#372230=CARTESIAN_POINT('Ctrl Pts',(-1.35705080756888,6.03041012221051E-16,
1.4375));
#372231=CARTESIAN_POINT('Ctrl Pts',(-1.01778810567666,-0.587620236790416,
1.47916666666667));
#372232=CARTESIAN_POINT('Ctrl Pts',(-0.678525403784438,-1.17524047358083,
1.52083333333333));
#372233=CARTESIAN_POINT('Ctrl Pts',(-1.43925448419919E-16,-1.17524047358083,
1.5625));
#372234=CARTESIAN_POINT('Ctrl Pts',(-1.43925448419919E-16,-1.17524047358083,
1.));
#372235=CARTESIAN_POINT('Ctrl Pts',(0.678525403784437,-1.17524047358083,
1.04166666666667));
#372236=CARTESIAN_POINT('Ctrl Pts',(1.01778810567666,-0.587620236790417,
1.08333333333333));
#372237=CARTESIAN_POINT('Ctrl Pts',(1.35705080756888,2.7065942666714E-16,
1.125));
#372238=CARTESIAN_POINT('Ctrl Pts',(1.01778810567666,0.587620236790417,
1.16666666666667));
#372239=CARTESIAN_POINT('Ctrl Pts',(0.678525403784439,1.17524047358083,
1.20833333333333));
#372240=CARTESIAN_POINT('Ctrl Pts',(0.,1.17524047358083,1.25));
#372241=CARTESIAN_POINT('Ctrl Pts',(-0.678525403784438,1.17524047358083,
1.29166666666667));
#372242=CARTESIAN_POINT('Ctrl Pts',(-1.01778810567666,0.587620236790418,
1.33333333333333));
#372243=CARTESIAN_POINT('Ctrl Pts',(-1.35705080756888,6.03041012221051E-16,
1.375));
#372244=CARTESIAN_POINT('Ctrl Pts',(-1.01778810567666,-0.587620236790416,
1.41666666666667));
#372245=CARTESIAN_POINT('Ctrl Pts',(-0.678525403784438,-1.17524047358083,
1.45833333333333));
#372246=CARTESIAN_POINT('Ctrl Pts',(-1.43925448419919E-16,-1.17524047358083,
1.5));
#372247=CARTESIAN_POINT('Origin',(6.93889390390723E-17,9.71445146547012E-16,
-9.21875));
#372248=CARTESIAN_POINT('',(6.93889390390724E-17,-1.17524047358083,2.0625));
#372249=CARTESIAN_POINT('',(6.93889390390724E-17,-1.17524047358083,2.));
#372250=CARTESIAN_POINT('',(2.82703326498063E-16,-1.17524047358083,-9.21875));
#372251=CARTESIAN_POINT('Ctrl Pts',(-1.43925448419919E-16,-1.17524047358083,
1.5625));
#372252=CARTESIAN_POINT('Ctrl Pts',(0.678525403784437,-1.17524047358083,
1.60416666666667));
#372253=CARTESIAN_POINT('Ctrl Pts',(1.01778810567666,-0.587620236790417,
1.64583333333333));
#372254=CARTESIAN_POINT('Ctrl Pts',(1.35705080756888,2.7065942666714E-16,
1.6875));
#372255=CARTESIAN_POINT('Ctrl Pts',(1.01778810567666,0.587620236790417,
1.72916666666667));
#372256=CARTESIAN_POINT('Ctrl Pts',(0.678525403784439,1.17524047358083,
1.77083333333333));
#372257=CARTESIAN_POINT('Ctrl Pts',(0.,1.17524047358083,1.8125));
#372258=CARTESIAN_POINT('Ctrl Pts',(-0.678525403784438,1.17524047358083,
1.85416666666667));
#372259=CARTESIAN_POINT('Ctrl Pts',(-1.01778810567666,0.587620236790418,
1.89583333333333));
#372260=CARTESIAN_POINT('Ctrl Pts',(-1.35705080756888,6.03041012221051E-16,
1.9375));
#372261=CARTESIAN_POINT('Ctrl Pts',(-1.01778810567666,-0.587620236790416,
1.97916666666667));
#372262=CARTESIAN_POINT('Ctrl Pts',(-0.678525403784438,-1.17524047358083,
2.02083333333333));
#372263=CARTESIAN_POINT('Ctrl Pts',(-1.43925448419919E-16,-1.17524047358083,
2.0625));
#372264=CARTESIAN_POINT('Ctrl Pts',(-1.43925448419919E-16,-1.17524047358083,
1.5));
#372265=CARTESIAN_POINT('Ctrl Pts',(0.678525403784437,-1.17524047358083,
1.54166666666667));
#372266=CARTESIAN_POINT('Ctrl Pts',(1.01778810567666,-0.587620236790417,
1.58333333333333));
#372267=CARTESIAN_POINT('Ctrl Pts',(1.35705080756888,2.7065942666714E-16,
1.625));
#372268=CARTESIAN_POINT('Ctrl Pts',(1.01778810567666,0.587620236790417,
1.66666666666667));
#372269=CARTESIAN_POINT('Ctrl Pts',(0.678525403784439,1.17524047358083,
1.70833333333333));
#372270=CARTESIAN_POINT('Ctrl Pts',(0.,1.17524047358083,1.75));
#372271=CARTESIAN_POINT('Ctrl Pts',(-0.678525403784438,1.17524047358083,
1.79166666666667));
#372272=CARTESIAN_POINT('Ctrl Pts',(-1.01778810567666,0.587620236790418,
1.83333333333333));
#372273=CARTESIAN_POINT('Ctrl Pts',(-1.35705080756888,6.03041012221051E-16,
1.875));
#372274=CARTESIAN_POINT('Ctrl Pts',(-1.01778810567666,-0.587620236790416,
1.91666666666667));
#372275=CARTESIAN_POINT('Ctrl Pts',(-0.678525403784438,-1.17524047358083,
1.95833333333333));
#372276=CARTESIAN_POINT('Ctrl Pts',(-1.43925448419919E-16,-1.17524047358083,
2.));
#372277=CARTESIAN_POINT('Origin',(6.93889390390723E-17,9.71445146547012E-16,
-9.21875));
#372278=CARTESIAN_POINT('',(6.93889390390724E-17,-1.17524047358083,2.5625));
#372279=CARTESIAN_POINT('',(6.93889390390724E-17,-1.17524047358083,2.5));
#372280=CARTESIAN_POINT('',(2.82703326498063E-16,-1.17524047358083,-9.21875));
#372281=CARTESIAN_POINT('Ctrl Pts',(-1.43925448419919E-16,-1.17524047358083,
2.0625));
#372282=CARTESIAN_POINT('Ctrl Pts',(0.678525403784437,-1.17524047358083,
2.10416666666667));
#372283=CARTESIAN_POINT('Ctrl Pts',(1.01778810567666,-0.587620236790417,
2.14583333333333));
#372284=CARTESIAN_POINT('Ctrl Pts',(1.35705080756888,2.7065942666714E-16,
2.1875));
#372285=CARTESIAN_POINT('Ctrl Pts',(1.01778810567666,0.587620236790417,
2.22916666666667));
#372286=CARTESIAN_POINT('Ctrl Pts',(0.678525403784439,1.17524047358083,
2.27083333333333));
#372287=CARTESIAN_POINT('Ctrl Pts',(0.,1.17524047358083,2.3125));
#372288=CARTESIAN_POINT('Ctrl Pts',(-0.678525403784438,1.17524047358083,
2.35416666666667));
#372289=CARTESIAN_POINT('Ctrl Pts',(-1.01778810567666,0.587620236790418,
2.39583333333333));
#372290=CARTESIAN_POINT('Ctrl Pts',(-1.35705080756888,6.03041012221051E-16,
2.4375));
#372291=CARTESIAN_POINT('Ctrl Pts',(-1.01778810567666,-0.587620236790416,
2.47916666666667));
#372292=CARTESIAN_POINT('Ctrl Pts',(-0.678525403784438,-1.17524047358083,
2.52083333333333));
#372293=CARTESIAN_POINT('Ctrl Pts',(-1.43925448419919E-16,-1.17524047358083,
2.5625));
#372294=CARTESIAN_POINT('Ctrl Pts',(-1.43925448419919E-16,-1.17524047358083,
2.));
#372295=CARTESIAN_POINT('Ctrl Pts',(0.678525403784437,-1.17524047358083,
2.04166666666667));
#372296=CARTESIAN_POINT('Ctrl Pts',(1.01778810567666,-0.587620236790417,
2.08333333333333));
#372297=CARTESIAN_POINT('Ctrl Pts',(1.35705080756888,2.7065942666714E-16,
2.125));
#372298=CARTESIAN_POINT('Ctrl Pts',(1.01778810567666,0.587620236790417,
2.16666666666667));
#372299=CARTESIAN_POINT('Ctrl Pts',(0.678525403784439,1.17524047358083,
2.20833333333333));
#372300=CARTESIAN_POINT('Ctrl Pts',(0.,1.17524047358083,2.25));
#372301=CARTESIAN_POINT('Ctrl Pts',(-0.678525403784438,1.17524047358083,
2.29166666666667));
#372302=CARTESIAN_POINT('Ctrl Pts',(-1.01778810567666,0.587620236790418,
2.33333333333333));
#372303=CARTESIAN_POINT('Ctrl Pts',(-1.35705080756888,6.03041012221051E-16,
2.375));
#372304=CARTESIAN_POINT('Ctrl Pts',(-1.01778810567666,-0.587620236790416,
2.41666666666667));
#372305=CARTESIAN_POINT('Ctrl Pts',(-0.678525403784438,-1.17524047358083,
2.45833333333333));
#372306=CARTESIAN_POINT('Ctrl Pts',(-1.43925448419919E-16,-1.17524047358083,
2.5));
#372307=CARTESIAN_POINT('Origin',(6.93889390390723E-17,9.71445146547012E-16,
-9.21875));
#372308=CARTESIAN_POINT('',(6.93889390390724E-17,-1.17524047358083,3.0625));
#372309=CARTESIAN_POINT('',(6.93889390390724E-17,-1.17524047358083,3.));
#372310=CARTESIAN_POINT('',(2.82703326498063E-16,-1.17524047358083,-9.21875));
#372311=CARTESIAN_POINT('Ctrl Pts',(-1.43925448419919E-16,-1.17524047358083,
2.5625));
#372312=CARTESIAN_POINT('Ctrl Pts',(0.678525403784437,-1.17524047358083,
2.60416666666667));
#372313=CARTESIAN_POINT('Ctrl Pts',(1.01778810567666,-0.587620236790417,
2.64583333333333));
#372314=CARTESIAN_POINT('Ctrl Pts',(1.35705080756888,2.7065942666714E-16,
2.6875));
#372315=CARTESIAN_POINT('Ctrl Pts',(1.01778810567666,0.587620236790417,
2.72916666666667));
#372316=CARTESIAN_POINT('Ctrl Pts',(0.678525403784439,1.17524047358083,
2.77083333333333));
#372317=CARTESIAN_POINT('Ctrl Pts',(0.,1.17524047358083,2.8125));
#372318=CARTESIAN_POINT('Ctrl Pts',(-0.678525403784438,1.17524047358083,
2.85416666666667));
#372319=CARTESIAN_POINT('Ctrl Pts',(-1.01778810567666,0.587620236790418,
2.89583333333333));
#372320=CARTESIAN_POINT('Ctrl Pts',(-1.35705080756888,6.03041012221051E-16,
2.9375));
#372321=CARTESIAN_POINT('Ctrl Pts',(-1.01778810567666,-0.587620236790416,
2.97916666666667));
#372322=CARTESIAN_POINT('Ctrl Pts',(-0.678525403784438,-1.17524047358083,
3.02083333333333));
#372323=CARTESIAN_POINT('Ctrl Pts',(-1.43925448419919E-16,-1.17524047358083,
3.0625));
#372324=CARTESIAN_POINT('Ctrl Pts',(-1.43925448419919E-16,-1.17524047358083,
2.5));
#372325=CARTESIAN_POINT('Ctrl Pts',(0.678525403784437,-1.17524047358083,
2.54166666666667));
#372326=CARTESIAN_POINT('Ctrl Pts',(1.01778810567666,-0.587620236790417,
2.58333333333333));
#372327=CARTESIAN_POINT('Ctrl Pts',(1.35705080756888,2.7065942666714E-16,
2.625));
#372328=CARTESIAN_POINT('Ctrl Pts',(1.01778810567666,0.587620236790417,
2.66666666666667));
#372329=CARTESIAN_POINT('Ctrl Pts',(0.678525403784439,1.17524047358083,
2.70833333333333));
#372330=CARTESIAN_POINT('Ctrl Pts',(0.,1.17524047358083,2.75));
#372331=CARTESIAN_POINT('Ctrl Pts',(-0.678525403784438,1.17524047358083,
2.79166666666667));
#372332=CARTESIAN_POINT('Ctrl Pts',(-1.01778810567666,0.587620236790418,
2.83333333333333));
#372333=CARTESIAN_POINT('Ctrl Pts',(-1.35705080756888,6.03041012221051E-16,
2.875));
#372334=CARTESIAN_POINT('Ctrl Pts',(-1.01778810567666,-0.587620236790416,
2.91666666666667));
#372335=CARTESIAN_POINT('Ctrl Pts',(-0.678525403784438,-1.17524047358083,
2.95833333333333));
#372336=CARTESIAN_POINT('Ctrl Pts',(-1.43925448419919E-16,-1.17524047358083,
3.));
#372337=CARTESIAN_POINT('Origin',(6.93889390390723E-17,9.71445146547012E-16,
-9.21875));
#372338=CARTESIAN_POINT('',(6.93889390390724E-17,-1.17524047358083,3.5625));
#372339=CARTESIAN_POINT('',(6.93889390390724E-17,-1.17524047358083,3.5));
#372340=CARTESIAN_POINT('',(2.82703326498063E-16,-1.17524047358083,-9.21875));
#372341=CARTESIAN_POINT('Ctrl Pts',(-1.43925448419919E-16,-1.17524047358083,
3.0625));
#372342=CARTESIAN_POINT('Ctrl Pts',(0.678525403784437,-1.17524047358083,
3.10416666666667));
#372343=CARTESIAN_POINT('Ctrl Pts',(1.01778810567666,-0.587620236790417,
3.14583333333333));
#372344=CARTESIAN_POINT('Ctrl Pts',(1.35705080756888,2.7065942666714E-16,
3.1875));
#372345=CARTESIAN_POINT('Ctrl Pts',(1.01778810567666,0.587620236790417,
3.22916666666667));
#372346=CARTESIAN_POINT('Ctrl Pts',(0.678525403784439,1.17524047358083,
3.27083333333333));
#372347=CARTESIAN_POINT('Ctrl Pts',(0.,1.17524047358083,3.3125));
#372348=CARTESIAN_POINT('Ctrl Pts',(-0.678525403784438,1.17524047358083,
3.35416666666667));
#372349=CARTESIAN_POINT('Ctrl Pts',(-1.01778810567666,0.587620236790418,
3.39583333333333));
#372350=CARTESIAN_POINT('Ctrl Pts',(-1.35705080756888,6.03041012221051E-16,
3.4375));
#372351=CARTESIAN_POINT('Ctrl Pts',(-1.01778810567666,-0.587620236790416,
3.47916666666667));
#372352=CARTESIAN_POINT('Ctrl Pts',(-0.678525403784438,-1.17524047358083,
3.52083333333333));
#372353=CARTESIAN_POINT('Ctrl Pts',(-1.43925448419919E-16,-1.17524047358083,
3.5625));
#372354=CARTESIAN_POINT('Ctrl Pts',(-1.43925448419919E-16,-1.17524047358083,
3.));
#372355=CARTESIAN_POINT('Ctrl Pts',(0.678525403784437,-1.17524047358083,
3.04166666666667));
#372356=CARTESIAN_POINT('Ctrl Pts',(1.01778810567666,-0.587620236790417,
3.08333333333333));
#372357=CARTESIAN_POINT('Ctrl Pts',(1.35705080756888,2.7065942666714E-16,
3.125));
#372358=CARTESIAN_POINT('Ctrl Pts',(1.01778810567666,0.587620236790417,
3.16666666666667));
#372359=CARTESIAN_POINT('Ctrl Pts',(0.678525403784439,1.17524047358083,
3.20833333333333));
#372360=CARTESIAN_POINT('Ctrl Pts',(0.,1.17524047358083,3.25));
#372361=CARTESIAN_POINT('Ctrl Pts',(-0.678525403784438,1.17524047358083,
3.29166666666667));
#372362=CARTESIAN_POINT('Ctrl Pts',(-1.01778810567666,0.587620236790418,
3.33333333333333));
#372363=CARTESIAN_POINT('Ctrl Pts',(-1.35705080756888,6.03041012221051E-16,
3.375));
#372364=CARTESIAN_POINT('Ctrl Pts',(-1.01778810567666,-0.587620236790416,
3.41666666666667));
#372365=CARTESIAN_POINT('Ctrl Pts',(-0.678525403784438,-1.17524047358083,
3.45833333333333));
#372366=CARTESIAN_POINT('Ctrl Pts',(-1.43925448419919E-16,-1.17524047358083,
3.5));
#372367=CARTESIAN_POINT('Origin',(6.93889390390723E-17,9.71445146547012E-16,
-9.21875));
#372368=CARTESIAN_POINT('',(6.93889390390724E-17,-1.17524047358083,4.0625));
#372369=CARTESIAN_POINT('',(6.93889390390724E-17,-1.17524047358083,4.));
#372370=CARTESIAN_POINT('',(2.82703326498063E-16,-1.17524047358083,-9.21875));
#372371=CARTESIAN_POINT('Ctrl Pts',(-1.43925448419919E-16,-1.17524047358083,
3.5625));
#372372=CARTESIAN_POINT('Ctrl Pts',(0.678525403784437,-1.17524047358083,
3.60416666666667));
#372373=CARTESIAN_POINT('Ctrl Pts',(1.01778810567666,-0.587620236790417,
3.64583333333333));
#372374=CARTESIAN_POINT('Ctrl Pts',(1.35705080756888,2.7065942666714E-16,
3.6875));
#372375=CARTESIAN_POINT('Ctrl Pts',(1.01778810567666,0.587620236790417,
3.72916666666667));
#372376=CARTESIAN_POINT('Ctrl Pts',(0.678525403784439,1.17524047358083,
3.77083333333333));
#372377=CARTESIAN_POINT('Ctrl Pts',(0.,1.17524047358083,3.8125));
#372378=CARTESIAN_POINT('Ctrl Pts',(-0.678525403784438,1.17524047358083,
3.85416666666667));
#372379=CARTESIAN_POINT('Ctrl Pts',(-1.01778810567666,0.587620236790418,
3.89583333333333));
#372380=CARTESIAN_POINT('Ctrl Pts',(-1.35705080756888,6.03041012221051E-16,
3.9375));
#372381=CARTESIAN_POINT('Ctrl Pts',(-1.01778810567666,-0.587620236790416,
3.97916666666667));
#372382=CARTESIAN_POINT('Ctrl Pts',(-0.678525403784438,-1.17524047358083,
4.02083333333333));
#372383=CARTESIAN_POINT('Ctrl Pts',(-1.43925448419919E-16,-1.17524047358083,
4.0625));
#372384=CARTESIAN_POINT('Ctrl Pts',(-1.43925448419919E-16,-1.17524047358083,
3.5));
#372385=CARTESIAN_POINT('Ctrl Pts',(0.678525403784437,-1.17524047358083,
3.54166666666667));
#372386=CARTESIAN_POINT('Ctrl Pts',(1.01778810567666,-0.587620236790417,
3.58333333333333));
#372387=CARTESIAN_POINT('Ctrl Pts',(1.35705080756888,2.7065942666714E-16,
3.625));
#372388=CARTESIAN_POINT('Ctrl Pts',(1.01778810567666,0.587620236790417,
3.66666666666667));
#372389=CARTESIAN_POINT('Ctrl Pts',(0.678525403784439,1.17524047358083,
3.70833333333333));
#372390=CARTESIAN_POINT('Ctrl Pts',(0.,1.17524047358083,3.75));
#372391=CARTESIAN_POINT('Ctrl Pts',(-0.678525403784438,1.17524047358083,
3.79166666666667));
#372392=CARTESIAN_POINT('Ctrl Pts',(-1.01778810567666,0.587620236790418,
3.83333333333333));
#372393=CARTESIAN_POINT('Ctrl Pts',(-1.35705080756888,6.03041012221051E-16,
3.875));
#372394=CARTESIAN_POINT('Ctrl Pts',(-1.01778810567666,-0.587620236790416,
3.91666666666667));
#372395=CARTESIAN_POINT('Ctrl Pts',(-0.678525403784438,-1.17524047358083,
3.95833333333333));
#372396=CARTESIAN_POINT('Ctrl Pts',(-1.43925448419919E-16,-1.17524047358083,
4.));
#372397=CARTESIAN_POINT('Origin',(6.93889390390723E-17,9.71445146547012E-16,
-9.21875));
#372398=CARTESIAN_POINT('',(6.93889390390724E-17,-1.17524047358083,4.5625));
#372399=CARTESIAN_POINT('',(6.93889390390724E-17,-1.17524047358083,4.5));
#372400=CARTESIAN_POINT('',(2.82703326498063E-16,-1.17524047358083,-9.21875));
#372401=CARTESIAN_POINT('Ctrl Pts',(-1.43925448419919E-16,-1.17524047358083,
4.0625));
#372402=CARTESIAN_POINT('Ctrl Pts',(0.678525403784437,-1.17524047358083,
4.10416666666667));
#372403=CARTESIAN_POINT('Ctrl Pts',(1.01778810567666,-0.587620236790417,
4.14583333333333));
#372404=CARTESIAN_POINT('Ctrl Pts',(1.35705080756888,2.7065942666714E-16,
4.1875));
#372405=CARTESIAN_POINT('Ctrl Pts',(1.01778810567666,0.587620236790417,
4.22916666666667));
#372406=CARTESIAN_POINT('Ctrl Pts',(0.678525403784439,1.17524047358083,
4.27083333333333));
#372407=CARTESIAN_POINT('Ctrl Pts',(0.,1.17524047358083,4.3125));
#372408=CARTESIAN_POINT('Ctrl Pts',(-0.678525403784438,1.17524047358083,
4.35416666666667));
#372409=CARTESIAN_POINT('Ctrl Pts',(-1.01778810567666,0.587620236790418,
4.39583333333333));
#372410=CARTESIAN_POINT('Ctrl Pts',(-1.35705080756888,6.03041012221051E-16,
4.4375));
#372411=CARTESIAN_POINT('Ctrl Pts',(-1.01778810567666,-0.587620236790416,
4.47916666666667));
#372412=CARTESIAN_POINT('Ctrl Pts',(-0.678525403784438,-1.17524047358083,
4.52083333333333));
#372413=CARTESIAN_POINT('Ctrl Pts',(-1.43925448419919E-16,-1.17524047358083,
4.5625));
#372414=CARTESIAN_POINT('Ctrl Pts',(-1.43925448419919E-16,-1.17524047358083,
4.));
#372415=CARTESIAN_POINT('Ctrl Pts',(0.678525403784437,-1.17524047358083,
4.04166666666667));
#372416=CARTESIAN_POINT('Ctrl Pts',(1.01778810567666,-0.587620236790417,
4.08333333333333));
#372417=CARTESIAN_POINT('Ctrl Pts',(1.35705080756888,2.7065942666714E-16,
4.125));
#372418=CARTESIAN_POINT('Ctrl Pts',(1.01778810567666,0.587620236790417,
4.16666666666667));
#372419=CARTESIAN_POINT('Ctrl Pts',(0.678525403784439,1.17524047358083,
4.20833333333333));
#372420=CARTESIAN_POINT('Ctrl Pts',(0.,1.17524047358083,4.25));
#372421=CARTESIAN_POINT('Ctrl Pts',(-0.678525403784438,1.17524047358083,
4.29166666666667));
#372422=CARTESIAN_POINT('Ctrl Pts',(-1.01778810567666,0.587620236790418,
4.33333333333333));
#372423=CARTESIAN_POINT('Ctrl Pts',(-1.35705080756888,6.03041012221051E-16,
4.375));
#372424=CARTESIAN_POINT('Ctrl Pts',(-1.01778810567666,-0.587620236790416,
4.41666666666667));
#372425=CARTESIAN_POINT('Ctrl Pts',(-0.678525403784438,-1.17524047358083,
4.45833333333333));
#372426=CARTESIAN_POINT('Ctrl Pts',(-1.43925448419919E-16,-1.17524047358083,
4.5));
#372427=CARTESIAN_POINT('Origin',(6.93889390390723E-17,9.71445146547012E-16,
-9.21875));
#372428=CARTESIAN_POINT('',(6.93889390390724E-17,-1.17524047358083,5.0625));
#372429=CARTESIAN_POINT('',(6.93889390390724E-17,-1.17524047358083,5.));
#372430=CARTESIAN_POINT('',(2.82703326498063E-16,-1.17524047358083,-9.21875));
#372431=CARTESIAN_POINT('Ctrl Pts',(-1.43925448419919E-16,-1.17524047358083,
4.5625));
#372432=CARTESIAN_POINT('Ctrl Pts',(0.678525403784437,-1.17524047358083,
4.60416666666667));
#372433=CARTESIAN_POINT('Ctrl Pts',(1.01778810567666,-0.587620236790417,
4.64583333333333));
#372434=CARTESIAN_POINT('Ctrl Pts',(1.35705080756888,2.7065942666714E-16,
4.6875));
#372435=CARTESIAN_POINT('Ctrl Pts',(1.01778810567666,0.587620236790417,
4.72916666666667));
#372436=CARTESIAN_POINT('Ctrl Pts',(0.678525403784439,1.17524047358083,
4.77083333333333));
#372437=CARTESIAN_POINT('Ctrl Pts',(0.,1.17524047358083,4.8125));
#372438=CARTESIAN_POINT('Ctrl Pts',(-0.678525403784438,1.17524047358083,
4.85416666666667));
#372439=CARTESIAN_POINT('Ctrl Pts',(-1.01778810567666,0.587620236790418,
4.89583333333333));
#372440=CARTESIAN_POINT('Ctrl Pts',(-1.35705080756888,6.03041012221051E-16,
4.9375));
#372441=CARTESIAN_POINT('Ctrl Pts',(-1.01778810567666,-0.587620236790416,
4.97916666666667));
#372442=CARTESIAN_POINT('Ctrl Pts',(-0.678525403784438,-1.17524047358083,
5.02083333333334));
#372443=CARTESIAN_POINT('Ctrl Pts',(-1.43925448419919E-16,-1.17524047358083,
5.0625));
#372444=CARTESIAN_POINT('Ctrl Pts',(-1.43925448419919E-16,-1.17524047358083,
4.5));
#372445=CARTESIAN_POINT('Ctrl Pts',(0.678525403784437,-1.17524047358083,
4.54166666666667));
#372446=CARTESIAN_POINT('Ctrl Pts',(1.01778810567666,-0.587620236790417,
4.58333333333333));
#372447=CARTESIAN_POINT('Ctrl Pts',(1.35705080756888,2.7065942666714E-16,
4.625));
#372448=CARTESIAN_POINT('Ctrl Pts',(1.01778810567666,0.587620236790417,
4.66666666666667));
#372449=CARTESIAN_POINT('Ctrl Pts',(0.678525403784439,1.17524047358083,
4.70833333333333));
#372450=CARTESIAN_POINT('Ctrl Pts',(0.,1.17524047358083,4.75));
#372451=CARTESIAN_POINT('Ctrl Pts',(-0.678525403784438,1.17524047358083,
4.79166666666667));
#372452=CARTESIAN_POINT('Ctrl Pts',(-1.01778810567666,0.587620236790418,
4.83333333333333));
#372453=CARTESIAN_POINT('Ctrl Pts',(-1.35705080756888,6.03041012221051E-16,
4.875));
#372454=CARTESIAN_POINT('Ctrl Pts',(-1.01778810567666,-0.587620236790416,
4.91666666666667));
#372455=CARTESIAN_POINT('Ctrl Pts',(-0.678525403784438,-1.17524047358083,
4.95833333333333));
#372456=CARTESIAN_POINT('Ctrl Pts',(-1.43925448419919E-16,-1.17524047358083,
5.));
#372457=CARTESIAN_POINT('Origin',(0.,2.04523456705693E-15,3.99999999999998));
#372458=CARTESIAN_POINT('',(-1.02859918696353E-15,-1.5,5.25));
#372459=CARTESIAN_POINT('',(-3.11727555887454E-14,-1.5,5.3125));
#372460=CARTESIAN_POINT('',(-1.83697019872103E-16,-1.5,3.99999999999998));
#372461=CARTESIAN_POINT('',(0.,1.5,5.5));
#372462=CARTESIAN_POINT('Ctrl Pts',(2.34187669256869E-15,-1.5,5.25));
#372463=CARTESIAN_POINT('Ctrl Pts',(0.1013142184298,-1.5,5.25487448260693));
#372464=CARTESIAN_POINT('Ctrl Pts',(0.202585377762413,-1.48973761941226,
5.26003195965966));
#372465=CARTESIAN_POINT('Ctrl Pts',(0.497494643078012,-1.42906343675683,
5.27590618226536));
#372466=CARTESIAN_POINT('Ctrl Pts',(0.682749667466072,-1.35039445539259,
5.28700451826429));
#372467=CARTESIAN_POINT('Ctrl Pts',(1.00543736318142,-1.12954128016014,
5.3086646476862));
#372468=CARTESIAN_POINT('Ctrl Pts',(1.14147220648853,-0.991881889660697,
5.31903349909473));
#372469=CARTESIAN_POINT('Ctrl Pts',(1.35790964618256,-0.667374587809761,
5.33846094198532));
#372470=CARTESIAN_POINT('Ctrl Pts',(1.43414603945203,-0.482241430142021,
5.34820880943671));
#372471=CARTESIAN_POINT('Ctrl Pts',(1.50990524563617,-0.0944424733214634,
5.36975319592674));
#372472=CARTESIAN_POINT('Ctrl Pts',(1.50925882253586,0.104265632731634,
5.38079253515191));
#372473=CARTESIAN_POINT('Ctrl Pts',(1.43263199824449,0.483378097020384,
5.40185433872351));
#372474=CARTESIAN_POINT('Ctrl Pts',(1.35997826725094,0.660697896700975,
5.41125406779552));
#372475=CARTESIAN_POINT('Ctrl Pts',(1.14752287537316,0.986274573606487,
5.43051962918385));
#372476=CARTESIAN_POINT('Ctrl Pts',(1.00682301552788,1.12952668237106,5.44126827959036));
#372477=CARTESIAN_POINT('Ctrl Pts',(0.716631896201004,1.32646655903961,
5.46070065845836));
#372478=CARTESIAN_POINT('Ctrl Pts',(0.578704042072479,1.39218522049725,
5.46916223380784));
#372479=CARTESIAN_POINT('Ctrl Pts',(0.292687271883244,1.4784772415699,5.48532022266499));
#372480=CARTESIAN_POINT('Ctrl Pts',(0.146711014173142,1.50000000000011,
5.49294136303951));
#372481=CARTESIAN_POINT('Ctrl Pts',(-1.07483466571523E-12,1.5,5.50000000000005));
#372482=CARTESIAN_POINT('',(-1.83697019872103E-16,-1.5,5.5));
#372483=CARTESIAN_POINT('Origin',(0.,1.86551418677864E-15,5.5));
#372484=CARTESIAN_POINT('',(-1.83697019872103E-16,-1.5,5.875));
#372485=CARTESIAN_POINT('',(-1.83697019872103E-16,-1.5,3.99999999999998));
#372486=CARTESIAN_POINT('Origin',(0.,1.82058409170907E-15,5.875));
#372487=CARTESIAN_POINT('',(1.05094390383306,1.07028823734363,5.5));
#372488=CARTESIAN_POINT('Origin',(0.,1.86551418677864E-15,5.5));
#372489=CARTESIAN_POINT('Ctrl Pts',(1.05094390383211,1.07028823734456,5.50000000000007));
#372490=CARTESIAN_POINT('Ctrl Pts',(1.15240189416463,0.970663993412324,
5.49235126005502));
#372491=CARTESIAN_POINT('Ctrl Pts',(1.23913482730881,0.857166793728004,
5.48512037742933));
#372492=CARTESIAN_POINT('Ctrl Pts',(1.37842494689544,0.608569005404991,
5.47130938918917));
#372493=CARTESIAN_POINT('Ctrl Pts',(1.43008604020435,0.474609193904058,
5.46386717743895));
#372494=CARTESIAN_POINT('Ctrl Pts',(1.50591325346079,0.144072283175914,
5.44550401573184));
#372495=CARTESIAN_POINT('Ctrl Pts',(1.51182377709547,-0.0540169751539241,
5.43449905693574));
#372496=CARTESIAN_POINT('Ctrl Pts',(1.44639389913366,-0.444944484987569,
5.41278086194498));
#372497=CARTESIAN_POINT('Ctrl Pts',(1.37422890585589,-0.633632259374769,
5.4026833896331));
#372498=CARTESIAN_POINT('Ctrl Pts',(1.16483810558126,-0.964245461497677,
5.38342536999877));
#372499=CARTESIAN_POINT('Ctrl Pts',(1.03247383541499,-1.1048043760253,5.3731525767887));
#372500=CARTESIAN_POINT('Ctrl Pts',(0.716072516089344,-1.33294901920865,
5.35159236001545));
#372501=CARTESIAN_POINT('Ctrl Pts',(0.533315805628695,-1.41601407028835,
5.34049211115374));
#372502=CARTESIAN_POINT('Ctrl Pts',(0.228050315786412,-1.48698613535804,
5.32383357217391));
#372503=CARTESIAN_POINT('Ctrl Pts',(0.11409269091585,-1.5,5.31798928715107));
#372504=CARTESIAN_POINT('Ctrl Pts',(-6.63705201908726E-14,-1.5,5.3125));
#372505=CARTESIAN_POINT('Origin',(0.,2.04523456705693E-15,3.99999999999998));
#372506=CARTESIAN_POINT('',(-9.30610584359856E-14,-1.5,4.74999999999999));
#372507=CARTESIAN_POINT('',(-1.24089882572763E-13,-1.5,4.81249999999999));
#372508=CARTESIAN_POINT('',(-1.83697019872103E-16,-1.5,3.99999999999998));
#372509=CARTESIAN_POINT('Ctrl Pts',(-1.86101134502792E-13,-1.5,4.74999999999999));
#372510=CARTESIAN_POINT('Ctrl Pts',(0.132337359508786,-1.50000000000001,
4.75636708417802));
#372511=CARTESIAN_POINT('Ctrl Pts',(0.264341985951988,-1.48249172459084,
4.76320450071267));
#372512=CARTESIAN_POINT('Ctrl Pts',(0.583774760997631,-1.39586701723942,
4.78097945913859));
#372513=CARTESIAN_POINT('Ctrl Pts',(0.762797992040203,-1.306664258553,4.79207057276601));
#372514=CARTESIAN_POINT('Ctrl Pts',(1.06996317836528,-1.0684234189941,4.81346686578241));
#372515=CARTESIAN_POINT('Ctrl Pts',(1.19699132836069,-0.923897060647313,
4.8235931315638));
#372516=CARTESIAN_POINT('Ctrl Pts',(1.39415333877414,-0.588066282504838,
4.84240772593883));
#372517=CARTESIAN_POINT('Ctrl Pts',(1.45974822466939,-0.398344079750572,
4.85286977334732));
#372518=CARTESIAN_POINT('Ctrl Pts',(1.51269341320913,-0.00736604210121602,
4.87459077543895));
#372519=CARTESIAN_POINT('Ctrl Pts',(1.50075352346208,0.189841157089107,
4.88554673094952));
#372520=CARTESIAN_POINT('Ctrl Pts',(1.40321020875678,0.563169765903798,
4.906287209217));
#372521=CARTESIAN_POINT('Ctrl Pts',(1.32061199135457,0.736297374579946,
4.91524806412427));
#372522=CARTESIAN_POINT('Ctrl Pts',(1.08993684967038,1.04957253614588,4.93504851487444));
#372523=CARTESIAN_POINT('Ctrl Pts',(0.941322354847056,1.18467648763986,
4.94595162063192));
#372524=CARTESIAN_POINT('Ctrl Pts',(0.60474475673763,1.38625828944633,4.96774471236585));
#372525=CARTESIAN_POINT('Ctrl Pts',(0.421081105146126,1.45262981129201,
4.97842488730767));
#372526=CARTESIAN_POINT('Ctrl Pts',(0.0389123015268975,1.51189479414534,
4.9984582419685));
#372527=CARTESIAN_POINT('Ctrl Pts',(-0.155939684676095,1.50433577026112,
5.00738221351442));
#372528=CARTESIAN_POINT('Ctrl Pts',(-0.537476109603411,1.41443190762156,
5.0282362228353));
#372529=CARTESIAN_POINT('Ctrl Pts',(-0.719934574271997,1.33085837095527,
5.03933624693928));
#372530=CARTESIAN_POINT('Ctrl Pts',(-1.03559141172507,1.10187350663975,
5.06088398428763));
#372531=CARTESIAN_POINT('Ctrl Pts',(-1.16752312838274,0.960982260328454,
5.07114519769574));
#372532=CARTESIAN_POINT('Ctrl Pts',(-1.37608593538413,0.629656626788052,
5.09038317024674));
#372533=CARTESIAN_POINT('Ctrl Pts',(-1.44776902614139,0.440547850918076,
5.10052511939358));
#372534=CARTESIAN_POINT('Ctrl Pts',(-1.51197833241709,0.0492603879786804,
5.12226331177909));
#372535=CARTESIAN_POINT('Ctrl Pts',(-1.50545082908663,-0.148747153270871,
5.1332637307374));
#372536=CARTESIAN_POINT('Ctrl Pts',(-1.41794504592827,-0.524896618648321,
5.15416092325837));
#372537=CARTESIAN_POINT('Ctrl Pts',(-1.34016456864257,-0.700019794165874,
5.16329962974384));
#372538=CARTESIAN_POINT('Ctrl Pts',(-1.11829112315409,-1.01930451755138,
5.18284354096112));
#372539=CARTESIAN_POINT('Ctrl Pts',(-0.9734531234724,-1.15841480273464,
5.1936762370583));
#372540=CARTESIAN_POINT('Ctrl Pts',(-0.642123617261976,-1.36941735503731,
5.21547851736679));
#372541=CARTESIAN_POINT('Ctrl Pts',(-0.459826381711669,-1.44090204461358,
5.22623498302315));
#372542=CARTESIAN_POINT('Ctrl Pts',(-0.18001487423605,-1.4919012135564,
5.24111406403517));
#372543=CARTESIAN_POINT('Ctrl Pts',(-0.0900013938564301,-1.5,5.24566980591913));
#372544=CARTESIAN_POINT('Ctrl Pts',(-2.74887016421606E-16,-1.5,5.25));
#372545=CARTESIAN_POINT('Ctrl Pts',(-6.21618141576187E-14,-1.5,5.3125));
#372546=CARTESIAN_POINT('Ctrl Pts',(-0.0781666029860376,-1.49999999999999,
5.30873920756036));
#372547=CARTESIAN_POINT('Ctrl Pts',(-0.156380097833171,-1.49389088525685,
5.3048064614031));
#372548=CARTESIAN_POINT('Ctrl Pts',(-0.425120326327988,-1.45145985509196,
5.29069805140434));
#372549=CARTESIAN_POINT('Ctrl Pts',(-0.608648585849205,-1.38455614161338,
5.28000960741563));
#372550=CARTESIAN_POINT('Ctrl Pts',(-0.944693493081018,-1.18198957786974,
5.25821479028525));
#372551=CARTESIAN_POINT('Ctrl Pts',(-1.09292093000477,-1.04646448570185,
5.24731860850759));
#372552=CARTESIAN_POINT('Ctrl Pts',(-1.32268404489021,-0.732560575680372,
5.22754457243236));
#372553=CARTESIAN_POINT('Ctrl Pts',(-1.4047815617659,-0.55922860385983,
5.21856825576985));
#372554=CARTESIAN_POINT('Ctrl Pts',(-1.50129034805554,-0.185605472482953,
5.19781141513781));
#372555=CARTESIAN_POINT('Ctrl Pts',(-1.51267328803592,0.0116910409612078,
5.18685049772425));
#372556=CARTESIAN_POINT('Ctrl Pts',(-1.4585882153116,0.402573071914142,
5.16513482933798));
#372557=CARTESIAN_POINT('Ctrl Pts',(-1.39244195273024,0.592110506921991,
5.15471304727201));
#372558=CARTESIAN_POINT('Ctrl Pts',(-1.19427093735495,0.927422166609085,
5.13586432708022));
#372559=CARTESIAN_POINT('Ctrl Pts',(-1.06677763582743,1.07161391255723,
5.12572497647415));
#372560=CARTESIAN_POINT('Ctrl Pts',(-0.758802919877356,1.3089975002654,
5.10431354749692));
#372561=CARTESIAN_POINT('Ctrl Pts',(-0.579449637439399,1.39767670128007,
5.093221097533));
#372562=CARTESIAN_POINT('Ctrl Pts',(-0.200110007463219,1.49926990007539,
5.07214807777638));
#372563=CARTESIAN_POINT('Ctrl Pts',(-0.00420925884862429,1.51255730384018,
5.06305133205621));
#372564=CARTESIAN_POINT('Ctrl Pts',(0.380226113100054,1.46378504761527,
5.04320039170437));
#372565=CARTESIAN_POINT('Ctrl Pts',(0.565168529376356,1.40278531907301,
5.03260790864861));
#372566=CARTESIAN_POINT('Ctrl Pts',(0.908448348456497,1.21035688739411,
5.01074661643921));
#372567=CARTESIAN_POINT('Ctrl Pts',(1.0620114849816,1.07814223110912,4.99968567724709));
#372568=CARTESIAN_POINT('Ctrl Pts',(1.30181427141735,0.769134375830037,
4.97956460876981));
#372569=CARTESIAN_POINT('Ctrl Pts',(1.38886175096562,0.597792825375605,
4.97071071252075));
#372570=CARTESIAN_POINT('Ctrl Pts',(1.49550756795418,0.227092567281358,
4.95011625373774));
#372571=CARTESIAN_POINT('Ctrl Pts',(1.51233653549556,0.0307386628157603,
4.93920770348966));
#372572=CARTESIAN_POINT('Ctrl Pts',(1.46944397407567,-0.360886484990905,
4.91745075083374));
#372573=CARTESIAN_POINT('Ctrl Pts',(1.4087453892702,-0.552238149629713,
4.90682010279825));
#372574=CARTESIAN_POINT('Ctrl Pts',(1.2204081434847,-0.892623842777975,
4.88790978651224));
#372575=CARTESIAN_POINT('Ctrl Pts',(1.09748369894562,-1.04007136398357,
4.87807850452959));
#372576=CARTESIAN_POINT('Ctrl Pts',(0.797378551679508,-1.28577242495924,
4.8568146594281));
#372577=CARTESIAN_POINT('Ctrl Pts',(0.621299834175413,-1.37949731331861,
4.84573959906122));
#372578=CARTESIAN_POINT('Ctrl Pts',(0.291688127647154,-1.47865655639298,
4.82712672501815));
#372579=CARTESIAN_POINT('Ctrl Pts',(0.146113885494368,-1.50000000000002,
4.81952990759354));
#372580=CARTESIAN_POINT('Ctrl Pts',(-2.4983487501018E-13,-1.5,4.81249999999999));
#372581=CARTESIAN_POINT('Origin',(0.,2.04523456705693E-15,3.99999999999998));
#372582=CARTESIAN_POINT('',(-9.30610584359856E-14,-1.5,4.24999999999999));
#372583=CARTESIAN_POINT('',(-3.11727555887454E-14,-1.5,4.3125));
#372584=CARTESIAN_POINT('',(-1.83697019872103E-16,-1.5,3.99999999999998));
#372585=CARTESIAN_POINT('Ctrl Pts',(-1.85858273216155E-13,-1.5,4.24999999999999));
#372586=CARTESIAN_POINT('Ctrl Pts',(0.163534910421258,-1.50000000000002,
4.25786807704614));
#372587=CARTESIAN_POINT('Ctrl Pts',(0.326190684501579,-1.47326229929913,
4.26643657053385));
#372588=CARTESIAN_POINT('Ctrl Pts',(0.667990021365253,-1.35740629940923,
4.28609962101527));
#372589=CARTESIAN_POINT('Ctrl Pts',(0.840196725402017,-1.25810649223897,
4.2971432479032));
#372590=CARTESIAN_POINT('Ctrl Pts',(1.13122312734384,-1.00320978004929,
4.31822572642256));
#372591=CARTESIAN_POINT('Ctrl Pts',(1.2490305329715,-0.852050769110481,
4.32766384616067));
#372592=CARTESIAN_POINT('Ctrl Pts',(1.42604267402587,-0.505912163077925,
4.34689376871803));
#372593=CARTESIAN_POINT('Ctrl Pts',(1.48046532813874,-0.312640018756726,
4.35763111006921));
#372594=CARTESIAN_POINT('Ctrl Pts',(1.51047312143187,0.0796059131719647,
4.37942255073191));
#372595=CARTESIAN_POINT('Ctrl Pts',(1.4874208354067,0.274691213374741,4.3902606229654));
#372596=CARTESIAN_POINT('Ctrl Pts',(1.36911846990398,0.641930210830453,
4.41066278949071));
#372597=CARTESIAN_POINT('Ctrl Pts',(1.27625099543952,0.811012624525723,
4.41945780714498));
#372598=CARTESIAN_POINT('Ctrl Pts',(1.02638328536396,1.11199346834159,4.43984015194602));
#372599=CARTESIAN_POINT('Ctrl Pts',(0.869168052732768,1.23875949404383,
4.45092545184444));
#372600=CARTESIAN_POINT('Ctrl Pts',(0.521083697970173,1.41967196683104,
4.47269801463766));
#372601=CARTESIAN_POINT('Ctrl Pts',(0.334912309122096,1.47473694490812,
4.48318477248426));
#372602=CARTESIAN_POINT('Ctrl Pts',(-0.0519432957329438,1.51189047531382,
4.50282941396224));
#372603=CARTESIAN_POINT('Ctrl Pts',(-0.249069874090919,1.49214228260642,
4.51220164983219));
#372604=CARTESIAN_POINT('Ctrl Pts',(-0.625765335375153,1.37746828716819,
4.5335108074256));
#372605=CARTESIAN_POINT('Ctrl Pts',(-0.80148385209002,1.2832077073044,4.54458341794351));
#372606=CARTESIAN_POINT('Ctrl Pts',(-1.1007294145725,1.03662777910022,4.56583031923137));
#372607=CARTESIAN_POINT('Ctrl Pts',(-1.22316683171971,0.888831648925115,
4.57562046394874));
#372608=CARTESIAN_POINT('Ctrl Pts',(-1.41043936006761,0.547898537307782,
4.59456119237192));
#372609=CARTESIAN_POINT('Ctrl Pts',(-1.47054956730788,0.356356974518528,
4.60520239030466));
#372610=CARTESIAN_POINT('Ctrl Pts',(-1.51222837316115,-0.0353448297905851,
4.62696360165516));
#372611=CARTESIAN_POINT('Ctrl Pts',(-1.49481056950729,-0.231587514103256,
4.63786597300586));
#372612=CARTESIAN_POINT('Ctrl Pts',(-1.38706553932082,-0.601965922302877,
4.65844255123917));
#372613=CARTESIAN_POINT('Ctrl Pts',(-1.29947526964824,-0.773093177466047,
4.66728711075724));
#372614=CARTESIAN_POINT('Ctrl Pts',(-1.05872747359096,-1.08135566705396,
4.68743294142861));
#372615=CARTESIAN_POINT('Ctrl Pts',(-0.904815168934766,-1.21306506743986,
4.69849664509418));
#372616=CARTESIAN_POINT('Ctrl Pts',(-0.561070447600619,-1.40442192262524,
4.72035053891));
#372617=CARTESIAN_POINT('Ctrl Pts',(-0.376005221910598,-1.46486781226288,
4.73093354622241));
#372618=CARTESIAN_POINT('Ctrl Pts',(-0.123202739728906,-1.49620944194601,
4.74396711214189));
#372619=CARTESIAN_POINT('Ctrl Pts',(-0.0615704629692202,-1.49999999999999,
4.74703768971922));
#372620=CARTESIAN_POINT('Ctrl Pts',(-1.85938419852099E-13,-1.5,4.74999999999999));
#372621=CARTESIAN_POINT('Ctrl Pts',(-2.47996068125655E-13,-1.5,4.81249999999999));
#372622=CARTESIAN_POINT('Ctrl Pts',(-0.0492637934033634,-1.49999999999999,
4.81012979463477));
#372623=CARTESIAN_POINT('Ctrl Pts',(-0.0985824301404427,-1.49757322656534,
4.80768954024514));
#372624=CARTESIAN_POINT('Ctrl Pts',(-0.339292525452773,-1.47374263063355,
4.7954464093866));
#372625=CARTESIAN_POINT('Ctrl Pts',(-0.525353669177403,-1.41810503365377,
4.78494904963034));
#372626=CARTESIAN_POINT('Ctrl Pts',(-0.872991424837885,-1.23607824286241,
4.76316702056855));
#372627=CARTESIAN_POINT('Ctrl Pts',(-1.02986284823744,-1.10878319847344,
4.75208356723598));
#372628=CARTESIAN_POINT('Ctrl Pts',(-1.27876514977376,-0.807023777370858,
4.73172604352809));
#372629=CARTESIAN_POINT('Ctrl Pts',(-1.37107046921521,-0.637726763123372,
4.72292926461787));
#372630=CARTESIAN_POINT('Ctrl Pts',(-1.48825946539048,-0.270152588186515,
4.70250847712138));
#372631=CARTESIAN_POINT('Ctrl Pts',(-1.51071949717048,-0.0749376417989757,
4.69166320232207));
#372632=CARTESIAN_POINT('Ctrl Pts',(-1.47948007658163,0.317267354827136,
4.66987403584285));
#372633=CARTESIAN_POINT('Ctrl Pts',(-1.42445466752569,0.510365031604566,
4.65914638713299));
#372634=CARTESIAN_POINT('Ctrl Pts',(-1.24635752091359,0.85595920847827,
4.63994671064001));
#372635=CARTESIAN_POINT('Ctrl Pts',(-1.12806576335496,1.00676220302361,
4.63047513926063));
#372636=CARTESIAN_POINT('Ctrl Pts',(-0.836175776888841,1.26079227363434,
4.60937518488867));
#372637=CARTESIAN_POINT('Ctrl Pts',(-0.663594441140983,1.35956972361122,
4.59832804344617));
#372638=CARTESIAN_POINT('Ctrl Pts',(-0.289247880464149,1.48509060641666,
4.57683059495905));
#372639=CARTESIAN_POINT('Ctrl Pts',(-0.0910715305443453,1.51024593205019,
4.5671662902798));
#372640=CARTESIAN_POINT('Ctrl Pts',(0.297701778274559,1.4826354295215,4.54769446733454));
#372641=CARTESIAN_POINT('Ctrl Pts',(0.484737018724916,1.43242588434229,
4.53730102054439));
#372642=CARTESIAN_POINT('Ctrl Pts',(0.836463753097666,1.26098931384478,
4.51561643318852));
#372643=CARTESIAN_POINT('Ctrl Pts',(0.996521375751348,1.13873717146129,
4.50451976438413));
#372644=CARTESIAN_POINT('Ctrl Pts',(1.25453023926176,0.84439732766198,4.48393020037851));
#372645=CARTESIAN_POINT('Ctrl Pts',(1.35217355313513,0.677110988015738,
4.4751172771119));
#372646=CARTESIAN_POINT('Ctrl Pts',(1.47982766403363,0.31272423517926,4.45487356862099));
#372647=CARTESIAN_POINT('Ctrl Pts',(1.50783339833044,0.118797860144214,
4.44409988111904));
#372648=CARTESIAN_POINT('Ctrl Pts',(1.48817173561793,-0.273638462821338,
4.42229786317651));
#372649=CARTESIAN_POINT('Ctrl Pts',(1.4388361788813,-0.468300107990309,
4.41148332733379));
#372650=CARTESIAN_POINT('Ctrl Pts',(1.27096497526889,-0.818967732484933,
4.39200179263965));
#372651=CARTESIAN_POINT('Ctrl Pts',(1.15719181702216,-0.973131571865142,
4.38281065136992));
#372652=CARTESIAN_POINT('Ctrl Pts',(0.873387965745884,-1.23521327749103,
4.36187608483048));
#372653=CARTESIAN_POINT('Ctrl Pts',(0.704364537477269,-1.338815408904,4.3508661043626));
#372654=CARTESIAN_POINT('Ctrl Pts',(0.353475962893003,-1.46855342446925,
4.33038013618092));
#372655=CARTESIAN_POINT('Ctrl Pts',(0.17734521529577,-1.5,4.32103252564921));
#372656=CARTESIAN_POINT('Ctrl Pts',(-5.98132654516803E-14,-1.5,4.3125));
#372657=CARTESIAN_POINT('Origin',(0.,2.04523456705693E-15,3.99999999999998));
#372658=CARTESIAN_POINT('',(-2.29292018146855E-16,-1.5,3.75));
#372659=CARTESIAN_POINT('',(-4.8449908341125E-15,-1.5,3.8125));
#372660=CARTESIAN_POINT('',(-1.83697019872103E-16,-1.5,3.99999999999998));
#372661=CARTESIAN_POINT('Ctrl Pts',(2.42861286636753E-15,-1.5,3.75));
#372662=CARTESIAN_POINT('Ctrl Pts',(0.193317174447722,-1.5,3.7593009768922));
#372663=CARTESIAN_POINT('Ctrl Pts',(0.384935667136526,-1.46262884767149,
3.76955831348497));
#372664=CARTESIAN_POINT('Ctrl Pts',(0.745639566529835,-1.31618466565995,
3.79098058188077));
#372665=CARTESIAN_POINT('Ctrl Pts',(0.910865964988617,-1.20774522917046,
3.80194224725221));
#372666=CARTESIAN_POINT('Ctrl Pts',(1.18629623939077,-0.937468647541969,
3.82270157533098));
#372667=CARTESIAN_POINT('Ctrl Pts',(1.29542242527005,-0.779754510200248,
3.83168030498901));
#372668=CARTESIAN_POINT('Ctrl Pts',(1.45254177348479,-0.423894276102234,
3.85145031799445));
#372669=CARTESIAN_POINT('Ctrl Pts',(1.49588111718185,-0.227782106418506,
3.86234543853244));
#372670=CARTESIAN_POINT('Ctrl Pts',(1.50345672710943,0.164529044750317,
3.88414050248626));
#372671=CARTESIAN_POINT('Ctrl Pts',(1.46971337247465,0.356943553614525,
3.89483019742316));
#372672=CARTESIAN_POINT('Ctrl Pts',(1.33112237295684,0.717914269568467,
3.91488412608726));
#372673=CARTESIAN_POINT('Ctrl Pts',(1.22776875417754,0.883105026681858,
3.92379297679183));
#372674=CARTESIAN_POINT('Ctrl Pts',(0.960169961217741,1.16944379999735,
3.94462168453532));
#372675=CARTESIAN_POINT('Ctrl Pts',(0.796899563869198,1.28626107029131,
3.95572195936514));
#372676=CARTESIAN_POINT('Ctrl Pts',(0.441174140060695,1.44636211553748,
3.97728405805476));
#372677=CARTESIAN_POINT('Ctrl Pts',(0.253275421369734,1.49079566610575,
3.98755860466638));
#372678=CARTESIAN_POINT('Ctrl Pts',(-0.137708502264893,1.50698986612346,
4.00681966635236));
#372679=CARTESIAN_POINT('Ctrl Pts',(-0.337180643988774,1.47523796094839,
4.01691044571594));
#372680=CARTESIAN_POINT('Ctrl Pts',(-0.708493892957603,1.33662597697244,
4.03862559562465));
#372681=CARTESIAN_POINT('Ctrl Pts',(-0.877146433261387,1.2325377380485,
4.04963123472341));
#372682=CARTESIAN_POINT('Ctrl Pts',(-1.16012139503677,0.969638499902146,
4.07054863053483));
#372683=CARTESIAN_POINT('Ctrl Pts',(-1.27343327571507,0.815126535815214,
4.07971519245486));
#372684=CARTESIAN_POINT('Ctrl Pts',(-1.4402476744218,0.463942020344171,
4.09922544331436));
#372685=CARTESIAN_POINT('Ctrl Pts',(-1.48899427959348,0.269128999797649,
4.11004838890027));
#372686=CARTESIAN_POINT('Ctrl Pts',(-1.50746366959263,-0.123311635354483,
4.13185064640872));
#372687=CARTESIAN_POINT('Ctrl Pts',(-1.47888959224984,-0.317096438885883,
4.14261646882713));
#372688=CARTESIAN_POINT('Ctrl Pts',(-1.35015742029248,-0.681150531106146,
4.1628416961727));
#372689=CARTESIAN_POINT('Ctrl Pts',(-1.25195759418559,-0.848229850102839,
4.17166043577936));
#372690=CARTESIAN_POINT('Ctrl Pts',(-0.993006531798035,-1.14179263176492,
4.19227374629023));
#372691=CARTESIAN_POINT('Ctrl Pts',(-0.832626718069013,-1.26351647183078,
4.20337124145558));
#372692=CARTESIAN_POINT('Ctrl Pts',(-0.4804930256072,-1.43384767725927,
4.22504470400639));
#372693=CARTESIAN_POINT('Ctrl Pts',(-0.293365512428091,-1.48349245009655,
4.23542690214965));
#372694=CARTESIAN_POINT('Ctrl Pts',(-0.0679647259223738,-1.49884641485544,
4.24669800156779));
#372695=CARTESIAN_POINT('Ctrl Pts',(-0.0339649311946905,-1.49999999999999,
4.24836586148598));
#372696=CARTESIAN_POINT('Ctrl Pts',(-1.85938419852099E-13,-1.5,4.24999999999999));
#372697=CARTESIAN_POINT('Ctrl Pts',(-6.21618141576187E-14,-1.5,4.3125));
#372698=CARTESIAN_POINT('Ctrl Pts',(-0.0220361068876159,-1.5,4.31143978731305));
#372699=CARTESIAN_POINT('Ctrl Pts',(-0.0440896866934215,-1.49951441502509,
4.31036524548832));
#372700=CARTESIAN_POINT('Ctrl Pts',(-0.257374002006283,-1.49010014052068,
4.29984209145821));
#372701=CARTESIAN_POINT('Ctrl Pts',(-0.445200616684323,-1.44513467194479,
4.28955623845232));
#372702=CARTESIAN_POINT('Ctrl Pts',(-0.800572894706048,-1.28398687415068,
4.26798205403763));
#372703=CARTESIAN_POINT('Ctrl Pts',(-0.963555031472045,-1.16666615388507,
4.25688166343012));
#372704=CARTESIAN_POINT('Ctrl Pts',(-1.23027480355594,-0.879585335516549,
4.23607463523564));
#372705=CARTESIAN_POINT('Ctrl Pts',(-1.33310063097869,-0.71420340219919,
4.22717796678877));
#372706=CARTESIAN_POINT('Ctrl Pts',(-1.4706923207297,-0.352916777050933,
4.20710648761387));
#372707=CARTESIAN_POINT('Ctrl Pts',(-1.50391414802456,-0.160357206271801,
4.19640873368169));
#372708=CARTESIAN_POINT('Ctrl Pts',(-1.49523538390863,0.231980923190581,
4.17461217093378));
#372709=CARTESIAN_POINT('Ctrl Pts',(-1.45134634220585,0.427968435029026,
4.16372397583165));
#372710=CARTESIAN_POINT('Ctrl Pts',(-1.29324177051268,0.783359016052853,
4.14398005466366));
#372711=CARTESIAN_POINT('Ctrl Pts',(-1.18369387177651,0.940746994757387,
4.13498530366013));
#372712=CARTESIAN_POINT('Ctrl Pts',(-0.907501794458939,1.21028380197535,
4.11420987261069));
#372713=CARTESIAN_POINT('Ctrl Pts',(-0.741925439127871,1.31828993756297,
4.10324340606755));
#372714=CARTESIAN_POINT('Ctrl Pts',(-0.375817827893553,1.46571065719209,
4.08153402541964));
#372715=CARTESIAN_POINT('Ctrl Pts',(-0.178470546812078,1.50254525226168,
4.07115736963867));
#372716=CARTESIAN_POINT('Ctrl Pts',(0.211061997787556,1.49728809463546,
4.05226994419216));
#372717=CARTESIAN_POINT('Ctrl Pts',(0.399615093233784,1.45832188862504,
4.04211578454639));
#372718=CARTESIAN_POINT('Ctrl Pts',(0.758793702467989,1.30901333118062,
4.02068733572334));
#372719=CARTESIAN_POINT('Ctrl Pts',(0.924938044307028,1.19740529082038,
4.00959348900624));
#372720=CARTESIAN_POINT('Ctrl Pts',(1.20152709152664,0.91876120286303,3.98854597871294));
#372721=CARTESIAN_POINT('Ctrl Pts',(1.31033315597123,0.755519761486827,
3.97947332008253));
#372722=CARTESIAN_POINT('Ctrl Pts',(1.45911184323506,0.397812888832886,
3.9596007160462));
#372723=CARTESIAN_POINT('Ctrl Pts',(1.49813742054345,0.206955371786397,
3.94899752065473));
#372724=CARTESIAN_POINT('Ctrl Pts',(1.50180400732931,-0.186695812584385,
3.92712801041191));
#372725=CARTESIAN_POINT('Ctrl Pts',(1.4633855571079,-0.385733709395978,
3.91607034947793));
#372726=CARTESIAN_POINT('Ctrl Pts',(1.31440271657819,-0.747402673668362,
3.89597762924058));
#372727=CARTESIAN_POINT('Ctrl Pts',(1.20901812608092,-0.908045177286519,
3.88711210123208));
#372728=CARTESIAN_POINT('Ctrl Pts',(0.940358863902646,-1.18484804164848,
3.86649725799934));
#372729=CARTESIAN_POINT('Ctrl Pts',(0.778280646850072,-1.29707823040083,
3.85558176090246));
#372730=CARTESIAN_POINT('Ctrl Pts',(0.417063112188425,-1.45449684338638,
3.83382993491346));
#372731=CARTESIAN_POINT('Ctrl Pts',(0.220852438302694,-1.49691451375519,
3.82321147584329));
#372732=CARTESIAN_POINT('Ctrl Pts',(0.0147017533215045,-1.49994598046505,
3.81320883897905));
#372733=CARTESIAN_POINT('Ctrl Pts',(0.00734980117470292,-1.5,3.81285361747389));
#372734=CARTESIAN_POINT('Ctrl Pts',(-1.70803542250024E-16,-1.5,3.8125));
#372735=CARTESIAN_POINT('Origin',(0.,2.04523456705693E-15,3.99999999999998));
#372736=CARTESIAN_POINT('',(3.08529632092537E-14,-1.5,3.25));
#372737=CARTESIAN_POINT('',(9.27932528099019E-14,-1.5,3.31250000000001));
#372738=CARTESIAN_POINT('',(-1.83697019872103E-16,-1.5,3.99999999999998));
#372739=CARTESIAN_POINT('Ctrl Pts',(6.18896234383795E-14,-1.5,3.25));
#372740=CARTESIAN_POINT('Ctrl Pts',(0.0236193760181181,-1.5,3.25113638775851));
#372741=CARTESIAN_POINT('Ctrl Pts',(0.0472571121222557,-1.49944213161188,
3.25228915521126));
#372742=CARTESIAN_POINT('Ctrl Pts',(0.26952666508563,-1.48892536666519,
3.26327523642389));
#372743=CARTESIAN_POINT('Ctrl Pts',(0.46428967906935,-1.44012316639196,
3.27400139297746));
#372744=CARTESIAN_POINT('Ctrl Pts',(0.819657363376108,-1.27124126752953,
3.29579019251773));
#372745=CARTESIAN_POINT('Ctrl Pts',(0.977550814569531,-1.15425150163482,
3.30663656044951));
#372746=CARTESIAN_POINT('Ctrl Pts',(1.2374143858276,-0.869097677339169,
3.32706019191482));
#372747=CARTESIAN_POINT('Ctrl Pts',(1.33794863026607,-0.704568367963706,
3.33585731289099));
#372748=CARTESIAN_POINT('Ctrl Pts',(1.47500556900581,-0.33820133932665,
3.35621103670416));
#372749=CARTESIAN_POINT('Ctrl Pts',(1.50690689687966,-0.138704427976324,
3.36729419844584));
#372750=CARTESIAN_POINT('Ctrl Pts',(1.49090952643366,0.253397825780057,
3.38907765698787));
#372751=CARTESIAN_POINT('Ctrl Pts',(1.44614680111722,0.442379325511738,
3.39957662919518));
#372752=CARTESIAN_POINT('Ctrl Pts',(1.28614841229457,0.79640059753073,3.41924447764068));
#372753=CARTESIAN_POINT('Ctrl Pts',(1.1711814584489,0.957485365441749,3.42858165484803));
#372754=CARTESIAN_POINT('Ctrl Pts',(0.884638191269975,1.22737339053452,
3.44986486380396));
#372755=CARTESIAN_POINT('Ctrl Pts',(0.715474203179367,1.33308805117331,
3.46094028832681));
#372756=CARTESIAN_POINT('Ctrl Pts',(0.352688975476681,1.47031697544214,
3.48220671529584));
#372757=CARTESIAN_POINT('Ctrl Pts',(0.16354229998072,1.50313990839815,3.49204434774589));
#372758=CARTESIAN_POINT('Ctrl Pts',(-0.22541776572076,1.49623432439379,
3.51095001941019));
#372759=CARTESIAN_POINT('Ctrl Pts',(-0.421502081379421,1.45321725354962,
3.52157904908053));
#372760=CARTESIAN_POINT('Ctrl Pts',(-0.782187844893288,1.29471707709067,
3.54333533364808));
#372761=CARTESIAN_POINT('Ctrl Pts',(-0.943880324387888,1.18203523116139,
3.55424481797074));
#372762=CARTESIAN_POINT('Ctrl Pts',(-1.21171955625412,0.904447836702659,
3.57484199997938));
#372763=CARTESIAN_POINT('Ctrl Pts',(-1.31665163765559,0.743446995699806,
3.5836973891279));
#372764=CARTESIAN_POINT('Ctrl Pts',(-1.46452924323748,0.381335799830201,
3.60381467778732));
#372765=CARTESIAN_POINT('Ctrl Pts',(-1.50234222138092,0.182246636753049,
3.61487518684716));
#372766=CARTESIAN_POINT('Ctrl Pts',(-1.49752713751633,-0.21127662527178,
3.63673759029298));
#372767=CARTESIAN_POINT('Ctrl Pts',(-1.45796575375281,-0.401967180432297,
3.64733151002412));
#372768=CARTESIAN_POINT('Ctrl Pts',(-1.30814645231051,-0.759336240874781,
3.66718534671537));
#372769=CARTESIAN_POINT('Ctrl Pts',(-1.1987759596943,-0.92237829952708,
3.67627881751247));
#372770=CARTESIAN_POINT('Ctrl Pts',(-0.92126584426853,-1.20022289459525,
3.69734843458468));
#372771=CARTESIAN_POINT('Ctrl Pts',(-0.754834825628767,-1.311291111728,
3.70844107895614));
#372772=CARTESIAN_POINT('Ctrl Pts',(-0.395318964041526,-1.45948519404714,
3.72985479619822));
#372773=CARTESIAN_POINT('Ctrl Pts',(-0.206707458644523,-1.49788856755131,
3.73999613185777));
#372774=CARTESIAN_POINT('Ctrl Pts',(-0.0106224566113999,-1.49997179727876,
3.74948814340919));
#372775=CARTESIAN_POINT('Ctrl Pts',(-0.00531062459895978,-1.5,3.74974449245485));
#372776=CARTESIAN_POINT('Ctrl Pts',(-2.74887016421606E-16,-1.5,3.75));
#372777=CARTESIAN_POINT('Ctrl Pts',(1.00613961606655E-15,-1.5,3.8125));
#372778=CARTESIAN_POINT('Ctrl Pts',(-0.182773440490596,-1.5,3.80370630874434));
#372779=CARTESIAN_POINT('Ctrl Pts',(-0.364128623411885,-1.46659527466693,
3.7940529444007));
#372780=CARTESIAN_POINT('Ctrl Pts',(-0.719708419004184,-1.33081615141452,
3.77317346119616));
#372781=CARTESIAN_POINT('Ctrl Pts',(-0.888588458717918,-1.22452674710187,
3.76209573304391));
#372782=CARTESIAN_POINT('Ctrl Pts',(-1.17417053184609,-0.953781845274569,
3.7408349674268));
#372783=CARTESIAN_POINT('Ctrl Pts',(-1.28853656997239,-0.79248842607806,
3.73152713478205));
#372784=CARTESIAN_POINT('Ctrl Pts',(-1.44745392865247,-0.438107871400596,
3.71183932618886));
#372785=CARTESIAN_POINT('Ctrl Pts',(-1.49166782250349,-0.248938403619751,
3.70132991131215));
#372786=CARTESIAN_POINT('Ctrl Pts',(-1.50648239108423,0.143329287662172,
3.67953726179648));
#372787=CARTESIAN_POINT('Ctrl Pts',(-1.47395433674677,0.342790948256581,
3.66845605843013));
#372788=CARTESIAN_POINT('Ctrl Pts',(-1.33574739983272,0.708712101293154,
3.64812710548365));
#372789=CARTESIAN_POINT('Ctrl Pts',(-1.23474837821021,0.872864648331606,
3.63932728548026));
#372790=CARTESIAN_POINT('Ctrl Pts',(-0.974041709728056,1.15722403395568,
3.61888515822173));
#372791=CARTESIAN_POINT('Ctrl Pts',(-0.815742745402805,1.27376574153387,
3.60803172609465));
#372792=CARTESIAN_POINT('Ctrl Pts',(-0.45980061970787,1.44156217831801,
3.5862454404546));
#372793=CARTESIAN_POINT('Ctrl Pts',(-0.26489011284581,1.48975679839026,
3.57552906487442));
#372794=CARTESIAN_POINT('Ctrl Pts',(0.123531837441048,1.50692421504699,
3.55636423239308));
#372795=CARTESIAN_POINT('Ctrl Pts',(0.313201827534702,1.47919447145629,
3.54685313869835));
#372796=CARTESIAN_POINT('Ctrl Pts',(0.678774778125591,1.35206517988781,
3.52573313270211));
#372797=CARTESIAN_POINT('Ctrl Pts',(0.850301629224248,1.25132059946621,
3.51468208266359));
#372798=CARTESIAN_POINT('Ctrl Pts',(1.14507492269931,0.988874219287773,
3.4932096187416));
#372799=CARTESIAN_POINT('Ctrl Pts',(1.26524264242336,0.829583920442607,
3.48358799558008));
#372800=CARTESIAN_POINT('Ctrl Pts',(1.43448023552564,0.478669870633699,
3.4640927705907));
#372801=CARTESIAN_POINT('Ctrl Pts',(1.48389686604776,0.291356187896974,
3.45368645488311));
#372802=CARTESIAN_POINT('Ctrl Pts',(1.50995189198597,-0.0991931473211767,
3.43198926959321));
#372803=CARTESIAN_POINT('Ctrl Pts',(1.48339355440948,-0.298913730684295,
3.42089368162859));
#372804=CARTESIAN_POINT('Ctrl Pts',(1.35617351730245,-0.66903123867981,
3.40033159785107));
#372805=CARTESIAN_POINT('Ctrl Pts',(1.25959301474578,-0.836800304160145,
3.39152441095101));
#372806=CARTESIAN_POINT('Ctrl Pts',(1.00689720493403,-1.12865830545299,
3.37125941143027));
#372807=CARTESIAN_POINT('Ctrl Pts',(0.852486342285255,-1.24938664153487,
3.3604767504461));
#372808=CARTESIAN_POINT('Ctrl Pts',(0.502115094222749,-1.42737944320944,
3.33867526142305));
#372809=CARTESIAN_POINT('Ctrl Pts',(0.308678900877465,-1.48130708221946,
3.32787056825897));
#372810=CARTESIAN_POINT('Ctrl Pts',(0.0735707215714186,-1.49864822341032,
3.31607722234164));
#372811=CARTESIAN_POINT('Ctrl Pts',(0.0367671122311343,-1.5,3.31426895851199));
#372812=CARTESIAN_POINT('Ctrl Pts',(1.85770202639676E-13,-1.5,3.31250000000001));
#372813=CARTESIAN_POINT('Origin',(0.,2.04523456705693E-15,3.99999999999998));
#372814=CARTESIAN_POINT('',(1.08281712706529E-13,-1.5,2.75000000000001));
#372815=CARTESIAN_POINT('',(6.17977475022196E-14,-1.5,2.8125));
#372816=CARTESIAN_POINT('',(-1.83697019872103E-16,-1.5,3.99999999999998));
#372817=CARTESIAN_POINT('Ctrl Pts',(2.16747122432931E-13,-1.5,2.75000000000001));
#372818=CARTESIAN_POINT('Ctrl Pts',(0.0522124451313231,-1.5,2.75251207243764));
#372819=CARTESIAN_POINT('Ctrl Pts',(0.10447874118418,-1.49727405122371,
2.75510245657833));
#372820=CARTESIAN_POINT('Ctrl Pts',(0.354406824394528,-1.47104006355408,
2.76785584896801));
#372821=CARTESIAN_POINT('Ctrl Pts',(0.546107038494388,-1.41113817496362,
2.77874297116893));
#372822=CARTESIAN_POINT('Ctrl Pts',(0.890309400649009,-1.22263015121861,
2.80053974903232));
#372823=CARTESIAN_POINT('Ctrl Pts',(1.04051930921944,-1.09763783034302,
2.81123873554121));
#372824=CARTESIAN_POINT('Ctrl Pts',(1.28472571765059,-0.797945454648135,
2.83131291005875));
#372825=CARTESIAN_POINT('Ctrl Pts',(1.37660375336644,-0.626260206772226,
2.84020776629049));
#372826=CARTESIAN_POINT('Ctrl Pts',(1.49202937496029,-0.251793770944039,
2.86101145716983));
#372827=CARTESIAN_POINT('Ctrl Pts',(1.5122301925727,-0.0519865643527668,
2.87211185753601));
#372828=CARTESIAN_POINT('Ctrl Pts',(1.47426865201774,0.336381921397972,
2.89368788452216));
#372829=CARTESIAN_POINT('Ctrl Pts',(1.41937297020844,0.521558431255365,
2.90397546840313));
#372830=CARTESIAN_POINT('Ctrl Pts',(1.23907502217178,0.868665674093023,
2.92325920411633));
#372831=CARTESIAN_POINT('Ctrl Pts',(1.11252577833543,1.02577158220901,2.93330056692789));
#372832=CARTESIAN_POINT('Ctrl Pts',(0.807873326352072,1.27902322098119,
2.95499293260172));
#372833=CARTESIAN_POINT('Ctrl Pts',(0.633675855472049,1.37368732240572,
2.96600357070002));
#372834=CARTESIAN_POINT('Ctrl Pts',(0.264849678828112,1.48860078663452,
2.9869407690705));
#372835=CARTESIAN_POINT('Ctrl Pts',(0.0744641039108102,1.51013733163361,
2.99613575158486));
#372836=CARTESIAN_POINT('Ctrl Pts',(-0.313170845636526,1.48036428077972,
3.01561287598095));
#372837=CARTESIAN_POINT('Ctrl Pts',(-0.506445454007791,1.4258491961316,
3.02642611281874));
#372838=CARTESIAN_POINT('Ctrl Pts',(-0.856226709513093,1.24681742407431,
3.04822807610006));
#372839=CARTESIAN_POINT('Ctrl Pts',(-1.01023130739802,1.12566531934954,
3.05900296201285));
#372840=CARTESIAN_POINT('Ctrl Pts',(-1.26209924684952,0.83303798094694,
3.07924950107758));
#372841=CARTESIAN_POINT('Ctrl Pts',(-1.35822194558857,0.664891162678306,
3.08806160207349));
#372842=CARTESIAN_POINT('Ctrl Pts',(-1.48429856811928,0.294344634871367,
3.10864752028499));
#372843=CARTESIAN_POINT('Ctrl Pts',(-1.5102380377602,0.09460703958459,3.11974405335647));
#372844=CARTESIAN_POINT('Ctrl Pts',(-1.48302106788286,-0.295745923053602,
3.14143032905859));
#372845=CARTESIAN_POINT('Ctrl Pts',(-1.43306828305171,-0.482858861267118,
3.15182549229268));
#372846=CARTESIAN_POINT('Ctrl Pts',(-1.26275751331793,-0.833407725948767,
3.17130042921943));
#372847=CARTESIAN_POINT('Ctrl Pts',(-1.14197808626569,-0.992488035128005,
3.18095899912744));
#372848=CARTESIAN_POINT('Ctrl Pts',(-0.846247312071301,-1.25405610530601,
3.20245313236201));
#372849=CARTESIAN_POINT('Ctrl Pts',(-0.674453619273247,-1.35421681136905,
3.21350080209559));
#372850=CARTESIAN_POINT('Ctrl Pts',(-0.330944750833914,-1.47246172076396,
3.23331246105066));
#372851=CARTESIAN_POINT('Ctrl Pts',(-0.165961922362418,-1.5,3.2420151532874));
#372852=CARTESIAN_POINT('Ctrl Pts',(6.6717464886068E-14,-1.5,3.25));
#372853=CARTESIAN_POINT('Ctrl Pts',(1.88425663960601E-13,-1.5,3.31250000000001));
#372854=CARTESIAN_POINT('Ctrl Pts',(-0.152607701100013,-1.5,3.30515765855747));
#372855=CARTESIAN_POINT('Ctrl Pts',(-0.304524679208517,-1.4767167661864,
3.29720179304546));
#372856=CARTESIAN_POINT('Ctrl Pts',(-0.637881204779632,-1.37174810773761,
3.27824737366289));
#372857=CARTESIAN_POINT('Ctrl Pts',(-0.811840182694752,-1.27651825179612,
3.26723249465947));
#372858=CARTESIAN_POINT('Ctrl Pts',(-1.11558185250335,-1.02240635105325,
3.2455600528476));
#372859=CARTESIAN_POINT('Ctrl Pts',(-1.24153613759052,-0.865097180051025,
3.23556095444722));
#372860=CARTESIAN_POINT('Ctrl Pts',(-1.42081536541909,-0.517635286571265,
3.21625751592057));
#372861=CARTESIAN_POINT('Ctrl Pts',(-1.47521081639495,-0.332255685912234,
3.20595864921729));
#372862=CARTESIAN_POINT('Ctrl Pts',(-1.51208229193674,0.0563280922715262,
3.18437066154042));
#372863=CARTESIAN_POINT('Ctrl Pts',(-1.49129795191174,0.2561354974193,3.17327025014332));
#372864=CARTESIAN_POINT('Ctrl Pts',(-1.37478505061458,0.630208162207134,
3.15248843543289));
#372865=CARTESIAN_POINT('Ctrl Pts',(-1.28247518031101,0.801530606296313,
3.14360504348462));
#372866=CARTESIAN_POINT('Ctrl Pts',(-1.03749078900277,1.10051002620746,
3.12351324257578));
#372867=CARTESIAN_POINT('Ctrl Pts',(-0.886892799455015,1.22511913749658,
3.11280622922291));
#372868=CARTESIAN_POINT('Ctrl Pts',(-0.542114383767811,1.4126764710966,
3.09100814403059));
#372869=CARTESIAN_POINT('Ctrl Pts',(-0.350247890791992,1.47203555681224,
3.08012809959115));
#372870=CARTESIAN_POINT('Ctrl Pts',(0.0366799443214752,1.51154513430789,
3.06041453718074));
#372871=CARTESIAN_POINT('Ctrl Pts',(0.227673498706082,1.49475418374031,
3.05140033656785));
#372872=CARTESIAN_POINT('Ctrl Pts',(0.598892177156894,1.38913607705811,
3.03060623327681));
#372873=CARTESIAN_POINT('Ctrl Pts',(0.774981653006425,1.29914199429579,
3.01963428878759));
#372874=CARTESIAN_POINT('Ctrl Pts',(1.08494916107576,1.0547200111272,2.99793147056981));
#372875=CARTESIAN_POINT('Ctrl Pts',(1.21501958033426,0.901790420280011,
2.98759946779328));
#372876=CARTESIAN_POINT('Ctrl Pts',(1.40413285092575,0.561118340799233,
2.96867324115546));
#372877=CARTESIAN_POINT('Ctrl Pts',(1.46406184662414,0.378076856399767,
2.95850426979994));
#372878=CARTESIAN_POINT('Ctrl Pts',(1.51302625577521,-0.00793947459916036,
2.93705891807778));
#372879=CARTESIAN_POINT('Ctrl Pts',(1.49873234713959,-0.207651602247236,
2.92596379987511));
#372880=CARTESIAN_POINT('Ctrl Pts',(1.39437436880055,-0.586042286108765,
2.90494209521614));
#372881=CARTESIAN_POINT('Ctrl Pts',(1.30687737144127,-0.761440127297383,
2.89589271886943));
#372882=CARTESIAN_POINT('Ctrl Pts',(1.07053769069727,-1.06828631993652,
2.87599831532686));
#372883=CARTESIAN_POINT('Ctrl Pts',(0.924283752090724,-1.19706732666361,
2.86538441923795));
#372884=CARTESIAN_POINT('Ctrl Pts',(0.584410274341166,-1.39598135855799,
2.84350685914068));
#372885=CARTESIAN_POINT('Ctrl Pts',(0.392530146371773,-1.4615871174733,
2.83245263998732));
#372886=CARTESIAN_POINT('Ctrl Pts',(0.129150917970223,-1.49583416689111,
2.81882949402433));
#372887=CARTESIAN_POINT('Ctrl Pts',(0.0645467119743484,-1.5,2.8156055051278));
#372888=CARTESIAN_POINT('Ctrl Pts',(1.23779192024311E-13,-1.5,2.8125));
#372889=CARTESIAN_POINT('Origin',(0.,2.04523456705693E-15,3.99999999999998));
#372890=CARTESIAN_POINT('',(1.53125027804872E-14,-1.5,2.25));
#372891=CARTESIAN_POINT('',(1.52431070176988E-14,-1.5,2.3125));
#372892=CARTESIAN_POINT('',(-1.83697019872103E-16,-1.5,3.99999999999998));
#372893=CARTESIAN_POINT('Ctrl Pts',(3.08087025808465E-14,-1.5,2.25));
#372894=CARTESIAN_POINT('Ctrl Pts',(0.0808582836836842,-1.5,2.25389029598758));
#372895=CARTESIAN_POINT('Ctrl Pts',(0.16175453469314,-1.49346296475911,
2.25796400299127));
#372896=CARTESIAN_POINT('Ctrl Pts',(0.43941581054574,-1.44809001830053,
2.27258334697821));
#372897=CARTESIAN_POINT('Ctrl Pts',(0.628462258701575,-1.37661598127761,
2.28366423837319));
#372898=CARTESIAN_POINT('Ctrl Pts',(0.960882035050376,-1.16779804180548,
2.30545829063843));
#372899=CARTESIAN_POINT('Ctrl Pts',(1.10266810963985,-1.03498199083381,
2.31596931108195));
#372900=CARTESIAN_POINT('Ctrl Pts',(1.33024348271686,-0.720282150838644,
2.33566019854628));
#372901=CARTESIAN_POINT('Ctrl Pts',(1.41281889958196,-0.540655708541785,
2.34496357174773));
#372902=CARTESIAN_POINT('Ctrl Pts',(1.50468845633309,-0.158024426932706,
2.36622086517045));
#372903=CARTESIAN_POINT('Ctrl Pts',(1.5123965356432,0.0413809023853515,
2.37729893902146));
#372904=CARTESIAN_POINT('Ctrl Pts',(1.45121353764186,0.424524588612146,
2.39858469936739));
#372905=CARTESIAN_POINT('Ctrl Pts',(1.38569001068393,0.605026344035973,
2.40847057894424));
#372906=CARTESIAN_POINT('Ctrl Pts',(1.18638164624256,0.939163043957149,
2.42734138209721));
#372907=CARTESIAN_POINT('Ctrl Pts',(1.05161195027867,1.08794060110316,2.43795820203822));
#372908=CARTESIAN_POINT('Ctrl Pts',(0.734778389573018,1.32220909884669,
2.45970932210568));
#372909=CARTESIAN_POINT('Ctrl Pts',(0.556575816602285,1.40654416171405,
2.47062573803046));
#372910=CARTESIAN_POINT('Ctrl Pts',(0.182569497469227,1.50097846673481,
2.4912433005891));
#372911=CARTESIAN_POINT('Ctrl Pts',(-0.00923039425979297,1.51201094511843,
2.50011046018654));
#372912=CARTESIAN_POINT('Ctrl Pts',(-0.396962349093565,1.46038094829539,
2.52019938913968));
#372913=CARTESIAN_POINT('Ctrl Pts',(-0.588583117065401,1.3942181726357,
2.53125660251669));
#372914=CARTESIAN_POINT('Ctrl Pts',(-0.927767071615718,1.19436080871201,
2.55312719158105));
#372915=CARTESIAN_POINT('Ctrl Pts',(-1.0736052072278,1.06519365227555,2.56373180871987));
#372916=CARTESIAN_POINT('Ctrl Pts',(-1.30912426207158,0.757606940798347,
2.58360729984813));
#372917=CARTESIAN_POINT('Ctrl Pts',(-1.39616247157342,0.58181724405329,
2.59267681977487));
#372918=CARTESIAN_POINT('Ctrl Pts',(-1.49935819859759,0.203023435309446,
2.61372092026064));
#372919=CARTESIAN_POINT('Ctrl Pts',(-1.51303547644827,0.00333102406007514,
2.62481494310783));
#372920=CARTESIAN_POINT('Ctrl Pts',(-1.46292579985952,-0.382421581918602,
2.64624564343997));
#372921=CARTESIAN_POINT('Ctrl Pts',(-1.4024745750708,-0.56523185884661,
2.65640176993597));
#372922=CARTESIAN_POINT('Ctrl Pts',(-1.21240661635006,-0.90529816770916,
2.67529434265056));
#372923=CARTESIAN_POINT('Ctrl Pts',(-1.08189976900056,-1.05784684540797,
2.68566504102233));
#372924=CARTESIAN_POINT('Ctrl Pts',(-0.771275797713282,-1.30133724975859,
2.70737356615202));
#372925=CARTESIAN_POINT('Ctrl Pts',(-0.594982522266591,-1.39080747307205,
2.71834076430257));
#372926=CARTESIAN_POINT('Ctrl Pts',(-0.27394416727951,-1.4811861030294,
2.73629724685739));
#372927=CARTESIAN_POINT('Ctrl Pts',(-0.13718321777196,-1.5,2.74339976935758));
#372928=CARTESIAN_POINT('Ctrl Pts',(2.12121986642444E-13,-1.5,2.75000000000001));
#372929=CARTESIAN_POINT('Ctrl Pts',(1.25732757538799E-13,-1.5,2.8125));
#372930=CARTESIAN_POINT('Ctrl Pts',(-0.125068644536108,-1.5,2.80648263203416));
#372931=CARTESIAN_POINT('Ctrl Pts',(-0.249879261089443,-1.48436218482603,
2.80004329469055));
#372932=CARTESIAN_POINT('Ctrl Pts',(-0.560819973154951,-1.40486536800048,
2.78287490779431));
#372933=CARTESIAN_POINT('Ctrl Pts',(-0.738819729590105,-1.31996381251163,
2.7719525139785));
#372934=CARTESIAN_POINT('Ctrl Pts',(-1.05497027342245,-1.08468356605574,
2.75020615144477));
#372935=CARTESIAN_POINT('Ctrl Pts',(-1.18927677596674,-0.935493387614889,
2.73960015520493));
#372936=CARTESIAN_POINT('Ctrl Pts',(-1.38757347699829,-0.600708235287357,
2.72076001316361));
#372937=CARTESIAN_POINT('Ctrl Pts',(-1.45254878301697,-0.419955776142848,
2.71083087645234));
#372938=CARTESIAN_POINT('Ctrl Pts',(-1.51253033572044,-0.0365073802504774,
2.68952818779166));
#372939=CARTESIAN_POINT('Ctrl Pts',(-1.50417280301816,0.162937666001922,
2.6784479074443));
#372940=CARTESIAN_POINT('Ctrl Pts',(-1.41106400963208,0.54515718868444,
2.6572134895175));
#372941=CARTESIAN_POINT('Ctrl Pts',(-1.32800083044783,0.724362315220717,
2.64793896098909));
#372942=CARTESIAN_POINT('Ctrl Pts',(-1.09956096666915,1.03829286473376,
2.62822784987654));
#372943=CARTESIAN_POINT('Ctrl Pts',(-0.957331683565913,1.17071965804038,
2.61770631826639));
#372944=CARTESIAN_POINT('Ctrl Pts',(-0.624168195026001,1.37857754843603,
2.59590315216156));
#372945=CARTESIAN_POINT('Ctrl Pts',(-0.434836132007832,1.44948073533607,
2.58482437606297));
#372946=CARTESIAN_POINT('Ctrl Pts',(-0.0486163057092892,1.51132307459164,
2.56452452324922));
#372947=CARTESIAN_POINT('Ctrl Pts',(0.143934424738931,1.5052396812014,2.55572049846095));
#372948=CARTESIAN_POINT('Ctrl Pts',(0.520236531724272,1.4203186948451,2.53525673860956));
#372949=CARTESIAN_POINT('Ctrl Pts',(0.700094458610885,1.34082435632475,
2.52439514399756));
#372950=CARTESIAN_POINT('Ctrl Pts',(1.02261141707528,1.11524984086218,2.50261208083574));
#372951=CARTESIAN_POINT('Ctrl Pts',(1.16127195756225,0.970045360100909,
2.49190731467214));
#372952=CARTESIAN_POINT('Ctrl Pts',(1.36916321610676,0.641468401698581,
2.4727780040985));
#372953=CARTESIAN_POINT('Ctrl Pts',(1.43933947070695,0.463059693474664,
2.46322553852634));
#372954=CARTESIAN_POINT('Ctrl Pts',(1.51063981501737,0.0825332381250036,
2.4420851798958));
#372955=CARTESIAN_POINT('Ctrl Pts',(1.50840435404898,-0.116454606961533,
2.43103029961322));
#372956=CARTESIAN_POINT('Ctrl Pts',(1.42705084815203,-0.502498436699463,
2.40958342018333));
#372957=CARTESIAN_POINT('Ctrl Pts',(1.34861280625527,-0.68571361679187,
2.40000423009386));
#372958=CARTESIAN_POINT('Ctrl Pts',(1.12832858207098,-1.00685537477425,
2.38048519602788));
#372959=CARTESIAN_POINT('Ctrl Pts',(0.990299485101312,-1.14287804995166,
2.37006586035978));
#372960=CARTESIAN_POINT('Ctrl Pts',(0.66422042262994,-1.35964487887696,
2.34835607334839));
#372961=CARTESIAN_POINT('Ctrl Pts',(0.477633199931601,-1.43586269523415,
2.33726172984523));
#372962=CARTESIAN_POINT('Ctrl Pts',(0.1885624580824,-1.49111209387676,2.32181910177559));
#372963=CARTESIAN_POINT('Ctrl Pts',(0.0942846646342436,-1.5,2.31703627304225));
#372964=CARTESIAN_POINT('Ctrl Pts',(3.06699110552697E-14,-1.5,2.3125));
#372965=CARTESIAN_POINT('Origin',(0.,2.04523456705693E-15,3.99999999999998));
#372966=CARTESIAN_POINT('',(-1.56323089387029E-14,-1.5,1.75));
#372967=CARTESIAN_POINT('',(-6.21522480643445E-14,-1.5,1.81249999999999));
#372968=CARTESIAN_POINT('',(-1.83697019872103E-16,-1.5,3.99999999999998));
#372969=CARTESIAN_POINT('Ctrl Pts',(-3.27862736959617E-14,-1.5,1.75));
#372970=CARTESIAN_POINT('Ctrl Pts',(0.110465980352864,-1.5,1.75531479695775));
#372971=CARTESIAN_POINT('Ctrl Pts',(0.220826650588412,-1.48780022182646,
1.7609634099072));
#372972=CARTESIAN_POINT('Ctrl Pts',(0.523187787936054,-1.41980742425771,
1.7773994557319));
#372973=CARTESIAN_POINT('Ctrl Pts',(0.706663478164997,-1.33798206582024,
1.78849986061712));
#372974=CARTESIAN_POINT('Ctrl Pts',(1.02486460638805,-1.11188867721038,
1.81008969144261));
#372975=CARTESIAN_POINT('Ctrl Pts',(1.15827642974689,-0.972142672853255,
1.82039030424109));
#372976=CARTESIAN_POINT('Ctrl Pts',(1.36967438783033,-0.643260876612614,
1.83969679869269));
#372977=CARTESIAN_POINT('Ctrl Pts',(1.44300442220864,-0.45559082607096,
1.84968939855165));
#372978=CARTESIAN_POINT('Ctrl Pts',(1.51138716216324,-0.0655426848016987,
1.87135873973328));
#372979=CARTESIAN_POINT('Ctrl Pts',(1.50697374411077,0.132736822001649,
1.88237426788902));
#372980=CARTESIAN_POINT('Ctrl Pts',(1.42338094597886,0.50996348712316,1.90333130484022));
#372981=CARTESIAN_POINT('Ctrl Pts',(1.34745527842838,0.685872585531904,
1.91255587728802));
#372982=CARTESIAN_POINT('Ctrl Pts',(1.12898409138924,1.00744632259985,1.93199968098273));
#372983=CARTESIAN_POINT('Ctrl Pts',(0.9856297739892,1.14807028978956,1.94280304010526));
#372984=CARTESIAN_POINT('Ctrl Pts',(0.65639193832536,1.36266393223992,1.96460443737176));
#372985=CARTESIAN_POINT('Ctrl Pts',(0.474658265785483,1.43611088421253,
1.97538829587892));
#372986=CARTESIAN_POINT('Ctrl Pts',(0.0955931180921214,1.5091936725856,
1.99565615375549));
#372987=CARTESIAN_POINT('Ctrl Pts',(-0.0979742429755275,1.50904098461822,
2.00446264950139));
#372988=CARTESIAN_POINT('Ctrl Pts',(-0.482146305565531,1.43434467581502,
2.02502103394744));
#372989=CARTESIAN_POINT('Ctrl Pts',(-0.668434095227935,1.35756902850466,
2.0361164662762));
#372990=CARTESIAN_POINT('Ctrl Pts',(-0.993748366577721,1.13987096052055,
2.05781532500923));
#372991=CARTESIAN_POINT('Ctrl Pts',(-1.13132684273033,1.00347457456687,
2.06822336102806));
#372992=CARTESIAN_POINT('Ctrl Pts',(-1.35074056268981,0.681569212981403,
2.0877217241512));
#372993=CARTESIAN_POINT('Ctrl Pts',(-1.42868159347472,0.497921452399993,
2.09733769708893));
#372994=CARTESIAN_POINT('Ctrl Pts',(-1.50877191600071,0.111477628688774,
2.11880679840622));
#372995=CARTESIAN_POINT('Ctrl Pts',(-1.51035481506967,-0.0874505114863162,
2.12985836174928));
#372996=CARTESIAN_POINT('Ctrl Pts',(-1.43784842849668,-0.467658955411782,
2.15098105307848));
#372997=CARTESIAN_POINT('Ctrl Pts',(-1.36711298429262,-0.645820324970424,
2.16049753268028));
#372998=CARTESIAN_POINT('Ctrl Pts',(-1.15819103191155,-0.973722457299709,
2.17965768736555));
#372999=CARTESIAN_POINT('Ctrl Pts',(-1.01906810208961,-1.118489200093,2.19037254085841));
#373000=CARTESIAN_POINT('Ctrl Pts',(-0.695882317517152,-1.34300659885496,
2.21215841857856));
#373001=CARTESIAN_POINT('Ctrl Pts',(-0.515833568513887,-1.42191558898578,
2.22301293444644));
#373002=CARTESIAN_POINT('Ctrl Pts',(-0.218540308087038,-1.48805180668198,
2.23915358026597));
#373003=CARTESIAN_POINT('Ctrl Pts',(-0.109320999056845,-1.5,2.24474029098054));
#373004=CARTESIAN_POINT('Ctrl Pts',(3.46944695195361E-14,-1.5,2.25));
#373005=CARTESIAN_POINT('Ctrl Pts',(3.06699110552697E-14,-1.5,2.3125));
#373006=CARTESIAN_POINT('Ctrl Pts',(-0.0965880711665686,-1.5,2.30785290425929));
#373007=CARTESIAN_POINT('Ctrl Pts',(-0.193158137690027,-1.4906725807854,
2.30294757978916));
#373008=CARTESIAN_POINT('Ctrl Pts',(-0.479015211220926,-1.43467130791224,
2.28763868401328));
#373009=CARTESIAN_POINT('Ctrl Pts',(-0.660579011765522,-1.36064740788891,
2.27684697214157));
#373010=CARTESIAN_POINT('Ctrl Pts',(-0.989193594360455,-1.14500049552058,
2.2550463036546));
#373011=CARTESIAN_POINT('Ctrl Pts',(-1.13210802585101,-1.00393400821821,
2.24425181632741));
#373012=CARTESIAN_POINT('Ctrl Pts',(-1.34957613319165,-0.681688912067382,
2.22483762446378));
#373013=CARTESIAN_POINT('Ctrl Pts',(-1.42495560561359,-0.505546483895616,
2.21558591577195));
#373014=CARTESIAN_POINT('Ctrl Pts',(-1.50739111574804,-0.128003682012438,
2.19461131566733));
#373015=CARTESIAN_POINT('Ctrl Pts',(-1.51117896410855,0.0703519564588762,
2.18359155797448));
#373016=CARTESIAN_POINT('Ctrl Pts',(-1.44156601709098,0.460030181085983,
2.16194276771742));
#373017=CARTESIAN_POINT('Ctrl Pts',(-1.36775091328919,0.647276578730561,
2.15199270819955));
#373018=CARTESIAN_POINT('Ctrl Pts',(-1.1555150408507,0.975433740479151,
2.13266602831064));
#373019=CARTESIAN_POINT('Ctrl Pts',(-1.02166635155199,1.11483732583894,
2.12235390842865));
#373020=CARTESIAN_POINT('Ctrl Pts',(-0.702715978000763,1.34006834118604,
2.10075198433335));
#373021=CARTESIAN_POINT('Ctrl Pts',(-0.518941844775744,1.42137322325474,
2.0896516782797));
#373022=CARTESIAN_POINT('Ctrl Pts',(-0.136491021717308,1.50615937001468,
2.06889583373266));
#373023=CARTESIAN_POINT('Ctrl Pts',(0.0579178943444623,1.51122112856893,
2.06002512202488));
#373024=CARTESIAN_POINT('Ctrl Pts',(0.439062286518284,1.44732779216569,
2.03991248900632));
#373025=CARTESIAN_POINT('Ctrl Pts',(0.62211066169564,1.37858561025607,2.02919606489633));
#373026=CARTESIAN_POINT('Ctrl Pts',(0.956291225897921,1.17262469136765,
2.00739665836887));
#373027=CARTESIAN_POINT('Ctrl Pts',(1.10317084007132,1.0356521579006,1.99652511704077));
#373028=CARTESIAN_POINT('Ctrl Pts',(1.32977620972735,0.71958221691235,1.97684284052687));
#373029=CARTESIAN_POINT('Ctrl Pts',(1.41014293676257,0.545538436502839,
1.9678076909168));
#373030=CARTESIAN_POINT('Ctrl Pts',(1.50306004150702,0.170899505389093,
1.94699441696604));
#373031=CARTESIAN_POINT('Ctrl Pts',(1.51250765220232,-0.0266949177684643,
1.93601694901284));
#373032=CARTESIAN_POINT('Ctrl Pts',(1.45446866407842,-0.417219669807208,
1.91432112945513));
#373033=CARTESIAN_POINT('Ctrl Pts',(1.38641298054374,-0.606104201316678,
1.90403426447937));
#373034=CARTESIAN_POINT('Ctrl Pts',(1.18475132210135,-0.939591370600925,
1.88506828093367));
#373035=CARTESIAN_POINT('Ctrl Pts',(1.05565072199852,-1.0826106135082,1.87488416866775));
#373036=CARTESIAN_POINT('Ctrl Pts',(0.744885128346205,-1.31699893814408,
1.85342166527648));
#373037=CARTESIAN_POINT('Ctrl Pts',(0.564398045291385,-1.40385240762055,
1.84232538006989));
#373038=CARTESIAN_POINT('Ctrl Pts',(0.250343776141915,-1.48430541194397,
1.82498063132477));
#373039=CARTESIAN_POINT('Ctrl Pts',(0.125295181136604,-1.5,1.81852826721312));
#373040=CARTESIAN_POINT('Ctrl Pts',(-1.25906229886397E-13,-1.49999999999999,
1.81249999999999));
#373041=CARTESIAN_POINT('Origin',(0.,2.04523456705693E-15,3.99999999999998));
#373042=CARTESIAN_POINT('',(-1.08601518864753E-13,-1.5,1.24999999999999));
#373043=CARTESIAN_POINT('',(-1.08584123502877E-13,-1.5,1.31249999999999));
#373044=CARTESIAN_POINT('',(-1.83697019872103E-16,-1.5,3.99999999999998));
#373045=CARTESIAN_POINT('Ctrl Pts',(-2.14515905039292E-13,-1.5,1.24999999999999));
#373046=CARTESIAN_POINT('Ctrl Pts',(0.142046010209568,-1.50000000000002,
1.25683419185265));
#373047=CARTESIAN_POINT('Ctrl Pts',(0.283618928461168,-1.47982853466809,
1.26420594053933));
#373048=CARTESIAN_POINT('Ctrl Pts',(0.610273392442458,-1.38443304740553,
1.28257198541148));
#373049=CARTESIAN_POINT('Ctrl Pts',(0.787232533826629,-1.29203315350746,
1.29365259979035));
#373050=CARTESIAN_POINT('Ctrl Pts',(1.08945269237421,-1.04850212355775,
1.31495792477995));
#373051=CARTESIAN_POINT('Ctrl Pts',(1.21357794911698,-0.901910093035529,
1.32489388372028));
#373052=CARTESIAN_POINT('Ctrl Pts',(1.40452842820938,-0.562873685428105,
1.34372923969847));
#373053=CARTESIAN_POINT('Ctrl Pts',(1.46666942429647,-0.371996296491918,
1.35433353908381));
#373054=CARTESIAN_POINT('Ctrl Pts',(1.51254266554068,0.0194245347427818,
1.37607914081908));
#373055=CARTESIAN_POINT('Ctrl Pts',(1.49716203510275,0.216044242038897,
1.38700245789108));
#373056=CARTESIAN_POINT('Ctrl Pts',(1.39321705231764,0.587531249040284,
1.40764062494672));
#373057=CARTESIAN_POINT('Ctrl Pts',(1.30749811300545,0.759400562987588,
1.41652076112397));
#373058=CARTESIAN_POINT('Ctrl Pts',(1.07001351269348,1.07022980169436,1.43658088980348));
#373059=CARTESIAN_POINT('Ctrl Pts',(0.917312276987485,1.20367827683049,
1.44763463351896));
#373060=CARTESIAN_POINT('Ctrl Pts',(0.575184773746649,1.39872671094257,
1.46951326275207));
#373061=CARTESIAN_POINT('Ctrl Pts',(0.390550034024555,1.46108197715838,
1.48012859653698));
#373062=CARTESIAN_POINT('Ctrl Pts',(0.00667963752372162,1.51250336222095,
1.50002594140708));
#373063=CARTESIAN_POINT('Ctrl Pts',(-0.188950779722364,1.50067134499163,
1.50907225015607));
#373064=CARTESIAN_POINT('Ctrl Pts',(-0.568861669400175,1.40204066404771,
1.53009046249537));
#373065=CARTESIAN_POINT('Ctrl Pts',(-0.749014905039891,1.31464516172283,
1.54118574192872));
#373066=CARTESIAN_POINT('Ctrl Pts',(-1.05895709623939,1.07936663988191,
1.56263335705116));
#373067=CARTESIAN_POINT('Ctrl Pts',(-1.18758289078589,0.935998387392519,
1.57280431993471));
#373068=CARTESIAN_POINT('Ctrl Pts',(-1.38821273327314,0.601967247945771,
1.59173577049441));
#373069=CARTESIAN_POINT('Ctrl Pts',(-1.45570368464549,0.412887480677177,
1.60206180662908));
#373070=CARTESIAN_POINT('Ctrl Pts',(-1.51257219096668,0.0222530178901751,
1.62376372122836));
#373071=CARTESIAN_POINT('Ctrl Pts',(-1.50255110561474,-0.175255140108835,
1.63473639667275));
#373072=CARTESIAN_POINT('Ctrl Pts',(-1.40857020455048,-0.549594300042889,
1.65553301666909));
#373073=CARTESIAN_POINT('Ctrl Pts',(-1.32769205341188,-0.723426877757731,
1.66454991067901));
#373074=CARTESIAN_POINT('Ctrl Pts',(-1.10015281575383,-1.0388579891019,
1.68425937267021));
#373075=CARTESIAN_POINT('Ctrl Pts',(-0.952873363457998,-1.17540418952279,
1.69513830863433));
#373076=CARTESIAN_POINT('Ctrl Pts',(-0.618138225247735,-1.38036373829122,
1.71693658127953));
#373077=CARTESIAN_POINT('Ctrl Pts',(-0.434946138927554,-1.44856289323058,
1.7276448356126));
#373078=CARTESIAN_POINT('Ctrl Pts',(-0.163054354521467,-1.4933575782512,
1.74197053199517));
#373079=CARTESIAN_POINT('Ctrl Pts',(-0.0815074860315138,-1.49999999999999,
1.7460784692499));
#373080=CARTESIAN_POINT('Ctrl Pts',(-3.10809208575337E-14,-1.5,1.75));
#373081=CARTESIAN_POINT('Ctrl Pts',(-1.24120799108817E-13,-1.5,1.81249999999999));
#373082=CARTESIAN_POINT('Ctrl Pts',(-0.0679352573890632,-1.49999999999999,
1.80923146340491));
#373083=CARTESIAN_POINT('Ctrl Pts',(-0.13593055666763,-1.49538533503665,
1.80583185290518));
#373084=CARTESIAN_POINT('Ctrl Pts',(-0.394898614181489,-1.45992007408125,
1.7923871002911));
#373085=CARTESIAN_POINT('Ctrl Pts',(-0.579400643834895,-1.39699345401102,
1.78176228058195));
#373086=CARTESIAN_POINT('Ctrl Pts',(-0.92103628833535,-1.20084185565978,
1.75987667246243));
#373087=CARTESIAN_POINT('Ctrl Pts',(-1.07337112290149,-1.06687452860672,
1.74882614467676));
#373088=CARTESIAN_POINT('Ctrl Pts',(-1.3098763453813,-0.755278781434875,
1.72879184443336));
#373089=CARTESIAN_POINT('Ctrl Pts',(-1.39503524027109,-0.58318558970749,
1.71989919942817));
#373090=CARTESIAN_POINT('Ctrl Pts',(-1.49783729078981,-0.211367390247104,
1.69924263279148));
#373091=CARTESIAN_POINT('Ctrl Pts',(-1.51260439447891,-0.0146384036827817,
1.68831324464902));
#373092=CARTESIAN_POINT('Ctrl Pts',(-1.46547054554408,0.376689140912213,
1.66657282550485));
#373093=CARTESIAN_POINT('Ctrl Pts',(-1.40272058491593,0.567362552788369,
1.6559798581784));
#373094=CARTESIAN_POINT('Ctrl Pts',(-1.21066545730874,0.905826170861375,
1.63717632384101));
#373095=CARTESIAN_POINT('Ctrl Pts',(-1.08603023851022,1.05205660652591,
1.62719452625359));
#373096=CARTESIAN_POINT('Ctrl Pts',(-0.782913804513272,1.29466475481155,
1.6058717147931));
#373097=CARTESIAN_POINT('Ctrl Pts',(-0.605584098510224,1.38650019717125,
1.59478895082509));
#373098=CARTESIAN_POINT('Ctrl Pts',(-0.227706574714818,1.49544911728569,
1.5735819510927));
#373099=CARTESIAN_POINT('Ctrl Pts',(-0.0311225690518228,1.51236222680461,
1.56434078049065));
#373100=CARTESIAN_POINT('Ctrl Pts',(0.354688511733669,1.47013891344908,
1.54460556639624));
#373101=CARTESIAN_POINT('Ctrl Pts',(0.540347704282607,1.41248683200107,
1.53407158762304));
#373102=CARTESIAN_POINT('Ctrl Pts',(0.886385588657729,1.22654525458887,
1.51225778833156));
#373103=CARTESIAN_POINT('Ctrl Pts',(1.04203298693861,1.09739470579444,1.50118168414592));
#373104=CARTESIAN_POINT('Ctrl Pts',(1.28752949502232,0.792903459705068,
1.48091213772451));
#373105=CARTESIAN_POINT('Ctrl Pts',(1.37785847669754,0.622845987199162,
1.47210255484438));
#373106=CARTESIAN_POINT('Ctrl Pts',(1.49111190625469,0.254094740726321,
1.45161637448478));
#373107=CARTESIAN_POINT('Ctrl Pts',(1.51147456813654,0.0584358280814496,
1.44074643489339));
#373108=CARTESIAN_POINT('Ctrl Pts',(1.47588274641145,-0.333593357307579,
1.41896703570512));
#373109=CARTESIAN_POINT('Ctrl Pts',(1.41873210864635,-0.526059065733415,
1.40827449634813));
#373110=CARTESIAN_POINT('Ctrl Pts',(1.23680525040245,-0.869720120377004,
1.38918221553459));
#373111=CARTESIAN_POINT('Ctrl Pts',(1.11679411652883,-1.01926735639925,
1.37958546652839));
#373112=CARTESIAN_POINT('Ctrl Pts',(0.821845392338527,-1.27021444053289,
1.35842398708231));
#373113=CARTESIAN_POINT('Ctrl Pts',(0.647947697679443,-1.36712826231966,
1.34736527974188));
#373114=CARTESIAN_POINT('Ctrl Pts',(0.311311645264392,-1.47566491337257,
1.32815396314479));
#373115=CARTESIAN_POINT('Ctrl Pts',(0.156016598079475,-1.50000000000002,
1.32000635207494));
#373116=CARTESIAN_POINT('Ctrl Pts',(-2.21801743638395E-13,-1.49999999999999,
1.31249999999999));
#373117=CARTESIAN_POINT('Origin',(0.,2.04523456705693E-15,3.99999999999998));
#373118=CARTESIAN_POINT('',(-6.21175810866611E-14,-1.5,0.749999999999995));
#373119=CARTESIAN_POINT('',(-1.77250281061063E-16,-1.5,0.812500000000001));
#373120=CARTESIAN_POINT('',(-1.83697019872103E-16,-1.5,3.99999999999998));
#373121=CARTESIAN_POINT('Ctrl Pts',(-1.26981758441502E-13,-1.5,0.749999999999995));
#373122=CARTESIAN_POINT('Ctrl Pts',(0.173384566787578,-1.50000000000001,
0.758341968859011));
#373123=CARTESIAN_POINT('Ctrl Pts',(0.345657063026003,-1.4699430379504,
0.767465348811296));
#373124=CARTESIAN_POINT('Ctrl Pts',(0.693992244817146,-1.34424321965294,
0.787716294678613));
#373125=CARTESIAN_POINT('Ctrl Pts',(0.863938649032978,-1.24186420207643,
0.798736706463112));
#373126=CARTESIAN_POINT('Ctrl Pts',(1.14981628665739,-0.981834134196356,
0.81971405815737));
#373127=CARTESIAN_POINT('Ctrl Pts',(1.26474494903649,-0.828538224367302,
0.828970098646288));
#373128=CARTESIAN_POINT('Ctrl Pts',(1.43525308335351,-0.479166451138578,
0.84837964160344));
#373129=CARTESIAN_POINT('Ctrl Pts',(1.48605755906629,-0.284890893244485,
0.859172728153113));
#373130=CARTESIAN_POINT('Ctrl Pts',(1.5086978727434,0.107518734382283,0.880973263021266));
#373131=CARTESIAN_POINT('Ctrl Pts',(1.48211426808514,0.301791556356168,
0.891766197575371));
#373132=CARTESIAN_POINT('Ctrl Pts',(1.35715289650818,0.667005850024354,
0.912055880556936));
#373133=CARTESIAN_POINT('Ctrl Pts',(1.26089428601025,0.83480906539487,0.920857669418136));
#373134=CARTESIAN_POINT('Ctrl Pts',(1.00523551024145,1.13107944512606,0.941387790772681));
#373135=CARTESIAN_POINT('Ctrl Pts',(0.84598771678392,1.25464405070159,0.952481953962604));
#373136=CARTESIAN_POINT('Ctrl Pts',(0.495289357898476,1.42882999593108,
0.974193435100107));
#373137=CARTESIAN_POINT('Ctrl Pts',(0.308491280707698,1.48044575440365,
0.984614532847973));
#373138=CARTESIAN_POINT('Ctrl Pts',(-0.0797322763589896,1.51082443319568,
1.00413679963482));
#373139=CARTESIAN_POINT('Ctrl Pts',(-0.27760059194994,1.48724731902885,
1.01371030584558));
#373140=CARTESIAN_POINT('Ctrl Pts',(-0.652645548149537,1.3648820972632,
1.03515369865185));
#373141=CARTESIAN_POINT('Ctrl Pts',(-0.826150819576611,1.2674080418253,
1.04620908756659));
#373142=CARTESIAN_POINT('Ctrl Pts',(-1.12018365389917,1.01553559153652,
1.06735220585628));
#373143=CARTESIAN_POINT('Ctrl Pts',(-1.23967930040037,0.865613174862536,
1.07691037917434));
#373144=CARTESIAN_POINT('Ctrl Pts',(-1.42046156818003,0.521372499608716,
1.09603486113288));
#373145=CARTESIAN_POINT('Ctrl Pts',(-1.47697743270121,0.328715277685212,
1.10673804012863));
#373146=CARTESIAN_POINT('Ctrl Pts',(-1.51126764366641,-0.0633715758174975,
1.128520643101));
#373147=CARTESIAN_POINT('Ctrl Pts',(-1.49027702721395,-0.258900036336387,
1.13938333535205));
#373148=CARTESIAN_POINT('Ctrl Pts',(-1.37584643246876,-0.62730047372594,
1.15985002631814));
#373149=CARTESIAN_POINT('Ctrl Pts',(-1.28492805400909,-0.797130166849572,
1.16865470814546));
#373150=CARTESIAN_POINT('Ctrl Pts',(-1.03841395698962,-1.10080759809765,
1.18895060736956));
#373151=CARTESIAN_POINT('Ctrl Pts',(-0.882399037793513,-1.22940552156971,
1.20002904321007));
#373152=CARTESIAN_POINT('Ctrl Pts',(-0.535879186602947,-1.41418011314842,
1.22183361486762));
#373153=CARTESIAN_POINT('Ctrl Pts',(-0.350097780224434,-1.47123122899152,
1.23235678016741));
#373154=CARTESIAN_POINT('Ctrl Pts',(-0.105814197624947,-1.49720410709341,
1.24483134835127));
#373155=CARTESIAN_POINT('Ctrl Pts',(-0.0528780712322903,-1.49999999999999,
1.24745590261165));
#373156=CARTESIAN_POINT('Ctrl Pts',(-2.17019340709635E-13,-1.5,1.24999999999999));
#373157=CARTESIAN_POINT('Ctrl Pts',(-2.16984549985882E-13,-1.5,1.31249999999999));
#373158=CARTESIAN_POINT('Ctrl Pts',(-0.0405322108119921,-1.49999999999999,
1.31054989309807));
#373159=CARTESIAN_POINT('Ctrl Pts',(-0.0811087443154879,-1.49835720581244,
1.30855202054776));
#373160=CARTESIAN_POINT('Ctrl Pts',(-0.313115738324047,-1.47948217772521,
1.29686527250828));
#373161=CARTESIAN_POINT('Ctrl Pts',(-0.499808848192362,-1.4272632921762,
1.28643247147317));
#373162=CARTESIAN_POINT('Ctrl Pts',(-0.850059522106373,-1.25189938256099,
1.26470980835596));
#373163=CARTESIAN_POINT('Ctrl Pts',(-1.00895664386298,-1.1277731486574,
1.25361691607922));
#373164=CARTESIAN_POINT('Ctrl Pts',(-1.26360571809193,-0.83067644960973,
1.23311242069832));
#373165=CARTESIAN_POINT('Ctrl Pts',(-1.35927065028476,-0.662651140882278,
1.22431395227122));
#373166=CARTESIAN_POINT('Ctrl Pts',(-1.48307334863835,-0.297082086435002,
1.20400456035748));
#373167=CARTESIAN_POINT('Ctrl Pts',(-1.50904390700285,-0.102663343036432,
1.19320351905756));
#373168=CARTESIAN_POINT('Ctrl Pts',(-1.48512163304604,0.289727796531464,
1.17140401130379));
#373169=CARTESIAN_POINT('Ctrl Pts',(-1.43368604030662,0.483833715114844,
1.16062034916027));
#373170=CARTESIAN_POINT('Ctrl Pts',(-1.26204439514748,0.832645785094674,
1.14124190082806));
#373171=CARTESIAN_POINT('Ctrl Pts',(-1.14661700524226,0.985568902270797,
1.13195638910085));
#373172=CARTESIAN_POINT('Ctrl Pts',(-0.859845498615502,1.24471185801849,
1.11096067311784));
#373173=CARTESIAN_POINT('Ctrl Pts',(-0.6895034643601,1.34656063150023,1.09993595557682));
#373174=CARTESIAN_POINT('Ctrl Pts',(-0.316872979842725,1.47960511561658,
1.07831208291712));
#373175=CARTESIAN_POINT('Ctrl Pts',(-0.117955001656985,1.50854144107688,
1.06841237491536));
#373176=CARTESIAN_POINT('Ctrl Pts',(0.272102436470558,1.48750490166672,
1.04906137935655));
#373177=CARTESIAN_POINT('Ctrl Pts',(0.459657314220201,1.44062637172882,
1.03873545970634));
#373178=CARTESIAN_POINT('Ctrl Pts',(0.81373421671715,1.27571866671084,1.0171191572083));
#373179=CARTESIAN_POINT('Ctrl Pts',(0.975666881366397,1.15659220468503,
1.00601909985821));
#373180=CARTESIAN_POINT('Ctrl Pts',(1.23921847007258,0.866851603428119,
0.985290618099559));
#373181=CARTESIAN_POINT('Ctrl Pts',(1.34014951631224,0.700779301288413,
0.976432183404897));
#373182=CARTESIAN_POINT('Ctrl Pts',(1.47413432584509,0.338358760845283,
0.956297708935835));
#373183=CARTESIAN_POINT('Ctrl Pts',(1.50546906377203,0.145287134359055,
0.945571507464378));
#373184=CARTESIAN_POINT('Ctrl Pts',(1.49280633965443,-0.247122392043873,
0.923770978219772));
#373185=CARTESIAN_POINT('Ctrl Pts',(1.446936108067,-0.442646750903302,0.912908513838693));
#373186=CARTESIAN_POINT('Ctrl Pts',(1.28528021777334,-0.796334054501323,
0.89325921919436));
#373187=CARTESIAN_POINT('Ctrl Pts',(1.17420552689302,-0.952547821731117,
0.884200994704871));
#373188=CARTESIAN_POINT('Ctrl Pts',(0.895258274487633,-1.2193995977598,
0.863367589431912));
#373189=CARTESIAN_POINT('Ctrl Pts',(0.728423672339838,-1.32582725035303,
0.85238443221042));
#373190=CARTESIAN_POINT('Ctrl Pts',(0.371751064568077,-1.46517581908719,
0.831353219792006));
#373191=CARTESIAN_POINT('Ctrl Pts',(0.186619235362833,-1.5,0.821478722147725));
#373192=CARTESIAN_POINT('Ctrl Pts',(-1.04083408558608E-16,-1.5,0.812500000000001));
#373193=CARTESIAN_POINT('Origin',(0.,2.04523456705693E-15,3.99999999999998));
#373194=CARTESIAN_POINT('',(-4.50788613606587E-8,-1.49999999999999,0.249999995662285));
#373195=CARTESIAN_POINT('',(1.52431070176988E-14,-1.5,0.312500000000002));
#373196=CARTESIAN_POINT('',(-1.83697019872103E-16,-1.5,3.99999999999998));
#373197=CARTESIAN_POINT('Ctrl Pts',(-4.51837430147789E-8,-1.49999999999999,
0.249999997826096));
#373198=CARTESIAN_POINT('Ctrl Pts',(0.00348282355345849,-1.50000000010491,
0.250167567429258));
#373199=CARTESIAN_POINT('Ctrl Pts',(0.00696619430317118,-1.49998786983704,
0.250335498128669));
#373200=CARTESIAN_POINT('Ctrl Pts',(0.209254267662016,-1.49857856147727,
0.260107235050405));
#373201=CARTESIAN_POINT('Ctrl Pts',(0.405777232132074,-1.45768418329109,
0.270698405536583));
#373202=CARTESIAN_POINT('Ctrl Pts',(0.768330064713747,-1.30301918211526,
0.292437986859785));
#373203=CARTESIAN_POINT('Ctrl Pts',(0.931381977277525,-1.19194128837559,
0.303368322708991));
#373204=CARTESIAN_POINT('Ctrl Pts',(1.20212022338398,-0.917133022467638,
0.324027785590003));
#373205=CARTESIAN_POINT('Ctrl Pts',(1.30865255207445,-0.757395376448475,
0.332922479086215));
#373206=CARTESIAN_POINT('Ctrl Pts',(1.46043143136339,-0.396851323959125,
0.352952704224513));
#373207=CARTESIAN_POINT('Ctrl Pts',(1.50038276079889,-0.197951118063682,
0.364002715663149));
#373208=CARTESIAN_POINT('Ctrl Pts',(1.49962649441611,0.196009289988444,
0.385889404999379));
#373209=CARTESIAN_POINT('Ctrl Pts',(1.46195998285909,0.387282791440873,
0.396515710635625));
#373210=CARTESIAN_POINT('Ctrl Pts',(1.31581458969238,0.745840837156813,
0.416435602064289));
#373211=CARTESIAN_POINT('Ctrl Pts',(1.20843055145291,0.909586471241854,
0.425458982186326));
#373212=CARTESIAN_POINT('Ctrl Pts',(0.934170098346782,1.19024237788855,
0.446450341795587));
#373213=CARTESIAN_POINT('Ctrl Pts',(0.768757015230046,1.3032101208217,0.457546775326919));
#373214=CARTESIAN_POINT('Ctrl Pts',(0.410444839870971,1.45532904822187,
0.479011603662826));
#373215=CARTESIAN_POINT('Ctrl Pts',(0.222046611647017,1.49571599277423,
0.489197777215388));
#373216=CARTESIAN_POINT('Ctrl Pts',(-0.167599313780493,1.50379997668454,
0.508169180651858));
#373217=CARTESIAN_POINT('Ctrl Pts',(-0.365223633275425,1.46838801912668,
0.518449940828671));
#373218=CARTESIAN_POINT('Ctrl Pts',(-0.732524358587354,1.32355716682777,
0.540144784445228));
#373219=CARTESIAN_POINT('Ctrl Pts',(-0.89897911089993,1.21664955586623,
0.551122998309901));
#373220=CARTESIAN_POINT('Ctrl Pts',(-1.1770918951988,0.948982970424738,
0.571938888812166));
#373221=CARTESIAN_POINT('Ctrl Pts',(-1.28770388209791,0.792414448668057,
0.580976975074022));
#373222=CARTESIAN_POINT('Ctrl Pts',(-1.44828613126506,0.438210499638932,
0.600654972242306));
#373223=CARTESIAN_POINT('Ctrl Pts',(-1.49355746160076,0.242543837284878,
0.611525342373087));
#373224=CARTESIAN_POINT('Ctrl Pts',(-1.50501452892094,-0.149848383426528,
0.633324910190388));
#373225=CARTESIAN_POINT('Ctrl Pts',(-1.47310810476986,-0.34276700151942,
0.644042611195548));
#373226=CARTESIAN_POINT('Ctrl Pts',(-1.33803206466294,-0.704845530579388,
0.664158085032213));
#373227=CARTESIAN_POINT('Ctrl Pts',(-1.23652944619448,-0.870708896224865,
0.673027140843388));
#373228=CARTESIAN_POINT('Ctrl Pts',(-0.972020111275437,-1.15964785062779,
0.693779434220025));
#373229=CARTESIAN_POINT('Ctrl Pts',(-0.809768461712522,-1.27822989206776,
0.704879715944881));
#373230=CARTESIAN_POINT('Ctrl Pts',(-0.455296254992094,-1.44200309956987,
0.726483523706352));
#373231=CARTESIAN_POINT('Ctrl Pts',(-0.267657278756777,-1.48830399007212,
0.736797444006965));
#373232=CARTESIAN_POINT('Ctrl Pts',(-0.0509015997152728,-1.4993528318024,
0.747533018747499));
#373233=CARTESIAN_POINT('Ctrl Pts',(-0.0254396825847984,-1.49999999999999,
0.748776032700964));
#373234=CARTESIAN_POINT('Ctrl Pts',(-1.2405146515345E-13,-1.5,0.749999999999995));
#373235=CARTESIAN_POINT('Ctrl Pts',(-1.70803542250024E-16,-1.5,0.812500000000001));
#373236=CARTESIAN_POINT('Ctrl Pts',(-0.0119425753744356,-1.5,0.811925412574397));
#373237=CARTESIAN_POINT('Ctrl Pts',(-0.0238908671823992,-1.49985737526137,
0.81134658831845));
#373238=CARTESIAN_POINT('Ctrl Pts',(-0.226821223276692,-1.49500698913326,
0.801448364060632));
#373239=CARTESIAN_POINT('Ctrl Pts',(-0.415148767636273,-1.45400207372324,
0.791248425429924));
#373240=CARTESIAN_POINT('Ctrl Pts',(-0.773077310249116,-1.30066201483827,
0.769768134314104));
#373241=CARTESIAN_POINT('Ctrl Pts',(-0.938168916315346,-1.187104171216,
0.758670776168768));
#373242=CARTESIAN_POINT('Ctrl Pts',(-1.21141488703134,-0.905575960850558,
0.737703995207406));
#373243=CARTESIAN_POINT('Ctrl Pts',(-1.31818157918045,-0.741610570018196,
0.728700587223223));
#373244=CARTESIAN_POINT('Ctrl Pts',(-1.46317859948516,-0.382682975762146,
0.70876016532011));
#373245=CARTESIAN_POINT('Ctrl Pts',(-1.50025101871615,-0.191231002705516,
0.698123944594742));
#373246=CARTESIAN_POINT('Ctrl Pts',(-1.49973635554699,0.202857738527839,
0.676230125637334));
#373247=CARTESIAN_POINT('Ctrl Pts',(-1.45911625076073,0.401694321978298,
0.665183648778974));
#373248=CARTESIAN_POINT('Ctrl Pts',(-1.30611837209093,0.761745197464029,
0.6451808223631));
#373249=CARTESIAN_POINT('Ctrl Pts',(-1.19908428845553,0.921089090541452,
0.636271828322799));
#373250=CARTESIAN_POINT('Ctrl Pts',(-0.92743766004034,1.19502329549003,
0.615592940348674));
#373251=CARTESIAN_POINT('Ctrl Pts',(-0.763962245148437,1.30559446577423,
0.604656304385748));
#373252=CARTESIAN_POINT('Ctrl Pts',(-0.400831821334879,1.45905114337201,
0.582922498235279));
#373253=CARTESIAN_POINT('Ctrl Pts',(-0.204176053948586,1.4992783205916,
0.572343471625999));
#373254=CARTESIAN_POINT('Ctrl Pts',(0.18503638089729,1.50067236949698,0.553578756042776));
#373255=CARTESIAN_POINT('Ctrl Pts',(0.373923463154697,1.46509146512387,
0.543539917466597));
#373256=CARTESIAN_POINT('Ctrl Pts',(0.735156364550241,1.32237962218791,
0.522195873535526));
#373257=CARTESIAN_POINT('Ctrl Pts',(0.902980093128755,1.21399098351906,
0.511110655111013));
#373258=CARTESIAN_POINT('Ctrl Pts',(1.18503413357111,0.940122108026969,
0.489932854999392));
#373259=CARTESIAN_POINT('Ctrl Pts',(1.29720572931344,0.778063845741863,
0.480725769207872));
#373260=CARTESIAN_POINT('Ctrl Pts',(1.45215110685594,0.42237084518817,0.460965046954891));
#373261=CARTESIAN_POINT('Ctrl Pts',(1.49434106495004,0.232523854121758,
0.450417991895646));
#373262=CARTESIAN_POINT('Ctrl Pts',(1.50479969486777,-0.16032215158135,
0.42859321380103));
#373263=CARTESIAN_POINT('Ctrl Pts',(1.46996649084184,-0.3596378809732,0.417520117723705));
#373264=CARTESIAN_POINT('Ctrl Pts',(1.3275358794875,-0.723908254097641,
0.397282874772348));
#373265=CARTESIAN_POINT('Ctrl Pts',(1.22482468313652,-0.886680660751951,
0.388466053355688));
#373266=CARTESIAN_POINT('Ctrl Pts',(0.96101225989259,-1.16810260828488,
0.367956095904041));
#373267=CARTESIAN_POINT('Ctrl Pts',(0.801227349234453,-1.28297879352365,
0.35707743566011));
#373268=CARTESIAN_POINT('Ctrl Pts',(0.443193904486032,-1.44675205425625,
0.335302286275506));
#373269=CARTESIAN_POINT('Ctrl Pts',(0.247755919662054,-1.49270029722171,
0.324622931764132));
#373270=CARTESIAN_POINT('Ctrl Pts',(0.0326763919887163,-1.49973322184082,
0.314079554146987));
#373271=CARTESIAN_POINT('Ctrl Pts',(0.0163333853167089,-1.5,0.313285840367448));
#373272=CARTESIAN_POINT('Ctrl Pts',(3.06699110552697E-14,-1.5,0.312500000000002));
#373273=CARTESIAN_POINT('Origin',(0.,2.04523456705693E-15,3.99999999999998));
#373274=CARTESIAN_POINT('',(7.73382353572088E-14,-1.5,-0.249999999999993));
#373275=CARTESIAN_POINT('',(1.08229622940747E-13,-1.5,-0.18749999999999));
#373276=CARTESIAN_POINT('',(-1.83697019872103E-16,-1.5,3.99999999999998));
#373277=CARTESIAN_POINT('Ctrl Pts',(1.5486016773429E-13,-1.5,-0.249999999999993));
#373278=CARTESIAN_POINT('Ctrl Pts',(0.032860455885365,-1.5,-0.248419000579072));
#373279=CARTESIAN_POINT('Ctrl Pts',(0.0657519915310822,-1.49892021763245,
-0.246806511877816));
#373280=CARTESIAN_POINT('Ctrl Pts',(0.297065083808075,-1.48367883097131,
-0.235254083685017));
#373281=CARTESIAN_POINT('Ctrl Pts',(0.490910090902343,-1.43127059459545,
-0.224471927088997));
#373282=CARTESIAN_POINT('Ctrl Pts',(0.842790719159963,-1.25597008082433,
-0.202672603752536));
#373283=CARTESIAN_POINT('Ctrl Pts',(0.998245550468655,-1.13634232069776,
-0.191870286357112));
#373284=CARTESIAN_POINT('Ctrl Pts',(1.25307683006948,-0.846472584804176,
-0.171557773592667));
#373285=CARTESIAN_POINT('Ctrl Pts',(1.35083608504267,-0.679675474119084,
-0.162759748562156));
#373286=CARTESIAN_POINT('Ctrl Pts',(1.48099815554993,-0.310667784306506,
-0.142259321350346));
#373287=CARTESIAN_POINT('Ctrl Pts',(1.50915093165956,-0.110999542458538,
-0.131166641247681));
#373288=CARTESIAN_POINT('Ctrl Pts',(1.48609240045633,0.280039930965759,
-0.109442226057442));
#373289=CARTESIAN_POINT('Ctrl Pts',(1.43805988182893,0.467863568677401,
-0.0990075795179057));
#373290=CARTESIAN_POINT('Ctrl Pts',(1.2715841280139,0.819713330899575,-0.0794603705055627));
#373291=CARTESIAN_POINT('Ctrl Pts',(1.15298332135301,0.979542414678213,
-0.069930091060669));
#373292=CARTESIAN_POINT('Ctrl Pts',(0.860672783550812,1.24423569732698,
-0.0485137025687251));
#373293=CARTESIAN_POINT('Ctrl Pts',(0.689840047383048,1.34647667691424,
-0.0374544815068962));
#373294=CARTESIAN_POINT('Ctrl Pts',(0.325093633437915,1.47663503667349,
-0.0162901014904864));
#373295=CARTESIAN_POINT('Ctrl Pts',(0.135586908706809,1.50589444815122,
-0.00668716285755389));
#373296=CARTESIAN_POINT('Ctrl Pts',(-0.253006716819572,1.49181979884168,
0.0124000191485191));
#373297=CARTESIAN_POINT('Ctrl Pts',(-0.44828599000737,1.44518296954627,
0.0230908650407911));
#373298=CARTESIAN_POINT('Ctrl Pts',(-0.805683809008424,1.28017481456344,
0.0448697354854288));
#373299=CARTESIAN_POINT('Ctrl Pts',(-0.965015455486543,1.1647865999199,
0.0557408110853518));
#373300=CARTESIAN_POINT('Ctrl Pts',(-1.22787773770585,0.88246416929183,
0.076230068274947));
#373301=CARTESIAN_POINT('Ctrl Pts',(-1.33006509885902,0.71927082538992,
0.0850405097005798));
#373302=CARTESIAN_POINT('Ctrl Pts',(-1.47120566569572,0.354494062141217,
0.105305885436618));
#373303=CARTESIAN_POINT('Ctrl Pts',(-1.50533426870155,0.155131010997178,
0.116381610500176));
#373304=CARTESIAN_POINT('Ctrl Pts',(-1.49354326838503,-0.23754326002992,
0.138196847779459));
#373305=CARTESIAN_POINT('Ctrl Pts',(-1.45073378385078,-0.427185465663105,
0.148732525870191));
#373306=CARTESIAN_POINT('Ctrl Pts',(-1.29457497008243,-0.782478789741982,
0.168471043874573));
#373307=CARTESIAN_POINT('Ctrl Pts',(-1.18173521246989,-0.944303668118952,
0.177707728861905));
#373308=CARTESIAN_POINT('Ctrl Pts',(-0.898603989372673,-1.21722222304294,
0.198910957154612));
#373309=CARTESIAN_POINT('Ctrl Pts',(-0.730455409049272,-1.32497165006399,
0.209994049136883));
#373310=CARTESIAN_POINT('Ctrl Pts',(-0.37209496343298,-1.46509978331248,
0.231128122261297));
#373311=CARTESIAN_POINT('Ctrl Pts',(-0.186815895788635,-1.49999999437264,
0.241011815866812));
#373312=CARTESIAN_POINT('Ctrl Pts',(-4.5183745252253E-8,-1.49999999999999,
0.249999997826096));
#373313=CARTESIAN_POINT('Ctrl Pts',(3.2682190287403E-14,-1.5,0.312500000000002));
#373314=CARTESIAN_POINT('Ctrl Pts',(-0.173451403441322,-1.5,0.304154815460988));
#373315=CARTESIAN_POINT('Ctrl Pts',(-0.345738678826419,-1.46991848495802,
0.295030042419132));
#373316=CARTESIAN_POINT('Ctrl Pts',(-0.694724820475537,-1.34397330137361,
0.274740961528629));
#373317=CARTESIAN_POINT('Ctrl Pts',(-0.865246151889541,-1.24107115352004,
0.263678357149826));
#373318=CARTESIAN_POINT('Ctrl Pts',(-1.15646444213004,-0.975386913975008,
0.242286992862745));
#373319=CARTESIAN_POINT('Ctrl Pts',(-1.27437325899852,-0.815319430751239,
0.23279552393062));
#373320=CARTESIAN_POINT('Ctrl Pts',(-1.43962337775053,-0.463056308150473,
0.2132253504528));
#373321=CARTESIAN_POINT('Ctrl Pts',(-1.48703970257091,-0.275009459948132,
0.202778303330447));
#373322=CARTESIAN_POINT('Ctrl Pts',(-1.50876566366178,0.116240468830023,
0.181042196176105));
#373323=CARTESIAN_POINT('Ctrl Pts',(-1.47990453460223,0.315881524199714,
0.169951026433344));
#373324=CARTESIAN_POINT('Ctrl Pts',(-1.34843726471597,0.684393653585345,
0.149478130356364));
#373325=CARTESIAN_POINT('Ctrl Pts',(-1.2501541581696,0.850760295813159,
0.140682506206385));
#373326=CARTESIAN_POINT('Ctrl Pts',(-0.994373222012351,1.13974345531941,
0.120348930191437));
#373327=CARTESIAN_POINT('Ctrl Pts',(-0.838455863131078,1.25887818084316,
0.109538054833435));
#373328=CARTESIAN_POINT('Ctrl Pts',(-0.485909638788608,1.43297539889288,
0.0877401328715617));
#373329=CARTESIAN_POINT('Ctrl Pts',(-0.291886496354003,1.48470586992773,
0.0769682325500131));
#373330=CARTESIAN_POINT('Ctrl Pts',(0.0961134619130744,1.50891295317755,
0.0576281568749298));
#373331=CARTESIAN_POINT('Ctrl Pts',(0.286173113423018,1.48464949424262,
0.0483050867231545));
#373332=CARTESIAN_POINT('Ctrl Pts',(0.653585225433785,1.3643677539121,0.0272868037884504));
#373333=CARTESIAN_POINT('Ctrl Pts',(0.826634636240301,1.2670229746827,0.0162569384838358));
#373334=CARTESIAN_POINT('Ctrl Pts',(1.12695650359022,1.0097041504712,-0.00534004921298362));
#373335=CARTESIAN_POINT('Ctrl Pts',(1.25068904169858,0.851635471447732,
-0.0151869182529077));
#373336=CARTESIAN_POINT('Ctrl Pts',(1.4261416971664,0.502848746380216,-0.034563958534436));
#373337=CARTESIAN_POINT('Ctrl Pts',(1.4786500184448,0.316717507606887,-0.0449045829107318));
#373338=CARTESIAN_POINT('Ctrl Pts',(1.51141470029083,-0.0726489674713217,
-0.0665360537484097));
#373339=CARTESIAN_POINT('Ctrl Pts',(1.48843464297174,-0.27244234664173,
-0.0776356859245436));
#373340=CARTESIAN_POINT('Ctrl Pts',(1.3678393689196,-0.645023521480528,
-0.0983346400822544));
#373341=CARTESIAN_POINT('Ctrl Pts',(1.27390529358518,-0.814986953888903,
-0.107181062815792));
#373342=CARTESIAN_POINT('Ctrl Pts',(1.02599149417605,-1.11127283481478,
-0.127338984410234));
#373343=CARTESIAN_POINT('Ctrl Pts',(0.873937684757876,-1.2344253143386,
-0.138075578935803));
#373344=CARTESIAN_POINT('Ctrl Pts',(0.52700932844199,-1.41837933893976,
-0.159877011278209));
#373345=CARTESIAN_POINT('Ctrl Pts',(0.334529625819275,-1.47568594816069,
-0.170729545544577));
#373346=CARTESIAN_POINT('Ctrl Pts',(0.0910182157037006,-1.49793118858919,
-0.183063417071561));
#373347=CARTESIAN_POINT('Ctrl Pts',(0.0454853740099916,-1.5,-0.185311583922599));
#373348=CARTESIAN_POINT('Ctrl Pts',(2.16642942901365E-13,-1.5,-0.18749999999999));
#373349=CARTESIAN_POINT('Origin',(0.,2.04523456705693E-15,3.99999999999998));
#373350=CARTESIAN_POINT('',(7.73382353572088E-14,-1.5,-0.749999999999992));
#373351=CARTESIAN_POINT('',(3.08182550266226E-14,-1.5,-0.687499999999998));
#373352=CARTESIAN_POINT('',(-1.83697019872103E-16,-1.5,3.99999999999998));
#373353=CARTESIAN_POINT('Ctrl Pts',(1.5486016773429E-13,-1.5,-0.749999999999992));
#373354=CARTESIAN_POINT('Ctrl Pts',(0.0605270531518406,-1.5,-0.747087890797456));
#373355=CARTESIAN_POINT('Ctrl Pts',(0.121111815912754,-1.49633682152687,
-0.744071250082467));
#373356=CARTESIAN_POINT('Ctrl Pts',(0.380907005258931,-1.46468181567999,
-0.730692542489233));
#373357=CARTESIAN_POINT('Ctrl Pts',(0.573458929788626,-1.40053904367085,
-0.719646640033961));
#373358=CARTESIAN_POINT('Ctrl Pts',(0.915125828010041,-1.20410581994117,
-0.697751705291916));
#373359=CARTESIAN_POINT('Ctrl Pts',(1.06246375204514,-1.07634209434518,
-0.687113913738957));
#373360=CARTESIAN_POINT('Ctrl Pts',(1.30094807582981,-0.771436277330007,
-0.667170225332875));
#373361=CARTESIAN_POINT('Ctrl Pts',(1.38964235735141,-0.59705846915719,
-0.658169914953168));
#373362=CARTESIAN_POINT('Ctrl Pts',(1.49703089523062,-0.219727003413118,
-0.637207055745163));
#373363=CARTESIAN_POINT('Ctrl Pts',(1.51293605277923,-0.0199721092192588,
-0.626109561623282));
#373364=CARTESIAN_POINT('Ctrl Pts',(1.46696719957355,0.366717079076811,
-0.604626828940168));
#373365=CARTESIAN_POINT('Ctrl Pts',(1.40840564943819,0.550355260220075,
-0.594424707765542));
#373366=CARTESIAN_POINT('Ctrl Pts',(1.22179400429212,0.89259639043274,-0.575411311642616));
#373367=CARTESIAN_POINT('Ctrl Pts',(1.09286815607941,1.0465149197047,-0.565177451461071));
#373368=CARTESIAN_POINT('Ctrl Pts',(0.784626975107821,1.29336119748035,
-0.543490349677642));
#373369=CARTESIAN_POINT('Ctrl Pts',(0.609076727214449,1.38472090647381,
-0.532506414743584));
#373370=CARTESIAN_POINT('Ctrl Pts',(0.238548693852844,1.4930503343714,-0.511670225651682));
#373371=CARTESIAN_POINT('Ctrl Pts',(0.0477382601695704,1.51122894014668,
-0.502608723117359));
#373372=CARTESIAN_POINT('Ctrl Pts',(-0.339405970527289,1.47457237426477,
-0.482963999692192));
#373373=CARTESIAN_POINT('Ctrl Pts',(-0.531698004873539,1.41662884683185,
-0.472102802447431));
#373374=CARTESIAN_POINT('Ctrl Pts',(-0.877963968207817,1.23155521756417,
-0.450302139372585));
#373375=CARTESIAN_POINT('Ctrl Pts',(-1.02956797170921,1.10794943345765,
-0.439574594350313));
#373376=CARTESIAN_POINT('Ctrl Pts',(-1.27657478448722,0.810828070813583,
-0.419437102345001));
#373377=CARTESIAN_POINT('Ctrl Pts',(-1.37000627001517,0.640445066970175,
-0.410580281498331));
#373378=CARTESIAN_POINT('Ctrl Pts',(-1.48933954887378,0.267400636282404,
-0.389855590904567));
#373379=CARTESIAN_POINT('Ctrl Pts',(-1.51164004661096,0.0676004233373413,
-0.378755579074287));
#373380=CARTESIAN_POINT('Ctrl Pts',(-1.4776034925801,-0.321528438969358,
-0.357137308946137));
#373381=CARTESIAN_POINT('Ctrl Pts',(-1.42451030310986,-0.507429171138638,
-0.346809490492288));
#373382=CARTESIAN_POINT('Ctrl Pts',(-1.24787445641846,-0.855807485190914,
-0.327455139711605));
#373383=CARTESIAN_POINT('Ctrl Pts',(-1.12345714577022,-1.01364197081179,
-0.317562302383004));
#373384=CARTESIAN_POINT('Ctrl Pts',(-0.822078108419088,-1.2699733049106,
-0.295941881851693));
#373385=CARTESIAN_POINT('Ctrl Pts',(-0.648745156586937,-1.36666587614998,
-0.284916491561733));
#373386=CARTESIAN_POINT('Ctrl Pts',(-0.312337813768908,-1.4754965967708,
-0.265708010161154));
#373387=CARTESIAN_POINT('Ctrl Pts',(-0.156554135230396,-1.5,-0.257532214343177));
#373388=CARTESIAN_POINT('Ctrl Pts',(1.55014889813287E-13,-1.5,-0.249999999999993));
#373389=CARTESIAN_POINT('Ctrl Pts',(2.14377127161214E-13,-1.5,-0.18749999999999));
#373390=CARTESIAN_POINT('Ctrl Pts',(-0.143866319824192,-1.5,-0.194421771539806));
#373391=CARTESIAN_POINT('Ctrl Pts',(-0.287202401435548,-1.47930819185578,
-0.201892804430179));
#373392=CARTESIAN_POINT('Ctrl Pts',(-0.613653851873503,-1.38270765947202,
-0.220282555284259));
#373393=CARTESIAN_POINT('Ctrl Pts',(-0.788957812087736,-1.29073374629065,
-0.231271701924271));
#373394=CARTESIAN_POINT('Ctrl Pts',(-1.09791823757522,-1.04158724780001,
-0.253057303395467));
#373395=CARTESIAN_POINT('Ctrl Pts',(-1.22730056572081,-0.885449105131343,
-0.26330838304826));
#373396=CARTESIAN_POINT('Ctrl Pts',(-1.41241538793125,-0.540029980306386,
-0.282498334427425));
#373397=CARTESIAN_POINT('Ctrl Pts',(-1.4696637265307,-0.355830537243378,
-0.292731636819814));
#373398=CARTESIAN_POINT('Ctrl Pts',(-1.51276028827358,0.0314809184981216,
-0.314248939916565));
#373399=CARTESIAN_POINT('Ctrl Pts',(-1.49531235561511,0.231264916379955,
-0.32534805091));
#373400=CARTESIAN_POINT('Ctrl Pts',(-1.38503041627651,0.607574273005967,
-0.346254126278111));
#373401=CARTESIAN_POINT('Ctrl Pts',(-1.29519151853042,0.780980599048122,
-0.355212307872812));
#373402=CARTESIAN_POINT('Ctrl Pts',(-1.05465300357619,1.08402094088197,
-0.375203009842583));
#373403=CARTESIAN_POINT('Ctrl Pts',(-0.906280583038949,1.21079931160738,
-0.38586320266308));
#373404=CARTESIAN_POINT('Ctrl Pts',(-0.56482212083892,1.40375369382997,
-0.407651474536063));
#373405=CARTESIAN_POINT('Ctrl Pts',(-0.373924919213404,1.46620146978531,
-0.41857068087477));
#373406=CARTESIAN_POINT('Ctrl Pts',(0.0125016797145877,1.51196053764197,
-0.438433724502437));
#373407=CARTESIAN_POINT('Ctrl Pts',(0.203910620206974,1.49820204996122,
-0.447360597345563));
#373408=CARTESIAN_POINT('Ctrl Pts',(0.576612990887898,1.39848768859079,
-0.468062091886984));
#373409=CARTESIAN_POINT('Ctrl Pts',(0.753840313387179,1.31147603597659,
-0.479005935766771));
#373410=CARTESIAN_POINT('Ctrl Pts',(1.06750320474121,1.07236929448121,-0.500738902593701));
#373411=CARTESIAN_POINT('Ctrl Pts',(1.20003911969275,0.921619379896505,
-0.511298923339085));
#373412=CARTESIAN_POINT('Ctrl Pts',(1.39455116730487,0.584424044107407,
-0.530031997549591));
#373413=CARTESIAN_POINT('Ctrl Pts',(1.4574360415234,0.402715778033152,-0.540126901220382));
#373414=CARTESIAN_POINT('Ctrl Pts',(1.51289210709091,0.0182420408411633,
-0.561486553286604));
#373415=CARTESIAN_POINT('Ctrl Pts',(1.50209794537431,-0.181333525994842,
-0.572574084777493));
#373416=CARTESIAN_POINT('Ctrl Pts',(1.4043552255257,-0.561995603514428,
-0.593721977973025));
#373417=CARTESIAN_POINT('Ctrl Pts',(1.31946718554587,-0.739628522719427,
-0.602895675512057));
#373418=CARTESIAN_POINT('Ctrl Pts',(1.08778462340069,-1.05066302556747,
-0.622682355281814));
#373419=CARTESIAN_POINT('Ctrl Pts',(0.943897572384442,-1.18161263521891,
-0.63324261340856));
#373420=CARTESIAN_POINT('Ctrl Pts',(0.607960621860351,-1.3858364241278,
-0.655078270501792));
#373421=CARTESIAN_POINT('Ctrl Pts',(0.417568947214438,-1.45458270049018,
-0.666148113006993));
#373422=CARTESIAN_POINT('Ctrl Pts',(0.146526068430488,-1.49463699899561,
-0.680301288995575));
#373423=CARTESIAN_POINT('Ctrl Pts',(0.0732374219065056,-1.5,-0.683976362895629));
#373424=CARTESIAN_POINT('Ctrl Pts',(6.18202070731173E-14,-1.5,-0.687499999999998));
#373425=CARTESIAN_POINT('Origin',(0.,2.04523456705693E-15,3.99999999999998));
#373426=CARTESIAN_POINT('',(-2.29292018146854E-16,-1.5,-1.25));
#373427=CARTESIAN_POINT('',(-1.77250281061063E-16,-1.5,-1.1875));
#373428=CARTESIAN_POINT('',(-1.83697019872103E-16,-1.5,3.99999999999998));
#373429=CARTESIAN_POINT('Ctrl Pts',(-2.74887016421606E-16,-1.5,-1.25));
#373430=CARTESIAN_POINT('Ctrl Pts',(0.0900358162878159,-1.5,-1.24566814976913));
#373431=CARTESIAN_POINT('Ctrl Pts',(0.180082196644308,-1.49189502111387,
-1.24111065297187));
#373432=CARTESIAN_POINT('Ctrl Pts',(0.465578429116048,-1.43984022717801,
-1.22592874258447));
#373433=CARTESIAN_POINT('Ctrl Pts',(0.652956059384571,-1.36511486420352,
-1.21483782761776));
#373434=CARTESIAN_POINT('Ctrl Pts',(0.981061243802619,-1.15084317520299,
-1.19309986821111));
#373435=CARTESIAN_POINT('Ctrl Pts',(1.12028672749574,-1.01582386492302,
-1.18265084260709));
#373436=CARTESIAN_POINT('Ctrl Pts',(1.342886050056,-0.696718611169778,-1.16307699288048));
#373437=CARTESIAN_POINT('Ctrl Pts',(1.42264260296975,-0.514649669801069,
-1.15359164832228));
#373438=CARTESIAN_POINT('Ctrl Pts',(1.5073476097853,-0.129677478171334,
-1.13220430434285));
#373439=CARTESIAN_POINT('Ctrl Pts',(1.5113195465766,0.0694589165068009,
-1.12114117130517));
#373440=CARTESIAN_POINT('Ctrl Pts',(1.44322862617289,0.450825439691474,
-1.09995414223936));
#373441=CARTESIAN_POINT('Ctrl Pts',(1.37453556995427,0.629894589817241,
-1.09030196817094));
#373442=CARTESIAN_POINT('Ctrl Pts',(1.1693792801673,0.960254665911306,-1.07125471279601));
#373443=CARTESIAN_POINT('Ctrl Pts',(1.03195084041089,1.1066117276265,-1.06057720996884));
#373444=CARTESIAN_POINT('Ctrl Pts',(0.711223003369554,1.33497784091084,
-1.03880268156769));
#373445=CARTESIAN_POINT('Ctrl Pts',(0.531879763453132,1.41602128727827,
-1.02792281907056));
#373446=CARTESIAN_POINT('Ctrl Pts',(0.156303877194832,1.50398228927571,
-1.00740955465126));
#373447=CARTESIAN_POINT('Ctrl Pts',(-0.0360004374524879,1.51165277426085,
-0.998591616319393));
#373448=CARTESIAN_POINT('Ctrl Pts',(-0.422715986129613,1.45308522923991,
-0.978358879558099));
#373449=CARTESIAN_POINT('Ctrl Pts',(-0.612794656082124,1.38369525968752,
-0.967286216131843));
#373450=CARTESIAN_POINT('Ctrl Pts',(-0.947909934791437,1.17838584415295,
-0.945459935447073));
#373451=CARTESIAN_POINT('Ctrl Pts',(-1.09130502719597,1.0469943407134,-0.934911071862623));
#373452=CARTESIAN_POINT('Ctrl Pts',(-1.32202372870725,0.735097289813444,
-0.915146806191128));
#373453=CARTESIAN_POINT('Ctrl Pts',(-1.40637010167788,0.556998399808634,
-0.905944355544917));
#373454=CARTESIAN_POINT('Ctrl Pts',(-1.50273781462483,0.175871277265909,
-0.884770626514766));
#373455=CARTESIAN_POINT('Ctrl Pts',(-1.51280764934617,-0.0236685359105637,
-0.873685081338296));
#373456=CARTESIAN_POINT('Ctrl Pts',(-1.45599503486762,-0.407914323054937,
-0.852338093163609));
#373457=CARTESIAN_POINT('Ctrl Pts',(-1.39246163036462,-0.589330217116489,
-0.842291224285139));
#373458=CARTESIAN_POINT('Ctrl Pts',(-1.19682557106127,-0.925814031427701,
-0.823531907373551));
#373459=CARTESIAN_POINT('Ctrl Pts',(-1.06374166172616,-1.07608073639503,
-0.812954829662284));
#373460=CARTESIAN_POINT('Ctrl Pts',(-0.749400300188114,-1.31400853300462,
-0.791221968392454));
#373461=CARTESIAN_POINT('Ctrl Pts',(-0.571941574505609,-1.40039569225495,
-0.780284338159708));
#373462=CARTESIAN_POINT('Ctrl Pts',(-0.257687088986563,-1.48336447077953,
-0.762860073883319));
#373463=CARTESIAN_POINT('Ctrl Pts',(-0.128997012608126,-1.5,-0.756206371662836));
#373464=CARTESIAN_POINT('Ctrl Pts',(1.55639390264639E-13,-1.5,-0.749999999999992));
#373465=CARTESIAN_POINT('Ctrl Pts',(6.50521303491303E-14,-1.5,-0.687499999999997));
#373466=CARTESIAN_POINT('Ctrl Pts',(-0.116639952633668,-1.5,-0.693111842337607));
#373467=CARTESIAN_POINT('Ctrl Pts',(-0.23311324418047,-1.48639868526909,
-0.69909348048802));
#373468=CARTESIAN_POINT('Ctrl Pts',(-0.536820232812539,-1.41416492733363,
-0.715712083067463));
#373469=CARTESIAN_POINT('Ctrl Pts',(-0.715940634650769,-1.332463629502,
-0.72659949791434));
#373470=CARTESIAN_POINT('Ctrl Pts',(-1.03590028118403,-1.10291468377004,
-0.748369923189322));
#373471=CARTESIAN_POINT('Ctrl Pts',(-1.17280179174001,-0.956070753908902,
-0.759035598238684));
#373472=CARTESIAN_POINT('Ctrl Pts',(-1.3767933757908,-0.624954618657059,
-0.778047818326026));
#373473=CARTESIAN_POINT('Ctrl Pts',(-1.44485502153325,-0.445602379258366,
-0.787744312263425));
#373474=CARTESIAN_POINT('Ctrl Pts',(-1.51157510457803,-0.0638798043074548,
-0.808951121982921));
#373475=CARTESIAN_POINT('Ctrl Pts',(-1.50686154990082,0.135315468900849,
-0.820017526050049));
#373476=CARTESIAN_POINT('Ctrl Pts',(-1.42072944177977,0.519826796441412,
-0.841379266468969));
#373477=CARTESIAN_POINT('Ctrl Pts',(-1.34041147848882,0.701408342574253,
-0.850826321066076));
#373478=CARTESIAN_POINT('Ctrl Pts',(-1.11301247659109,1.02506664015431,
-0.870757568913055));
#373479=CARTESIAN_POINT('Ctrl Pts',(-0.967454351703998,1.16343026506801,
-0.881604171497448));
#373480=CARTESIAN_POINT('Ctrl Pts',(-0.635115562016325,1.37266797728933,
-0.903405987644295));
#373481=CARTESIAN_POINT('Ctrl Pts',(-0.452550112791165,1.44319101552553,
-0.914148645199875));
#373482=CARTESIAN_POINT('Ctrl Pts',(-0.0721853899205506,1.51056168593121,
-0.934320358972779));
#373483=CARTESIAN_POINT('Ctrl Pts',(0.121898984874503,1.5073650006368,-0.943160284293108));
#373484=CARTESIAN_POINT('Ctrl Pts',(0.505015634751395,1.42640810437434,
-0.963841795378523));
#373485=CARTESIAN_POINT('Ctrl Pts',(0.689756384050045,1.34681347846234,
-0.974941100654235));
#373486=CARTESIAN_POINT('Ctrl Pts',(1.01114244221697,1.12442097539839,-0.996581364116831));
#373487=CARTESIAN_POINT('Ctrl Pts',(1.14641454539783,0.986147182545734,
-1.00693058490596));
#373488=CARTESIAN_POINT('Ctrl Pts',(1.36138438016108,0.660361894575678,
-1.02632291723582));
#373489=CARTESIAN_POINT('Ctrl Pts',(1.43677705693931,0.474492717363865,
-1.03613929347965));
#373490=CARTESIAN_POINT('Ctrl Pts',(1.51039363418377,0.0860327684066216,
-1.05772040175505));
#373491=CARTESIAN_POINT('Ctrl Pts',(1.50864909123881,-0.112557774460352,
-1.06875320969211));
#373492=CARTESIAN_POINT('Ctrl Pts',(1.42999222080605,-0.491124924634311,
-1.08978471803511));
#373493=CARTESIAN_POINT('Ctrl Pts',(1.35638881218185,-0.668032060615846,
-1.09913049230816));
#373494=CARTESIAN_POINT('Ctrl Pts',(1.14218573227621,-0.992451568091215,
-1.11844799578065));
#373495=CARTESIAN_POINT('Ctrl Pts',(1.00071070989974,-1.13494655346006,
-1.1292129100064));
#373496=CARTESIAN_POINT('Ctrl Pts',(0.674145277752562,-1.35400436702194,
-1.15100973595186));
#373497=CARTESIAN_POINT('Ctrl Pts',(0.493146045688107,-1.42990112156553,
-1.16182630874659));
#373498=CARTESIAN_POINT('Ctrl Pts',(0.202873194368312,-1.48970817965823,
-1.17745337498649));
#373499=CARTESIAN_POINT('Ctrl Pts',(0.101459517442463,-1.49999999999999,
-1.18261852669106));
#373500=CARTESIAN_POINT('Ctrl Pts',(-1.52655665885959E-15,-1.5,-1.1875));
#373501=CARTESIAN_POINT('Origin',(0.,2.04523456705693E-15,3.99999999999998));
#373502=CARTESIAN_POINT('',(-3.11589194069134E-14,-1.5,-1.75));
#373503=CARTESIAN_POINT('',(-7.75886181951911E-14,-1.5,-1.68750000000001));
#373504=CARTESIAN_POINT('',(-1.83697019872103E-16,-1.5,3.99999999999998));
#373505=CARTESIAN_POINT('Ctrl Pts',(-6.02989880249538E-14,-1.49999999999999,
-1.75));
#373506=CARTESIAN_POINT('Ctrl Pts',(0.118890713075185,-1.5,-1.74427986790016));
#373507=CARTESIAN_POINT('Ctrl Pts',(0.237602307351081,-1.48586871165855,
-1.7381758178703));
#373508=CARTESIAN_POINT('Ctrl Pts',(0.546666267057612,-1.41088712561192,
-1.72122314934122));
#373509=CARTESIAN_POINT('Ctrl Pts',(0.728459862929731,-1.32619188177961,
-1.71012395521974));
#373510=CARTESIAN_POINT('Ctrl Pts',(1.042461392657,-1.09535588767151,-1.68860443862946));
#373511=CARTESIAN_POINT('Ctrl Pts',(1.1734329245697,-0.953733812956441,
-1.67836912134243));
#373512=CARTESIAN_POINT('Ctrl Pts',(1.38015928113032,-0.620831811155973,
-1.65917571704723));
#373513=CARTESIAN_POINT('Ctrl Pts',(1.45077075562653,-0.4307868926055,-1.64893260514475));
#373514=CARTESIAN_POINT('Ctrl Pts',(1.51226779727029,-0.0387070076876947,
-1.62715038931598));
#373515=CARTESIAN_POINT('Ctrl Pts',(1.50437321178324,0.159112556164134,
-1.61616041354643));
#373516=CARTESIAN_POINT('Ctrl Pts',(1.41433511710263,0.534558138909894,
-1.59530232561611));
#373517=CARTESIAN_POINT('Ctrl Pts',(1.3353474978557,0.709175132572235,-1.58621429387427));
#373518=CARTESIAN_POINT('Ctrl Pts',(1.11126353645838,1.02696264563013,-1.56660561833651));
#373519=CARTESIAN_POINT('Ctrl Pts',(0.965468576997061,1.16507896747882,
-1.55575449058309));
#373520=CARTESIAN_POINT('Ctrl Pts',(0.632798716902561,1.3737330804517,-1.5339529568941));
#373521=CARTESIAN_POINT('Ctrl Pts',(0.450145830252578,1.44393850638475,
-1.52321491506744));
#373522=CARTESIAN_POINT('Ctrl Pts',(0.0696414072599108,1.51068893531618,
-1.50305370889912));
#373523=CARTESIAN_POINT('Ctrl Pts',(-0.124500319721521,1.50716026437133,
-1.49420887180708));
#373524=CARTESIAN_POINT('Ctrl Pts',(-0.50749951875255,1.42552135196551,
-1.47351406668525));
#373525=CARTESIAN_POINT('Ctrl Pts',(-0.692069231833775,1.34562133072832,
-1.46241450718991));
#373526=CARTESIAN_POINT('Ctrl Pts',(-1.0130232940995,1.122721426836,-1.44078093367235));
#373527=CARTESIAN_POINT('Ctrl Pts',(-1.14804257451774,0.984245374055827,
-1.43043825849274));
#373528=CARTESIAN_POINT('Ctrl Pts',(-1.36252636145643,0.658037569027983,
-1.41105757456481));
#373529=CARTESIAN_POINT('Ctrl Pts',(-1.43763913704559,0.47192412387742,
-1.40121800688207));
#373530=CARTESIAN_POINT('Ctrl Pts',(-1.51054509999985,0.0832463366017405,
-1.37962479647787));
#373531=CARTESIAN_POINT('Ctrl Pts',(-1.5084370634031,-0.115303956207632,
-1.36859422465513));
#373532=CARTESIAN_POINT('Ctrl Pts',(-1.42910812788447,-0.493689801146634,
-1.34757278882518));
#373533=CARTESIAN_POINT('Ctrl Pts',(-1.35518963527169,-0.670460604022503,
-1.33824435272663));
#373534=CARTESIAN_POINT('Ctrl Pts',(-1.14040697609685,-0.994495332354895,
-1.31890965254308));
#373535=CARTESIAN_POINT('Ctrl Pts',(-0.99867560474559,-1.13673807636535,
-1.30813941142593));
#373536=CARTESIAN_POINT('Ctrl Pts',(-0.67174415438103,-1.35519238150162,
-1.28634173954371));
#373537=CARTESIAN_POINT('Ctrl Pts',(-0.490643410544042,-1.4307572611263,
-1.2755295015093));
#373538=CARTESIAN_POINT('Ctrl Pts',(-0.20115025991711,-1.48988270973585,
-1.25995888223323));
#373539=CARTESIAN_POINT('Ctrl Pts',(-0.100595398491377,-1.5,-1.25483989836652));
#373540=CARTESIAN_POINT('Ctrl Pts',(-6.07153216591882E-16,-1.5,-1.25));
#373541=CARTESIAN_POINT('Ctrl Pts',(-1.70803542250024E-16,-1.5,-1.1875));
#373542=CARTESIAN_POINT('Ctrl Pts',(-0.0891224322423083,-1.5,-1.19178790502049));
#373543=CARTESIAN_POINT('Ctrl Pts',(-0.17825876817414,-1.49205861462193,
-1.1962970730207));
#373544=CARTESIAN_POINT('Ctrl Pts',(-0.462982132261434,-1.44068225222714,
-1.21142295344003));
#373545=CARTESIAN_POINT('Ctrl Pts',(-0.650528214500254,-1.36627879298293,
-1.22251303128566));
#373546=CARTESIAN_POINT('Ctrl Pts',(-0.979066611739039,-1.15254596551894,
-1.24425686527785));
#373547=CARTESIAN_POINT('Ctrl Pts',(-1.11854839282021,-1.01774373462307,
-1.25471219201281));
#373548=CARTESIAN_POINT('Ctrl Pts',(-1.34164444619969,-0.699076518440931,
-1.2742977730018));
#373549=CARTESIAN_POINT('Ctrl Pts',(-1.42168329624434,-0.51725270976017,
-1.28376373834652));
#373550=CARTESIAN_POINT('Ctrl Pts',(-1.50710590224472,-0.132511918964616,
-1.30513822672405));
#373551=CARTESIAN_POINT('Ctrl Pts',(-1.5114505885865,0.0666544100360032,
-1.31620302277964));
#373552=CARTESIAN_POINT('Ctrl Pts',(-1.44404865814611,0.448200094555797,
-1.33740000525297));
#373553=CARTESIAN_POINT('Ctrl Pts',(-1.37567310705197,0.627411452301136,
-1.34707432600766));
#373554=CARTESIAN_POINT('Ctrl Pts',(-1.17110246502015,0.958151941051232,
-1.36610397141006));
#373555=CARTESIAN_POINT('Ctrl Pts',(-1.03393881583429,1.10475411093668,
-1.37677554305525));
#373556=CARTESIAN_POINT('Ctrl Pts',(-0.713596781309212,1.33371543591048,
-1.39854804318224));
#373557=CARTESIAN_POINT('Ctrl Pts',(-0.534365319017502,1.41508980830061,
-1.40943172016541));
#373558=CARTESIAN_POINT('Ctrl Pts',(-0.158945587367972,1.50370072773037,
-1.4299555248546));
#373559=CARTESIAN_POINT('Ctrl Pts',(0.0333068351863567,1.51170981039486,
-1.43877720334395));
#373560=CARTESIAN_POINT('Ctrl Pts',(0.420126818038397,1.45384098740134,
-1.45899555575162));
#373561=CARTESIAN_POINT('Ctrl Pts',(0.610363243336896,1.3847747412201,-1.47006681686964));
#373562=CARTESIAN_POINT('Ctrl Pts',(0.945892390419239,1.18001118896129,
-1.49189784693702));
#373563=CARTESIAN_POINT('Ctrl Pts',(1.08953518990553,1.04884180942881,-1.50245245822548));
#373564=CARTESIAN_POINT('Ctrl Pts',(1.32073903794679,0.737378727795451,
-1.52222801081843));
#373565=CARTESIAN_POINT('Ctrl Pts',(1.40535812934366,0.55951452188571,-1.5314158598951));
#373566=CARTESIAN_POINT('Ctrl Pts',(1.50241818589091,0.178621252830884,
-1.55257659706482));
#373567=CARTESIAN_POINT('Ctrl Pts',(1.51285259677747,-0.0209368779816766,
-1.56366315988774));
#373568=CARTESIAN_POINT('Ctrl Pts',(1.45671497336007,-0.405351321204523,
-1.58501951784456));
#373569=CARTESIAN_POINT('Ctrl Pts',(1.39348794957596,-0.586908934735619,
-1.59509213906472));
#373570=CARTESIAN_POINT('Ctrl Pts',(1.19841716461937,-0.923752394666512,
-1.61383424935772));
#373571=CARTESIAN_POINT('Ctrl Pts',(1.06559381468328,-1.07424619729206,
-1.62440509916735));
#373572=CARTESIAN_POINT('Ctrl Pts',(0.751639208296201,-1.3127339875866,
-1.64613490805144));
#373573=CARTESIAN_POINT('Ctrl Pts',(0.574296844781584,-1.39943597200853,
-1.65707568495043));
#373574=CARTESIAN_POINT('Ctrl Pts',(0.259343809553784,-1.48314872736857,
-1.67455422423856));
#373575=CARTESIAN_POINT('Ctrl Pts',(0.129830828717176,-1.50000000000001,
-1.68125351134092));
#373576=CARTESIAN_POINT('Ctrl Pts',(-1.55327140038963E-13,-1.5,-1.68750000000001));
#373577=CARTESIAN_POINT('Origin',(0.,2.04523456705693E-15,3.99999999999998));
#373578=CARTESIAN_POINT('',(-1.24084586568037E-13,-1.5,-2.25000000000001));
#373579=CARTESIAN_POINT('',(-7.76217529874747E-14,-1.5,-2.18750000000001));
#373580=CARTESIAN_POINT('',(-1.83697019872103E-16,-1.5,3.99999999999998));
#373581=CARTESIAN_POINT('Ctrl Pts',(-2.50077736296817E-13,-1.49999999999999,
-2.25000000000001));
#373582=CARTESIAN_POINT('Ctrl Pts',(0.15137822816204,-1.50000000000002,
-2.24271681160177));
#373583=CARTESIAN_POINT('Ctrl Pts',(0.302123674236074,-1.47709065200341,
-2.23482769716825));
#373584=CARTESIAN_POINT('Ctrl Pts',(0.635500754617079,-1.37298397441661,
-2.21589623275476));
#373585=CARTESIAN_POINT('Ctrl Pts',(0.810426639220842,-1.27755733234257,
-2.20482936715013));
#373586=CARTESIAN_POINT('Ctrl Pts',(1.10779197182812,-1.02906110387188,
-2.18361969790135));
#373587=CARTESIAN_POINT('Ctrl Pts',(1.22916603383622,-0.880500500729423,
-2.17391669448497));
#373588=CARTESIAN_POINT('Ctrl Pts',(1.41410422301827,-0.538371936808744,
-2.15490955204493));
#373589=CARTESIAN_POINT('Ctrl Pts',(1.47292312942534,-0.346420806891367,
-2.14424560038285));
#373590=CARTESIAN_POINT('Ctrl Pts',(1.51194236713472,0.0454357372948264,
-2.12247579237251));
#373591=CARTESIAN_POINT('Ctrl Pts',(1.49323620480947,0.24142868694008,-2.11158729516999));
#373592=CARTESIAN_POINT('Ctrl Pts',(1.38308362845326,0.611098841720022,
-2.09105006434889));
#373593=CARTESIAN_POINT('Ctrl Pts',(1.29430022173091,0.781757708685455,
-2.08222322321111));
#373594=CARTESIAN_POINT('Ctrl Pts',(1.05147957165038,1.0883793409421,-2.06202324167436));
#373595=CARTESIAN_POINT('Ctrl Pts',(0.896805860442969,1.21897585527822,
-2.0509538183204));
#373596=CARTESIAN_POINT('Ctrl Pts',(0.552051291897144,1.40797513353587,
-2.02911682645594));
#373597=CARTESIAN_POINT('Ctrl Pts',(0.366722026935949,1.46720368714329,
-2.0185549304379));
#373598=CARTESIAN_POINT('Ctrl Pts',(-0.018444638594273,1.51251237367315,
-1.99876501597651));
#373599=CARTESIAN_POINT('Ctrl Pts',(-0.214704164387485,1.49731244788828,
-1.98959538684923));
#373600=CARTESIAN_POINT('Ctrl Pts',(-0.593279482434409,1.39183463507412,
-1.96845123412248));
#373601=CARTESIAN_POINT('Ctrl Pts',(-0.771570684384589,1.30148301662169,
-1.95736342748991));
#373602=CARTESIAN_POINT('Ctrl Pts',(-1.07694491947251,1.06136375609258,
-1.9360011232948));
#373603=CARTESIAN_POINT('Ctrl Pts',(-1.20294566781614,0.916105716146694,
-1.92590396390956));
#373604=CARTESIAN_POINT('Ctrl Pts',(-1.3978809398763,0.579142218359234,
-1.90716503909892));
#373605=CARTESIAN_POINT('Ctrl Pts',(-1.46225987747819,0.389018390923116,
-1.89661213282906));
#373606=CARTESIAN_POINT('Ctrl Pts',(-1.51269414803051,-0.00216019987483579,
-1.87487998889584));
#373607=CARTESIAN_POINT('Ctrl Pts',(-1.49952897924019,-0.199165252005918,
-1.86393526377745));
#373608=CARTESIAN_POINT('Ctrl Pts',(-1.39970813854547,-0.571842430541103,
-1.84323097608105));
#373609=CARTESIAN_POINT('Ctrl Pts',(-1.31600412169686,-0.744521148433023,
-1.834301801481));
#373610=CARTESIAN_POINT('Ctrl Pts',(-1.08331725769131,-1.05640436976061,
-1.81444322670214));
#373611=CARTESIAN_POINT('Ctrl Pts',(-0.933852575747988,-1.19057451095622,
-1.80352515547273));
#373612=CARTESIAN_POINT('Ctrl Pts',(-0.596109210807379,-1.38997725389203,
-1.78173650516906));
#373613=CARTESIAN_POINT('Ctrl Pts',(-0.412152027269476,-1.45517302032402,
-1.77107486753748));
#373614=CARTESIAN_POINT('Ctrl Pts',(-0.147590902778664,-1.49455896509157,
-1.75725211047933));
#373615=CARTESIAN_POINT('Ctrl Pts',(-0.0737683192890569,-1.49999999999999,
-1.7535491799166));
#373616=CARTESIAN_POINT('Ctrl Pts',(-6.21341417939547E-14,-1.5,-1.75));
#373617=CARTESIAN_POINT('Ctrl Pts',(-1.5499353937051E-13,-1.5,-1.68750000000001));
#373618=CARTESIAN_POINT('Ctrl Pts',(-0.0596763528147572,-1.49999999999999,
-1.69037117986349));
#373619=CARTESIAN_POINT('Ctrl Pts',(-0.119410271247936,-1.49643905972868,
-1.69334404436148));
#373620=CARTESIAN_POINT('Ctrl Pts',(-0.376383239736843,-1.46557247182356,
-1.70656506729203));
#373621=CARTESIAN_POINT('Ctrl Pts',(-0.5671766414312,-1.4028042181917,-1.7174881817119));
#373622=CARTESIAN_POINT('Ctrl Pts',(-0.908284760041371,-1.20929160666783,
-1.73927510404054));
#373623=CARTESIAN_POINT('Ctrl Pts',(-1.05642384570278,-1.08228973211698,
-1.74993027897119));
#373624=CARTESIAN_POINT('Ctrl Pts',(-1.29649837243605,-0.7788274321849,
-1.76991037835556));
#373625=CARTESIAN_POINT('Ctrl Pts',(-1.38607890643986,-0.605202148773951,
-1.77887765840131));
#373626=CARTESIAN_POINT('Ctrl Pts',(-1.49570810019784,-0.228661286203849,
-1.79979659521076));
#373627=CARTESIAN_POINT('Ctrl Pts',(-1.51280761426486,-0.0288828491712062,
-1.81089539726813));
#373628=CARTESIAN_POINT('Ctrl Pts',(-1.46906203259689,0.358289953203854,
-1.83240499740008));
#373629=CARTESIAN_POINT('Ctrl Pts',(-1.41151678854936,0.542363502300319,
-1.84263130568322));
#373630=CARTESIAN_POINT('Ctrl Pts',(-1.22579098571212,0.887567173592386,
-1.86180928742167));
#373631=CARTESIAN_POINT('Ctrl Pts',(-1.09604694951024,1.04358172875388,
-1.87208813124212));
#373632=CARTESIAN_POINT('Ctrl Pts',(-0.786539963597927,1.2922030619363,
-1.89388544118879));
#373633=CARTESIAN_POINT('Ctrl Pts',(-0.611098183816944,1.38383399431454,
-1.90487169143127));
#373634=CARTESIAN_POINT('Ctrl Pts',(-0.240708184574894,1.49270255667511,
-1.92571621531081));
#373635=CARTESIAN_POINT('Ctrl Pts',(-0.0499335931999016,1.51115673901871,
-1.93478765945971));
#373636=CARTESIAN_POINT('Ctrl Pts',(0.337252655791109,1.47506620261309,
-1.95441868144999));
#373637=CARTESIAN_POINT('Ctrl Pts',(0.52962784592717,1.41740390921588,-1.96527606747301));
#373638=CARTESIAN_POINT('Ctrl Pts',(0.876186819683551,1.23282448716524,
-1.98707710004012));
#373639=CARTESIAN_POINT('Ctrl Pts',(1.02798965381075,1.10941871911367,-1.99780865530381));
#373640=CARTESIAN_POINT('Ctrl Pts',(1.27539717593949,0.81266630562079,-2.01795517785921));
#373641=CARTESIAN_POINT('Ctrl Pts',(1.36905073696059,0.642468802256435,
-2.02680728876339));
#373642=CARTESIAN_POINT('Ctrl Pts',(1.48894178607173,0.269628878302083,
-2.04752061787197));
#373643=CARTESIAN_POINT('Ctrl Pts',(1.51154254627943,0.0698314094303458,
-2.05862047725374));
#373644=CARTESIAN_POINT('Ctrl Pts',(1.47806787363015,-0.319402952898901,
-2.08024460849425));
#373645=CARTESIAN_POINT('Ctrl Pts',(1.42523301741552,-0.505405768351132,
-2.0905780982416));
#373646=CARTESIAN_POINT('Ctrl Pts',(1.24912008159399,-0.853964715151503,
-2.10994248417496));
#373647=CARTESIAN_POINT('Ctrl Pts',(1.12500564835859,-1.01190277176006,
-2.11981488416656));
#373648=CARTESIAN_POINT('Ctrl Pts',(0.824093856174803,-1.26867097782277,
-2.14142495968661));
#373649=CARTESIAN_POINT('Ctrl Pts',(0.650885962917394,-1.36565198501259,
-2.15245234520282));
#373650=CARTESIAN_POINT('Ctrl Pts',(0.313880864981918,-1.47525183690481,
-2.17171095086744));
#373651=CARTESIAN_POINT('Ctrl Pts',(0.157333807750998,-1.50000000000001,
-2.17993027364519));
#373652=CARTESIAN_POINT('Ctrl Pts',(-1.5484141746569E-13,-1.5,-2.18750000000001));
#373653=CARTESIAN_POINT('Origin',(0.,2.04523456705693E-15,3.99999999999998));
#373654=CARTESIAN_POINT('',(-7.92750261663246E-15,-1.5,-2.75));
#373655=CARTESIAN_POINT('',(2.81886895545316E-8,-1.49999999999999,-2.68749999728754));
#373656=CARTESIAN_POINT('',(-1.83697019872103E-16,-1.5,3.99999999999998));
#373657=CARTESIAN_POINT('Ctrl Pts',(-1.57512891618694E-14,-1.49999999999999,
-2.75));
#373658=CARTESIAN_POINT('Ctrl Pts',(0.175163016033045,-1.5,-2.74157246546177));
#373659=CARTESIAN_POINT('Ctrl Pts',(0.349117234507293,-1.46932142419033,
-2.73235090656183));
#373660=CARTESIAN_POINT('Ctrl Pts',(0.699332793758691,-1.3415912281678,
-2.71195309161052));
#373661=CARTESIAN_POINT('Ctrl Pts',(0.869557542793228,-1.23806504880211,
-2.70088742234943));
#373662=CARTESIAN_POINT('Ctrl Pts',(1.15974259819827,-0.971446494831827,
-2.67951981641807));
#373663=CARTESIAN_POINT('Ctrl Pts',(1.27699845725887,-0.811153772458503,
-2.67006409846992));
#373664=CARTESIAN_POINT('Ctrl Pts',(1.44108871190044,-0.458500535932944,
-2.65047225199627));
#373665=CARTESIAN_POINT('Ctrl Pts',(1.48792081687523,-0.270244218523759,
-2.64001356769576));
#373666=CARTESIAN_POINT('Ctrl Pts',(1.50838416942693,0.121200861562273,
-2.61826661880209));
#373667=CARTESIAN_POINT('Ctrl Pts',(1.47885227826653,0.320813943583571,
-2.60717700313424));
#373668=CARTESIAN_POINT('Ctrl Pts',(1.34615009396296,0.688855334413892,
-2.58673025919923));
#373669=CARTESIAN_POINT('Ctrl Pts',(1.24737073993788,0.854815193722011,
-2.57793595288125));
#373670=CARTESIAN_POINT('Ctrl Pts',(0.99069001715621,1.14295689273815,-2.55758245976466));
#373671=CARTESIAN_POINT('Ctrl Pts',(0.834335404076568,1.26162241498806,
-2.5467635804285));
#373672=CARTESIAN_POINT('Ctrl Pts',(0.481161746154804,1.43457608369148,
-2.52496723631409));
#373673=CARTESIAN_POINT('Ctrl Pts',(0.286971912806408,1.48566319164258,
-2.51420518726898));
#373674=CARTESIAN_POINT('Ctrl Pts',(-0.101108231842388,1.5085871782716,
-2.49489689519761));
#373675=CARTESIAN_POINT('Ctrl Pts',(-0.291094986015094,1.48369344631382,
-2.48554172613075));
#373676=CARTESIAN_POINT('Ctrl Pts',(-0.658176161474092,1.36216847385968,
-2.46450483116266));
#373677=CARTESIAN_POINT('Ctrl Pts',(-0.830953964747722,1.26420474562025,
-2.45347084055351));
#373678=CARTESIAN_POINT('Ctrl Pts',(-1.13027043874279,1.0059499679797,-2.43189622616067));
#373679=CARTESIAN_POINT('Ctrl Pts',(-1.25335341632362,0.847659026260113,
-2.42209216812556));
#373680=CARTESIAN_POINT('Ctrl Pts',(-1.42768057231883,0.498484823681387,
-2.40269360131563));
#373681=CARTESIAN_POINT('Ctrl Pts',(-1.47963142692091,0.312135909405832,
-2.39234088385588));
#373682=CARTESIAN_POINT('Ctrl Pts',(-1.51118459316081,-0.0774529204248046,
-2.3706970599764));
#373683=CARTESIAN_POINT('Ctrl Pts',(-1.48755760137254,-0.27723771912035,
-2.35959790449331));
#373684=CARTESIAN_POINT('Ctrl Pts',(-1.36576210682761,-0.649376506090869,
-2.3389235274394));
#373685=CARTESIAN_POINT('Ctrl Pts',(-1.27134960904108,-0.818941361342293,
-2.33008613210933));
#373686=CARTESIAN_POINT('Ctrl Pts',(-1.01876421638275,-1.11895309720847,
-2.30959995240885));
#373687=CARTESIAN_POINT('Ctrl Pts',(-0.860805519902715,-1.24456301647905,
-2.29851099665078));
#373688=CARTESIAN_POINT('Ctrl Pts',(-0.511759732876251,-1.42304305712749,
-2.27675974448561));
#373689=CARTESIAN_POINT('Ctrl Pts',(-0.325354062737634,-1.47685928132321,
-2.26629640238298));
#373690=CARTESIAN_POINT('Ctrl Pts',(-0.0892703169527611,-1.49801001581249,
-2.25435029746548));
#373691=CARTESIAN_POINT('Ctrl Pts',(-0.0446103398246381,-1.49999999999999,
-2.25214631597553));
#373692=CARTESIAN_POINT('Ctrl Pts',(-2.47985476116201E-13,-1.5,-2.25000000000001));
#373693=CARTESIAN_POINT('Ctrl Pts',(-1.55059808955077E-13,-1.5,-2.18750000000001));
#373694=CARTESIAN_POINT('Ctrl Pts',(-0.0320907701424565,-1.49999999999999,
-2.18904396789835));
#373695=CARTESIAN_POINT('Ctrl Pts',(-0.0642115404450032,-1.49897020703486,
-2.19061798454009));
#373696=CARTESIAN_POINT('Ctrl Pts',(-0.294774887254793,-1.48413534957626,
-2.20212304810943));
#373697=CARTESIAN_POINT('Ctrl Pts',(-0.488698988986171,-1.43202683042019,
-2.21290068466963));
#373698=CARTESIAN_POINT('Ctrl Pts',(-0.840874537428373,-1.25725825310949,
-2.2346994213473));
#373699=CARTESIAN_POINT('Ctrl Pts',(-0.996534144617197,-1.13784836038626,
-2.24550553915453));
#373700=CARTESIAN_POINT('Ctrl Pts',(-1.25178559953188,-0.848370697709088,
-2.26582737669052));
#373701=CARTESIAN_POINT('Ctrl Pts',(-1.3497766463203,-0.681764192329304,
-2.27462421153712));
#373702=CARTESIAN_POINT('Ctrl Pts',(-1.48051643545944,-0.312975601528768,
-2.2951124665816));
#373703=CARTESIAN_POINT('Ctrl Pts',(-1.50898267362771,-0.113319091924842,
-2.30620449489293));
#373704=CARTESIAN_POINT('Ctrl Pts',(-1.48651373348182,0.277814066187296,
-2.32793411478806));
#373705=CARTESIAN_POINT('Ctrl Pts',(-1.438753797226,0.465736733279212,-2.33837426295983));
#373706=CARTESIAN_POINT('Ctrl Pts',(-1.27282051378257,0.81776959295667,
-2.35793164405303));
#373707=CARTESIAN_POINT('Ctrl Pts',(-1.15452623884263,0.977704243723731,
-2.36744461498256));
#373708=CARTESIAN_POINT('Ctrl Pts',(-0.862699185980956,1.2428365926044,
-2.38884993807868));
#373709=CARTESIAN_POINT('Ctrl Pts',(-0.692004024660368,1.34537042866645,
-2.39991067496967));
#373710=CARTESIAN_POINT('Ctrl Pts',(-0.327420632201285,1.47612274447825,
-2.42108371039041));
#373711=CARTESIAN_POINT('Ctrl Pts',(-0.137945278740974,1.50568186893175,
-2.43070527498944));
#373712=CARTESIAN_POINT('Ctrl Pts',(0.250680959569865,1.49221214633594,
-2.44977722255901));
#373713=CARTESIAN_POINT('Ctrl Pts',(0.446030851030766,1.44588029580342,
-2.46046299444223));
#373714=CARTESIAN_POINT('Ctrl Pts',(0.803710783288726,1.28141890135308,
-2.48224025027471));
#373715=CARTESIAN_POINT('Ctrl Pts',(0.963243425251321,1.16625730467924,
-2.49311470133078));
#373716=CARTESIAN_POINT('Ctrl Pts',(1.22652673135604,0.88433369310823,-2.51361313673437));
#373717=CARTESIAN_POINT('Ctrl Pts',(1.32894620751343,0.72132701314505,-2.52242627704736));
#373718=CARTESIAN_POINT('Ctrl Pts',(1.47065864309764,0.356774492714373,
-2.54267919484907));
#373719=CARTESIAN_POINT('Ctrl Pts',(1.50509953521437,0.157432120196595,
-2.55375377110006));
#373720=CARTESIAN_POINT('Ctrl Pts',(1.49389896064446,-0.235318813030891,
-2.57557326739048));
#373721=CARTESIAN_POINT('Ctrl Pts',(1.45136396314214,-0.425052033288715,
-2.58611400184925));
#373722=CARTESIAN_POINT('Ctrl Pts',(1.29574302933759,-0.780522660203829,
-2.6058623700112));
#373723=CARTESIAN_POINT('Ctrl Pts',(1.18319968994291,-0.942451018260852,
-2.61508580666042));
#373724=CARTESIAN_POINT('Ctrl Pts',(0.900546019732095,-1.21579125958081,
-2.63627777219017));
#373725=CARTESIAN_POINT('Ctrl Pts',(0.732541205007289,-1.32382425951471,
-2.64736182427221));
#373726=CARTESIAN_POINT('Ctrl Pts',(0.373645074360534,-1.46480484870421,
-2.66854534988637));
#373727=CARTESIAN_POINT('Ctrl Pts',(0.187602774442,-1.49999999646629,-2.67847395720811));
#373728=CARTESIAN_POINT('Ctrl Pts',(2.82541730636798E-8,-1.5,-2.68749999864062));
#373729=CARTESIAN_POINT('Origin',(0.,2.04523456705693E-15,3.99999999999998));
#373730=CARTESIAN_POINT('',(7.56010857688836E-15,-1.5,-3.25));
#373731=CARTESIAN_POINT('',(5.4022942157451E-14,-1.5,-3.18749999999999));
#373732=CARTESIAN_POINT('',(-1.83697019872103E-16,-1.5,3.99999999999998));
#373733=CARTESIAN_POINT('Ctrl Pts',(1.53039141736488E-14,-1.5,-3.25));
#373734=CARTESIAN_POINT('Ctrl Pts',(0.0154330977189969,-1.5,-3.24925747473979));
#373735=CARTESIAN_POINT('Ctrl Pts',(0.0308755078629297,-1.49976182060752,
-3.2485078853411));
#373736=CARTESIAN_POINT('Ctrl Pts',(0.237395999187744,-1.49338117750452,
-3.23839442348327));
#373737=CARTESIAN_POINT('Ctrl Pts',(0.425559701281857,-1.4510066607058,
-3.22816432323422));
#373738=CARTESIAN_POINT('Ctrl Pts',(0.782623369709154,-1.29496299027641,
-3.20665054307637));
#373739=CARTESIAN_POINT('Ctrl Pts',(0.946995122227405,-1.1801001721097,
-3.19555156960811));
#373740=CARTESIAN_POINT('Ctrl Pts',(1.21798910903121,-0.896644503164139,
-3.17463959675713));
#373741=CARTESIAN_POINT('Ctrl Pts',(1.32339002900625,-0.732190954109843,
-3.16567727522832));
#373742=CARTESIAN_POINT('Ctrl Pts',(1.4658352660189,-0.372445769911063,
-3.14569143166172));
#373743=CARTESIAN_POINT('Ctrl Pts',(1.50158458221272,-0.180603642510261,
-3.13503353569501));
#373744=CARTESIAN_POINT('Ctrl Pts',(1.49826067554571,0.211574253785341,
-3.1132458747897));
#373745=CARTESIAN_POINT('Ctrl Pts',(1.45704443977926,0.408152285478764,
-3.10232487302896));
#373746=CARTESIAN_POINT('Ctrl Pts',(1.30373031096641,0.765814626563727,
-3.08245474296868));
#373747=CARTESIAN_POINT('Ctrl Pts',(1.19622559605682,0.924790202756146,
-3.07353148074802));
#373748=CARTESIAN_POINT('Ctrl Pts',(0.92372723529977,1.19790343580508,-3.05283441855748));
#373749=CARTESIAN_POINT('Ctrl Pts',(0.759855816388863,1.30799769726818,
-3.04189197730955));
#373750=CARTESIAN_POINT('Ctrl Pts',(0.396187080606716,1.46031857135712,
-3.02016382170989));
#373751=CARTESIAN_POINT('Ctrl Pts',(0.199408818214532,1.49991927713665,
-3.00959630354133));
#373752=CARTESIAN_POINT('Ctrl Pts',(-0.189856778671457,1.50007709674746,
-2.99086336990089));
#373753=CARTESIAN_POINT('Ctrl Pts',(-0.378687652851797,1.46387523445677,
-2.98077691609773));
#373754=CARTESIAN_POINT('Ctrl Pts',(-0.739566877190839,1.31992792042753,
-2.9594155698205));
#373755=CARTESIAN_POINT('Ctrl Pts',(-0.907083090981407,1.21093924646165,
-2.94832847906098));
#373756=CARTESIAN_POINT('Ctrl Pts',(-1.18812362100217,0.936178993106713,
-2.92717468099606));
#373757=CARTESIAN_POINT('Ctrl Pts',(-1.29966801217108,0.773901223266376,
-2.91799451240369));
#373758=CARTESIAN_POINT('Ctrl Pts',(-1.45347108661435,0.41783299888567,
-2.89821294438254));
#373759=CARTESIAN_POINT('Ctrl Pts',(-1.49507687549898,0.227795003267051,
-2.88765527795928));
#373760=CARTESIAN_POINT('Ctrl Pts',(-1.50427996417078,-0.165208685895577,
-2.86582173967247));
#373761=CARTESIAN_POINT('Ctrl Pts',(-1.46878317917199,-0.364477662027525,
-2.85475124099847));
#373762=CARTESIAN_POINT('Ctrl Pts',(-1.32513837329591,-0.728269669186224,
-2.8345405739341));
#373763=CARTESIAN_POINT('Ctrl Pts',(-1.22193340796847,-0.890646368877972,
-2.82571678825526));
#373764=CARTESIAN_POINT('Ctrl Pts',(-0.957225466308382,-1.17121810923077,
-2.80518736201984));
#373765=CARTESIAN_POINT('Ctrl Pts',(-0.797014441261015,-1.28560969202727,
-2.79430166151675));
#373766=CARTESIAN_POINT('Ctrl Pts',(-0.438385311437803,-1.44821577761855,
-2.77253027375232));
#373767=CARTESIAN_POINT('Ctrl Pts',(-0.242799898516706,-1.4935139455441,
-2.76186188374332));
#373768=CARTESIAN_POINT('Ctrl Pts',(-0.0293617344802457,-1.49978458922724,
-2.75141865074141));
#373769=CARTESIAN_POINT('Ctrl Pts',(-0.0146769070534305,-1.5,-2.75070614301985));
#373770=CARTESIAN_POINT('Ctrl Pts',(-1.56713082133928E-14,-1.5,-2.75));
#373771=CARTESIAN_POINT('Ctrl Pts',(2.82541728888338E-8,-1.5,-2.68749999864062));
#373772=CARTESIAN_POINT('Ctrl Pts',(-0.0027320928716755,-1.50000000005146,
-2.687631447881));
#373773=CARTESIAN_POINT('Ctrl Pts',(-0.00546452515622478,-1.49999253561752,
-2.68776311943298));
#373774=CARTESIAN_POINT('Ctrl Pts',(-0.207001458014825,-1.49889115499487,
-2.6974901635423));
#373775=CARTESIAN_POINT('Ctrl Pts',(-0.40358363203981,-1.45829274468987,
-2.70807596141949));
#373776=CARTESIAN_POINT('Ctrl Pts',(-0.766393227447706,-1.30416358286693,
-2.72981301182346));
#373777=CARTESIAN_POINT('Ctrl Pts',(-0.92963322737301,-1.19331031809287,
-2.74074615733658));
#373778=CARTESIAN_POINT('Ctrl Pts',(-1.20077459221899,-0.918889747502195,
-2.76141424596263));
#373779=CARTESIAN_POINT('Ctrl Pts',(-1.30752956616432,-0.759326959880522,
-2.77031516889539));
#373780=CARTESIAN_POINT('Ctrl Pts',(-1.45984960981038,-0.399001644028943,
-2.79033324199826));
#373781=CARTESIAN_POINT('Ctrl Pts',(-1.50009780204417,-0.200129413280295,
-2.80138169926208));
#373782=CARTESIAN_POINT('Ctrl Pts',(-1.49990559923608,0.193888453867102,
-2.82327158077027));
#373783=CARTESIAN_POINT('Ctrl Pts',(-1.46250271323157,0.385241403380367,
-2.83390230018768));
#373784=CARTESIAN_POINT('Ctrl Pts',(-1.31686710612883,0.743963622581648,
-2.85383131236553));
#373785=CARTESIAN_POINT('Ctrl Pts',(-1.20975732903253,0.90780681842778,
-2.86284571276972));
#373786=CARTESIAN_POINT('Ctrl Pts',(-0.935947302566849,1.18885033502406,
-2.88382616816019));
#373787=CARTESIAN_POINT('Ctrl Pts',(-0.770676738163206,1.30208025119187,
-2.89492302734659));
#373788=CARTESIAN_POINT('Ctrl Pts',(-0.412534434467264,1.45474160075709,
-2.91639475001066));
#373789=CARTESIAN_POINT('Ctrl Pts',(-0.224167349469574,1.4954029972334,
-2.92658704884861));
#373790=CARTESIAN_POINT('Ctrl Pts',(0.16549812277975,1.50403330736282,-2.94557456846029));
#373791=CARTESIAN_POINT('Ctrl Pts',(0.363174829007174,1.46889642578174,
-2.95583724528012));
#373792=CARTESIAN_POINT('Ctrl Pts',(0.730704038992162,1.32456691867321,
-2.97752915561535));
#373793=CARTESIAN_POINT('Ctrl Pts',(0.897327655309507,1.21787230515505,
-2.98850957735759));
#373794=CARTESIAN_POINT('Ctrl Pts',(1.17581111208616,0.950567488669378,
-3.0093332527101));
#373795=CARTESIAN_POINT('Ctrl Pts',(1.28662860170944,0.794156643403929,
-3.01838018647743));
#373796=CARTESIAN_POINT('Ctrl Pts',(1.44768797357916,0.440182107776354,
-3.03804543845674));
#373797=CARTESIAN_POINT('Ctrl Pts',(1.49322546113538,0.244578440345993,
-3.04891230886954));
#373798=CARTESIAN_POINT('Ctrl Pts',(1.50521819068071,-0.147821929795448,
-3.07071232943296));
#373799=CARTESIAN_POINT('Ctrl Pts',(1.47356569707093,-0.340808737409749,
-3.08143381874486));
#373800=CARTESIAN_POINT('Ctrl Pts',(1.33897451148274,-0.703039340644609,
-3.1015577411468));
#373801=CARTESIAN_POINT('Ctrl Pts',(1.23772603215813,-0.868995531784903,
-3.11042197661755));
#373802=CARTESIAN_POINT('Ctrl Pts',(0.973642324634376,-1.15829099819762,
-3.13116369509797));
#373803=CARTESIAN_POINT('Ctrl Pts',(0.811532249540049,-1.27711513932012,
-3.14226389030921));
#373804=CARTESIAN_POINT('Ctrl Pts',(0.457235322458853,-1.44139275207604,
-3.16387327618216));
#373805=CARTESIAN_POINT('Ctrl Pts',(0.26963351173158,-1.48795042209609,
-3.17419254112082));
#373806=CARTESIAN_POINT('Ctrl Pts',(0.0522115465392471,-1.49931910388413,
-3.18496905701478));
#373807=CARTESIAN_POINT('Ctrl Pts',(0.0260941836402007,-1.5,-3.18624454300425));
#373808=CARTESIAN_POINT('Ctrl Pts',(1.08229581334774E-13,-1.5,-3.18749999999999));
#373809=CARTESIAN_POINT('Origin',(0.,2.04523456705693E-15,3.99999999999998));
#373810=CARTESIAN_POINT('',(1.15973386931536E-13,-1.49999999999999,-3.74999999999999));
#373811=CARTESIAN_POINT('',(1.15973386931537E-13,-1.49999999999999,-3.68749999999999));
#373812=CARTESIAN_POINT('',(-1.83697019872103E-16,-1.5,3.99999999999998));
#373813=CARTESIAN_POINT('Ctrl Pts',(2.32130470882944E-13,-1.49999999999999,
-3.74999999999999));
#373814=CARTESIAN_POINT('Ctrl Pts',(0.0420030761821631,-1.49999999999999,
-3.74797912605495));
#373815=CARTESIAN_POINT('Ctrl Pts',(0.0840524578334832,-1.49823581808009,
-3.74590701918365));
#373816=CARTESIAN_POINT('Ctrl Pts',(0.317532157721825,-1.47854786920351,
-3.73412683441645));
#373817=CARTESIAN_POINT('Ctrl Pts',(0.504123157769973,-1.42575275674287,
-3.72368293983925));
#373818=CARTESIAN_POINT('Ctrl Pts',(0.853942399427975,-1.24926412137683,
-3.70194979163417));
#373819=CARTESIAN_POINT('Ctrl Pts',(1.01250261650075,-1.12460203240067,
-3.69085822382847));
#373820=CARTESIAN_POINT('Ctrl Pts',(1.26618588593558,-0.826716944862991,
-3.67037829607211));
#373821=CARTESIAN_POINT('Ctrl Pts',(1.36128392355952,-0.658478841679479,
-3.66158215787108));
#373822=CARTESIAN_POINT('Ctrl Pts',(1.48397740638111,-0.292571139284737,
-3.64125395218248));
#373823=CARTESIAN_POINT('Ctrl Pts',(1.50936051504709,-0.0980144946652442,
-3.63044524970362));
#373824=CARTESIAN_POINT('Ctrl Pts',(1.48421097083258,0.294354999955967,
-3.60864694444689));
#373825=CARTESIAN_POINT('Ctrl Pts',(1.43217179477893,0.488296558661019,
-3.59787241340772));
#373826=CARTESIAN_POINT('Ctrl Pts',(1.25944573706426,0.836571673933364,
-3.57852379589259));
#373827=CARTESIAN_POINT('Ctrl Pts',(1.14354006376931,0.989138303288629,
-3.56920919965695));
#373828=CARTESIAN_POINT('Ctrl Pts',(0.85591204017378,1.24742962295239,-3.54819593103996));
#373829=CARTESIAN_POINT('Ctrl Pts',(0.685192166379378,1.34876859625304,
-3.53716719580178));
#373830=CARTESIAN_POINT('Ctrl Pts',(0.312269766249229,1.48055548880213,
-3.5155642114447));
#373831=CARTESIAN_POINT('Ctrl Pts',(0.113476387161101,1.50885794998208,
-3.50570568938901));
#373832=CARTESIAN_POINT('Ctrl Pts',(-0.27636898959008,1.48672502335481,
-3.48633444143745));
#373833=CARTESIAN_POINT('Ctrl Pts',(-0.463841446690415,1.43929184955474,
-3.47599708047863));
#373834=CARTESIAN_POINT('Ctrl Pts',(-0.817535381145995,1.27329545295664,
-3.45436896210629));
#373835=CARTESIAN_POINT('Ctrl Pts',(-0.979160045924644,1.15364690708048,
-3.4432692210777));
#373836=CARTESIAN_POINT('Ctrl Pts',(-1.24179108047367,0.863137736198284,
-3.42256368034533));
#373837=CARTESIAN_POINT('Ctrl Pts',(-1.34217373310823,0.696864398573333,
-3.41371468880963));
#373838=CARTESIAN_POINT('Ctrl Pts',(-1.47510896404006,0.334115757684514,
-3.39356198653803));
#373839=CARTESIAN_POINT('Ctrl Pts',(-1.50589322665991,0.140898531544399,
-3.38282769619691));
#373840=CARTESIAN_POINT('Ctrl Pts',(-1.492070616974,-0.25152412225069,-3.36102643765274));
#373841=CARTESIAN_POINT('Ctrl Pts',(-1.4456247627367,-0.446909828186021,
-3.35017167621189));
#373842=CARTESIAN_POINT('Ctrl Pts',(-1.28293685010969,-0.800099124751201,
-3.33055004862493));
#373843=CARTESIAN_POINT('Ctrl Pts',(-1.17141645804915,-0.955972075839512,
-3.32147168739789));
#373844=CARTESIAN_POINT('Ctrl Pts',(-0.89166584427233,-1.22203810273209,
-3.30062145674782));
#373845=CARTESIAN_POINT('Ctrl Pts',(-0.724466581195555,-1.32800215144422,
-3.28963363265478));
#373846=CARTESIAN_POINT('Ctrl Pts',(-0.368720817963472,-1.46575064069154,
-3.26869145971749));
#373847=CARTESIAN_POINT('Ctrl Pts',(-0.185075007272709,-1.49999999999999,
-3.2589044254391));
#373848=CARTESIAN_POINT('Ctrl Pts',(1.67227343084164E-14,-1.49999999999999,
-3.25));
#373849=CARTESIAN_POINT('Ctrl Pts',(1.05748743095546E-13,-1.5,-3.1875));
#373850=CARTESIAN_POINT('Ctrl Pts',(-0.172624793809803,-1.5,-3.19580541426457));
#373851=CARTESIAN_POINT('Ctrl Pts',(-0.344156579903346,-1.47020600738534,
-3.20488585207672));
#373852=CARTESIAN_POINT('Ctrl Pts',(-0.691996997468058,-1.34527564392206,
-3.2250916198437));
#373853=CARTESIAN_POINT('Ctrl Pts',(-0.86211954019817,-1.24313224950465,
-3.23611396100867));
#373854=CARTESIAN_POINT('Ctrl Pts',(-1.14839476463202,-0.983496554079989,
-3.25709948681679));
#373855=CARTESIAN_POINT('Ctrl Pts',(-1.26354520632856,-0.830366556260505,
-3.26636852465207));
#373856=CARTESIAN_POINT('Ctrl Pts',(-1.4345577472031,-0.48124365055675,
-3.28576424163561));
#373857=CARTESIAN_POINT('Ctrl Pts',(-1.48564309176012,-0.287043308368793,
-3.29655314953494));
#373858=CARTESIAN_POINT('Ctrl Pts',(-1.50885375884096,0.105358613817684,
-3.31835325632308));
#373859=CARTESIAN_POINT('Ctrl Pts',(-1.48254282957616,0.299696593854507,
-3.32914981076958));
#373860=CARTESIAN_POINT('Ctrl Pts',(-1.35809696534895,0.665068852552179,
-3.34944826958612));
#373861=CARTESIAN_POINT('Ctrl Pts',(-1.26210268023943,0.832970856633082,
-3.35824846916903));
#373862=CARTESIAN_POINT('Ctrl Pts',(-1.00689323710206,1.12960922700053,
-3.37876719395939));
#373863=CARTESIAN_POINT('Ctrl Pts',(-0.84780130228411,1.25342394453506,
-3.38986080595143));
#373864=CARTESIAN_POINT('Ctrl Pts',(-0.497301745488257,1.42813436872872,
-3.41157729107906));
#373865=CARTESIAN_POINT('Ctrl Pts',(-0.310550154863041,1.48001861721066,
-3.42200361029681));
#373866=CARTESIAN_POINT('Ctrl Pts',(0.0775679172145885,1.51092539479631,
-3.4415354713457));
#373867=CARTESIAN_POINT('Ctrl Pts',(0.275377779215376,1.48764844687008,
-3.45109221827783));
#373868=CARTESIAN_POINT('Ctrl Pts',(0.650554370936392,1.36588439585195,
-3.47252524521366));
#373869=CARTESIAN_POINT('Ctrl Pts',(0.824234619747844,1.26865964712896,
-3.4835821275452));
#373870=CARTESIAN_POINT('Ctrl Pts',(1.11867540841364,1.01719913638398,-3.50473343078228));
#373871=CARTESIAN_POINT('Ctrl Pts',(1.23840059250391,0.867443918796923,
-3.51430867117782));
#373872=CARTESIAN_POINT('Ctrl Pts',(1.41969290810348,0.523461335807366,
-3.53341881467724));
#373873=CARTESIAN_POINT('Ctrl Pts',(1.47649168137935,0.33088917789354,-3.54411726789468));
#373874=CARTESIAN_POINT('Ctrl Pts',(1.51136182986144,-0.061172518020671,
-3.56589847322325));
#373875=CARTESIAN_POINT('Ctrl Pts',(1.49065092451211,-0.256759346419735,
-3.57676440813431));
#373876=CARTESIAN_POINT('Ctrl Pts',(1.37674479462488,-0.625316213987474,
-3.59723978966586));
#373877=CARTESIAN_POINT('Ctrl Pts',(1.2860891936887,-0.795247355491489,
-3.60604654247091));
#373878=CARTESIAN_POINT('Ctrl Pts',(1.04002858388445,-1.09928771354101,
-3.62633070458124));
#373879=CARTESIAN_POINT('Ctrl Pts',(0.884177261008663,-1.22813210013013,
-3.63740811558783));
#373880=CARTESIAN_POINT('Ctrl Pts',(0.53787178324674,-1.41342704098718,
-3.65921682734561));
#373881=CARTESIAN_POINT('Ctrl Pts',(0.352144619071328,-1.47074607461982,
-3.669744825077));
#373882=CARTESIAN_POINT('Ctrl Pts',(0.107185427923135,-1.49713116707827,
-3.68226334889112));
#373883=CARTESIAN_POINT('Ctrl Pts',(0.0535634300530825,-1.49999999999999,
-3.68492292827002));
#373884=CARTESIAN_POINT('Ctrl Pts',(2.32130470882946E-13,-1.49999999999999,
-3.68749999999999));
#373885=CARTESIAN_POINT('Origin',(0.,2.04523456705693E-15,3.99999999999998));
#373886=CARTESIAN_POINT('',(4.6279136560691E-14,-1.5,-4.24999999999999));
#373887=CARTESIAN_POINT('',(7.56010857688827E-15,-1.5,-4.1875));
#373888=CARTESIAN_POINT('',(-1.83697019872103E-16,-1.5,3.99999999999998));
#373889=CARTESIAN_POINT('Ctrl Pts',(9.2741970141254E-14,-1.49999999999999,
-4.25));
#373890=CARTESIAN_POINT('Ctrl Pts',(0.0693232899188041,-1.49999999999999,
-4.24666468165869));
#373891=CARTESIAN_POINT('Ctrl Pts',(0.138705632270155,-1.49519485879729,
-4.24319304601137));
#373892=CARTESIAN_POINT('Ctrl Pts',(0.399009714721784,-1.45880886234304,
-4.22965843788142));
#373893=CARTESIAN_POINT('Ctrl Pts',(0.583384578401812,-1.39534188150886,
-4.21902472642679));
#373894=CARTESIAN_POINT('Ctrl Pts',(0.924551674788282,-1.19814759239858,
-4.19713269770673));
#373895=CARTESIAN_POINT('Ctrl Pts',(1.07653828060304,-1.0636902135809,-4.18608531153565));
#373896=CARTESIAN_POINT('Ctrl Pts',(1.31211599018145,-0.751370166077832,
-4.16607551682389));
#373897=CARTESIAN_POINT('Ctrl Pts',(1.39674515418371,-0.57906444187859,
-4.15717024677103));
#373898=CARTESIAN_POINT('Ctrl Pts',(1.49846374621891,-0.206933243758507,
-4.13649629131991));
#373899=CARTESIAN_POINT('Ctrl Pts',(1.51264892419061,-0.0101024249300511,
-4.12556124582944));
#373900=CARTESIAN_POINT('Ctrl Pts',(1.46432051278063,0.381132946040274,
-4.1038259474422));
#373901=CARTESIAN_POINT('Ctrl Pts',(1.40099407937911,0.571611205590939,
-4.09324382191161));
#373902=CARTESIAN_POINT('Ctrl Pts',(1.20789244880423,0.909530858192071,
-4.07447050787821));
#373903=CARTESIAN_POINT('Ctrl Pts',(1.08277279888511,1.05541873660482,-4.06444441011438));
#373904=CARTESIAN_POINT('Ctrl Pts',(0.778806050866134,1.29714949545131,
-4.0431050598303));
#373905=CARTESIAN_POINT('Ctrl Pts',(0.601126187418435,1.38844780784244,
-4.03202036918128));
#373906=CARTESIAN_POINT('Ctrl Pts',(0.222993889241262,1.49613749901354,
-4.01083609019249));
#373907=CARTESIAN_POINT('Ctrl Pts',(0.0265280057553068,1.51242862909709,
-4.00162156896913));
#373908=CARTESIAN_POINT('Ctrl Pts',(-0.359050275912133,1.46908704568924,
-3.98186649237049));
#373909=CARTESIAN_POINT('Ctrl Pts',(-0.544591484364593,1.41086374167892,
-3.97132232281638));
#373910=CARTESIAN_POINT('Ctrl Pts',(-0.89016755138681,1.22381363159918,
-3.94949995014855));
#373911=CARTESIAN_POINT('Ctrl Pts',(-1.04546374828784,1.09413852903051,
-3.93842617220901));
#373912=CARTESIAN_POINT('Ctrl Pts',(-1.28999177385172,0.78887462257984,
-3.91818175913674));
#373913=CARTESIAN_POINT('Ctrl Pts',(-1.37976064818862,0.618599897004113,
-3.90936666094467));
#373914=CARTESIAN_POINT('Ctrl Pts',(-1.49189268104597,0.249515467065523,
-3.88886197039252));
#373915=CARTESIAN_POINT('Ctrl Pts',(-1.51165667168068,0.0537341457075633,
-3.87798523031708));
#373916=CARTESIAN_POINT('Ctrl Pts',(-1.47482512978302,-0.338236073364855,
-3.85620910703528));
#373917=CARTESIAN_POINT('Ctrl Pts',(-1.41707052806472,-0.530517375765477,
-3.84552681245747));
#373918=CARTESIAN_POINT('Ctrl Pts',(-1.23405402718182,-0.873625163654692,
-3.82646526868585));
#373919=CARTESIAN_POINT('Ctrl Pts',(-1.11355085321239,-1.02281532049236,
-3.8168308703912));
#373920=CARTESIAN_POINT('Ctrl Pts',(-0.817728849491741,-1.27287830481274,
-3.79565193359227));
#373921=CARTESIAN_POINT('Ctrl Pts',(-0.643458386551141,-1.36925621168849,
-3.78459017795484));
#373922=CARTESIAN_POINT('Ctrl Pts',(-0.307993231357976,-1.47618493681224,
-3.76547986078575));
#373923=CARTESIAN_POINT('Ctrl Pts',(-0.154340990313575,-1.49999999999999,
-3.75742573435872));
#373924=CARTESIAN_POINT('Ctrl Pts',(2.21316021065121E-13,-1.49999999999999,
-3.74999999999999));
#373925=CARTESIAN_POINT('Ctrl Pts',(2.33910113500713E-13,-1.5,-3.68749999999999));
#373926=CARTESIAN_POINT('Ctrl Pts',(-0.141276695353502,-1.5,-3.69429717817437));
#373927=CARTESIAN_POINT('Ctrl Pts',(-0.282092362620038,-1.48004645163004,
-3.70162644035696));
#373928=CARTESIAN_POINT('Ctrl Pts',(-0.608182943233829,-1.38535690811647,
-3.71994574582936));
#373929=CARTESIAN_POINT('Ctrl Pts',(-0.785307562700868,-1.29320857142521,
-3.73102733407602));
#373930=CARTESIAN_POINT('Ctrl Pts',(-1.08792750627408,-1.05008895026412,
-3.75234046570973));
#373931=CARTESIAN_POINT('Ctrl Pts',(-1.21228015028828,-0.903658276744491,
-3.76229676240296));
#373932=CARTESIAN_POINT('Ctrl Pts',(-1.40372356070962,-0.564877289250618,
-3.78111792837485));
#373933=CARTESIAN_POINT('Ctrl Pts',(-1.46613635494529,-0.3740906654696,
-3.79171718525157));
#373934=CARTESIAN_POINT('Ctrl Pts',(-1.51257207849374,0.0172890465575684,
-3.81346050258642));
#373935=CARTESIAN_POINT('Ctrl Pts',(-1.49746513068593,0.213957744631522,
-3.82438654136831));
#373936=CARTESIAN_POINT('Ctrl Pts',(-1.394030070704,0.585592642461911,-3.84503292458111));
#373937=CARTESIAN_POINT('Ctrl Pts',(-1.30856115445774,0.757561799800549,
-3.8539185387629));
#373938=CARTESIAN_POINT('Ctrl Pts',(-1.07151362690525,1.06873333016387,
-3.87396714687104));
#373939=CARTESIAN_POINT('Ctrl Pts',(-0.918975741690193,1.20241353352463,
-3.8850194682775));
#373940=CARTESIAN_POINT('Ctrl Pts',(-0.577067375488448,1.3979545577994,
-3.90690123733498));
#373941=CARTESIAN_POINT('Ctrl Pts',(-0.392491661844923,1.46056490371438,
-3.91752081677356));
#373942=CARTESIAN_POINT('Ctrl Pts',(-0.00872809933920568,1.51248465847023,
-3.93742686519327));
#373943=CARTESIAN_POINT('Ctrl Pts',(0.18685186838331,1.50092573252532,-3.94646419991666));
#373944=CARTESIAN_POINT('Ctrl Pts',(0.566868952789501,1.40285153334342,
-3.96747206372549));
#373945=CARTESIAN_POINT('Ctrl Pts',(0.74717147729129,1.31569795057346,-3.97856780583493));
#373946=CARTESIAN_POINT('Ctrl Pts',(1.05748170470374,1.08081664238639,-4.00002209439531));
#373947=CARTESIAN_POINT('Ctrl Pts',(1.18631966062852,0.937604065057542,
-4.01019894058792));
#373948=CARTESIAN_POINT('Ctrl Pts',(1.3874104900289,0.603815469614292,-4.0291458330574));
#373949=CARTESIAN_POINT('Ctrl Pts',(1.45515371489895,0.414822693444069,
-4.03945429480855));
#373950=CARTESIAN_POINT('Ctrl Pts',(1.51254497872842,0.0242368175648848,
-4.06115351013518));
#373951=CARTESIAN_POINT('Ctrl Pts',(1.50277995913657,-0.173310068174655,
-4.07212833712071));
#373952=CARTESIAN_POINT('Ctrl Pts',(1.40927410874699,-0.547783208284312,
-4.09293240046014));
#373953=CARTESIAN_POINT('Ctrl Pts',(1.3286244643216,-0.721710061443943,
-4.101957360696));
#373954=CARTESIAN_POINT('Ctrl Pts',(1.10150240283646,-1.0374267303463,-4.12165468344362));
#373955=CARTESIAN_POINT('Ctrl Pts',(0.954401438343342,-1.17416356172977,
-4.13253032721384));
#373956=CARTESIAN_POINT('Ctrl Pts',(0.61991370621179,-1.37957069884262,
-4.1543291295381));
#373957=CARTESIAN_POINT('Ctrl Pts',(0.436785632905365,-1.44801250520404,
-4.16504104436089));
#373958=CARTESIAN_POINT('Ctrl Pts',(0.164305308462188,-1.49325512192942,
-4.17940749943655));
#373959=CARTESIAN_POINT('Ctrl Pts',(0.08213376367161,-1.5,-4.18354833745289));
#373960=CARTESIAN_POINT('Ctrl Pts',(1.53039141736487E-14,-1.5,-4.1875));
#373961=CARTESIAN_POINT('Origin',(0.,2.04523456705693E-15,3.99999999999998));
#373962=CARTESIAN_POINT('',(7.56010857688836E-15,-1.5,-4.75));
#373963=CARTESIAN_POINT('',(-7.92750261663254E-15,-1.5,-4.6875));
#373964=CARTESIAN_POINT('',(-1.83697019872103E-16,-1.5,3.99999999999998));
#373965=CARTESIAN_POINT('Ctrl Pts',(1.53039141736488E-14,-1.5,-4.75));
#373966=CARTESIAN_POINT('Ctrl Pts',(0.0979950813416671,-1.5,-4.74528520945068));
#373967=CARTESIAN_POINT('Ctrl Pts',(0.195964627823619,-1.49039890558719,
-4.74030495038083));
#373968=CARTESIAN_POINT('Ctrl Pts',(0.48310212608443,-1.43330761243503,
-4.72490417180033));
#373969=CARTESIAN_POINT('Ctrl Pts',(0.66450478786642,-1.35874230503128,
-4.71410517362704));
#373970=CARTESIAN_POINT('Ctrl Pts',(0.992531086681102,-1.14210808027211,
-4.69230538361246));
#373971=CARTESIAN_POINT('Ctrl Pts',(1.13503121685614,-1.00062738452671,
-4.68151932357652));
#373972=CARTESIAN_POINT('Ctrl Pts',(1.35155687454217,-0.677752945802649,
-4.66213299360489));
#373973=CARTESIAN_POINT('Ctrl Pts',(1.42642341357834,-0.501390609042993,
-4.65285503383571));
#373974=CARTESIAN_POINT('Ctrl Pts',(1.50777006032532,-0.123551390243716,
-4.63186396612464));
#373975=CARTESIAN_POINT('Ctrl Pts',(1.51096921547043,0.0748740853935728,
-4.62084032858923));
#373976=CARTESIAN_POINT('Ctrl Pts',(1.44020051357598,0.464202881123239,
-4.5992109510487));
#373977=CARTESIAN_POINT('Ctrl Pts',(1.36592984409968,0.651051461324218,
-4.58930023411752));
#373978=CARTESIAN_POINT('Ctrl Pts',(1.15290584784697,0.978526060633627,
-4.56995459567167));
#373979=CARTESIAN_POINT('Ctrl Pts',(1.01864650714161,1.11760592881781,-4.55963171045843));
#373980=CARTESIAN_POINT('Ctrl Pts',(0.698992571526539,1.34202256564563,
-4.53801855784309));
#373981=CARTESIAN_POINT('Ctrl Pts',(0.51493865994717,1.42283631721542,-4.52691843346095));
#373982=CARTESIAN_POINT('Ctrl Pts',(0.132294604949322,1.50652034927885,
-4.50618390633501));
#373983=CARTESIAN_POINT('Ctrl Pts',(-0.0620202766589267,1.51104502951983,
-4.49732285442352));
#373984=CARTESIAN_POINT('Ctrl Pts',(-0.442941434862766,1.44615212709081,
-4.47719319603141));
#373985=CARTESIAN_POINT('Ctrl Pts',(-0.625852808074851,1.37689799405716,
-4.46646914256698));
#373986=CARTESIAN_POINT('Ctrl Pts',(-0.959507530504752,1.16999394844625,
-4.44466883764907));
#373987=CARTESIAN_POINT('Ctrl Pts',(-1.10600885552506,1.03262040074767,
-4.43380435748213));
#373988=CARTESIAN_POINT('Ctrl Pts',(-1.33173288654911,0.715948899065067,
-4.41414777437365));
#373989=CARTESIAN_POINT('Ctrl Pts',(-1.41161727845045,0.541705253267488,
-4.40509473629263));
#373990=CARTESIAN_POINT('Ctrl Pts',(-1.50352918131627,0.166783910363671,
-4.38426577279797));
#373991=CARTESIAN_POINT('Ctrl Pts',(-1.51243471580371,-0.0308905016303464,
-4.37328386102053));
#373992=CARTESIAN_POINT('Ctrl Pts',(-1.45329021145476,-0.421308564944836,
-4.35159396861417));
#373993=CARTESIAN_POINT('Ctrl Pts',(-1.38470154651078,-0.610007171654256,
-4.34134350722837));
#373994=CARTESIAN_POINT('Ctrl Pts',(-1.18206653673657,-0.942977568277008,
-4.32234504809104));
#373995=CARTESIAN_POINT('Ctrl Pts',(-1.05251826643873,-1.08566569770916,
-4.31214859487936));
#373996=CARTESIAN_POINT('Ctrl Pts',(-0.740977133552966,-1.31921053196782,
-4.29067220862757));
#373997=CARTESIAN_POINT('Ctrl Pts',(-0.560176122715327,-1.40555085271442,
-4.27957507369487));
#373998=CARTESIAN_POINT('Ctrl Pts',(-0.247304238444433,-1.48468591115563,
-4.26232382207658));
#373999=CARTESIAN_POINT('Ctrl Pts',(-0.123766901248376,-1.5,-4.25595473781271));
#374000=CARTESIAN_POINT('Ctrl Pts',(8.97198981775205E-14,-1.5,-4.25));
#374001=CARTESIAN_POINT('Ctrl Pts',(1.6826817716975E-14,-1.49999999999999,
-4.1875));
#374002=CARTESIAN_POINT('Ctrl Pts',(-0.109787828417629,-1.49999999999999,
-4.19278216935755));
#374003=CARTESIAN_POINT('Ctrl Pts',(-0.219475581345938,-1.4879495279894,
-4.1983942591644));
#374004=CARTESIAN_POINT('Ctrl Pts',(-0.521290520832159,-1.4205088711852,
-4.21478868878879));
#374005=CARTESIAN_POINT('Ctrl Pts',(-0.704899784450703,-1.33891602798461,
-4.22588906147013));
#374006=CARTESIAN_POINT('Ctrl Pts',(-1.02343609181701,-1.11320780716232,
-4.24748431950447));
#374007=CARTESIAN_POINT('Ctrl Pts',(-1.15704329256801,-0.973614691781268,
-4.2577900854861));
#374008=CARTESIAN_POINT('Ctrl Pts',(-1.36881592191344,-0.645056780305522,
-4.27710560951818));
#374009=CARTESIAN_POINT('Ctrl Pts',(-1.44236294662618,-0.457576254107109,
-4.28707909699394));
#374010=CARTESIAN_POINT('Ctrl Pts',(-1.51129595325695,-0.0676933169888792,
-4.30873926016718));
#374011=CARTESIAN_POINT('Ctrl Pts',(-1.50716221617281,0.130620471611318,
-4.31975669286719));
#374012=CARTESIAN_POINT('Ctrl Pts',(-1.42408684985495,0.50798862270464,
-4.34072159015016));
#374013=CARTESIAN_POINT('Ctrl Pts',(-1.34840552196579,0.684001993990453,
-4.34995819779821));
#374014=CARTESIAN_POINT('Ctrl Pts',(-1.13038299794658,1.00587621585134,
-4.36938876198311));
#374015=CARTESIAN_POINT('Ctrl Pts',(-0.987225298387312,1.14669832783564,
-4.38018816534744));
#374016=CARTESIAN_POINT('Ctrl Pts',(-0.658265867242106,1.36176339312966,
-4.40198926294929));
#374017=CARTESIAN_POINT('Ctrl Pts',(-0.476607967494566,1.43546849574518,
-4.41277664668747));
#374018=CARTESIAN_POINT('Ctrl Pts',(-0.0976586420292757,1.50905587449095,
-4.43305294846374));
#374019=CARTESIAN_POINT('Ctrl Pts',(0.0958638183741212,1.50917093989091,
-4.44185750178158));
#374020=CARTESIAN_POINT('Ctrl Pts',(0.480126971699187,1.43502584781182,
-4.46240495725699));
#374021=CARTESIAN_POINT('Ctrl Pts',(0.666548976661914,1.35849973316441,
-4.47349991555954));
#374022=CARTESIAN_POINT('Ctrl Pts',(0.992205866389971,1.14121814093558,
-4.49520368975601));
#374023=CARTESIAN_POINT('Ctrl Pts',(1.12998615066959,1.00498883680653,-4.50561679411108));
#374024=CARTESIAN_POINT('Ctrl Pts',(1.34978962446225,0.683425221208888,
-4.52512441633016));
#374025=CARTESIAN_POINT('Ctrl Pts',(1.42795326901029,0.499971247219071,
-4.53472381959884));
#374026=CARTESIAN_POINT('Ctrl Pts',(1.50860936195778,0.113706312543667,
-4.55618298263636));
#374027=CARTESIAN_POINT('Ctrl Pts',(1.51048440759924,-0.0852488195093594,
-4.5672360455282));
#374028=CARTESIAN_POINT('Ctrl Pts',(1.43851795645481,-0.465599791205705,
-4.58836665506689));
#374029=CARTESIAN_POINT('Ctrl Pts',(1.36803298263095,-0.643871835427663,
-4.59789914452992));
#374030=CARTESIAN_POINT('Ctrl Pts',(1.15957266202618,-0.97207640577981,
-4.61704549000219));
#374031=CARTESIAN_POINT('Ctrl Pts',(1.02065669668349,-1.11703943284086,
-4.62775583825267));
#374032=CARTESIAN_POINT('Ctrl Pts',(0.697770099942208,-1.34203064007821,
-4.64954048263812));
#374033=CARTESIAN_POINT('Ctrl Pts',(0.517806603748821,-1.42120190289142,
-4.66039818213056));
#374034=CARTESIAN_POINT('Ctrl Pts',(0.219906998174013,-1.48790138370002,
-4.6765836469422));
#374035=CARTESIAN_POINT('Ctrl Pts',(0.110007116758885,-1.5,-4.68220728012721));
#374036=CARTESIAN_POINT('Ctrl Pts',(-1.65145674912992E-14,-1.5,-4.6875));
#374037=CARTESIAN_POINT('Origin',(0.,2.04523456705693E-15,3.99999999999998));
#374038=CARTESIAN_POINT('',(-6.2134141793955E-14,-1.5,-5.25000000000001));
#374039=CARTESIAN_POINT('',(-1.00853169777756E-13,-1.5,-5.18750000000001));
#374040=CARTESIAN_POINT('',(-1.83697019872103E-16,-1.5,3.99999999999998));
#374041=CARTESIAN_POINT('Ctrl Pts',(-1.24518451105615E-13,-1.49999999999999,
-5.25000000000001));
#374042=CARTESIAN_POINT('Ctrl Pts',(0.126459591807601,-1.50000000000001,
-5.24391571005236));
#374043=CARTESIAN_POINT('Ctrl Pts',(0.252644307137019,-1.4840124481302,
-5.23740054644236));
#374044=CARTESIAN_POINT('Ctrl Pts',(0.564762610399708,-1.40329255650796,
-5.22014152836333));
#374045=CARTESIAN_POINT('Ctrl Pts',(0.742572157483927,-1.31786453941667,
-5.20921366206577));
#374046=CARTESIAN_POINT('Ctrl Pts',(1.0580845573139,-1.08164511676511,-5.18747191402202));
#374047=CARTESIAN_POINT('Ctrl Pts',(1.19195911089947,-0.932072521810604,
-5.17687607725521));
#374048=CARTESIAN_POINT('Ctrl Pts',(1.38931421438151,-0.596685101977259,
-5.15806450819417));
#374049=CARTESIAN_POINT('Ctrl Pts',(1.45377925744972,-0.415698533628166,
-5.14809436297933));
#374050=CARTESIAN_POINT('Ctrl Pts',(1.51264085248949,-0.0319672768883563,
-5.12677595982711));
#374051=CARTESIAN_POINT('Ctrl Pts',(1.50367803973268,0.167512915529909,
-5.11569372691499));
#374052=CARTESIAN_POINT('Ctrl Pts',(1.40941588211803,0.549347408453337,
-5.09448069953035));
#374053=CARTESIAN_POINT('Ctrl Pts',(1.32589865595609,0.728160736685422,
-5.08523230836436));
#374054=CARTESIAN_POINT('Ctrl Pts',(1.09665318872791,1.04137334491635,-5.06550238045117));
#374055=CARTESIAN_POINT('Ctrl Pts',(0.954011352740898,1.17343566962486,
-5.05497112400887));
#374056=CARTESIAN_POINT('Ctrl Pts',(0.620156428552317,1.38039557202895,
-5.03315963530176));
#374057=CARTESIAN_POINT('Ctrl Pts',(0.430559381159025,1.45076520782745,
-5.02208293100041));
#374058=CARTESIAN_POINT('Ctrl Pts',(0.0441633336528842,1.51145122361622,
-5.00180671983615));
#374059=CARTESIAN_POINT('Ctrl Pts',(-0.148299786727769,1.50480739621165,
-4.99299846196797));
#374060=CARTESIAN_POINT('Ctrl Pts',(-0.52434652523053,1.41881411933161,
-4.97251720269054));
#374061=CARTESIAN_POINT('Ctrl Pts',(-0.70402444441196,1.33877315524592,
-4.96164908465981));
#374062=CARTESIAN_POINT('Ctrl Pts',(-1.02591325372277,1.11221258184287,
-4.93986885283989));
#374063=CARTESIAN_POINT('Ctrl Pts',(-1.16414042313644,0.96660041979913,
-4.92917361277171));
#374064=CARTESIAN_POINT('Ctrl Pts',(-1.37106782256107,0.6373938083197,-4.91007318552835));
#374065=CARTESIAN_POINT('Ctrl Pts',(-1.44072127261361,0.458753032930355,
-4.90048627960722));
#374066=CARTESIAN_POINT('Ctrl Pts',(-1.51089207521126,0.0779298891515337,
-4.87932943828618));
#374067=CARTESIAN_POINT('Ctrl Pts',(-1.50804545052884,-0.121111949225657,
-4.86827155837634));
#374068=CARTESIAN_POINT('Ctrl Pts',(-1.42551074484792,-0.506779807045686,
-4.84684556627523));
#374069=CARTESIAN_POINT('Ctrl Pts',(-1.34660798787456,-0.68959075654184,
-4.83730007489818));
#374070=CARTESIAN_POINT('Ctrl Pts',(-1.12550874088751,-1.01001651653471,
-4.81776171686236));
#374071=CARTESIAN_POINT('Ctrl Pts',(-0.987058116230062,-1.14568753259791,
-4.80733186874265));
#374072=CARTESIAN_POINT('Ctrl Pts',(-0.660264453047603,-1.36157902302987,
-4.78561201544666));
#374073=CARTESIAN_POINT('Ctrl Pts',(-0.473397980327392,-1.43727290020981,
-4.77451879038659));
#374074=CARTESIAN_POINT('Ctrl Pts',(-0.185580428376253,-1.49139155404108,
-4.75916786602213));
#374075=CARTESIAN_POINT('Ctrl Pts',(-0.0927904026472573,-1.5,-4.75446438032889));
#374076=CARTESIAN_POINT('Ctrl Pts',(1.53039141736488E-14,-1.5,-4.75));
#374077=CARTESIAN_POINT('Ctrl Pts',(-1.5671308213393E-14,-1.5,-4.6875));
#374078=CARTESIAN_POINT('Ctrl Pts',(-0.0801408922694299,-1.49999999999999,
-4.69135578047707));
#374079=CARTESIAN_POINT('Ctrl Pts',(-0.160321345391785,-1.49357843265124,
-4.69539184119727));
#374080=CARTESIAN_POINT('Ctrl Pts',(-0.437363833383036,-1.44871509963516,
-4.70996725781039));
#374081=CARTESIAN_POINT('Ctrl Pts',(-0.626538492873636,-1.37749677542739,
-4.72104721464233));
#374082=CARTESIAN_POINT('Ctrl Pts',(-0.959291920697377,-1.16910879918003,
-4.74284537629875));
#374083=CARTESIAN_POINT('Ctrl Pts',(-1.10127676354813,-1.03646702810196,
-4.75336111887653));
#374084=CARTESIAN_POINT('Ctrl Pts',(-1.32923971646631,-0.722111941960987,
-4.77306107728872));
#374085=CARTESIAN_POINT('Ctrl Pts',(-1.41203388153095,-0.542674501574207,
-4.78235141657912));
#374086=CARTESIAN_POINT('Ctrl Pts',(-1.50445922943713,-0.160227643083699,
-4.80359846427304));
#374087=CARTESIAN_POINT('Ctrl Pts',(-1.51245847028538,0.0391957489669181,
-4.81467754160918));
#374088=CARTESIAN_POINT('Ctrl Pts',(-1.45181407158714,0.422476196298371,
-4.83597089979427));
#374089=CARTESIAN_POINT('Ctrl Pts',(-1.38653641547424,0.603090284120421,
-4.84587607683253));
#374090=CARTESIAN_POINT('Ctrl Pts',(-1.18768177155032,0.937517984135334,
-4.86473313368287));
#374091=CARTESIAN_POINT('Ctrl Pts',(-1.05311969738469,1.08648082145367,
-4.87534511108691));
#374092=CARTESIAN_POINT('Ctrl Pts',(-0.736592126888934,1.32120342148533,
-4.89709412314598));
#374093=CARTESIAN_POINT('Ctrl Pts',(-0.558480316497194,1.4057926596232,
-4.90801323267833));
#374094=CARTESIAN_POINT('Ctrl Pts',(-0.184596736411954,1.50072769862936,
-4.92863879922915));
#374095=CARTESIAN_POINT('Ctrl Pts',(0.00716528927516818,1.5120192998048,
-4.93751087070187));
#374096=CARTESIAN_POINT('Ctrl Pts',(0.394973694910186,1.46092392160392,
-4.95758862737863));
#374097=CARTESIAN_POINT('Ctrl Pts',(0.586711051446983,1.39501101129075,
-4.96864450942151));
#374098=CARTESIAN_POINT('Ctrl Pts',(0.926204769872095,1.19557672223827,
-4.99051824992749));
#374099=CARTESIAN_POINT('Ctrl Pts',(1.07222963706745,1.06658270381478,-5.00112704180456));
#374100=CARTESIAN_POINT('Ctrl Pts',(1.30811708788819,0.759328293706288,
-5.02101102679895));
#374101=CARTESIAN_POINT('Ctrl Pts',(1.39536130354334,0.583714614795568,
-5.03007141028904));
#374102=CARTESIAN_POINT('Ctrl Pts',(1.49907896999085,0.205101626873878,
-5.05110546517359));
#374103=CARTESIAN_POINT('Ctrl Pts',(1.51303307166772,0.0054001348051989,
-5.06219999251074));
#374104=CARTESIAN_POINT('Ctrl Pts',(1.46343746122895,-0.380471291437901,
-5.08363729396869));
#374105=CARTESIAN_POINT('Ctrl Pts',(1.40322060533542,-0.563385559529108,
-5.09379919775153));
#374106=CARTESIAN_POINT('Ctrl Pts',(1.21358105044737,-0.90372417817919,
-5.11270689878765));
#374107=CARTESIAN_POINT('Ctrl Pts',(1.0832700197804,-1.05644402571708,-5.12306014758717));
#374108=CARTESIAN_POINT('Ctrl Pts',(0.772940467773571,-1.30035290347364,
-5.14476613172391));
#374109=CARTESIAN_POINT('Ctrl Pts',(0.596738508392062,-1.39005838763646,
-5.15573547145182));
#374110=CARTESIAN_POINT('Ctrl Pts',(0.275187786580223,-1.48101383286055,
-5.17373262791328));
#374111=CARTESIAN_POINT('Ctrl Pts',(0.137809822202473,-1.50000000000001,
-5.18086962183787));
#374112=CARTESIAN_POINT('Ctrl Pts',(-2.00776895109556E-13,-1.49999999999999,
-5.18750000000001));
#374113=CARTESIAN_POINT('Origin',(0.,2.04523456705693E-15,3.99999999999998));
#374114=CARTESIAN_POINT('',(-9.31093641809959E-14,-1.49999999999999,-5.75000000000001));
#374115=CARTESIAN_POINT('',(-3.50308222052939E-14,-1.49999999999999,-5.6875));
#374116=CARTESIAN_POINT('',(-1.83697019872103E-16,-1.5,3.99999999999998));
#374117=CARTESIAN_POINT('Ctrl Pts',(-1.85788884277116E-13,-1.49999999999999,
-5.75000000000001));
#374118=CARTESIAN_POINT('Ctrl Pts',(0.154014098631083,-1.50000000000001,
-5.7425899932247));
#374119=CARTESIAN_POINT('Ctrl Pts',(0.307309583004072,-1.4762855174169,
-5.73455582516667));
#374120=CARTESIAN_POINT('Ctrl Pts',(0.641758139830316,-1.36994648501272,
-5.71551079946263));
#374121=CARTESIAN_POINT('Ctrl Pts',(0.815495357558683,-1.274194834344,-5.70449209560319));
#374122=CARTESIAN_POINT('Ctrl Pts',(1.11839551347547,-1.01929042407315,
-5.68283812699377));
#374123=CARTESIAN_POINT('Ctrl Pts',(1.24380131179792,-0.861793831632132,
-5.67287743509064));
#374124=CARTESIAN_POINT('Ctrl Pts',(1.42213916078022,-0.514004943539909,
-5.65355583019663));
#374125=CARTESIAN_POINT('Ctrl Pts',(1.47607154328307,-0.328438783103053,
-5.64324659906125));
#374126=CARTESIAN_POINT('Ctrl Pts',(1.51193448137251,0.0603413622924671,
-5.62164770209483));
#374127=CARTESIAN_POINT('Ctrl Pts',(1.49061052871905,0.26014748319706,-5.61054736204458));
#374128=CARTESIAN_POINT('Ctrl Pts',(1.37309306628448,0.633855035717469,
-5.589785831349));
#374129=CARTESIAN_POINT('Ctrl Pts',(1.28038394458198,0.804842593549846,
-5.58091242921279));
#374130=CARTESIAN_POINT('Ctrl Pts',(1.03467992929997,1.10316165015626,-5.5608043488045));
#374131=CARTESIAN_POINT('Ctrl Pts',(0.883723504268778,1.22741493681494,
-5.5500899742339));
#374132=CARTESIAN_POINT('Ctrl Pts',(0.538414130864237,1.41409054620938,
-5.52829083566554));
#374133=CARTESIAN_POINT('Ctrl Pts',(0.346395106010818,1.47294668593921,
-5.51741742325455));
#374134=CARTESIAN_POINT('Ctrl Pts',(-0.0406105562722997,1.51144182268113,
-5.49772829529252));
#374135=CARTESIAN_POINT('Ctrl Pts',(-0.231538528745554,1.49415771958094,
-5.48869781177453));
#374136=CARTESIAN_POINT('Ctrl Pts',(-0.602512606107136,1.38757672171473,
-5.46788872988154));
#374137=CARTESIAN_POINT('Ctrl Pts',(-0.778411779409511,1.2970973463507,
-5.45691246097785));
#374138=CARTESIAN_POINT('Ctrl Pts',(-1.08776831186437,1.05181315973582,
-5.43521508824229));
#374139=CARTESIAN_POINT('Ctrl Pts',(-1.21743313452807,0.898531461080216,
-5.42491841450443));
#374140=CARTESIAN_POINT('Ctrl Pts',(-1.40565955761461,0.557300116317758,
-5.40596111757318));
#374141=CARTESIAN_POINT('Ctrl Pts',(-1.46510361883548,0.374045587193807,
-5.39578031039963));
#374142=CARTESIAN_POINT('Ctrl Pts',(-1.51300517467058,-0.0122122812649184,
-5.3743215399297));
#374143=CARTESIAN_POINT('Ctrl Pts',(-1.49813931299167,-0.211941038534931,
-5.36322549785915));
#374144=CARTESIAN_POINT('Ctrl Pts',(-1.39270451515173,-0.589956695012463,
-5.34222462805484));
#374145=CARTESIAN_POINT('Ctrl Pts',(-1.30478227037473,-0.764991809558107,
-5.33319326043181));
#374146=CARTESIAN_POINT('Ctrl Pts',(-1.06768136212527,-1.07115012178327,
-5.31328134010309));
#374147=CARTESIAN_POINT('Ctrl Pts',(-0.921042220249182,-1.19957139300912,
-5.30265890356605));
#374148=CARTESIAN_POINT('Ctrl Pts',(-0.58053074595446,-1.39760743819024,
-5.2807750363655));
#374149=CARTESIAN_POINT('Ctrl Pts',(-0.388411166202108,-1.46269511984064,
-5.26972368761799));
#374150=CARTESIAN_POINT('Ctrl Pts',(-0.126300182789163,-1.49601611959712,
-5.25618728372217));
#374151=CARTESIAN_POINT('Ctrl Pts',(-0.0631212183253676,-1.49999999999999,
-5.25303692103264));
#374152=CARTESIAN_POINT('Ctrl Pts',(-1.24084586568038E-13,-1.49999999999999,
-5.25000000000001));
#374153=CARTESIAN_POINT('Ctrl Pts',(-2.0152264253564E-13,-1.5,-5.18750000000001));
#374154=CARTESIAN_POINT('Ctrl Pts',(-0.0515794141709448,-1.49999999999999,
-5.18998161572135));
#374155=CARTESIAN_POINT('Ctrl Pts',(-0.103212185204464,-1.49733974540289,
-5.1925396945369));
#374156=CARTESIAN_POINT('Ctrl Pts',(-0.352539087313576,-1.47148866811489,
-5.20525352618786));
#374157=CARTESIAN_POINT('Ctrl Pts',(-0.5443141847556,-1.41183053316366,
-5.21613748028084));
#374158=CARTESIAN_POINT('Ctrl Pts',(-0.888775620428316,-1.22374931416049,
-5.23793486713741));
#374159=CARTESIAN_POINT('Ctrl Pts',(-1.03915996200753,-1.09892897471503,
-5.2486374687964));
#374160=CARTESIAN_POINT('Ctrl Pts',(-1.28371590709219,-0.799556796655997,
-5.26871956602526));
#374161=CARTESIAN_POINT('Ctrl Pts',(-1.37578798701838,-0.628034648928745,
-5.27760918617054));
#374162=CARTESIAN_POINT('Ctrl Pts',(-1.49170226899784,-0.253745006143942,
-5.29840305521414));
#374163=CARTESIAN_POINT('Ctrl Pts',(-1.51216527352526,-0.0539375062348138,
-5.30950347187576));
#374164=CARTESIAN_POINT('Ctrl Pts',(-1.47469344897427,0.33452809305927,
-5.33108489405877));
#374165=CARTESIAN_POINT('Ctrl Pts',(-1.42002246298498,0.519796028805142,
-5.34137755715577));
#374166=CARTESIAN_POINT('Ctrl Pts',(-1.24018233990018,0.867062757702468,
-5.36067015320562));
#374167=CARTESIAN_POINT('Ctrl Pts',(-1.11390065900744,1.02426007244313,
-5.37069243156819));
#374168=CARTESIAN_POINT('Ctrl Pts',(-0.809657539496625,1.27789866355297,
-5.3923758519003));
#374169=CARTESIAN_POINT('Ctrl Pts',(-0.635567058477546,1.37281716149636,
-5.40338840901649));
#374170=CARTESIAN_POINT('Ctrl Pts',(-0.266873761100909,1.48823898832821,
-5.42433333541366));
#374171=CARTESIAN_POINT('Ctrl Pts',(-0.0765198328215434,1.51003416255151,
-5.43353971108922));
#374172=CARTESIAN_POINT('Ctrl Pts',(0.311151008931872,1.48078997964258,
-5.45300387157364));
#374173=CARTESIAN_POINT('Ctrl Pts',(0.504498514843458,1.42653902888245,
-5.46381327864352));
#374174=CARTESIAN_POINT('Ctrl Pts',(0.854545493613196,1.24797427576227,
-5.48561505379311));
#374175=CARTESIAN_POINT('Ctrl Pts',(1.00873294315632,1.12701258997474,-5.4963934477455));
#374176=CARTESIAN_POINT('Ctrl Pts',(1.26097329689781,0.8347311900718,-5.51664829519834));
#374177=CARTESIAN_POINT('Ctrl Pts',(1.35730195217515,0.666754413238933,
-5.52545808815331));
#374178=CARTESIAN_POINT('Ctrl Pts',(1.48389311483301,0.296400750530683,
-5.54603329163711));
#374179=CARTESIAN_POINT('Ctrl Pts',(1.51011101383677,0.0966705802162286,
-5.55712941221014));
#374180=CARTESIAN_POINT('Ctrl Pts',(1.48341672623158,-0.293771154987738,
-5.57882061972147));
#374181=CARTESIAN_POINT('Ctrl Pts',(1.43370508323016,-0.48097460288667,
-5.58922081127141));
#374182=CARTESIAN_POINT('Ctrl Pts',(1.26387722187823,-0.831687904208848,
-5.60870488356709));
#374183=CARTESIAN_POINT('Ctrl Pts',(1.14337324878343,-0.990862750387745,
-5.61834672754103));
#374184=CARTESIAN_POINT('Ctrl Pts',(0.848073356367948,-1.25282640619913,
-5.63983111845616));
#374185=CARTESIAN_POINT('Ctrl Pts',(0.676399536691874,-1.35325001025456,
-5.65088032351349));
#374186=CARTESIAN_POINT('Ctrl Pts',(0.332360099323595,-1.47222341002712,
-5.67073774532188));
#374187=CARTESIAN_POINT('Ctrl Pts',(0.166678078102972,-1.5,-5.67948069722827));
#374188=CARTESIAN_POINT('Ctrl Pts',(-7.03603841856193E-14,-1.49999999999999,
-5.6875));
#374189=CARTESIAN_POINT('Origin',(0.,2.04523456705693E-15,3.99999999999998));
#374190=CARTESIAN_POINT('',(1.6836001146047E-16,-1.49999999999999,-6.25));
#374191=CARTESIAN_POINT('',(8.96943871370729E-16,-1.49999999999999,-6.1875));
#374192=CARTESIAN_POINT('',(-1.83697019872103E-16,-1.5,3.99999999999998));
#374193=CARTESIAN_POINT('Ctrl Pts',(-3.46944695195361E-16,-1.49999999999999,
-6.25));
#374194=CARTESIAN_POINT('Ctrl Pts',(0.184225546784952,-1.49999999999999,
-6.24113644424768));
#374195=CARTESIAN_POINT('Ctrl Pts',(0.366990843976295,-1.46606186050117,
-6.23140041868945));
#374196=CARTESIAN_POINT('Ctrl Pts',(0.723575025607657,-1.32872633861587,
-6.21042937864373));
#374197=CARTESIAN_POINT('Ctrl Pts',(0.892193681677509,-1.22191184689028,
-6.19934964055644));
#374198=CARTESIAN_POINT('Ctrl Pts',(1.17689583931665,-0.950384706872383,
-6.1781094810544));
#374199=CARTESIAN_POINT('Ctrl Pts',(1.29071292993964,-0.788900396449992,
-6.16882779980274));
#374200=CARTESIAN_POINT('Ctrl Pts',(1.44864026327719,-0.434191587073927,
-6.1491217548374));
#374201=CARTESIAN_POINT('Ctrl Pts',(1.49235076568262,-0.244851310904274,
-6.13860285060576));
#374202=CARTESIAN_POINT('Ctrl Pts',(1.50608106375903,0.147564878348468,
-6.11680195120283));
#374203=CARTESIAN_POINT('Ctrl Pts',(1.4729787888214,0.346992580603692,-6.10572263441087));
#374204=CARTESIAN_POINT('Ctrl Pts',(1.33371884038559,0.712504109963185,
-6.08541643833535));
#374205=CARTESIAN_POINT('Ctrl Pts',(1.23229372293241,0.876312040285589,
-6.07661342493556));
#374206=CARTESIAN_POINT('Ctrl Pts',(0.970814115657846,1.15994198807361,
-6.05615437180415));
#374207=CARTESIAN_POINT('Ctrl Pts',(0.812144175300407,1.27607139308219,
-6.04529454393355));
#374208=CARTESIAN_POINT('Ctrl Pts',(0.455677918591778,1.4428701772103,-6.02351075360213));
#374209=CARTESIAN_POINT('Ctrl Pts',(0.260633800603809,1.49050693322332,
-6.01280344587753));
#374210=CARTESIAN_POINT('Ctrl Pts',(-0.127850612998576,1.50656622384496,
-5.99366638940726));
#374211=CARTESIAN_POINT('Ctrl Pts',(-0.317461551819455,1.47828890900868,
-5.98412303810574));
#374212=CARTESIAN_POINT('Ctrl Pts',(-0.682739682995172,1.35007577555382,
-5.96298710989615));
#374213=CARTESIAN_POINT('Ctrl Pts',(-0.854019612196042,1.24879521492711,
-5.95193305155395));
#374214=CARTESIAN_POINT('Ctrl Pts',(-1.14791226642593,0.985543370965803,
-5.93048058341343));
#374215=CARTESIAN_POINT('Ctrl Pts',(-1.26751861985257,0.826060200022174,
-5.92089223333453));
#374216=CARTESIAN_POINT('Ctrl Pts',(-1.43576888205435,0.474810965013767,
-5.90137838694517));
#374217=CARTESIAN_POINT('Ctrl Pts',(-1.48469141456904,0.287313872985764,
-5.89096188183251));
#374218=CARTESIAN_POINT('Ctrl Pts',(-1.50967624051698,-0.10341320537901,
-5.86925482192336));
#374219=CARTESIAN_POINT('Ctrl Pts',(-1.48254819423185,-0.303116494536361,
-5.85816019474795));
#374220=CARTESIAN_POINT('Ctrl Pts',(-1.35427630041851,-0.672838245320214,
-5.83762009748218));
#374221=CARTESIAN_POINT('Ctrl Pts',(-1.25727455558041,-0.840259727840265,
-5.82881676893021));
#374222=CARTESIAN_POINT('Ctrl Pts',(-1.00381612065346,-1.13140836976017,
-5.80853478201853));
#374223=CARTESIAN_POINT('Ctrl Pts',(-0.849031785362385,-1.25174491652487,
-5.79774503536007));
#374224=CARTESIAN_POINT('Ctrl Pts',(-0.498119450944072,-1.42877830793129,
-5.77594416359281));
#374225=CARTESIAN_POINT('Ctrl Pts',(-0.304535941796269,-1.48216403035491,
-5.76514743593239));
#374226=CARTESIAN_POINT('Ctrl Pts',(-0.0707802209747663,-1.49874880089135,
-5.75344017050019));
#374227=CARTESIAN_POINT('Ctrl Pts',(-0.0353728198106626,-1.49999999999999,
-5.75170187558664));
#374228=CARTESIAN_POINT('Ctrl Pts',(-1.8603503134212E-13,-1.49999999999999,
-5.75000000000001));
#374229=CARTESIAN_POINT('Ctrl Pts',(-6.98779473907157E-14,-1.49999999999999,
-5.6875));
#374230=CARTESIAN_POINT('Ctrl Pts',(-0.0229199955894006,-1.49999999999999,
-5.68860273880195));
#374231=CARTESIAN_POINT('Ctrl Pts',(-0.0458574412197106,-1.49947467953825,
-5.68972090940436));
#374232=CARTESIAN_POINT('Ctrl Pts',(-0.267439001380728,-1.48930157366741,
-5.70066434346242));
#374233=CARTESIAN_POINT('Ctrl Pts',(-0.462268677088592,-1.44077292807513,
-5.71138610853854));
#374234=CARTESIAN_POINT('Ctrl Pts',(-0.817895460871673,-1.27237960162864,
-5.73317380255219));
#374235=CARTESIAN_POINT('Ctrl Pts',(-0.975971679508033,-1.15559144028853,
-5.74402336376015));
#374236=CARTESIAN_POINT('Ctrl Pts',(-1.23621500950152,-0.870795301504995,
-5.76445533066746));
#374237=CARTESIAN_POINT('Ctrl Pts',(-1.3369586063428,-0.706435810274456,
-5.7732535660958));
#374238=CARTESIAN_POINT('Ctrl Pts',(-1.47453372400099,-0.340269498138311,
-5.79359613899225));
#374239=CARTESIAN_POINT('Ctrl Pts',(-1.50671739912168,-0.140788233463958,
-5.80467843147416));
#374240=CARTESIAN_POINT('Ctrl Pts',(-1.49125281491075,0.251388985978111,
-5.8264660547765));
#374241=CARTESIAN_POINT('Ctrl Pts',(-1.44673726812926,0.440455366519274,
-5.83696974258434));
#374242=CARTESIAN_POINT('Ctrl Pts',(-1.28722595845462,0.79463863076866,
-5.8566465905982));
#374243=CARTESIAN_POINT('Ctrl Pts',(-1.1725299540558,0.955817438983461,
-5.86597044403223));
#374244=CARTESIAN_POINT('Ctrl Pts',(-0.886419821865895,1.22609190056284,
-5.88724354811813));
#374245=CARTESIAN_POINT('Ctrl Pts',(-0.717383582587183,1.33206570215302,
-5.89832002468317));
#374246=CARTESIAN_POINT('Ctrl Pts',(-0.354747129091054,1.4698244043826,
-5.91959400980432));
#374247=CARTESIAN_POINT('Ctrl Pts',(-0.165626270643064,1.50291400057419,
-5.92945035787782));
#374248=CARTESIAN_POINT('Ctrl Pts',(0.223359368904149,1.49654276868739,
-5.94834241684997));
#374249=CARTESIAN_POINT('Ctrl Pts',(0.419500896834944,1.45379593874528,
-5.95896669245532));
#374250=CARTESIAN_POINT('Ctrl Pts',(0.780426854798376,1.29578325048949,
-5.98072099204473));
#374251=CARTESIAN_POINT('Ctrl Pts',(0.942293426823095,1.18330491199423,
-5.99163319941387));
#374252=CARTESIAN_POINT('Ctrl Pts',(1.21050251090383,0.906071204019553,
-6.01223835132093));
#374253=CARTESIAN_POINT('Ctrl Pts',(1.31563867143019,0.745232081922239,
-6.02109821767093));
#374254=CARTESIAN_POINT('Ctrl Pts',(1.46401492968457,0.383320238168483,
-6.0412044312128));
#374255=CARTESIAN_POINT('Ctrl Pts',(1.50210104752628,0.184253983531882,
-6.05226366758151));
#374256=CARTESIAN_POINT('Ctrl Pts',(1.49780399834789,-0.209327391973654,
-6.07412929955404));
#374257=CARTESIAN_POINT('Ctrl Pts',(1.45848425593042,-0.400093452658332,
-6.08472741403652));
#374258=CARTESIAN_POINT('Ctrl Pts',(1.30913443149913,-0.757615020015232,
-6.10458972333413));
#374259=CARTESIAN_POINT('Ctrl Pts',(1.20001875731217,-0.920747042116454,
-6.11367371067817));
#374260=CARTESIAN_POINT('Ctrl Pts',(0.9229242446361,-1.1989526463398,-6.13473336008587));
#374261=CARTESIAN_POINT('Ctrl Pts',(0.756622398667581,-1.31026458135817,
-6.14582655957554));
#374262=CARTESIAN_POINT('Ctrl Pts',(0.397258326831598,-1.45896173369225,
-6.1672469479969));
#374263=CARTESIAN_POINT('Ctrl Pts',(0.208672976728849,-1.4976191275389,
-6.1773940813799));
#374264=CARTESIAN_POINT('Ctrl Pts',(0.0119181219976294,-1.4999644986125,
-6.18692560293834));
#374265=CARTESIAN_POINT('Ctrl Pts',(0.00595830572275474,-1.49999999999999,
-6.18721333088225));
#374266=CARTESIAN_POINT('Ctrl Pts',(-1.83697019872102E-16,-1.49999999999999,
-6.1875));
#374267=CARTESIAN_POINT('Origin',(0.,2.04523456705693E-15,3.99999999999998));
#374268=CARTESIAN_POINT('',(3.85353309639304E-14,-1.5,-6.75));
#374269=CARTESIAN_POINT('',(9.66138729396351E-14,-1.49999999999999,-6.68749999999999));
#374270=CARTESIAN_POINT('',(-1.83697019872103E-16,-1.5,3.99999999999998));
#374271=CARTESIAN_POINT('Ctrl Pts',(7.72543589477329E-14,-1.49999999999999,
-6.75));
#374272=CARTESIAN_POINT('Ctrl Pts',(0.0232667500201416,-1.49999999999999,
-6.74888057796773));
#374273=CARTESIAN_POINT('Ctrl Pts',(0.0465526615425619,-1.49945866467968,
-6.74774519693496));
#374274=CARTESIAN_POINT('Ctrl Pts',(0.26109336989109,-1.48945893012235,
-6.7371453318875));
#374275=CARTESIAN_POINT('Ctrl Pts',(0.448853229789164,-1.44401059158026,
-6.72684927756784));
#374276=CARTESIAN_POINT('Ctrl Pts',(0.803902279500261,-1.28191306194867,
-6.70526426304256));
#374277=CARTESIAN_POINT('Ctrl Pts',(0.96662140318891,-1.16413583124507,
-6.69416384581213));
#374278=CARTESIAN_POINT('Ctrl Pts',(1.23254250830526,-0.876382347002333,
-6.67337655833688));
#374279=CARTESIAN_POINT('Ctrl Pts',(1.33488958156617,-0.710826583354251,
-6.66449036574186));
#374280=CARTESIAN_POINT('Ctrl Pts',(1.4715727808645,-0.349253418196932,
-6.64440296767756));
#374281=CARTESIAN_POINT('Ctrl Pts',(1.50431998104034,-0.156563169032898,
-6.63369795383511));
#374282=CARTESIAN_POINT('Ctrl Pts',(1.49463806837838,0.235796778059404,
-6.61190017899665));
#374283=CARTESIAN_POINT('Ctrl Pts',(1.4502495785818,0.431669580882313,-6.6010183566176));
#374284=CARTESIAN_POINT('Ctrl Pts',(1.29124981480343,0.786632339865288,
-6.58129820334077));
#374285=CARTESIAN_POINT('Ctrl Pts',(1.18131804850252,0.943724119100809,
-6.57228829891116));
#374286=CARTESIAN_POINT('Ctrl Pts',(0.904432822699591,1.21258683472204,
-6.55149824350625));
#374287=CARTESIAN_POINT('Ctrl Pts',(0.73853881639193,1.32019753175719,-6.54052747837761));
#374288=CARTESIAN_POINT('Ctrl Pts',(0.37199886870174,1.4666851530346,-6.51882321633093));
#374289=CARTESIAN_POINT('Ctrl Pts',(0.174550537027293,1.5030068728719,-6.50848159087472));
#374290=CARTESIAN_POINT('Ctrl Pts',(-0.215025253801735,1.49673036131451,
-6.48956376935605));
#374291=CARTESIAN_POINT('Ctrl Pts',(-0.403523717010473,1.45725170989118,
-6.47939800361023));
#374292=CARTESIAN_POINT('Ctrl Pts',(-0.762392310665629,1.30692900901181,
-6.45795629976771));
#374293=CARTESIAN_POINT('Ctrl Pts',(-0.928274152621032,1.19483005017501,
-6.4468614459578));
#374294=CARTESIAN_POINT('Ctrl Pts',(-1.20402389510064,0.915459286317851,
-6.42583413129097));
#374295=CARTESIAN_POINT('Ctrl Pts',(-1.31231660320128,0.752036143782759,
-6.41677978576566));
#374296=CARTESIAN_POINT('Ctrl Pts',(-1.46014657514565,0.394022007304996,
-6.3968901115169));
#374297=CARTESIAN_POINT('Ctrl Pts',(-1.49868303625013,0.203013542218261,
-6.3862785301232));
#374298=CARTESIAN_POINT('Ctrl Pts',(-1.501301757405,-0.190751443848303,
-6.36440269756394));
#374299=CARTESIAN_POINT('Ctrl Pts',(-1.46233116010113,-0.389741049238268,
-6.35334771948672));
#374300=CARTESIAN_POINT('Ctrl Pts',(-1.31234084291122,-0.751005695645993,
-6.33327746135296));
#374301=CARTESIAN_POINT('Ctrl Pts',(-1.2065431930395,-0.911321883774327,
-6.32440200633597));
#374302=CARTESIAN_POINT('Ctrl Pts',(-0.937135562044617,-1.18740768650955,
-6.30377107557028));
#374303=CARTESIAN_POINT('Ctrl Pts',(-0.774706139362372,-1.2992242782468,
-6.29285016989064));
#374304=CARTESIAN_POINT('Ctrl Pts',(-0.413005804342069,-1.45565358411587,
-6.27110259591178));
#374305=CARTESIAN_POINT('Ctrl Pts',(-0.216681381152124,-1.49752351779781,
-6.26049387898363));
#374306=CARTESIAN_POINT('Ctrl Pts',(-0.0119189402414127,-1.49996449327836,
-6.25057443657752));
#374307=CARTESIAN_POINT('Ctrl Pts',(-0.00595875314440546,-1.49999999999999,
-6.25028669064433));
#374308=CARTESIAN_POINT('Ctrl Pts',(-1.83697019872102E-16,-1.49999999999999,
-6.25));
#374309=CARTESIAN_POINT('Ctrl Pts',(-5.55111512312578E-16,-1.49999999999999,
-6.1875));
#374310=CARTESIAN_POINT('Ctrl Pts',(-0.192662798346109,-1.49999999999999,
-6.19676949320733));
#374311=CARTESIAN_POINT('Ctrl Pts',(-0.383648229024422,-1.46288166459859,
-6.20698934889733));
#374312=CARTESIAN_POINT('Ctrl Pts',(-0.743963998216072,-1.3171361389242,
-6.22837353624962));
#374313=CARTESIAN_POINT('Ctrl Pts',(-0.90934848008717,-1.20889212997927,
-6.23933737886988));
#374314=CARTESIAN_POINT('Ctrl Pts',(-1.18512264087765,-0.938949350636919,
-6.2601039799045));
#374315=CARTESIAN_POINT('Ctrl Pts',(-1.29443917043375,-0.7813825258734,
-6.26908985967365));
#374316=CARTESIAN_POINT('Ctrl Pts',(-1.45200343693213,-0.425734227595574,
-6.28884809846687));
#374317=CARTESIAN_POINT('Ctrl Pts',(-1.49559102134978,-0.229678146345099,
-6.29974010298079));
#374318=CARTESIAN_POINT('Ctrl Pts',(-1.50366469040147,0.162645572469948,
-6.32153586513718));
#374319=CARTESIAN_POINT('Ctrl Pts',(-1.47015674430518,0.355125750711791,
-6.33222920837284));
#374320=CARTESIAN_POINT('Ctrl Pts',(-1.33201695307452,0.716239199926321,
-6.35229106666254));
#374321=CARTESIAN_POINT('Ctrl Pts',(-1.22890179572686,0.881516273384371,
-6.36119433126865));
#374322=CARTESIAN_POINT('Ctrl Pts',(-0.961699964356268,1.16819037229097,
-6.38201325478854));
#374323=CARTESIAN_POINT('Ctrl Pts',(-0.798559586219515,1.28523512905986,
-6.39311359313487));
#374324=CARTESIAN_POINT('Ctrl Pts',(-0.442993303102102,1.44580907279673,
-6.41468117123361));
#374325=CARTESIAN_POINT('Ctrl Pts',(-0.255126968641665,1.49048289525025,
-6.42496083397724));
#374326=CARTESIAN_POINT('Ctrl Pts',(0.135766507784468,1.50715365684147,
-6.44423078184137));
#374327=CARTESIAN_POINT('Ctrl Pts',(0.33518385049537,1.47568001957899,-6.45430209553762));
#374328=CARTESIAN_POINT('Ctrl Pts',(0.706628778545216,1.33761690521872,
-6.47600833448086));
#374329=CARTESIAN_POINT('Ctrl Pts',(0.875449082209859,1.23374816864286,
-6.48701594781064));
#374330=CARTESIAN_POINT('Ctrl Pts',(1.15879866469514,0.971218242450404,
-6.50794110890399));
#374331=CARTESIAN_POINT('Ctrl Pts',(1.27231898273961,0.816863702036046,
-6.51711868322019));
#374332=CARTESIAN_POINT('Ctrl Pts',(1.43961121071636,0.465912722300956,
-6.53661595987214));
#374333=CARTESIAN_POINT('Ctrl Pts',(1.48862412376949,0.27116790750538,-6.54743511624967));
#374334=CARTESIAN_POINT('Ctrl Pts',(1.50763248614143,-0.121271229630326,
-6.56923729053499));
#374335=CARTESIAN_POINT('Ctrl Pts',(1.47931526745495,-0.315120236426917,
-6.58000667980147));
#374336=CARTESIAN_POINT('Ctrl Pts',(1.35107045234328,-0.679324824317332,
-6.60024026801761));
#374337=CARTESIAN_POINT('Ctrl Pts',(1.25312237646632,-0.84649771413236,
-6.60905628027751));
#374338=CARTESIAN_POINT('Ctrl Pts',(0.994597339128767,-1.14041209074646,
-6.62965886017505));
#374339=CARTESIAN_POINT('Ctrl Pts',(0.834363033638614,-1.26237496255653,
-6.64075599434268));
#374340=CARTESIAN_POINT('Ctrl Pts',(0.48241297577243,-1.43320619890963,
-6.66243451151779));
#374341=CARTESIAN_POINT('Ctrl Pts',(0.29532698578952,-1.48310641479776,
-6.67282180751565));
#374342=CARTESIAN_POINT('Ctrl Pts',(0.0692686773756122,-1.49880173726729,
-6.68413402412997));
#374343=CARTESIAN_POINT('Ctrl Pts',(0.0346164231920939,-1.49999999999999,
-6.68583451656264));
#374344=CARTESIAN_POINT('Ctrl Pts',(1.93411442899142E-13,-1.49999999999999,
-6.68749999999999));
#374345=CARTESIAN_POINT('Origin',(0.,2.04523456705693E-15,3.99999999999998));
#374346=CARTESIAN_POINT('',(1.21781241129107E-13,-1.49999999999999,-7.24999999999999));
#374347=CARTESIAN_POINT('',(8.11262617461138E-14,-1.49999999999999,-7.18749999999999));
#374348=CARTESIAN_POINT('',(-1.83697019872103E-16,-1.5,3.99999999999998));
#374349=CARTESIAN_POINT('Ctrl Pts',(2.43746179278087E-13,-1.49999999999999,
-7.24999999999999));
#374350=CARTESIAN_POINT('Ctrl Pts',(0.0505804368405312,-1.49999999999999,
-7.24756644759786));
#374351=CARTESIAN_POINT('Ctrl Pts',(0.101216981078785,-1.49744178419118,
-7.245059134177));
#374352=CARTESIAN_POINT('Ctrl Pts',(0.34323090569452,-1.47283692653746,
-7.2327317655318));
#374353=CARTESIAN_POINT('Ctrl Pts',(0.529191373170625,-1.41668427876357,
-7.2222249425973));
#374354=CARTESIAN_POINT('Ctrl Pts',(0.876424344163527,-1.23365577819351,
-7.20043456347528));
#374355=CARTESIAN_POINT('Ctrl Pts',(1.03298496670605,-1.10588550053493,
-7.18935286263176));
#374356=CARTESIAN_POINT('Ctrl Pts',(1.2810179099327,-0.80342656691991,-7.16901773504191));
#374357=CARTESIAN_POINT('Ctrl Pts',(1.37281774817456,-0.633935948345838,
-7.16021866379694));
#374358=CARTESIAN_POINT('Ctrl Pts',(1.48900331988238,-0.266060519028003,
-7.13978113994595));
#374359=CARTESIAN_POINT('Ctrl Pts',(1.51092916119493,-0.0707302567385103,
-7.12892945870764));
#374360=CARTESIAN_POINT('Ctrl Pts',(1.47857984332832,0.321434519883531,
-7.10714252667309));
#374361=CARTESIAN_POINT('Ctrl Pts',(1.42301176927557,0.514373323390137,
-7.09642370425605));
#374362=CARTESIAN_POINT('Ctrl Pts',(1.24393735982193,0.85947590277909,-7.07725133873445));
#374363=CARTESIAN_POINT('Ctrl Pts',(1.125208310326,1.00995833176182,-7.06774887863388));
#374364=CARTESIAN_POINT('Ctrl Pts',(0.832539360702016,1.26320526018224,
-7.04663320032924));
#374365=CARTESIAN_POINT('Ctrl Pts',(0.659621221770886,1.36151009664086,
-7.03558298258931));
#374366=CARTESIAN_POINT('Ctrl Pts',(0.285019425604324,1.48588424625999,
-7.01410510777858));
#374367=CARTESIAN_POINT('Ctrl Pts',(0.0869552392775818,1.51046555989123,
-7.00447434589729));
#374368=CARTESIAN_POINT('Ctrl Pts',(-0.301619063180882,1.48184988803323,
-6.98498417627974));
#374369=CARTESIAN_POINT('Ctrl Pts',(-0.488569448527852,1.4311299529593,
-6.97458063458559));
#374370=CARTESIAN_POINT('Ctrl Pts',(-0.839925423151456,1.25869501755417,
-6.95288615305792));
#374371=CARTESIAN_POINT('Ctrl Pts',(-0.999690372362026,1.13596602621689,
-6.94179031970685));
#374372=CARTESIAN_POINT('Ctrl Pts',(-1.2568468840452,0.840924871256338,
-6.92122228363205));
#374373=CARTESIAN_POINT('Ctrl Pts',(-1.35398756602698,0.673450998433365,
-6.91241394435736));
#374374=CARTESIAN_POINT('Ctrl Pts',(-1.4806657203477,0.308763861472977,
-6.89215354785956));
#374375=CARTESIAN_POINT('Ctrl Pts',(-1.50815645010109,0.114710740560849,
-6.88137281892));
#374376=CARTESIAN_POINT('Ctrl Pts',(-1.48741533558303,-0.277718535298315,
-6.85957119248338));
#374377=CARTESIAN_POINT('Ctrl Pts',(-1.43754704272193,-0.472241568275601,
-6.84876435731798));
#374378=CARTESIAN_POINT('Ctrl Pts',(-1.2687196939139,-0.82244032610959,
-6.82930887077165));
#374379=CARTESIAN_POINT('Ctrl Pts',(-1.15452830518383,-0.976289341653814,
-6.82009478726942));
#374380=CARTESIAN_POINT('Ctrl Pts',(-0.869973418591145,-1.23762907166495,
-6.79914469696021));
#374381=CARTESIAN_POINT('Ctrl Pts',(-0.700614908967324,-1.34078938616193,
-6.78813086757523));
#374382=CARTESIAN_POINT('Ctrl Pts',(-0.350645763193648,-1.46906016400802,
-6.76772989203613));
#374383=CARTESIAN_POINT('Ctrl Pts',(-0.175911284893246,-1.5,-6.75846353564056));
#374384=CARTESIAN_POINT('Ctrl Pts',(7.79237785408782E-14,-1.5,-6.75));
#374385=CARTESIAN_POINT('Ctrl Pts',(1.91322652165482E-13,-1.49999999999999,
-6.68749999999999));
#374386=CARTESIAN_POINT('Ctrl Pts',(-0.162786381555151,-1.5,-6.69533206343426));
#374387=CARTESIAN_POINT('Ctrl Pts',(-0.324710088578347,-1.47350658779939,
-6.70385854953744));
#374388=CARTESIAN_POINT('Ctrl Pts',(-0.666002058072663,-1.35838692766106,
-6.72347673541294));
#374389=CARTESIAN_POINT('Ctrl Pts',(-0.838378458746723,-1.25932329927725,
-6.7345219663123));
#374390=CARTESIAN_POINT('Ctrl Pts',(-1.12979566663392,-1.00481857195472,
-6.75561235902294));
#374391=CARTESIAN_POINT('Ctrl Pts',(-1.24782220338759,-0.85382075474369,
-6.76506551362534));
#374392=CARTESIAN_POINT('Ctrl Pts',(-1.4253255584943,-0.507928449458877,
-6.78428175280783));
#374393=CARTESIAN_POINT('Ctrl Pts',(-1.48002113080588,-0.314735041226525,
-6.79501471993186));
#374394=CARTESIAN_POINT('Ctrl Pts',(-1.51058643373556,0.0774928425069627,
-6.81680515791705));
#374395=CARTESIAN_POINT('Ctrl Pts',(-1.48780216978478,0.272637047754367,
-6.82764650265302));
#374396=CARTESIAN_POINT('Ctrl Pts',(-1.3700037705473,0.640027882315319,
-6.84805710457308));
#374397=CARTESIAN_POINT('Ctrl Pts',(-1.27739092395359,0.809207407080584,
-6.8568528173796));
#374398=CARTESIAN_POINT('Ctrl Pts',(-1.02796030885468,1.11054098969522,
-6.87722393073875));
#374399=CARTESIAN_POINT('Ctrl Pts',(-0.870900564212917,1.23754669865543,
-6.88830840758607));
#374400=CARTESIAN_POINT('Ctrl Pts',(-0.523018030216007,1.41896393786654,
-6.91008528156273));
#374401=CARTESIAN_POINT('Ctrl Pts',(-0.336896352617723,1.474288258976,-6.92057685164883));
#374402=CARTESIAN_POINT('Ctrl Pts',(0.0498552654747803,1.51195041648126,
-6.94023061859191));
#374403=CARTESIAN_POINT('Ctrl Pts',(0.246926905216432,1.49248780031196,
-6.94958894847998));
#374404=CARTESIAN_POINT('Ctrl Pts',(0.623742977622026,1.37838936499508,
-6.97088792119753));
#374405=CARTESIAN_POINT('Ctrl Pts',(0.799624885290026,1.28437132678396,
-6.98196165559821));
#374406=CARTESIAN_POINT('Ctrl Pts',(1.09925996059572,1.03818943041962,-7.00321624089053));
#374407=CARTESIAN_POINT('Ctrl Pts',(1.22191799893799,0.890551336592612,
-7.01302492574487));
#374408=CARTESIAN_POINT('Ctrl Pts',(1.40967318496998,0.549866213456369,
-7.03195187703022));
#374409=CARTESIAN_POINT('Ctrl Pts',(1.47005016346408,0.358410495614678,
-7.04258830579921));
#374410=CARTESIAN_POINT('Ctrl Pts',(1.51227913759432,-0.0332570310114007,
-7.06434761283399));
#374411=CARTESIAN_POINT('Ctrl Pts',(1.49512817303511,-0.229550342745992,
-7.07525279681925));
#374412=CARTESIAN_POINT('Ctrl Pts',(1.38788135235578,-0.600074744888264,
-7.09583748582715));
#374413=CARTESIAN_POINT('Ctrl Pts',(1.30053724896104,-0.771299092575987,
-7.10468618056224));
#374414=CARTESIAN_POINT('Ctrl Pts',(1.06021787981432,-1.07989970708138,
-7.12482079089309));
#374415=CARTESIAN_POINT('Ctrl Pts',(0.9064637152035,-1.21183833271368,-7.13588325341013));
#374416=CARTESIAN_POINT('Ctrl Pts',(0.562929411680457,-1.40368124708872,
-7.15774052513845));
#374417=CARTESIAN_POINT('Ctrl Pts',(0.377919674176932,-1.46437831282019,
-7.16832783988797));
#374418=CARTESIAN_POINT('Ctrl Pts',(0.124490572931739,-1.49612975091501,
-7.18140293759819));
#374419=CARTESIAN_POINT('Ctrl Pts',(0.0622143729691964,-1.49999999999999,
-7.1845067095849));
#374420=CARTESIAN_POINT('Ctrl Pts',(1.624362205121E-13,-1.49999999999999,
-7.18749999999999));
#374421=CARTESIAN_POINT('Origin',(0.,2.04523456705693E-15,3.99999999999998));
#374422=CARTESIAN_POINT('',(5.62415717769822E-15,-1.49999999999999,-7.75));
#374423=CARTESIAN_POINT('',(1.752254379318E-15,-1.49999999999999,-7.6875));
#374424=CARTESIAN_POINT('',(-1.83697019872103E-16,-1.5,3.99999999999998));
#374425=CARTESIAN_POINT('Ctrl Pts',(1.14320113752685E-14,-1.49999999999999,
-7.75));
#374426=CARTESIAN_POINT('Ctrl Pts',(0.0793911424341125,-1.49999999999999,
-7.7461802918787));
#374427=CARTESIAN_POINT('Ctrl Pts',(0.158826622847581,-1.49369800153929,
-7.74218339503251));
#374428=CARTESIAN_POINT('Ctrl Pts',(0.428724322123408,-1.45040567746368,
-7.72799537136398));
#374429=CARTESIAN_POINT('Ctrl Pts',(0.612130401408451,-1.38302694792622,
-7.71729961088408));
#374430=CARTESIAN_POINT('Ctrl Pts',(0.94769719923993,-1.1795822442898,-7.69550340402815));
#374431=CARTESIAN_POINT('Ctrl Pts',(1.09557798558456,-1.04368206740413,
-7.68461348146432));
#374432=CARTESIAN_POINT('Ctrl Pts',(1.32452628266381,-0.729217625494919,
-7.66486307799885));
#374433=CARTESIAN_POINT('Ctrl Pts',(1.40617678145354,-0.555702613677449,
-7.65587236742646));
#374434=CARTESIAN_POINT('Ctrl Pts',(1.50176023982819,-0.181816780657192,
-7.63510093225867));
#374435=CARTESIAN_POINT('Ctrl Pts',(1.51264482580004,0.0155582913297568,
-7.62413565048162));
#374436=CARTESIAN_POINT('Ctrl Pts',(1.45754056210491,0.406351840753956,
-7.60242489773583));
#374437=CARTESIAN_POINT('Ctrl Pts',(1.39090164260854,0.59572276810637,-7.59203859847834));
#374438=CARTESIAN_POINT('Ctrl Pts',(1.19182946286311,0.930567676884839,
-7.57315948629859));
#374439=CARTESIAN_POINT('Ctrl Pts',(1.06392093210996,1.07445894599363,-7.56300850454596));
#374440=CARTESIAN_POINT('Ctrl Pts',(0.755224267438086,1.31107367371899,
-7.5415836980164));
#374441=CARTESIAN_POINT('Ctrl Pts',(0.575577084393085,1.3992836939761,-7.53049014055174));
#374442=CARTESIAN_POINT('Ctrl Pts',(0.196027137929204,1.49979221781333,
-7.50943713179834));
#374443=CARTESIAN_POINT('Ctrl Pts',(0.000225705107454212,1.51254645028954,
-7.50035937175002));
#374444=CARTESIAN_POINT('Ctrl Pts',(-0.384003545441531,1.46280504294404,
-7.48049142755418));
#374445=CARTESIAN_POINT('Ctrl Pts',(-0.568834589062393,1.40130948299218,
-7.46989052982309));
#374446=CARTESIAN_POINT('Ctrl Pts',(-0.911695294333243,1.20792225401907,
-7.44802276897806));
#374447=CARTESIAN_POINT('Ctrl Pts',(-1.06494436667421,1.07525582562551,
-7.43696439098082));
#374448=CARTESIAN_POINT('Ctrl Pts',(-1.30390007262948,0.765581267101937,
-7.41686555814758));
#374449=CARTESIAN_POINT('Ctrl Pts',(-1.39046161160093,0.594047214686918,
-7.4080026230381));
#374450=CARTESIAN_POINT('Ctrl Pts',(-1.4961212510204,0.223059015381023,
-7.38739216752111));
#374451=CARTESIAN_POINT('Ctrl Pts',(-1.51242162242496,0.0266068244045978,
-7.37647815691131));
#374452=CARTESIAN_POINT('Ctrl Pts',(-1.46844042785702,-0.364946348707522,
-7.35472520284953));
#374453=CARTESIAN_POINT('Ctrl Pts',(-1.40721461990083,-0.556126100840495,
-7.3441041055088));
#374454=CARTESIAN_POINT('Ctrl Pts',(-1.21792271522213,-0.896019815330353,
-7.32522112137048));
#374455=CARTESIAN_POINT('Ctrl Pts',(-1.09456049740161,-1.04315479321923,
-7.31535221111767));
#374456=CARTESIAN_POINT('Ctrl Pts',(-0.79368356374764,-1.28806524540754,
-7.29407319478149));
#374457=CARTESIAN_POINT('Ctrl Pts',(-0.617282604111907,-1.38130777081686,
-7.28299602950365));
#374458=CARTESIAN_POINT('Ctrl Pts',(-0.288744953791062,-1.47908794514549,
-7.26447313847911));
#374459=CARTESIAN_POINT('Ctrl Pts',(-0.144629888666687,-1.49999999999999,
-7.25695850876289));
#374460=CARTESIAN_POINT('Ctrl Pts',(2.4308680068863E-13,-1.49999999999999,
-7.24999999999999));
#374461=CARTESIAN_POINT('Ctrl Pts',(1.61641533491519E-13,-1.5,-7.18749999999999));
#374462=CARTESIAN_POINT('Ctrl Pts',(-0.131622357866343,-1.5,-7.19383268364545));
#374463=CARTESIAN_POINT('Ctrl Pts',(-0.262921317301102,-1.48268039727666,
-7.20063090785231));
#374464=CARTESIAN_POINT('Ctrl Pts',(-0.581813302325864,-1.39668966571048,
-7.21836223706774));
#374465=CARTESIAN_POINT('Ctrl Pts',(-0.760986449107481,-1.30772428277316,
-7.22945396974872));
#374466=CARTESIAN_POINT('Ctrl Pts',(-1.06851918038896,-1.06987201850085,
-7.25085715252211));
#374467=CARTESIAN_POINT('Ctrl Pts',(-1.19575846111547,-0.925497279701485,
-7.26098936468145));
#374468=CARTESIAN_POINT('Ctrl Pts',(-1.3933783893132,-0.589901638636698,
-7.27981945905066));
#374469=CARTESIAN_POINT('Ctrl Pts',(-1.45922347640908,-0.400263072301958,
-7.29026316264993));
#374470=CARTESIAN_POINT('Ctrl Pts',(-1.51268581454927,-0.00932820601693203,
-7.31198176633244));
#374471=CARTESIAN_POINT('Ctrl Pts',(-1.50099855028636,0.187919703858646,
-7.32293998354775));
#374472=CARTESIAN_POINT('Ctrl Pts',(-1.40392453846296,0.56138202670716,
-7.34368789037266));
#374473=CARTESIAN_POINT('Ctrl Pts',(-1.32155358063126,0.734602306409417,
-7.35265567666203));
#374474=CARTESIAN_POINT('Ctrl Pts',(-1.09129230738471,1.04816296412075,
-7.3724441456062));
#374475=CARTESIAN_POINT('Ctrl Pts',(-0.942853330910693,1.1834581959791,
-7.38334412007661));
#374476=CARTESIAN_POINT('Ctrl Pts',(-0.60651714013915,1.38548711548125,
-7.40513801703057));
#374477=CARTESIAN_POINT('Ctrl Pts',(-0.422914749264889,1.45210020630605,
-7.41582195481419));
#374478=CARTESIAN_POINT('Ctrl Pts',(-0.0408496404733512,1.5118368221128,
-7.43586342137066));
#374479=CARTESIAN_POINT('Ctrl Pts',(0.153956628964715,1.50453306863169,
-7.44478132319164));
#374480=CARTESIAN_POINT('Ctrl Pts',(0.535587727485882,1.41515179392173,
-7.46562537116655));
#374481=CARTESIAN_POINT('Ctrl Pts',(0.718181777986944,1.33180900745106,
-7.47672550891929));
#374482=CARTESIAN_POINT('Ctrl Pts',(1.03417691378856,1.10320535164218,-7.49827893352934));
#374483=CARTESIAN_POINT('Ctrl Pts',(1.1663051313683,0.962464837359553,-7.50854541409168));
#374484=CARTESIAN_POINT('Ctrl Pts',(1.37524402475767,0.631462669396288,
-7.52779249595254));
#374485=CARTESIAN_POINT('Ctrl Pts',(1.44714609790656,0.442545202076605,
-7.53791415544024));
#374486=CARTESIAN_POINT('Ctrl Pts',(1.51190998266283,0.05142103028195,-7.5596432760955));
#374487=CARTESIAN_POINT('Ctrl Pts',(1.50566267484778,-0.146623862090228,
-7.57064577011617));
#374488=CARTESIAN_POINT('Ctrl Pts',(1.41867570620449,-0.522916883378641,
-7.59155093796553));
#374489=CARTESIAN_POINT('Ctrl Pts',(1.34114187901499,-0.698143998507512,
-7.60070050344159));
#374490=CARTESIAN_POINT('Ctrl Pts',(1.11972047582304,-1.01773391998754,
-7.62023114348858));
#374491=CARTESIAN_POINT('Ctrl Pts',(0.975078857061156,-1.1570464511819,
-7.6310600091491));
#374492=CARTESIAN_POINT('Ctrl Pts',(0.644025265587001,-1.3685277794625,
-7.65286231383638));
#374493=CARTESIAN_POINT('Ctrl Pts',(0.461801781543798,-1.44027365666263,
-7.66362248633347));
#374494=CARTESIAN_POINT('Ctrl Pts',(0.181365339759811,-1.49177900289783,
-7.67854569499177));
#374495=CARTESIAN_POINT('Ctrl Pts',(0.0906779845837288,-1.49999999999999,
-7.68313725343258));
#374496=CARTESIAN_POINT('Ctrl Pts',(3.68820577850811E-15,-1.49999999999999,
-7.6875));
#374497=CARTESIAN_POINT('Origin',(0.,2.04523456705693E-15,3.99999999999998));
#374498=CARTESIAN_POINT('',(-4.27253208704016E-15,-1.49999999999999,-8.25));
#374499=CARTESIAN_POINT('',(-3.69667736044839E-14,-1.49999999999999,-8.1875));
#374500=CARTESIAN_POINT('',(-1.83697019872103E-16,-1.5,3.99999999999998));
#374501=CARTESIAN_POINT('Ctrl Pts',(-8.11850586757146E-15,-1.49999999999999,
-8.25));
#374502=CARTESIAN_POINT('Ctrl Pts',(0.106980697927961,-1.5,-8.2448528887711));
#374503=CARTESIAN_POINT('Ctrl Pts',(0.213877795545196,-1.48855780985152,
-8.23939196114871));
#374504=CARTESIAN_POINT('Ctrl Pts',(0.509095079291007,-1.42432975528461,
-8.22340420033518));
#374505=CARTESIAN_POINT('Ctrl Pts',(0.689431848522612,-1.34631612532873,
-8.21256069820357));
#374506=CARTESIAN_POINT('Ctrl Pts',(1.01363305676546,-1.12341811902394,
-8.19077094901311));
#374507=CARTESIAN_POINT('Ctrl Pts',(1.15345990845384,-0.979323296244408,
-8.1800408925085));
#374508=CARTESIAN_POINT('Ctrl Pts',(1.36395558444277,-0.652454566336543,
-8.16083372763366));
#374509=CARTESIAN_POINT('Ctrl Pts',(1.43554513383051,-0.474669224619041,
-8.15137051247875));
#374510=CARTESIAN_POINT('Ctrl Pts',(1.50988936886954,-0.0949478172424911,
-8.13027487873561));
#374511=CARTESIAN_POINT('Ctrl Pts',(1.50930086684915,0.103885255945463,
-8.11922859689184));
#374512=CARTESIAN_POINT('Ctrl Pts',(1.43113940933133,0.490935718138837,
-8.09772579343666));
#374513=CARTESIAN_POINT('Ctrl Pts',(1.35395742288841,0.67524459106288,-8.08805217935172));
#374514=CARTESIAN_POINT('Ctrl Pts',(1.13587079804451,0.998311822706801,
-8.06858539195381));
#374515=CARTESIAN_POINT('Ctrl Pts',(0.998980064342097,1.13527418490466,
-8.0581947233967));
#374516=CARTESIAN_POINT('Ctrl Pts',(0.6748347447419,1.35438460105627,-8.03651287398741));
#374517=CARTESIAN_POINT('Ctrl Pts',(0.489005750514352,1.43200713177716,
-8.02541599092512));
#374518=CARTESIAN_POINT('Ctrl Pts',(0.105145394201939,1.50857778172861,
-8.00482053842245));
#374519=CARTESIAN_POINT('Ctrl Pts',(-0.088574936488778,1.5096411960585,
-7.99600624738277));
#374520=CARTESIAN_POINT('Ctrl Pts',(-0.468032439517269,1.43827208746729,
-7.97576711451751));
#374521=CARTESIAN_POINT('Ctrl Pts',(-0.650020674823016,1.36570207352387,
-7.96499536774327));
#374522=CARTESIAN_POINT('Ctrl Pts',(-0.980198636604201,1.15271161612822,
-7.94319327155604));
#374523=CARTESIAN_POINT('Ctrl Pts',(-1.12421838283135,1.01276247139593,
-7.93237664204241));
#374524=CARTESIAN_POINT('Ctrl Pts',(-1.34421180483883,0.692210599243926,
-7.91288798492019));
#374525=CARTESIAN_POINT('Ctrl Pts',(-1.42096690840797,0.516654177373473,
-7.90370300985401));
#374526=CARTESIAN_POINT('Ctrl Pts',(-1.50631278814488,0.139908538316974,
-7.8827726965731));
#374527=CARTESIAN_POINT('Ctrl Pts',(-1.51167357144707,-0.058251900989222,
-7.87176378327831));
#374528=CARTESIAN_POINT('Ctrl Pts',(-1.44515794855276,-0.448857478504078,
-7.85006347341638));
#374529=CARTESIAN_POINT('Ctrl Pts',(-1.372564451948,-0.637170911603667,
-7.84000501266196));
#374530=CARTESIAN_POINT('Ctrl Pts',(-1.16243630201622,-0.967148785610963,
-7.82072916527892));
#374531=CARTESIAN_POINT('Ctrl Pts',(-1.02968703215297,-1.10741027035704,
-7.81044611070068));
#374532=CARTESIAN_POINT('Ctrl Pts',(-0.712623718683101,-1.33480374195274,
-7.78887490959674));
#374533=CARTESIAN_POINT('Ctrl Pts',(-0.529602220340034,-1.41741453994902,
-7.77777453926331));
#374534=CARTESIAN_POINT('Ctrl Pts',(-0.225399412709512,-1.48728797854404,
-7.7611976460073));
#374535=CARTESIAN_POINT('Ctrl Pts',(-0.112761604857976,-1.49999999999999,
-7.75542524524325));
#374536=CARTESIAN_POINT('Ctrl Pts',(1.13797860024079E-14,-1.49999999999999,
-7.75));
#374537=CARTESIAN_POINT('Ctrl Pts',(3.62557206479153E-15,-1.49999999999999,
-7.6875));
#374538=CARTESIAN_POINT('Ctrl Pts',(-0.100589452564642,-1.49999999999999,
-7.69233961229299));
#374539=CARTESIAN_POINT('Ctrl Pts',(-0.201140026213281,-1.48988389579456,
-7.69745835691791));
#374540=CARTESIAN_POINT('Ctrl Pts',(-0.495451818355405,-1.42977698559595,
-7.71328807601389));
#374541=CARTESIAN_POINT('Ctrl Pts',(-0.68084559408579,-1.3513596664345,
-7.72438609707316));
#374542=CARTESIAN_POINT('Ctrl Pts',(-1.00388517650595,-1.1309253649979,
-7.74605152126882));
#374543=CARTESIAN_POINT('Ctrl Pts',(-1.14012647132286,-0.993433368167938,
-7.75642565575609));
#374544=CARTESIAN_POINT('Ctrl Pts',(-1.35696148220815,-0.669272841972499,
-7.77586259414244));
#374545=CARTESIAN_POINT('Ctrl Pts',(-1.43342607099873,-0.484338668640413,
-7.7855922961867));
#374546=CARTESIAN_POINT('Ctrl Pts',(-1.50976492154754,-0.0967196035284116,
-7.80712668869292));
#374547=CARTESIAN_POINT('Ctrl Pts',(-1.50941611595624,0.102019322792505,
-7.81816774015519));
#374548=CARTESIAN_POINT('Ctrl Pts',(-1.43333942566545,0.481278957691876,
-7.83923771987182));
#374549=CARTESIAN_POINT('Ctrl Pts',(-1.36094252496436,0.658710809425312,
-7.84865247805577));
#374550=CARTESIAN_POINT('Ctrl Pts',(-1.14895997271597,0.984599762393011,
-7.86790396427189));
#374551=CARTESIAN_POINT('Ctrl Pts',(-1.008470386414,1.1280558078679,-7.87864816279645));
#374552=CARTESIAN_POINT('Ctrl Pts',(-0.683316256690496,1.34941791257009,
-7.90044109550962));
#374553=CARTESIAN_POINT('Ctrl Pts',(-0.50271108544479,1.42658382171831,
-7.91127396333894));
#374554=CARTESIAN_POINT('Ctrl Pts',(-0.125331847764131,1.50694188021935,
-7.93166279866909));
#374555=CARTESIAN_POINT('Ctrl Pts',(0.0676000990502314,1.51063252236472,
-7.94045706343858));
#374556=CARTESIAN_POINT('Ctrl Pts',(0.453053101091752,1.44385482655744,
-7.96085711564061));
#374557=CARTESIAN_POINT('Ctrl Pts',(0.641237598800616,1.37068394705898,
-7.97194367093858));
#374558=CARTESIAN_POINT('Ctrl Pts',(0.97142244740165,1.15901668018185,-7.9937093431759));
#374559=CARTESIAN_POINT('Ctrl Pts',(1.11187991864011,1.02504781595698,-8.00418846375125));
#374560=CARTESIAN_POINT('Ctrl Pts',(1.33686960467276,0.708053997096517,
-8.0238186689248));
#374561=CARTESIAN_POINT('Ctrl Pts',(1.41798274070534,0.527162031521857,
-8.03321322047106));
#374562=CARTESIAN_POINT('Ctrl Pts',(1.50613608811588,0.143308064344835,
-8.05453844086978));
#374563=CARTESIAN_POINT('Ctrl Pts',(1.5119022342726,-0.0559660969908603,
-8.06560922761065));
#374564=CARTESIAN_POINT('Ctrl Pts',(1.44712806489012,-0.438191225159822,
-8.08684395695337));
#374565=CARTESIAN_POINT('Ctrl Pts',(1.37996060665107,-0.617946335458259,
-8.09660512367491));
#374566=CARTESIAN_POINT('Ctrl Pts',(1.17761874744159,-0.950130047800848,
-8.115567626258));
#374567=CARTESIAN_POINT('Ctrl Pts',(1.04146583313214,-1.09765952383988,
-8.12621632740304));
#374568=CARTESIAN_POINT('Ctrl Pts',(0.722600625896706,-1.32887769876841,
-8.14798046392043));
#374569=CARTESIAN_POINT('Ctrl Pts',(0.54379957003011,-1.41150887834165,
-8.15887834427547));
#374570=CARTESIAN_POINT('Ctrl Pts',(0.237977572203931,-1.48582269186709,
-8.17565648460415));
#374571=CARTESIAN_POINT('Ctrl Pts',(0.119084432358742,-1.5,-8.18177054757678));
#374572=CARTESIAN_POINT('Ctrl Pts',(-7.39339145461315E-14,-1.49999999999999,
-8.1875));
#374573=CARTESIAN_POINT('Origin',(0.,-1.17768352285132E-13,1004.));
#374574=CARTESIAN_POINT('',(2.62566781617011E-12,1.22263611415546,5.22263611415551));
#374575=CARTESIAN_POINT('',(-1.22464679914734E-13,999.999999999989,1004.));
#374576=CARTESIAN_POINT('',(1.16245326511946,-0.172894699616898,5.17524047358083));
#374577=CARTESIAN_POINT('Ctrl Pts',(1.16245326511952,-0.172894699616907,
5.17524047358087));
#374578=CARTESIAN_POINT('Ctrl Pts',(1.19399906804494,-0.0751204590618667,
5.19205905165469));
#374579=CARTESIAN_POINT('Ctrl Pts',(1.21273427617106,0.0263505697178082,
5.20876352342307));
#374580=CARTESIAN_POINT('Ctrl Pts',(1.22403798349754,0.238694528089334,
5.24237097580138));
#374581=CARTESIAN_POINT('Ctrl Pts',(1.21468846965962,0.348742451219363,
5.25905662677932));
#374582=CARTESIAN_POINT('Ctrl Pts',(1.14440902939163,0.659449163520211,
5.30459309397949));
#374583=CARTESIAN_POINT('Ctrl Pts',(1.05176705868767,0.820265983472114,
5.32729141130241));
#374584=CARTESIAN_POINT('Ctrl Pts',(0.868371046406527,1.07627483107919,
5.37112509845121));
#374585=CARTESIAN_POINT('Ctrl Pts',(0.734430946342676,1.20185061729893,
5.39690248949309));
#374586=CARTESIAN_POINT('Ctrl Pts',(0.496444765757832,1.35014966254729,
5.43521886790191));
#374587=CARTESIAN_POINT('Ctrl Pts',(0.407566921813029,1.39321113075102,
5.44830739519754));
#374588=CARTESIAN_POINT('Ctrl Pts',(0.17654814223105,1.47628188585813,5.47964000519515));
#374589=CARTESIAN_POINT('Ctrl Pts',(0.0614240005287953,1.49300777123951,
5.49300777123956));
#374590=CARTESIAN_POINT('Ctrl Pts',(-3.08060338411093E-14,1.49999999999988,
5.49999999999993));
#374591=CARTESIAN_POINT('',(0.943477955795688,0.700742119235096,5.17524047358083));
#374592=CARTESIAN_POINT('Origin',(-2.08166817117217E-15,1.38777878078145E-16,
5.17524047358094));
#374593=CARTESIAN_POINT('Ctrl Pts',(0.943477955795631,0.700742119235054,
5.17524047358087));
#374594=CARTESIAN_POINT('Ctrl Pts',(0.89439950803542,0.772851645360285,
5.17883611947854));
#374595=CARTESIAN_POINT('Ctrl Pts',(0.83757969138554,0.839368825375372,
5.18257660489706));
#374596=CARTESIAN_POINT('Ctrl Pts',(0.712505185698739,0.956945420110407,
5.19008020169398));
#374597=CARTESIAN_POINT('Ctrl Pts',(0.645022284217815,1.00809919656745,
5.19381777605465));
#374598=CARTESIAN_POINT('Ctrl Pts',(0.446868995932777,1.12761359942621,
5.20401348413372));
#374599=CARTESIAN_POINT('Ctrl Pts',(0.308091646309466,1.17965824671919,
5.21034872100051));
#374600=CARTESIAN_POINT('Ctrl Pts',(0.107758738784782,1.21505485062343,
5.21851908836561));
#374601=CARTESIAN_POINT('Ctrl Pts',(0.0531588445461745,1.22064681749215,
5.2206468174922));
#374602=CARTESIAN_POINT('Ctrl Pts',(5.25148536208059E-12,1.22263611415546,
5.22263611415551));
#374603=CARTESIAN_POINT('Origin',(0.,1.84795814293585E-15,-9.));
#374604=CARTESIAN_POINT('',(-1.41298094714294,2.50437193139947E-10,-8.76225952643789));
#374605=CARTESIAN_POINT('',(-1.17524047358083,1.70403269451593E-15,-9.));
#374606=CARTESIAN_POINT('',(-1.17524047358083,1.70403269451593E-15,-9.));
#374607=CARTESIAN_POINT('Ctrl Pts',(-1.41298094714294,5.0087271136201E-10,
-8.76225952643789));
#374608=CARTESIAN_POINT('Ctrl Pts',(-1.40661633259335,0.170222827651176,
-8.76862414092715));
#374609=CARTESIAN_POINT('Ctrl Pts',(-1.36949767217021,0.337954367729962,
-8.77498443124136));
#374610=CARTESIAN_POINT('Ctrl Pts',(-1.25144210016968,0.618423802974436,
-8.78575720460891));
#374611=CARTESIAN_POINT('Ctrl Pts',(-1.16041076134757,0.786810302099258,
-8.79168857309288));
#374612=CARTESIAN_POINT('Ctrl Pts',(-0.870331100473633,1.07132672691966,
-8.80664103487819));
#374613=CARTESIAN_POINT('Ctrl Pts',(-0.718622501884707,1.17036468694909,
-8.81361329796119));
#374614=CARTESIAN_POINT('Ctrl Pts',(-0.397528466238866,1.29897691831306,
-8.82702012864551));
#374615=CARTESIAN_POINT('Ctrl Pts',(-0.232920329340296,1.33196165968486,
-8.83334360207825));
#374616=CARTESIAN_POINT('Ctrl Pts',(0.154659368267121,1.33761280872929,
-8.84697406884231));
#374617=CARTESIAN_POINT('Ctrl Pts',(0.32663216391228,1.28673458420506,-8.85349457293248));
#374618=CARTESIAN_POINT('Ctrl Pts',(0.596915603944153,1.17829870466726,
-8.86497740055058));
#374619=CARTESIAN_POINT('Ctrl Pts',(0.738687100801235,1.08684240050756,
-8.87179108117765));
#374620=CARTESIAN_POINT('Ctrl Pts',(0.983024626099762,0.852598849977181,
-8.88529312369776));
#374621=CARTESIAN_POINT('Ctrl Pts',(1.08299149273678,0.710087044469093,
-8.89149869999885));
#374622=CARTESIAN_POINT('Ctrl Pts',(1.21210093543402,0.413830143095868,
-8.90353581540508));
#374623=CARTESIAN_POINT('Ctrl Pts',(1.24700885086701,0.264141347306251,
-8.90969437811077));
#374624=CARTESIAN_POINT('Ctrl Pts',(1.26190809160109,-0.0512728550184668,
-8.92287899600932));
#374625=CARTESIAN_POINT('Ctrl Pts',(1.23765032069058,-0.2143650511596,-8.92981109575828));
#374626=CARTESIAN_POINT('Ctrl Pts',(1.1437214259834,-0.477800630596949,
-8.94119025592916));
#374627=CARTESIAN_POINT('Ctrl Pts',(1.07131936092985,-0.633771724466625,
-8.94724597180567));
#374628=CARTESIAN_POINT('Ctrl Pts',(0.833879668056824,-0.894264904214086,
-8.96158207726312));
#374629=CARTESIAN_POINT('Ctrl Pts',(0.714102016460339,-0.98463286044948,
-8.96802984706955));
#374630=CARTESIAN_POINT('Ctrl Pts',(0.493798039929723,-1.09406106811124,
-8.97884116477498));
#374631=CARTESIAN_POINT('Ctrl Pts',(0.401788558101966,-1.1265752151692,
-8.98311244451451));
#374632=CARTESIAN_POINT('Ctrl Pts',(0.20619495746093,-1.16997545830358,
-8.99170978455801));
#374633=CARTESIAN_POINT('Ctrl Pts',(0.103058272401581,-1.17925262541455,
-8.99598784816628));
#374634=CARTESIAN_POINT('Ctrl Pts',(-1.21430643318376E-16,-1.17524047358083,
-9.));
#374635=CARTESIAN_POINT('Origin',(0.,1.84795814293585E-15,-9.));
#374636=CARTESIAN_POINT('Origin',(0.,1.84795814293585E-15,-9.));
#374637=CARTESIAN_POINT('Origin',(0.,1.84795814293585E-15,-9.));
#374638=CARTESIAN_POINT('',(1.20419349529493,-0.894381364905022,-8.67524047358084));
#374639=CARTESIAN_POINT('Ctrl Pts',(1.20419349529493,-0.894381364905017,
-8.67524047358084));
#374640=CARTESIAN_POINT('Ctrl Pts',(1.13095118605837,-0.9716143545478,-8.68798858402793));
#374641=CARTESIAN_POINT('Ctrl Pts',(1.04930823985346,-1.04028664032772,
-8.70142161163385));
#374642=CARTESIAN_POINT('Ctrl Pts',(0.878046559880868,-1.15411572512553,
-8.72843423103745));
#374643=CARTESIAN_POINT('Ctrl Pts',(0.789772643293612,-1.20019602678898,
-8.74187275401195));
#374644=CARTESIAN_POINT('Ctrl Pts',(0.529623955243905,-1.30275449886039,
-8.78033713619089));
#374645=CARTESIAN_POINT('Ctrl Pts',(0.350730680924542,-1.33604442248835,
-8.8055512491075));
#374646=CARTESIAN_POINT('Ctrl Pts',(0.0206766763463416,-1.33358695022529,
-8.8497597206349));
#374647=CARTESIAN_POINT('Ctrl Pts',(-0.151348172730456,-1.30940596959337,
-8.87093339811554));
#374648=CARTESIAN_POINT('Ctrl Pts',(-0.428302486918901,-1.1896603066116,
-8.91545734281534));
#374649=CARTESIAN_POINT('Ctrl Pts',(-0.522196352027943,-1.13301202682058,
-8.93233880671145));
#374650=CARTESIAN_POINT('Ctrl Pts',(-0.688752455704374,-0.998922351205504,
-8.9663014666125));
#374651=CARTESIAN_POINT('Ctrl Pts',(-0.761425017394258,-0.922956233174634,
-8.98321102010998));
#374652=CARTESIAN_POINT('Ctrl Pts',(-0.82340787416506,-0.838564036615864,
-8.99999999999999));
#374653=CARTESIAN_POINT('',(0.243337884005315,-1.48013062741361,-8.67524047358084));
#374654=CARTESIAN_POINT('Origin',(0.,1.84795814293585E-15,-8.67524047358084));
#374655=CARTESIAN_POINT('Ctrl Pts',(0.243337884005315,-1.48013062741361,
-8.67524047358084));
#374656=CARTESIAN_POINT('Ctrl Pts',(0.101094102340477,-1.4987275388269,
-8.67996543537092));
#374657=CARTESIAN_POINT('Ctrl Pts',(-0.0426671899127046,-1.49755833949873,
-8.68419131194465));
#374658=CARTESIAN_POINT('Ctrl Pts',(-0.318529374136382,-1.45339200249797,
-8.69334244704395));
#374659=CARTESIAN_POINT('Ctrl Pts',(-0.446787711019286,-1.41439763313783,
-8.69795944692342));
#374660=CARTESIAN_POINT('Ctrl Pts',(-0.738263562285435,-1.28017117867732,
-8.70937165618806));
#374661=CARTESIAN_POINT('Ctrl Pts',(-0.891914693261224,-1.16979592346254,
-8.7161885798986));
#374662=CARTESIAN_POINT('Ctrl Pts',(-1.13959614737799,-0.907361178122547,
-8.728880211953));
#374663=CARTESIAN_POINT('Ctrl Pts',(-1.24531907020817,-0.750705326305741,
-8.73469659578812));
#374664=CARTESIAN_POINT('Ctrl Pts',(-1.38528494839894,-0.392021122233477,
-8.74772314591134));
#374665=CARTESIAN_POINT('Ctrl Pts',(-1.41799325611942,-0.206165197918358,
-8.75455854148613));
#374666=CARTESIAN_POINT('Ctrl Pts',(-1.41341885699457,-0.0128948780533315,
-8.76177751154181));
#374667=CARTESIAN_POINT('Ctrl Pts',(-1.41322194947896,-0.006445652832508,
-8.76201852410416));
#374668=CARTESIAN_POINT('Ctrl Pts',(-1.41298094714294,5.00872780991692E-10,
-8.76225952643789));
#374669=CARTESIAN_POINT('Origin',(0.,-1.17768352285132E-13,1004.));
#374670=CARTESIAN_POINT('Ctrl Pts',(5.25317636612677E-12,1.22263611415552,
5.22263611415548));
#374671=CARTESIAN_POINT('Ctrl Pts',(-0.115296684347476,1.2269507171431,
5.22695071714306));
#374672=CARTESIAN_POINT('Ctrl Pts',(-0.223766436349468,1.2148855018304,
5.23131700863417));
#374673=CARTESIAN_POINT('Ctrl Pts',(-0.478278179729571,1.15760022383143,
5.24208637023804));
#374674=CARTESIAN_POINT('Ctrl Pts',(-0.627381439373727,1.09194410272621,
5.24897616624381));
#374675=CARTESIAN_POINT('Ctrl Pts',(-0.883573773271131,0.913573132610325,
5.26199412924211));
#374676=CARTESIAN_POINT('Ctrl Pts',(-0.990681696781001,0.805713791835157,
5.26803702740709));
#374677=CARTESIAN_POINT('Ctrl Pts',(-1.15952482909877,0.559571469320968,
5.27899700986098));
#374678=CARTESIAN_POINT('Ctrl Pts',(-1.23606073166015,0.401676792848018,
5.28542047422328));
#374679=CARTESIAN_POINT('Ctrl Pts',(-1.30927486236648,0.0515901063597925,
5.29982019456112));
#374680=CARTESIAN_POINT('Ctrl Pts',(-1.3119373462125,-0.115337847574361,
5.3065789426825));
#374681=CARTESIAN_POINT('Ctrl Pts',(-1.25338969407816,-0.447917213019407,
5.31984699526509));
#374682=CARTESIAN_POINT('Ctrl Pts',(-1.19047975461417,-0.608427371489105,
5.3257816690615));
#374683=CARTESIAN_POINT('Ctrl Pts',(-1.00849050415241,-0.89486065873855,
5.3379211316854));
#374684=CARTESIAN_POINT('Ctrl Pts',(-0.893778927178617,-1.01791957302403,
5.34432830437151));
#374685=CARTESIAN_POINT('Ctrl Pts',(-0.614965052842258,-1.22385703407752,
5.35783782669075));
#374686=CARTESIAN_POINT('Ctrl Pts',(-0.450478262988456,-1.30080821357337,
5.36482096360993));
#374687=CARTESIAN_POINT('Ctrl Pts',(-0.0535197887087344,-1.39752886138873,
5.3797460760767));
#374688=CARTESIAN_POINT('Ctrl Pts',(0.138282520270641,-1.38497571780285,
5.38572569203872));
#374689=CARTESIAN_POINT('Ctrl Pts',(0.442514830477669,-1.3366523083962,
5.39679114172506));
#374690=CARTESIAN_POINT('Ctrl Pts',(0.610880602891162,-1.27592998523196,
5.40347638258105));
#374691=CARTESIAN_POINT('Ctrl Pts',(0.923558005877193,-1.0907204668723,
5.41706648777078));
#374692=CARTESIAN_POINT('Ctrl Pts',(1.06322528601953,-0.965103528812707,
5.42383292975859));
#374693=CARTESIAN_POINT('Ctrl Pts',(1.28282155738663,-0.670543286431297,
5.43610666219767));
#374694=CARTESIAN_POINT('Ctrl Pts',(1.36291448343688,-0.5044383426778,5.44192300791259));
#374695=CARTESIAN_POINT('Ctrl Pts',(1.45957001512327,-0.148199386829699,
5.45502607686382));
#374696=CARTESIAN_POINT('Ctrl Pts',(1.47330898038679,0.0407919157890449,
5.46188119746995));
#374697=CARTESIAN_POINT('Ctrl Pts',(1.43234406746629,0.381079555584754,
5.47405531723903));
#374698=CARTESIAN_POINT('Ctrl Pts',(1.38942465639446,0.531038759436448,
5.47935753809352));
#374699=CARTESIAN_POINT('Ctrl Pts',(1.25533045048584,0.817592101860293,
5.48939547357438));
#374700=CARTESIAN_POINT('Ctrl Pts',(1.16271769295252,0.952788278842525,
5.49447277254087));
#374701=CARTESIAN_POINT('Ctrl Pts',(1.0509439038327,1.07028823734397,5.50000000000003));
#374702=CARTESIAN_POINT('Origin',(0.,2.04523456705693E-15,3.99999999999998));
#374703=CARTESIAN_POINT('Ctrl Pts',(-7.37498501890957E-14,-1.49999999999999,
-8.1875));
#374704=CARTESIAN_POINT('Ctrl Pts',(-0.0707075837041045,-1.49999999999999,
-8.19090192020711));
#374705=CARTESIAN_POINT('Ctrl Pts',(-0.141469114138096,-1.49500106821859,
-8.19444529514366));
#374706=CARTESIAN_POINT('Ctrl Pts',(-0.410293528228611,-1.4566657614053,
-8.20844398543069));
#374707=CARTESIAN_POINT('Ctrl Pts',(-0.601123534669336,-1.38883044981847,
-8.2195096126071));
#374708=CARTESIAN_POINT('Ctrl Pts',(-0.938214653084433,-1.18614462758204,
-8.24135807833242));
#374709=CARTESIAN_POINT('Ctrl Pts',(-1.0827939343619,-1.05582191021027,
-8.25193422772871));
#374710=CARTESIAN_POINT('Ctrl Pts',(-1.31583506474116,-0.746005663469679,
-8.27175243119567));
#374711=CARTESIAN_POINT('Ctrl Pts',(-1.40148555690714,-0.56902757212789,
-8.28088735710405));
#374712=CARTESIAN_POINT('Ctrl Pts',(-1.50116293429005,-0.18902395801905,
-8.30199866899899));
#374713=CARTESIAN_POINT('Ctrl Pts',(-1.51297807672142,0.0105976379183958,
-8.31308875766218));
#374714=CARTESIAN_POINT('Ctrl Pts',(-1.45941370735621,0.395532893185297,
-8.33447404962145));
#374715=CARTESIAN_POINT('Ctrl Pts',(-1.39738912175206,0.577635365282228,
-8.34459085362684));
#374716=CARTESIAN_POINT('Ctrl Pts',(-1.20444714400469,0.915854641577226,
-8.363380813421));
#374717=CARTESIAN_POINT('Ctrl Pts',(-1.07262763202685,1.06724487327345,
-8.37387220325007));
#374718=CARTESIAN_POINT('Ctrl Pts',(-0.760035204662309,1.30790925908279,
-8.3955969352519));
#374719=CARTESIAN_POINT('Ctrl Pts',(-0.583135101083686,1.39579330471248,
-8.40654926894335));
#374720=CARTESIAN_POINT('Ctrl Pts',(-0.210863302817571,1.49723221581078,
-8.42727795171891));
#374721=CARTESIAN_POINT('Ctrl Pts',(-0.0195780693232269,1.51187814134585,
-8.43622810132984));
#374722=CARTESIAN_POINT('Ctrl Pts',(0.366999280241712,1.46794990166863,
-8.45604754161259));
#374723=CARTESIAN_POINT('Ctrl Pts',(0.558185703277335,1.40640519943362,
-8.46695557774176));
#374724=CARTESIAN_POINT('Ctrl Pts',(0.900625440472865,1.21502563541599,
-8.48874731627983));
#374725=CARTESIAN_POINT('Ctrl Pts',(1.0496529255059,1.08887867255185,-8.49942148679832));
#374726=CARTESIAN_POINT('Ctrl Pts',(1.29149614569776,0.787026721220456,
-8.51944195058082));
#374727=CARTESIAN_POINT('Ctrl Pts',(1.38206102761909,0.614234598378379,
-8.5283758556457));
#374728=CARTESIAN_POINT('Ctrl Pts',(1.494175951662,0.238578192797074,-8.54924565595578));
#374729=CARTESIAN_POINT('Ctrl Pts',(1.51260341881051,0.0387817213571734,
-8.56034545992466));
#374730=CARTESIAN_POINT('Ctrl Pts',(1.47133257046456,-0.348913673671884,
-8.58188409298183));
#374731=CARTESIAN_POINT('Ctrl Pts',(1.4149199778164,-0.5334643634612,-8.59213690908124));
#374732=CARTESIAN_POINT('Ctrl Pts',(1.23152121190892,-0.879487024884344,
-8.61136039027141));
#374733=CARTESIAN_POINT('Ctrl Pts',(1.10315197137068,-1.03597125398216,
-8.62153488864168));
#374734=CARTESIAN_POINT('Ctrl Pts',(0.846015702352284,-1.24559117952707,
-8.63972913886261));
#374735=CARTESIAN_POINT('Ctrl Pts',(0.733793370559806,-1.31483324275516,
-8.64705182896356));
#374736=CARTESIAN_POINT('Ctrl Pts',(0.495789405867406,-1.42161138720955,
-8.66146885962202));
#374737=CARTESIAN_POINT('Ctrl Pts',(0.371204802885295,-1.45910892507311,
-8.66850453740173));
#374738=CARTESIAN_POINT('Ctrl Pts',(0.243337884005354,-1.4801306274136,
-8.67524047358083));
#374739=CARTESIAN_POINT('Ctrl Pts',(1.20419349529492,-0.894381364905029,
-8.67524047358084));
#374740=CARTESIAN_POINT('Ctrl Pts',(1.2782414791322,-0.794683289815975,
-8.66890844732269));
#374741=CARTESIAN_POINT('Ctrl Pts',(1.33960503944486,-0.686208596444366,
-8.66312269980246));
#374742=CARTESIAN_POINT('Ctrl Pts',(1.43592702107561,-0.452405413158382,
-8.65013363406435));
#374743=CARTESIAN_POINT('Ctrl Pts',(1.46942479488015,-0.327630086744163,
-8.64320167148566));
#374744=CARTESIAN_POINT('Ctrl Pts',(1.51302216223568,-0.00378489863631561,
-8.62521027214634));
#374745=CARTESIAN_POINT('Ctrl Pts',(1.5002965148524,0.195873440965775,-8.61411814216845));
#374746=CARTESIAN_POINT('Ctrl Pts',(1.39889719309338,0.575286936544728,
-8.59303961463629));
#374747=CARTESIAN_POINT('Ctrl Pts',(1.3125677242591,0.751683001948557,-8.58393752735663));
#374748=CARTESIAN_POINT('Ctrl Pts',(1.07831502519926,1.06041034665218,-8.56409127954316));
#374749=CARTESIAN_POINT('Ctrl Pts',(0.933119620966255,1.19017001906558,
-8.55350112705509));
#374750=CARTESIAN_POINT('Ctrl Pts',(0.595003215773495,1.39147663810463,
-8.53164164339661));
#374751=CARTESIAN_POINT('Ctrl Pts',(0.403785151285716,1.4584959421497,-8.52058001264486));
#374752=CARTESIAN_POINT('Ctrl Pts',(0.0163176781344214,1.51196127815833,
-8.50045282692856));
#374753=CARTESIAN_POINT('Ctrl Pts',(-0.175613308436975,1.50181829121292,
-8.49160130884752));
#374754=CARTESIAN_POINT('Ctrl Pts',(-0.55003902760651,1.40910092939278,
-8.47101126076191));
#374755=CARTESIAN_POINT('Ctrl Pts',(-0.728550060234893,1.3256379036634,
-8.46010422731876));
#374756=CARTESIAN_POINT('Ctrl Pts',(-1.04642765622587,1.09292919435903,
-8.43834620353686));
#374757=CARTESIAN_POINT('Ctrl Pts',(-1.18190714024603,0.944789086303314,
-8.42771294082126));
#374758=CARTESIAN_POINT('Ctrl Pts',(-1.38276976512002,0.611651413680171,
-8.40879510903664));
#374759=CARTESIAN_POINT('Ctrl Pts',(-1.44913555775106,0.431533165346498,
-8.39897406474137));
#374760=CARTESIAN_POINT('Ctrl Pts',(-1.51216067476163,0.0488592118263083,
-8.37771440065692));
#374761=CARTESIAN_POINT('Ctrl Pts',(-1.50544860899612,-0.150481167469412,
-8.3666399351405));
#374762=CARTESIAN_POINT('Ctrl Pts',(-1.41548304772181,-0.533741161849835,
-8.34534771323048));
#374763=CARTESIAN_POINT('Ctrl Pts',(-1.33365689272042,-0.714015609107781,
-8.33599849691514));
#374764=CARTESIAN_POINT('Ctrl Pts',(-1.10740755095398,-1.02989318455475,
-8.31633869328833));
#374765=CARTESIAN_POINT('Ctrl Pts',(-0.966302286143343,-1.16330258406064,
-8.30584394641685));
#374766=CARTESIAN_POINT('Ctrl Pts',(-0.635026717709483,-1.37358591619412,
-8.28406423952887));
#374767=CARTESIAN_POINT('Ctrl Pts',(-0.446420881426595,-1.44593213710974,
-8.27298031975216));
#374768=CARTESIAN_POINT('Ctrl Pts',(-0.166651770674125,-1.49306059659345,
-8.25821079826063));
#374769=CARTESIAN_POINT('Ctrl Pts',(-0.0833099133578137,-1.49999999999999,
-8.25400825007527));
#374770=CARTESIAN_POINT('Ctrl Pts',(-7.92750261663253E-15,-1.49999999999999,
-8.25));
#374771=CARTESIAN_POINT('Origin',(0.,1.73472347597681E-15,5.875));
#374772=CARTESIAN_POINT('',(-1.99005104861445E-16,-1.625,6.));
#374773=CARTESIAN_POINT('Origin',(-1.99005104861445E-16,-1.625,5.875));
#374774=CARTESIAN_POINT('Origin',(0.,1.80560739335254E-15,6.));
#374775=CARTESIAN_POINT('Origin',(0.,2.35813972515597E-15,7.5));
#374776=CARTESIAN_POINT('',(0.,2.35813972515597E-15,6.77831216351297));
#374777=CARTESIAN_POINT('',(-1.25,2.54592904999812E-15,7.5));
#374778=CARTESIAN_POINT('',(-1.25,2.20505887526255E-15,7.5));
#374779=CARTESIAN_POINT('',(-0.625,-1.08253175473055,7.5));
#374780=CARTESIAN_POINT('Origin',(0.,2.35813972515597E-15,7.5));
#374781=CARTESIAN_POINT('',(0.625,-1.08253175473055,7.5));
#374782=CARTESIAN_POINT('Origin',(0.,2.35813972515597E-15,7.5));
#374783=CARTESIAN_POINT('',(1.25,1.79477175062954E-15,7.5));
#374784=CARTESIAN_POINT('Origin',(0.,2.35813972515597E-15,7.5));
#374785=CARTESIAN_POINT('',(0.625,1.08253175473055,7.5));
#374786=CARTESIAN_POINT('Origin',(0.,2.35813972515597E-15,7.5));
#374787=CARTESIAN_POINT('',(-0.625,1.08253175473055,7.5));
#374788=CARTESIAN_POINT('Origin',(0.,2.35813972515597E-15,7.5));
#374789=CARTESIAN_POINT('Origin',(0.,2.35813972515597E-15,7.5));
#374790=CARTESIAN_POINT('Origin',(0.,-7.70371977754894E-31,9.));
#374791=CARTESIAN_POINT('',(1.25,0.721687836487031,9.));
#374792=CARTESIAN_POINT('',(1.25,-0.721687836487032,9.));
#374793=CARTESIAN_POINT('Ctrl Pts',(1.25,0.721687836487026,9.));
#374794=CARTESIAN_POINT('Ctrl Pts',(1.25,-7.7715611723761E-16,8.63915608175649));
#374795=CARTESIAN_POINT('Ctrl Pts',(1.25,-0.721687836487028,9.));
#374796=CARTESIAN_POINT('Origin',(0.,-7.70371977754894E-31,9.));
#374797=CARTESIAN_POINT('Origin',(0.,1.73472347597681E-15,6.055));
#374798=CARTESIAN_POINT('',(-2.54610912703474,1.42291503670651E-15,6.01610912703474));
#374799=CARTESIAN_POINT('Origin',(0.,1.84795814293585E-15,6.01610912703474));
#374800=CARTESIAN_POINT('',(-2.50721825406948,1.42767779501581E-15,6.));
#374801=CARTESIAN_POINT('Origin',(-2.50721825406948,1.42767779501581E-15,
6.055));
#374802=CARTESIAN_POINT('Origin',(0.,1.84795814293585E-15,6.));
#374803=CARTESIAN_POINT('Origin',(0.,1.84795814293585E-15,6.01610912703474));
#374804=CARTESIAN_POINT('',(-2.73389087296526,1.51315307225634E-15,6.20389087296526));
#374805=CARTESIAN_POINT('Origin',(0.,1.84795814293585E-15,6.20389087296526));
#374806=CARTESIAN_POINT('',(-2.54610912703474,1.53614970366555E-15,6.01610912703474));
#374807=CARTESIAN_POINT('Origin',(0.,1.73472347597681E-15,6.24278174593052));
#374808=CARTESIAN_POINT('',(-2.75,1.39794560621129E-15,6.24278174593052));
#374809=CARTESIAN_POINT('Origin',(0.,1.84795814293585E-15,6.24278174593052));
#374810=CARTESIAN_POINT('Origin',(-2.695,1.4046811636066E-15,6.24278174593052));
#374811=CARTESIAN_POINT('Origin',(0.,1.84795814293585E-15,8.79610912703474));
#374812=CARTESIAN_POINT('',(-2.73365018604124,0.0362762407020289,8.79610912703474));
#374813=CARTESIAN_POINT('',(-2.73365018604124,-0.0362762407020486,8.79610912703474));
#374814=CARTESIAN_POINT('Origin',(0.,1.84795814293585E-15,8.79610912703474));
#374815=CARTESIAN_POINT('',(-2.66979042840331,-0.0685319131367817,8.85933012996512));
#374816=CARTESIAN_POINT('Ctrl Pts',(-2.73365018604124,-0.0362762407020486,
8.79610912703474));
#374817=CARTESIAN_POINT('Ctrl Pts',(-2.72808418062094,-0.0390874501823592,
8.80163734024559));
#374818=CARTESIAN_POINT('Ctrl Pts',(-2.72251616230074,-0.0418997250385102,
8.80716298614018));
#374819=CARTESIAN_POINT('Ctrl Pts',(-2.71694609217046,-0.0447130856437622,
8.8126860086129));
#374820=CARTESIAN_POINT('Ctrl Pts',(-2.70124415813737,-0.052643901881576,
8.82825531609049));
#374821=CARTESIAN_POINT('Ctrl Pts',(-2.68552590846928,-0.0605833515018367,
8.84380379913848));
#374822=CARTESIAN_POINT('Ctrl Pts',(-2.66979042840331,-0.0685319131367817,
8.85933012996512));
#374823=CARTESIAN_POINT('',(-2.66869591238441,-0.102662953079004,8.85933012996512));
#374824=CARTESIAN_POINT('Origin',(-2.67852080896312,-0.0858949510114057,
8.84999761231046));
#374825=CARTESIAN_POINT('',(-2.73035783527281,-0.138943861495087,8.79610912703474));
#374826=CARTESIAN_POINT('Ctrl Pts',(-2.66869591238441,-0.102662953079004,
8.85933012996512));
#374827=CARTESIAN_POINT('Ctrl Pts',(-2.6740857579175,-0.105834453458509,
8.8538223528706));
#374828=CARTESIAN_POINT('Ctrl Pts',(-2.67947351161323,-0.109004669736153,
8.84831178811348));
#374829=CARTESIAN_POINT('Ctrl Pts',(-2.68485921376854,-0.112173626398928,
8.84279849653635));
#374830=CARTESIAN_POINT('Ctrl Pts',(-2.7000414174675,-0.121106861876859,
8.82725662040549));
#374831=CARTESIAN_POINT('Ctrl Pts',(-2.71520733790511,-0.130030099226532,
8.81169306718667));
#374832=CARTESIAN_POINT('Ctrl Pts',(-2.73035783527281,-0.138943861495087,
8.79610912703474));
#374833=CARTESIAN_POINT('',(-2.7257093818291,-0.211347276044891,8.79610912703474));
#374834=CARTESIAN_POINT('Origin',(0.,1.84795814293585E-15,8.79610912703474));
#374835=CARTESIAN_POINT('',(-2.65991420288366,-0.23944516702142,8.85933012996512));
#374836=CARTESIAN_POINT('Ctrl Pts',(-2.7257093818291,-0.211347276044891,
8.79610912703474));
#374837=CARTESIAN_POINT('Ctrl Pts',(-2.71997469755407,-0.21379609440213,
8.80163734024559));
#374838=CARTESIAN_POINT('Ctrl Pts',(-2.714237936256,-0.216245846979342,
8.80716298614018));
#374839=CARTESIAN_POINT('Ctrl Pts',(-2.70849905779933,-0.218696551614944,
8.8126860086129));
#374840=CARTESIAN_POINT('Ctrl Pts',(-2.69232125593275,-0.225605046772597,
8.82825531609049));
#374841=CARTESIAN_POINT('Ctrl Pts',(-2.67612661881068,-0.232521112228163,
8.84380379913848));
#374842=CARTESIAN_POINT('Ctrl Pts',(-2.65991420288366,-0.23944516702142,
8.85933012996512));
#374843=CARTESIAN_POINT('',(-2.65663515242803,-0.273435955199435,8.85933012996512));
#374844=CARTESIAN_POINT('Origin',(-2.66751419228412,-0.257331888075536,
8.84999761231045));
#374845=CARTESIAN_POINT('',(-2.71584585849932,-0.313593013561955,8.79610912703474));
#374846=CARTESIAN_POINT('Ctrl Pts',(-2.65663515242803,-0.273435955199435,
8.85933012996512));
#374847=CARTESIAN_POINT('Ctrl Pts',(-2.66181072521843,-0.276946267980235,
8.8538223528706));
#374848=CARTESIAN_POINT('Ctrl Pts',(-2.66698429274206,-0.280455165273019,
8.84831178811348));
#374849=CARTESIAN_POINT('Ctrl Pts',(-2.67215589364419,-0.283962674096302,
8.84279849653635));
#374850=CARTESIAN_POINT('Ctrl Pts',(-2.68673454951515,-0.293850282414642,
8.82725662040549));
#374851=CARTESIAN_POINT('Ctrl Pts',(-2.70129759616275,-0.303726869874814,
8.81169306718667));
#374852=CARTESIAN_POINT('Ctrl Pts',(-2.71584585849932,-0.313593013561955,
8.79610912703474));
#374853=CARTESIAN_POINT('',(-2.7065680531042,-0.385549840096616,8.79610912703474));
#374854=CARTESIAN_POINT('Origin',(0.,1.84795814293585E-15,8.79610912703474));
#374855=CARTESIAN_POINT('',(-2.63910781935455,-0.40937448935394,8.85933012996512));
#374856=CARTESIAN_POINT('Ctrl Pts',(-2.7065680531042,-0.385549840096616,
8.79610912703474));
#374857=CARTESIAN_POINT('Ctrl Pts',(-2.70068825502221,-0.387626204610885,
8.80163734024559));
#374858=CARTESIAN_POINT('Ctrl Pts',(-2.69480632432897,-0.389703368350347,
8.80716298614018));
#374859=CARTESIAN_POINT('Ctrl Pts',(-2.68892221982847,-0.391781346545276,
8.8126860086129));
#374860=CARTESIAN_POINT('Ctrl Pts',(-2.67233502818641,-0.397639132134298,
8.82825531609049));
#374861=CARTESIAN_POINT('Ctrl Pts',(-2.65573055084804,-0.403503393828722,
8.84380379913848));
#374862=CARTESIAN_POINT('Ctrl Pts',(-2.63910781935455,-0.40937448935394,
8.85933012996512));
#374863=CARTESIAN_POINT('',(-2.63365770878388,-0.443085350328122,8.85933012996512));
#374864=CARTESIAN_POINT('Origin',(-2.645546187609,-0.427711393214038,8.84999761231048));
#374865=CARTESIAN_POINT('',(-2.69017388854615,-0.486953544670607,8.79610912703474));
#374866=CARTESIAN_POINT('Ctrl Pts',(-2.63365770878388,-0.443085350328122,
8.85933012996512));
#374867=CARTESIAN_POINT('Ctrl Pts',(-2.63859774129283,-0.446920050882042,
8.8538223528706));
#374868=CARTESIAN_POINT('Ctrl Pts',(-2.64353586334569,-0.450753210378334,
8.84831178811348));
#374869=CARTESIAN_POINT('Ctrl Pts',(-2.64847211177722,-0.454584858256012,
8.84279849653635));
#374870=CARTESIAN_POINT('Ctrl Pts',(-2.66238731299609,-0.465386209111295,
8.82725662040549));
#374871=CARTESIAN_POINT('Ctrl Pts',(-2.67628764317125,-0.47617556166557,
8.81169306718667));
#374872=CARTESIAN_POINT('Ctrl Pts',(-2.69017388854615,-0.486953544670607,
8.79610912703474));
#374873=CARTESIAN_POINT('',(-2.67630485569206,-0.558168097155203,8.79610912703474));
#374874=CARTESIAN_POINT('Origin',(0.,1.84795814293585E-15,8.79610912703474));
#374875=CARTESIAN_POINT('',(-2.60745677570886,-0.577621604099153,8.85933012996512));
#374876=CARTESIAN_POINT('Ctrl Pts',(-2.67630485569206,-0.558168097155203,
8.79610912703474));
#374877=CARTESIAN_POINT('Ctrl Pts',(-2.67030410515465,-0.559863475599333,
8.80163734024559));
#374878=CARTESIAN_POINT('Ctrl Pts',(-2.66430117518113,-0.56155951498969,
8.80716298614018));
#374879=CARTESIAN_POINT('Ctrl Pts',(-2.65829602368434,-0.563256227885819,
8.8126860086129));
#374880=CARTESIAN_POINT('Ctrl Pts',(-2.64136760259518,-0.568039233008733,
8.82825531609049));
#374881=CARTESIAN_POINT('Ctrl Pts',(-2.62442151639954,-0.572827593432832,
8.84380379913848));
#374882=CARTESIAN_POINT('Ctrl Pts',(-2.60745677570886,-0.577621604099153,
8.85933012996512));
#374883=CARTESIAN_POINT('',(-2.59985800069652,-0.610914012710802,8.85933012996512));
#374884=CARTESIAN_POINT('Origin',(-2.61270706618115,-0.59633334049403,8.84999761231046));
#374885=CARTESIAN_POINT('',(-2.65344741704445,-0.658313079212999,8.79610912703474));
#374886=CARTESIAN_POINT('Ctrl Pts',(-2.59985800069652,-0.610914012710802,
8.85933012996512));
#374887=CARTESIAN_POINT('Ctrl Pts',(-2.60454219327082,-0.615057343430724,
8.8538223528706));
#374888=CARTESIAN_POINT('Ctrl Pts',(-2.60922457805016,-0.619199013855944,
8.84831178811348));
#374889=CARTESIAN_POINT('Ctrl Pts',(-2.61390518990746,-0.623339055725002,
8.84279849653635));
#374890=CARTESIAN_POINT('Ctrl Pts',(-2.62709975592765,-0.63500976404968,
8.82725662040549));
#374891=CARTESIAN_POINT('Ctrl Pts',(-2.64028025019205,-0.646667545934106,
8.81169306718667));
#374892=CARTESIAN_POINT('Ctrl Pts',(-2.65344741704445,-0.658313079212999,
8.79610912703474));
#374893=CARTESIAN_POINT('',(-2.6350441475623,-0.728492721775898,8.79610912703474));
#374894=CARTESIAN_POINT('Origin',(0.,1.84795814293585E-15,8.79610912703474));
#374895=CARTESIAN_POINT('',(-2.56509113287406,-0.743495147773676,8.85933012996512));
#374896=CARTESIAN_POINT('Ctrl Pts',(-2.6350441475623,-0.728492721775898,
8.79610912703474));
#374897=CARTESIAN_POINT('Ctrl Pts',(-2.62894710294058,-0.729800147476205,
8.80163734024559));
#374898=CARTESIAN_POINT('Ctrl Pts',(-2.62284784101367,-0.731108093127803,
8.80716298614018));
#374899=CARTESIAN_POINT('Ctrl Pts',(-2.61674631897617,-0.732416568567897,
8.8126860086129));
#374900=CARTESIAN_POINT('Ctrl Pts',(-2.59954623095332,-0.736105138830703,
8.82825531609049));
#374901=CARTESIAN_POINT('Ctrl Pts',(-2.58232817100351,-0.739797921584393,
8.84380379913848));
#374902=CARTESIAN_POINT('Ctrl Pts',(-2.56509113287406,-0.743495147773676,
8.85933012996512));
#374903=CARTESIAN_POINT('',(-2.55537491841651,-0.776232298374609,8.85933012996512));
#374904=CARTESIAN_POINT('Origin',(-2.56913177099444,-0.762504826164824,
8.84999761231046));
#374905=CARTESIAN_POINT('',(-2.60581736094343,-0.826967464105193,8.79610912703474));
#374906=CARTESIAN_POINT('Ctrl Pts',(-2.55537491841651,-0.776232298374609,
8.85933012996512));
#374907=CARTESIAN_POINT('Ctrl Pts',(-2.55978402270411,-0.780667233425863,
8.8538223528706));
#374908=CARTESIAN_POINT('Ctrl Pts',(-2.5641914292865,-0.785100395767848,
8.84831178811348));
#374909=CARTESIAN_POINT('Ctrl Pts',(-2.56859717093147,-0.78953181930821,
8.84279849653635));
#374910=CARTESIAN_POINT('Ctrl Pts',(-2.58101688245097,-0.802023927658419,
8.82725662040549));
#374911=CARTESIAN_POINT('Ctrl Pts',(-2.59342337932647,-0.814502234546644,
8.81169306718667));
#374912=CARTESIAN_POINT('Ctrl Pts',(-2.60581736094343,-0.826967464105193,
8.79610912703474));
#374913=CARTESIAN_POINT('',(-2.582955477815,-0.895823813541617,8.79610912703474));
#374914=CARTESIAN_POINT('Origin',(0.,1.84795814293585E-15,8.79610912703474));
#374915=CARTESIAN_POINT('',(-2.51218498036396,-0.906313510406788,8.85933012996512));
#374916=CARTESIAN_POINT('Ctrl Pts',(-2.582955477815,-0.895823813541617,
8.79610912703474));
#374917=CARTESIAN_POINT('Ctrl Pts',(-2.57678719317314,-0.896737914005455,
8.80163734024559));
#374918=CARTESIAN_POINT('Ctrl Pts',(-2.57061666246838,-0.897652391289058,
8.80716298614018));
#374919=CARTESIAN_POINT('Ctrl Pts',(-2.56444384235301,-0.898567252466868,
8.8126860086129));
#374920=CARTESIAN_POINT('Ctrl Pts',(-2.54704276624755,-0.901146230743158,
8.82825531609049));
#374921=CARTESIAN_POINT('Ctrl Pts',(-2.52962348524517,-0.903728261390006,
8.84380379913848));
#374922=CARTESIAN_POINT('Ctrl Pts',(-2.51218498036396,-0.906313510406788,
8.85933012996512));
#374923=CARTESIAN_POINT('',(-2.50039125247053,-0.938360879023088,8.85933012996512));
#374924=CARTESIAN_POINT('Origin',(-2.51499936228368,-0.925543015948133,
8.84999761231046));
#374925=CARTESIAN_POINT('',(-2.54747944236023,-0.992223662303413,8.79610912703474));
#374926=CARTESIAN_POINT('Ctrl Pts',(-2.50039125247053,-0.938360879023088,
8.85933012996512));
#374927=CARTESIAN_POINT('Ctrl Pts',(-2.50450715051616,-0.943069194306258,
8.8538223528706));
#374928=CARTESIAN_POINT('Ctrl Pts',(-2.50862146792258,-0.947775631750034,
8.84831178811348));
#374929=CARTESIAN_POINT('Ctrl Pts',(-2.51273423521776,-0.952480227291835,
8.84279849653635));
#374930=CARTESIAN_POINT('Ctrl Pts',(-2.52432805697791,-0.965742402914816,
8.82725662040549));
#374931=CARTESIAN_POINT('Ctrl Pts',(-2.53590957550768,-0.978989958767248,
8.81169306718667));
#374932=CARTESIAN_POINT('Ctrl Pts',(-2.54747944236023,-0.992223662303413,
8.79610912703474));
#374933=CARTESIAN_POINT('',(-2.52025288996715,-1.05947377310389,8.79610912703474));
#374934=CARTESIAN_POINT('Origin',(0.,1.84795814293585E-15,8.79610912703474));
#374935=CARTESIAN_POINT('',(-2.44895572090755,-1.065407636422,8.85933012996512));
#374936=CARTESIAN_POINT('Ctrl Pts',(-2.52025288996715,-1.05947377310389,
8.79610912703474));
#374937=CARTESIAN_POINT('Ctrl Pts',(-2.51403871210983,-1.05999079209638,
8.80163734024559));
#374938=CARTESIAN_POINT('Ctrl Pts',(-2.50782226866146,-1.06050804322867,
8.80716298614018));
#374939=CARTESIAN_POINT('Ctrl Pts',(-2.50160351591014,-1.06102553078338,
8.8126860086129));
#374940=CARTESIAN_POINT('Ctrl Pts',(-2.48407295647631,-1.06248431949823,
8.82825531609049));
#374941=CARTESIAN_POINT('Ctrl Pts',(-2.46652403398342,-1.06394498792046,
8.84380379913848));
#374942=CARTESIAN_POINT('Ctrl Pts',(-2.44895572090755,-1.065407636422,8.85933012996512));
#374943=CARTESIAN_POINT('',(-2.43513294253591,-1.09663353354188,8.85933012996512));
#374944=CARTESIAN_POINT('Origin',(-2.45053228172762,-1.08477795095056,8.84999761231046));
#374945=CARTESIAN_POINT('',(-2.47867338431574,-1.15340260064192,8.79610912703474));
#374946=CARTESIAN_POINT('Ctrl Pts',(-2.43513294253591,-1.09663353354188,
8.85933012996512));
#374947=CARTESIAN_POINT('Ctrl Pts',(-2.43893872123164,-1.10159588157954,
8.8538223528706));
#374948=CARTESIAN_POINT('Ctrl Pts',(-2.44274304284934,-1.10655625436413,
8.84831178811348));
#374949=CARTESIAN_POINT('Ctrl Pts',(-2.44654593555174,-1.11151468971515,
8.84279849653635));
#374950=CARTESIAN_POINT('Ctrl Pts',(-2.45726622605206,-1.12549243548654,
8.82725662040549));
#374951=CARTESIAN_POINT('Ctrl Pts',(-2.46797517529222,-1.13945480325459,
8.81169306718667));
#374952=CARTESIAN_POINT('Ctrl Pts',(-2.47867338431574,-1.15340260064192,
8.79610912703474));
#374953=CARTESIAN_POINT('',(-2.44719404240188,-1.21877012767606,8.79610912703474));
#374954=CARTESIAN_POINT('Origin',(0.,1.84795814293585E-15,8.79610912703474));
#374955=CARTESIAN_POINT('',(-2.37566317709458,-1.22012377392993,8.85933012996512));
#374956=CARTESIAN_POINT('Ctrl Pts',(-2.44719404240188,-1.21877012767606,
8.79610912703474));
#374957=CARTESIAN_POINT('Ctrl Pts',(-2.44095950671885,-1.21888794065527,
8.80163734024559));
#374958=CARTESIAN_POINT('Ctrl Pts',(-2.43472269522642,-1.2190058401404,
8.80716298614018));
#374959=CARTESIAN_POINT('Ctrl Pts',(-2.42848356402812,-1.21912382760464,
8.8126860086129));
#374960=CARTESIAN_POINT('Ctrl Pts',(-2.41089555809493,-1.21945643228231,
8.82825531609049));
#374961=CARTESIAN_POINT('Ctrl Pts',(-2.39328910639829,-1.21978973628007,
8.84380379913848));
#374962=CARTESIAN_POINT('Ctrl Pts',(-2.37566317709458,-1.22012377392993,
8.85933012996512));
#374963=CARTESIAN_POINT('',(-2.35986814900602,-1.2503998856442,8.85933012996512));
#374964=CARTESIAN_POINT('Origin',(-2.37599543838843,-1.23955530066839,8.84999761231045));
#374965=CARTESIAN_POINT('',(-2.39968192566132,-1.30984196029031,8.79610912703474));
#374966=CARTESIAN_POINT('Ctrl Pts',(-2.35986814900602,-1.2503998856442,
8.85933012996512));
#374967=CARTESIAN_POINT('Ctrl Pts',(-2.36334816959087,-1.25559587508384,
8.8538223528706));
#374968=CARTESIAN_POINT('Ctrl Pts',(-2.36682686264629,-1.26078979997346,
8.84831178811348));
#374969=CARTESIAN_POINT('Ctrl Pts',(-2.37030425385408,-1.26598169985927,
8.84279849653635));
#374970=CARTESIAN_POINT('Ctrl Pts',(-2.38010696112141,-1.28061757822348,
8.82725662040549));
#374971=CARTESIAN_POINT('Ctrl Pts',(-2.38989933570247,-1.29523738354307,
8.81169306718667));
#374972=CARTESIAN_POINT('Ctrl Pts',(-2.39968192566132,-1.30984196029031,
8.79610912703474));
#374973=CARTESIAN_POINT('',(-2.3640791495949,-1.37305829436825,8.79610912703474));
#374974=CARTESIAN_POINT('Origin',(0.,1.84795814293585E-15,8.79610912703474));
#374975=CARTESIAN_POINT('',(-2.29260852370877,-1.36982616113506,8.85933012996512));
#374976=CARTESIAN_POINT('Ctrl Pts',(-2.3640791495949,-1.37305829436825,
8.79610912703474));
#374977=CARTESIAN_POINT('Ctrl Pts',(-2.35784987513059,-1.37277641721536,
8.80163734024559));
#374978=CARTESIAN_POINT('Ctrl Pts',(-2.35161832399032,-1.37249448057906,
8.80716298614018));
#374979=CARTESIAN_POINT('Ctrl Pts',(-2.34538445227342,-1.37221248311704,
8.8126860086129));
#374980=CARTESIAN_POINT('Ctrl Pts',(-2.32781127272986,-1.37141753701356,
8.82825531609049));
#374981=CARTESIAN_POINT('Ctrl Pts',(-2.31021964051606,-1.37062210696923,
8.84380379913848));
#374982=CARTESIAN_POINT('Ctrl Pts',(-2.29260852370877,-1.36982616113506,
8.85933012996512));
#374983=CARTESIAN_POINT('',(-2.27490615106174,-1.39902807640647,8.85933012996512));
#374984=CARTESIAN_POINT('Origin',(-2.29169512014346,-1.389239051772,8.84999761231045));
#374985=CARTESIAN_POINT('',(-2.3108296592442,-1.46089889836364,8.79610912703474));
#374986=CARTESIAN_POINT('Ctrl Pts',(-2.27490615106174,-1.39902807640647,
8.85933012996512));
#374987=CARTESIAN_POINT('Ctrl Pts',(-2.27804611338465,-1.40443635581295,
8.8538223528706));
#374988=CARTESIAN_POINT('Ctrl Pts',(-2.28118488318186,-1.40984248985614,
8.84831178811348));
#374989=CARTESIAN_POINT('Ctrl Pts',(-2.28432248354866,-1.41524651964645,
8.84279849653635));
#374990=CARTESIAN_POINT('Ctrl Pts',(-2.29316732615617,-1.43048038863989,
8.82725662040549));
#374991=CARTESIAN_POINT('Ctrl Pts',(-2.30200288711053,-1.44569755559503,
8.81169306718667));
#374992=CARTESIAN_POINT('Ctrl Pts',(-2.3108296592442,-1.46089889836364,
8.79610912703474));
#374993=CARTESIAN_POINT('',(-2.27124974846884,-1.52170427000879,8.79610912703474));
#374994=CARTESIAN_POINT('Origin',(0.,1.84795814293585E-15,8.79610912703474));
#374995=CARTESIAN_POINT('',(-2.20013305013606,-1.51389963881729,8.85933012996512));
#374996=CARTESIAN_POINT('Ctrl Pts',(-2.27124974846884,-1.52170427000879,
8.79610912703474));
#374997=CARTESIAN_POINT('Ctrl Pts',(-2.2650513326482,-1.52102386101749,
8.80163734024559));
#374998=CARTESIAN_POINT('Ctrl Pts',(-2.25885064864039,-1.52034324679787,
8.80716298614018));
#374999=CARTESIAN_POINT('Ctrl Pts',(-2.25264765272094,-1.51966242319765,
8.8126860086129));
#375000=CARTESIAN_POINT('Ctrl Pts',(-2.2351615115312,-1.51774319291709,
8.82825531609049));
#375001=CARTESIAN_POINT('Ctrl Pts',(-2.21765698659039,-1.51582229742333,
8.84380379913848));
#375002=CARTESIAN_POINT('Ctrl Pts',(-2.20013305013606,-1.51389963881729,
8.85933012996512));
#375003=CARTESIAN_POINT('',(-2.18059607577691,-1.54190736071221,8.85933012996512));
#375004=CARTESIAN_POINT('Origin',(-2.19797773508277,-1.53321412162103,8.84999761231045));
#375005=CARTESIAN_POINT('',(-2.21248169808584,-1.60595268950177,8.79610912703474));
#375006=CARTESIAN_POINT('Ctrl Pts',(-2.18059607577691,-1.54190736071221,
8.85933012996512));
#375007=CARTESIAN_POINT('Ctrl Pts',(-2.18338307705917,-1.54750570630536,
8.8538223528706));
#375008=CARTESIAN_POINT('Ctrl Pts',(-2.18616902571981,-1.55310183453774,
8.84831178811348));
#375009=CARTESIAN_POINT('Ctrl Pts',(-2.1889539421727,-1.55869578791498,
8.84279849653635));
#375010=CARTESIAN_POINT('Ctrl Pts',(-2.1968045747649,-1.5744650483023,8.82725662040549));
#375011=CARTESIAN_POINT('Ctrl Pts',(-2.20464701487737,-1.59021704628989,
8.81169306718667));
#375012=CARTESIAN_POINT('Ctrl Pts',(-2.21248169808584,-1.60595268950177,
8.79610912703474));
#375013=CARTESIAN_POINT('',(-2.16908729494479,-1.66409723639932,8.79610912703474));
#375014=CARTESIAN_POINT('Origin',(0.,1.84795814293585E-15,8.79610912703474));
#375015=CARTESIAN_POINT('',(-2.09861675793328,-1.65175217815317,8.85933012996512));
#375016=CARTESIAN_POINT('Ctrl Pts',(-2.16908729494479,-1.66409723639932,
8.79610912703474));
#375017=CARTESIAN_POINT('Ctrl Pts',(-2.16294520838798,-1.66302109151611,
8.80163734024559));
#375018=CARTESIAN_POINT('Ctrl Pts',(-2.15680087145326,-1.66194459650299,
8.80716298614018));
#375019=CARTESIAN_POINT('Ctrl Pts',(-2.15065424077203,-1.66086774441477,
8.8126860086129));
#375020=CARTESIAN_POINT('Ctrl Pts',(-2.13332699224101,-1.65783211648602,
8.82825531609049));
#375021=CARTESIAN_POINT('Ctrl Pts',(-2.1159815044209,-1.65479364891445,
8.84380379913848));
#375022=CARTESIAN_POINT('Ctrl Pts',(-2.09861675793328,-1.65175217815317,
8.85933012996512));
#375023=CARTESIAN_POINT('',(-2.07732546348032,-1.67845061693468,8.85933012996512));
#375024=CARTESIAN_POINT('Origin',(-2.09522838804386,-1.67088888577092,8.84999761231046));
#375025=CARTESIAN_POINT('',(-2.10504217505421,-1.74440727656297,8.79610912703474));
#375026=CARTESIAN_POINT('Ctrl Pts',(-2.07732546348032,-1.67845061693468,
8.85933012996512));
#375027=CARTESIAN_POINT('Ctrl Pts',(-2.07974805133586,-1.68421602391164,
8.8538223528706));
#375028=CARTESIAN_POINT('Ctrl Pts',(-2.08216973079929,-1.68997915064192,
8.84831178811348));
#375029=CARTESIAN_POINT('Ctrl Pts',(-2.08459051951921,-1.69574004085176,
8.84279849653635));
#375030=CARTESIAN_POINT('Ctrl Pts',(-2.09141468216282,-1.71197989335954,
8.82725662040549));
#375031=CARTESIAN_POINT('Ctrl Pts',(-2.09823177516478,-1.72820199404106,
8.81169306718667));
#375032=CARTESIAN_POINT('Ctrl Pts',(-2.10504217505421,-1.74440727656297,
8.79610912703474));
#375033=CARTESIAN_POINT('',(-2.05801159645804,-1.79965207029775,8.79610912703474));
#375034=CARTESIAN_POINT('Origin',(0.,1.84795814293585E-15,8.79610912703474));
#375035=CARTESIAN_POINT('',(-1.98847679932027,-1.78281731348928,8.85933012996512));
#375036=CARTESIAN_POINT('Ctrl Pts',(-2.05801159645804,-1.79965207029775,
8.79610912703474));
#375037=CARTESIAN_POINT('Ctrl Pts',(-2.0519510783162,-1.79818461163279,
8.80163734024559));
#375038=CARTESIAN_POINT('Ctrl Pts',(-2.04588833685299,-1.79671665937508,
8.80716298614018));
#375039=CARTESIAN_POINT('Ctrl Pts',(-2.03982332923389,-1.79524820381508,
8.8126860086129));
#375040=CARTESIAN_POINT('Ctrl Pts',(-2.0227261747425,-1.79110865228443,
8.82825531609049));
#375041=CARTESIAN_POINT('Ctrl Pts',(-2.00561100037312,-1.78696509835006,
8.84380379913848));
#375042=CARTESIAN_POINT('Ctrl Pts',(-1.98847679932027,-1.78281731348928,
8.85933012996512));
#375043=CARTESIAN_POINT('',(-1.96551867526937,-1.80809675954565,8.85933012996512));
#375044=CARTESIAN_POINT('Origin',(-1.98386929813342,-1.80169760908463,8.84999761231047));
#375045=CARTESIAN_POINT('',(-1.98895258219515,-1.87569371995058,8.79610912703474));
#375046=CARTESIAN_POINT('Ctrl Pts',(-1.96551867526937,-1.80809675954565,
8.85933012996512));
#375047=CARTESIAN_POINT('Ctrl Pts',(-1.96756689476505,-1.81400553661246,
8.8538223528706));
#375048=CARTESIAN_POINT('Ctrl Pts',(-1.96961435383092,-1.81991197991672,
8.84831178811348));
#375049=CARTESIAN_POINT('Ctrl Pts',(-1.97166106727775,-1.82581613422559,
8.84279849653635));
#375050=CARTESIAN_POINT('Ctrl Pts',(-1.97743071802469,-1.84245984581643,
8.82725662040549));
#375051=CARTESIAN_POINT('Ctrl Pts',(-1.98319445101873,-1.85908538910055,
8.81169306718667));
#375052=CARTESIAN_POINT('Ctrl Pts',(-1.98895258219515,-1.87569371995058,
8.79610912703474));
#375053=CARTESIAN_POINT('',(-1.93847908687934,-1.92781174781517,8.79610912703474));
#375054=CARTESIAN_POINT('Origin',(0.,1.84795814293585E-15,8.79610912703474));
#375055=CARTESIAN_POINT('',(-1.87016576301192,-1.90655647007116,8.85933012996512));
#375056=CARTESIAN_POINT('Ctrl Pts',(-1.93847908687934,-1.92781174781517,
8.79610912703474));
#375057=CARTESIAN_POINT('Ctrl Pts',(-1.93252504112149,-1.92595900547087,
8.80163734024559));
#375058=CARTESIAN_POINT('Ctrl Pts',(-1.92656880823491,-1.92410562809928,
8.80716298614018));
#375059=CARTESIAN_POINT('Ctrl Pts',(-1.9206103460952,-1.92225160326638,
8.8126860086129));
#375060=CARTESIAN_POINT('Ctrl Pts',(-1.90381354151856,-1.91702513843901,
8.82825531609049));
#375061=CARTESIAN_POINT('Ctrl Pts',(-1.88699901052261,-1.91179352489374,
8.84380379913848));
#375062=CARTESIAN_POINT('Ctrl Pts',(-1.87016576301192,-1.90655647007116,
8.85933012996512));
#375063=CARTESIAN_POINT('',(-1.84563514921931,-1.9303130447361,8.85933012996512));
#375064=CARTESIAN_POINT('Origin',(-1.86435806373832,-1.92510277045971,8.84999761231044));
#375065=CARTESIAN_POINT('',(-1.86468995654685,-1.99927253550787,8.79610912703474));
#375066=CARTESIAN_POINT('Ctrl Pts',(-1.84563514921931,-1.9303130447361,
8.85933012996512));
#375067=CARTESIAN_POINT('Ctrl Pts',(-1.84730058378188,-1.93634091146037,
8.8538223528706));
#375068=CARTESIAN_POINT('Ctrl Pts',(-1.84896540900169,-1.94236640049616,
8.84831178811348));
#375069=CARTESIAN_POINT('Ctrl Pts',(-1.85062963679087,-1.94838955746755,
8.84279849653635));
#375070=CARTESIAN_POINT('Ctrl Pts',(-1.85532106690864,-1.96536873556046,
8.82725662040549));
#375071=CARTESIAN_POINT('Ctrl Pts',(-1.86000775547958,-1.98232940352366,
8.81169306718667));
#375072=CARTESIAN_POINT('Ctrl Pts',(-1.86468995654685,-1.99927253550787,
8.79610912703474));
#375073=CARTESIAN_POINT('',(-1.8109809509302,-2.0480496333465,8.79610912703474));
#375074=CARTESIAN_POINT('Origin',(0.,1.84795814293585E-15,8.79610912703474));
#375075=CARTESIAN_POINT('',(-1.74416981443405,-2.02246117716243,8.85933012996512));
#375076=CARTESIAN_POINT('Ctrl Pts',(-1.8109809509302,-2.0480496333465,8.79610912703474));
#375077=CARTESIAN_POINT('Ctrl Pts',(-1.80515784400749,-2.04581922063857,
8.80163734024559));
#375078=CARTESIAN_POINT('Ctrl Pts',(-1.79933259513609,-2.04358803407826,
8.80716298614018));
#375079=CARTESIAN_POINT('Ctrl Pts',(-1.79350516307478,-2.04135605855819,
8.8126860086129));
#375080=CARTESIAN_POINT('Ctrl Pts',(-1.77707773008581,-2.03506415709914,
8.82825531609049));
#375081=CARTESIAN_POINT('Ctrl Pts',(-1.76063293697783,-2.02876598176521,
8.84380379913848));
#375082=CARTESIAN_POINT('Ctrl Pts',(-1.74416981443405,-2.02246117716243,
8.85933012996512));
#375083=CARTESIAN_POINT('',(-1.71816751245361,-2.04459725957488,8.85933012996512));
#375084=CARTESIAN_POINT('Origin',(-1.73718578215576,-2.0405972716177,8.84999761231045));
#375085=CARTESIAN_POINT('',(-1.73276491989237,-2.11463591137414,8.79610912703474));
#375086=CARTESIAN_POINT('Ctrl Pts',(-1.71816751245361,-2.04459725957488,
8.85933012996512));
#375087=CARTESIAN_POINT('Ctrl Pts',(-1.71944331845521,-2.05071944615927,
8.8538223528706));
#375088=CARTESIAN_POINT('Ctrl Pts',(-1.72071866870505,-2.05683922089966,
8.84831178811348));
#375089=CARTESIAN_POINT('Ctrl Pts',(-1.72199357216761,-2.06295663008962,
8.84279849653635));
#375090=CARTESIAN_POINT('Ctrl Pts',(-1.72558750356354,-2.0802015035998,
8.82725662040549));
#375091=CARTESIAN_POINT('Ctrl Pts',(-1.72917788910274,-2.09742760121936,
8.81169306718667));
#375092=CARTESIAN_POINT('Ctrl Pts',(-1.73276491989237,-2.11463591137414,
8.79610912703474));
#375093=CARTESIAN_POINT('',(-1.67604110579949,-2.15987164362913,8.79610912703474));
#375094=CARTESIAN_POINT('Origin',(0.,1.84795814293585E-15,8.79610912703474));
#375095=CARTESIAN_POINT('',(-1.61100669796542,-2.13005515746017,8.85933012996512));
#375096=CARTESIAN_POINT('Ctrl Pts',(-1.67604110579949,-2.15987164362913,
8.79610912703474));
#375097=CARTESIAN_POINT('Ctrl Pts',(-1.67037286610732,-2.15727272580181,
8.80163734024559));
#375098=CARTESIAN_POINT('Ctrl Pts',(-1.66470253844822,-2.15467289847695,
8.80716298614018));
#375099=CARTESIAN_POINT('Ctrl Pts',(-1.65903008263363,-2.15207214393587,
8.8126860086129));
#375100=CARTESIAN_POINT('Ctrl Pts',(-1.64303952507815,-2.14474066061786,
8.82825531609049));
#375101=CARTESIAN_POINT('Ctrl Pts',(-1.62703204504044,-2.13740180404866,
8.84380379913848));
#375102=CARTESIAN_POINT('Ctrl Pts',(-1.61100669796542,-2.13005515746017,
8.85933012996512));
#375103=CARTESIAN_POINT('',(-1.58363955683346,-2.15047978570934,8.85933012996512));
#375104=CARTESIAN_POINT('Origin',(-1.60287503156913,-2.14770652087987,8.84999761231047));
#375105=CARTESIAN_POINT('',(-1.59371958050514,-2.2213097946926,8.79610912703474));
#375106=CARTESIAN_POINT('Ctrl Pts',(-1.58363955683346,-2.15047978570934,
8.85933012996512));
#375107=CARTESIAN_POINT('Ctrl Pts',(-1.58452049171358,-2.15667113477596,
8.8538223528706));
#375108=CARTESIAN_POINT('Ctrl Pts',(-1.5854011263057,-2.16286004775386,
8.84831178811348));
#375109=CARTESIAN_POINT('Ctrl Pts',(-1.58628146658985,-2.16904657141585,
8.84279849653635));
#375110=CARTESIAN_POINT('Ctrl Pts',(-1.58876313102894,-2.18648627745903,
8.82725662040549));
#375111=CARTESIAN_POINT('Ctrl Pts',(-1.59124245987209,-2.20390701900485,
8.81169306718667));
#375112=CARTESIAN_POINT('Ctrl Pts',(-1.59371958050514,-2.2213097946926,
8.79610912703474));
#375113=CARTESIAN_POINT('',(-1.53421404825535,-2.26281827803708,8.79610912703474));
#375114=CARTESIAN_POINT('Origin',(0.,1.84795814293585E-15,8.79610912703474));
#375115=CARTESIAN_POINT('',(-1.471223609415,-2.22889628422052,8.85933012996512));
#375116=CARTESIAN_POINT('Ctrl Pts',(-1.53421404825535,-2.26281827803708,
8.79610912703474));
#375117=CARTESIAN_POINT('Ctrl Pts',(-1.52872396780646,-2.25986153460119,
8.80163734024559));
#375118=CARTESIAN_POINT('Ctrl Pts',(-1.52323186195229,-2.25690374975992,
8.80716298614018));
#375119=CARTESIAN_POINT('Ctrl Pts',(-1.51773769172211,-2.2539449032561,
8.8126860086129));
#375120=CARTESIAN_POINT('Ctrl Pts',(-1.50224971823107,-2.24560396471667,
8.82825531609049));
#375121=CARTESIAN_POINT('Ctrl Pts',(-1.48674532943269,-2.23725458384803,
8.84380379913848));
#375122=CARTESIAN_POINT('Ctrl Pts',(-1.471223609415,-2.22889628422052,8.85933012996512));
#375123=CARTESIAN_POINT('',(-1.44260408658466,-2.24752552912784,8.85933012996512));
#375124=CARTESIAN_POINT('Origin',(-1.46197772366218,-2.24599038336614,8.84999761231047));
#375125=CARTESIAN_POINT('',(-1.44812530550984,-2.31885583959521,8.79610912703474));
#375126=CARTESIAN_POINT('Ctrl Pts',(-1.44260408658466,-2.24752552912784,
8.85933012996512));
#375127=CARTESIAN_POINT('Ctrl Pts',(-1.44308653039291,-2.25376059909534,
8.8538223528706));
#375128=CARTESIAN_POINT('Ctrl Pts',(-1.44356883061088,-2.25999321873981,
8.84831178811348));
#375129=CARTESIAN_POINT('Ctrl Pts',(-1.44405099020956,-2.2662234351211,
8.84279849653635));
#375130=CARTESIAN_POINT('Ctrl Pts',(-1.44541019000032,-2.28378631020434,
8.82725662040549));
#375131=CARTESIAN_POINT('Ctrl Pts',(-1.44676827405338,-2.30133011011268,
8.81169306718667));
#375132=CARTESIAN_POINT('Ctrl Pts',(-1.44812530550984,-2.31885583959521,
8.79610912703474));
#375133=CARTESIAN_POINT('',(-1.38608257609906,-2.35646650676757,8.79610912703474));
#375134=CARTESIAN_POINT('Origin',(0.,1.84795814293585E-15,8.79610912703474));
#375135=CARTESIAN_POINT('',(-1.32539494747702,-2.31857839805225,8.85933012996512));
#375136=CARTESIAN_POINT('Ctrl Pts',(-1.38608257609906,-2.35646650676757,
8.79610912703474));
#375137=CARTESIAN_POINT('Ctrl Pts',(-1.38079321481162,-2.35316408761611,
8.80163734024559));
#375138=CARTESIAN_POINT('Ctrl Pts',(-1.37550189900339,-2.34986049943078,
8.80716298614018));
#375139=CARTESIAN_POINT('Ctrl Pts',(-1.37020859108158,-2.34655571949919,
8.8126860086129));
#375140=CARTESIAN_POINT('Ctrl Pts',(-1.35528684506023,-2.33723960044392,
8.82825531609049));
#375141=CARTESIAN_POINT('Ctrl Pts',(-1.34034925836043,-2.32791400467276,
8.84380379913848));
#375142=CARTESIAN_POINT('Ctrl Pts',(-1.32539494747702,-2.31857839805225,
8.85933012996512));
#375143=CARTESIAN_POINT('',(-1.29564064670648,-2.33533570805445,8.85933012996512));
#375144=CARTESIAN_POINT('Origin',(-1.31507283569547,-2.33504498960374,8.84999761231046));
#375145=CARTESIAN_POINT('',(-1.29658037301229,-2.40687320845991,8.79610912703474));
#375146=CARTESIAN_POINT('Ctrl Pts',(-1.29564064670648,-2.33533570805445,
8.85933012996512));
#375147=CARTESIAN_POINT('Ctrl Pts',(-1.29572261697777,-2.34158887768291,
8.8538223528706));
#375148=CARTESIAN_POINT('Ctrl Pts',(-1.29580460094654,-2.34783959282294,
8.84831178811348));
#375149=CARTESIAN_POINT('Ctrl Pts',(-1.29588659856254,-2.35408790062804,
8.84279849653635));
#375150=CARTESIAN_POINT('Ctrl Pts',(-1.29611774846148,-2.3717017751304,
8.82725662040549));
#375151=CARTESIAN_POINT('Ctrl Pts',(-1.29634900706577,-2.38929654216429,
8.81169306718667));
#375152=CARTESIAN_POINT('Ctrl Pts',(-1.29658037301229,-2.40687320845991,
8.79610912703474));
#375153=CARTESIAN_POINT('',(-1.23225539332379,-2.44043150916128,8.79610912703474));
#375154=CARTESIAN_POINT('Origin',(0.,1.84795814293585E-15,8.79610912703474));
#375155=CARTESIAN_POINT('',(-1.17411995340352,-2.39873297591288,8.85933012996512));
#375156=CARTESIAN_POINT('Ctrl Pts',(-1.23225539332379,-2.44043150916128,
8.79610912703474));
#375157=CARTESIAN_POINT('Ctrl Pts',(-1.2271884863179,-2.4367969846429,8.80163734024559));
#375158=CARTESIAN_POINT('Ctrl Pts',(-1.22211970370725,-2.43316116826599,
8.80716298614018));
#375159=CARTESIAN_POINT('Ctrl Pts',(-1.21704900943148,-2.42952403495622,
8.8126860086129));
#375160=CARTESIAN_POINT('Ctrl Pts',(-1.20275480753492,-2.41927101731662,
8.82825531609049));
#375161=CARTESIAN_POINT('Ctrl Pts',(-1.18844540468156,-2.4090075275163,
8.84380379913848));
#375162=CARTESIAN_POINT('Ctrl Pts',(-1.17411995340352,-2.39873297591288,
8.85933012996512));
#375163=CARTESIAN_POINT('',(-1.14335314149693,-2.41354949162872,8.85933012996512));
#375164=CARTESIAN_POINT('Origin',(-1.16276403136464,-2.4145043951135,8.84999761231045));
#375165=CARTESIAN_POINT('',(-1.13970751364642,-2.48500021903835,8.79610912703474));
#375166=CARTESIAN_POINT('Ctrl Pts',(-1.14335314149693,-2.41354949162872,
8.85933012996512));
#375167=CARTESIAN_POINT('Ctrl Pts',(-1.14303430139784,-2.41979506530284,
8.8538223528706));
#375168=CARTESIAN_POINT('Ctrl Pts',(-1.14271563222769,-2.42603819040914,
8.84831178811348));
#375169=CARTESIAN_POINT('Ctrl Pts',(-1.14239713091521,-2.43227891400102,
8.84279849653635));
#375170=CARTESIAN_POINT('Ctrl Pts',(-1.14149928107782,-2.44987140873401,
8.82725662040549));
#375171=CARTESIAN_POINT('Ctrl Pts',(-1.14060276394214,-2.46744484222164,
8.81169306718667));
#375172=CARTESIAN_POINT('Ctrl Pts',(-1.13970751364642,-2.48500021903835,
8.79610912703474));
#375173=CARTESIAN_POINT('',(-1.07336460881941,-2.51436825501292,8.79610912703474));
#375174=CARTESIAN_POINT('Origin',(0.,1.84795814293585E-15,8.79610912703474));
#375175=CARTESIAN_POINT('',(-1.01802024859356,-2.46903064544887,8.85933012996512));
#375176=CARTESIAN_POINT('Ctrl Pts',(-1.07336460881941,-2.51436825501292,
8.79610912703474));
#375177=CARTESIAN_POINT('Ctrl Pts',(-1.0685409771028,-2.51041656016848,
8.80163734024559));
#375178=CARTESIAN_POINT('Ctrl Pts',(-1.06371555640473,-2.50646345594936,
8.80716298614018));
#375179=CARTESIAN_POINT('Ctrl Pts',(-1.05888831234543,-2.50250891502235,
8.8126860086129));
#375180=CARTESIAN_POINT('Ctrl Pts',(-1.04528039251535,-2.49136113064716,
8.82825531609049));
#375181=CARTESIAN_POINT('Ctrl Pts',(-1.03165797391411,-2.48020192169879,
8.84380379913848));
#375182=CARTESIAN_POINT('Ctrl Pts',(-1.01802024859356,-2.46903064544887,
8.85933012996512));
#375183=CARTESIAN_POINT('',(-0.986367352980499,-2.48184548263714,8.85933012996512));
#375184=CARTESIAN_POINT('Origin',(-1.00567718021682,-2.48404208415414,8.84999761231045));
#375185=CARTESIAN_POINT('',(-0.978151351640474,-2.5529158306859,8.79610912703474));
#375186=CARTESIAN_POINT('Ctrl Pts',(-0.986367352980499,-2.48184548263714,
8.85933012996512));
#375187=CARTESIAN_POINT('Ctrl Pts',(-0.985649012693377,-2.48805779595503,
8.8538223528706));
#375188=CARTESIAN_POINT('Ctrl Pts',(-0.984930999864287,-2.49426767668739,
8.84831178811348));
#375189=CARTESIAN_POINT('Ctrl Pts',(-0.984213308413545,-2.50047517159418,
8.84279849653635));
#375190=CARTESIAN_POINT('Ctrl Pts',(-0.982190148297381,-2.51797399522336,
8.82725662040549));
#375191=CARTESIAN_POINT('Ctrl Pts',(-0.98016953940294,-2.53545388215705,
8.81169306718667));
#375192=CARTESIAN_POINT('Ctrl Pts',(-0.978151351640474,-2.5529158306859,
8.79610912703474));
#375193=CARTESIAN_POINT('',(-0.910063138901394,-2.57797292237442,8.79610912703474));
#375194=CARTESIAN_POINT('Origin',(0.,1.84795814293585E-15,8.79610912703474));
#375195=CARTESIAN_POINT('',(-0.857737280217463,-2.5291825384573,8.85933012996512));
#375196=CARTESIAN_POINT('Ctrl Pts',(-0.910063138901394,-2.57797292237442,
8.79610912703474));
#375197=CARTESIAN_POINT('Ctrl Pts',(-0.905502603811463,-2.57372029556567,
8.80163734024559));
#375198=CARTESIAN_POINT('Ctrl Pts',(-0.900940373714666,-2.56946614765751,
8.80716298614018));
#375199=CARTESIAN_POINT('Ctrl Pts',(-0.896376416053125,-2.56521044917018,
8.8126860086129));
#375200=CARTESIAN_POINT('Ctrl Pts',(-0.883510696150999,-2.55321370669659,
8.82825531609049));
#375201=CARTESIAN_POINT('Ctrl Pts',(-0.870631239241901,-2.54120463418337,
8.84380379913848));
#375202=CARTESIAN_POINT('Ctrl Pts',(-0.857737280217463,-2.5291825384573,
8.85933012996512));
#375203=CARTESIAN_POINT('',(-0.825328369435533,-2.53994303820322,8.85933012996512));
#375204=CARTESIAN_POINT('Origin',(-0.844457785818422,-2.54337231144563,
8.84999761231047));
#375205=CARTESIAN_POINT('',(-0.812575755917834,-2.61034096358643,8.79610912703474));
#375206=CARTESIAN_POINT('Ctrl Pts',(-0.825328369435533,-2.53994303820322,
8.85933012996512));
#375207=CARTESIAN_POINT('Ctrl Pts',(-0.824213480774706,-2.54609656343692,
8.8538223528706));
#375208=CARTESIAN_POINT('Ctrl Pts',(-0.823099074755404,-2.5522476820634,
8.84831178811348));
#375209=CARTESIAN_POINT('Ctrl Pts',(-0.821985142314512,-2.55839644035702,
8.84279849653635));
#375210=CARTESIAN_POINT('Ctrl Pts',(-0.818844985518465,-2.57572968646262,
8.82725662040549));
#375211=CARTESIAN_POINT('Ctrl Pts',(-0.815708587980628,-2.59304419823752,
8.81169306718667));
#375212=CARTESIAN_POINT('Ctrl Pts',(-0.812575755917834,-2.61034096358643,
8.79610912703474));
#375213=CARTESIAN_POINT('',(-0.743022024337704,-2.63098414602442,8.79610912703474));
#375214=CARTESIAN_POINT('Origin',(0.,1.84795814293585E-15,8.79610912703474));
#375215=CARTESIAN_POINT('',(-0.693929685372884,-2.57894147790725,8.85933012996512));
#375216=CARTESIAN_POINT('Ctrl Pts',(-0.743022024337704,-2.63098414602442,
8.79610912703474));
#375217=CARTESIAN_POINT('Ctrl Pts',(-0.738743326091364,-2.6264480622071,
8.80163734024559));
#375218=CARTESIAN_POINT('Ctrl Pts',(-0.734463033777905,-2.62191035181617,
8.80716298614018));
#375219=CARTESIAN_POINT('Ctrl Pts',(-0.730181116795117,-2.61737098334645,
8.8126860086129));
#375220=CARTESIAN_POINT('Ctrl Pts',(-0.718110464823709,-2.60457457996258,
8.82825531609049));
#375221=CARTESIAN_POINT('Ctrl Pts',(-0.706026894057835,-2.59176499173941,
8.84380379913848));
#375222=CARTESIAN_POINT('Ctrl Pts',(-0.693929685372884,-2.57894147790725,
8.85933012996512));
#375223=CARTESIAN_POINT('',(-0.660897934588176,-2.58760342300926,8.85933012996512));
#375224=CARTESIAN_POINT('Origin',(-0.679768333242473,-2.59225127635776,
8.84999761231045));
#375225=CARTESIAN_POINT('',(-0.643661112117175,-2.6570396455512,8.79610912703474));
#375226=CARTESIAN_POINT('Ctrl Pts',(-0.660897934588176,-2.58760342300926,
8.85933012996512));
#375227=CARTESIAN_POINT('Ctrl Pts',(-0.659391078870295,-2.59367287400364,
8.8538223528706));
#375228=CARTESIAN_POINT('Ctrl Pts',(-0.657884858994153,-2.59973995425839,
8.84831178811348));
#375229=CARTESIAN_POINT('Ctrl Pts',(-0.656379262950449,-2.60580470937212,
8.84279849653635));
#375230=CARTESIAN_POINT('Ctrl Pts',(-0.652135013052355,-2.62290115192791,
8.82725662040549));
#375231=CARTESIAN_POINT('Ctrl Pts',(-0.64789571500136,-2.6399791395012,
8.81169306718667));
#375232=CARTESIAN_POINT('Ctrl Pts',(-0.643661112117175,-2.6570396455512,
8.79610912703474));
#375233=CARTESIAN_POINT('',(-0.572927672898287,-2.67318409147408,8.79610912703474));
#375234=CARTESIAN_POINT('Origin',(0.,1.84795814293585E-15,8.79610912703474));
#375235=CARTESIAN_POINT('',(-0.527270584603657,-2.61810299364327,8.85933012996512));
#375236=CARTESIAN_POINT('Ctrl Pts',(-0.572927672898287,-2.67318409147408,
8.79610912703474));
#375237=CARTESIAN_POINT('Ctrl Pts',(-0.56894839358441,-2.66838319038958,
8.80163734024559));
#375238=CARTESIAN_POINT('Ctrl Pts',(-0.564967627693525,-2.66358056394121,
8.80716298614018));
#375239=CARTESIAN_POINT('Ctrl Pts',(-0.56098534670484,-2.65877617872783,
8.8126860086129));
#375240=CARTESIAN_POINT('Ctrl Pts',(-0.549759363562247,-2.64523269760001,
8.82825531609049));
#375241=CARTESIAN_POINT('Ctrl Pts',(-0.538521332923791,-2.63167523101254,
8.84380379913848));
#375242=CARTESIAN_POINT('Ctrl Pts',(-0.527270584603657,-2.61810299364327,
8.85933012996512));
#375243=CARTESIAN_POINT('',(-0.493751728365434,-2.62463079031095,8.85933012996512));
#375244=CARTESIAN_POINT('Origin',(-0.512285566775374,-2.63047812473917,
8.84999761231046));
#375245=CARTESIAN_POINT('',(-0.472101526741951,-2.69281998167918,8.79610912703474));
#375246=CARTESIAN_POINT('Ctrl Pts',(-0.493751728365434,-2.62463079031095,
8.85933012996512));
#375247=CARTESIAN_POINT('Ctrl Pts',(-0.491859097583863,-2.63059122639,8.8538223528706));
#375248=CARTESIAN_POINT('Ctrl Pts',(-0.489967253231435,-2.63654933733887,
8.84831178811348));
#375249=CARTESIAN_POINT('Ctrl Pts',(-0.488076180402012,-2.64250516789305,
8.84279849653635));
#375250=CARTESIAN_POINT('Ctrl Pts',(-0.482745277935091,-2.6592945539494,
8.82725662040549));
#375251=CARTESIAN_POINT('Ctrl Pts',(-0.477420499555957,-2.67606584020692,
8.81169306718667));
#375252=CARTESIAN_POINT('Ctrl Pts',(-0.472101526741951,-2.69281998167918,
8.79610912703474));
#375253=CARTESIAN_POINT('',(-0.40047903875833,-2.70439935009569,8.79610912703474));
#375254=CARTESIAN_POINT('Origin',(0.,1.84795814293585E-15,8.79610912703474));
#375255=CARTESIAN_POINT('',(-0.358444815903108,-2.64650616259708,8.85933012996512));
#375256=CARTESIAN_POINT('Ctrl Pts',(-0.40047903875833,-2.70439935009569,
8.79610912703474));
#375257=CARTESIAN_POINT('Ctrl Pts',(-0.396815530089169,-2.69935335967635,
8.80163734024559));
#375258=CARTESIAN_POINT('Ctrl Pts',(-0.393150648441775,-2.69430555219278,
8.80716298614018));
#375259=CARTESIAN_POINT('Ctrl Pts',(-0.389484367493974,-2.68925589248512,
8.8126860086129));
#375260=CARTESIAN_POINT('Ctrl Pts',(-0.379149183152894,-2.67502098668236,
8.82825531609049));
#375261=CARTESIAN_POINT('Ctrl Pts',(-0.3688028721203,-2.66077135226888,
8.84380379913848));
#375262=CARTESIAN_POINT('Ctrl Pts',(-0.358444815903108,-2.64650616259708,
8.85933012996512));
#375263=CARTESIAN_POINT('',(-0.324576590381425,-2.65087298671372,8.85933012996512));
#375264=CARTESIAN_POINT('Origin',(-0.342697709029489,-2.65789577427027,
8.84999761231044));
#375265=CARTESIAN_POINT('',(-0.298601974927885,-2.71753494289437,8.79610912703474));
#375266=CARTESIAN_POINT('Ctrl Pts',(-0.324576590381425,-2.65087298671372,
8.85933012996512));
#375267=CARTESIAN_POINT('Ctrl Pts',(-0.322305961762013,-2.65669991516707,
8.8538223528706));
#375268=CARTESIAN_POINT('Ctrl Pts',(-0.320036266927543,-2.66252457365416,
8.84831178811348));
#375269=CARTESIAN_POINT('Ctrl Pts',(-0.317767488136291,-2.66834700586353,
8.84279849653635));
#375270=CARTESIAN_POINT('Ctrl Pts',(-0.311371838922255,-2.68476034423181,
8.82725662040549));
#375271=CARTESIAN_POINT('Ctrl Pts',(-0.304983460871502,-2.70115601236091,
8.81169306718667));
#375272=CARTESIAN_POINT('Ctrl Pts',(-0.298601974927885,-2.71753494289437,
8.79610912703474));
#375273=CARTESIAN_POINT('',(-0.22638475034563,-2.7245016516959,8.79610912703474));
#375274=CARTESIAN_POINT('Origin',(0.,1.84795814293585E-15,8.79610912703474));
#375275=CARTESIAN_POINT('',(-0.188146120567841,-2.66403427005499,8.85933012996512));
#375276=CARTESIAN_POINT('Ctrl Pts',(-0.22638475034563,-2.7245016516959,
8.79610912703474));
#375277=CARTESIAN_POINT('Ctrl Pts',(-0.223052066464128,-2.71923130699873,
8.80163734024559));
#375278=CARTESIAN_POINT('Ctrl Pts',(-0.219718128845028,-2.71395906100366,
8.80716298614018));
#375279=CARTESIAN_POINT('Ctrl Pts',(-0.216382913472939,-2.70868487693661,
8.8126860086129));
#375280=CARTESIAN_POINT('Ctrl Pts',(-0.206980997422721,-2.69381704074023,
8.82825531609049));
#375281=CARTESIAN_POINT('Ctrl Pts',(-0.197568921207299,-2.67893379330507,
8.84380379913848));
#375282=CARTESIAN_POINT('Ctrl Pts',(-0.188146120567841,-2.66403427005499,
8.85933012996512));
#375283=CARTESIAN_POINT('',(-0.154067697566079,-2.66622217740361,8.85933012996512));
#375284=CARTESIAN_POINT('Origin',(-0.171701632888769,-2.674391559948,8.84999761231045));
#375285=CARTESIAN_POINT('',(-0.123875403548917,-2.7310829701198,8.79610912703474));
#375286=CARTESIAN_POINT('Ctrl Pts',(-0.154067697566079,-2.66622217740361,
8.85933012996512));
#375287=CARTESIAN_POINT('Ctrl Pts',(-0.151428401608871,-2.67189165413237,
8.8538223528706));
#375288=CARTESIAN_POINT('Ctrl Pts',(-0.148790182955282,-2.67755892538658,
8.84831178811348));
#375289=CARTESIAN_POINT('Ctrl Pts',(-0.146153021100905,-2.68322403362827,
8.84279849653635));
#375290=CARTESIAN_POINT('Ctrl Pts',(-0.138718906234236,-2.69919387838049,
8.82725662040549));
#375291=CARTESIAN_POINT('Ctrl Pts',(-0.131293179727579,-2.71514655506395,
8.81169306718667));
#375292=CARTESIAN_POINT('Ctrl Pts',(-0.123875403548917,-2.7310829701198,
8.79610912703474));
#375293=CARTESIAN_POINT('',(-0.0513601984344042,-2.73340839160553,8.79610912703474));
#375294=CARTESIAN_POINT('Origin',(0.,1.84795814293585E-15,8.79610912703474));
#375295=CARTESIAN_POINT('',(-0.0170742924659647,-2.67061528926368,8.85933012996512));
#375296=CARTESIAN_POINT('Ctrl Pts',(-0.0513601984344042,-2.73340839160553,
8.79610912703474));
#375297=CARTESIAN_POINT('Ctrl Pts',(-0.0483720340534879,-2.72793534960737,
8.80163734024559));
#375298=CARTESIAN_POINT('Ctrl Pts',(-0.045382740327487,-2.72246032989048,
8.80716298614018));
#375299=CARTESIAN_POINT('Ctrl Pts',(-0.0423922956464754,-2.71698329421768,
8.8126860086129));
#375300=CARTESIAN_POINT('Ctrl Pts',(-0.0339622823768732,-2.70154362275576,
8.82825531609049));
#375301=CARTESIAN_POINT('Ctrl Pts',(-0.0255231172186754,-2.68608792075508,
8.84380379913848));
#375302=CARTESIAN_POINT('Ctrl Pts',(-0.0170742924659647,-2.67061528926368,
8.85933012996512));
#375303=CARTESIAN_POINT('',(0.0170742924659647,-2.67061528926368,8.85933012996512));
#375304=CARTESIAN_POINT('Origin',(2.09135199175786E-9,-2.67989769705071,
8.84999761231045));
#375305=CARTESIAN_POINT('',(0.0513601984344042,-2.73340839160553,8.79610912703474));
#375306=CARTESIAN_POINT('Ctrl Pts',(0.0170742924659647,-2.67061528926368,
8.85933012996512));
#375307=CARTESIAN_POINT('Ctrl Pts',(0.0200714103277523,-2.67610401717189,
8.8538223528706));
#375308=CARTESIAN_POINT('Ctrl Pts',(0.0230673117941167,-2.68159061315999,
8.84831178811348));
#375309=CARTESIAN_POINT('Ctrl Pts',(0.0260620200478886,-2.68707511828909,
8.84279849653635));
#375310=CARTESIAN_POINT('Ctrl Pts',(0.0345040521945901,-2.70253584590764,
8.82725662040549));
#375311=CARTESIAN_POINT('Ctrl Pts',(0.0429366132541237,-2.71797997817513,
8.81169306718667));
#375312=CARTESIAN_POINT('Ctrl Pts',(0.0513601984344042,-2.73340839160553,
8.79610912703474));
#375313=CARTESIAN_POINT('',(0.123875403548956,-2.73108297011979,8.79610912703474));
#375314=CARTESIAN_POINT('Origin',(0.,1.84795814293585E-15,8.79610912703474));
#375315=CARTESIAN_POINT('',(0.154067697566117,-2.6662221774036,8.85933012996512));
#375316=CARTESIAN_POINT('Ctrl Pts',(0.123875403548956,-2.73108297011979,
8.79610912703474));
#375317=CARTESIAN_POINT('Ctrl Pts',(0.126506769420886,-2.72542972072417,
8.80163734024559));
#375318=CARTESIAN_POINT('Ctrl Pts',(0.129139135604666,-2.71977442531588,
8.80716298614018));
#375319=CARTESIAN_POINT('Ctrl Pts',(0.131772521215958,-2.71411704435172,
8.8126860086129));
#375320=CARTESIAN_POINT('Ctrl Pts',(0.139195990972187,-2.6981689825461,
8.82825531609049));
#375321=CARTESIAN_POINT('Ctrl Pts',(0.146627566733329,-2.68220433677466,
8.84380379913848));
#375322=CARTESIAN_POINT('Ctrl Pts',(0.154067697566117,-2.6662221774036,
8.85933012996512));
#375323=CARTESIAN_POINT('',(0.18814612056788,-2.66403427005499,8.85933012996512));
#375324=CARTESIAN_POINT('Origin',(0.171701637062919,-2.67439155968,8.84999761231045));
#375325=CARTESIAN_POINT('',(0.226384750345669,-2.7245016516959,8.79610912703474));
#375326=CARTESIAN_POINT('Ctrl Pts',(0.18814612056788,-2.66403427005499,
8.85933012996512));
#375327=CARTESIAN_POINT('Ctrl Pts',(0.191488744534073,-2.66931969478233,
8.8538223528706));
#375328=CARTESIAN_POINT('Ctrl Pts',(0.194830018011469,-2.67460306990455,
8.84831178811348));
#375329=CARTESIAN_POINT('Ctrl Pts',(0.198169966766059,-2.67988443491305,
8.84279849653635));
#375330=CARTESIAN_POINT('Ctrl Pts',(0.207585226071892,-2.69477251395182,
8.82725662040549));
#375331=CARTESIAN_POINT('Ctrl Pts',(0.216989970482129,-2.70964463855111,
8.81169306718667));
#375332=CARTESIAN_POINT('Ctrl Pts',(0.226384750345669,-2.7245016516959,
8.79610912703474));
#375333=CARTESIAN_POINT('',(0.298601974927924,-2.71753494289437,8.79610912703474));
#375334=CARTESIAN_POINT('Origin',(0.,1.84795814293585E-15,8.79610912703474));
#375335=CARTESIAN_POINT('',(0.324576590381463,-2.65087298671371,8.85933012996512));
#375336=CARTESIAN_POINT('Ctrl Pts',(0.298601974927924,-2.71753494289437,
8.79610912703474));
#375337=CARTESIAN_POINT('Ctrl Pts',(0.300865729444074,-2.71172471651568,
8.80163734024559));
#375338=CARTESIAN_POINT('Ctrl Pts',(0.303130351128344,-2.70591238423786,
8.80716298614018));
#375339=CARTESIAN_POINT('Ctrl Pts',(0.305395856523578,-2.70009790537424,
8.8126860086129));
#375340=CARTESIAN_POINT('Ctrl Pts',(0.311782278136876,-2.68370698723172,
8.82825531609049));
#375341=CARTESIAN_POINT('Ctrl Pts',(0.318175726562094,-2.6672989998434,
8.84380379913848));
#375342=CARTESIAN_POINT('Ctrl Pts',(0.324576590381463,-2.65087298671371,
8.85933012996512));
#375343=CARTESIAN_POINT('',(0.358444815903146,-2.64650616259708,8.85933012996512));
#375344=CARTESIAN_POINT('Origin',(0.342697713177886,-2.65789577373536,8.84999761231047));
#375345=CARTESIAN_POINT('',(0.400479038758368,-2.70439935009568,8.79610912703474));
#375346=CARTESIAN_POINT('Ctrl Pts',(0.358444815903146,-2.64650616259708,
8.85933012996512));
#375347=CARTESIAN_POINT('Ctrl Pts',(0.362119210414878,-2.65156656519963,
8.8538223528706));
#375348=CARTESIAN_POINT('Ctrl Pts',(0.365792125893886,-2.65662500893431,
8.84831178811348));
#375349=CARTESIAN_POINT('Ctrl Pts',(0.369463590583444,-2.66168153156055,
8.84279849653635));
#375350=CARTESIAN_POINT('Ctrl Pts',(0.379813387728354,-2.67593578370929,
8.82725662040549));
#375351=CARTESIAN_POINT('Ctrl Pts',(0.390151669377202,-2.69017478789034,
8.81169306718667));
#375352=CARTESIAN_POINT('Ctrl Pts',(0.400479038758368,-2.70439935009568,
8.79610912703474));
#375353=CARTESIAN_POINT('',(0.47210152674199,-2.69281998167918,8.79610912703474));
#375354=CARTESIAN_POINT('Origin',(0.,1.84795814293585E-15,8.79610912703474));
#375355=CARTESIAN_POINT('',(0.493751728365472,-2.62463079031094,8.85933012996512));
#375356=CARTESIAN_POINT('Ctrl Pts',(0.47210152674199,-2.69281998167918,
8.79610912703474));
#375357=CARTESIAN_POINT('Ctrl Pts',(0.473988367649479,-2.6868766537839,
8.80163734024559));
#375358=CARTESIAN_POINT('Ctrl Pts',(0.475875939017978,-2.68093116875663,
8.80716298614018));
#375359=CARTESIAN_POINT('Ctrl Pts',(0.477764254749538,-2.67498348493439,
8.8126860086129));
#375360=CARTESIAN_POINT('Ctrl Pts',(0.483087385043613,-2.65821706425346,
8.82825531609049));
#375361=CARTESIAN_POINT('Ctrl Pts',(0.488416434081935,-2.64143315918795,
8.84380379913848));
#375362=CARTESIAN_POINT('Ctrl Pts',(0.493751728365472,-2.62463079031094,
8.85933012996512));
#375363=CARTESIAN_POINT('',(0.527270584603695,-2.61810299364326,8.85933012996512));
#375364=CARTESIAN_POINT('Origin',(0.512285570880988,-2.63047812393962,8.84999761231044));
#375365=CARTESIAN_POINT('',(0.572927672898325,-2.67318409147408,8.79610912703474));
#375366=CARTESIAN_POINT('Ctrl Pts',(0.527270584603695,-2.61810299364326,
8.85933012996512));
#375367=CARTESIAN_POINT('Ctrl Pts',(0.531261650785761,-2.62291757984128,
8.8538223528706));
#375368=CARTESIAN_POINT('Ctrl Pts',(0.53525111546884,-2.62773030595808,
8.84831178811348));
#375369=CARTESIAN_POINT('Ctrl Pts',(0.53923900925743,-2.63254120786596,
8.84279849653635));
#375370=CARTESIAN_POINT('Ctrl Pts',(0.550480814704924,-2.64610305934507,
8.82725662040549));
#375371=CARTESIAN_POINT('Ctrl Pts',(0.561710151375533,-2.65965043198543,
8.81169306718667));
#375372=CARTESIAN_POINT('Ctrl Pts',(0.572927672898325,-2.67318409147408,
8.79610912703474));
#375373=CARTESIAN_POINT('',(0.643661112117213,-2.65703964555119,8.79610912703474));
#375374=CARTESIAN_POINT('Origin',(0.,1.84795814293585E-15,8.79610912703474));
#375375=CARTESIAN_POINT('',(0.660897934588214,-2.58760342300925,8.85933012996512));
#375376=CARTESIAN_POINT('Ctrl Pts',(0.643661112117213,-2.65703964555119,
8.79610912703474));
#375377=CARTESIAN_POINT('Ctrl Pts',(0.645163285982027,-2.65098763854848,
8.80163734024559));
#375378=CARTESIAN_POINT('Ctrl Pts',(0.646666050599119,-2.64493343204504,
8.80716298614018));
#375379=CARTESIAN_POINT('Ctrl Pts',(0.64816941717262,-2.63887698357279,
8.8126860086129));
#375380=CARTESIAN_POINT('Ctrl Pts',(0.652407382263286,-2.62180395717242,
8.82825531609049));
#375381=CARTESIAN_POINT('Ctrl Pts',(0.656650133709137,-2.60471310309575,
8.84380379913848));
#375382=CARTESIAN_POINT('Ctrl Pts',(0.660897934588214,-2.58760342300925,
8.85933012996512));
#375383=CARTESIAN_POINT('',(0.693929685372921,-2.57894147790724,8.85933012996512));
#375384=CARTESIAN_POINT('Origin',(0.679768337288427,-2.59225127529681,8.84999761231044));
#375385=CARTESIAN_POINT('',(0.743022024337742,-2.63098414602441,8.79610912703474));
#375386=CARTESIAN_POINT('Ctrl Pts',(0.693929685372921,-2.57894147790724,
8.85933012996512));
#375387=CARTESIAN_POINT('Ctrl Pts',(0.698221023078299,-2.58349046353331,
8.8538223528706));
#375388=CARTESIAN_POINT('Ctrl Pts',(0.702510643399328,-2.58803769550829,
8.84831178811348));
#375389=CARTESIAN_POINT('Ctrl Pts',(0.706798579175972,-2.59258320766993,
8.84279849653635));
#375390=CARTESIAN_POINT('Ctrl Pts',(0.718886197936108,-2.60539692992268,
8.82725662040549));
#375391=CARTESIAN_POINT('Ctrl Pts',(0.730960445875413,-2.61819700196228,
8.81169306718667));
#375392=CARTESIAN_POINT('Ctrl Pts',(0.743022024337742,-2.63098414602441,
8.79610912703474));
#375393=CARTESIAN_POINT('',(0.812575755917872,-2.61034096358642,8.79610912703474));
#375394=CARTESIAN_POINT('Origin',(0.,1.84795814293585E-15,8.79610912703474));
#375395=CARTESIAN_POINT('',(0.82532836943557,-2.53994303820321,8.85933012996512));
#375396=CARTESIAN_POINT('Ctrl Pts',(0.812575755917872,-2.61034096358642,
8.79610912703474));
#375397=CARTESIAN_POINT('Ctrl Pts',(0.813687089985383,-2.6042051464712,
8.80163734024559));
#375398=CARTESIAN_POINT('Ctrl Pts',(0.814798872668915,-2.59806709652474,
8.80716298614018));
#375399=CARTESIAN_POINT('Ctrl Pts',(0.815911112428636,-2.59192677064835,
8.8126860086129));
#375400=CARTESIAN_POINT('Ctrl Pts',(0.819046497608294,-2.57461729525616,
8.82825531609049));
#375401=CARTESIAN_POINT('Ctrl Pts',(0.822185517085916,-2.55728972215373,
8.84380379913848));
#375402=CARTESIAN_POINT('Ctrl Pts',(0.82532836943557,-2.53994303820321,
8.85933012996512));
#375403=CARTESIAN_POINT('',(0.857737280217499,-2.52918253845728,8.85933012996512));
#375404=CARTESIAN_POINT('Origin',(0.844457789788073,-2.5433723101276,8.84999761231049));
#375405=CARTESIAN_POINT('',(0.910063138901431,-2.57797292237441,8.79610912703474));
#375406=CARTESIAN_POINT('Ctrl Pts',(0.857737280217499,-2.52918253845728,
8.85933012996512));
#375407=CARTESIAN_POINT('Ctrl Pts',(0.862311255419068,-2.53344723075371,
8.8538223528706));
#375408=CARTESIAN_POINT('Ctrl Pts',(0.866883404408027,-2.53771028303531,
8.84831178811348));
#375409=CARTESIAN_POINT('Ctrl Pts',(0.871453762124861,-2.54197172696624,
8.84279849653635));
#375410=CARTESIAN_POINT('Ctrl Pts',(0.884337523579365,-2.55398466565934,
8.82725662040549));
#375411=CARTESIAN_POINT('Ctrl Pts',(0.897207067112666,-2.56598483885656,
8.81169306718667));
#375412=CARTESIAN_POINT('Ctrl Pts',(0.910063138901431,-2.57797292237441,
8.79610912703474));
#375413=CARTESIAN_POINT('',(0.97815135164051,-2.55291583068589,8.79610912703474));
#375414=CARTESIAN_POINT('Origin',(0.,1.84795814293585E-15,8.79610912703474));
#375415=CARTESIAN_POINT('',(0.986367352980535,-2.48184548263713,8.85933012996512));
#375416=CARTESIAN_POINT('Ctrl Pts',(0.97815135164051,-2.55291583068589,
8.79610912703474));
#375417=CARTESIAN_POINT('Ctrl Pts',(0.978867279200656,-2.54672141684682,
8.80163734024559));
#375418=CARTESIAN_POINT('Ctrl Pts',(0.979583511397104,-2.54052474602117,
8.80716298614018));
#375419=CARTESIAN_POINT('Ctrl Pts',(0.980300053911298,-2.53432577465677,
8.8126860086129));
#375420=CARTESIAN_POINT('Ctrl Pts',(0.982319975209707,-2.51685097862002,
8.82825531609049));
#375421=CARTESIAN_POINT('Ctrl Pts',(0.984342363814749,-2.49935788920645,
8.84380379913848));
#375422=CARTESIAN_POINT('Ctrl Pts',(0.986367352980535,-2.48184548263713,
8.85933012996512));
#375423=CARTESIAN_POINT('',(1.01802024859359,-2.46903064544885,8.85933012996512));
#375424=CARTESIAN_POINT('Origin',(1.00567718409387,-2.48404208258446,8.84999761231049));
#375425=CARTESIAN_POINT('',(1.07336460881944,-2.51436825501291,8.79610912703474));
#375426=CARTESIAN_POINT('Ctrl Pts',(1.01802024859359,-2.46903064544885,
8.85933012996512));
#375427=CARTESIAN_POINT('Ctrl Pts',(1.02285806584614,-2.47299351988022,
8.8538223528706));
#375428=CARTESIAN_POINT('Ctrl Pts',(1.02769395556211,-2.47695487467219,
8.84831178811348));
#375429=CARTESIAN_POINT('Ctrl Pts',(1.03252795463893,-2.48091473918521,
8.84279849653635));
#375430=CARTESIAN_POINT('Ctrl Pts',(1.04615491664843,-2.49207753057682,
8.82725662040549));
#375431=CARTESIAN_POINT('Ctrl Pts',(1.05976687206084,-2.50322849364596,
8.81169306718667));
#375432=CARTESIAN_POINT('Ctrl Pts',(1.07336460881944,-2.51436825501291,
8.79610912703474));
#375433=CARTESIAN_POINT('',(1.13970751364645,-2.48500021903834,8.79610912703474));
#375434=CARTESIAN_POINT('Origin',(0.,1.84795814293585E-15,8.79610912703474));
#375435=CARTESIAN_POINT('',(1.14335314149697,-2.4135494916287,8.85933012996512));
#375436=CARTESIAN_POINT('Ctrl Pts',(1.13970751364645,-2.48500021903834,
8.79610912703474));
#375437=CARTESIAN_POINT('Ctrl Pts',(1.14002509279932,-2.47877266265058,
8.80163734024559));
#375438=CARTESIAN_POINT('Ctrl Pts',(1.14034283135696,-2.47254283439536,
8.80716298614018));
#375439=CARTESIAN_POINT('Ctrl Pts',(1.14066073219874,-2.46631069044594,
8.8126860086129));
#375440=CARTESIAN_POINT('Ctrl Pts',(1.14155688932601,-2.44874238144989,
8.82825531609049));
#375441=CARTESIAN_POINT('Ctrl Pts',(1.14245433662989,-2.43115565858184,
8.84380379913848));
#375442=CARTESIAN_POINT('Ctrl Pts',(1.14335314149697,-2.4135494916287,8.85933012996512));
#375443=CARTESIAN_POINT('',(1.17411995340356,-2.39873297591286,8.85933012996512));
#375444=CARTESIAN_POINT('Origin',(1.16276403513316,-2.41450439329867,8.84999761231046));
#375445=CARTESIAN_POINT('',(1.23225539332383,-2.44043150916126,8.79610912703474));
#375446=CARTESIAN_POINT('Ctrl Pts',(1.17411995340356,-2.39873297591286,
8.85933012996512));
#375447=CARTESIAN_POINT('Ctrl Pts',(1.17920173307828,-2.40237774817809,
8.8538223528706));
#375448=CARTESIAN_POINT('Ctrl Pts',(1.18428149181312,-2.40602112742388,
8.84831178811348));
#375449=CARTESIAN_POINT('Ctrl Pts',(1.18935926831084,-2.40966314058634,
8.84279849653635));
#375450=CARTESIAN_POINT('Ctrl Pts',(1.20367343476546,-2.4199299143722,8.82725662040549));
#375451=CARTESIAN_POINT('Ctrl Pts',(1.21797186761244,-2.43018584561414,
8.81169306718667));
#375452=CARTESIAN_POINT('Ctrl Pts',(1.23225539332383,-2.44043150916126,
8.79610912703474));
#375453=CARTESIAN_POINT('',(1.29658037301232,-2.40687320845989,8.79610912703474));
#375454=CARTESIAN_POINT('Origin',(0.,1.84795814293585E-15,8.79610912703474));
#375455=CARTESIAN_POINT('',(1.29564064670651,-2.33533570805443,8.85933012996512));
#375456=CARTESIAN_POINT('Ctrl Pts',(1.29658037301232,-2.40687320845989,
8.79610912703474));
#375457=CARTESIAN_POINT('Ctrl Pts',(1.29649829875706,-2.40063809988845,
8.80163734024559));
#375458=CARTESIAN_POINT('Ctrl Pts',(1.29641623802,-2.39440071390423,8.80716298614018));
#375459=CARTESIAN_POINT('Ctrl Pts',(1.29633419086661,-2.3881610065861,8.8126860086129));
#375460=CARTESIAN_POINT('Ctrl Pts',(1.29610290132089,-2.37057137658079,
8.82825531609049));
#375461=CARTESIAN_POINT('Ctrl Pts',(1.29587171952014,-2.35296328787486,
8.84380379913848));
#375462=CARTESIAN_POINT('Ctrl Pts',(1.29564064670651,-2.33533570805443,
8.85933012996512));
#375463=CARTESIAN_POINT('',(1.32539494747705,-2.31857839805223,8.85933012996512));
#375464=CARTESIAN_POINT('Origin',(1.31507283933998,-2.33504498755122,8.84999761231044));
#375465=CARTESIAN_POINT('',(1.38608257609909,-2.35646650676755,8.79610912703474));
#375466=CARTESIAN_POINT('Ctrl Pts',(1.32539494747705,-2.31857839805223,
8.85933012996512));
#375467=CARTESIAN_POINT('Ctrl Pts',(1.33069980745122,-2.32189009100029,
8.8538223528706));
#375468=CARTESIAN_POINT('Ctrl Pts',(1.33600256138669,-2.32520052327308,
8.84831178811348));
#375469=CARTESIAN_POINT('Ctrl Pts',(1.3413032496325,-2.32850971927166,8.84279849653635));
#375470=CARTESIAN_POINT('Ctrl Pts',(1.3562458005519,-2.33783828707609,8.82725662040549));
#375471=CARTESIAN_POINT('Ctrl Pts',(1.37117195550587,-2.34715704266946,
8.81169306718667));
#375472=CARTESIAN_POINT('Ctrl Pts',(1.38608257609909,-2.35646650676755,
8.79610912703474));
#375473=CARTESIAN_POINT('',(1.44812530550987,-2.31885583959519,8.79610912703474));
#375474=CARTESIAN_POINT('Origin',(0.,1.84795814293585E-15,8.79610912703474));
#375475=CARTESIAN_POINT('',(1.44260408658469,-2.24752552912782,8.85933012996512));
#375476=CARTESIAN_POINT('Ctrl Pts',(1.44812530550987,-2.31885583959519,
8.79610912703474));
#375477=CARTESIAN_POINT('Ctrl Pts',(1.44764391510719,-2.31263880023861,
8.80163734024559));
#375478=CARTESIAN_POINT('Ctrl Pts',(1.4471623922806,-2.30641948728234,8.80716298614018));
#375479=CARTESIAN_POINT('Ctrl Pts',(1.4466807342814,-2.30019785689126,8.8126860086129));
#375480=CARTESIAN_POINT('Ctrl Pts',(1.44532294848104,-2.28265918543935,
8.82825531609049));
#375481=CARTESIAN_POINT('Ctrl Pts',(1.44396408755126,-2.26510208630896,
8.84380379913848));
#375482=CARTESIAN_POINT('Ctrl Pts',(1.44260408658469,-2.24752552912782,
8.85933012996512));
#375483=CARTESIAN_POINT('',(1.47122360941503,-2.2288962842205,8.85933012996512));
#375484=CARTESIAN_POINT('Origin',(1.46197772716769,-2.24599038108432,8.84999761231046));
#375485=CARTESIAN_POINT('',(1.53421404825539,-2.26281827803705,8.79610912703474));
#375486=CARTESIAN_POINT('Ctrl Pts',(1.47122360941503,-2.2288962842205,8.85933012996512));
#375487=CARTESIAN_POINT('Ctrl Pts',(1.47672975088113,-2.23186128939471,
8.8538223528706));
#375488=CARTESIAN_POINT('Ctrl Pts',(1.48223370986387,-2.2348251714182,8.84831178811348));
#375489=CARTESIAN_POINT('Ctrl Pts',(1.48773552819277,-2.23778795205674,
8.84279849653635));
#375490=CARTESIAN_POINT('Ctrl Pts',(1.50324506143006,-2.24613998079365,
8.82725662040549));
#375491=CARTESIAN_POINT('Ctrl Pts',(1.51873760371866,-2.25448326797285,
8.81169306718667));
#375492=CARTESIAN_POINT('Ctrl Pts',(1.53421404825539,-2.26281827803705,
8.79610912703474));
#375493=CARTESIAN_POINT('',(1.59371958050517,-2.22130979469258,8.79610912703474));
#375494=CARTESIAN_POINT('Origin',(0.,1.84795814293585E-15,8.79610912703474));
#375495=CARTESIAN_POINT('',(1.58363955683349,-2.15047978570931,8.85933012996512));
#375496=CARTESIAN_POINT('Ctrl Pts',(1.59371958050517,-2.22130979469258,
8.79610912703474));
#375497=CARTESIAN_POINT('Ctrl Pts',(1.5928408520915,-2.21513637169913,8.80163734024559));
#375498=CARTESIAN_POINT('Ctrl Pts',(1.59196184585596,-2.20896068826177,
8.80716298614018));
#375499=CARTESIAN_POINT('Ctrl Pts',(1.59108255624699,-2.20278270081156,
8.8126860086129));
#375500=CARTESIAN_POINT('Ctrl Pts',(1.58860385362508,-2.18536705807609,
8.82825531609049));
#375501=CARTESIAN_POINT('Ctrl Pts',(1.58612289741731,-2.16793309440754,
8.84380379913848));
#375502=CARTESIAN_POINT('Ctrl Pts',(1.58363955683349,-2.15047978570931,
8.85933012996512));
#375503=CARTESIAN_POINT('',(1.61100669796545,-2.13005515746015,8.85933012996512));
#375504=CARTESIAN_POINT('Origin',(1.60287503492125,-2.14770651837813,8.84999761231045));
#375505=CARTESIAN_POINT('',(1.67604110579952,-2.15987164362911,8.79610912703474));
#375506=CARTESIAN_POINT('Ctrl Pts',(1.61100669796545,-2.13005515746015,
8.85933012996512));
#375507=CARTESIAN_POINT('Ctrl Pts',(1.61669149500713,-2.13266129101826,
8.8538223528706));
#375508=CARTESIAN_POINT('Ctrl Pts',(1.62237404208909,-2.13526644356547,
8.84831178811348));
#375509=CARTESIAN_POINT('Ctrl Pts',(1.62805438234943,-2.1378706341428,8.84279849653635));
#375510=CARTESIAN_POINT('Ctrl Pts',(1.64406716590575,-2.1452118035346,8.82725662040549));
#375511=CARTESIAN_POINT('Ctrl Pts',(1.66006243334958,-2.15254533794299,
8.81169306718667));
#375512=CARTESIAN_POINT('Ctrl Pts',(1.67604110579952,-2.15987164362911,
8.79610912703474));
#375513=CARTESIAN_POINT('',(1.7327649198924,-2.11463591137412,8.79610912703474));
#375514=CARTESIAN_POINT('Origin',(0.,1.84795814293585E-15,8.79610912703474));
#375515=CARTESIAN_POINT('',(1.71816751245364,-2.04459725957486,8.85933012996512));
#375516=CARTESIAN_POINT('Ctrl Pts',(1.7327649198924,-2.11463591137412,8.79610912703474));
#375517=CARTESIAN_POINT('Ctrl Pts',(1.73149246435127,-2.10853147266307,
8.80163734024559));
#375518=CARTESIAN_POINT('Ctrl Pts',(1.73021958673196,-2.10242479595255,
8.80716298614018));
#375519=CARTESIAN_POINT('Ctrl Pts',(1.72894627870281,-2.09631583811882,
8.8126860086129));
#375520=CARTESIAN_POINT('Ctrl Pts',(1.72535684478011,-2.07909478871142,
8.82825531609049));
#375521=CARTESIAN_POINT('Ctrl Pts',(1.72176398807558,-2.06185560040101,
8.84380379913848));
#375522=CARTESIAN_POINT('Ctrl Pts',(1.71816751245364,-2.04459725957486,
8.85933012996512));
#375523=CARTESIAN_POINT('',(1.74416981443408,-2.0224611771624,8.85933012996512));
#375524=CARTESIAN_POINT('Origin',(1.7371857853407,-2.04059726890633,8.84999761231044));
#375525=CARTESIAN_POINT('',(1.81098095093023,-2.04804963334647,8.79610912703474));
#375526=CARTESIAN_POINT('Ctrl Pts',(1.74416981443408,-2.0224611771624,8.85933012996512));
#375527=CARTESIAN_POINT('Ctrl Pts',(1.75000990700091,-2.0246977299426,8.8538223528706));
#375528=CARTESIAN_POINT('Ctrl Pts',(1.75584769137722,-2.02693344788291,
8.84831178811348));
#375529=CARTESIAN_POINT('Ctrl Pts',(1.76168321183244,-2.02916834722135,
8.84279849653635));
#375530=CARTESIAN_POINT('Ctrl Pts',(1.77813344574543,-2.03546849082835,
8.82725662040549));
#375531=CARTESIAN_POINT('Ctrl Pts',(1.79456571035959,-2.0417621374,8.81169306718667));
#375532=CARTESIAN_POINT('Ctrl Pts',(1.81098095093023,-2.04804963334647,
8.79610912703474));
#375533=CARTESIAN_POINT('',(1.86468995654688,-1.99927253550784,8.79610912703474));
#375534=CARTESIAN_POINT('Origin',(0.,1.84795814293585E-15,8.79610912703474));
#375535=CARTESIAN_POINT('',(1.84563514921934,-1.93031304473608,8.85933012996512));
#375536=CARTESIAN_POINT('Ctrl Pts',(1.86468995654688,-1.99927253550784,
8.79610912703474));
#375537=CARTESIAN_POINT('Ctrl Pts',(1.86302900267106,-1.99326216552726,
8.80163734024559));
#375538=CARTESIAN_POINT('Ctrl Pts',(1.86136748419513,-1.98724958918806,
8.80716298614018));
#375539=CARTESIAN_POINT('Ctrl Pts',(1.85970539004164,-1.98123476398891,
8.8126860086129));
#375540=CARTESIAN_POINT('Ctrl Pts',(1.85501997457207,-1.9642790728955,8.82825531609049));
#375541=CARTESIAN_POINT('Ctrl Pts',(1.85032998118963,-1.94730549946579,
8.84380379913848));
#375542=CARTESIAN_POINT('Ctrl Pts',(1.84563514921934,-1.93031304473608,
8.85933012996512));
#375543=CARTESIAN_POINT('',(1.87016576301195,-1.90655647007113,8.85933012996512));
#375544=CARTESIAN_POINT('Origin',(1.86435806674298,-1.92510276754984,8.84999761231046));
#375545=CARTESIAN_POINT('',(1.93847908687937,-1.92781174781514,8.79610912703474));
#375546=CARTESIAN_POINT('Ctrl Pts',(1.87016576301195,-1.90655647007113,
8.85933012996512));
#375547=CARTESIAN_POINT('Ctrl Pts',(1.87613715291088,-1.90841425159831,
8.8538223528706));
#375548=CARTESIAN_POINT('Ctrl Pts',(1.88210618587333,-1.91027134788713,
8.84831178811348));
#375549=CARTESIAN_POINT('Ctrl Pts',(1.88807290711817,-1.91212777230593,
8.84279849653635));
#375550=CARTESIAN_POINT('Ctrl Pts',(1.90489299384811,-1.91736100148666,
8.82725662040549));
#375551=CARTESIAN_POINT('Ctrl Pts',(1.9216947319326,-1.92258889827782,8.81169306718667));
#375552=CARTESIAN_POINT('Ctrl Pts',(1.93847908687937,-1.92781174781514,
8.79610912703474));
#375553=CARTESIAN_POINT('',(1.98895258219517,-1.87569371995055,8.79610912703474));
#375554=CARTESIAN_POINT('Origin',(0.,1.84795814293585E-15,8.79610912703474));
#375555=CARTESIAN_POINT('',(1.9655186752694,-1.80809675954562,8.85933012996512));
#375556=CARTESIAN_POINT('Ctrl Pts',(1.98895258219517,-1.87569371995055,
8.79610912703474));
#375557=CARTESIAN_POINT('Ctrl Pts',(1.9869099552004,-1.86980211659991,8.80163734024559));
#375558=CARTESIAN_POINT('Ctrl Pts',(1.98486662340368,-1.86390834759789,
8.80716298614018));
#375559=CARTESIAN_POINT('Ctrl Pts',(1.98282257302722,-1.85801237124025,
8.8126860086129));
#375560=CARTESIAN_POINT('Ctrl Pts',(1.97706042938797,-1.84139171303252,
8.82825531609049));
#375561=CARTESIAN_POINT('Ctrl Pts',(1.97129257151643,-1.82475350253755,
8.84380379913848));
#375562=CARTESIAN_POINT('Ctrl Pts',(1.9655186752694,-1.80809675954562,8.85933012996512));
#375563=CARTESIAN_POINT('',(1.9884767993203,-1.78281731348926,8.85933012996512));
#375564=CARTESIAN_POINT('Origin',(1.98386930094547,-1.80169760598823,8.84999761231048));
#375565=CARTESIAN_POINT('',(2.05801159645807,-1.79965207029772,8.79610912703474));
#375566=CARTESIAN_POINT('Ctrl Pts',(1.9884767993203,-1.78281731348926,8.85933012996512));
#375567=CARTESIAN_POINT('Ctrl Pts',(1.99455494882937,-1.78428868974062,
8.8538223528706));
#375568=CARTESIAN_POINT('Ctrl Pts',(2.00063070234118,-1.78575953317098,
8.84831178811348));
#375569=CARTESIAN_POINT('Ctrl Pts',(2.00670410583818,-1.78722985422398,
8.84279849653635));
#375570=CARTESIAN_POINT('Ctrl Pts',(2.02382492804081,-1.79137466451721,
8.82725662040549));
#375571=CARTESIAN_POINT('Ctrl Pts',(2.04092709764987,-1.7955153289786,8.81169306718667));
#375572=CARTESIAN_POINT('Ctrl Pts',(2.05801159645807,-1.79965207029772,
8.79610912703474));
#375573=CARTESIAN_POINT('',(2.10504217505423,-1.74440727656294,8.79610912703474));
#375574=CARTESIAN_POINT('Origin',(0.,1.84795814293585E-15,8.79610912703474));
#375575=CARTESIAN_POINT('',(2.07732546348034,-1.67845061693465,8.85933012996512));
#375576=CARTESIAN_POINT('Ctrl Pts',(2.10504217505423,-1.74440727656294,
8.79610912703474));
#375577=CARTESIAN_POINT('Ctrl Pts',(2.10262626853298,-1.73865864970415,
8.80163734024559));
#375578=CARTESIAN_POINT('Ctrl Pts',(2.1002095199041,-1.73290790680036,8.80716298614018));
#375579=CARTESIAN_POINT('Ctrl Pts',(2.09779191274614,-1.72715500711575,
8.8126860086129));
#375580=CARTESIAN_POINT('Ctrl Pts',(2.09097671882138,-1.7109376796434,8.82825531609049));
#375581=CARTESIAN_POINT('Ctrl Pts',(2.08415469782594,-1.69470320205899,
8.84380379913848));
#375582=CARTESIAN_POINT('Ctrl Pts',(2.07732546348034,-1.67845061693465,
8.85933012996512));
#375583=CARTESIAN_POINT('',(2.09861675793331,-1.65175217815314,8.85933012996512));
#375584=CARTESIAN_POINT('Origin',(2.09522839065179,-1.67088888250073,8.84999761231043));
#375585=CARTESIAN_POINT('',(2.16908729494481,-1.66409723639929,8.79610912703474));
#375586=CARTESIAN_POINT('Ctrl Pts',(2.09861675793331,-1.65175217815314,
8.85933012996512));
#375587=CARTESIAN_POINT('Ctrl Pts',(2.10477669063244,-1.65283110292807,
8.8538223528706));
#375588=CARTESIAN_POINT('Ctrl Pts',(2.11093419811917,-1.6539096494888,8.84831178811348));
#375589=CARTESIAN_POINT('Ctrl Pts',(2.11708932695063,-1.65498782531142,
8.84279849653635));
#375590=CARTESIAN_POINT('Ctrl Pts',(2.1344405314951,-1.65802718480261,8.82725662040549));
#375591=CARTESIAN_POINT('Ctrl Pts',(2.1517728561454,-1.66106360205577,8.81169306718667));
#375592=CARTESIAN_POINT('Ctrl Pts',(2.16908729494481,-1.66409723639929,
8.79610912703474));
#375593=CARTESIAN_POINT('',(2.21248169808586,-1.60595268950174,8.79610912703474));
#375594=CARTESIAN_POINT('Origin',(0.,1.84795814293585E-15,8.79610912703474));
#375595=CARTESIAN_POINT('',(2.18059607577693,-1.54190736071218,8.85933012996512));
#375596=CARTESIAN_POINT('Ctrl Pts',(2.21248169808586,-1.60595268950174,
8.79610912703474));
#375597=CARTESIAN_POINT('Ctrl Pts',(2.20970243951623,-1.60037066147564,
8.80163734024559));
#375598=CARTESIAN_POINT('Ctrl Pts',(2.20692220499371,-1.59478657570621,
8.80716298614018));
#375599=CARTESIAN_POINT('Ctrl Pts',(2.20414097552062,-1.58920039259344,
8.8126860086129));
#375600=CARTESIAN_POINT('Ctrl Pts',(2.19630073640405,-1.57345303633365,
8.82825531609049));
#375601=CARTESIAN_POINT('Ctrl Pts',(2.18845258543231,-1.55768900261046,
8.84380379913848));
#375602=CARTESIAN_POINT('Ctrl Pts',(2.18059607577693,-1.54190736071218,
8.85933012996512));
#375603=CARTESIAN_POINT('',(2.20013305013608,-1.51389963881726,8.85933012996512));
#375604=CARTESIAN_POINT('Origin',(2.19797773747577,-1.53321411819045,8.84999761231047));
#375605=CARTESIAN_POINT('',(2.27124974846887,-1.52170427000876,8.79610912703474));
#375606=CARTESIAN_POINT('Ctrl Pts',(2.20013305013608,-1.51389963881726,
8.85933012996512));
#375607=CARTESIAN_POINT('Ctrl Pts',(2.20634945354051,-1.51458167858243,
8.8538223528706));
#375608=CARTESIAN_POINT('Ctrl Pts',(2.21256341248313,-1.51526349629436,
8.84831178811348));
#375609=CARTESIAN_POINT('Ctrl Pts',(2.21877497390439,-1.51594509643089,
8.84279849653635));
#375610=CARTESIAN_POINT('Ctrl Pts',(2.23628526096942,-1.51786651573993,
8.82725662040549));
#375611=CARTESIAN_POINT('Ctrl Pts',(2.2537765184212,-1.51978620849507,8.81169306718667));
#375612=CARTESIAN_POINT('Ctrl Pts',(2.27124974846887,-1.52170427000876,
8.79610912703474));
#375613=CARTESIAN_POINT('',(2.31082965924422,-1.46089889836361,8.79610912703474));
#375614=CARTESIAN_POINT('Origin',(0.,1.84795814293585E-15,8.79610912703474));
#375615=CARTESIAN_POINT('',(2.27490615106176,-1.39902807640644,8.85933012996512));
#375616=CARTESIAN_POINT('Ctrl Pts',(2.31082965924422,-1.46089889836361,
8.79610912703474));
#375617=CARTESIAN_POINT('Ctrl Pts',(2.30769846919582,-1.4555064069207,8.80163734024559));
#375618=CARTESIAN_POINT('Ctrl Pts',(2.30456617335967,-1.45011192449183,
8.80716298614018));
#375619=CARTESIAN_POINT('Ctrl Pts',(2.30143275023993,-1.44471541277554,
8.8126860086129));
#375620=CARTESIAN_POINT('Ctrl Pts',(2.29259968315581,-1.42950273699299,
8.82825531609049));
#375621=CARTESIAN_POINT('Ctrl Pts',(2.28375765194352,-1.41427392492697,
8.84380379913848));
#375622=CARTESIAN_POINT('Ctrl Pts',(2.27490615106176,-1.39902807640644,
8.85933012996512));
#375623=CARTESIAN_POINT('',(2.29260852370879,-1.36982616113503,8.85933012996512));
#375624=CARTESIAN_POINT('Origin',(2.29169512231177,-1.38923904819516,8.84999761231045));
#375625=CARTESIAN_POINT('',(2.36407914959492,-1.37305829436821,8.79610912703474));
#375626=CARTESIAN_POINT('Ctrl Pts',(2.29260852370879,-1.36982616113503,
8.85933012996512));
#375627=CARTESIAN_POINT('Ctrl Pts',(2.2988558532835,-1.37010851324274,8.8538223528706));
#375628=CARTESIAN_POINT('Ctrl Pts',(2.30510072919182,-1.37039080037066,
8.84831178811348));
#375629=CARTESIAN_POINT('Ctrl Pts',(2.31134319856465,-1.37067302397992,
8.84279849653635));
#375630=CARTESIAN_POINT('Ctrl Pts',(2.32894061462473,-1.37146860758273,
8.82725662040549));
#375631=CARTESIAN_POINT('Ctrl Pts',(2.34651892954927,-1.37226368741055,
8.81169306718667));
#375632=CARTESIAN_POINT('Ctrl Pts',(2.36407914959492,-1.37305829436821,
8.79610912703474));
#375633=CARTESIAN_POINT('',(2.39968192566134,-1.30984196029027,8.79610912703474));
#375634=CARTESIAN_POINT('Origin',(0.,1.84795814293585E-15,8.79610912703474));
#375635=CARTESIAN_POINT('',(2.35986814900604,-1.25039988564417,8.85933012996512));
#375636=CARTESIAN_POINT('Ctrl Pts',(2.39968192566134,-1.30984196029027,
8.79610912703474));
#375637=CARTESIAN_POINT('Ctrl Pts',(2.39621167086572,-1.30466116433458,
8.80163734024559));
#375638=CARTESIAN_POINT('Ctrl Pts',(2.3927401849914,-1.29947845233168,8.80716298614018));
#375639=CARTESIAN_POINT('Ctrl Pts',(2.38926744413273,-1.29429378743606,
8.8126860086129));
#375640=CARTESIAN_POINT('Ctrl Pts',(2.3794778460484,-1.27967830427864,8.82825531609049));
#375641=CARTESIAN_POINT('Ctrl Pts',(2.36967826839842,-1.26504729232515,
8.84380379913848));
#375642=CARTESIAN_POINT('Ctrl Pts',(2.35986814900604,-1.25039988564417,
8.85933012996512));
#375643=CARTESIAN_POINT('',(2.3756631770946,-1.2201237739299,8.85933012996512));
#375644=CARTESIAN_POINT('Origin',(2.37599544032312,-1.23955529695998,8.84999761231044));
#375645=CARTESIAN_POINT('',(2.44719404240189,-1.21877012767603,8.79610912703474));
#375646=CARTESIAN_POINT('Ctrl Pts',(2.3756631770946,-1.2201237739299,8.85933012996512));
#375647=CARTESIAN_POINT('Ctrl Pts',(2.38191576122233,-1.22000527813478,
8.8538223528706));
#375648=CARTESIAN_POINT('Ctrl Pts',(2.38816589256171,-1.21988687470032,
8.84831178811348));
#375649=CARTESIAN_POINT('Ctrl Pts',(2.39441361824044,-1.21976856206496,
8.84279849653635));
#375650=CARTESIAN_POINT('Ctrl Pts',(2.41202585173836,-1.21943504073788,
8.82725662040549));
#375651=CARTESIAN_POINT('Ctrl Pts',(2.42961899106908,-1.21910224048481,
8.81169306718667));
#375652=CARTESIAN_POINT('Ctrl Pts',(2.44719404240189,-1.21877012767603,
8.79610912703474));
#375653=CARTESIAN_POINT('',(2.47867338431575,-1.15340260064189,8.79610912703474));
#375654=CARTESIAN_POINT('Origin',(0.,1.84795814293585E-15,8.79610912703474));
#375655=CARTESIAN_POINT('',(2.43513294253592,-1.09663353354185,8.85933012996512));
#375656=CARTESIAN_POINT('Ctrl Pts',(2.47867338431575,-1.15340260064189,
8.79610912703474));
#375657=CARTESIAN_POINT('Ctrl Pts',(2.47487832479424,-1.14845478917526,
8.80163734024559));
#375658=CARTESIAN_POINT('Ctrl Pts',(2.47108191396185,-1.14350514447364,
8.80716298614018));
#375659=CARTESIAN_POINT('Ctrl Pts',(2.46728412560133,-1.13855363129886,
8.8126860086129));
#375660=CARTESIAN_POINT('Ctrl Pts',(2.45657822407517,-1.12459539892188,
8.82825531609049));
#375661=CARTESIAN_POINT('Ctrl Pts',(2.44586136855408,-1.11062230904737,
8.84380379913848));
#375662=CARTESIAN_POINT('Ctrl Pts',(2.43513294253592,-1.09663353354185,
8.85933012996512));
#375663=CARTESIAN_POINT('',(2.44895572090757,-1.06540763642197,8.85933012996512));
#375664=CARTESIAN_POINT('Origin',(2.45053228342073,-1.08477794712581,8.84999761231046));
#375665=CARTESIAN_POINT('',(2.52025288996717,-1.05947377310385,8.79610912703474));
#375666=CARTESIAN_POINT('Ctrl Pts',(2.44895572090757,-1.06540763642197,
8.85933012996512));
#375667=CARTESIAN_POINT('Ctrl Pts',(2.45518786637896,-1.06488877964865,
8.8538223528706));
#375668=CARTESIAN_POINT('Ctrl Pts',(2.46141757001909,-1.06437017219693,
8.84831178811348));
#375669=CARTESIAN_POINT('Ctrl Pts',(2.46764487875877,-1.06385180948896,
8.84279849653635));
#375670=CARTESIAN_POINT('Ctrl Pts',(2.48519955724927,-1.06239055374265,
8.82725662040549));
#375671=CARTESIAN_POINT('Ctrl Pts',(2.50273522700295,-1.06093124095632,
8.81169306718667));
#375672=CARTESIAN_POINT('Ctrl Pts',(2.52025288996717,-1.05947377310385,
8.79610912703474));
#375673=CARTESIAN_POINT('',(2.54747944236024,-0.992223662303376,8.79610912703474));
#375674=CARTESIAN_POINT('Origin',(0.,1.84795814293585E-15,8.79610912703474));
#375675=CARTESIAN_POINT('',(2.50039125247055,-0.938360879023052,8.85933012996512));
#375676=CARTESIAN_POINT('Ctrl Pts',(2.54747944236024,-0.992223662303376,
8.79610912703474));
#375677=CARTESIAN_POINT('Ctrl Pts',(2.54337517282645,-0.987529166944447,
8.80163734024559));
#375678=CARTESIAN_POINT('Ctrl Pts',(2.53926943730241,-0.982832928695883,
8.80716298614018));
#375679=CARTESIAN_POINT('Ctrl Pts',(2.53516220736704,-0.97813491407166,
8.8126860086129));
#375680=CARTESIAN_POINT('Ctrl Pts',(2.52358399524484,-0.964891289845987,
8.82825531609049));
#375681=CARTESIAN_POINT('Ctrl Pts',(2.51199389971073,-0.951633540473973,
8.84380379913848));
#375682=CARTESIAN_POINT('Ctrl Pts',(2.50039125247055,-0.938360879023052,
8.85933012996512));
#375683=CARTESIAN_POINT('',(2.51218498036397,-0.906313510406752,8.85933012996512));
#375684=CARTESIAN_POINT('Origin',(2.51499936372827,-0.925543012022764,8.84999761231044));
#375685=CARTESIAN_POINT('',(2.58295547781501,-0.89582381354158,8.79610912703474));
#375686=CARTESIAN_POINT('Ctrl Pts',(2.51218498036397,-0.906313510406752,
8.85933012996512));
#375687=CARTESIAN_POINT('Ctrl Pts',(2.51837107795649,-0.905396424749024,
8.8538223528706));
#375688=CARTESIAN_POINT('Ctrl Pts',(2.52455475470885,-0.904479744349289,
8.84831178811348));
#375689=CARTESIAN_POINT('Ctrl Pts',(2.53073605716211,-0.903563461632256,
8.84279849653635));
#375690=CARTESIAN_POINT('Ctrl Pts',(2.5481610447058,-0.90098047608002,8.82725662040549));
#375691=CARTESIAN_POINT('Ctrl Pts',(2.56556718705404,-0.898400647389695,
8.81169306718667));
#375692=CARTESIAN_POINT('Ctrl Pts',(2.58295547781501,-0.89582381354158,
8.79610912703474));
#375693=CARTESIAN_POINT('',(2.60581736094344,-0.826967464105156,8.79610912703474));
#375694=CARTESIAN_POINT('Origin',(0.,1.84795814293585E-15,8.79610912703474));
#375695=CARTESIAN_POINT('',(2.55537491841653,-0.776232298374573,8.85933012996512));
#375696=CARTESIAN_POINT('Ctrl Pts',(2.60581736094344,-0.826967464105156,
8.79610912703474));
#375697=CARTESIAN_POINT('Ctrl Pts',(2.60142074672124,-0.822545575542315,
8.80163734024559));
#375698=CARTESIAN_POINT('Ctrl Pts',(2.59702255785351,-0.81812204159711,
8.80716298614018));
#375699=CARTESIAN_POINT('Ctrl Pts',(2.5926227638321,-0.813696830673264,
8.8126860086129));
#375700=CARTESIAN_POINT('Ctrl Pts',(2.58021981847098,-0.80122223549159,
8.82825531609049));
#375701=CARTESIAN_POINT('Ctrl Pts',(2.56780410911246,-0.788734305558017,
8.84380379913848));
#375702=CARTESIAN_POINT('Ctrl Pts',(2.55537491841653,-0.776232298374573,
8.85933012996512));
#375703=CARTESIAN_POINT('',(2.56509113287407,-0.74349514777364,8.85933012996512));
#375704=CARTESIAN_POINT('Origin',(2.56913177218453,-0.762504822154957,8.84999761231048));
#375705=CARTESIAN_POINT('',(2.63504414756231,-0.728492721775861,8.79610912703474));
#375706=CARTESIAN_POINT('Ctrl Pts',(2.56509113287407,-0.74349514777364,
8.85933012996512));
#375707=CARTESIAN_POINT('Ctrl Pts',(2.5712057625858,-0.742183601733178,
8.8538223528706));
#375708=CARTESIAN_POINT('Ctrl Pts',(2.57731800239621,-0.740872615221825,
8.84831178811348));
#375709=CARTESIAN_POINT('Ctrl Pts',(2.5834278982654,-0.739562177697958,
8.84279849653635));
#375710=CARTESIAN_POINT('Ctrl Pts',(2.60065159185081,-0.735868076381477,
8.82725662040549));
#375711=CARTESIAN_POINT('Ctrl Pts',(2.6178566812211,-0.732178332856615,
8.81169306718667));
#375712=CARTESIAN_POINT('Ctrl Pts',(2.63504414756231,-0.728492721775861,
8.79610912703474));
#375713=CARTESIAN_POINT('',(2.65344741704446,-0.65831307921296,8.79610912703474));
#375714=CARTESIAN_POINT('Origin',(0.,1.84795814293585E-15,8.79610912703474));
#375715=CARTESIAN_POINT('',(2.59985800069653,-0.610914012710764,8.85933012996512));
#375716=CARTESIAN_POINT('Ctrl Pts',(2.65344741704446,-0.65831307921296,
8.79610912703474));
#375717=CARTESIAN_POINT('Ctrl Pts',(2.64877652476476,-0.654181967934804,
8.80163734024559));
#375718=CARTESIAN_POINT('Ctrl Pts',(2.6441039556548,-0.650049315542785,
8.80716298614018));
#375719=CARTESIAN_POINT('Ctrl Pts',(2.63942967724473,-0.645915092460206,
8.8126860086129));
#375720=CARTESIAN_POINT('Ctrl Pts',(2.62625296500761,-0.634260787109924,
8.82825531609049));
#375721=CARTESIAN_POINT('Ctrl Pts',(2.6130626606376,-0.622593992197544,
8.84380379913848));
#375722=CARTESIAN_POINT('Ctrl Pts',(2.59985800069653,-0.610914012710764,
8.85933012996512));
#375723=CARTESIAN_POINT('',(2.60745677570887,-0.577621604099114,8.85933012996512));
#375724=CARTESIAN_POINT('Origin',(2.61270706711191,-0.596333336416159,8.84999761231045));
#375725=CARTESIAN_POINT('',(2.67630485569207,-0.558168097155164,8.79610912703474));
#375726=CARTESIAN_POINT('Ctrl Pts',(2.60745677570887,-0.577621604099114,
8.85933012996512));
#375727=CARTESIAN_POINT('Ctrl Pts',(2.61347481121474,-0.575920987099925,
8.8538223528706));
#375728=CARTESIAN_POINT('Ctrl Pts',(2.61949049757874,-0.574221081601735,
8.84831178811348));
#375729=CARTESIAN_POINT('Ctrl Pts',(2.62550387999116,-0.572521874139906,
8.84279849653635));
#375730=CARTESIAN_POINT('Ctrl Pts',(2.64245550376689,-0.567731836913873,
8.82725662040549));
#375731=CARTESIAN_POINT('Ctrl Pts',(2.65938884075651,-0.562947340502065,
8.81169306718667));
#375732=CARTESIAN_POINT('Ctrl Pts',(2.67630485569207,-0.558168097155164,
8.79610912703474));
#375733=CARTESIAN_POINT('',(2.69017388854615,-0.486953544670569,8.79610912703474));
#375734=CARTESIAN_POINT('Origin',(0.,1.84795814293585E-15,8.79610912703474));
#375735=CARTESIAN_POINT('',(2.63365770878388,-0.443085350328085,8.85933012996512));
#375736=CARTESIAN_POINT('Ctrl Pts',(2.69017388854615,-0.486953544670569,
8.79610912703474));
#375737=CARTESIAN_POINT('Ctrl Pts',(2.68524791190724,-0.48313018629946,
8.80163734024559));
#375738=CARTESIAN_POINT('Ctrl Pts',(2.68032016314379,-0.479305397415756,
8.80716298614018));
#375739=CARTESIAN_POINT('Ctrl Pts',(2.67539060795768,-0.475479150583879,
8.8126860086129));
#375740=CARTESIAN_POINT('Ctrl Pts',(2.66149427478153,-0.464693025105514,
8.82825531609049));
#375741=CARTESIAN_POINT('Ctrl Pts',(2.64758357719,-0.45389530657714,8.84380379913848));
#375742=CARTESIAN_POINT('Ctrl Pts',(2.63365770878388,-0.443085350328085,
8.85933012996512));
#375743=CARTESIAN_POINT('',(2.63910781935456,-0.409374489353903,8.85933012996512));
#375744=CARTESIAN_POINT('Origin',(2.64554618827659,-0.427711389084919,8.84999761231045));
#375745=CARTESIAN_POINT('',(2.7065680531042,-0.385549840096578,8.79610912703474));
#375746=CARTESIAN_POINT('Ctrl Pts',(2.63910781935456,-0.409374489353903,
8.85933012996512));
#375747=CARTESIAN_POINT('Ctrl Pts',(2.6450045312558,-0.407291789596017,
8.8538223528706));
#375748=CARTESIAN_POINT('Ctrl Pts',(2.65089894442778,-0.40520995038731,
8.84831178811348));
#375749=CARTESIAN_POINT('Ctrl Pts',(2.65679110310522,-0.403128955395459,
8.84279849653635));
#375750=CARTESIAN_POINT('Ctrl Pts',(2.67340099921307,-0.397262665550295,
8.82725662040549));
#375751=CARTESIAN_POINT('Ctrl Pts',(2.68999300110815,-0.391403076773568,
8.81169306718667));
#375752=CARTESIAN_POINT('Ctrl Pts',(2.7065680531042,-0.385549840096578,
8.79610912703474));
#375753=CARTESIAN_POINT('',(2.71584585849932,-0.313593013561915,8.79610912703474));
#375754=CARTESIAN_POINT('Origin',(0.,1.84795814293585E-15,8.79610912703474));
#375755=CARTESIAN_POINT('',(2.65663515242804,-0.273435955199396,8.85933012996512));
#375756=CARTESIAN_POINT('Ctrl Pts',(2.71584585849932,-0.313593013561915,
8.79610912703474));
#375757=CARTESIAN_POINT('Ctrl Pts',(2.71068503939582,-0.310093119097509,
8.80163734024559));
#375758=CARTESIAN_POINT('Ctrl Pts',(2.70552236015555,-0.306591910600058,
8.80716298614018));
#375759=CARTESIAN_POINT('Ctrl Pts',(2.70035778479304,-0.303089362887842,
8.8126860086129));
#375760=CARTESIAN_POINT('Ctrl Pts',(2.68579893369164,-0.293215739784602,
8.82825531609049));
#375761=CARTESIAN_POINT('Ctrl Pts',(2.67122500491882,-0.283331467781771,
8.84380379913848));
#375762=CARTESIAN_POINT('Ctrl Pts',(2.65663515242804,-0.273435955199396,
8.85933012996512));
#375763=CARTESIAN_POINT('',(2.65991420288367,-0.239445167021381,8.85933012996512));
#375764=CARTESIAN_POINT('Origin',(2.66751419268574,-0.25733188391212,8.84999761231047));
#375765=CARTESIAN_POINT('',(2.7257093818291,-0.211347276044851,8.79610912703474));
#375766=CARTESIAN_POINT('Ctrl Pts',(2.65991420288367,-0.239445167021381,
8.85933012996512));
#375767=CARTESIAN_POINT('Ctrl Pts',(2.66566536032625,-0.236988942764841,
8.8538223528706));
#375768=CARTESIAN_POINT('Ctrl Pts',(2.67141427889812,-0.234533724569479,
8.84831178811348));
#375769=CARTESIAN_POINT('Ctrl Pts',(2.67716100169672,-0.2320794933024,8.84279849653635));
#375770=CARTESIAN_POINT('Ctrl Pts',(2.69336091651076,-0.225161056681394,
8.82725662040549));
#375771=CARTESIAN_POINT('Ctrl Pts',(2.70954340321654,-0.218250453846909,
8.81169306718667));
#375772=CARTESIAN_POINT('Ctrl Pts',(2.7257093818291,-0.211347276044851,
8.79610912703474));
#375773=CARTESIAN_POINT('',(2.73035783527281,-0.138943861495048,8.79610912703474));
#375774=CARTESIAN_POINT('Origin',(0.,1.84795814293585E-15,8.79610912703474));
#375775=CARTESIAN_POINT('',(2.66869591238441,-0.102662953078966,8.85933012996512));
#375776=CARTESIAN_POINT('Ctrl Pts',(2.73035783527281,-0.138943861495048,
8.79610912703474));
#375777=CARTESIAN_POINT('Ctrl Pts',(2.72498338061741,-0.135781812754423,
8.80163734024559));
#375778=CARTESIAN_POINT('Ctrl Pts',(2.7196069854567,-0.132618571859948,
8.80716298614018));
#375779=CARTESIAN_POINT('Ctrl Pts',(2.71422861226575,-0.129454115987237,
8.8126860086129));
#375780=CARTESIAN_POINT('Ctrl Pts',(2.69906706868114,-0.120533568094338,
8.82825531609049));
#375781=CARTESIAN_POINT('Ctrl Pts',(2.68388979612647,-0.11160335921088,
8.84380379913848));
#375782=CARTESIAN_POINT('Ctrl Pts',(2.66869591238441,-0.102662953078966,
8.85933012996512));
#375783=CARTESIAN_POINT('',(2.66979042840332,-0.0685319131367438,8.85933012996512));
#375784=CARTESIAN_POINT('Origin',(2.67852080909721,-0.0858949468308122,
8.84999761231043));
#375785=CARTESIAN_POINT('',(2.73365018604124,-0.0362762407020098,8.79610912703474));
#375786=CARTESIAN_POINT('Ctrl Pts',(2.66979042840332,-0.0685319131367438,
8.85933012996512));
#375787=CARTESIAN_POINT('Ctrl Pts',(2.67537239864768,-0.0657122575338778,
8.8538223528706));
#375788=CARTESIAN_POINT('Ctrl Pts',(2.6809521990799,-0.0628937493700682,
8.84831178811348));
#375789=CARTESIAN_POINT('Ctrl Pts',(2.68652987148302,-0.0600763667904682,
8.84279849653635));
#375790=CARTESIAN_POINT('Ctrl Pts',(2.7022532360784,-0.0521342127336968,
8.82725662040549));
#375791=CARTESIAN_POINT('Ctrl Pts',(2.71795971028587,-0.0442009929908208,
8.81169306718667));
#375792=CARTESIAN_POINT('Ctrl Pts',(2.73365018604124,-0.0362762407020098,
8.79610912703474));
#375793=CARTESIAN_POINT('',(2.73389087296526,1.51315307225634E-15,8.79610912703474));
#375794=CARTESIAN_POINT('Origin',(0.,1.84795814293585E-15,8.79610912703474));
#375795=CARTESIAN_POINT('',(2.54610912703474,1.53614970366555E-15,8.98389087296526));
#375796=CARTESIAN_POINT('',(2.73389087296526,1.51315307225634E-15,8.79610912703474));
#375797=CARTESIAN_POINT('',(-2.54610912703474,2.0465319152471E-15,8.98389087296526));
#375798=CARTESIAN_POINT('Origin',(0.,1.84795814293585E-15,8.98389087296526));
#375799=CARTESIAN_POINT('Origin',(0.,1.84795814293585E-15,8.98389087296526));
#375800=CARTESIAN_POINT('',(2.73365018604124,0.0362762407020695,8.79610912703474));
#375801=CARTESIAN_POINT('Origin',(0.,1.84795814293585E-15,8.79610912703474));
#375802=CARTESIAN_POINT('',(2.66979042840331,0.0685319131368021,8.85933012996512));
#375803=CARTESIAN_POINT('Ctrl Pts',(2.73365018604124,0.0362762407020695,
8.79610912703474));
#375804=CARTESIAN_POINT('Ctrl Pts',(2.72808418062094,0.0390874501823801,
8.80163734024559));
#375805=CARTESIAN_POINT('Ctrl Pts',(2.72251616230074,0.041899725038531,
8.80716298614018));
#375806=CARTESIAN_POINT('Ctrl Pts',(2.71694609217046,0.044713085643783,
8.8126860086129));
#375807=CARTESIAN_POINT('Ctrl Pts',(2.70124415813737,0.0526439018815967,
8.82825531609049));
#375808=CARTESIAN_POINT('Ctrl Pts',(2.68552590846928,0.0605833515018572,
8.84380379913848));
#375809=CARTESIAN_POINT('Ctrl Pts',(2.66979042840331,0.0685319131368021,
8.85933012996512));
#375810=CARTESIAN_POINT('',(2.66869591238441,0.102662953079024,8.85933012996512));
#375811=CARTESIAN_POINT('Origin',(2.67852080896314,0.0858949510114288,8.84999761231043));
#375812=CARTESIAN_POINT('',(2.7303578352728,0.138943861495108,8.79610912703474));
#375813=CARTESIAN_POINT('Ctrl Pts',(2.66869591238441,0.102662953079024,
8.85933012996512));
#375814=CARTESIAN_POINT('Ctrl Pts',(2.67408575791749,0.105834453458529,
8.8538223528706));
#375815=CARTESIAN_POINT('Ctrl Pts',(2.67947351161322,0.109004669736173,
8.84831178811348));
#375816=CARTESIAN_POINT('Ctrl Pts',(2.68485921376854,0.112173626398948,
8.84279849653635));
#375817=CARTESIAN_POINT('Ctrl Pts',(2.7000414174675,0.12110686187688,8.82725662040549));
#375818=CARTESIAN_POINT('Ctrl Pts',(2.71520733790511,0.130030099226553,
8.81169306718667));
#375819=CARTESIAN_POINT('Ctrl Pts',(2.7303578352728,0.138943861495108,8.79610912703474));
#375820=CARTESIAN_POINT('',(2.7257093818291,0.211347276044911,8.79610912703474));
#375821=CARTESIAN_POINT('Origin',(0.,1.84795814293585E-15,8.79610912703474));
#375822=CARTESIAN_POINT('',(2.65991420288366,0.239445167021439,8.85933012996512));
#375823=CARTESIAN_POINT('Ctrl Pts',(2.7257093818291,0.211347276044911,8.79610912703474));
#375824=CARTESIAN_POINT('Ctrl Pts',(2.71997469755407,0.21379609440215,8.80163734024559));
#375825=CARTESIAN_POINT('Ctrl Pts',(2.714237936256,0.216245846979362,8.80716298614018));
#375826=CARTESIAN_POINT('Ctrl Pts',(2.70849905779933,0.218696551614963,
8.8126860086129));
#375827=CARTESIAN_POINT('Ctrl Pts',(2.69232125593275,0.225605046772616,
8.82825531609049));
#375828=CARTESIAN_POINT('Ctrl Pts',(2.67612661881068,0.232521112228182,
8.84380379913848));
#375829=CARTESIAN_POINT('Ctrl Pts',(2.65991420288366,0.239445167021439,
8.85933012996512));
#375830=CARTESIAN_POINT('',(2.65663515242803,0.273435955199454,8.85933012996512));
#375831=CARTESIAN_POINT('Origin',(2.66751419228414,0.257331888075556,8.84999761231043));
#375832=CARTESIAN_POINT('',(2.71584585849932,0.313593013561975,8.79610912703474));
#375833=CARTESIAN_POINT('Ctrl Pts',(2.65663515242803,0.273435955199454,
8.85933012996512));
#375834=CARTESIAN_POINT('Ctrl Pts',(2.66181072521843,0.276946267980254,
8.8538223528706));
#375835=CARTESIAN_POINT('Ctrl Pts',(2.66698429274206,0.280455165273038,
8.84831178811348));
#375836=CARTESIAN_POINT('Ctrl Pts',(2.67215589364419,0.283962674096321,
8.84279849653635));
#375837=CARTESIAN_POINT('Ctrl Pts',(2.68673454951515,0.293850282414661,
8.82725662040549));
#375838=CARTESIAN_POINT('Ctrl Pts',(2.70129759616275,0.303726869874833,
8.81169306718667));
#375839=CARTESIAN_POINT('Ctrl Pts',(2.71584585849932,0.313593013561975,
8.79610912703474));
#375840=CARTESIAN_POINT('',(2.70656805310419,0.385549840096635,8.79610912703474));
#375841=CARTESIAN_POINT('Origin',(0.,1.84795814293585E-15,8.79610912703474));
#375842=CARTESIAN_POINT('',(2.63910781935455,0.409374489353958,8.85933012996512));
#375843=CARTESIAN_POINT('Ctrl Pts',(2.70656805310419,0.385549840096635,
8.79610912703474));
#375844=CARTESIAN_POINT('Ctrl Pts',(2.70068825502221,0.387626204610903,
8.80163734024559));
#375845=CARTESIAN_POINT('Ctrl Pts',(2.69480632432897,0.389703368350366,
8.80716298614018));
#375846=CARTESIAN_POINT('Ctrl Pts',(2.68892221982847,0.391781346545295,
8.8126860086129));
#375847=CARTESIAN_POINT('Ctrl Pts',(2.67233502818641,0.397639132134316,
8.82825531609049));
#375848=CARTESIAN_POINT('Ctrl Pts',(2.65573055084804,0.40350339382874,8.84380379913848));
#375849=CARTESIAN_POINT('Ctrl Pts',(2.63910781935455,0.409374489353958,
8.85933012996512));
#375850=CARTESIAN_POINT('',(2.63365770878388,0.44308535032814,8.85933012996512));
#375851=CARTESIAN_POINT('Origin',(2.64554618760903,0.427711393214063,8.84999761231044));
#375852=CARTESIAN_POINT('',(2.69017388854614,0.486953544670625,8.79610912703474));
#375853=CARTESIAN_POINT('Ctrl Pts',(2.63365770878388,0.44308535032814,8.85933012996512));
#375854=CARTESIAN_POINT('Ctrl Pts',(2.63859774129283,0.446920050882059,
8.8538223528706));
#375855=CARTESIAN_POINT('Ctrl Pts',(2.64353586334568,0.450753210378352,
8.84831178811348));
#375856=CARTESIAN_POINT('Ctrl Pts',(2.64847211177721,0.45458485825603,8.84279849653635));
#375857=CARTESIAN_POINT('Ctrl Pts',(2.66238731299609,0.465386209111313,
8.82725662040549));
#375858=CARTESIAN_POINT('Ctrl Pts',(2.67628764317124,0.476175561665589,
8.81169306718667));
#375859=CARTESIAN_POINT('Ctrl Pts',(2.69017388854614,0.486953544670625,
8.79610912703474));
#375860=CARTESIAN_POINT('',(2.67630485569206,0.558168097155223,8.79610912703474));
#375861=CARTESIAN_POINT('Origin',(0.,1.84795814293585E-15,8.79610912703474));
#375862=CARTESIAN_POINT('',(2.60745677570886,0.577621604099172,8.85933012996512));
#375863=CARTESIAN_POINT('Ctrl Pts',(2.67630485569206,0.558168097155223,
8.79610912703474));
#375864=CARTESIAN_POINT('Ctrl Pts',(2.67030410515465,0.559863475599352,
8.80163734024559));
#375865=CARTESIAN_POINT('Ctrl Pts',(2.66430117518113,0.561559514989709,
8.80716298614018));
#375866=CARTESIAN_POINT('Ctrl Pts',(2.65829602368433,0.563256227885838,
8.8126860086129));
#375867=CARTESIAN_POINT('Ctrl Pts',(2.64136760259518,0.568039233008752,
8.82825531609049));
#375868=CARTESIAN_POINT('Ctrl Pts',(2.62442151639954,0.572827593432851,
8.84380379913848));
#375869=CARTESIAN_POINT('Ctrl Pts',(2.60745677570886,0.577621604099172,
8.85933012996512));
#375870=CARTESIAN_POINT('',(2.59985800069652,0.610914012710821,8.85933012996512));
#375871=CARTESIAN_POINT('Origin',(2.61270706618112,0.596333340494042,8.84999761231048));
#375872=CARTESIAN_POINT('',(2.65344741704445,0.658313079213018,8.79610912703474));
#375873=CARTESIAN_POINT('Ctrl Pts',(2.59985800069652,0.610914012710821,
8.85933012996512));
#375874=CARTESIAN_POINT('Ctrl Pts',(2.60454219327082,0.615057343430743,
8.8538223528706));
#375875=CARTESIAN_POINT('Ctrl Pts',(2.60922457805015,0.619199013855962,
8.84831178811348));
#375876=CARTESIAN_POINT('Ctrl Pts',(2.61390518990746,0.623339055725021,
8.84279849653635));
#375877=CARTESIAN_POINT('Ctrl Pts',(2.62709975592764,0.635009764049699,
8.82725662040549));
#375878=CARTESIAN_POINT('Ctrl Pts',(2.64028025019204,0.646667545934124,
8.81169306718667));
#375879=CARTESIAN_POINT('Ctrl Pts',(2.65344741704445,0.658313079213018,
8.79610912703474));
#375880=CARTESIAN_POINT('',(2.63504414756229,0.728492721775916,8.79610912703474));
#375881=CARTESIAN_POINT('Origin',(0.,1.84795814293585E-15,8.79610912703474));
#375882=CARTESIAN_POINT('',(2.56509113287406,0.743495147773693,8.85933012996512));
#375883=CARTESIAN_POINT('Ctrl Pts',(2.63504414756229,0.728492721775916,
8.79610912703474));
#375884=CARTESIAN_POINT('Ctrl Pts',(2.62894710294057,0.729800147476222,
8.80163734024559));
#375885=CARTESIAN_POINT('Ctrl Pts',(2.62284784101366,0.731108093127821,
8.80716298614018));
#375886=CARTESIAN_POINT('Ctrl Pts',(2.61674631897617,0.732416568567915,
8.8126860086129));
#375887=CARTESIAN_POINT('Ctrl Pts',(2.59954623095331,0.73610513883072,8.82825531609049));
#375888=CARTESIAN_POINT('Ctrl Pts',(2.58232817100351,0.73979792158441,8.84380379913848));
#375889=CARTESIAN_POINT('Ctrl Pts',(2.56509113287406,0.743495147773693,
8.85933012996512));
#375890=CARTESIAN_POINT('',(2.55537491841651,0.776232298374626,8.85933012996512));
#375891=CARTESIAN_POINT('Origin',(2.56913177099444,0.762504826164844,8.84999761231045));
#375892=CARTESIAN_POINT('',(2.60581736094343,0.82696746410521,8.79610912703474));
#375893=CARTESIAN_POINT('Ctrl Pts',(2.55537491841651,0.776232298374626,
8.85933012996512));
#375894=CARTESIAN_POINT('Ctrl Pts',(2.55978402270411,0.78066723342588,8.8538223528706));
#375895=CARTESIAN_POINT('Ctrl Pts',(2.5641914292865,0.785100395767865,8.84831178811348));
#375896=CARTESIAN_POINT('Ctrl Pts',(2.56859717093147,0.789531819308227,
8.84279849653635));
#375897=CARTESIAN_POINT('Ctrl Pts',(2.58101688245096,0.802023927658437,
8.82725662040549));
#375898=CARTESIAN_POINT('Ctrl Pts',(2.59342337932647,0.814502234546662,
8.81169306718667));
#375899=CARTESIAN_POINT('Ctrl Pts',(2.60581736094343,0.82696746410521,8.79610912703474));
#375900=CARTESIAN_POINT('',(2.58295547781499,0.895823813541636,8.79610912703474));
#375901=CARTESIAN_POINT('Origin',(0.,1.84795814293585E-15,8.79610912703474));
#375902=CARTESIAN_POINT('',(2.51218498036395,0.906313510406806,8.85933012996512));
#375903=CARTESIAN_POINT('Ctrl Pts',(2.58295547781499,0.895823813541636,
8.79610912703474));
#375904=CARTESIAN_POINT('Ctrl Pts',(2.57678719317313,0.896737914005474,
8.80163734024559));
#375905=CARTESIAN_POINT('Ctrl Pts',(2.57061666246837,0.897652391289077,
8.80716298614018));
#375906=CARTESIAN_POINT('Ctrl Pts',(2.564443842353,0.898567252466887,8.8126860086129));
#375907=CARTESIAN_POINT('Ctrl Pts',(2.54704276624754,0.901146230743177,
8.82825531609049));
#375908=CARTESIAN_POINT('Ctrl Pts',(2.52962348524516,0.903728261390025,
8.84380379913848));
#375909=CARTESIAN_POINT('Ctrl Pts',(2.51218498036395,0.906313510406806,
8.85933012996512));
#375910=CARTESIAN_POINT('',(2.50039125247053,0.938360879023106,8.85933012996512));
#375911=CARTESIAN_POINT('Origin',(2.51499936228368,0.925543015948154,8.84999761231046));
#375912=CARTESIAN_POINT('',(2.54747944236022,0.992223662303432,8.79610912703474));
#375913=CARTESIAN_POINT('Ctrl Pts',(2.50039125247053,0.938360879023106,
8.85933012996512));
#375914=CARTESIAN_POINT('Ctrl Pts',(2.50450715051616,0.943069194306276,
8.8538223528706));
#375915=CARTESIAN_POINT('Ctrl Pts',(2.50862146792257,0.947775631750053,
8.84831178811348));
#375916=CARTESIAN_POINT('Ctrl Pts',(2.51273423521776,0.952480227291854,
8.84279849653635));
#375917=CARTESIAN_POINT('Ctrl Pts',(2.5243280569779,0.965742402914834,8.82725662040549));
#375918=CARTESIAN_POINT('Ctrl Pts',(2.53590957550767,0.978989958767267,
8.81169306718667));
#375919=CARTESIAN_POINT('Ctrl Pts',(2.54747944236022,0.992223662303432,
8.79610912703474));
#375920=CARTESIAN_POINT('',(2.52025288996714,1.05947377310391,8.79610912703474));
#375921=CARTESIAN_POINT('Origin',(0.,1.84795814293585E-15,8.79610912703474));
#375922=CARTESIAN_POINT('',(2.44895572090754,1.06540763642202,8.85933012996512));
#375923=CARTESIAN_POINT('Ctrl Pts',(2.52025288996714,1.05947377310391,8.79610912703474));
#375924=CARTESIAN_POINT('Ctrl Pts',(2.51403871210982,1.0599907920964,8.80163734024559));
#375925=CARTESIAN_POINT('Ctrl Pts',(2.50782226866145,1.06050804322869,8.80716298614018));
#375926=CARTESIAN_POINT('Ctrl Pts',(2.50160351591013,1.0610255307834,8.8126860086129));
#375927=CARTESIAN_POINT('Ctrl Pts',(2.4840729564763,1.06248431949825,8.82825531609049));
#375928=CARTESIAN_POINT('Ctrl Pts',(2.46652403398341,1.06394498792048,8.84380379913848));
#375929=CARTESIAN_POINT('Ctrl Pts',(2.44895572090754,1.06540763642202,8.85933012996512));
#375930=CARTESIAN_POINT('',(2.4351329425359,1.0966335335419,8.85933012996512));
#375931=CARTESIAN_POINT('Origin',(2.45053228172764,1.08477795095059,8.84999761231044));
#375932=CARTESIAN_POINT('',(2.47867338431573,1.15340260064194,8.79610912703474));
#375933=CARTESIAN_POINT('Ctrl Pts',(2.4351329425359,1.0966335335419,8.85933012996512));
#375934=CARTESIAN_POINT('Ctrl Pts',(2.43893872123164,1.10159588157956,8.8538223528706));
#375935=CARTESIAN_POINT('Ctrl Pts',(2.44274304284933,1.10655625436414,8.84831178811348));
#375936=CARTESIAN_POINT('Ctrl Pts',(2.44654593555173,1.11151468971517,8.84279849653635));
#375937=CARTESIAN_POINT('Ctrl Pts',(2.45726622605205,1.12549243548656,8.82725662040549));
#375938=CARTESIAN_POINT('Ctrl Pts',(2.46797517529221,1.13945480325461,8.81169306718667));
#375939=CARTESIAN_POINT('Ctrl Pts',(2.47867338431573,1.15340260064194,8.79610912703474));
#375940=CARTESIAN_POINT('',(2.44719404240187,1.21877012767608,8.79610912703474));
#375941=CARTESIAN_POINT('Origin',(0.,1.84795814293585E-15,8.79610912703474));
#375942=CARTESIAN_POINT('',(2.37566317709457,1.22012377392995,8.85933012996512));
#375943=CARTESIAN_POINT('Ctrl Pts',(2.44719404240187,1.21877012767608,8.79610912703474));
#375944=CARTESIAN_POINT('Ctrl Pts',(2.44095950671884,1.21888794065528,8.80163734024559));
#375945=CARTESIAN_POINT('Ctrl Pts',(2.43472269522642,1.21900584014042,8.80716298614018));
#375946=CARTESIAN_POINT('Ctrl Pts',(2.42848356402811,1.21912382760466,8.8126860086129));
#375947=CARTESIAN_POINT('Ctrl Pts',(2.41089555809492,1.21945643228233,8.82825531609049));
#375948=CARTESIAN_POINT('Ctrl Pts',(2.39328910639828,1.21978973628009,8.84380379913848));
#375949=CARTESIAN_POINT('Ctrl Pts',(2.37566317709457,1.22012377392995,8.85933012996512));
#375950=CARTESIAN_POINT('',(2.35986814900601,1.25039988564422,8.85933012996512));
#375951=CARTESIAN_POINT('Origin',(2.37599543838842,1.23955530066841,8.84999761231045));
#375952=CARTESIAN_POINT('',(2.39968192566131,1.30984196029033,8.79610912703474));
#375953=CARTESIAN_POINT('Ctrl Pts',(2.35986814900601,1.25039988564422,8.85933012996512));
#375954=CARTESIAN_POINT('Ctrl Pts',(2.36334816959086,1.25559587508386,8.8538223528706));
#375955=CARTESIAN_POINT('Ctrl Pts',(2.36682686264628,1.26078979997348,8.84831178811348));
#375956=CARTESIAN_POINT('Ctrl Pts',(2.37030425385407,1.26598169985929,8.84279849653635));
#375957=CARTESIAN_POINT('Ctrl Pts',(2.3801069611214,1.2806175782235,8.82725662040549));
#375958=CARTESIAN_POINT('Ctrl Pts',(2.38989933570246,1.29523738354309,8.81169306718667));
#375959=CARTESIAN_POINT('Ctrl Pts',(2.39968192566131,1.30984196029033,8.79610912703474));
#375960=CARTESIAN_POINT('',(2.36407914959489,1.37305829436826,8.79610912703474));
#375961=CARTESIAN_POINT('Origin',(0.,1.84795814293585E-15,8.79610912703474));
#375962=CARTESIAN_POINT('',(2.29260852370876,1.36982616113508,8.85933012996512));
#375963=CARTESIAN_POINT('Ctrl Pts',(2.36407914959489,1.37305829436826,8.79610912703474));
#375964=CARTESIAN_POINT('Ctrl Pts',(2.35784987513058,1.37277641721537,8.80163734024559));
#375965=CARTESIAN_POINT('Ctrl Pts',(2.35161832399031,1.37249448057907,8.80716298614018));
#375966=CARTESIAN_POINT('Ctrl Pts',(2.34538445227341,1.37221248311705,8.8126860086129));
#375967=CARTESIAN_POINT('Ctrl Pts',(2.32781127272985,1.37141753701358,8.82825531609049));
#375968=CARTESIAN_POINT('Ctrl Pts',(2.31021964051605,1.37062210696925,8.84380379913848));
#375969=CARTESIAN_POINT('Ctrl Pts',(2.29260852370876,1.36982616113508,8.85933012996512));
#375970=CARTESIAN_POINT('',(2.27490615106173,1.39902807640649,8.85933012996512));
#375971=CARTESIAN_POINT('Origin',(2.29169512014344,1.38923905177201,8.84999761231047));
#375972=CARTESIAN_POINT('',(2.31082965924419,1.46089889836366,8.79610912703474));
#375973=CARTESIAN_POINT('Ctrl Pts',(2.27490615106173,1.39902807640649,8.85933012996512));
#375974=CARTESIAN_POINT('Ctrl Pts',(2.27804611338464,1.40443635581296,8.8538223528706));
#375975=CARTESIAN_POINT('Ctrl Pts',(2.28118488318185,1.40984248985616,8.84831178811348));
#375976=CARTESIAN_POINT('Ctrl Pts',(2.28432248354865,1.41524651964647,8.84279849653635));
#375977=CARTESIAN_POINT('Ctrl Pts',(2.29316732615615,1.43048038863991,8.82725662040549));
#375978=CARTESIAN_POINT('Ctrl Pts',(2.30200288711052,1.44569755559504,8.81169306718667));
#375979=CARTESIAN_POINT('Ctrl Pts',(2.31082965924419,1.46089889836366,8.79610912703474));
#375980=CARTESIAN_POINT('',(2.27124974846883,1.5217042700088,8.79610912703474));
#375981=CARTESIAN_POINT('Origin',(0.,1.84795814293585E-15,8.79610912703474));
#375982=CARTESIAN_POINT('',(2.20013305013605,1.51389963881731,8.85933012996512));
#375983=CARTESIAN_POINT('Ctrl Pts',(2.27124974846883,1.5217042700088,8.79610912703474));
#375984=CARTESIAN_POINT('Ctrl Pts',(2.26505133264819,1.52102386101751,8.80163734024559));
#375985=CARTESIAN_POINT('Ctrl Pts',(2.25885064864038,1.52034324679789,8.80716298614018));
#375986=CARTESIAN_POINT('Ctrl Pts',(2.25264765272093,1.51966242319766,8.8126860086129));
#375987=CARTESIAN_POINT('Ctrl Pts',(2.23516151153118,1.5177431929171,8.82825531609049));
#375988=CARTESIAN_POINT('Ctrl Pts',(2.21765698659038,1.51582229742335,8.84380379913848));
#375989=CARTESIAN_POINT('Ctrl Pts',(2.20013305013605,1.51389963881731,8.85933012996512));
#375990=CARTESIAN_POINT('',(2.1805960757769,1.54190736071222,8.85933012996512));
#375991=CARTESIAN_POINT('Origin',(2.19797773508275,1.53321412162104,8.84999761231047));
#375992=CARTESIAN_POINT('',(2.21248169808583,1.60595268950179,8.79610912703474));
#375993=CARTESIAN_POINT('Ctrl Pts',(2.1805960757769,1.54190736071222,8.85933012996512));
#375994=CARTESIAN_POINT('Ctrl Pts',(2.18338307705916,1.54750570630538,8.8538223528706));
#375995=CARTESIAN_POINT('Ctrl Pts',(2.1861690257198,1.55310183453776,8.84831178811348));
#375996=CARTESIAN_POINT('Ctrl Pts',(2.18895394217269,1.55869578791499,8.84279849653635));
#375997=CARTESIAN_POINT('Ctrl Pts',(2.19680457476489,1.57446504830231,8.82725662040549));
#375998=CARTESIAN_POINT('Ctrl Pts',(2.20464701487736,1.5902170462899,8.81169306718667));
#375999=CARTESIAN_POINT('Ctrl Pts',(2.21248169808583,1.60595268950179,8.79610912703474));
#376000=CARTESIAN_POINT('',(2.16908729494478,1.66409723639934,8.79610912703474));
#376001=CARTESIAN_POINT('Origin',(0.,1.84795814293585E-15,8.79610912703474));
#376002=CARTESIAN_POINT('',(2.09861675793327,1.65175217815318,8.85933012996512));
#376003=CARTESIAN_POINT('Ctrl Pts',(2.16908729494478,1.66409723639934,8.79610912703474));
#376004=CARTESIAN_POINT('Ctrl Pts',(2.16294520838797,1.66302109151613,8.80163734024559));
#376005=CARTESIAN_POINT('Ctrl Pts',(2.15680087145325,1.661944596503,8.80716298614018));
#376006=CARTESIAN_POINT('Ctrl Pts',(2.15065424077201,1.66086774441479,8.8126860086129));
#376007=CARTESIAN_POINT('Ctrl Pts',(2.13332699224099,1.65783211648603,8.82825531609049));
#376008=CARTESIAN_POINT('Ctrl Pts',(2.11598150442088,1.65479364891447,8.84380379913848));
#376009=CARTESIAN_POINT('Ctrl Pts',(2.09861675793327,1.65175217815318,8.85933012996512));
#376010=CARTESIAN_POINT('',(2.07732546348031,1.6784506169347,8.85933012996512));
#376011=CARTESIAN_POINT('Origin',(2.09522838804386,1.67088888577093,8.84999761231045));
#376012=CARTESIAN_POINT('',(2.10504217505419,1.74440727656298,8.79610912703474));
#376013=CARTESIAN_POINT('Ctrl Pts',(2.07732546348031,1.6784506169347,8.85933012996512));
#376014=CARTESIAN_POINT('Ctrl Pts',(2.07974805133585,1.68421602391166,8.8538223528706));
#376015=CARTESIAN_POINT('Ctrl Pts',(2.08216973079928,1.68997915064194,8.84831178811348));
#376016=CARTESIAN_POINT('Ctrl Pts',(2.0845905195192,1.69574004085178,8.84279849653635));
#376017=CARTESIAN_POINT('Ctrl Pts',(2.09141468216281,1.71197989335955,8.82725662040549));
#376018=CARTESIAN_POINT('Ctrl Pts',(2.09823177516477,1.72820199404107,8.81169306718667));
#376019=CARTESIAN_POINT('Ctrl Pts',(2.10504217505419,1.74440727656298,8.79610912703474));
#376020=CARTESIAN_POINT('',(2.05801159645803,1.79965207029777,8.79610912703474));
#376021=CARTESIAN_POINT('Origin',(0.,1.84795814293585E-15,8.79610912703474));
#376022=CARTESIAN_POINT('',(1.98847679932026,1.7828173134893,8.85933012996512));
#376023=CARTESIAN_POINT('Ctrl Pts',(2.05801159645803,1.79965207029777,8.79610912703474));
#376024=CARTESIAN_POINT('Ctrl Pts',(2.05195107831618,1.7981846116328,8.80163734024559));
#376025=CARTESIAN_POINT('Ctrl Pts',(2.04588833685297,1.79671665937509,8.80716298614018));
#376026=CARTESIAN_POINT('Ctrl Pts',(2.03982332923388,1.7952482038151,8.8126860086129));
#376027=CARTESIAN_POINT('Ctrl Pts',(2.02272617474248,1.79110865228445,8.82825531609049));
#376028=CARTESIAN_POINT('Ctrl Pts',(2.00561100037311,1.78696509835008,8.84380379913848));
#376029=CARTESIAN_POINT('Ctrl Pts',(1.98847679932026,1.7828173134893,8.85933012996512));
#376030=CARTESIAN_POINT('',(1.96551867526936,1.80809675954566,8.85933012996512));
#376031=CARTESIAN_POINT('Origin',(1.9838692981334,1.80169760908465,8.84999761231047));
#376032=CARTESIAN_POINT('',(1.98895258219513,1.87569371995059,8.79610912703474));
#376033=CARTESIAN_POINT('Ctrl Pts',(1.96551867526936,1.80809675954566,8.85933012996512));
#376034=CARTESIAN_POINT('Ctrl Pts',(1.96756689476504,1.81400553661248,8.8538223528706));
#376035=CARTESIAN_POINT('Ctrl Pts',(1.9696143538309,1.81991197991674,8.84831178811348));
#376036=CARTESIAN_POINT('Ctrl Pts',(1.97166106727774,1.8258161342256,8.84279849653635));
#376037=CARTESIAN_POINT('Ctrl Pts',(1.97743071802468,1.84245984581644,8.82725662040549));
#376038=CARTESIAN_POINT('Ctrl Pts',(1.98319445101872,1.85908538910056,8.81169306718667));
#376039=CARTESIAN_POINT('Ctrl Pts',(1.98895258219513,1.87569371995059,8.79610912703474));
#376040=CARTESIAN_POINT('',(1.93847908687933,1.92781174781519,8.79610912703474));
#376041=CARTESIAN_POINT('Origin',(0.,1.84795814293585E-15,8.79610912703474));
#376042=CARTESIAN_POINT('',(1.8701657630119,1.90655647007117,8.85933012996512));
#376043=CARTESIAN_POINT('Ctrl Pts',(1.93847908687933,1.92781174781519,8.79610912703474));
#376044=CARTESIAN_POINT('Ctrl Pts',(1.93252504112147,1.92595900547089,8.80163734024559));
#376045=CARTESIAN_POINT('Ctrl Pts',(1.9265688082349,1.9241056280993,8.80716298614018));
#376046=CARTESIAN_POINT('Ctrl Pts',(1.92061034609519,1.9222516032664,8.8126860086129));
#376047=CARTESIAN_POINT('Ctrl Pts',(1.90381354151855,1.91702513843903,8.82825531609049));
#376048=CARTESIAN_POINT('Ctrl Pts',(1.88699901052259,1.91179352489375,8.84380379913848));
#376049=CARTESIAN_POINT('Ctrl Pts',(1.8701657630119,1.90655647007117,8.85933012996512));
#376050=CARTESIAN_POINT('',(1.8456351492193,1.93031304473611,8.85933012996512));
#376051=CARTESIAN_POINT('Origin',(1.86435806373829,1.92510277045971,8.84999761231047));
#376052=CARTESIAN_POINT('',(1.86468995654684,1.99927253550788,8.79610912703474));
#376053=CARTESIAN_POINT('Ctrl Pts',(1.8456351492193,1.93031304473611,8.85933012996512));
#376054=CARTESIAN_POINT('Ctrl Pts',(1.84730058378186,1.93634091146039,8.8538223528706));
#376055=CARTESIAN_POINT('Ctrl Pts',(1.84896540900168,1.94236640049617,8.84831178811348));
#376056=CARTESIAN_POINT('Ctrl Pts',(1.85062963679086,1.94838955746756,8.84279849653635));
#376057=CARTESIAN_POINT('Ctrl Pts',(1.85532106690863,1.96536873556047,8.82725662040549));
#376058=CARTESIAN_POINT('Ctrl Pts',(1.86000775547956,1.98232940352367,8.81169306718667));
#376059=CARTESIAN_POINT('Ctrl Pts',(1.86468995654684,1.99927253550788,8.79610912703474));
#376060=CARTESIAN_POINT('',(1.81098095093019,2.04804963334651,8.79610912703474));
#376061=CARTESIAN_POINT('Origin',(0.,1.84795814293585E-15,8.79610912703474));
#376062=CARTESIAN_POINT('',(1.74416981443404,2.02246117716244,8.85933012996512));
#376063=CARTESIAN_POINT('Ctrl Pts',(1.81098095093019,2.04804963334651,8.79610912703474));
#376064=CARTESIAN_POINT('Ctrl Pts',(1.80515784400747,2.04581922063858,8.80163734024559));
#376065=CARTESIAN_POINT('Ctrl Pts',(1.79933259513608,2.04358803407827,8.80716298614018));
#376066=CARTESIAN_POINT('Ctrl Pts',(1.79350516307477,2.0413560585582,8.8126860086129));
#376067=CARTESIAN_POINT('Ctrl Pts',(1.77707773008579,2.03506415709916,8.82825531609049));
#376068=CARTESIAN_POINT('Ctrl Pts',(1.76063293697782,2.02876598176522,8.84380379913848));
#376069=CARTESIAN_POINT('Ctrl Pts',(1.74416981443404,2.02246117716244,8.85933012996512));
#376070=CARTESIAN_POINT('',(1.71816751245359,2.0445972595749,8.85933012996512));
#376071=CARTESIAN_POINT('Origin',(1.73718578215574,2.0405972716177,8.84999761231047));
#376072=CARTESIAN_POINT('',(1.73276491989236,2.11463591137415,8.79610912703474));
#376073=CARTESIAN_POINT('Ctrl Pts',(1.71816751245359,2.0445972595749,8.85933012996512));
#376074=CARTESIAN_POINT('Ctrl Pts',(1.7194433184552,2.05071944615928,8.8538223528706));
#376075=CARTESIAN_POINT('Ctrl Pts',(1.72071866870503,2.05683922089967,8.84831178811348));
#376076=CARTESIAN_POINT('Ctrl Pts',(1.7219935721676,2.06295663008964,8.84279849653635));
#376077=CARTESIAN_POINT('Ctrl Pts',(1.72558750356353,2.08020150359982,8.82725662040549));
#376078=CARTESIAN_POINT('Ctrl Pts',(1.72917788910273,2.09742760121938,8.81169306718667));
#376079=CARTESIAN_POINT('Ctrl Pts',(1.73276491989236,2.11463591137415,8.79610912703474));
#376080=CARTESIAN_POINT('',(1.67604110579947,2.15987164362914,8.79610912703474));
#376081=CARTESIAN_POINT('Origin',(0.,1.84795814293585E-15,8.79610912703474));
#376082=CARTESIAN_POINT('',(1.61100669796541,2.13005515746019,8.85933012996512));
#376083=CARTESIAN_POINT('Ctrl Pts',(1.67604110579947,2.15987164362914,8.79610912703474));
#376084=CARTESIAN_POINT('Ctrl Pts',(1.6703728661073,2.15727272580182,8.80163734024559));
#376085=CARTESIAN_POINT('Ctrl Pts',(1.6647025384482,2.15467289847697,8.80716298614018));
#376086=CARTESIAN_POINT('Ctrl Pts',(1.65903008263362,2.15207214393589,8.8126860086129));
#376087=CARTESIAN_POINT('Ctrl Pts',(1.64303952507813,2.14474066061787,8.82825531609049));
#376088=CARTESIAN_POINT('Ctrl Pts',(1.62703204504042,2.13740180404867,8.84380379913848));
#376089=CARTESIAN_POINT('Ctrl Pts',(1.61100669796541,2.13005515746019,8.85933012996512));
#376090=CARTESIAN_POINT('',(1.58363955683344,2.15047978570935,8.85933012996512));
#376091=CARTESIAN_POINT('Origin',(1.60287503156912,2.14770652087988,8.84999761231047));
#376092=CARTESIAN_POINT('',(1.59371958050512,2.22130979469261,8.79610912703474));
#376093=CARTESIAN_POINT('Ctrl Pts',(1.58363955683344,2.15047978570935,8.85933012996512));
#376094=CARTESIAN_POINT('Ctrl Pts',(1.58452049171356,2.15667113477597,8.8538223528706));
#376095=CARTESIAN_POINT('Ctrl Pts',(1.58540112630568,2.16286004775387,8.84831178811348));
#376096=CARTESIAN_POINT('Ctrl Pts',(1.58628146658983,2.16904657141586,8.84279849653635));
#376097=CARTESIAN_POINT('Ctrl Pts',(1.58876313102893,2.18648627745904,8.82725662040549));
#376098=CARTESIAN_POINT('Ctrl Pts',(1.59124245987207,2.20390701900486,8.81169306718667));
#376099=CARTESIAN_POINT('Ctrl Pts',(1.59371958050512,2.22130979469261,8.79610912703474));
#376100=CARTESIAN_POINT('',(1.53421404825534,2.26281827803709,8.79610912703474));
#376101=CARTESIAN_POINT('Origin',(0.,1.84795814293585E-15,8.79610912703474));
#376102=CARTESIAN_POINT('',(1.47122360941498,2.22889628422053,8.85933012996512));
#376103=CARTESIAN_POINT('Ctrl Pts',(1.53421404825534,2.26281827803709,8.79610912703474));
#376104=CARTESIAN_POINT('Ctrl Pts',(1.52872396780644,2.2598615346012,8.80163734024559));
#376105=CARTESIAN_POINT('Ctrl Pts',(1.52323186195228,2.25690374975993,8.80716298614018));
#376106=CARTESIAN_POINT('Ctrl Pts',(1.51773769172209,2.25394490325611,8.8126860086129));
#376107=CARTESIAN_POINT('Ctrl Pts',(1.50224971823106,2.24560396471668,8.82825531609049));
#376108=CARTESIAN_POINT('Ctrl Pts',(1.48674532943268,2.23725458384804,8.84380379913848));
#376109=CARTESIAN_POINT('Ctrl Pts',(1.47122360941498,2.22889628422053,8.85933012996512));
#376110=CARTESIAN_POINT('',(1.44260408658464,2.24752552912785,8.85933012996512));
#376111=CARTESIAN_POINT('Origin',(1.46197772366217,2.24599038336617,8.84999761231045));
#376112=CARTESIAN_POINT('',(1.44812530550982,2.31885583959522,8.79610912703474));
#376113=CARTESIAN_POINT('Ctrl Pts',(1.44260408658464,2.24752552912785,8.85933012996512));
#376114=CARTESIAN_POINT('Ctrl Pts',(1.4430865303929,2.25376059909535,8.8538223528706));
#376115=CARTESIAN_POINT('Ctrl Pts',(1.44356883061086,2.25999321873982,8.84831178811348));
#376116=CARTESIAN_POINT('Ctrl Pts',(1.44405099020954,2.26622343512111,8.84279849653635));
#376117=CARTESIAN_POINT('Ctrl Pts',(1.44541019000031,2.28378631020436,8.82725662040549));
#376118=CARTESIAN_POINT('Ctrl Pts',(1.44676827405337,2.30133011011269,8.81169306718667));
#376119=CARTESIAN_POINT('Ctrl Pts',(1.44812530550982,2.31885583959522,8.79610912703474));
#376120=CARTESIAN_POINT('',(1.38608257609904,2.35646650676758,8.79610912703474));
#376121=CARTESIAN_POINT('Origin',(0.,1.84795814293585E-15,8.79610912703474));
#376122=CARTESIAN_POINT('',(1.325394947477,2.31857839805226,8.85933012996512));
#376123=CARTESIAN_POINT('Ctrl Pts',(1.38608257609904,2.35646650676758,8.79610912703474));
#376124=CARTESIAN_POINT('Ctrl Pts',(1.3807932148116,2.35316408761612,8.80163734024559));
#376125=CARTESIAN_POINT('Ctrl Pts',(1.37550189900337,2.34986049943079,8.80716298614018));
#376126=CARTESIAN_POINT('Ctrl Pts',(1.37020859108156,2.3465557194992,8.8126860086129));
#376127=CARTESIAN_POINT('Ctrl Pts',(1.35528684506022,2.33723960044393,8.82825531609049));
#376128=CARTESIAN_POINT('Ctrl Pts',(1.34034925836042,2.32791400467277,8.84380379913848));
#376129=CARTESIAN_POINT('Ctrl Pts',(1.325394947477,2.31857839805226,8.85933012996512));
#376130=CARTESIAN_POINT('',(1.29564064670646,2.33533570805445,8.85933012996512));
#376131=CARTESIAN_POINT('Origin',(1.31507283569545,2.33504498960377,8.84999761231045));
#376132=CARTESIAN_POINT('',(1.29658037301227,2.40687320845992,8.79610912703474));
#376133=CARTESIAN_POINT('Ctrl Pts',(1.29564064670646,2.33533570805445,8.85933012996512));
#376134=CARTESIAN_POINT('Ctrl Pts',(1.29572261697775,2.34158887768292,8.8538223528706));
#376135=CARTESIAN_POINT('Ctrl Pts',(1.29580460094652,2.34783959282295,8.84831178811348));
#376136=CARTESIAN_POINT('Ctrl Pts',(1.29588659856252,2.35408790062805,8.84279849653635));
#376137=CARTESIAN_POINT('Ctrl Pts',(1.29611774846146,2.37170177513041,8.82725662040549));
#376138=CARTESIAN_POINT('Ctrl Pts',(1.29634900706576,2.3892965421643,8.81169306718667));
#376139=CARTESIAN_POINT('Ctrl Pts',(1.29658037301227,2.40687320845992,8.79610912703474));
#376140=CARTESIAN_POINT('',(1.23225539332378,2.44043150916129,8.79610912703474));
#376141=CARTESIAN_POINT('Origin',(0.,1.84795814293585E-15,8.79610912703474));
#376142=CARTESIAN_POINT('',(1.17411995340351,2.39873297591288,8.85933012996512));
#376143=CARTESIAN_POINT('Ctrl Pts',(1.23225539332378,2.44043150916129,8.79610912703474));
#376144=CARTESIAN_POINT('Ctrl Pts',(1.22718848631789,2.43679698464291,8.80163734024559));
#376145=CARTESIAN_POINT('Ctrl Pts',(1.22211970370724,2.433161168266,8.80716298614018));
#376146=CARTESIAN_POINT('Ctrl Pts',(1.21704900943146,2.42952403495623,8.8126860086129));
#376147=CARTESIAN_POINT('Ctrl Pts',(1.20275480753491,2.41927101731663,8.82825531609049));
#376148=CARTESIAN_POINT('Ctrl Pts',(1.18844540468154,2.40900752751631,8.84380379913848));
#376149=CARTESIAN_POINT('Ctrl Pts',(1.17411995340351,2.39873297591288,8.85933012996512));
#376150=CARTESIAN_POINT('',(1.14335314149692,2.41354949162872,8.85933012996512));
#376151=CARTESIAN_POINT('Origin',(1.16276403136462,2.41450439511349,8.84999761231047));
#376152=CARTESIAN_POINT('',(1.1397075136464,2.48500021903836,8.79610912703474));
#376153=CARTESIAN_POINT('Ctrl Pts',(1.14335314149692,2.41354949162872,8.85933012996512));
#376154=CARTESIAN_POINT('Ctrl Pts',(1.14303430139782,2.41979506530285,8.8538223528706));
#376155=CARTESIAN_POINT('Ctrl Pts',(1.14271563222767,2.42603819040915,8.84831178811348));
#376156=CARTESIAN_POINT('Ctrl Pts',(1.1423971309152,2.43227891400103,8.84279849653635));
#376157=CARTESIAN_POINT('Ctrl Pts',(1.1414992810778,2.44987140873402,8.82725662040549));
#376158=CARTESIAN_POINT('Ctrl Pts',(1.14060276394212,2.46744484222165,8.81169306718667));
#376159=CARTESIAN_POINT('Ctrl Pts',(1.1397075136464,2.48500021903836,8.79610912703474));
#376160=CARTESIAN_POINT('',(1.07336460881939,2.51436825501293,8.79610912703474));
#376161=CARTESIAN_POINT('Origin',(0.,1.84795814293585E-15,8.79610912703474));
#376162=CARTESIAN_POINT('',(1.01802024859354,2.46903064544887,8.85933012996512));
#376163=CARTESIAN_POINT('Ctrl Pts',(1.07336460881939,2.51436825501293,8.79610912703474));
#376164=CARTESIAN_POINT('Ctrl Pts',(1.06854097710278,2.51041656016849,8.80163734024559));
#376165=CARTESIAN_POINT('Ctrl Pts',(1.06371555640471,2.50646345594937,8.80716298614018));
#376166=CARTESIAN_POINT('Ctrl Pts',(1.05888831234541,2.50250891502236,8.8126860086129));
#376167=CARTESIAN_POINT('Ctrl Pts',(1.04528039251534,2.49136113064717,8.82825531609049));
#376168=CARTESIAN_POINT('Ctrl Pts',(1.03165797391409,2.4802019216988,8.84380379913848));
#376169=CARTESIAN_POINT('Ctrl Pts',(1.01802024859354,2.46903064544887,8.85933012996512));
#376170=CARTESIAN_POINT('',(0.986367352980481,2.48184548263715,8.85933012996512));
#376171=CARTESIAN_POINT('Origin',(1.00567718021681,2.48404208415414,8.84999761231047));
#376172=CARTESIAN_POINT('',(0.978151351640454,2.55291583068591,8.79610912703474));
#376173=CARTESIAN_POINT('Ctrl Pts',(0.986367352980481,2.48184548263715,
8.85933012996512));
#376174=CARTESIAN_POINT('Ctrl Pts',(0.985649012693359,2.48805779595504,
8.8538223528706));
#376175=CARTESIAN_POINT('Ctrl Pts',(0.984930999864269,2.4942676766874,8.84831178811348));
#376176=CARTESIAN_POINT('Ctrl Pts',(0.984213308413526,2.50047517159419,
8.84279849653635));
#376177=CARTESIAN_POINT('Ctrl Pts',(0.982190148297363,2.51797399522337,
8.82725662040549));
#376178=CARTESIAN_POINT('Ctrl Pts',(0.980169539402921,2.53545388215706,
8.81169306718667));
#376179=CARTESIAN_POINT('Ctrl Pts',(0.978151351640454,2.55291583068591,
8.79610912703474));
#376180=CARTESIAN_POINT('',(0.910063138901376,2.57797292237443,8.79610912703474));
#376181=CARTESIAN_POINT('Origin',(0.,1.84795814293585E-15,8.79610912703474));
#376182=CARTESIAN_POINT('',(0.857737280217445,2.5291825384573,8.85933012996512));
#376183=CARTESIAN_POINT('Ctrl Pts',(0.910063138901376,2.57797292237443,
8.79610912703474));
#376184=CARTESIAN_POINT('Ctrl Pts',(0.905502603811445,2.57372029556567,
8.80163734024559));
#376185=CARTESIAN_POINT('Ctrl Pts',(0.900940373714648,2.56946614765751,
8.80716298614018));
#376186=CARTESIAN_POINT('Ctrl Pts',(0.896376416053107,2.56521044917019,
8.8126860086129));
#376187=CARTESIAN_POINT('Ctrl Pts',(0.883510696150981,2.5532137066966,8.82825531609049));
#376188=CARTESIAN_POINT('Ctrl Pts',(0.870631239241884,2.54120463418338,
8.84380379913848));
#376189=CARTESIAN_POINT('Ctrl Pts',(0.857737280217445,2.5291825384573,8.85933012996512));
#376190=CARTESIAN_POINT('',(0.825328369435515,2.53994303820323,8.85933012996512));
#376191=CARTESIAN_POINT('Origin',(0.844457785818413,2.54337231144565,8.84999761231045));
#376192=CARTESIAN_POINT('',(0.812575755917816,2.61034096358643,8.79610912703474));
#376193=CARTESIAN_POINT('Ctrl Pts',(0.825328369435515,2.53994303820323,
8.85933012996512));
#376194=CARTESIAN_POINT('Ctrl Pts',(0.824213480774689,2.54609656343693,
8.8538223528706));
#376195=CARTESIAN_POINT('Ctrl Pts',(0.823099074755386,2.5522476820634,8.84831178811348));
#376196=CARTESIAN_POINT('Ctrl Pts',(0.821985142314494,2.55839644035703,
8.84279849653635));
#376197=CARTESIAN_POINT('Ctrl Pts',(0.818844985518447,2.57572968646262,
8.82725662040549));
#376198=CARTESIAN_POINT('Ctrl Pts',(0.81570858798061,2.59304419823753,8.81169306718667));
#376199=CARTESIAN_POINT('Ctrl Pts',(0.812575755917816,2.61034096358643,
8.79610912703474));
#376200=CARTESIAN_POINT('',(0.743022024337684,2.63098414602443,8.79610912703474));
#376201=CARTESIAN_POINT('Origin',(0.,1.84795814293585E-15,8.79610912703474));
#376202=CARTESIAN_POINT('',(0.693929685372865,2.57894147790726,8.85933012996512));
#376203=CARTESIAN_POINT('Ctrl Pts',(0.743022024337684,2.63098414602443,
8.79610912703474));
#376204=CARTESIAN_POINT('Ctrl Pts',(0.738743326091345,2.6264480622071,8.80163734024559));
#376205=CARTESIAN_POINT('Ctrl Pts',(0.734463033777886,2.62191035181617,
8.80716298614018));
#376206=CARTESIAN_POINT('Ctrl Pts',(0.730181116795098,2.61737098334645,
8.8126860086129));
#376207=CARTESIAN_POINT('Ctrl Pts',(0.71811046482369,2.60457457996258,8.82825531609049));
#376208=CARTESIAN_POINT('Ctrl Pts',(0.706026894057816,2.59176499173941,
8.84380379913848));
#376209=CARTESIAN_POINT('Ctrl Pts',(0.693929685372865,2.57894147790726,
8.85933012996512));
#376210=CARTESIAN_POINT('',(0.660897934588157,2.58760342300926,8.85933012996512));
#376211=CARTESIAN_POINT('Origin',(0.679768333242446,2.59225127635775,8.84999761231048));
#376212=CARTESIAN_POINT('',(0.643661112117155,2.65703964555121,8.79610912703474));
#376213=CARTESIAN_POINT('Ctrl Pts',(0.660897934588157,2.58760342300926,
8.85933012996512));
#376214=CARTESIAN_POINT('Ctrl Pts',(0.659391078870276,2.59367287400365,
8.8538223528706));
#376215=CARTESIAN_POINT('Ctrl Pts',(0.657884858994133,2.5997399542584,8.84831178811348));
#376216=CARTESIAN_POINT('Ctrl Pts',(0.65637926295043,2.60580470937213,8.84279849653635));
#376217=CARTESIAN_POINT('Ctrl Pts',(0.652135013052335,2.62290115192791,
8.82725662040549));
#376218=CARTESIAN_POINT('Ctrl Pts',(0.647895715001341,2.63997913950121,
8.81169306718667));
#376219=CARTESIAN_POINT('Ctrl Pts',(0.643661112117155,2.65703964555121,
8.79610912703474));
#376220=CARTESIAN_POINT('',(0.572927672898268,2.67318409147409,8.79610912703474));
#376221=CARTESIAN_POINT('Origin',(0.,1.84795814293585E-15,8.79610912703474));
#376222=CARTESIAN_POINT('',(0.527270584603639,2.61810299364327,8.85933012996512));
#376223=CARTESIAN_POINT('Ctrl Pts',(0.572927672898268,2.67318409147409,
8.79610912703474));
#376224=CARTESIAN_POINT('Ctrl Pts',(0.568948393584391,2.66838319038958,
8.80163734024559));
#376225=CARTESIAN_POINT('Ctrl Pts',(0.564967627693506,2.66358056394121,
8.80716298614018));
#376226=CARTESIAN_POINT('Ctrl Pts',(0.560985346704822,2.65877617872783,
8.8126860086129));
#376227=CARTESIAN_POINT('Ctrl Pts',(0.549759363562228,2.64523269760001,
8.82825531609049));
#376228=CARTESIAN_POINT('Ctrl Pts',(0.538521332923773,2.63167523101254,
8.84380379913848));
#376229=CARTESIAN_POINT('Ctrl Pts',(0.527270584603639,2.61810299364327,
8.85933012996512));
#376230=CARTESIAN_POINT('',(0.493751728365416,2.62463079031095,8.85933012996512));
#376231=CARTESIAN_POINT('Origin',(0.512285566775364,2.63047812473921,8.84999761231043));
#376232=CARTESIAN_POINT('',(0.472101526741932,2.69281998167919,8.79610912703474));
#376233=CARTESIAN_POINT('Ctrl Pts',(0.493751728365416,2.62463079031095,
8.85933012996512));
#376234=CARTESIAN_POINT('Ctrl Pts',(0.491859097583844,2.63059122639,8.8538223528706));
#376235=CARTESIAN_POINT('Ctrl Pts',(0.489967253231417,2.63654933733887,
8.84831178811348));
#376236=CARTESIAN_POINT('Ctrl Pts',(0.488076180401994,2.64250516789305,
8.84279849653635));
#376237=CARTESIAN_POINT('Ctrl Pts',(0.482745277935072,2.6592945539494,8.82725662040549));
#376238=CARTESIAN_POINT('Ctrl Pts',(0.477420499555938,2.67606584020692,
8.81169306718667));
#376239=CARTESIAN_POINT('Ctrl Pts',(0.472101526741932,2.69281998167919,
8.79610912703474));
#376240=CARTESIAN_POINT('',(0.40047903875831,2.70439935009569,8.79610912703474));
#376241=CARTESIAN_POINT('Origin',(0.,1.84795814293585E-15,8.79610912703474));
#376242=CARTESIAN_POINT('',(0.358444815903088,2.64650616259708,8.85933012996512));
#376243=CARTESIAN_POINT('Ctrl Pts',(0.40047903875831,2.70439935009569,8.79610912703474));
#376244=CARTESIAN_POINT('Ctrl Pts',(0.396815530089149,2.69935335967635,
8.80163734024559));
#376245=CARTESIAN_POINT('Ctrl Pts',(0.393150648441755,2.69430555219278,
8.80716298614018));
#376246=CARTESIAN_POINT('Ctrl Pts',(0.389484367493953,2.68925589248512,
8.8126860086129));
#376247=CARTESIAN_POINT('Ctrl Pts',(0.379149183152874,2.67502098668236,
8.82825531609049));
#376248=CARTESIAN_POINT('Ctrl Pts',(0.36880287212028,2.66077135226888,8.84380379913848));
#376249=CARTESIAN_POINT('Ctrl Pts',(0.358444815903088,2.64650616259708,
8.85933012996512));
#376250=CARTESIAN_POINT('',(0.324576590381406,2.65087298671372,8.85933012996512));
#376251=CARTESIAN_POINT('Origin',(0.342697709029468,2.65789577427024,8.84999761231047));
#376252=CARTESIAN_POINT('',(0.298601974927864,2.71753494289438,8.79610912703474));
#376253=CARTESIAN_POINT('Ctrl Pts',(0.324576590381406,2.65087298671372,
8.85933012996512));
#376254=CARTESIAN_POINT('Ctrl Pts',(0.322305961761993,2.65669991516707,
8.8538223528706));
#376255=CARTESIAN_POINT('Ctrl Pts',(0.320036266927523,2.66252457365416,
8.84831178811348));
#376256=CARTESIAN_POINT('Ctrl Pts',(0.317767488136271,2.66834700586353,
8.84279849653635));
#376257=CARTESIAN_POINT('Ctrl Pts',(0.311371838922235,2.68476034423181,
8.82725662040549));
#376258=CARTESIAN_POINT('Ctrl Pts',(0.304983460871482,2.70115601236091,
8.81169306718667));
#376259=CARTESIAN_POINT('Ctrl Pts',(0.298601974927864,2.71753494289438,
8.79610912703474));
#376260=CARTESIAN_POINT('',(0.226384750345611,2.72450165169591,8.79610912703474));
#376261=CARTESIAN_POINT('Origin',(0.,1.84795814293585E-15,8.79610912703474));
#376262=CARTESIAN_POINT('',(0.188146120567823,2.66403427005499,8.85933012996512));
#376263=CARTESIAN_POINT('Ctrl Pts',(0.226384750345611,2.72450165169591,
8.79610912703474));
#376264=CARTESIAN_POINT('Ctrl Pts',(0.223052066464109,2.71923130699874,
8.80163734024559));
#376265=CARTESIAN_POINT('Ctrl Pts',(0.219718128845009,2.71395906100366,
8.80716298614018));
#376266=CARTESIAN_POINT('Ctrl Pts',(0.21638291347292,2.70868487693661,8.8126860086129));
#376267=CARTESIAN_POINT('Ctrl Pts',(0.206980997422702,2.69381704074024,
8.82825531609049));
#376268=CARTESIAN_POINT('Ctrl Pts',(0.19756892120728,2.67893379330508,8.84380379913848));
#376269=CARTESIAN_POINT('Ctrl Pts',(0.188146120567823,2.66403427005499,
8.85933012996512));
#376270=CARTESIAN_POINT('',(0.15406769756606,2.66622217740361,8.85933012996512));
#376271=CARTESIAN_POINT('Origin',(0.171701632888751,2.67439155994798,8.84999761231047));
#376272=CARTESIAN_POINT('',(0.123875403548898,2.7310829701198,8.79610912703474));
#376273=CARTESIAN_POINT('Ctrl Pts',(0.15406769756606,2.66622217740361,8.85933012996512));
#376274=CARTESIAN_POINT('Ctrl Pts',(0.151428401608852,2.67189165413237,
8.8538223528706));
#376275=CARTESIAN_POINT('Ctrl Pts',(0.148790182955263,2.67755892538658,
8.84831178811348));
#376276=CARTESIAN_POINT('Ctrl Pts',(0.146153021100887,2.68322403362827,
8.84279849653635));
#376277=CARTESIAN_POINT('Ctrl Pts',(0.138718906234218,2.69919387838049,
8.82725662040549));
#376278=CARTESIAN_POINT('Ctrl Pts',(0.13129317972756,2.71514655506395,8.81169306718667));
#376279=CARTESIAN_POINT('Ctrl Pts',(0.123875403548898,2.7310829701198,8.79610912703474));
#376280=CARTESIAN_POINT('',(0.0513601984344042,2.73340839160553,8.79610912703474));
#376281=CARTESIAN_POINT('Origin',(0.,1.84795814293585E-15,8.79610912703474));
#376282=CARTESIAN_POINT('',(0.0170742924659647,2.67061528926368,8.85933012996512));
#376283=CARTESIAN_POINT('Ctrl Pts',(0.0513601984344042,2.73340839160553,
8.79610912703474));
#376284=CARTESIAN_POINT('Ctrl Pts',(0.0483720340534879,2.72793534960737,
8.80163734024559));
#376285=CARTESIAN_POINT('Ctrl Pts',(0.045382740327487,2.72246032989048,
8.80716298614018));
#376286=CARTESIAN_POINT('Ctrl Pts',(0.0423922956464754,2.71698329421768,
8.8126860086129));
#376287=CARTESIAN_POINT('Ctrl Pts',(0.0339622823768732,2.70154362275576,
8.82825531609049));
#376288=CARTESIAN_POINT('Ctrl Pts',(0.0255231172186754,2.68608792075508,
8.84380379913848));
#376289=CARTESIAN_POINT('Ctrl Pts',(0.0170742924659647,2.67061528926368,
8.85933012996512));
#376290=CARTESIAN_POINT('',(-0.0170742924659647,2.67061528926368,8.85933012996512));
#376291=CARTESIAN_POINT('Origin',(-2.09135470009489E-9,2.6798976970507,
8.84999761231047));
#376292=CARTESIAN_POINT('',(-0.0513601984344042,2.73340839160553,8.79610912703474));
#376293=CARTESIAN_POINT('Ctrl Pts',(-0.0170742924659647,2.67061528926368,
8.85933012996512));
#376294=CARTESIAN_POINT('Ctrl Pts',(-0.0200714103277523,2.67610401717189,
8.8538223528706));
#376295=CARTESIAN_POINT('Ctrl Pts',(-0.0230673117941167,2.68159061315999,
8.84831178811348));
#376296=CARTESIAN_POINT('Ctrl Pts',(-0.0260620200478886,2.68707511828909,
8.84279849653635));
#376297=CARTESIAN_POINT('Ctrl Pts',(-0.0345040521945901,2.70253584590764,
8.82725662040549));
#376298=CARTESIAN_POINT('Ctrl Pts',(-0.0429366132541237,2.71797997817513,
8.81169306718667));
#376299=CARTESIAN_POINT('Ctrl Pts',(-0.0513601984344042,2.73340839160553,
8.79610912703474));
#376300=CARTESIAN_POINT('',(-0.123875403548937,2.73108297011979,8.79610912703474));
#376301=CARTESIAN_POINT('Origin',(0.,1.84795814293585E-15,8.79610912703474));
#376302=CARTESIAN_POINT('',(-0.154067697566098,2.66622217740361,8.85933012996512));
#376303=CARTESIAN_POINT('Ctrl Pts',(-0.123875403548937,2.73108297011979,
8.79610912703474));
#376304=CARTESIAN_POINT('Ctrl Pts',(-0.126506769420867,2.72542972072417,
8.80163734024559));
#376305=CARTESIAN_POINT('Ctrl Pts',(-0.129139135604647,2.71977442531588,
8.80716298614018));
#376306=CARTESIAN_POINT('Ctrl Pts',(-0.131772521215939,2.71411704435172,
8.8126860086129));
#376307=CARTESIAN_POINT('Ctrl Pts',(-0.139195990972168,2.6981689825461,
8.82825531609049));
#376308=CARTESIAN_POINT('Ctrl Pts',(-0.146627566733311,2.68220433677466,
8.84380379913848));
#376309=CARTESIAN_POINT('Ctrl Pts',(-0.154067697566098,2.66622217740361,
8.85933012996512));
#376310=CARTESIAN_POINT('',(-0.188146120567861,2.66403427005499,8.85933012996512));
#376311=CARTESIAN_POINT('Origin',(-0.171701637062902,2.67439155968,8.84999761231046));
#376312=CARTESIAN_POINT('',(-0.22638475034565,2.7245016516959,8.79610912703474));
#376313=CARTESIAN_POINT('Ctrl Pts',(-0.188146120567861,2.66403427005499,
8.85933012996512));
#376314=CARTESIAN_POINT('Ctrl Pts',(-0.191488744534055,2.66931969478233,
8.8538223528706));
#376315=CARTESIAN_POINT('Ctrl Pts',(-0.19483001801145,2.67460306990455,
8.84831178811348));
#376316=CARTESIAN_POINT('Ctrl Pts',(-0.19816996676604,2.67988443491305,
8.84279849653635));
#376317=CARTESIAN_POINT('Ctrl Pts',(-0.207585226071873,2.69477251395182,
8.82725662040549));
#376318=CARTESIAN_POINT('Ctrl Pts',(-0.21698997048211,2.70964463855111,
8.81169306718667));
#376319=CARTESIAN_POINT('Ctrl Pts',(-0.22638475034565,2.7245016516959,8.79610912703474));
#376320=CARTESIAN_POINT('',(-0.298601974927905,2.71753494289437,8.79610912703474));
#376321=CARTESIAN_POINT('Origin',(0.,1.84795814293585E-15,8.79610912703474));
#376322=CARTESIAN_POINT('',(-0.324576590381445,2.65087298671372,8.85933012996512));
#376323=CARTESIAN_POINT('Ctrl Pts',(-0.298601974927905,2.71753494289437,
8.79610912703474));
#376324=CARTESIAN_POINT('Ctrl Pts',(-0.300865729444055,2.71172471651568,
8.80163734024559));
#376325=CARTESIAN_POINT('Ctrl Pts',(-0.303130351128325,2.70591238423786,
8.80716298614018));
#376326=CARTESIAN_POINT('Ctrl Pts',(-0.305395856523559,2.70009790537424,
8.8126860086129));
#376327=CARTESIAN_POINT('Ctrl Pts',(-0.311782278136857,2.68370698723172,
8.82825531609049));
#376328=CARTESIAN_POINT('Ctrl Pts',(-0.318175726562075,2.6672989998434,
8.84380379913848));
#376329=CARTESIAN_POINT('Ctrl Pts',(-0.324576590381445,2.65087298671372,
8.85933012996512));
#376330=CARTESIAN_POINT('',(-0.358444815903127,2.64650616259708,8.85933012996512));
#376331=CARTESIAN_POINT('Origin',(-0.342697713177869,2.65789577373535,8.84999761231049));
#376332=CARTESIAN_POINT('',(-0.400479038758349,2.70439935009568,8.79610912703474));
#376333=CARTESIAN_POINT('Ctrl Pts',(-0.358444815903127,2.64650616259708,
8.85933012996512));
#376334=CARTESIAN_POINT('Ctrl Pts',(-0.36211921041486,2.65156656519963,
8.8538223528706));
#376335=CARTESIAN_POINT('Ctrl Pts',(-0.365792125893867,2.65662500893431,
8.84831178811348));
#376336=CARTESIAN_POINT('Ctrl Pts',(-0.369463590583425,2.66168153156055,
8.84279849653635));
#376337=CARTESIAN_POINT('Ctrl Pts',(-0.379813387728335,2.67593578370929,
8.82725662040549));
#376338=CARTESIAN_POINT('Ctrl Pts',(-0.390151669377183,2.69017478789034,
8.81169306718667));
#376339=CARTESIAN_POINT('Ctrl Pts',(-0.400479038758349,2.70439935009568,
8.79610912703474));
#376340=CARTESIAN_POINT('',(-0.472101526741971,2.69281998167918,8.79610912703474));
#376341=CARTESIAN_POINT('Origin',(0.,1.84795814293585E-15,8.79610912703474));
#376342=CARTESIAN_POINT('',(-0.493751728365454,2.62463079031095,8.85933012996512));
#376343=CARTESIAN_POINT('Ctrl Pts',(-0.472101526741971,2.69281998167918,
8.79610912703474));
#376344=CARTESIAN_POINT('Ctrl Pts',(-0.47398836764946,2.6868766537839,8.80163734024559));
#376345=CARTESIAN_POINT('Ctrl Pts',(-0.475875939017959,2.68093116875663,
8.80716298614018));
#376346=CARTESIAN_POINT('Ctrl Pts',(-0.477764254749519,2.67498348493439,
8.8126860086129));
#376347=CARTESIAN_POINT('Ctrl Pts',(-0.483087385043594,2.65821706425347,
8.82825531609049));
#376348=CARTESIAN_POINT('Ctrl Pts',(-0.488416434081916,2.64143315918795,
8.84380379913848));
#376349=CARTESIAN_POINT('Ctrl Pts',(-0.493751728365454,2.62463079031095,
8.85933012996512));
#376350=CARTESIAN_POINT('',(-0.527270584603676,2.61810299364327,8.85933012996512));
#376351=CARTESIAN_POINT('Origin',(-0.512285570880968,2.63047812393962,8.84999761231045));
#376352=CARTESIAN_POINT('',(-0.572927672898306,2.67318409147408,8.79610912703474));
#376353=CARTESIAN_POINT('Ctrl Pts',(-0.527270584603676,2.61810299364327,
8.85933012996512));
#376354=CARTESIAN_POINT('Ctrl Pts',(-0.531261650785743,2.62291757984128,
8.8538223528706));
#376355=CARTESIAN_POINT('Ctrl Pts',(-0.535251115468821,2.62773030595809,
8.84831178811348));
#376356=CARTESIAN_POINT('Ctrl Pts',(-0.539239009257411,2.63254120786596,
8.84279849653635));
#376357=CARTESIAN_POINT('Ctrl Pts',(-0.550480814704906,2.64610305934508,
8.82725662040549));
#376358=CARTESIAN_POINT('Ctrl Pts',(-0.561710151375514,2.65965043198544,
8.81169306718667));
#376359=CARTESIAN_POINT('Ctrl Pts',(-0.572927672898306,2.67318409147408,
8.79610912703474));
#376360=CARTESIAN_POINT('',(-0.643661112117194,2.6570396455512,8.79610912703474));
#376361=CARTESIAN_POINT('Origin',(0.,1.84795814293585E-15,8.79610912703474));
#376362=CARTESIAN_POINT('',(-0.660897934588195,2.58760342300925,8.85933012996512));
#376363=CARTESIAN_POINT('Ctrl Pts',(-0.643661112117194,2.6570396455512,
8.79610912703474));
#376364=CARTESIAN_POINT('Ctrl Pts',(-0.645163285982008,2.65098763854848,
8.80163734024559));
#376365=CARTESIAN_POINT('Ctrl Pts',(-0.6466660505991,2.64493343204505,8.80716298614018));
#376366=CARTESIAN_POINT('Ctrl Pts',(-0.648169417172601,2.63887698357279,
8.8126860086129));
#376367=CARTESIAN_POINT('Ctrl Pts',(-0.652407382263267,2.62180395717242,
8.82825531609049));
#376368=CARTESIAN_POINT('Ctrl Pts',(-0.656650133709119,2.60471310309576,
8.84380379913848));
#376369=CARTESIAN_POINT('Ctrl Pts',(-0.660897934588195,2.58760342300925,
8.85933012996512));
#376370=CARTESIAN_POINT('',(-0.693929685372903,2.57894147790724,8.85933012996512));
#376371=CARTESIAN_POINT('Origin',(-0.679768337288401,2.59225127529679,8.84999761231047));
#376372=CARTESIAN_POINT('',(-0.743022024337723,2.63098414602442,8.79610912703474));
#376373=CARTESIAN_POINT('Ctrl Pts',(-0.693929685372903,2.57894147790724,
8.85933012996512));
#376374=CARTESIAN_POINT('Ctrl Pts',(-0.698221023078281,2.58349046353331,
8.8538223528706));
#376375=CARTESIAN_POINT('Ctrl Pts',(-0.702510643399309,2.5880376955083,
8.84831178811348));
#376376=CARTESIAN_POINT('Ctrl Pts',(-0.706798579175954,2.59258320766994,
8.84279849653635));
#376377=CARTESIAN_POINT('Ctrl Pts',(-0.718886197936089,2.60539692992268,
8.82725662040549));
#376378=CARTESIAN_POINT('Ctrl Pts',(-0.730960445875394,2.61819700196228,
8.81169306718667));
#376379=CARTESIAN_POINT('Ctrl Pts',(-0.743022024337723,2.63098414602442,
8.79610912703474));
#376380=CARTESIAN_POINT('',(-0.812575755917853,2.61034096358642,8.79610912703474));
#376381=CARTESIAN_POINT('Origin',(0.,1.84795814293585E-15,8.79610912703474));
#376382=CARTESIAN_POINT('',(-0.825328369435551,2.53994303820322,8.85933012996512));
#376383=CARTESIAN_POINT('Ctrl Pts',(-0.812575755917853,2.61034096358642,
8.79610912703474));
#376384=CARTESIAN_POINT('Ctrl Pts',(-0.813687089985364,2.6042051464712,
8.80163734024559));
#376385=CARTESIAN_POINT('Ctrl Pts',(-0.814798872668896,2.59806709652475,
8.80716298614018));
#376386=CARTESIAN_POINT('Ctrl Pts',(-0.815911112428618,2.59192677064835,
8.8126860086129));
#376387=CARTESIAN_POINT('Ctrl Pts',(-0.819046497608276,2.57461729525617,
8.82825531609049));
#376388=CARTESIAN_POINT('Ctrl Pts',(-0.822185517085898,2.55728972215373,
8.84380379913848));
#376389=CARTESIAN_POINT('Ctrl Pts',(-0.825328369435551,2.53994303820322,
8.85933012996512));
#376390=CARTESIAN_POINT('',(-0.857737280217481,2.52918253845729,8.85933012996512));
#376391=CARTESIAN_POINT('Origin',(-0.844457789788063,2.54337231012762,8.84999761231047));
#376392=CARTESIAN_POINT('',(-0.910063138901412,2.57797292237441,8.79610912703474));
#376393=CARTESIAN_POINT('Ctrl Pts',(-0.857737280217481,2.52918253845729,
8.85933012996512));
#376394=CARTESIAN_POINT('Ctrl Pts',(-0.86231125541905,2.53344723075372,
8.8538223528706));
#376395=CARTESIAN_POINT('Ctrl Pts',(-0.866883404408009,2.53771028303531,
8.84831178811348));
#376396=CARTESIAN_POINT('Ctrl Pts',(-0.871453762124842,2.54197172696625,
8.84279849653635));
#376397=CARTESIAN_POINT('Ctrl Pts',(-0.884337523579347,2.55398466565935,
8.82725662040549));
#376398=CARTESIAN_POINT('Ctrl Pts',(-0.897207067112648,2.56598483885656,
8.81169306718667));
#376399=CARTESIAN_POINT('Ctrl Pts',(-0.910063138901412,2.57797292237441,
8.79610912703474));
#376400=CARTESIAN_POINT('',(-0.978151351640492,2.55291583068589,8.79610912703474));
#376401=CARTESIAN_POINT('Origin',(0.,1.84795814293585E-15,8.79610912703474));
#376402=CARTESIAN_POINT('',(-0.986367352980517,2.48184548263713,8.85933012996512));
#376403=CARTESIAN_POINT('Ctrl Pts',(-0.978151351640492,2.55291583068589,
8.79610912703474));
#376404=CARTESIAN_POINT('Ctrl Pts',(-0.978867279200638,2.54672141684682,
8.80163734024559));
#376405=CARTESIAN_POINT('Ctrl Pts',(-0.979583511397086,2.54052474602118,
8.80716298614018));
#376406=CARTESIAN_POINT('Ctrl Pts',(-0.98030005391128,2.53432577465677,
8.8126860086129));
#376407=CARTESIAN_POINT('Ctrl Pts',(-0.982319975209689,2.51685097862003,
8.82825531609049));
#376408=CARTESIAN_POINT('Ctrl Pts',(-0.984342363814731,2.49935788920646,
8.84380379913848));
#376409=CARTESIAN_POINT('Ctrl Pts',(-0.986367352980517,2.48184548263713,
8.85933012996512));
#376410=CARTESIAN_POINT('',(-1.01802024859358,2.46903064544886,8.85933012996512));
#376411=CARTESIAN_POINT('Origin',(-1.00567718409386,2.48404208258451,8.84999761231045));
#376412=CARTESIAN_POINT('',(-1.07336460881942,2.51436825501291,8.79610912703474));
#376413=CARTESIAN_POINT('Ctrl Pts',(-1.01802024859358,2.46903064544886,
8.85933012996512));
#376414=CARTESIAN_POINT('Ctrl Pts',(-1.02285806584612,2.47299351988022,
8.8538223528706));
#376415=CARTESIAN_POINT('Ctrl Pts',(-1.02769395556209,2.47695487467219,
8.84831178811348));
#376416=CARTESIAN_POINT('Ctrl Pts',(-1.03252795463892,2.48091473918522,
8.84279849653635));
#376417=CARTESIAN_POINT('Ctrl Pts',(-1.04615491664841,2.49207753057683,
8.82725662040549));
#376418=CARTESIAN_POINT('Ctrl Pts',(-1.05976687206082,2.50322849364597,
8.81169306718667));
#376419=CARTESIAN_POINT('Ctrl Pts',(-1.07336460881942,2.51436825501291,
8.79610912703474));
#376420=CARTESIAN_POINT('',(-1.13970751364643,2.48500021903835,8.79610912703474));
#376421=CARTESIAN_POINT('Origin',(0.,1.84795814293585E-15,8.79610912703474));
#376422=CARTESIAN_POINT('',(-1.14335314149695,2.41354949162871,8.85933012996512));
#376423=CARTESIAN_POINT('Ctrl Pts',(-1.13970751364643,2.48500021903835,
8.79610912703474));
#376424=CARTESIAN_POINT('Ctrl Pts',(-1.1400250927993,2.47877266265059,8.80163734024559));
#376425=CARTESIAN_POINT('Ctrl Pts',(-1.14034283135694,2.47254283439536,
8.80716298614018));
#376426=CARTESIAN_POINT('Ctrl Pts',(-1.14066073219872,2.46631069044595,
8.8126860086129));
#376427=CARTESIAN_POINT('Ctrl Pts',(-1.14155688932599,2.4487423814499,8.82825531609049));
#376428=CARTESIAN_POINT('Ctrl Pts',(-1.14245433662987,2.43115565858184,
8.84380379913848));
#376429=CARTESIAN_POINT('Ctrl Pts',(-1.14335314149695,2.41354949162871,
8.85933012996512));
#376430=CARTESIAN_POINT('',(-1.17411995340354,2.39873297591287,8.85933012996512));
#376431=CARTESIAN_POINT('Origin',(-1.16276403513314,2.41450439329868,8.84999761231045));
#376432=CARTESIAN_POINT('',(-1.23225539332381,2.44043150916127,8.79610912703474));
#376433=CARTESIAN_POINT('Ctrl Pts',(-1.17411995340354,2.39873297591287,
8.85933012996512));
#376434=CARTESIAN_POINT('Ctrl Pts',(-1.17920173307826,2.4023777481781,8.8538223528706));
#376435=CARTESIAN_POINT('Ctrl Pts',(-1.1842814918131,2.40602112742389,8.84831178811348));
#376436=CARTESIAN_POINT('Ctrl Pts',(-1.18935926831082,2.40966314058634,
8.84279849653635));
#376437=CARTESIAN_POINT('Ctrl Pts',(-1.20367343476545,2.41992991437221,
8.82725662040549));
#376438=CARTESIAN_POINT('Ctrl Pts',(-1.21797186761242,2.43018584561415,
8.81169306718667));
#376439=CARTESIAN_POINT('Ctrl Pts',(-1.23225539332381,2.44043150916127,
8.79610912703474));
#376440=CARTESIAN_POINT('',(-1.29658037301231,2.4068732084599,8.79610912703474));
#376441=CARTESIAN_POINT('Origin',(0.,1.84795814293585E-15,8.79610912703474));
#376442=CARTESIAN_POINT('',(-1.2956406467065,2.33533570805444,8.85933012996512));
#376443=CARTESIAN_POINT('Ctrl Pts',(-1.29658037301231,2.4068732084599,8.79610912703474));
#376444=CARTESIAN_POINT('Ctrl Pts',(-1.29649829875704,2.40063809988846,
8.80163734024559));
#376445=CARTESIAN_POINT('Ctrl Pts',(-1.29641623801998,2.39440071390424,
8.80716298614018));
#376446=CARTESIAN_POINT('Ctrl Pts',(-1.29633419086659,2.38816100658611,
8.8126860086129));
#376447=CARTESIAN_POINT('Ctrl Pts',(-1.29610290132087,2.3705713765808,8.82825531609049));
#376448=CARTESIAN_POINT('Ctrl Pts',(-1.29587171952012,2.35296328787487,
8.84380379913848));
#376449=CARTESIAN_POINT('Ctrl Pts',(-1.2956406467065,2.33533570805444,8.85933012996512));
#376450=CARTESIAN_POINT('',(-1.32539494747703,2.31857839805224,8.85933012996512));
#376451=CARTESIAN_POINT('Origin',(-1.31507283933995,2.33504498755122,8.84999761231046));
#376452=CARTESIAN_POINT('',(-1.38608257609908,2.35646650676756,8.79610912703474));
#376453=CARTESIAN_POINT('Ctrl Pts',(-1.32539494747703,2.31857839805224,
8.85933012996512));
#376454=CARTESIAN_POINT('Ctrl Pts',(-1.3306998074512,2.3218900910003,8.8538223528706));
#376455=CARTESIAN_POINT('Ctrl Pts',(-1.33600256138667,2.32520052327309,
8.84831178811348));
#376456=CARTESIAN_POINT('Ctrl Pts',(-1.34130324963248,2.32850971927167,
8.84279849653635));
#376457=CARTESIAN_POINT('Ctrl Pts',(-1.35624580055189,2.3378382870761,8.82725662040549));
#376458=CARTESIAN_POINT('Ctrl Pts',(-1.37117195550585,2.34715704266947,
8.81169306718667));
#376459=CARTESIAN_POINT('Ctrl Pts',(-1.38608257609908,2.35646650676756,
8.79610912703474));
#376460=CARTESIAN_POINT('',(-1.44812530550985,2.3188558395952,8.79610912703474));
#376461=CARTESIAN_POINT('Origin',(0.,1.84795814293585E-15,8.79610912703474));
#376462=CARTESIAN_POINT('',(-1.44260408658468,2.24752552912783,8.85933012996512));
#376463=CARTESIAN_POINT('Ctrl Pts',(-1.44812530550985,2.3188558395952,8.79610912703474));
#376464=CARTESIAN_POINT('Ctrl Pts',(-1.44764391510717,2.31263880023862,
8.80163734024559));
#376465=CARTESIAN_POINT('Ctrl Pts',(-1.44716239228058,2.30641948728235,
8.80716298614018));
#376466=CARTESIAN_POINT('Ctrl Pts',(-1.44668073428138,2.30019785689127,
8.8126860086129));
#376467=CARTESIAN_POINT('Ctrl Pts',(-1.44532294848102,2.28265918543936,
8.82825531609049));
#376468=CARTESIAN_POINT('Ctrl Pts',(-1.44396408755124,2.26510208630897,
8.84380379913848));
#376469=CARTESIAN_POINT('Ctrl Pts',(-1.44260408658468,2.24752552912783,
8.85933012996512));
#376470=CARTESIAN_POINT('',(-1.47122360941501,2.22889628422051,8.85933012996512));
#376471=CARTESIAN_POINT('Origin',(-1.46197772716767,2.24599038108432,8.84999761231047));
#376472=CARTESIAN_POINT('',(-1.53421404825537,2.26281827803707,8.79610912703474));
#376473=CARTESIAN_POINT('Ctrl Pts',(-1.47122360941501,2.22889628422051,
8.85933012996512));
#376474=CARTESIAN_POINT('Ctrl Pts',(-1.47672975088111,2.23186128939472,
8.8538223528706));
#376475=CARTESIAN_POINT('Ctrl Pts',(-1.48223370986385,2.23482517141821,
8.84831178811348));
#376476=CARTESIAN_POINT('Ctrl Pts',(-1.48773552819275,2.23778795205675,
8.84279849653635));
#376477=CARTESIAN_POINT('Ctrl Pts',(-1.50324506143004,2.24613998079366,
8.82725662040549));
#376478=CARTESIAN_POINT('Ctrl Pts',(-1.51873760371865,2.25448326797286,
8.81169306718667));
#376479=CARTESIAN_POINT('Ctrl Pts',(-1.53421404825537,2.26281827803707,
8.79610912703474));
#376480=CARTESIAN_POINT('',(-1.59371958050516,2.22130979469259,8.79610912703474));
#376481=CARTESIAN_POINT('Origin',(0.,1.84795814293585E-15,8.79610912703474));
#376482=CARTESIAN_POINT('',(-1.58363955683347,2.15047978570932,8.85933012996512));
#376483=CARTESIAN_POINT('Ctrl Pts',(-1.59371958050516,2.22130979469259,
8.79610912703474));
#376484=CARTESIAN_POINT('Ctrl Pts',(-1.59284085209148,2.21513637169914,
8.80163734024559));
#376485=CARTESIAN_POINT('Ctrl Pts',(-1.59196184585595,2.20896068826178,
8.80716298614018));
#376486=CARTESIAN_POINT('Ctrl Pts',(-1.59108255624697,2.20278270081157,
8.8126860086129));
#376487=CARTESIAN_POINT('Ctrl Pts',(-1.58860385362506,2.1853670580761,8.82825531609049));
#376488=CARTESIAN_POINT('Ctrl Pts',(-1.58612289741729,2.16793309440755,
8.84380379913848));
#376489=CARTESIAN_POINT('Ctrl Pts',(-1.58363955683347,2.15047978570932,
8.85933012996512));
#376490=CARTESIAN_POINT('',(-1.61100669796544,2.13005515746016,8.85933012996512));
#376491=CARTESIAN_POINT('Origin',(-1.60287503492123,2.14770651837814,8.84999761231046));
#376492=CARTESIAN_POINT('',(-1.6760411057995,2.15987164362912,8.79610912703474));
#376493=CARTESIAN_POINT('Ctrl Pts',(-1.61100669796544,2.13005515746016,
8.85933012996512));
#376494=CARTESIAN_POINT('Ctrl Pts',(-1.61669149500712,2.13266129101827,
8.8538223528706));
#376495=CARTESIAN_POINT('Ctrl Pts',(-1.62237404208907,2.13526644356548,
8.84831178811348));
#376496=CARTESIAN_POINT('Ctrl Pts',(-1.62805438234941,2.13787063414281,
8.84279849653635));
#376497=CARTESIAN_POINT('Ctrl Pts',(-1.64406716590573,2.14521180353462,
8.82725662040549));
#376498=CARTESIAN_POINT('Ctrl Pts',(-1.66006243334957,2.152545337943,8.81169306718667));
#376499=CARTESIAN_POINT('Ctrl Pts',(-1.6760411057995,2.15987164362912,8.79610912703474));
#376500=CARTESIAN_POINT('',(-1.73276491989239,2.11463591137413,8.79610912703474));
#376501=CARTESIAN_POINT('Origin',(0.,1.84795814293585E-15,8.79610912703474));
#376502=CARTESIAN_POINT('',(-1.71816751245362,2.04459725957487,8.85933012996512));
#376503=CARTESIAN_POINT('Ctrl Pts',(-1.73276491989239,2.11463591137413,
8.79610912703474));
#376504=CARTESIAN_POINT('Ctrl Pts',(-1.73149246435126,2.10853147266309,
8.80163734024559));
#376505=CARTESIAN_POINT('Ctrl Pts',(-1.73021958673194,2.10242479595256,
8.80716298614018));
#376506=CARTESIAN_POINT('Ctrl Pts',(-1.7289462787028,2.09631583811883,8.8126860086129));
#376507=CARTESIAN_POINT('Ctrl Pts',(-1.7253568447801,2.07909478871143,8.82825531609049));
#376508=CARTESIAN_POINT('Ctrl Pts',(-1.72176398807556,2.06185560040102,
8.84380379913848));
#376509=CARTESIAN_POINT('Ctrl Pts',(-1.71816751245362,2.04459725957487,
8.85933012996512));
#376510=CARTESIAN_POINT('',(-1.74416981443406,2.02246117716241,8.85933012996512));
#376511=CARTESIAN_POINT('Origin',(-1.73718578534068,2.04059726890635,8.84999761231045));
#376512=CARTESIAN_POINT('',(-1.81098095093021,2.04804963334648,8.79610912703474));
#376513=CARTESIAN_POINT('Ctrl Pts',(-1.74416981443406,2.02246117716241,
8.85933012996512));
#376514=CARTESIAN_POINT('Ctrl Pts',(-1.7500099070009,2.02469772994261,8.8538223528706));
#376515=CARTESIAN_POINT('Ctrl Pts',(-1.7558476913772,2.02693344788292,8.84831178811348));
#376516=CARTESIAN_POINT('Ctrl Pts',(-1.76168321183243,2.02916834722137,
8.84279849653635));
#376517=CARTESIAN_POINT('Ctrl Pts',(-1.77813344574541,2.03546849082836,
8.82725662040549));
#376518=CARTESIAN_POINT('Ctrl Pts',(-1.79456571035958,2.04176213740001,
8.81169306718667));
#376519=CARTESIAN_POINT('Ctrl Pts',(-1.81098095093021,2.04804963334648,
8.79610912703474));
#376520=CARTESIAN_POINT('',(-1.86468995654687,1.99927253550785,8.79610912703474));
#376521=CARTESIAN_POINT('Origin',(0.,1.84795814293585E-15,8.79610912703474));
#376522=CARTESIAN_POINT('',(-1.84563514921932,1.93031304473609,8.85933012996512));
#376523=CARTESIAN_POINT('Ctrl Pts',(-1.86468995654687,1.99927253550785,
8.79610912703474));
#376524=CARTESIAN_POINT('Ctrl Pts',(-1.86302900267104,1.99326216552728,
8.80163734024559));
#376525=CARTESIAN_POINT('Ctrl Pts',(-1.86136748419512,1.98724958918807,
8.80716298614018));
#376526=CARTESIAN_POINT('Ctrl Pts',(-1.85970539004162,1.98123476398892,
8.8126860086129));
#376527=CARTESIAN_POINT('Ctrl Pts',(-1.85501997457205,1.96427907289552,
8.82825531609049));
#376528=CARTESIAN_POINT('Ctrl Pts',(-1.85032998118961,1.94730549946581,
8.84380379913848));
#376529=CARTESIAN_POINT('Ctrl Pts',(-1.84563514921932,1.93031304473609,
8.85933012996512));
#376530=CARTESIAN_POINT('',(-1.87016576301193,1.90655647007114,8.85933012996512));
#376531=CARTESIAN_POINT('Origin',(-1.86435806674296,1.92510276754984,8.84999761231048));
#376532=CARTESIAN_POINT('',(-1.93847908687936,1.92781174781516,8.79610912703474));
#376533=CARTESIAN_POINT('Ctrl Pts',(-1.87016576301193,1.90655647007114,
8.85933012996512));
#376534=CARTESIAN_POINT('Ctrl Pts',(-1.87613715291086,1.90841425159832,
8.8538223528706));
#376535=CARTESIAN_POINT('Ctrl Pts',(-1.88210618587332,1.91027134788715,
8.84831178811348));
#376536=CARTESIAN_POINT('Ctrl Pts',(-1.88807290711816,1.91212777230594,
8.84279849653635));
#376537=CARTESIAN_POINT('Ctrl Pts',(-1.9048929938481,1.91736100148667,8.82725662040549));
#376538=CARTESIAN_POINT('Ctrl Pts',(-1.92169473193259,1.92258889827783,
8.81169306718667));
#376539=CARTESIAN_POINT('Ctrl Pts',(-1.93847908687936,1.92781174781516,
8.79610912703474));
#376540=CARTESIAN_POINT('',(-1.98895258219516,1.87569371995056,8.79610912703474));
#376541=CARTESIAN_POINT('Origin',(0.,1.84795814293585E-15,8.79610912703474));
#376542=CARTESIAN_POINT('',(-1.96551867526938,1.80809675954563,8.85933012996512));
#376543=CARTESIAN_POINT('Ctrl Pts',(-1.98895258219516,1.87569371995056,
8.79610912703474));
#376544=CARTESIAN_POINT('Ctrl Pts',(-1.98690995520039,1.86980211659992,
8.80163734024559));
#376545=CARTESIAN_POINT('Ctrl Pts',(-1.98486662340367,1.86390834759791,
8.80716298614018));
#376546=CARTESIAN_POINT('Ctrl Pts',(-1.98282257302721,1.85801237124026,
8.8126860086129));
#376547=CARTESIAN_POINT('Ctrl Pts',(-1.97706042938795,1.84139171303254,
8.82825531609049));
#376548=CARTESIAN_POINT('Ctrl Pts',(-1.97129257151642,1.82475350253757,
8.84380379913848));
#376549=CARTESIAN_POINT('Ctrl Pts',(-1.96551867526938,1.80809675954563,
8.85933012996512));
#376550=CARTESIAN_POINT('',(-1.98847679932028,1.78281731348927,8.85933012996512));
#376551=CARTESIAN_POINT('Origin',(-1.98386930094549,1.80169760598827,8.84999761231044));
#376552=CARTESIAN_POINT('',(-2.05801159645805,1.79965207029774,8.79610912703474));
#376553=CARTESIAN_POINT('Ctrl Pts',(-1.98847679932028,1.78281731348927,
8.85933012996512));
#376554=CARTESIAN_POINT('Ctrl Pts',(-1.99455494882936,1.78428868974064,
8.8538223528706));
#376555=CARTESIAN_POINT('Ctrl Pts',(-2.00063070234117,1.78575953317099,
8.84831178811348));
#376556=CARTESIAN_POINT('Ctrl Pts',(-2.00670410583817,1.787229854224,8.84279849653635));
#376557=CARTESIAN_POINT('Ctrl Pts',(-2.0238249280408,1.79137466451723,8.82725662040549));
#376558=CARTESIAN_POINT('Ctrl Pts',(-2.04092709764985,1.79551532897861,
8.81169306718667));
#376559=CARTESIAN_POINT('Ctrl Pts',(-2.05801159645805,1.79965207029774,
8.79610912703474));
#376560=CARTESIAN_POINT('',(-2.10504217505422,1.74440727656295,8.79610912703474));
#376561=CARTESIAN_POINT('Origin',(0.,1.84795814293585E-15,8.79610912703474));
#376562=CARTESIAN_POINT('',(-2.07732546348033,1.67845061693467,8.85933012996512));
#376563=CARTESIAN_POINT('Ctrl Pts',(-2.10504217505422,1.74440727656295,
8.79610912703474));
#376564=CARTESIAN_POINT('Ctrl Pts',(-2.10262626853296,1.73865864970416,
8.80163734024559));
#376565=CARTESIAN_POINT('Ctrl Pts',(-2.10020951990409,1.73290790680038,
8.80716298614018));
#376566=CARTESIAN_POINT('Ctrl Pts',(-2.09779191274612,1.72715500711577,
8.8126860086129));
#376567=CARTESIAN_POINT('Ctrl Pts',(-2.09097671882137,1.71093767964342,
8.82825531609049));
#376568=CARTESIAN_POINT('Ctrl Pts',(-2.08415469782593,1.694703202059,8.84380379913848));
#376569=CARTESIAN_POINT('Ctrl Pts',(-2.07732546348033,1.67845061693467,
8.85933012996512));
#376570=CARTESIAN_POINT('',(-2.0986167579333,1.65175217815315,8.85933012996512));
#376571=CARTESIAN_POINT('Origin',(-2.09522839065177,1.67088888250074,8.84999761231044));
#376572=CARTESIAN_POINT('',(-2.1690872949448,1.66409723639931,8.79610912703474));
#376573=CARTESIAN_POINT('Ctrl Pts',(-2.0986167579333,1.65175217815315,8.85933012996512));
#376574=CARTESIAN_POINT('Ctrl Pts',(-2.10477669063242,1.65283110292808,
8.8538223528706));
#376575=CARTESIAN_POINT('Ctrl Pts',(-2.11093419811916,1.65390964948881,
8.84831178811348));
#376576=CARTESIAN_POINT('Ctrl Pts',(-2.11708932695062,1.65498782531144,
8.84279849653635));
#376577=CARTESIAN_POINT('Ctrl Pts',(-2.13444053149509,1.65802718480262,
8.82725662040549));
#376578=CARTESIAN_POINT('Ctrl Pts',(-2.15177285614539,1.66106360205579,
8.81169306718667));
#376579=CARTESIAN_POINT('Ctrl Pts',(-2.1690872949448,1.66409723639931,8.79610912703474));
#376580=CARTESIAN_POINT('',(-2.21248169808585,1.60595268950176,8.79610912703474));
#376581=CARTESIAN_POINT('Origin',(0.,1.84795814293585E-15,8.79610912703474));
#376582=CARTESIAN_POINT('',(-2.18059607577692,1.54190736071219,8.85933012996512));
#376583=CARTESIAN_POINT('Ctrl Pts',(-2.21248169808585,1.60595268950176,
8.79610912703474));
#376584=CARTESIAN_POINT('Ctrl Pts',(-2.20970243951622,1.60037066147566,
8.80163734024559));
#376585=CARTESIAN_POINT('Ctrl Pts',(-2.2069222049937,1.59478657570622,8.80716298614018));
#376586=CARTESIAN_POINT('Ctrl Pts',(-2.2041409755206,1.58920039259345,8.8126860086129));
#376587=CARTESIAN_POINT('Ctrl Pts',(-2.19630073640404,1.57345303633367,
8.82825531609049));
#376588=CARTESIAN_POINT('Ctrl Pts',(-2.18845258543229,1.55768900261048,
8.84380379913848));
#376589=CARTESIAN_POINT('Ctrl Pts',(-2.18059607577692,1.54190736071219,
8.85933012996512));
#376590=CARTESIAN_POINT('',(-2.20013305013607,1.51389963881728,8.85933012996512));
#376591=CARTESIAN_POINT('Origin',(-2.19797773747577,1.53321411819047,8.84999761231046));
#376592=CARTESIAN_POINT('',(-2.27124974846885,1.52170427000877,8.79610912703474));
#376593=CARTESIAN_POINT('Ctrl Pts',(-2.20013305013607,1.51389963881728,
8.85933012996512));
#376594=CARTESIAN_POINT('Ctrl Pts',(-2.20634945354049,1.51458167858244,
8.8538223528706));
#376595=CARTESIAN_POINT('Ctrl Pts',(-2.21256341248311,1.51526349629438,
8.84831178811348));
#376596=CARTESIAN_POINT('Ctrl Pts',(-2.21877497390438,1.51594509643091,
8.84279849653635));
#376597=CARTESIAN_POINT('Ctrl Pts',(-2.23628526096941,1.51786651573995,
8.82725662040549));
#376598=CARTESIAN_POINT('Ctrl Pts',(-2.25377651842119,1.51978620849509,
8.81169306718667));
#376599=CARTESIAN_POINT('Ctrl Pts',(-2.27124974846885,1.52170427000877,
8.79610912703474));
#376600=CARTESIAN_POINT('',(-2.31082965924421,1.46089889836363,8.79610912703474));
#376601=CARTESIAN_POINT('Origin',(0.,1.84795814293585E-15,8.79610912703474));
#376602=CARTESIAN_POINT('',(-2.27490615106175,1.39902807640646,8.85933012996512));
#376603=CARTESIAN_POINT('Ctrl Pts',(-2.31082965924421,1.46089889836363,
8.79610912703474));
#376604=CARTESIAN_POINT('Ctrl Pts',(-2.30769846919581,1.45550640692072,
8.80163734024559));
#376605=CARTESIAN_POINT('Ctrl Pts',(-2.30456617335966,1.45011192449184,
8.80716298614018));
#376606=CARTESIAN_POINT('Ctrl Pts',(-2.30143275023992,1.44471541277555,
8.8126860086129));
#376607=CARTESIAN_POINT('Ctrl Pts',(-2.2925996831558,1.429502736993,8.82825531609049));
#376608=CARTESIAN_POINT('Ctrl Pts',(-2.28375765194351,1.41427392492699,
8.84380379913848));
#376609=CARTESIAN_POINT('Ctrl Pts',(-2.27490615106175,1.39902807640646,
8.85933012996512));
#376610=CARTESIAN_POINT('',(-2.29260852370878,1.36982616113504,8.85933012996512));
#376611=CARTESIAN_POINT('Origin',(-2.29169512231175,1.38923904819517,8.84999761231045));
#376612=CARTESIAN_POINT('',(-2.36407914959491,1.37305829436823,8.79610912703474));
#376613=CARTESIAN_POINT('Ctrl Pts',(-2.29260852370878,1.36982616113504,
8.85933012996512));
#376614=CARTESIAN_POINT('Ctrl Pts',(-2.29885585328349,1.37010851324275,
8.8538223528706));
#376615=CARTESIAN_POINT('Ctrl Pts',(-2.30510072919181,1.37039080037067,
8.84831178811348));
#376616=CARTESIAN_POINT('Ctrl Pts',(-2.31134319856464,1.37067302397993,
8.84279849653635));
#376617=CARTESIAN_POINT('Ctrl Pts',(-2.32894061462472,1.37146860758275,
8.82725662040549));
#376618=CARTESIAN_POINT('Ctrl Pts',(-2.34651892954926,1.37226368741056,
8.81169306718667));
#376619=CARTESIAN_POINT('Ctrl Pts',(-2.36407914959491,1.37305829436823,
8.79610912703474));
#376620=CARTESIAN_POINT('',(-2.39968192566133,1.30984196029029,8.79610912703474));
#376621=CARTESIAN_POINT('Origin',(0.,1.84795814293585E-15,8.79610912703474));
#376622=CARTESIAN_POINT('',(-2.35986814900603,1.25039988564418,8.85933012996512));
#376623=CARTESIAN_POINT('Ctrl Pts',(-2.39968192566133,1.30984196029029,
8.79610912703474));
#376624=CARTESIAN_POINT('Ctrl Pts',(-2.39621167086571,1.3046611643346,8.80163734024559));
#376625=CARTESIAN_POINT('Ctrl Pts',(-2.39274018499139,1.29947845233169,
8.80716298614018));
#376626=CARTESIAN_POINT('Ctrl Pts',(-2.38926744413272,1.29429378743607,
8.8126860086129));
#376627=CARTESIAN_POINT('Ctrl Pts',(-2.37947784604839,1.27967830427866,
8.82825531609049));
#376628=CARTESIAN_POINT('Ctrl Pts',(-2.36967826839841,1.26504729232517,
8.84380379913848));
#376629=CARTESIAN_POINT('Ctrl Pts',(-2.35986814900603,1.25039988564418,
8.85933012996512));
#376630=CARTESIAN_POINT('',(-2.37566317709459,1.22012377392992,8.85933012996512));
#376631=CARTESIAN_POINT('Origin',(-2.3759954403231,1.23955529695999,8.84999761231045));
#376632=CARTESIAN_POINT('',(-2.44719404240189,1.21877012767605,8.79610912703474));
#376633=CARTESIAN_POINT('Ctrl Pts',(-2.37566317709459,1.22012377392992,
8.85933012996512));
#376634=CARTESIAN_POINT('Ctrl Pts',(-2.38191576122232,1.2200052781348,8.8538223528706));
#376635=CARTESIAN_POINT('Ctrl Pts',(-2.3881658925617,1.21988687470034,8.84831178811348));
#376636=CARTESIAN_POINT('Ctrl Pts',(-2.39441361824043,1.21976856206498,
8.84279849653635));
#376637=CARTESIAN_POINT('Ctrl Pts',(-2.41202585173835,1.2194350407379,8.82725662040549));
#376638=CARTESIAN_POINT('Ctrl Pts',(-2.42961899106907,1.21910224048483,
8.81169306718667));
#376639=CARTESIAN_POINT('Ctrl Pts',(-2.44719404240189,1.21877012767605,
8.79610912703474));
#376640=CARTESIAN_POINT('',(-2.47867338431574,1.1534026006419,8.79610912703474));
#376641=CARTESIAN_POINT('Origin',(0.,1.84795814293585E-15,8.79610912703474));
#376642=CARTESIAN_POINT('',(-2.43513294253591,1.09663353354187,8.85933012996512));
#376643=CARTESIAN_POINT('Ctrl Pts',(-2.47867338431574,1.1534026006419,8.79610912703474));
#376644=CARTESIAN_POINT('Ctrl Pts',(-2.47487832479423,1.14845478917528,
8.80163734024559));
#376645=CARTESIAN_POINT('Ctrl Pts',(-2.47108191396184,1.14350514447366,
8.80716298614018));
#376646=CARTESIAN_POINT('Ctrl Pts',(-2.46728412560132,1.13855363129887,
8.8126860086129));
#376647=CARTESIAN_POINT('Ctrl Pts',(-2.45657822407516,1.12459539892189,
8.82825531609049));
#376648=CARTESIAN_POINT('Ctrl Pts',(-2.44586136855407,1.11062230904738,
8.84380379913848));
#376649=CARTESIAN_POINT('Ctrl Pts',(-2.43513294253591,1.09663353354187,
8.85933012996512));
#376650=CARTESIAN_POINT('',(-2.44895572090756,1.06540763642198,8.85933012996512));
#376651=CARTESIAN_POINT('Origin',(-2.4505322834207,1.08477794712582,8.84999761231048));
#376652=CARTESIAN_POINT('',(-2.52025288996716,1.05947377310387,8.79610912703474));
#376653=CARTESIAN_POINT('Ctrl Pts',(-2.44895572090756,1.06540763642198,
8.85933012996512));
#376654=CARTESIAN_POINT('Ctrl Pts',(-2.45518786637895,1.06488877964867,
8.8538223528706));
#376655=CARTESIAN_POINT('Ctrl Pts',(-2.46141757001908,1.06437017219694,
8.84831178811348));
#376656=CARTESIAN_POINT('Ctrl Pts',(-2.46764487875876,1.06385180948897,
8.84279849653635));
#376657=CARTESIAN_POINT('Ctrl Pts',(-2.48519955724926,1.06239055374266,
8.82725662040549));
#376658=CARTESIAN_POINT('Ctrl Pts',(-2.50273522700294,1.06093124095634,
8.81169306718667));
#376659=CARTESIAN_POINT('Ctrl Pts',(-2.52025288996716,1.05947377310387,
8.79610912703474));
#376660=CARTESIAN_POINT('',(-2.54747944236023,0.992223662303395,8.79610912703474));
#376661=CARTESIAN_POINT('Origin',(0.,1.84795814293585E-15,8.79610912703474));
#376662=CARTESIAN_POINT('',(-2.50039125247054,0.93836087902307,8.85933012996512));
#376663=CARTESIAN_POINT('Ctrl Pts',(-2.54747944236023,0.992223662303395,
8.79610912703474));
#376664=CARTESIAN_POINT('Ctrl Pts',(-2.54337517282644,0.987529166944465,
8.80163734024559));
#376665=CARTESIAN_POINT('Ctrl Pts',(-2.5392694373024,0.982832928695902,
8.80716298614018));
#376666=CARTESIAN_POINT('Ctrl Pts',(-2.53516220736704,0.978134914071679,
8.8126860086129));
#376667=CARTESIAN_POINT('Ctrl Pts',(-2.52358399524484,0.964891289846006,
8.82825531609049));
#376668=CARTESIAN_POINT('Ctrl Pts',(-2.51199389971072,0.951633540473991,
8.84380379913848));
#376669=CARTESIAN_POINT('Ctrl Pts',(-2.50039125247054,0.93836087902307,
8.85933012996512));
#376670=CARTESIAN_POINT('',(-2.51218498036397,0.90631351040677,8.85933012996512));
#376671=CARTESIAN_POINT('Origin',(-2.51499936372825,0.925543012022779,8.84999761231046));
#376672=CARTESIAN_POINT('',(-2.58295547781501,0.895823813541599,8.79610912703474));
#376673=CARTESIAN_POINT('Ctrl Pts',(-2.51218498036397,0.90631351040677,
8.85933012996512));
#376674=CARTESIAN_POINT('Ctrl Pts',(-2.51837107795648,0.905396424749042,
8.8538223528706));
#376675=CARTESIAN_POINT('Ctrl Pts',(-2.52455475470884,0.904479744349307,
8.84831178811348));
#376676=CARTESIAN_POINT('Ctrl Pts',(-2.53073605716211,0.903563461632275,
8.84279849653635));
#376677=CARTESIAN_POINT('Ctrl Pts',(-2.5481610447058,0.900980476080039,
8.82725662040549));
#376678=CARTESIAN_POINT('Ctrl Pts',(-2.56556718705404,0.898400647389714,
8.81169306718667));
#376679=CARTESIAN_POINT('Ctrl Pts',(-2.58295547781501,0.895823813541599,
8.79610912703474));
#376680=CARTESIAN_POINT('',(-2.60581736094344,0.826967464105174,8.79610912703474));
#376681=CARTESIAN_POINT('Origin',(0.,1.84795814293585E-15,8.79610912703474));
#376682=CARTESIAN_POINT('',(-2.55537491841652,0.77623229837459,8.85933012996512));
#376683=CARTESIAN_POINT('Ctrl Pts',(-2.60581736094344,0.826967464105174,
8.79610912703474));
#376684=CARTESIAN_POINT('Ctrl Pts',(-2.60142074672124,0.822545575542333,
8.80163734024559));
#376685=CARTESIAN_POINT('Ctrl Pts',(-2.59702255785351,0.818122041597128,
8.80716298614018));
#376686=CARTESIAN_POINT('Ctrl Pts',(-2.59262276383209,0.813696830673282,
8.8126860086129));
#376687=CARTESIAN_POINT('Ctrl Pts',(-2.58021981847098,0.801222235491608,
8.82825531609049));
#376688=CARTESIAN_POINT('Ctrl Pts',(-2.56780410911246,0.788734305558035,
8.84380379913848));
#376689=CARTESIAN_POINT('Ctrl Pts',(-2.55537491841652,0.77623229837459,
8.85933012996512));
#376690=CARTESIAN_POINT('',(-2.56509113287407,0.743495147773657,8.85933012996512));
#376691=CARTESIAN_POINT('Origin',(-2.56913177218455,0.762504822154984,8.84999761231045));
#376692=CARTESIAN_POINT('',(-2.6350441475623,0.72849272177588,8.79610912703474));
#376693=CARTESIAN_POINT('Ctrl Pts',(-2.56509113287407,0.743495147773657,
8.85933012996512));
#376694=CARTESIAN_POINT('Ctrl Pts',(-2.57120576258579,0.742183601733196,
8.8538223528706));
#376695=CARTESIAN_POINT('Ctrl Pts',(-2.5773180023962,0.740872615221843,
8.84831178811348));
#376696=CARTESIAN_POINT('Ctrl Pts',(-2.58342789826539,0.739562177697975,
8.84279849653635));
#376697=CARTESIAN_POINT('Ctrl Pts',(-2.60065159185081,0.735868076381495,
8.82725662040549));
#376698=CARTESIAN_POINT('Ctrl Pts',(-2.61785668122109,0.732178332856633,
8.81169306718667));
#376699=CARTESIAN_POINT('Ctrl Pts',(-2.6350441475623,0.72849272177588,8.79610912703474));
#376700=CARTESIAN_POINT('',(-2.65344741704446,0.65831307921298,8.79610912703474));
#376701=CARTESIAN_POINT('Origin',(0.,1.84795814293585E-15,8.79610912703474));
#376702=CARTESIAN_POINT('',(-2.59985800069653,0.610914012710784,8.85933012996512));
#376703=CARTESIAN_POINT('Ctrl Pts',(-2.65344741704446,0.65831307921298,
8.79610912703474));
#376704=CARTESIAN_POINT('Ctrl Pts',(-2.64877652476476,0.654181967934824,
8.80163734024559));
#376705=CARTESIAN_POINT('Ctrl Pts',(-2.6441039556548,0.650049315542805,
8.80716298614018));
#376706=CARTESIAN_POINT('Ctrl Pts',(-2.63942967724473,0.645915092460226,
8.8126860086129));
#376707=CARTESIAN_POINT('Ctrl Pts',(-2.62625296500761,0.634260787109944,
8.82825531609049));
#376708=CARTESIAN_POINT('Ctrl Pts',(-2.6130626606376,0.622593992197563,
8.84380379913848));
#376709=CARTESIAN_POINT('Ctrl Pts',(-2.59985800069653,0.610914012710784,
8.85933012996512));
#376710=CARTESIAN_POINT('',(-2.60745677570887,0.577621604099134,8.85933012996512));
#376711=CARTESIAN_POINT('Origin',(-2.61270706711189,0.596333336416169,8.84999761231047));
#376712=CARTESIAN_POINT('',(-2.67630485569206,0.558168097155184,8.79610912703474));
#376713=CARTESIAN_POINT('Ctrl Pts',(-2.60745677570887,0.577621604099134,
8.85933012996512));
#376714=CARTESIAN_POINT('Ctrl Pts',(-2.61347481121473,0.575920987099945,
8.8538223528706));
#376715=CARTESIAN_POINT('Ctrl Pts',(-2.61949049757874,0.574221081601754,
8.84831178811348));
#376716=CARTESIAN_POINT('Ctrl Pts',(-2.62550387999116,0.572521874139925,
8.84279849653635));
#376717=CARTESIAN_POINT('Ctrl Pts',(-2.64245550376689,0.567731836913893,
8.82725662040549));
#376718=CARTESIAN_POINT('Ctrl Pts',(-2.65938884075651,0.562947340502084,
8.81169306718667));
#376719=CARTESIAN_POINT('Ctrl Pts',(-2.67630485569206,0.558168097155184,
8.79610912703474));
#376720=CARTESIAN_POINT('',(-2.69017388854615,0.486953544670587,8.79610912703474));
#376721=CARTESIAN_POINT('Origin',(0.,1.84795814293585E-15,8.79610912703474));
#376722=CARTESIAN_POINT('',(-2.63365770878388,0.443085350328103,8.85933012996512));
#376723=CARTESIAN_POINT('Ctrl Pts',(-2.69017388854615,0.486953544670587,
8.79610912703474));
#376724=CARTESIAN_POINT('Ctrl Pts',(-2.68524791190724,0.483130186299479,
8.80163734024559));
#376725=CARTESIAN_POINT('Ctrl Pts',(-2.68032016314379,0.479305397415775,
8.80716298614018));
#376726=CARTESIAN_POINT('Ctrl Pts',(-2.67539060795767,0.475479150583897,
8.8126860086129));
#376727=CARTESIAN_POINT('Ctrl Pts',(-2.66149427478153,0.464693025105533,
8.82825531609049));
#376728=CARTESIAN_POINT('Ctrl Pts',(-2.64758357718999,0.453895306577159,
8.84380379913848));
#376729=CARTESIAN_POINT('Ctrl Pts',(-2.63365770878388,0.443085350328103,
8.85933012996512));
#376730=CARTESIAN_POINT('',(-2.63910781935455,0.409374489353921,8.85933012996512));
#376731=CARTESIAN_POINT('Origin',(-2.64554618827658,0.427711389084935,8.84999761231045));
#376732=CARTESIAN_POINT('',(-2.7065680531042,0.385549840096597,8.79610912703474));
#376733=CARTESIAN_POINT('Ctrl Pts',(-2.63910781935455,0.409374489353921,
8.85933012996512));
#376734=CARTESIAN_POINT('Ctrl Pts',(-2.6450045312558,0.407291789596035,
8.8538223528706));
#376735=CARTESIAN_POINT('Ctrl Pts',(-2.65089894442778,0.405209950387328,
8.84831178811348));
#376736=CARTESIAN_POINT('Ctrl Pts',(-2.65679110310522,0.403128955395477,
8.84279849653635));
#376737=CARTESIAN_POINT('Ctrl Pts',(-2.67340099921306,0.397262665550314,
8.82725662040549));
#376738=CARTESIAN_POINT('Ctrl Pts',(-2.68999300110814,0.391403076773586,
8.81169306718667));
#376739=CARTESIAN_POINT('Ctrl Pts',(-2.7065680531042,0.385549840096597,
8.79610912703474));
#376740=CARTESIAN_POINT('',(-2.71584585849932,0.313593013561936,8.79610912703474));
#376741=CARTESIAN_POINT('Origin',(0.,1.84795814293585E-15,8.79610912703474));
#376742=CARTESIAN_POINT('',(-2.65663515242803,0.273435955199415,8.85933012996512));
#376743=CARTESIAN_POINT('Ctrl Pts',(-2.71584585849932,0.313593013561936,
8.79610912703474));
#376744=CARTESIAN_POINT('Ctrl Pts',(-2.71068503939582,0.310093119097529,
8.80163734024559));
#376745=CARTESIAN_POINT('Ctrl Pts',(-2.70552236015554,0.306591910600078,
8.80716298614018));
#376746=CARTESIAN_POINT('Ctrl Pts',(-2.70035778479303,0.303089362887862,
8.8126860086129));
#376747=CARTESIAN_POINT('Ctrl Pts',(-2.68579893369164,0.293215739784622,
8.82825531609049));
#376748=CARTESIAN_POINT('Ctrl Pts',(-2.67122500491882,0.283331467781791,
8.84380379913848));
#376749=CARTESIAN_POINT('Ctrl Pts',(-2.65663515242803,0.273435955199415,
8.85933012996512));
#376750=CARTESIAN_POINT('',(-2.65991420288366,0.239445167021401,8.85933012996512));
#376751=CARTESIAN_POINT('Origin',(-2.66751419268574,0.257331883912138,8.84999761231047));
#376752=CARTESIAN_POINT('',(-2.7257093818291,0.211347276044871,8.79610912703474));
#376753=CARTESIAN_POINT('Ctrl Pts',(-2.65991420288366,0.239445167021401,
8.85933012996512));
#376754=CARTESIAN_POINT('Ctrl Pts',(-2.66566536032624,0.236988942764861,
8.8538223528706));
#376755=CARTESIAN_POINT('Ctrl Pts',(-2.67141427889812,0.234533724569499,
8.84831178811348));
#376756=CARTESIAN_POINT('Ctrl Pts',(-2.67716100169672,0.23207949330242,
8.84279849653635));
#376757=CARTESIAN_POINT('Ctrl Pts',(-2.69336091651076,0.225161056681414,
8.82725662040549));
#376758=CARTESIAN_POINT('Ctrl Pts',(-2.70954340321653,0.218250453846929,
8.81169306718667));
#376759=CARTESIAN_POINT('Ctrl Pts',(-2.7257093818291,0.211347276044871,
8.79610912703474));
#376760=CARTESIAN_POINT('',(-2.73035783527281,0.138943861495067,8.79610912703474));
#376761=CARTESIAN_POINT('Origin',(0.,1.84795814293585E-15,8.79610912703474));
#376762=CARTESIAN_POINT('',(-2.66869591238441,0.102662953078985,8.85933012996512));
#376763=CARTESIAN_POINT('Ctrl Pts',(-2.73035783527281,0.138943861495067,
8.79610912703474));
#376764=CARTESIAN_POINT('Ctrl Pts',(-2.72498338061741,0.135781812754442,
8.80163734024559));
#376765=CARTESIAN_POINT('Ctrl Pts',(-2.71960698545669,0.132618571859967,
8.80716298614018));
#376766=CARTESIAN_POINT('Ctrl Pts',(-2.71422861226575,0.129454115987256,
8.8126860086129));
#376767=CARTESIAN_POINT('Ctrl Pts',(-2.69906706868114,0.120533568094357,
8.82825531609049));
#376768=CARTESIAN_POINT('Ctrl Pts',(-2.68388979612647,0.111603359210898,
8.84380379913848));
#376769=CARTESIAN_POINT('Ctrl Pts',(-2.66869591238441,0.102662953078985,
8.85933012996512));
#376770=CARTESIAN_POINT('',(-2.66979042840332,0.0685319131367625,8.85933012996512));
#376771=CARTESIAN_POINT('Origin',(-2.67852080909719,0.0858949468308337,
8.84999761231045));
#376772=CARTESIAN_POINT('Ctrl Pts',(-2.66979042840332,0.0685319131367625,
8.85933012996512));
#376773=CARTESIAN_POINT('Ctrl Pts',(-2.67537239864768,0.0657122575338965,
8.8538223528706));
#376774=CARTESIAN_POINT('Ctrl Pts',(-2.6809521990799,0.0628937493700869,
8.84831178811348));
#376775=CARTESIAN_POINT('Ctrl Pts',(-2.68652987148302,0.0600763667904869,
8.84279849653635));
#376776=CARTESIAN_POINT('Ctrl Pts',(-2.7022532360784,0.0521342127337157,
8.82725662040549));
#376777=CARTESIAN_POINT('Ctrl Pts',(-2.71795971028587,0.0442009929908397,
8.81169306718667));
#376778=CARTESIAN_POINT('Ctrl Pts',(-2.73365018604124,0.0362762407020289,
8.79610912703474));
#376779=CARTESIAN_POINT('Origin',(0.,1.73472347597681E-15,8.945));
#376780=CARTESIAN_POINT('',(-2.50721825406948,1.42767779501581E-15,9.));
#376781=CARTESIAN_POINT('Origin',(0.,1.84795814293585E-15,9.));
#376782=CARTESIAN_POINT('Origin',(-2.50721825406948,1.42767779501581E-15,
8.945));
#376783=CARTESIAN_POINT('Origin',(0.,1.84795814293585E-15,9.));
#376784=CARTESIAN_POINT('',(2.74983646666349,-0.0299901084967912,8.75721825406948));
#376785=CARTESIAN_POINT('',(2.74983646666349,0.0299901084968513,8.75721825406948));
#376786=CARTESIAN_POINT('Origin',(0.,1.84795814293585E-15,8.75721825406948));
#376787=CARTESIAN_POINT('',(2.74983646666349,-0.0299901084967912,7.51860402984325));
#376788=CARTESIAN_POINT('',(2.74983646666349,-0.0299901084967912,9.));
#376789=CARTESIAN_POINT('',(2.74956360331414,-0.0489897063694301,7.49482233047033));
#376790=CARTESIAN_POINT('Origin',(2.74937751092705,-0.0583021276914146,
7.53025004711371));
#376791=CARTESIAN_POINT('',(2.74705311126524,-0.127276093151676,7.49482233047033));
#376792=CARTESIAN_POINT('Origin',(1.8470086919802E-15,-5.92299737674606E-17,
7.49482233047033));
#376793=CARTESIAN_POINT('',(2.74610810557233,-0.146254136727608,7.51860402984325));
#376794=CARTESIAN_POINT('Origin',(2.74746646844579,-0.117918295378179,7.5303083625674));
#376795=CARTESIAN_POINT('',(2.74610810557233,-0.146254136727603,8.75721825406948));
#376796=CARTESIAN_POINT('',(2.74610810557234,-0.146254136727603,9.));
#376797=CARTESIAN_POINT('',(2.74226515987506,-0.206111117932571,8.75721825406948));
#376798=CARTESIAN_POINT('Origin',(0.,1.84795814293585E-15,8.75721825406948));
#376799=CARTESIAN_POINT('',(2.74226515987506,-0.206111117932571,7.51860402984325));
#376800=CARTESIAN_POINT('',(2.74226515987506,-0.206111117932571,9.));
#376801=CARTESIAN_POINT('',(2.74077554873748,-0.225054196678863,7.49482233047033));
#376802=CARTESIAN_POINT('Origin',(2.7399931898145,-0.234335561652256,7.53025004711365));
#376803=CARTESIAN_POINT('',(2.73325438874111,-0.303018887905443,7.49482233047033));
#376804=CARTESIAN_POINT('Origin',(1.83941893708273E-15,-1.77446532635421E-16,
7.49482233047033));
#376805=CARTESIAN_POINT('',(2.73109539723704,-0.321897392332831,7.51860402984325));
#376806=CARTESIAN_POINT('Origin',(2.73426645279687,-0.293706800616635,7.53030836256733));
#376807=CARTESIAN_POINT('',(2.73109539723704,-0.321897392332826,8.75721825406948));
#376808=CARTESIAN_POINT('',(2.73109539723704,-0.321897392332826,9.));
#376809=CARTESIAN_POINT('',(2.72342529733067,-0.381385172574072,8.75721825406948));
#376810=CARTESIAN_POINT('Origin',(0.,1.84795814293585E-15,8.75721825406948));
#376811=CARTESIAN_POINT('',(2.72342529733067,-0.381385172574072,7.51860402984325));
#376812=CARTESIAN_POINT('',(2.72342529733067,-0.381385172574073,9.));
#376813=CARTESIAN_POINT('',(2.72072505953655,-0.40019389102017,7.49482233047033));
#376814=CARTESIAN_POINT('Origin',(2.7193496489583,-0.409406060525646,7.53025004711384));
#376815=CARTESIAN_POINT('',(2.70822413765242,-0.477516513051461,7.49482233047033));
#376816=CARTESIAN_POINT('Origin',(1.82427061521867E-15,-2.94933925638621E-16,
7.49482233047033));
#376817=CARTESIAN_POINT('',(2.70486003209637,-0.496217902506188,7.51860402984325));
#376818=CARTESIAN_POINT('Origin',(2.70983074979512,-0.46828840161129,7.53030836256747));
#376819=CARTESIAN_POINT('',(2.70486003209637,-0.496217902506183,8.75721825406948));
#376820=CARTESIAN_POINT('',(2.70486003209637,-0.496217902506183,9.));
#376821=CARTESIAN_POINT('',(2.69339429606666,-0.555092033734601,8.75721825406948));
#376822=CARTESIAN_POINT('Origin',(0.,1.84795814293585E-15,8.75721825406948));
#376823=CARTESIAN_POINT('',(2.69339429606666,-0.555092033734601,7.51860402984325));
#376824=CARTESIAN_POINT('',(2.69339429606666,-0.555092033734602,9.));
#376825=CARTESIAN_POINT('',(2.68949452747228,-0.573689102821954,7.49482233047033));
#376826=CARTESIAN_POINT('Origin',(2.6875317170959,-0.582794222078666,7.53025004711359));
#376827=CARTESIAN_POINT('',(2.67206521266985,-0.650051920418378,7.49482233047033));
#376828=CARTESIAN_POINT('Origin',(1.80162597409185E-15,-4.11209371878242E-16,
7.49482233047033));
#376829=CARTESIAN_POINT('',(2.66750981689316,-0.668499346879738,7.51860402984325));
#376830=CARTESIAN_POINT('Origin',(2.67425977098555,-0.640945705116414,7.53030836256731));
#376831=CARTESIAN_POINT('',(2.66750981689316,-0.668499346879733,8.75721825406948));
#376832=CARTESIAN_POINT('',(2.66750981689316,-0.668499346879733,9.));
#376833=CARTESIAN_POINT('',(2.65229555990884,-0.72651790266165,8.75721825406948));
#376834=CARTESIAN_POINT('Origin',(0.,1.84795814293585E-15,8.75721825406948));
#376835=CARTESIAN_POINT('',(2.65229555990884,-0.72651790266165,7.51860402984325));
#376836=CARTESIAN_POINT('',(2.65229555990884,-0.72651790266165,9.));
#376837=CARTESIAN_POINT('',(2.64721228549987,-0.744826903044317,7.49482233047033));
#376838=CARTESIAN_POINT('Origin',(2.64467014093421,-0.7537875571643,7.53025004711347));
#376839=CARTESIAN_POINT('',(2.62492619857224,-0.819916125008598,7.49482233047033));
#376840=CARTESIAN_POINT('Origin',(1.77157806538993E-15,-5.25795070604684E-16,
7.49482233047033));
#376841=CARTESIAN_POINT('',(2.61919823167327,-0.838033784044301,7.51860402984325));
#376842=CARTESIAN_POINT('Origin',(2.62769968515011,-0.810969225236613,7.53030836256735));
#376843=CARTESIAN_POINT('',(2.61919823167327,-0.838033784044296,8.75721825406948));
#376844=CARTESIAN_POINT('',(2.61919823167328,-0.838033784044296,9.));
#376845=CARTESIAN_POINT('',(2.60029797237974,-0.894958353689057,8.75721825406948));
#376846=CARTESIAN_POINT('Origin',(0.,1.84795814293585E-15,8.75721825406948));
#376847=CARTESIAN_POINT('',(2.60029797237974,-0.894958353689057,7.51860402984325));
#376848=CARTESIAN_POINT('',(2.60029797237974,-0.894958353689057,9.));
#376849=CARTESIAN_POINT('',(2.59405208042108,-0.912904049757199,7.49482233047033));
#376850=CARTESIAN_POINT('Origin',(2.59094104788344,-0.921683417490723,7.53025004711346));
#376851=CARTESIAN_POINT('',(2.56700079967978,-0.986411118369699,7.49482233047033));
#376852=CARTESIAN_POINT('Origin',(1.73425036241502E-15,-6.38220164603321E-16,
7.49482233047033));
#376853=CARTESIAN_POINT('',(2.56012379910318,-1.00412456063254,7.51860402984325));
#376854=CARTESIAN_POINT('Origin',(2.57034181766862,-0.977660298857871,7.53030836256752));
#376855=CARTESIAN_POINT('',(2.56012379910319,-1.00412456063254,8.75721825406948));
#376856=CARTESIAN_POINT('',(2.56012379910319,-1.00412456063254,9.));
#376857=CARTESIAN_POINT('',(2.53761520271997,-1.05972122887319,8.75721825406948));
#376858=CARTESIAN_POINT('Origin',(0.,1.84795814293585E-15,8.75721825406948));
#376859=CARTESIAN_POINT('',(2.53761520271997,-1.05972122887319,7.51860402984325));
#376860=CARTESIAN_POINT('',(2.53761520271997,-1.05972122887319,9.));
#376861=CARTESIAN_POINT('',(2.53023235892141,-1.07722987791233,7.49482233047033));
#376862=CARTESIAN_POINT('Origin',(2.52656522231176,-1.08579188295431,7.53025004711358));
#376863=CARTESIAN_POINT('',(2.4985270438815,-1.1488527368609,7.49482233047033));
#376864=CARTESIAN_POINT('Origin',(1.68979625270541E-15,-7.48022675047808E-16,
7.49482233047033));
#376865=CARTESIAN_POINT('',(2.49052926869775,-1.1660891740171,7.51860402984325));
#376866=CARTESIAN_POINT('Origin',(2.50242186432163,-1.1403339566039,7.53030836256736));
#376867=CARTESIAN_POINT('',(2.49052926869775,-1.1660891740171,8.75721825406948));
#376868=CARTESIAN_POINT('',(2.49052926869775,-1.1660891740171,9.));
#376869=CARTESIAN_POINT('',(2.46450482787546,-1.2201294822184,8.75721825406948));
#376870=CARTESIAN_POINT('Origin',(0.,1.84795814293585E-15,8.75721825406948));
#376871=CARTESIAN_POINT('',(2.46450482787546,-1.2201294822184,7.51860402984325));
#376872=CARTESIAN_POINT('',(2.46450482787547,-1.2201294822184,9.));
#376873=CARTESIAN_POINT('',(2.4560153699258,-1.23712913743403,7.49482233047033));
#376874=CARTESIAN_POINT('Origin',(2.45180719829513,-1.24543859666903,7.53025004711348));
#376875=CARTESIAN_POINT('',(2.41978630452754,-1.3065734730282,7.49482233047033));
#376876=CARTESIAN_POINT('Origin',(1.63839840773327E-15,-8.5475139987016E-16,
7.49482233047033));
#376877=CARTESIAN_POINT('',(2.41070061931038,-1.32326207686028,7.51860402984325));
#376878=CARTESIAN_POINT('Origin',(2.42421892276641,-1.29832173752123,7.53030836256741));
#376879=CARTESIAN_POINT('',(2.41070061931038,-1.32326207686027,8.75721825406948));
#376880=CARTESIAN_POINT('',(2.41070061931038,-1.32326207686027,9.));
#376881=CARTESIAN_POINT('',(2.38126727405859,-1.37552396180421,8.75721825406948));
#376882=CARTESIAN_POINT('Origin',(0.,1.84795814293585E-15,8.75721825406948));
#376883=CARTESIAN_POINT('',(2.38126727405859,-1.37552396180421,7.51860402984325));
#376884=CARTESIAN_POINT('',(2.38126727405859,-1.37552396180421,9.));
#376885=CARTESIAN_POINT('',(2.37170608696151,-1.39194476796664,7.49482233047033));
#376886=CARTESIAN_POINT('Origin',(2.36697417258961,-1.39996753604449,7.53025004711367));
#376887=CARTESIAN_POINT('',(2.33110214420574,-1.45892521853569,7.49482233047033));
#376888=CARTESIAN_POINT('Origin',(1.5802680322684E-15,-9.57967767846848E-16,
7.49482233047033));
#376889=CARTESIAN_POINT('',(2.3209658839846,-1.47499741199082,7.51860402984325));
#376890=CARTESIAN_POINT('Origin',(2.33605434566413,-1.45097443593007,7.53030836256728));
#376891=CARTESIAN_POINT('',(2.3209658839846,-1.47499741199081,8.75721825406948));
#376892=CARTESIAN_POINT('',(2.3209658839846,-1.47499741199081,9.));
#376893=CARTESIAN_POINT('',(2.28824458223239,-1.52526611838201,8.75721825406948));
#376894=CARTESIAN_POINT('Origin',(0.,1.84795814293585E-15,8.75721825406948));
#376895=CARTESIAN_POINT('',(2.28824458223239,-1.52526611838201,7.51860402984325));
#376896=CARTESIAN_POINT('',(2.28824458223239,-1.52526611838201,9.));
#376897=CARTESIAN_POINT('',(2.27765095495655,-1.54104059887647,7.49482233047033));
#376898=CARTESIAN_POINT('Origin',(2.27241474229462,-1.54874370852212,7.53025004711368));
#376899=CARTESIAN_POINT('',(2.23283898515356,-1.60528192738174,7.49482233047033));
#376900=CARTESIAN_POINT('Origin',(1.51564399649251E-15,-1.05724764078201E-15,
7.49482233047033));
#376901=CARTESIAN_POINT('',(2.22169380199591,-1.62067166636953,7.51860402984325));
#376902=CARTESIAN_POINT('Origin',(2.23829042017357,-1.59766476914842,7.53030836256744));
#376903=CARTESIAN_POINT('',(2.22169380199591,-1.62067166636952,8.75721825406948));
#376904=CARTESIAN_POINT('',(2.22169380199591,-1.62067166636952,9.));
#376905=CARTESIAN_POINT('',(2.18581900259087,-1.66874062931082,8.75721825406948));
#376906=CARTESIAN_POINT('Origin',(0.,1.84795814293585E-15,8.75721825406948));
#376907=CARTESIAN_POINT('',(2.18581900259087,-1.66874062931082,7.51860402984325));
#376908=CARTESIAN_POINT('',(2.18581900259087,-1.66874062931082,9.));
#376909=CARTESIAN_POINT('',(2.17423646662307,-1.68380396341334,7.49482233047033));
#376910=CARTESIAN_POINT('Origin',(2.16851747239208,-1.69115576089697,7.53025004711369));
#376911=CARTESIAN_POINT('',(2.12540061176892,-1.74504218845629,7.49482233047033));
#376912=CARTESIAN_POINT('Origin',(1.44479185443041E-15,-1.15218305638229E-15,
7.49482233047033));
#376913=CARTESIAN_POINT('',(2.11329230362299,-1.75968623323814,7.51860402984325));
#376914=CARTESIAN_POINT('Origin',(2.13132887923455,-1.73778995513257,7.53030836256725));
#376915=CARTESIAN_POINT('',(2.11329230362299,-1.75968623323814,8.75721825406948));
#376916=CARTESIAN_POINT('',(2.113292303623,-1.75968623323814,9.));
#376917=CARTESIAN_POINT('',(2.07441142381099,-1.80535792705005,8.75721825406948));
#376918=CARTESIAN_POINT('Origin',(0.,1.84795814293585E-15,8.75721825406948));
#376919=CARTESIAN_POINT('',(2.07441142381099,-1.80535792705005,7.51860402984325));
#376920=CARTESIAN_POINT('',(2.07441142381099,-1.80535792705005,9.));
#376921=CARTESIAN_POINT('',(2.06188757427597,-1.81964821628972,7.49482233047033));
#376922=CARTESIAN_POINT('Origin',(2.05570929904995,-1.82661849149851,7.5302500471137));
#376923=CARTESIAN_POINT('',(2.00922851137352,-1.8776316968681,7.49482233047033));
#376924=CARTESIAN_POINT('Origin',(1.36800275273158E-15,-1.24238390466141E-15,
7.49482233047033));
#376925=CARTESIAN_POINT('',(1.99620683387471,-1.89146987192287,7.51860402984325));
#376926=CARTESIAN_POINT('Origin',(2.01560925076226,-1.87077418943614,7.53030836256729));
#376927=CARTESIAN_POINT('',(1.99620683387471,-1.89146987192287,8.75721825406948));
#376928=CARTESIAN_POINT('',(1.99620683387471,-1.89146987192287,9.));
#376929=CARTESIAN_POINT('',(1.95447964353083,-1.93455662181897,8.75721825406948));
#376930=CARTESIAN_POINT('Origin',(0.,1.84795814293585E-15,8.75721825406948));
#376931=CARTESIAN_POINT('',(1.95447964353083,-1.93455662181897,7.51860402984325));
#376932=CARTESIAN_POINT('',(1.95447964353083,-1.93455662181897,9.));
#376933=CARTESIAN_POINT('',(1.94106594361268,-1.94801514433206,7.49482233047033));
#376934=CARTESIAN_POINT('Origin',(1.93445377524964,-1.95457525491017,7.53025004711394));
#376935=CARTESIAN_POINT('',(1.88480006004672,-2.00250561388673,7.49482233047033));
#376936=CARTESIAN_POINT('Origin',(1.2855922342861E-15,-1.32747953098576E-15,
7.49482233047033));
#376937=CARTESIAN_POINT('',(1.87091852206101,-2.01548105518485,7.51860402984325));
#376938=CARTESIAN_POINT('Origin',(1.89160705153173,-1.99607101131556,7.53030836256725));
#376939=CARTESIAN_POINT('',(1.87091852206101,-2.01548105518485,8.75721825406948));
#376940=CARTESIAN_POINT('',(1.87091852206102,-2.01548105518485,9.));
#376941=CARTESIAN_POINT('',(1.82651648716082,-2.05580580846774,8.75721825406948));
#376942=CARTESIAN_POINT('Origin',(0.,1.84795814293585E-15,8.75721825406948));
#376943=CARTESIAN_POINT('',(1.82651648716082,-2.05580580846774,7.51860402984325));
#376944=CARTESIAN_POINT('',(1.82651648716082,-2.05580580846774,9.));
#376945=CARTESIAN_POINT('',(1.81226805662974,-2.06837726029839,7.49482233047033));
#376946=CARTESIAN_POINT('Origin',(1.80524916594823,-2.07450024934391,7.53025004711344));
#376947=CARTESIAN_POINT('',(1.75262656098485,-2.11915080580181,7.49482233047033));
#376948=CARTESIAN_POINT('Origin',(1.19789894159128E-15,-1.40712025917382E-15,
7.49482233047033));
#376949=CARTESIAN_POINT('',(1.7379422047294,-2.13121019447175,7.51860402984325));
#376950=CARTESIAN_POINT('Origin',(1.75983183317822,-2.1131655492534,7.53030836256758));
#376951=CARTESIAN_POINT('',(1.73794220472941,-2.13121019447175,8.75721825406948));
#376952=CARTESIAN_POINT('',(1.73794220472941,-2.13121019447175,9.));
#376953=CARTESIAN_POINT('',(1.69104778275851,-2.16860724808056,8.75721825406948));
#376954=CARTESIAN_POINT('Origin',(0.,1.84795814293585E-15,8.75721825406948));
#376955=CARTESIAN_POINT('',(1.69104778275851,-2.16860724808056,7.51860402984325));
#376956=CARTESIAN_POINT('',(1.69104778275851,-2.16860724808056,9.));
#376957=CARTESIAN_POINT('',(1.67602317147183,-2.18023997043663,7.49482233047033));
#376958=CARTESIAN_POINT('Origin',(1.6686264005988,-2.18590067727457,7.53025004711363));
#376959=CARTESIAN_POINT('',(1.61325114344667,-2.22708795249942,7.49482233047033));
#376960=CARTESIAN_POINT('Origin',(1.10528322519694E-15,-1.48097882839059E-15,
7.49482233047033));
#376961=CARTESIAN_POINT('',(1.59782431009112,-2.23818173392641,7.51860402984325));
#376962=CARTESIAN_POINT('Origin',(1.62082508833912,-2.22157663667706,7.53030836256737));
#376963=CARTESIAN_POINT('',(1.59782431009113,-2.23818173392641,8.75721825406948));
#376964=CARTESIAN_POINT('',(1.59782431009113,-2.23818173392641,9.));
#376965=CARTESIAN_POINT('',(1.54863020028824,-2.27249741534621,8.75721825406948));
#376966=CARTESIAN_POINT('Origin',(0.,1.84795814293585E-15,8.75721825406948));
#376967=CARTESIAN_POINT('',(1.54863020028824,-2.27249741534621,7.51860402984325));
#376968=CARTESIAN_POINT('',(1.54863020028824,-2.27249741534621,9.));
#376969=CARTESIAN_POINT('',(1.5328911475965,-2.28314360687634,7.49482233047033));
#376970=CARTESIAN_POINT('Origin',(1.52514689145007,-2.28831877044806,7.53025004711377));
#376971=CARTESIAN_POINT('',(1.46724653091878,-2.32587351709134,7.49482233047033));
#376972=CARTESIAN_POINT('Origin',(1.00812566294775E-15,-1.54875173793254E-15,
7.49482233047033));
#376973=CARTESIAN_POINT('',(1.45114061263044,-2.33595610454789,7.51860402984325));
#376974=CARTESIAN_POINT('Origin',(1.47515802554624,-2.32085878917382,7.53030836256734));
#376975=CARTESIAN_POINT('',(1.45114061263045,-2.33595610454789,8.75721825406948));
#376976=CARTESIAN_POINT('',(1.45114061263045,-2.33595610454789,9.));
#376977=CARTESIAN_POINT('',(1.39984896414485,-2.36704940328304,8.75721825406948));
#376978=CARTESIAN_POINT('Origin',(0.,1.84795814293585E-15,8.75721825406948));
#376979=CARTESIAN_POINT('',(1.39984896414485,-2.36704940328304,7.51860402984325));
#376980=CARTESIAN_POINT('',(1.39984896414485,-2.36704940328304,9.));
#376981=CARTESIAN_POINT('',(1.38346014519158,-2.37666531650262,7.49482233047033));
#376982=CARTESIAN_POINT('Origin',(1.37540022658149,-2.38133367095087,7.53025004711378));
#376983=CARTESIAN_POINT('',(1.31521268767195,-2.41510156850322,7.49482233047033));
#376984=CARTESIAN_POINT('Origin',(9.06825496107236E-16,-1.61016049437712E-15,
7.49482233047033));
#376985=CARTESIAN_POINT('',(1.29849386712378,-2.42413153047477,7.51860402984325));
#376986=CARTESIAN_POINT('Origin',(1.3234292220059,-2.41060403508326,7.53030836256716));
#376987=CARTESIAN_POINT('',(1.29849386712378,-2.42413153047477,8.75721825406948));
#376988=CARTESIAN_POINT('',(1.29849386712378,-2.42413153047477,9.));
#376989=CARTESIAN_POINT('',(1.24531544834112,-2.45187467749128,8.75721825406948));
#376990=CARTESIAN_POINT('Origin',(0.,1.84795814293585E-15,8.75721825406948));
#376991=CARTESIAN_POINT('',(1.24531544834112,-2.45187467749128,7.51860402984325));
#376992=CARTESIAN_POINT('',(1.24531544834112,-2.45187467749128,9.));
#376993=CARTESIAN_POINT('',(1.22834420829879,-2.46042079855028,7.49482233047033));
#376994=CARTESIAN_POINT('Origin',(1.22000174715932,-2.46456316060533,7.53025004711397));
#376995=CARTESIAN_POINT('',(1.15777435337925,-2.49440544953247,7.49482233047033));
#376996=CARTESIAN_POINT('Origin',(8.01798988789759E-16,-1.66495275597196E-15,
7.49482233047033));
#376997=CARTESIAN_POINT('',(1.14051133179104,-2.50234567996835,7.51860402984325));
#376998=CARTESIAN_POINT('Origin',(1.16626216391798,-2.49044359193944,7.53030836256744));
#376999=CARTESIAN_POINT('',(1.14051133179105,-2.50234567996834,8.75721825406948));
#377000=CARTESIAN_POINT('',(1.14051133179105,-2.50234567996834,9.));
#377001=CARTESIAN_POINT('',(1.08566466424083,-2.52662467272424,8.75721825406948));
#377002=CARTESIAN_POINT('Origin',(0.,1.84795814293585E-15,8.75721825406948));
#377003=CARTESIAN_POINT('',(1.08566466424083,-2.52662467272424,7.51860402984325));
#377004=CARTESIAN_POINT('',(1.08566466424083,-2.52662467272424,9.));
#377005=CARTESIAN_POINT('',(1.0681807415751,-2.5340658837781,7.49482233047033));
#377006=CARTESIAN_POINT('Origin',(1.05959001886878,-2.5376652315856,7.53025004711381));
#377007=CARTESIAN_POINT('',(0.995578475926683,-2.5634592835213,7.49482233047033));
#377008=CARTESIAN_POINT('Origin',(6.93477717442E-16,-1.71290336956127E-15,
7.49482233047033));
#377009=CARTESIAN_POINT('',(0.977842190757062,-2.57027715431147,7.51860402984325));
#377010=CARTESIAN_POINT('Origin',(1.00430268443587,-2.56004938187796,7.53030836256745));
#377011=CARTESIAN_POINT('',(0.977842190757066,-2.57027715431146,8.75721825406948));
#377012=CARTESIAN_POINT('',(0.977842190757067,-2.57027715431146,9.));
#377013=CARTESIAN_POINT('',(0.921552651160842,-2.59099222521767,8.75721825406948));
#377014=CARTESIAN_POINT('Origin',(0.,1.84795814293585E-15,8.75721825406948));
#377015=CARTESIAN_POINT('',(0.921552651160842,-2.59099222521767,7.51860402984325));
#377016=CARTESIAN_POINT('',(0.921552651160842,-2.59099222521767,9.));
#377017=CARTESIAN_POINT('',(0.903627891060228,-2.59729794873404,7.49482233047033));
#377018=CARTESIAN_POINT('Origin',(0.894824207909509,-2.60033949180176,7.53025004711349));
#377019=CARTESIAN_POINT('',(0.829291552965625,-2.62197931345384,7.49482233047033));
#377020=CARTESIAN_POINT('Origin',(5.82306797402768E-16,-1.75381529578843E-15,
7.49482233047033));
#377021=CARTESIAN_POINT('',(0.811154886414768,-2.6276468085048,7.51860402984325));
#377022=CARTESIAN_POINT('Origin',(0.838216309801055,-2.61913537977752,7.53030836256733));
#377023=CARTESIAN_POINT('',(0.811154886414773,-2.6276468085048,8.75721825406948));
#377024=CARTESIAN_POINT('',(0.811154886414773,-2.6276468085048,9.));
#377025=CARTESIAN_POINT('',(0.753653780564806,-2.6447128348916,8.75721825406948));
#377026=CARTESIAN_POINT('Origin',(0.,1.84795814293585E-15,8.75721825406948));
#377027=CARTESIAN_POINT('',(0.753653780564806,-2.6447128348916,7.51860402984325));
#377028=CARTESIAN_POINT('',(0.753653780564806,-2.6447128348916,9.));
#377029=CARTESIAN_POINT('',(0.735361839713413,-2.64985715929997,7.49482233047033));
#377030=CARTESIAN_POINT('Origin',(0.726381372340523,-2.65232839927514,7.53025004711344));
#377031=CARTESIAN_POINT('',(0.65959689313095,-2.6697250679746,7.49482233047033));
#377032=CARTESIAN_POINT('Origin',(4.68743053828592E-16,-1.78752041877299E-15,
7.49482233047033));
#377033=CARTESIAN_POINT('',(0.641134372652019,-2.67421889833352,7.51860402984325));
#377034=CARTESIAN_POINT('Origin',(0.668685524552562,-2.66745878859875,7.53030836256735));
#377035=CARTESIAN_POINT('',(0.641134372652024,-2.67421889833351,8.75721825406948));
#377036=CARTESIAN_POINT('',(0.641134372652024,-2.67421889833351,9.));
#377037=CARTESIAN_POINT('',(0.582657984926201,-2.68756575223784,8.75721825406948));
#377038=CARTESIAN_POINT('Origin',(0.,1.84795814293585E-15,8.75721825406948));
#377039=CARTESIAN_POINT('',(0.582657984926201,-2.68756575223784,7.51860402984325));
#377040=CARTESIAN_POINT('',(0.582657984926201,-2.68756575223784,9.));
#377041=CARTESIAN_POINT('',(0.564074028832595,-2.69152753840576,7.49482233047033));
#377042=CARTESIAN_POINT('Origin',(0.554953679904234,-2.69341832043325,7.53025004711345));
#377043=CARTESIAN_POINT('',(0.487191808179311,-2.70650034953683,7.49482233047033));
#377044=CARTESIAN_POINT('Origin',(3.53253144501165E-16,-1.81388023693488E-15,
7.49482233047033));
#377045=CARTESIAN_POINT('',(0.468479300229151,-2.70980204909082,7.51860402984325));
#377046=CARTESIAN_POINT('Origin',(0.496406967050784,-2.70482103708957,7.53030836256699));
#377047=CARTESIAN_POINT('',(0.468479300229156,-2.70980204909082,8.75721825406948));
#377048=CARTESIAN_POINT('',(0.468479300229156,-2.70980204909082,9.));
#377049=CARTESIAN_POINT('',(0.409267922647788,-2.71937488542709,8.75721825406948));
#377050=CARTESIAN_POINT('Origin',(0.,1.84795814293585E-15,8.75721825406948));
#377051=CARTESIAN_POINT('',(0.409267922647788,-2.71937488542709,7.51860402984325));
#377052=CARTESIAN_POINT('',(0.409267922647788,-2.71937488542709,9.));
#377053=CARTESIAN_POINT('',(0.390468316773804,-2.72213785352539,7.49482233047033));
#377054=CARTESIAN_POINT('Origin',(0.38124556375981,-2.72344040797632,7.53025004711372));
#377055=CARTESIAN_POINT('',(0.312784747585547,-2.7321540406203,7.49482233047033));
#377056=CARTESIAN_POINT('Origin',(2.3631164223042E-16,-1.83278643212712E-15,
7.49482233047033));
#377057=CARTESIAN_POINT('',(0.293899145873147,-2.7342500419777,7.51860402984325));
#377058=CARTESIAN_POINT('Origin',(0.322088566843193,-2.73106859575657,7.53030836256759));
#377059=CARTESIAN_POINT('',(0.293899145873152,-2.7342500419777,8.75721825406948));
#377060=CARTESIAN_POINT('',(0.293899145873152,-2.7342500419777,9.));
#377061=CARTESIAN_POINT('',(0.234196090687521,-2.74000952390803,8.75721825406948));
#377062=CARTESIAN_POINT('Origin',(0.,1.84795814293585E-15,8.75721825406948));
#377063=CARTESIAN_POINT('',(0.234196090687521,-2.74000952390803,7.51860402984325));
#377064=CARTESIAN_POINT('',(0.234196090687521,-2.74000952390803,9.));
#377065=CARTESIAN_POINT('',(0.215258086646198,-2.74156232030815,7.49482233047033));
#377066=CARTESIAN_POINT('Origin',(0.205970827817083,-2.74227129470683,7.53025004711386));
#377067=CARTESIAN_POINT('',(0.137092387371836,-2.74658072470567,7.49482233047033));
#377068=CARTESIAN_POINT('Origin',(1.18399084733063E-16,-1.8441613147383E-15,
7.49482233047033));
#377069=CARTESIAN_POINT('',(0.118111296885581,-2.74746241494729,7.51860402984325));
#377070=CARTESIAN_POINT('Origin',(0.146446635625975,-2.74609360775133,7.53030836256733));
#377071=CARTESIAN_POINT('',(0.118111296885586,-2.74746241494729,8.75721825406948));
#377072=CARTESIAN_POINT('',(0.118111296885586,-2.74746241494729,9.));
#377073=CARTESIAN_POINT('',(0.058161896755696,-2.74938487552503,8.75721825406948));
#377074=CARTESIAN_POINT('Origin',(0.,1.84795814293585E-15,8.75721825406948));
#377075=CARTESIAN_POINT('',(0.058161896755696,-2.74938487552503,7.51860402984325));
#377076=CARTESIAN_POINT('',(0.058161896755696,-2.74938487552503,9.));
#377077=CARTESIAN_POINT('',(0.0391633148678293,-2.74972111945349,7.49482233047033));
#377078=CARTESIAN_POINT('Origin',(0.0298497135624777,-2.74983360047203,
7.5302500471137));
#377079=CARTESIAN_POINT('',(-0.0391633148678293,-2.74972111945349,7.49482233047033));
#377080=CARTESIAN_POINT('Origin',(0.,-1.84795814293585E-15,7.49482233047033));
#377081=CARTESIAN_POINT('',(-0.0581618967557012,-2.74938487552503,7.51860402984325));
#377082=CARTESIAN_POINT('Origin',(-0.0297970762295879,-2.74983433207657,
7.53030836256729));
#377083=CARTESIAN_POINT('',(-0.058161896755696,-2.74938487552503,8.75721825406948));
#377084=CARTESIAN_POINT('',(-0.058161896755696,-2.74938487552503,9.));
#377085=CARTESIAN_POINT('',(-0.118111296885546,-2.7474624149473,8.75721825406948));
#377086=CARTESIAN_POINT('Origin',(0.,1.84795814293585E-15,8.75721825406948));
#377087=CARTESIAN_POINT('',(-0.118111296885546,-2.7474624149473,7.51860402984325));
#377088=CARTESIAN_POINT('',(-0.118111296885546,-2.7474624149473,9.));
#377089=CARTESIAN_POINT('',(-0.137092387371797,-2.74658072470567,7.49482233047033));
#377090=CARTESIAN_POINT('Origin',(-0.146394059567869,-2.74609625013545,
7.53025004711355));
#377091=CARTESIAN_POINT('',(-0.215258086646159,-2.74156232030816,7.49482233047033));
#377092=CARTESIAN_POINT('Origin',(-1.18399084733036E-16,-1.8441613147383E-15,
7.49482233047033));
#377093=CARTESIAN_POINT('',(-0.234196090687486,-2.74000952390803,7.51860402984325));
#377094=CARTESIAN_POINT('Origin',(-0.205918345507357,-2.74227539729371,
7.53030836256732));
#377095=CARTESIAN_POINT('',(-0.234196090687482,-2.74000952390803,8.75721825406948));
#377096=CARTESIAN_POINT('',(-0.234196090687482,-2.74000952390803,9.));
#377097=CARTESIAN_POINT('',(-0.293899145873113,-2.7342500419777,8.75721825406948));
#377098=CARTESIAN_POINT('Origin',(0.,1.84795814293585E-15,8.75721825406948));
#377099=CARTESIAN_POINT('',(-0.293899145873113,-2.7342500419777,7.51860402984325));
#377100=CARTESIAN_POINT('',(-0.293899145873113,-2.7342500419777,9.));
#377101=CARTESIAN_POINT('',(-0.312784747585507,-2.73215404062031,7.49482233047033));
#377102=CARTESIAN_POINT('Origin',(-0.322036268106417,-2.73107460127124,
7.53025004711387));
#377103=CARTESIAN_POINT('',(-0.390468316773765,-2.7221378535254,7.49482233047033));
#377104=CARTESIAN_POINT('Origin',(-2.36311642230394E-16,-1.83278643212713E-15,
7.49482233047033));
#377105=CARTESIAN_POINT('',(-0.409267922647754,-2.71937488542709,7.51860402984325));
#377106=CARTESIAN_POINT('Origin',(-0.381193452134136,-2.72344786468713,
7.53030836256735));
#377107=CARTESIAN_POINT('',(-0.409267922647749,-2.71937488542709,8.75721825406948));
#377108=CARTESIAN_POINT('',(-0.409267922647749,-2.71937488542709,9.));
#377109=CARTESIAN_POINT('',(-0.468479300229117,-2.70980204909083,8.75721825406948));
#377110=CARTESIAN_POINT('Origin',(0.,1.84795814293585E-15,8.75721825406948));
#377111=CARTESIAN_POINT('',(-0.468479300229117,-2.70980204909083,7.51860402984325));
#377112=CARTESIAN_POINT('',(-0.468479300229117,-2.70980204909083,9.));
#377113=CARTESIAN_POINT('',(-0.487191808179271,-2.70650034953684,7.49482233047033));
#377114=CARTESIAN_POINT('Origin',(-0.496355160542152,-2.7048303810568,7.53025004711346));
#377115=CARTESIAN_POINT('',(-0.564074028832556,-2.69152753840577,7.49482233047033));
#377116=CARTESIAN_POINT('Origin',(-3.53253144501139E-16,-1.81388023693489E-15,
7.49482233047033));
#377117=CARTESIAN_POINT('',(-0.582657984926168,-2.68756575223785,7.51860402984325));
#377118=CARTESIAN_POINT('Origin',(-0.554902153100284,-2.69342910062684,
7.53030836256744));
#377119=CARTESIAN_POINT('',(-0.582657984926162,-2.68756575223785,8.75721825406948));
#377120=CARTESIAN_POINT('',(-0.582657984926162,-2.68756575223785,9.));
#377121=CARTESIAN_POINT('',(-0.641134372651986,-2.67421889833352,8.75721825406948));
#377122=CARTESIAN_POINT('Origin',(0.,1.84795814293585E-15,8.75721825406948));
#377123=CARTESIAN_POINT('',(-0.641134372651986,-2.67421889833352,7.51860402984325));
#377124=CARTESIAN_POINT('',(-0.641134372651986,-2.67421889833352,9.));
#377125=CARTESIAN_POINT('',(-0.659596893130912,-2.66972506797461,7.49482233047033));
#377126=CARTESIAN_POINT('Origin',(-0.668634423155866,-2.66747143262224,
7.53025004711362));
#377127=CARTESIAN_POINT('',(-0.735361839713374,-2.64985715929998,7.49482233047033));
#377128=CARTESIAN_POINT('Origin',(-4.68743053828567E-16,-1.78752041877299E-15,
7.49482233047033));
#377129=CARTESIAN_POINT('',(-0.753653780564774,-2.64471283489161,7.51860402984325));
#377130=CARTESIAN_POINT('Origin',(-0.726330642093332,-2.65234245865332,
7.53030836256738));
#377131=CARTESIAN_POINT('',(-0.753653780564768,-2.64471283489162,8.75721825406948));
#377132=CARTESIAN_POINT('',(-0.753653780564768,-2.64471283489162,9.));
#377133=CARTESIAN_POINT('',(-0.811154886414735,-2.62764680850481,8.75721825406948));
#377134=CARTESIAN_POINT('Origin',(0.,1.84795814293585E-15,8.75721825406948));
#377135=CARTESIAN_POINT('',(-0.811154886414735,-2.62764680850481,7.51860402984325));
#377136=CARTESIAN_POINT('',(-0.811154886414735,-2.62764680850481,9.));
#377137=CARTESIAN_POINT('',(-0.829291552965587,-2.62197931345385,7.49482233047033));
#377138=CARTESIAN_POINT('Origin',(-0.838166123503155,-2.6191512719002,7.53025004711377));
#377139=CARTESIAN_POINT('',(-0.903627891060191,-2.59729794873405,7.49482233047033));
#377140=CARTESIAN_POINT('Origin',(-5.82306797402743E-16,-1.75381529578843E-15,
7.49482233047033));
#377141=CARTESIAN_POINT('',(-0.92155265116081,-2.59099222521769,7.51860402984325));
#377142=CARTESIAN_POINT('Origin',(-0.894774482680656,-2.60035677259149,
7.53030836256724));
#377143=CARTESIAN_POINT('',(-0.921552651160805,-2.59099222521769,8.75721825406948));
#377144=CARTESIAN_POINT('',(-0.921552651160805,-2.59099222521769,9.));
#377145=CARTESIAN_POINT('',(-0.977842190757029,-2.57027715431148,8.75721825406948));
#377146=CARTESIAN_POINT('Origin',(0.,1.84795814293585E-15,8.75721825406948));
#377147=CARTESIAN_POINT('',(-0.977842190757029,-2.57027715431148,7.51860402984325));
#377148=CARTESIAN_POINT('',(-0.97784219075703,-2.57027715431148,9.));
#377149=CARTESIAN_POINT('',(-0.995578475926647,-2.56345928352131,7.49482233047033));
#377150=CARTESIAN_POINT('Origin',(-1.00425361946274,-2.56006845679578,7.53025004711368));
#377151=CARTESIAN_POINT('',(-1.06818074157507,-2.53406588377811,7.49482233047033));
#377152=CARTESIAN_POINT('Origin',(-6.93477717441975E-16,-1.71290336956128E-15,
7.49482233047033));
#377153=CARTESIAN_POINT('',(-1.0856646642408,-2.52662467272425,7.51860402984325));
#377154=CARTESIAN_POINT('Origin',(-1.0595415029899,-2.53768566277637,7.53030836256737));
#377155=CARTESIAN_POINT('',(-1.0856646642408,-2.52662467272425,8.75721825406948));
#377156=CARTESIAN_POINT('',(-1.0856646642408,-2.52662467272425,9.));
#377157=CARTESIAN_POINT('',(-1.14051133179101,-2.50234567996836,8.75721825406948));
#377158=CARTESIAN_POINT('Origin',(0.,1.84795814293585E-15,8.75721825406948));
#377159=CARTESIAN_POINT('',(-1.14051133179101,-2.50234567996836,7.51860402984325));
#377160=CARTESIAN_POINT('',(-1.14051133179101,-2.50234567996836,9.));
#377161=CARTESIAN_POINT('',(-1.15777435337921,-2.49440544953249,7.49482233047033));
#377162=CARTESIAN_POINT('Origin',(-1.16621442188832,-2.49046577126939,7.53025004711374));
#377163=CARTESIAN_POINT('',(-1.22834420829876,-2.4604207985503,7.49482233047033));
#377164=CARTESIAN_POINT('Origin',(-8.01798988789735E-16,-1.66495275597197E-15,
7.49482233047033));
#377165=CARTESIAN_POINT('',(-1.24531544834109,-2.4518746774913,7.51860402984325));
#377166=CARTESIAN_POINT('Origin',(-1.21995463999254,-2.464586658241,7.5303083625673));
#377167=CARTESIAN_POINT('',(-1.24531544834108,-2.4518746774913,8.75721825406948));
#377168=CARTESIAN_POINT('',(-1.24531544834108,-2.4518746774913,9.));
#377169=CARTESIAN_POINT('',(-1.29849386712375,-2.42413153047479,8.75721825406948));
#377170=CARTESIAN_POINT('Origin',(0.,1.84795814293585E-15,8.75721825406948));
#377171=CARTESIAN_POINT('',(-1.29849386712375,-2.42413153047479,7.51860402984325));
#377172=CARTESIAN_POINT('',(-1.29849386712375,-2.42413153047479,9.));
#377173=CARTESIAN_POINT('',(-1.31521268767192,-2.41510156850324,7.49482233047033));
#377174=CARTESIAN_POINT('Origin',(-1.32338299910195,-2.41062922768572,7.53025004711353));
#377175=CARTESIAN_POINT('',(-1.38346014519155,-2.37666531650264,7.49482233047033));
#377176=CARTESIAN_POINT('Origin',(-9.06825496107213E-16,-1.61016049437713E-15,
7.49482233047033));
#377177=CARTESIAN_POINT('',(-1.39984896414482,-2.36704940328306,7.51860402984325));
#377178=CARTESIAN_POINT('Origin',(-1.37535472169984,-2.38136013847482,7.53030836256751));
#377179=CARTESIAN_POINT('',(-1.39984896414481,-2.36704940328306,8.75721825406948));
#377180=CARTESIAN_POINT('',(-1.39984896414481,-2.36704940328306,9.));
#377181=CARTESIAN_POINT('',(-1.45114061263041,-2.33595610454791,8.75721825406948));
#377182=CARTESIAN_POINT('Origin',(0.,1.84795814293585E-15,8.75721825406948));
#377183=CARTESIAN_POINT('',(-1.45114061263041,-2.33595610454791,7.51860402984325));
#377184=CARTESIAN_POINT('',(-1.45114061263041,-2.33595610454791,9.));
#377185=CARTESIAN_POINT('',(-1.46724653091875,-2.32587351709136,7.49482233047033));
#377186=CARTESIAN_POINT('Origin',(-1.47511351170771,-2.32088689152705,7.53025004711358));
#377187=CARTESIAN_POINT('',(-1.53289114759647,-2.28314360687636,7.49482233047033));
#377188=CARTESIAN_POINT('Origin',(-1.00812566294773E-15,-1.54875173793256E-15,
7.49482233047033));
#377189=CARTESIAN_POINT('',(-1.54863020028821,-2.27249741534623,7.51860402984325));
#377190=CARTESIAN_POINT('Origin',(-1.52510317584316,-2.28834809909943,7.53030836256754));
#377191=CARTESIAN_POINT('',(-1.54863020028821,-2.27249741534623,8.75721825406948));
#377192=CARTESIAN_POINT('',(-1.54863020028821,-2.27249741534624,9.));
#377193=CARTESIAN_POINT('',(-1.5978243100911,-2.23818173392643,8.75721825406948));
#377194=CARTESIAN_POINT('Origin',(0.,1.84795814293585E-15,8.75721825406948));
#377195=CARTESIAN_POINT('',(-1.5978243100911,-2.23818173392643,7.51860402984325));
#377196=CARTESIAN_POINT('',(-1.5978243100911,-2.23818173392643,9.));
#377197=CARTESIAN_POINT('',(-1.61325114344663,-2.22708795249944,7.49482233047033));
#377198=CARTESIAN_POINT('Origin',(-1.62078246648316,-2.22160753330229,7.53025004711383));
#377199=CARTESIAN_POINT('',(-1.6760231714718,-2.18023997043665,7.49482233047033));
#377200=CARTESIAN_POINT('Origin',(-1.10528322519691E-15,-1.48097882839061E-15,
7.49482233047033));
#377201=CARTESIAN_POINT('',(-1.69104778275849,-2.16860724808058,7.51860402984325));
#377202=CARTESIAN_POINT('Origin',(-1.66858465390362,-2.18593274653549,7.53030836256711));
#377203=CARTESIAN_POINT('',(-1.69104778275848,-2.16860724808058,8.75721825406948));
#377204=CARTESIAN_POINT('',(-1.69104778275848,-2.16860724808058,9.));
#377205=CARTESIAN_POINT('',(-1.73794220472938,-2.13121019447177,8.75721825406948));
#377206=CARTESIAN_POINT('Origin',(0.,1.84795814293585E-15,8.75721825406948));
#377207=CARTESIAN_POINT('',(-1.73794220472938,-2.13121019447177,7.51860402984325));
#377208=CARTESIAN_POINT('',(-1.73794220472938,-2.13121019447177,9.));
#377209=CARTESIAN_POINT('',(-1.75262656098482,-2.11915080580183,7.49482233047033));
#377210=CARTESIAN_POINT('Origin',(-1.75979127844685,-2.11319911319003,7.53025004711381));
#377211=CARTESIAN_POINT('',(-1.81226805662971,-2.06837726029842,7.49482233047033));
#377212=CARTESIAN_POINT('Origin',(-1.19789894159126E-15,-1.40712025917384E-15,
7.49482233047033));
#377213=CARTESIAN_POINT('',(-1.8265164871608,-2.05580580846777,7.51860402984325));
#377214=CARTESIAN_POINT('Origin',(-1.80520955971039,-2.07453492743532,7.53030836256744));
#377215=CARTESIAN_POINT('',(-1.82651648716079,-2.05580580846777,8.75721825406948));
#377216=CARTESIAN_POINT('',(-1.82651648716079,-2.05580580846777,9.));
#377217=CARTESIAN_POINT('',(-1.87091852206099,-2.01548105518488,8.75721825406948));
#377218=CARTESIAN_POINT('Origin',(0.,1.84795814293585E-15,8.75721825406948));
#377219=CARTESIAN_POINT('',(-1.87091852206099,-2.01548105518488,7.51860402984325));
#377220=CARTESIAN_POINT('',(-1.87091852206099,-2.01548105518488,9.));
#377221=CARTESIAN_POINT('',(-1.88480006004669,-2.00250561388676,7.49482233047033));
#377222=CARTESIAN_POINT('Origin',(-1.89156873057341,-1.99610710464184,7.53025004711383));
#377223=CARTESIAN_POINT('',(-1.94106594361265,-1.94801514433209,7.49482233047033));
#377224=CARTESIAN_POINT('Origin',(-1.28559223428609E-15,-1.32747953098578E-15,
7.49482233047033));
#377225=CARTESIAN_POINT('',(-1.9544796435308,-1.934556621819,7.51860402984325));
#377226=CARTESIAN_POINT('Origin',(-1.93441647222029,-1.95461239933181,7.53030836256745));
#377227=CARTESIAN_POINT('',(-1.9544796435308,-1.934556621819,8.75721825406948));
#377228=CARTESIAN_POINT('',(-1.9544796435308,-1.934556621819,9.));
#377229=CARTESIAN_POINT('',(-1.99620683387468,-1.8914698719229,8.75721825406948));
#377230=CARTESIAN_POINT('Origin',(0.,1.84795814293585E-15,8.75721825406948));
#377231=CARTESIAN_POINT('',(-1.99620683387468,-1.8914698719229,7.51860402984325));
#377232=CARTESIAN_POINT('',(-1.99620683387468,-1.8914698719229,9.));
#377233=CARTESIAN_POINT('',(-2.00922851137349,-1.87763169686813,7.49482233047033));
#377234=CARTESIAN_POINT('Origin',(-2.01557332104574,-1.87081266383713,7.53025004711374));
#377235=CARTESIAN_POINT('',(-2.06188757427594,-1.81964821628975,7.49482233047033));
#377236=CARTESIAN_POINT('Origin',(-1.36800275273156E-15,-1.24238390466143E-15,
7.49482233047033));
#377237=CARTESIAN_POINT('',(-2.07441142381097,-1.80535792705008,7.51860402984325));
#377238=CARTESIAN_POINT('Origin',(-2.05567445251486,-1.82665794961634,7.53030836256737));
#377239=CARTESIAN_POINT('',(-2.07441142381097,-1.80535792705008,8.75721825406948));
#377240=CARTESIAN_POINT('',(-2.07441142381097,-1.80535792705008,9.));
#377241=CARTESIAN_POINT('',(-2.11329230362297,-1.75968623323817,8.75721825406948));
#377242=CARTESIAN_POINT('Origin',(0.,1.84795814293585E-15,8.75721825406948));
#377243=CARTESIAN_POINT('',(-2.11329230362297,-1.75968623323817,7.51860402984325));
#377244=CARTESIAN_POINT('',(-2.11329230362297,-1.75968623323817,9.));
#377245=CARTESIAN_POINT('',(-2.12540061176889,-1.74504218845632,7.49482233047033));
#377246=CARTESIAN_POINT('Origin',(-2.13129548840281,-1.73783065250862,7.53025004711368));
#377247=CARTESIAN_POINT('',(-2.17423646662304,-1.68380396341337,7.49482233047033));
#377248=CARTESIAN_POINT('Origin',(-1.4447918544304E-15,-1.15218305638231E-15,
7.49482233047033));
#377249=CARTESIAN_POINT('',(-2.18581900259085,-1.66874062931085,7.51860402984325));
#377250=CARTESIAN_POINT('Origin',(-2.16848522554312,-1.69119737056916,7.53030836256759));
#377251=CARTESIAN_POINT('',(-2.18581900259084,-1.66874062931085,8.75721825406948));
#377252=CARTESIAN_POINT('',(-2.18581900259084,-1.66874062931085,9.));
#377253=CARTESIAN_POINT('',(-2.22169380199589,-1.62067166636955,8.75721825406948));
#377254=CARTESIAN_POINT('Origin',(0.,1.84795814293585E-15,8.75721825406948));
#377255=CARTESIAN_POINT('',(-2.22169380199589,-1.62067166636955,7.51860402984325));
#377256=CARTESIAN_POINT('',(-2.22169380199589,-1.62067166636955,9.));
#377257=CARTESIAN_POINT('',(-2.23283898515353,-1.60528192738178,7.49482233047033));
#377258=CARTESIAN_POINT('Origin',(-2.2382597054367,-1.59770752226531,7.53025004711383));
#377259=CARTESIAN_POINT('',(-2.27765095495652,-1.5410405988765,7.49482233047033));
#377260=CARTESIAN_POINT('Origin',(-1.51564399649249E-15,-1.05724764078203E-15,
7.49482233047033));
#377261=CARTESIAN_POINT('',(-2.28824458223237,-1.52526611838204,7.51860402984325));
#377262=CARTESIAN_POINT('Origin',(-2.27238522764112,-1.54878729876548,7.53030836256757));
#377263=CARTESIAN_POINT('',(-2.28824458223237,-1.52526611838204,8.75721825406948));
#377264=CARTESIAN_POINT('',(-2.28824458223237,-1.52526611838205,9.));
#377265=CARTESIAN_POINT('',(-2.32096588398458,-1.47499741199084,8.75721825406948));
#377266=CARTESIAN_POINT('Origin',(0.,1.84795814293585E-15,8.75721825406948));
#377267=CARTESIAN_POINT('',(-2.32096588398458,-1.47499741199084,7.51860402984325));
#377268=CARTESIAN_POINT('',(-2.32096588398458,-1.47499741199084,9.));
#377269=CARTESIAN_POINT('',(-2.33110214420572,-1.45892521853572,7.49482233047033));
#377270=CARTESIAN_POINT('Origin',(-2.33602643323561,-1.45101906910599,7.53025004711374));
#377271=CARTESIAN_POINT('',(-2.37170608696149,-1.39194476796668,7.49482233047033));
#377272=CARTESIAN_POINT('Origin',(-1.58026803226839E-15,-9.5796776784687E-16,
7.49482233047033));
#377273=CARTESIAN_POINT('',(-2.38126727405858,-1.37552396180424,7.51860402984325));
#377274=CARTESIAN_POINT('Origin',(-2.36694751141368,-1.40001292773726,7.53030836256736));
#377275=CARTESIAN_POINT('',(-2.38126727405858,-1.37552396180425,8.75721825406948));
#377276=CARTESIAN_POINT('',(-2.38126727405858,-1.37552396180425,9.));
#377277=CARTESIAN_POINT('',(-2.41070061931036,-1.32326207686031,8.75721825406948));
#377278=CARTESIAN_POINT('Origin',(0.,1.84795814293585E-15,8.75721825406948));
#377279=CARTESIAN_POINT('',(-2.41070061931036,-1.32326207686031,7.51860402984325));
#377280=CARTESIAN_POINT('',(-2.41070061931036,-1.32326207686031,9.));
#377281=CARTESIAN_POINT('',(-2.41978630452752,-1.30657347302823,7.49482233047033));
#377282=CARTESIAN_POINT('Origin',(-2.42419392734421,-1.29836806734923,7.53025004711348));
#377283=CARTESIAN_POINT('',(-2.45601536992578,-1.23712913743406,7.49482233047033));
#377284=CARTESIAN_POINT('Origin',(-1.63839840773326E-15,-8.54751399870184E-16,
7.49482233047033));
#377285=CARTESIAN_POINT('',(-2.46450482787545,-1.22012948221843,7.51860402984325));
#377286=CARTESIAN_POINT('Origin',(-2.45178350015302,-1.24548560328744,7.53030836256769));
#377287=CARTESIAN_POINT('',(-2.46450482787545,-1.22012948221843,8.75721825406948));
#377288=CARTESIAN_POINT('',(-2.46450482787545,-1.22012948221843,9.));
#377289=CARTESIAN_POINT('',(-2.49052926869773,-1.16608917401713,8.75721825406948));
#377290=CARTESIAN_POINT('Origin',(0.,1.84795814293585E-15,8.75721825406948));
#377291=CARTESIAN_POINT('',(-2.49052926869773,-1.16608917401713,7.51860402984325));
#377292=CARTESIAN_POINT('',(-2.49052926869773,-1.16608917401713,9.));
#377293=CARTESIAN_POINT('',(-2.49852704388149,-1.14885273686093,7.49482233047033));
#377294=CARTESIAN_POINT('Origin',(-2.50239988861744,-1.14038179270459,7.53025004711334));
#377295=CARTESIAN_POINT('',(-2.5302323589214,-1.07722987791236,7.49482233047033));
#377296=CARTESIAN_POINT('Origin',(-1.6897962527054E-15,-7.48022675047831E-16,
7.49482233047033));
#377297=CARTESIAN_POINT('',(-2.53761520271995,-1.05972122887322,7.51860402984325));
#377298=CARTESIAN_POINT('Origin',(-2.5265445845846,-1.0858403113373,7.53030836256713));
#377299=CARTESIAN_POINT('',(-2.53761520271995,-1.05972122887323,8.75721825406948));
#377300=CARTESIAN_POINT('',(-2.53761520271995,-1.05972122887323,9.));
#377301=CARTESIAN_POINT('',(-2.56012379910317,-1.00412456063257,8.75721825406948));
#377302=CARTESIAN_POINT('Origin',(0.,1.84795814293585E-15,8.75721825406948));
#377303=CARTESIAN_POINT('',(-2.56012379910317,-1.00412456063257,7.51860402984325));
#377304=CARTESIAN_POINT('',(-2.56012379910317,-1.00412456063257,9.));
#377305=CARTESIAN_POINT('',(-2.56700079967977,-0.986411118369736,7.49482233047033));
#377306=CARTESIAN_POINT('Origin',(-2.5703229519854,-0.977709444662262,7.5302500471136));
#377307=CARTESIAN_POINT('',(-2.59405208042106,-0.912904049757236,7.49482233047033));
#377308=CARTESIAN_POINT('Origin',(-1.73425036241501E-15,-6.38220164603345E-16,
7.49482233047033));
#377309=CARTESIAN_POINT('',(-2.60029797237973,-0.89495835368909,7.51860402984325));
#377310=CARTESIAN_POINT('Origin',(-2.59092355537579,-0.921733068636329,
7.5303083625673));
#377311=CARTESIAN_POINT('',(-2.60029797237973,-0.894958353689095,8.75721825406948));
#377312=CARTESIAN_POINT('',(-2.60029797237973,-0.894958353689095,9.));
#377313=CARTESIAN_POINT('',(-2.61919823167326,-0.838033784044333,8.75721825406948));
#377314=CARTESIAN_POINT('Origin',(0.,1.84795814293585E-15,8.75721825406948));
#377315=CARTESIAN_POINT('',(-2.61919823167326,-0.838033784044333,7.51860402984325));
#377316=CARTESIAN_POINT('',(-2.61919823167326,-0.838033784044333,9.));
#377317=CARTESIAN_POINT('',(-2.62492619857223,-0.819916125008636,7.49482233047033));
#377318=CARTESIAN_POINT('Origin',(-2.62768400701105,-0.811019478793875,
7.53025004711377));
#377319=CARTESIAN_POINT('',(-2.64721228549986,-0.744826903044354,7.49482233047033));
#377320=CARTESIAN_POINT('Origin',(-1.77157806538992E-15,-5.25795070604709E-16,
7.49482233047033));
#377321=CARTESIAN_POINT('',(-2.65229555990883,-0.726517902661682,7.51860402984325));
#377322=CARTESIAN_POINT('Origin',(-2.64465586552658,-0.753838227045237,
7.53030836256741));
#377323=CARTESIAN_POINT('',(-2.65229555990883,-0.726517902661687,8.75721825406948));
#377324=CARTESIAN_POINT('',(-2.65229555990883,-0.726517902661687,9.));
#377325=CARTESIAN_POINT('',(-2.66750981689315,-0.668499346879772,8.75721825406948));
#377326=CARTESIAN_POINT('Origin',(0.,1.84795814293585E-15,8.75721825406948));
#377327=CARTESIAN_POINT('',(-2.66750981689315,-0.668499346879772,7.51860402984325));
#377328=CARTESIAN_POINT('',(-2.66750981689315,-0.668499346879772,9.));
#377329=CARTESIAN_POINT('',(-2.67206521266984,-0.650051920418417,7.49482233047033));
#377330=CARTESIAN_POINT('Origin',(-2.67424734481532,-0.640996859924407,
7.53025004711345));
#377331=CARTESIAN_POINT('',(-2.68949452747227,-0.573689102821993,7.49482233047033));
#377332=CARTESIAN_POINT('Origin',(-1.80162597409185E-15,-4.11209371878269E-16,
7.49482233047033));
#377333=CARTESIAN_POINT('',(-2.69339429606665,-0.555092033734636,7.51860402984325));
#377334=CARTESIAN_POINT('Origin',(-2.68752071744914,-0.582845702480928,
7.53030836256694));
#377335=CARTESIAN_POINT('',(-2.69339429606665,-0.555092033734641,8.75721825406948));
#377336=CARTESIAN_POINT('',(-2.69339429606665,-0.555092033734641,9.));
#377337=CARTESIAN_POINT('',(-2.70486003209636,-0.496217902506221,8.75721825406948));
#377338=CARTESIAN_POINT('Origin',(0.,1.84795814293585E-15,8.75721825406948));
#377339=CARTESIAN_POINT('',(-2.70486003209636,-0.496217902506221,7.51860402984325));
#377340=CARTESIAN_POINT('',(-2.70486003209636,-0.496217902506221,9.));
#377341=CARTESIAN_POINT('',(-2.70822413765241,-0.4775165130515,7.49482233047033));
#377342=CARTESIAN_POINT('Origin',(-2.7098216266556,-0.468340247463668,7.53025004711366));
#377343=CARTESIAN_POINT('',(-2.72072505953654,-0.400193891020209,7.49482233047033));
#377344=CARTESIAN_POINT('Origin',(-1.82427061521866E-15,-2.94933925638647E-16,
7.49482233047033));
#377345=CARTESIAN_POINT('',(-2.72342529733067,-0.381385172574106,7.51860402984325));
#377346=CARTESIAN_POINT('Origin',(-2.71934197027213,-0.409458139906076,
7.5303083625677));
#377347=CARTESIAN_POINT('',(-2.72342529733067,-0.381385172574111,8.75721825406948));
#377348=CARTESIAN_POINT('',(-2.72342529733067,-0.381385172574111,9.));
#377349=CARTESIAN_POINT('',(-2.73109539723703,-0.321897392332866,8.75721825406948));
#377350=CARTESIAN_POINT('Origin',(0.,1.84795814293585E-15,8.75721825406948));
#377351=CARTESIAN_POINT('',(-2.73109539723703,-0.321897392332866,7.51860402984325));
#377352=CARTESIAN_POINT('',(-2.73109539723703,-0.321897392332866,9.));
#377353=CARTESIAN_POINT('',(-2.73325438874111,-0.303018887905483,7.49482233047033));
#377354=CARTESIAN_POINT('Origin',(-2.734260670177,-0.293759124467549,7.53025004711372));
#377355=CARTESIAN_POINT('',(-2.74077554873748,-0.225054196678903,7.49482233047033));
#377356=CARTESIAN_POINT('Origin',(-1.83941893708273E-15,-1.77446532635447E-16,
7.49482233047033));
#377357=CARTESIAN_POINT('',(-2.74226515987506,-0.206111117932606,7.51860402984325));
#377358=CARTESIAN_POINT('Origin',(-2.73998886364241,-0.234388026004842,
7.53030836256716));
#377359=CARTESIAN_POINT('',(-2.74226515987506,-0.206111117932611,8.75721825406948));
#377360=CARTESIAN_POINT('',(-2.74226515987506,-0.206111117932611,9.));
#377361=CARTESIAN_POINT('',(-2.74610810557233,-0.146254136727642,8.75721825406948));
#377362=CARTESIAN_POINT('Origin',(0.,1.84795814293585E-15,8.75721825406948));
#377363=CARTESIAN_POINT('',(-2.74610810557233,-0.146254136727642,7.51860402984325));
#377364=CARTESIAN_POINT('',(-2.74610810557233,-0.146254136727642,9.));
#377365=CARTESIAN_POINT('',(-2.74705311126524,-0.127276093151715,7.49482233047033));
#377366=CARTESIAN_POINT('Origin',(-2.74746405010756,-0.117970882217936,
7.53025004711368));
#377367=CARTESIAN_POINT('',(-2.74956360331414,-0.0489897063694691,7.49482233047033));
#377368=CARTESIAN_POINT('Origin',(-1.8470086919802E-15,-5.92299737674868E-17,
7.49482233047033));
#377369=CARTESIAN_POINT('',(-2.74983646666349,-0.0299901084968253,7.51860402984325));
#377370=CARTESIAN_POINT('Origin',(-2.74937655504614,-0.0583547614294036,
7.53030836256751));
#377371=CARTESIAN_POINT('',(-2.74983646666349,-0.0299901084968303,8.75721825406948));
#377372=CARTESIAN_POINT('',(-2.74983646666349,-0.0299901084968303,9.));
#377373=CARTESIAN_POINT('',(-2.75,1.51118027317033E-15,8.75721825406948));
#377374=CARTESIAN_POINT('Origin',(0.,1.84795814293585E-15,8.75721825406948));
#377375=CARTESIAN_POINT('',(-2.75,1.51118027317033E-15,9.));
#377376=CARTESIAN_POINT('',(-2.74983646666349,0.0299901084968104,8.75721825406948));
#377377=CARTESIAN_POINT('Origin',(0.,1.84795814293585E-15,8.75721825406948));
#377378=CARTESIAN_POINT('',(-2.74983646666349,0.0299901084968104,7.51860402984325));
#377379=CARTESIAN_POINT('',(-2.74983646666349,0.0299901084968104,9.));
#377380=CARTESIAN_POINT('',(-2.74956360331414,0.0489897063694493,7.49482233047033));
#377381=CARTESIAN_POINT('Origin',(-2.74937751092704,0.0583021276915846,
7.5302500471139));
#377382=CARTESIAN_POINT('',(-2.74705311126524,0.127276093151695,7.49482233047033));
#377383=CARTESIAN_POINT('Origin',(-1.8470086919802E-15,5.92299737674735E-17,
7.49482233047033));
#377384=CARTESIAN_POINT('',(-2.74610810557233,0.146254136727627,7.51860402984325));
#377385=CARTESIAN_POINT('Origin',(-2.7474664684458,0.117918295377799,7.53030836256789));
#377386=CARTESIAN_POINT('',(-2.74610810557233,0.146254136727622,8.75721825406948));
#377387=CARTESIAN_POINT('',(-2.74610810557233,0.146254136727622,9.));
#377388=CARTESIAN_POINT('',(-2.74226515987506,0.206111117932592,8.75721825406948));
#377389=CARTESIAN_POINT('Origin',(0.,1.84795814293585E-15,8.75721825406948));
#377390=CARTESIAN_POINT('',(-2.74226515987506,0.206111117932592,7.51860402984325));
#377391=CARTESIAN_POINT('',(-2.74226515987506,0.206111117932592,9.));
#377392=CARTESIAN_POINT('',(-2.74077554873748,0.225054196678883,7.49482233047033));
#377393=CARTESIAN_POINT('Origin',(-2.73999318981449,0.234335561652496,7.53025004711391));
#377394=CARTESIAN_POINT('',(-2.73325438874111,0.303018887905463,7.49482233047033));
#377395=CARTESIAN_POINT('Origin',(-1.83941893708273E-15,1.77446532635434E-16,
7.49482233047033));
#377396=CARTESIAN_POINT('',(-2.73109539723704,0.321897392332852,7.51860402984325));
#377397=CARTESIAN_POINT('Origin',(-2.73426645279692,0.293706800616217,7.53030836256787));
#377398=CARTESIAN_POINT('',(-2.73109539723704,0.321897392332847,8.75721825406948));
#377399=CARTESIAN_POINT('',(-2.73109539723704,0.321897392332847,9.));
#377400=CARTESIAN_POINT('',(-2.72342529733067,0.381385172574091,8.75721825406948));
#377401=CARTESIAN_POINT('Origin',(0.,1.84795814293585E-15,8.75721825406948));
#377402=CARTESIAN_POINT('',(-2.72342529733067,0.381385172574091,7.51860402984325));
#377403=CARTESIAN_POINT('',(-2.72342529733067,0.381385172574092,9.));
#377404=CARTESIAN_POINT('',(-2.72072505953654,0.400193891020189,7.49482233047033));
#377405=CARTESIAN_POINT('Origin',(-2.71934964895829,0.409406060525678,7.53025004711383));
#377406=CARTESIAN_POINT('',(-2.70822413765242,0.47751651305148,7.49482233047033));
#377407=CARTESIAN_POINT('Origin',(-1.82427061521867E-15,2.94933925638634E-16,
7.49482233047033));
#377408=CARTESIAN_POINT('',(-2.70486003209637,0.496217902506207,7.51860402984325));
#377409=CARTESIAN_POINT('Origin',(-2.70983074979511,0.468288401611352,7.53030836256741));
#377410=CARTESIAN_POINT('',(-2.70486003209637,0.496217902506202,8.75721825406948));
#377411=CARTESIAN_POINT('',(-2.70486003209637,0.496217902506202,9.));
#377412=CARTESIAN_POINT('',(-2.69339429606665,0.555092033734621,8.75721825406948));
#377413=CARTESIAN_POINT('Origin',(0.,1.84795814293585E-15,8.75721825406948));
#377414=CARTESIAN_POINT('',(-2.69339429606665,0.555092033734621,7.51860402984325));
#377415=CARTESIAN_POINT('',(-2.69339429606665,0.555092033734622,9.));
#377416=CARTESIAN_POINT('',(-2.68949452747228,0.573689102821973,7.49482233047033));
#377417=CARTESIAN_POINT('Origin',(-2.68753171709593,0.582794222078531,7.5302500471134));
#377418=CARTESIAN_POINT('',(-2.67206521266985,0.650051920418398,7.49482233047033));
#377419=CARTESIAN_POINT('Origin',(-1.80162597409185E-15,4.11209371878256E-16,
7.49482233047033));
#377420=CARTESIAN_POINT('',(-2.66750981689315,0.668499346879758,7.51860402984325));
#377421=CARTESIAN_POINT('Origin',(-2.67425977098557,0.640945705116324,7.53030836256743));
#377422=CARTESIAN_POINT('',(-2.66750981689316,0.668499346879752,8.75721825406948));
#377423=CARTESIAN_POINT('',(-2.66750981689316,0.668499346879752,9.));
#377424=CARTESIAN_POINT('',(-2.65229555990883,0.726517902661668,8.75721825406948));
#377425=CARTESIAN_POINT('Origin',(0.,1.84795814293585E-15,8.75721825406948));
#377426=CARTESIAN_POINT('',(-2.65229555990883,0.726517902661668,7.51860402984325));
#377427=CARTESIAN_POINT('',(-2.65229555990883,0.726517902661668,9.));
#377428=CARTESIAN_POINT('',(-2.64721228549986,0.744826903044335,7.49482233047033));
#377429=CARTESIAN_POINT('Origin',(-2.64467014093422,0.753787557164282,7.53025004711341));
#377430=CARTESIAN_POINT('',(-2.62492619857223,0.819916125008616,7.49482233047033));
#377431=CARTESIAN_POINT('Origin',(-1.77157806538993E-15,5.25795070604696E-16,
7.49482233047033));
#377432=CARTESIAN_POINT('',(-2.61919823167327,0.838033784044319,7.51860402984325));
#377433=CARTESIAN_POINT('Origin',(-2.62769968515012,0.810969225236588,7.53030836256741));
#377434=CARTESIAN_POINT('',(-2.61919823167327,0.838033784044314,8.75721825406948));
#377435=CARTESIAN_POINT('',(-2.61919823167327,0.838033784044314,9.));
#377436=CARTESIAN_POINT('',(-2.60029797237973,0.894958353689077,8.75721825406948));
#377437=CARTESIAN_POINT('Origin',(0.,1.84795814293585E-15,8.75721825406948));
#377438=CARTESIAN_POINT('',(-2.60029797237973,0.894958353689077,7.51860402984325));
#377439=CARTESIAN_POINT('',(-2.60029797237973,0.894958353689077,9.));
#377440=CARTESIAN_POINT('',(-2.59405208042107,0.912904049757218,7.49482233047033));
#377441=CARTESIAN_POINT('Origin',(-2.59094104788336,0.921683417490968,7.53025004711374));
#377442=CARTESIAN_POINT('',(-2.56700079967978,0.986411118369718,7.49482233047033));
#377443=CARTESIAN_POINT('Origin',(-1.73425036241501E-15,6.38220164603333E-16,
7.49482233047033));
#377444=CARTESIAN_POINT('',(-2.56012379910318,1.00412456063256,7.51860402984325));
#377445=CARTESIAN_POINT('Origin',(-2.57034181766858,0.977660298857961,7.53030836256742));
#377446=CARTESIAN_POINT('',(-2.56012379910318,1.00412456063255,8.75721825406948));
#377447=CARTESIAN_POINT('',(-2.56012379910318,1.00412456063256,9.));
#377448=CARTESIAN_POINT('',(-2.53761520271996,1.05972122887321,8.75721825406948));
#377449=CARTESIAN_POINT('Origin',(0.,1.84795814293585E-15,8.75721825406948));
#377450=CARTESIAN_POINT('',(-2.53761520271996,1.05972122887321,7.51860402984325));
#377451=CARTESIAN_POINT('',(-2.53761520271996,1.05972122887321,9.));
#377452=CARTESIAN_POINT('',(-2.5302323589214,1.07722987791234,7.49482233047033));
#377453=CARTESIAN_POINT('Origin',(-2.52656522231168,1.08579188295449,7.53025004711381));
#377454=CARTESIAN_POINT('',(-2.49852704388149,1.14885273686092,7.49482233047033));
#377455=CARTESIAN_POINT('Origin',(-1.6897962527054E-15,7.48022675047819E-16,
7.49482233047033));
#377456=CARTESIAN_POINT('',(-2.49052926869774,1.16608917401712,7.51860402984325));
#377457=CARTESIAN_POINT('Origin',(-2.50242186432154,1.1403339566041,7.53030836256713));
#377458=CARTESIAN_POINT('',(-2.49052926869774,1.16608917401711,8.75721825406948));
#377459=CARTESIAN_POINT('',(-2.49052926869774,1.16608917401711,9.));
#377460=CARTESIAN_POINT('',(-2.46450482787546,1.22012948221842,8.75721825406948));
#377461=CARTESIAN_POINT('Origin',(0.,1.84795814293585E-15,8.75721825406948));
#377462=CARTESIAN_POINT('',(-2.46450482787546,1.22012948221842,7.51860402984325));
#377463=CARTESIAN_POINT('',(-2.46450482787546,1.22012948221842,9.));
#377464=CARTESIAN_POINT('',(-2.45601536992579,1.23712913743404,7.49482233047033));
#377465=CARTESIAN_POINT('Origin',(-2.45180719829502,1.24543859666924,7.53025004711375));
#377466=CARTESIAN_POINT('',(-2.41978630452753,1.30657347302821,7.49482233047033));
#377467=CARTESIAN_POINT('Origin',(-1.63839840773326E-15,8.54751399870172E-16,
7.49482233047033));
#377468=CARTESIAN_POINT('',(-2.41070061931037,1.3232620768603,7.51860402984325));
#377469=CARTESIAN_POINT('Origin',(-2.42421892276653,1.29832173752101,7.53030836256776));
#377470=CARTESIAN_POINT('',(-2.41070061931037,1.32326207686029,8.75721825406948));
#377471=CARTESIAN_POINT('',(-2.41070061931037,1.32326207686029,9.));
#377472=CARTESIAN_POINT('',(-2.38126727405858,1.37552396180423,8.75721825406948));
#377473=CARTESIAN_POINT('Origin',(0.,1.84795814293585E-15,8.75721825406948));
#377474=CARTESIAN_POINT('',(-2.38126727405858,1.37552396180423,7.51860402984325));
#377475=CARTESIAN_POINT('',(-2.38126727405859,1.37552396180423,9.));
#377476=CARTESIAN_POINT('',(-2.37170608696151,1.39194476796666,7.49482233047033));
#377477=CARTESIAN_POINT('Origin',(-2.36697417258968,1.39996753604437,7.53025004711349));
#377478=CARTESIAN_POINT('',(-2.33110214420573,1.45892521853571,7.49482233047033));
#377479=CARTESIAN_POINT('Origin',(-1.58026803226839E-15,9.57967767846859E-16,
7.49482233047033));
#377480=CARTESIAN_POINT('',(-2.32096588398459,1.47499741199083,7.51860402984325));
#377481=CARTESIAN_POINT('Origin',(-2.33605434566413,1.45097443593007,7.5303083625673));
#377482=CARTESIAN_POINT('',(-2.32096588398459,1.47499741199083,8.75721825406948));
#377483=CARTESIAN_POINT('',(-2.32096588398459,1.47499741199083,9.));
#377484=CARTESIAN_POINT('',(-2.28824458223238,1.52526611838203,8.75721825406948));
#377485=CARTESIAN_POINT('Origin',(0.,1.84795814293585E-15,8.75721825406948));
#377486=CARTESIAN_POINT('',(-2.28824458223238,1.52526611838203,7.51860402984325));
#377487=CARTESIAN_POINT('',(-2.28824458223238,1.52526611838203,9.));
#377488=CARTESIAN_POINT('',(-2.27765095495654,1.54104059887648,7.49482233047033));
#377489=CARTESIAN_POINT('Origin',(-2.27241474229455,1.54874370852221,7.53025004711377));
#377490=CARTESIAN_POINT('',(-2.23283898515355,1.60528192738176,7.49482233047033));
#377491=CARTESIAN_POINT('Origin',(-1.5156439964925E-15,1.05724764078202E-15,
7.49482233047033));
#377492=CARTESIAN_POINT('',(-2.2216938019959,1.62067166636954,7.51860402984325));
#377493=CARTESIAN_POINT('Origin',(-2.23829042017338,1.59766476914869,7.53030836256704));
#377494=CARTESIAN_POINT('',(-2.2216938019959,1.62067166636954,8.75721825406948));
#377495=CARTESIAN_POINT('',(-2.2216938019959,1.62067166636954,9.));
#377496=CARTESIAN_POINT('',(-2.18581900259086,1.66874062931084,8.75721825406948));
#377497=CARTESIAN_POINT('Origin',(0.,1.84795814293585E-15,8.75721825406948));
#377498=CARTESIAN_POINT('',(-2.18581900259086,1.66874062931084,7.51860402984325));
#377499=CARTESIAN_POINT('',(-2.18581900259086,1.66874062931084,9.));
#377500=CARTESIAN_POINT('',(-2.17423646662305,1.68380396341335,7.49482233047033));
#377501=CARTESIAN_POINT('Origin',(-2.16851747239199,1.69115576089708,7.53025004711385));
#377502=CARTESIAN_POINT('',(-2.1254006117689,1.74504218845631,7.49482233047033));
#377503=CARTESIAN_POINT('Origin',(-1.4447918544304E-15,1.1521830563823E-15,
7.49482233047033));
#377504=CARTESIAN_POINT('',(-2.11329230362298,1.75968623323816,7.51860402984325));
#377505=CARTESIAN_POINT('Origin',(-2.1313288792346,1.7377899551325,7.53030836256739));
#377506=CARTESIAN_POINT('',(-2.11329230362298,1.75968623323815,8.75721825406948));
#377507=CARTESIAN_POINT('',(-2.11329230362298,1.75968623323815,9.));
#377508=CARTESIAN_POINT('',(-2.07441142381098,1.80535792705007,8.75721825406948));
#377509=CARTESIAN_POINT('Origin',(0.,1.84795814293585E-15,8.75721825406948));
#377510=CARTESIAN_POINT('',(-2.07441142381098,1.80535792705007,7.51860402984325));
#377511=CARTESIAN_POINT('',(-2.07441142381098,1.80535792705007,9.));
#377512=CARTESIAN_POINT('',(-2.06188757427596,1.81964821628974,7.49482233047033));
#377513=CARTESIAN_POINT('Origin',(-2.05570929905008,1.82661849149836,7.53025004711345));
#377514=CARTESIAN_POINT('',(-2.0092285113735,1.87763169686811,7.49482233047033));
#377515=CARTESIAN_POINT('Origin',(-1.36800275273157E-15,1.24238390466142E-15,
7.49482233047033));
#377516=CARTESIAN_POINT('',(-1.9962068338747,1.89146987192289,7.51860402984325));
#377517=CARTESIAN_POINT('Origin',(-2.01560925076225,1.87077418943615,7.53030836256727));
#377518=CARTESIAN_POINT('',(-1.9962068338747,1.89146987192288,8.75721825406948));
#377519=CARTESIAN_POINT('',(-1.9962068338747,1.89146987192288,9.));
#377520=CARTESIAN_POINT('',(-1.95447964353081,1.93455662181898,8.75721825406948));
#377521=CARTESIAN_POINT('Origin',(0.,1.84795814293585E-15,8.75721825406948));
#377522=CARTESIAN_POINT('',(-1.95447964353081,1.93455662181898,7.51860402984325));
#377523=CARTESIAN_POINT('',(-1.95447964353081,1.93455662181899,9.));
#377524=CARTESIAN_POINT('',(-1.94106594361266,1.94801514433207,7.49482233047033));
#377525=CARTESIAN_POINT('Origin',(-1.93445377525002,1.95457525490979,7.53025004711328));
#377526=CARTESIAN_POINT('',(-1.88480006004671,2.00250561388675,7.49482233047033));
#377527=CARTESIAN_POINT('Origin',(-1.2855922342861E-15,1.32747953098577E-15,
7.49482233047033));
#377528=CARTESIAN_POINT('',(-1.870918522061,2.01548105518487,7.51860402984325));
#377529=CARTESIAN_POINT('Origin',(-1.89160705153176,1.99607101131553,7.5303083625673));
#377530=CARTESIAN_POINT('',(-1.870918522061,2.01548105518486,8.75721825406948));
#377531=CARTESIAN_POINT('',(-1.870918522061,2.01548105518486,9.));
#377532=CARTESIAN_POINT('',(-1.82651648716081,2.05580580846776,8.75721825406948));
#377533=CARTESIAN_POINT('Origin',(0.,1.84795814293585E-15,8.75721825406948));
#377534=CARTESIAN_POINT('',(-1.82651648716081,2.05580580846776,7.51860402984325));
#377535=CARTESIAN_POINT('',(-1.82651648716081,2.05580580846776,9.));
#377536=CARTESIAN_POINT('',(-1.81226805662972,2.0683772602984,7.49482233047033));
#377537=CARTESIAN_POINT('Origin',(-1.80524916594807,2.07450024934405,7.53025004711367));
#377538=CARTESIAN_POINT('',(-1.75262656098483,2.11915080580182,7.49482233047033));
#377539=CARTESIAN_POINT('Origin',(-1.19789894159127E-15,1.40712025917383E-15,
7.49482233047033));
#377540=CARTESIAN_POINT('',(-1.73794220472939,2.13121019447176,7.51860402984325));
#377541=CARTESIAN_POINT('Origin',(-1.75983183317789,2.11316554925368,7.53030836256706));
#377542=CARTESIAN_POINT('',(-1.73794220472939,2.13121019447176,8.75721825406948));
#377543=CARTESIAN_POINT('',(-1.73794220472939,2.13121019447176,9.));
#377544=CARTESIAN_POINT('',(-1.6910477827585,2.16860724808057,8.75721825406948));
#377545=CARTESIAN_POINT('Origin',(0.,1.84795814293585E-15,8.75721825406948));
#377546=CARTESIAN_POINT('',(-1.6910477827585,2.16860724808057,7.51860402984325));
#377547=CARTESIAN_POINT('',(-1.6910477827585,2.16860724808057,9.));
#377548=CARTESIAN_POINT('',(-1.67602317147181,2.18023997043664,7.49482233047033));
#377549=CARTESIAN_POINT('Origin',(-1.66862640059877,2.1859006772746,7.53025004711366));
#377550=CARTESIAN_POINT('',(-1.61325114344665,2.22708795249943,7.49482233047033));
#377551=CARTESIAN_POINT('Origin',(-1.10528322519692E-15,1.4809788283906E-15,
7.49482233047033));
#377552=CARTESIAN_POINT('',(-1.59782431009111,2.23818173392642,7.51860402984325));
#377553=CARTESIAN_POINT('Origin',(-1.62082508833914,2.22157663667705,7.53030836256742));
#377554=CARTESIAN_POINT('',(-1.59782431009111,2.23818173392642,8.75721825406948));
#377555=CARTESIAN_POINT('',(-1.59782431009111,2.23818173392642,9.));
#377556=CARTESIAN_POINT('',(-1.54863020028822,2.27249741534622,8.75721825406948));
#377557=CARTESIAN_POINT('Origin',(0.,1.84795814293585E-15,8.75721825406948));
#377558=CARTESIAN_POINT('',(-1.54863020028822,2.27249741534622,7.51860402984325));
#377559=CARTESIAN_POINT('',(-1.54863020028822,2.27249741534622,9.));
#377560=CARTESIAN_POINT('',(-1.53289114759649,2.28314360687635,7.49482233047033));
#377561=CARTESIAN_POINT('Origin',(-1.52514689144989,2.28831877044818,7.53025004711401));
#377562=CARTESIAN_POINT('',(-1.46724653091876,2.32587351709135,7.49482233047033));
#377563=CARTESIAN_POINT('Origin',(-1.00812566294774E-15,1.54875173793255E-15,
7.49482233047033));
#377564=CARTESIAN_POINT('',(-1.45114061263043,2.3359561045479,7.51860402984325));
#377565=CARTESIAN_POINT('Origin',(-1.47515802554598,2.32085878917399,7.53030836256696));
#377566=CARTESIAN_POINT('',(-1.45114061263043,2.3359561045479,8.75721825406948));
#377567=CARTESIAN_POINT('',(-1.45114061263043,2.3359561045479,9.));
#377568=CARTESIAN_POINT('',(-1.39984896414483,2.36704940328305,8.75721825406948));
#377569=CARTESIAN_POINT('Origin',(0.,1.84795814293585E-15,8.75721825406948));
#377570=CARTESIAN_POINT('',(-1.39984896414483,2.36704940328305,7.51860402984325));
#377571=CARTESIAN_POINT('',(-1.39984896414483,2.36704940328305,9.));
#377572=CARTESIAN_POINT('',(-1.38346014519156,2.37666531650263,7.49482233047033));
#377573=CARTESIAN_POINT('Origin',(-1.37540022658174,2.38133367095072,7.5302500471134));
#377574=CARTESIAN_POINT('',(-1.31521268767194,2.41510156850323,7.49482233047033));
#377575=CARTESIAN_POINT('Origin',(-9.06825496107225E-16,1.61016049437713E-15,
7.49482233047033));
#377576=CARTESIAN_POINT('',(-1.29849386712376,2.42413153047478,7.51860402984325));
#377577=CARTESIAN_POINT('Origin',(-1.3234292220062,2.4106040350831,7.53030836256761));
#377578=CARTESIAN_POINT('',(-1.29849386712377,2.42413153047478,8.75721825406948));
#377579=CARTESIAN_POINT('',(-1.29849386712377,2.42413153047478,9.));
#377580=CARTESIAN_POINT('',(-1.2453154483411,2.45187467749129,8.75721825406948));
#377581=CARTESIAN_POINT('Origin',(0.,1.84795814293585E-15,8.75721825406948));
#377582=CARTESIAN_POINT('',(-1.2453154483411,2.45187467749129,7.51860402984325));
#377583=CARTESIAN_POINT('',(-1.2453154483411,2.45187467749129,9.));
#377584=CARTESIAN_POINT('',(-1.22834420829878,2.46042079855029,7.49482233047033));
#377585=CARTESIAN_POINT('Origin',(-1.22000174715945,2.46456316060527,7.53025004711378));
#377586=CARTESIAN_POINT('',(-1.15777435337923,2.49440544953248,7.49482233047033));
#377587=CARTESIAN_POINT('Origin',(-8.01798988789747E-16,1.66495275597197E-15,
7.49482233047033));
#377588=CARTESIAN_POINT('',(-1.14051133179102,2.50234567996835,7.51860402984325));
#377589=CARTESIAN_POINT('Origin',(-1.16626216391795,2.49044359193945,7.53030836256741));
#377590=CARTESIAN_POINT('',(-1.14051133179103,2.50234567996835,8.75721825406948));
#377591=CARTESIAN_POINT('',(-1.14051133179103,2.50234567996835,9.));
#377592=CARTESIAN_POINT('',(-1.08566466424082,2.52662467272424,8.75721825406948));
#377593=CARTESIAN_POINT('Origin',(0.,1.84795814293585E-15,8.75721825406948));
#377594=CARTESIAN_POINT('',(-1.08566466424082,2.52662467272424,7.51860402984325));
#377595=CARTESIAN_POINT('',(-1.08566466424082,2.52662467272424,9.));
#377596=CARTESIAN_POINT('',(-1.06818074157508,2.53406588377811,7.49482233047033));
#377597=CARTESIAN_POINT('Origin',(-1.05959001886869,2.53766523158564,7.53025004711391));
#377598=CARTESIAN_POINT('',(-0.995578475926665,2.5634592835213,7.49482233047033));
#377599=CARTESIAN_POINT('Origin',(-6.93477717441988E-16,1.71290336956127E-15,
7.49482233047033));
#377600=CARTESIAN_POINT('',(-0.977842190757043,2.57027715431147,7.51860402984325));
#377601=CARTESIAN_POINT('Origin',(-1.00430268443603,2.56004938187791,7.53030836256769));
#377602=CARTESIAN_POINT('',(-0.977842190757048,2.57027715431147,8.75721825406948));
#377603=CARTESIAN_POINT('',(-0.977842190757048,2.57027715431147,9.));
#377604=CARTESIAN_POINT('',(-0.921552651160823,2.59099222521768,8.75721825406948));
#377605=CARTESIAN_POINT('Origin',(0.,1.84795814293585E-15,8.75721825406948));
#377606=CARTESIAN_POINT('',(-0.921552651160823,2.59099222521768,7.51860402984325));
#377607=CARTESIAN_POINT('',(-0.921552651160823,2.59099222521768,9.));
#377608=CARTESIAN_POINT('',(-0.90362789106021,2.59729794873405,7.49482233047033));
#377609=CARTESIAN_POINT('Origin',(-0.894824207909214,2.60033949180186,7.53025004711383));
#377610=CARTESIAN_POINT('',(-0.829291552965606,2.62197931345385,7.49482233047033));
#377611=CARTESIAN_POINT('Origin',(-5.82306797402756E-16,1.75381529578843E-15,
7.49482233047033));
#377612=CARTESIAN_POINT('',(-0.811154886414749,2.62764680850481,7.51860402984325));
#377613=CARTESIAN_POINT('Origin',(-0.838216309801102,2.61913537977751,7.5303083625674));
#377614=CARTESIAN_POINT('',(-0.811154886414754,2.6276468085048,8.75721825406948));
#377615=CARTESIAN_POINT('',(-0.811154886414754,2.6276468085048,9.));
#377616=CARTESIAN_POINT('',(-0.753653780564787,2.64471283489161,8.75721825406948));
#377617=CARTESIAN_POINT('Origin',(0.,1.84795814293585E-15,8.75721825406948));
#377618=CARTESIAN_POINT('',(-0.753653780564787,2.64471283489161,7.51860402984325));
#377619=CARTESIAN_POINT('',(-0.753653780564787,2.64471283489161,9.));
#377620=CARTESIAN_POINT('',(-0.735361839713394,2.64985715929998,7.49482233047033));
#377621=CARTESIAN_POINT('Origin',(-0.726381372340318,2.6523283992752,7.53025004711367));
#377622=CARTESIAN_POINT('',(-0.659596893130931,2.66972506797461,7.49482233047033));
#377623=CARTESIAN_POINT('Origin',(-4.6874305382858E-16,1.78752041877299E-15,
7.49482233047033));
#377624=CARTESIAN_POINT('',(-0.641134372652,2.67421889833352,7.51860402984325));
#377625=CARTESIAN_POINT('Origin',(-0.668685524552393,2.6674587885988,7.53030836256714));
#377626=CARTESIAN_POINT('',(-0.641134372652005,2.67421889833352,8.75721825406948));
#377627=CARTESIAN_POINT('',(-0.641134372652005,2.67421889833352,9.));
#377628=CARTESIAN_POINT('',(-0.582657984926182,2.68756575223785,8.75721825406948));
#377629=CARTESIAN_POINT('Origin',(0.,1.84795814293585E-15,8.75721825406948));
#377630=CARTESIAN_POINT('',(-0.582657984926182,2.68756575223785,7.51860402984325));
#377631=CARTESIAN_POINT('',(-0.582657984926182,2.68756575223785,9.));
#377632=CARTESIAN_POINT('',(-0.564074028832576,2.69152753840577,7.49482233047033));
#377633=CARTESIAN_POINT('Origin',(-0.554953679903967,2.69341832043331,7.53025004711374));
#377634=CARTESIAN_POINT('',(-0.487191808179291,2.70650034953684,7.49482233047033));
#377635=CARTESIAN_POINT('Origin',(-3.53253144501152E-16,1.81388023693489E-15,
7.49482233047033));
#377636=CARTESIAN_POINT('',(-0.468479300229132,2.70980204909083,7.51860402984325));
#377637=CARTESIAN_POINT('Origin',(-0.496406967051098,2.70482103708951,7.5303083625674));
#377638=CARTESIAN_POINT('',(-0.468479300229137,2.70980204909082,8.75721825406948));
#377639=CARTESIAN_POINT('',(-0.468479300229137,2.70980204909082,9.));
#377640=CARTESIAN_POINT('',(-0.409267922647769,2.71937488542709,8.75721825406948));
#377641=CARTESIAN_POINT('Origin',(0.,1.84795814293585E-15,8.75721825406948));
#377642=CARTESIAN_POINT('',(-0.409267922647769,2.71937488542709,7.51860402984325));
#377643=CARTESIAN_POINT('',(-0.409267922647769,2.71937488542709,9.));
#377644=CARTESIAN_POINT('',(-0.390468316773785,2.7221378535254,7.49482233047033));
#377645=CARTESIAN_POINT('Origin',(-0.381245563760008,2.72344040797629,7.53025004711346));
#377646=CARTESIAN_POINT('',(-0.312784747585528,2.73215404062031,7.49482233047033));
#377647=CARTESIAN_POINT('Origin',(-2.36311642230408E-16,1.83278643212713E-15,
7.49482233047033));
#377648=CARTESIAN_POINT('',(-0.293899145873127,2.7342500419777,7.51860402984325));
#377649=CARTESIAN_POINT('Origin',(-0.322088566843094,2.73106859575658,7.53030836256749));
#377650=CARTESIAN_POINT('',(-0.293899145873133,2.7342500419777,8.75721825406948));
#377651=CARTESIAN_POINT('',(-0.293899145873133,2.7342500419777,9.));
#377652=CARTESIAN_POINT('',(-0.234196090687502,2.74000952390803,8.75721825406948));
#377653=CARTESIAN_POINT('Origin',(0.,1.84795814293585E-15,8.75721825406948));
#377654=CARTESIAN_POINT('',(-0.234196090687502,2.74000952390803,7.51860402984325));
#377655=CARTESIAN_POINT('',(-0.234196090687502,2.74000952390803,9.));
#377656=CARTESIAN_POINT('',(-0.215258086646179,2.74156232030816,7.49482233047033));
#377657=CARTESIAN_POINT('Origin',(-0.205970827817116,2.74227129470683,7.53025004711379));
#377658=CARTESIAN_POINT('',(-0.137092387371817,2.74658072470567,7.49482233047033));
#377659=CARTESIAN_POINT('Origin',(-1.1839908473305E-16,1.8441613147383E-15,
7.49482233047033));
#377660=CARTESIAN_POINT('',(-0.118111296885561,2.7474624149473,7.51860402984325));
#377661=CARTESIAN_POINT('Origin',(-0.146446635625942,2.74609360775133,7.53030836256732));
#377662=CARTESIAN_POINT('',(-0.118111296885567,2.74746241494729,8.75721825406948));
#377663=CARTESIAN_POINT('',(-0.118111296885567,2.74746241494729,9.));
#377664=CARTESIAN_POINT('',(-0.058161896755696,2.74938487552503,8.75721825406948));
#377665=CARTESIAN_POINT('Origin',(0.,1.84795814293585E-15,8.75721825406948));
#377666=CARTESIAN_POINT('',(-0.058161896755696,2.74938487552503,7.51860402984325));
#377667=CARTESIAN_POINT('',(-0.058161896755696,2.74938487552503,9.));
#377668=CARTESIAN_POINT('',(-0.0391633148678293,2.74972111945349,7.49482233047033));
#377669=CARTESIAN_POINT('Origin',(-0.0298497135624777,2.74983360047203,
7.5302500471137));
#377670=CARTESIAN_POINT('',(0.0391633148678293,2.74972111945349,7.49482233047033));
#377671=CARTESIAN_POINT('Origin',(0.,1.84795814293585E-15,7.49482233047033));
#377672=CARTESIAN_POINT('',(0.058161896755696,2.74938487552503,7.51860402984325));
#377673=CARTESIAN_POINT('Origin',(0.0297970762297926,2.74983433207657,7.530308362567));
#377674=CARTESIAN_POINT('',(0.058161896755696,2.74938487552503,8.75721825406948));
#377675=CARTESIAN_POINT('',(0.058161896755696,2.74938487552503,9.));
#377676=CARTESIAN_POINT('',(0.118111296885527,2.7474624149473,8.75721825406948));
#377677=CARTESIAN_POINT('Origin',(0.,1.84795814293585E-15,8.75721825406948));
#377678=CARTESIAN_POINT('',(0.118111296885527,2.7474624149473,7.51860402984325));
#377679=CARTESIAN_POINT('',(0.118111296885527,2.7474624149473,9.));
#377680=CARTESIAN_POINT('',(0.137092387371777,2.74658072470567,7.49482233047033));
#377681=CARTESIAN_POINT('Origin',(0.146394059568022,2.74609625013544,7.53025004711377));
#377682=CARTESIAN_POINT('',(0.21525808664614,2.74156232030816,7.49482233047033));
#377683=CARTESIAN_POINT('Origin',(1.18399084733023E-16,1.8441613147383E-15,
7.49482233047033));
#377684=CARTESIAN_POINT('',(0.234196090687467,2.74000952390803,7.51860402984325));
#377685=CARTESIAN_POINT('Origin',(0.205918345507194,2.74227539729373,7.53030836256749));
#377686=CARTESIAN_POINT('',(0.234196090687462,2.74000952390803,8.75721825406948));
#377687=CARTESIAN_POINT('',(0.234196090687462,2.74000952390803,9.));
#377688=CARTESIAN_POINT('',(0.293899145873092,2.7342500419777,8.75721825406948));
#377689=CARTESIAN_POINT('Origin',(0.,1.84795814293585E-15,8.75721825406948));
#377690=CARTESIAN_POINT('',(0.293899145873092,2.7342500419777,7.51860402984325));
#377691=CARTESIAN_POINT('',(0.293899145873092,2.7342500419777,9.));
#377692=CARTESIAN_POINT('',(0.312784747585487,2.73215404062031,7.49482233047033));
#377693=CARTESIAN_POINT('Origin',(0.322036268106352,2.73107460127124,7.53025004711382));
#377694=CARTESIAN_POINT('',(0.390468316773744,2.7221378535254,7.49482233047033));
#377695=CARTESIAN_POINT('Origin',(2.3631164223038E-16,1.83278643212713E-15,
7.49482233047033));
#377696=CARTESIAN_POINT('',(0.409267922647734,2.71937488542709,7.51860402984325));
#377697=CARTESIAN_POINT('Origin',(0.38119345213415,2.72344786468714,7.5303083625673));
#377698=CARTESIAN_POINT('',(0.409267922647728,2.71937488542709,8.75721825406948));
#377699=CARTESIAN_POINT('',(0.409267922647728,2.71937488542709,9.));
#377700=CARTESIAN_POINT('',(0.468479300229098,2.70980204909083,8.75721825406948));
#377701=CARTESIAN_POINT('Origin',(0.,1.84795814293585E-15,8.75721825406948));
#377702=CARTESIAN_POINT('',(0.468479300229098,2.70980204909083,7.51860402984325));
#377703=CARTESIAN_POINT('',(0.468479300229098,2.70980204909083,9.));
#377704=CARTESIAN_POINT('',(0.487191808179253,2.70650034953684,7.49482233047033));
#377705=CARTESIAN_POINT('Origin',(0.496355160542298,2.70483038105678,7.53025004711366));
#377706=CARTESIAN_POINT('',(0.564074028832537,2.69152753840577,7.49482233047033));
#377707=CARTESIAN_POINT('Origin',(3.53253144501126E-16,1.81388023693489E-15,
7.49482233047033));
#377708=CARTESIAN_POINT('',(0.582657984926149,2.68756575223785,7.51860402984325));
#377709=CARTESIAN_POINT('Origin',(0.554902153100358,2.69342910062683,7.53030836256731));
#377710=CARTESIAN_POINT('',(0.582657984926143,2.68756575223785,8.75721825406948));
#377711=CARTESIAN_POINT('',(0.582657984926143,2.68756575223785,9.));
#377712=CARTESIAN_POINT('',(0.641134372651966,2.67421889833353,8.75721825406948));
#377713=CARTESIAN_POINT('Origin',(0.,1.84795814293585E-15,8.75721825406948));
#377714=CARTESIAN_POINT('',(0.641134372651966,2.67421889833353,7.51860402984325));
#377715=CARTESIAN_POINT('',(0.641134372651966,2.67421889833353,9.));
#377716=CARTESIAN_POINT('',(0.659596893130892,2.66972506797462,7.49482233047033));
#377717=CARTESIAN_POINT('Origin',(0.668634423155899,2.66747143262223,7.5302500471137));
#377718=CARTESIAN_POINT('',(0.735361839713355,2.64985715929999,7.49482233047033));
#377719=CARTESIAN_POINT('Origin',(4.68743053828553E-16,1.787520418773E-15,
7.49482233047033));
#377720=CARTESIAN_POINT('',(0.753653780564754,2.64471283489162,7.51860402984325));
#377721=CARTESIAN_POINT('Origin',(0.726330642093246,2.65234245865335,7.53030836256748));
#377722=CARTESIAN_POINT('',(0.753653780564748,2.64471283489162,8.75721825406948));
#377723=CARTESIAN_POINT('',(0.753653780564749,2.64471283489162,9.));
#377724=CARTESIAN_POINT('',(0.811154886414717,2.62764680850482,8.75721825406948));
#377725=CARTESIAN_POINT('Origin',(0.,1.84795814293585E-15,8.75721825406948));
#377726=CARTESIAN_POINT('',(0.811154886414717,2.62764680850482,7.51860402984325));
#377727=CARTESIAN_POINT('',(0.811154886414717,2.62764680850482,9.));
#377728=CARTESIAN_POINT('',(0.829291552965569,2.62197931345386,7.49482233047033));
#377729=CARTESIAN_POINT('Origin',(0.838166123502919,2.61915127190027,7.53025004711349));
#377730=CARTESIAN_POINT('',(0.903627891060173,2.59729794873406,7.49482233047033));
#377731=CARTESIAN_POINT('Origin',(5.82306797402731E-16,1.75381529578844E-15,
7.49482233047033));
#377732=CARTESIAN_POINT('',(0.921552651160791,2.59099222521769,7.51860402984325));
#377733=CARTESIAN_POINT('Origin',(0.894774482680453,2.60035677259156,7.53030836256745));
#377734=CARTESIAN_POINT('',(0.921552651160786,2.59099222521769,8.75721825406948));
#377735=CARTESIAN_POINT('',(0.921552651160786,2.5909922252177,9.));
#377736=CARTESIAN_POINT('',(0.97784219075701,2.57027715431148,8.75721825406948));
#377737=CARTESIAN_POINT('Origin',(0.,1.84795814293585E-15,8.75721825406948));
#377738=CARTESIAN_POINT('',(0.97784219075701,2.57027715431148,7.51860402984325));
#377739=CARTESIAN_POINT('',(0.97784219075701,2.57027715431149,9.));
#377740=CARTESIAN_POINT('',(0.995578475926628,2.56345928352132,7.49482233047033));
#377741=CARTESIAN_POINT('Origin',(1.00425361946275,2.56006845679578,7.53025004711372));
#377742=CARTESIAN_POINT('',(1.06818074157505,2.53406588377812,7.49482233047033));
#377743=CARTESIAN_POINT('Origin',(6.93477717441963E-16,1.71290336956128E-15,
7.49482233047033));
#377744=CARTESIAN_POINT('',(1.08566466424078,2.52662467272426,7.51860402984325));
#377745=CARTESIAN_POINT('Origin',(1.05954150299006,2.53768566277631,7.53030836256713));
#377746=CARTESIAN_POINT('',(1.08566466424078,2.52662467272426,8.75721825406948));
#377747=CARTESIAN_POINT('',(1.08566466424078,2.52662467272426,9.));
#377748=CARTESIAN_POINT('',(1.14051133179099,2.50234567996837,8.75721825406948));
#377749=CARTESIAN_POINT('Origin',(0.,1.84795814293585E-15,8.75721825406948));
#377750=CARTESIAN_POINT('',(1.14051133179099,2.50234567996837,7.51860402984325));
#377751=CARTESIAN_POINT('',(1.14051133179099,2.50234567996837,9.));
#377752=CARTESIAN_POINT('',(1.15777435337919,2.49440544953249,7.49482233047033));
#377753=CARTESIAN_POINT('Origin',(1.16621442188813,2.49046577126948,7.5302500471135));
#377754=CARTESIAN_POINT('',(1.22834420829874,2.46042079855031,7.49482233047033));
#377755=CARTESIAN_POINT('Origin',(8.01798988789723E-16,1.66495275597198E-15,
7.49482233047033));
#377756=CARTESIAN_POINT('',(1.24531544834107,2.4518746774913,7.51860402984325));
#377757=CARTESIAN_POINT('Origin',(1.21995463999246,2.46458665824104,7.53030836256742));
#377758=CARTESIAN_POINT('',(1.24531544834107,2.45187467749131,8.75721825406948));
#377759=CARTESIAN_POINT('',(1.24531544834107,2.45187467749131,9.));
#377760=CARTESIAN_POINT('',(1.29849386712373,2.4241315304748,8.75721825406948));
#377761=CARTESIAN_POINT('Origin',(0.,1.84795814293585E-15,8.75721825406948));
#377762=CARTESIAN_POINT('',(1.29849386712373,2.4241315304748,7.51860402984325));
#377763=CARTESIAN_POINT('',(1.29849386712373,2.4241315304748,9.));
#377764=CARTESIAN_POINT('',(1.3152126876719,2.41510156850325,7.49482233047033));
#377765=CARTESIAN_POINT('Origin',(1.3233829991019,2.41062922768575,7.53025004711348));
#377766=CARTESIAN_POINT('',(1.38346014519153,2.37666531650265,7.49482233047033));
#377767=CARTESIAN_POINT('Origin',(9.06825496107201E-16,1.61016049437714E-15,
7.49482233047033));
#377768=CARTESIAN_POINT('',(1.3998489641448,2.36704940328307,7.51860402984325));
#377769=CARTESIAN_POINT('Origin',(1.37535472169997,2.38136013847475,7.53030836256734));
#377770=CARTESIAN_POINT('',(1.3998489641448,2.36704940328307,8.75721825406948));
#377771=CARTESIAN_POINT('',(1.3998489641448,2.36704940328307,9.));
#377772=CARTESIAN_POINT('',(1.4511406126304,2.33595610454792,8.75721825406948));
#377773=CARTESIAN_POINT('Origin',(0.,1.84795814293585E-15,8.75721825406948));
#377774=CARTESIAN_POINT('',(1.4511406126304,2.33595610454792,7.51860402984325));
#377775=CARTESIAN_POINT('',(1.4511406126304,2.33595610454792,9.));
#377776=CARTESIAN_POINT('',(1.46724653091873,2.32587351709137,7.49482233047033));
#377777=CARTESIAN_POINT('Origin',(1.47511351170756,2.32088689152714,7.53025004711339));
#377778=CARTESIAN_POINT('',(1.53289114759645,2.28314360687637,7.49482233047033));
#377779=CARTESIAN_POINT('Origin',(1.00812566294772E-15,1.54875173793256E-15,
7.49482233047033));
#377780=CARTESIAN_POINT('',(1.5486302002882,2.27249741534624,7.51860402984325));
#377781=CARTESIAN_POINT('Origin',(1.52510317584322,2.28834809909939,7.5303083625674));
#377782=CARTESIAN_POINT('',(1.54863020028819,2.27249741534625,8.75721825406948));
#377783=CARTESIAN_POINT('',(1.54863020028819,2.27249741534625,9.));
#377784=CARTESIAN_POINT('',(1.59782431009108,2.23818173392644,8.75721825406948));
#377785=CARTESIAN_POINT('Origin',(0.,1.84795814293585E-15,8.75721825406948));
#377786=CARTESIAN_POINT('',(1.59782431009108,2.23818173392644,7.51860402984325));
#377787=CARTESIAN_POINT('',(1.59782431009108,2.23818173392644,9.));
#377788=CARTESIAN_POINT('',(1.61325114344662,2.22708795249945,7.49482233047033));
#377789=CARTESIAN_POINT('Origin',(1.62078246648304,2.22160753330238,7.53025004711372));
#377790=CARTESIAN_POINT('',(1.67602317147178,2.18023997043667,7.49482233047033));
#377791=CARTESIAN_POINT('Origin',(1.1052832251969E-15,1.48097882839062E-15,
7.49482233047033));
#377792=CARTESIAN_POINT('',(1.69104778275847,2.16860724808059,7.51860402984325));
#377793=CARTESIAN_POINT('Origin',(1.66858465390346,2.18593274653562,7.53030836256734));
#377794=CARTESIAN_POINT('',(1.69104778275847,2.16860724808059,8.75721825406948));
#377795=CARTESIAN_POINT('',(1.69104778275847,2.16860724808059,9.));
#377796=CARTESIAN_POINT('',(1.73794220472936,2.13121019447178,8.75721825406948));
#377797=CARTESIAN_POINT('Origin',(0.,1.84795814293585E-15,8.75721825406948));
#377798=CARTESIAN_POINT('',(1.73794220472936,2.13121019447178,7.51860402984325));
#377799=CARTESIAN_POINT('',(1.73794220472936,2.13121019447179,9.));
#377800=CARTESIAN_POINT('',(1.7526265609848,2.11915080580184,7.49482233047033));
#377801=CARTESIAN_POINT('Origin',(1.75979127844668,2.11319911319018,7.53025004711357));
#377802=CARTESIAN_POINT('',(1.8122680566297,2.06837726029843,7.49482233047033));
#377803=CARTESIAN_POINT('Origin',(1.19789894159125E-15,1.40712025917385E-15,
7.49482233047033));
#377804=CARTESIAN_POINT('',(1.82651648716078,2.05580580846778,7.51860402984325));
#377805=CARTESIAN_POINT('Origin',(1.80520955971042,2.0745349274353,7.53030836256737));
#377806=CARTESIAN_POINT('',(1.82651648716078,2.05580580846778,8.75721825406948));
#377807=CARTESIAN_POINT('',(1.82651648716078,2.05580580846778,9.));
#377808=CARTESIAN_POINT('',(1.87091852206097,2.01548105518489,8.75721825406948));
#377809=CARTESIAN_POINT('Origin',(0.,1.84795814293585E-15,8.75721825406948));
#377810=CARTESIAN_POINT('',(1.87091852206097,2.01548105518489,7.51860402984325));
#377811=CARTESIAN_POINT('',(1.87091852206097,2.01548105518489,9.));
#377812=CARTESIAN_POINT('',(1.88480006004668,2.00250561388678,7.49482233047033));
#377813=CARTESIAN_POINT('Origin',(1.89156873057342,1.99610710464183,7.53025004711385));
#377814=CARTESIAN_POINT('',(1.94106594361263,1.9480151443321,7.49482233047033));
#377815=CARTESIAN_POINT('Origin',(1.28559223428608E-15,1.32747953098579E-15,
7.49482233047033));
#377816=CARTESIAN_POINT('',(1.95447964353079,1.93455662181901,7.51860402984325));
#377817=CARTESIAN_POINT('Origin',(1.93441647222035,1.95461239933176,7.53030836256736));
#377818=CARTESIAN_POINT('',(1.95447964353078,1.93455662181901,8.75721825406948));
#377819=CARTESIAN_POINT('',(1.95447964353078,1.93455662181901,9.));
#377820=CARTESIAN_POINT('',(1.99620683387467,1.89146987192291,8.75721825406948));
#377821=CARTESIAN_POINT('Origin',(0.,1.84795814293585E-15,8.75721825406948));
#377822=CARTESIAN_POINT('',(1.99620683387467,1.89146987192291,7.51860402984325));
#377823=CARTESIAN_POINT('',(1.99620683387467,1.89146987192291,9.));
#377824=CARTESIAN_POINT('',(2.00922851137348,1.87763169686814,7.49482233047033));
#377825=CARTESIAN_POINT('Origin',(2.01557332104575,1.87081266383712,7.53025004711375));
#377826=CARTESIAN_POINT('',(2.06188757427593,1.81964821628977,7.49482233047033));
#377827=CARTESIAN_POINT('Origin',(1.36800275273155E-15,1.24238390466144E-15,
7.49482233047033));
#377828=CARTESIAN_POINT('',(2.07441142381096,1.80535792705009,7.51860402984325));
#377829=CARTESIAN_POINT('Origin',(2.05567445251497,1.82665794961622,7.53030836256716));
#377830=CARTESIAN_POINT('',(2.07441142381095,1.8053579270501,8.75721825406948));
#377831=CARTESIAN_POINT('',(2.07441142381095,1.8053579270501,9.));
#377832=CARTESIAN_POINT('',(2.11329230362296,1.75968623323818,8.75721825406948));
#377833=CARTESIAN_POINT('Origin',(0.,1.84795814293585E-15,8.75721825406948));
#377834=CARTESIAN_POINT('',(2.11329230362296,1.75968623323818,7.51860402984325));
#377835=CARTESIAN_POINT('',(2.11329230362296,1.75968623323818,9.));
#377836=CARTESIAN_POINT('',(2.12540061176888,1.74504218845634,7.49482233047033));
#377837=CARTESIAN_POINT('Origin',(2.13129548840287,1.73783065250855,7.5302500471138));
#377838=CARTESIAN_POINT('',(2.17423646662303,1.68380396341338,7.49482233047033));
#377839=CARTESIAN_POINT('Origin',(1.44479185443039E-15,1.15218305638232E-15,
7.49482233047033));
#377840=CARTESIAN_POINT('',(2.18581900259084,1.66874062931087,7.51860402984325));
#377841=CARTESIAN_POINT('Origin',(2.16848522554325,1.691197370569,7.53030836256729));
#377842=CARTESIAN_POINT('',(2.18581900259083,1.66874062931087,8.75721825406948));
#377843=CARTESIAN_POINT('',(2.18581900259083,1.66874062931087,9.));
#377844=CARTESIAN_POINT('',(2.22169380199588,1.62067166636957,8.75721825406948));
#377845=CARTESIAN_POINT('Origin',(0.,1.84795814293585E-15,8.75721825406948));
#377846=CARTESIAN_POINT('',(2.22169380199588,1.62067166636957,7.51860402984325));
#377847=CARTESIAN_POINT('',(2.22169380199588,1.62067166636957,9.));
#377848=CARTESIAN_POINT('',(2.23283898515352,1.60528192738179,7.49482233047033));
#377849=CARTESIAN_POINT('Origin',(2.23825970543661,1.59770752226543,7.53025004711368));
#377850=CARTESIAN_POINT('',(2.27765095495651,1.54104059887652,7.49482233047033));
#377851=CARTESIAN_POINT('Origin',(1.51564399649249E-15,1.05724764078204E-15,
7.49482233047033));
#377852=CARTESIAN_POINT('',(2.28824458223236,1.52526611838206,7.51860402984325));
#377853=CARTESIAN_POINT('Origin',(2.27238522764112,1.54878729876548,7.5303083625675));
#377854=CARTESIAN_POINT('',(2.28824458223236,1.52526611838206,8.75721825406948));
#377855=CARTESIAN_POINT('',(2.28824458223236,1.52526611838206,9.));
#377856=CARTESIAN_POINT('',(2.32096588398457,1.47499741199086,8.75721825406948));
#377857=CARTESIAN_POINT('Origin',(0.,1.84795814293585E-15,8.75721825406948));
#377858=CARTESIAN_POINT('',(2.32096588398457,1.47499741199086,7.51860402984325));
#377859=CARTESIAN_POINT('',(2.32096588398457,1.47499741199086,9.));
#377860=CARTESIAN_POINT('',(2.33110214420571,1.45892521853574,7.49482233047033));
#377861=CARTESIAN_POINT('Origin',(2.33602643323555,1.45101906910609,7.53025004711363));
#377862=CARTESIAN_POINT('',(2.37170608696149,1.39194476796669,7.49482233047033));
#377863=CARTESIAN_POINT('Origin',(1.58026803226838E-15,9.57967767846882E-16,
7.49482233047033));
#377864=CARTESIAN_POINT('',(2.38126727405857,1.37552396180426,7.51860402984325));
#377865=CARTESIAN_POINT('Origin',(2.36694751141372,1.40001292773719,7.53030836256726));
#377866=CARTESIAN_POINT('',(2.38126727405857,1.37552396180426,8.75721825406948));
#377867=CARTESIAN_POINT('',(2.38126727405857,1.37552396180426,9.));
#377868=CARTESIAN_POINT('',(2.41070061931035,1.32326207686033,8.75721825406948));
#377869=CARTESIAN_POINT('Origin',(0.,1.84795814293585E-15,8.75721825406948));
#377870=CARTESIAN_POINT('',(2.41070061931035,1.32326207686033,7.51860402984325));
#377871=CARTESIAN_POINT('',(2.41070061931035,1.32326207686033,9.));
#377872=CARTESIAN_POINT('',(2.41978630452751,1.30657347302825,7.49482233047033));
#377873=CARTESIAN_POINT('Origin',(2.42419392734427,1.29836806734912,7.53025004711366));
#377874=CARTESIAN_POINT('',(2.45601536992577,1.23712913743408,7.49482233047033));
#377875=CARTESIAN_POINT('Origin',(1.63839840773325E-15,8.54751399870196E-16,
7.49482233047033));
#377876=CARTESIAN_POINT('',(2.46450482787544,1.22012948221845,7.51860402984325));
#377877=CARTESIAN_POINT('Origin',(2.45178350015316,1.24548560328717,7.53030836256726));
#377878=CARTESIAN_POINT('',(2.46450482787544,1.22012948221845,8.75721825406948));
#377879=CARTESIAN_POINT('',(2.46450482787544,1.22012948221845,9.));
#377880=CARTESIAN_POINT('',(2.49052926869772,1.16608917401715,8.75721825406948));
#377881=CARTESIAN_POINT('Origin',(0.,1.84795814293585E-15,8.75721825406948));
#377882=CARTESIAN_POINT('',(2.49052926869772,1.16608917401715,7.51860402984325));
#377883=CARTESIAN_POINT('',(2.49052926869772,1.16608917401715,9.));
#377884=CARTESIAN_POINT('',(2.49852704388148,1.14885273686095,7.49482233047033));
#377885=CARTESIAN_POINT('Origin',(2.50239988861758,1.14038179270428,7.53025004711374));
#377886=CARTESIAN_POINT('',(2.53023235892139,1.07722987791238,7.49482233047033));
#377887=CARTESIAN_POINT('Origin',(1.68979625270539E-15,7.48022675047843E-16,
7.49482233047033));
#377888=CARTESIAN_POINT('',(2.53761520271995,1.05972122887324,7.51860402984325));
#377889=CARTESIAN_POINT('Origin',(2.52654458458447,1.08584031133761,7.53030836256753));
#377890=CARTESIAN_POINT('',(2.53761520271994,1.05972122887325,8.75721825406948));
#377891=CARTESIAN_POINT('',(2.53761520271995,1.05972122887325,9.));
#377892=CARTESIAN_POINT('',(2.56012379910316,1.00412456063259,8.75721825406948));
#377893=CARTESIAN_POINT('Origin',(0.,1.84795814293585E-15,8.75721825406948));
#377894=CARTESIAN_POINT('',(2.56012379910316,1.00412456063259,7.51860402984325));
#377895=CARTESIAN_POINT('',(2.56012379910316,1.00412456063259,9.));
#377896=CARTESIAN_POINT('',(2.56700079967976,0.986411118369754,7.49482233047033));
#377897=CARTESIAN_POINT('Origin',(2.57032295198543,0.977709444662182,7.53025004711375));
#377898=CARTESIAN_POINT('',(2.59405208042106,0.912904049757255,7.49482233047033));
#377899=CARTESIAN_POINT('Origin',(1.734250362415E-15,6.38220164603358E-16,
7.49482233047033));
#377900=CARTESIAN_POINT('',(2.60029797237972,0.894958353689109,7.51860402984325));
#377901=CARTESIAN_POINT('Origin',(2.5909235553758,0.921733068636293,7.53030836256721));
#377902=CARTESIAN_POINT('',(2.60029797237972,0.894958353689114,8.75721825406948));
#377903=CARTESIAN_POINT('',(2.60029797237972,0.894958353689114,9.));
#377904=CARTESIAN_POINT('',(2.61919823167326,0.838033784044351,8.75721825406948));
#377905=CARTESIAN_POINT('Origin',(0.,1.84795814293585E-15,8.75721825406948));
#377906=CARTESIAN_POINT('',(2.61919823167326,0.838033784044351,7.51860402984325));
#377907=CARTESIAN_POINT('',(2.61919823167326,0.838033784044351,9.));
#377908=CARTESIAN_POINT('',(2.62492619857222,0.819916125008653,7.49482233047033));
#377909=CARTESIAN_POINT('Origin',(2.62768400701103,0.81101947879393,7.53025004711372));
#377910=CARTESIAN_POINT('',(2.64721228549985,0.744826903044372,7.49482233047033));
#377911=CARTESIAN_POINT('Origin',(1.77157806538992E-15,5.25795070604721E-16,
7.49482233047033));
#377912=CARTESIAN_POINT('',(2.65229555990882,0.7265179026617,7.51860402984325));
#377913=CARTESIAN_POINT('Origin',(2.6446558655266,0.753838227045187,7.53030836256735));
#377914=CARTESIAN_POINT('',(2.65229555990882,0.726517902661705,8.75721825406948));
#377915=CARTESIAN_POINT('',(2.65229555990882,0.726517902661705,9.));
#377916=CARTESIAN_POINT('',(2.66750981689315,0.668499346879791,8.75721825406948));
#377917=CARTESIAN_POINT('Origin',(0.,1.84795814293585E-15,8.75721825406948));
#377918=CARTESIAN_POINT('',(2.66750981689315,0.668499346879791,7.51860402984325));
#377919=CARTESIAN_POINT('',(2.66750981689315,0.668499346879791,9.));
#377920=CARTESIAN_POINT('',(2.67206521266984,0.650051920418436,7.49482233047033));
#377921=CARTESIAN_POINT('Origin',(2.67424734481537,0.640996859924186,7.53025004711375));
#377922=CARTESIAN_POINT('',(2.68949452747227,0.573689102822012,7.49482233047033));
#377923=CARTESIAN_POINT('Origin',(1.80162597409184E-15,4.11209371878282E-16,
7.49482233047033));
#377924=CARTESIAN_POINT('',(2.69339429606665,0.555092033734655,7.51860402984325));
#377925=CARTESIAN_POINT('Origin',(2.68752071744906,0.582845702481334,7.53030836256744));
#377926=CARTESIAN_POINT('',(2.69339429606664,0.55509203373466,8.75721825406948));
#377927=CARTESIAN_POINT('',(2.69339429606664,0.55509203373466,9.));
#377928=CARTESIAN_POINT('',(2.70486003209636,0.49621790250624,8.75721825406948));
#377929=CARTESIAN_POINT('Origin',(0.,1.84795814293585E-15,8.75721825406948));
#377930=CARTESIAN_POINT('',(2.70486003209636,0.49621790250624,7.51860402984325));
#377931=CARTESIAN_POINT('',(2.70486003209636,0.49621790250624,9.));
#377932=CARTESIAN_POINT('',(2.70822413765241,0.477516513051518,7.49482233047033));
#377933=CARTESIAN_POINT('Origin',(2.70982162665562,0.468340247463557,7.5302500471138));
#377934=CARTESIAN_POINT('',(2.72072505953654,0.400193891020227,7.49482233047033));
#377935=CARTESIAN_POINT('Origin',(1.82427061521866E-15,2.94933925638659E-16,
7.49482233047033));
#377936=CARTESIAN_POINT('',(2.72342529733066,0.381385172574125,7.51860402984325));
#377937=CARTESIAN_POINT('Origin',(2.71934197027218,0.40945813990574,7.53030836256725));
#377938=CARTESIAN_POINT('',(2.72342529733066,0.38138517257413,8.75721825406948));
#377939=CARTESIAN_POINT('',(2.72342529733066,0.38138517257413,9.));
#377940=CARTESIAN_POINT('',(2.73109539723703,0.321897392332886,8.75721825406948));
#377941=CARTESIAN_POINT('Origin',(0.,1.84795814293585E-15,8.75721825406948));
#377942=CARTESIAN_POINT('',(2.73109539723703,0.321897392332886,7.51860402984325));
#377943=CARTESIAN_POINT('',(2.73109539723703,0.321897392332886,9.));
#377944=CARTESIAN_POINT('',(2.73325438874111,0.303018887905503,7.49482233047033));
#377945=CARTESIAN_POINT('Origin',(2.73426067017699,0.293759124467663,7.53025004711361));
#377946=CARTESIAN_POINT('',(2.74077554873748,0.225054196678923,7.49482233047033));
#377947=CARTESIAN_POINT('Origin',(1.83941893708273E-15,1.77446532635461E-16,
7.49482233047033));
#377948=CARTESIAN_POINT('',(2.74226515987506,0.206111117932626,7.51860402984325));
#377949=CARTESIAN_POINT('Origin',(2.7399888636424,0.234388026004939,7.53030836256727));
#377950=CARTESIAN_POINT('',(2.74226515987506,0.206111117932631,8.75721825406948));
#377951=CARTESIAN_POINT('',(2.74226515987506,0.206111117932631,9.));
#377952=CARTESIAN_POINT('',(2.74610810557233,0.146254136727663,8.75721825406948));
#377953=CARTESIAN_POINT('Origin',(0.,1.84795814293585E-15,8.75721825406948));
#377954=CARTESIAN_POINT('',(2.74610810557233,0.146254136727663,7.51860402984325));
#377955=CARTESIAN_POINT('',(2.74610810557233,0.146254136727663,9.));
#377956=CARTESIAN_POINT('',(2.74705311126524,0.127276093151736,7.49482233047033));
#377957=CARTESIAN_POINT('Origin',(2.74746405010757,0.117970882217837,7.53025004711382));
#377958=CARTESIAN_POINT('',(2.74956360331414,0.0489897063694902,7.49482233047033));
#377959=CARTESIAN_POINT('Origin',(1.8470086919802E-15,5.92299737675009E-17,
7.49482233047033));
#377960=CARTESIAN_POINT('',(2.74983646666349,0.029990108496846,7.51860402984325));
#377961=CARTESIAN_POINT('Origin',(2.74937655504614,0.0583547614292927,7.53030836256736));
#377962=CARTESIAN_POINT('',(2.74983646666349,0.0299901084968513,9.));
#377963=CARTESIAN_POINT('Origin',(0.,1.73472347597681E-15,8.75721825406948));
#377964=CARTESIAN_POINT('Origin',(2.69439583688069,0.0515030456391921,8.75693427654772));
#377965=CARTESIAN_POINT('Origin',(2.70228258044598,-0.048534448727824,8.76059769038453));
#377966=CARTESIAN_POINT('Origin',(0.,1.73472347597681E-15,8.75721825406948));
#377967=CARTESIAN_POINT('Origin',(2.33073265030338,-1.36834646567043,8.76059769038508));
#377968=CARTESIAN_POINT('Origin',(2.37295093746503,-1.27731176222123,8.75693427654889));
#377969=CARTESIAN_POINT('Origin',(0.,1.73472347597681E-15,8.75721825406948));
#377970=CARTESIAN_POINT('Origin',(2.28623780967396,-1.42672287677799,8.75693427654736));
#377971=CARTESIAN_POINT('Origin',(2.23827365103721,-1.51486560472308,8.7605976903849));
#377972=CARTESIAN_POINT('Origin',(0.,1.73472347597681E-15,8.75721825406948));
#377973=CARTESIAN_POINT('Origin',(2.19013004033039,-1.57027128100825,8.75693427654829));
#377974=CARTESIAN_POINT('Origin',(2.13661710522947,-1.65515983606784,8.76059769038414));
#377975=CARTESIAN_POINT('Origin',(0.,1.73472347597681E-15,8.75721825406948));
#377976=CARTESIAN_POINT('Origin',(2.08502255686731,-1.70736710371899,8.7569342765475));
#377977=CARTESIAN_POINT('Origin',(2.02618074143668,-1.78865266061642,8.76059769038484));
#377978=CARTESIAN_POINT('Origin',(0.,1.73472347597681E-15,8.75721825406948));
#377979=CARTESIAN_POINT('Origin',(1.97134726848432,-1.83744698877564,8.75693427654859));
#377980=CARTESIAN_POINT('Origin',(1.90741836636063,-1.91479552771699,8.7605976903845));
#377981=CARTESIAN_POINT('Origin',(0.,1.73472347597681E-15,8.75721825406948));
#377982=CARTESIAN_POINT('Origin',(1.84957129132088,-1.95997641002114,8.75693427654833));
#377983=CARTESIAN_POINT('Origin',(1.78081800007942,-2.0330700892728,8.76059769038499));
#377984=CARTESIAN_POINT('Origin',(0.,1.73472347597681E-15,8.75721825406948));
#377985=CARTESIAN_POINT('Origin',(1.72019502899002,-2.07445186778525,8.75693427654845));
#377986=CARTESIAN_POINT('Origin',(1.64689987064802,-2.14299032973772,8.76059769038419));
#377987=CARTESIAN_POINT('Origin',(0.,1.73472347597681E-15,8.75721825406948));
#377988=CARTESIAN_POINT('Origin',(1.5837501163042,-2.18040295785566,8.7569342765484));
#377989=CARTESIAN_POINT('Origin',(1.50621427639336,-2.24410456327018,8.76059769038494));
#377990=CARTESIAN_POINT('Origin',(0.,1.73472347597681E-15,8.75721825406948));
#377991=CARTESIAN_POINT('Origin',(1.44079723467694,-2.27739430447603,8.75693427654785));
#377992=CARTESIAN_POINT('Origin',(1.35933932459287,-2.33599728979191,8.76059769038486));
#377993=CARTESIAN_POINT('Origin',(0.,1.73472347597681E-15,8.75721825406948));
#377994=CARTESIAN_POINT('Origin',(1.29192380816251,-2.36502734939956,8.75693427654725));
#377995=CARTESIAN_POINT('Origin',(1.20687855593063,-2.41829090238031,8.76059769038491));
#377996=CARTESIAN_POINT('Origin',(0.,1.73472347597681E-15,8.75721825406948));
#377997=CARTESIAN_POINT('Origin',(1.13774158960398,-2.44294198965256,8.75693427654866));
#377998=CARTESIAN_POINT('Origin',(1.04945846440645,-2.49064723892815,8.76059769038441));
#377999=CARTESIAN_POINT('Origin',(0.,1.73472347597681E-15,8.75721825406948));
#378000=CARTESIAN_POINT('Origin',(0.978884146808586,-2.51081805725596,8.75693427654816));
#378001=CARTESIAN_POINT('Origin',(0.887725922945771,-2.55276897173096,8.76059769038499));
#378002=CARTESIAN_POINT('Origin',(0.,1.73472347597681E-15,8.75721825406948));
#378003=CARTESIAN_POINT('Origin',(0.816004259084044,-2.56837663489457,8.75693427654807));
#378004=CARTESIAN_POINT('Origin',(0.722345525249748,-2.60440082926027,8.76059769038484));
#378005=CARTESIAN_POINT('Origin',(0.,1.73472347597681E-15,8.75721825406948));
#378006=CARTESIAN_POINT('Origin',(0.649771234826351,-2.61538120202673,8.75693427654868));
#378007=CARTESIAN_POINT('Origin',(0.553996854849101,-2.6453306451417,8.76059769038543));
#378008=CARTESIAN_POINT('Origin',(0.,1.73472347597681E-15,8.75721825406948));
#378009=CARTESIAN_POINT('Origin',(0.48086816118962,-2.65163860679976,8.75693427654827));
#378010=CARTESIAN_POINT('Origin',(0.383371692537345,-2.67539022997661,8.7605976903844));
#378011=CARTESIAN_POINT('Origin',(0.,1.73472347597681E-15,8.75721825406948));
#378012=CARTESIAN_POINT('Origin',(0.309989097132222,-2.67699985976484,8.75693427654861));
#378013=CARTESIAN_POINT('Origin',(0.211171173710696,-2.69445606249166,8.76059769038521));
#378014=CARTESIAN_POINT('Origin',(0.,1.73472347597681E-15,8.75721825406948));
#378015=CARTESIAN_POINT('Origin',(0.137836221382254,-2.69136074609111,8.75693427654883));
#378016=CARTESIAN_POINT('Origin',(0.0381029072335807,-2.70244979708389,
8.76059769038479));
#378017=CARTESIAN_POINT('Origin',(0.,1.73472347597681E-15,8.75721825406948));
#378018=CARTESIAN_POINT('Origin',(-0.0348830529663535,-2.69466225381449,
8.7569342765482));
#378019=CARTESIAN_POINT('Origin',(-0.135121932261307,-2.69933858578882,
8.76059769038532));
#378020=CARTESIAN_POINT('Origin',(0.,1.73472347597681E-15,8.75721825406948));
#378021=CARTESIAN_POINT('Origin',(-0.207458985368108,-2.68689081633459,
8.75693427654791));
#378022=CARTESIAN_POINT('Origin',(-0.307791526754287,-2.68513521323456,
8.76059769038443));
#378023=CARTESIAN_POINT('Origin',(0.,1.73472347597681E-15,8.75721825406948));
#378024=CARTESIAN_POINT('Origin',(-0.379182424297982,-2.66807836815224,
8.75693427654677));
#378025=CARTESIAN_POINT('Origin',(-0.479196339841415,-2.6598980441342,8.76059769038531));
#378026=CARTESIAN_POINT('Origin',(0.,1.73472347597681E-15,8.75721825406948));
#378027=CARTESIAN_POINT('Origin',(-0.549347721314731,-2.63830221365879,
8.75693427654778));
#378028=CARTESIAN_POINT('Origin',(-0.648632032381716,-2.62373078342031,
8.76059769038475));
#378029=CARTESIAN_POINT('Origin',(0.,1.73472347597681E-15,8.75721825406948));
#378030=CARTESIAN_POINT('Origin',(-0.717255630709442,-2.59768470945429,
8.7569342765482));
#378031=CARTESIAN_POINT('Origin',(-0.815402356769413,-2.57678205013184,
8.76059769038535));
#378032=CARTESIAN_POINT('Origin',(0.,1.73472347597681E-15,8.75721825406948));
#378033=CARTESIAN_POINT('Origin',(-0.882216182865111,-2.54639276157493,
8.75693427654775));
#378034=CARTESIAN_POINT('Origin',(-0.978822017970119,-2.51924476667895,
8.76059769038503));
#378035=CARTESIAN_POINT('Origin',(0.,1.73472347597681E-15,8.75721825406948));
#378036=CARTESIAN_POINT('Origin',(-1.04355151949371,-2.48463713964208,8.75693427654898));
#378037=CARTESIAN_POINT('Origin',(-1.1382194895422,-2.45135536610346,8.76059769038475));
#378038=CARTESIAN_POINT('Origin',(0.,1.73472347597681E-15,8.75721825406948));
#378039=CARTESIAN_POINT('Origin',(-1.20059867908435,-2.41267161074603,8.75693427654834));
#378040=CARTESIAN_POINT('Origin',(-1.29293977308454,-2.37339282051633,8.76059769038498));
#378041=CARTESIAN_POINT('Origin',(0.,1.73472347597681E-15,8.75721825406948));
#378042=CARTESIAN_POINT('Origin',(-1.35271232117534,-2.33079189668547,8.75693427654807));
#378043=CARTESIAN_POINT('Origin',(-1.44234708976418,-2.28567749473594,8.76059769038434));
#378044=CARTESIAN_POINT('Origin',(0.,1.73472347597681E-15,8.75721825406948));
#378045=CARTESIAN_POINT('Origin',(-1.49926737818264,-2.23933445876821,8.75693427654765));
#378046=CARTESIAN_POINT('Origin',(-1.58582749287008,-2.18856982985657,8.76059769038499));
#378047=CARTESIAN_POINT('Origin',(0.,1.73472347597681E-15,8.75721825406948));
#378048=CARTESIAN_POINT('Origin',(-1.63966162394198,-2.13867511522477,8.75693427654776));
#378049=CARTESIAN_POINT('Origin',(-1.72279139064872,-2.08246886209855,8.76059769038511));
#378050=CARTESIAN_POINT('Origin',(0.,1.73472347597681E-15,8.75721825406948));
#378051=CARTESIAN_POINT('Origin',(-1.77331814838098,-2.02922749688787,8.75693427654726));
#378052=CARTESIAN_POINT('Origin',(-1.85267596906511,-1.96781058309659,8.76059769038474));
#378053=CARTESIAN_POINT('Origin',(0.,1.73472347597681E-15,8.75721825406948));
#378054=CARTESIAN_POINT('Origin',(-1.8996877281768,-1.91144134750023,8.75693427654833));
#378055=CARTESIAN_POINT('Origin',(-1.97494750452723,-1.84506614831579,8.76059769038486));
#378056=CARTESIAN_POINT('Origin',(0.,1.73472347597681E-15,8.75721825406948));
#378057=CARTESIAN_POINT('Origin',(-2.01825108361109,-1.78580067561075,8.75693427654771));
#378058=CARTESIAN_POINT('Origin',(-2.08910355706906,-1.71473994096737,8.7605976903854));
#378059=CARTESIAN_POINT('Origin',(0.,1.73472347597681E-15,8.75721825406948));
#378060=CARTESIAN_POINT('Origin',(-2.12852101243237,-1.65282176569325,8.75693427654811));
#378061=CARTESIAN_POINT('Origin',(-2.19467503498269,-1.57736749938913,8.76059769038525));
#378062=CARTESIAN_POINT('Origin',(0.,1.73472347597681E-15,8.75721825406948));
#378063=CARTESIAN_POINT('Origin',(-2.23004439184663,-1.51305105661106,8.7569342765483));
#378064=CARTESIAN_POINT('Origin',(-2.29122812242046,-1.43351331641059,8.76059769038468));
#378065=CARTESIAN_POINT('Origin',(0.,1.73472347597681E-15,8.75721825406948));
#378066=CARTESIAN_POINT('Origin',(-2.3224040405107,-1.3670628961886,8.75693427654811));
#378067=CARTESIAN_POINT('Origin',(-2.37836606203847,-1.28376851973026,8.7605976903854));
#378068=CARTESIAN_POINT('Origin',(0.,1.73472347597681E-15,8.75721825406948));
#378069=CARTESIAN_POINT('Origin',(-2.40522043282081,-1.21545718109189,8.75693427654895));
#378070=CARTESIAN_POINT('Origin',(-2.45573078534923,-1.12874844283407,8.76059769038575));
#378071=CARTESIAN_POINT('Origin',(0.,1.73472347597681E-15,8.75721825406948));
#378072=CARTESIAN_POINT('Origin',(-2.47815325844863,-1.05885689172298,8.75693427654761));
#378073=CARTESIAN_POINT('Origin',(-2.52300438410804,-0.969090096468077,
8.76059769038488));
#378074=CARTESIAN_POINT('Origin',(0.,1.73472347597681E-15,8.75721825406948));
#378075=CARTESIAN_POINT('Origin',(-2.54090282078107,-0.897905532262054,
8.75693427654849));
#378076=CARTESIAN_POINT('Origin',(-2.57991041667112,-0.805449551027988,
8.76059769038477));
#378077=CARTESIAN_POINT('Origin',(0.,1.73472347597681E-15,8.75721825406948));
#378078=CARTESIAN_POINT('Origin',(-2.59321126839827,-0.733264486368949,
8.7569342765483));
#378079=CARTESIAN_POINT('Origin',(-2.62621504394276,-0.638499240614201,
8.76059769038464));
#378080=CARTESIAN_POINT('Origin',(0.,1.73472347597681E-15,8.75721825406948));
#378081=CARTESIAN_POINT('Origin',(-2.63486365466874,-0.565610299417181,
8.75693427654712));
#378082=CARTESIAN_POINT('Origin',(-2.66172799027955,-0.468925199864443,
8.76059769038529));
#378083=CARTESIAN_POINT('Origin',(0.,1.73472347597681E-15,8.75721825406948));
#378084=CARTESIAN_POINT('Origin',(-2.6656888210123,-0.395631898420887,8.75693427654828));
#378085=CARTESIAN_POINT('Origin',(-2.68630332536147,-0.297424244881892,
8.76059769038425));
#378086=CARTESIAN_POINT('Origin',(0.,1.73472347597681E-15,8.75721825406948));
#378087=CARTESIAN_POINT('Origin',(-2.68556010019945,-0.224027761091513,
8.75693427654866));
#378088=CARTESIAN_POINT('Origin',(-2.69984006387362,-0.124701109882257,
8.76059769038511));
#378089=CARTESIAN_POINT('Origin',(0.,1.73472347597681E-15,8.75721825406948));
#378090=CARTESIAN_POINT('Origin',(-2.69439583688284,-0.0515030456383384,
8.75693427654858));
#378091=CARTESIAN_POINT('Origin',(-2.70228258044652,0.048534448727637,8.7605976903847));
#378092=CARTESIAN_POINT('Origin',(0.,1.73472347597681E-15,8.75721825406948));
#378093=CARTESIAN_POINT('Origin',(-2.69215972312632,0.121233306876663,8.75693427654841));
#378094=CARTESIAN_POINT('Origin',(-2.69362083825953,0.221570568876651,8.76059769038467));
#378095=CARTESIAN_POINT('Origin',(0.,1.73472347597681E-15,8.75721825406948));
#378096=CARTESIAN_POINT('Origin',(-2.67886094759852,0.293471485727828,8.75693427654727));
#378097=CARTESIAN_POINT('Origin',(-2.6738904302698,0.39369620803106,8.76059769038531));
#378098=CARTESIAN_POINT('Origin',(0.,1.73472347597681E-15,8.75721825406948));
#378099=CARTESIAN_POINT('Origin',(-2.65455415782992,0.464503727298469,8.75693427654893));
#378100=CARTESIAN_POINT('Origin',(-2.64317243295172,0.564204065019785,8.7605976903849));
#378101=CARTESIAN_POINT('Origin',(0.,1.73472347597681E-15,8.75721825406948));
#378102=CARTESIAN_POINT('Origin',(-2.61933923562136,0.633627223414736,8.75693427654828));
#378103=CARTESIAN_POINT('Origin',(-2.60159307314893,0.732393486483691,8.76059769038488));
#378104=CARTESIAN_POINT('Origin',(0.,1.73472347597681E-15,8.75721825406948));
#378105=CARTESIAN_POINT('Origin',(-2.57336088664725,0.80014700935721,8.75693427654763));
#378106=CARTESIAN_POINT('Origin',(-2.54932320936855,0.897573346013709,8.76059769038477));
#378107=CARTESIAN_POINT('Origin',(0.,1.73472347597681E-15,8.75721825406948));
#378108=CARTESIAN_POINT('Origin',(-2.51680804580947,0.963378819610446,8.75693427654892));
#378109=CARTESIAN_POINT('Origin',(-2.486577629693,1.05906488413606,8.76059769038485));
#378110=CARTESIAN_POINT('Origin',(0.,1.73472347597681E-15,8.75721825406948));
#378111=CARTESIAN_POINT('Origin',(-2.44991310085432,1.12265189964667,8.7569342765483));
#378112=CARTESIAN_POINT('Origin',(-2.41361416916817,1.21620449748084,8.76059769038502));
#378113=CARTESIAN_POINT('Origin',(0.,1.73472347597681E-15,8.75721825406948));
#378114=CARTESIAN_POINT('Origin',(-2.37295093746513,1.27731176222139,8.75693427654888));
#378115=CARTESIAN_POINT('Origin',(-2.33073265030128,1.36834646567015,8.76059769038433));
#378116=CARTESIAN_POINT('Origin',(0.,1.73472347597681E-15,8.75721825406948));
#378117=CARTESIAN_POINT('Origin',(-2.28623780967662,1.42672287678172,8.75693427654898));
#378118=CARTESIAN_POINT('Origin',(-2.23827365103789,1.51486560472324,8.76059769038512));
#378119=CARTESIAN_POINT('Origin',(0.,1.73472347597681E-15,8.75721825406948));
#378120=CARTESIAN_POINT('Origin',(-2.19013004032998,1.57027128100764,8.75693427654791));
#378121=CARTESIAN_POINT('Origin',(-2.13661710523201,1.65515983606856,8.76059769038523));
#378122=CARTESIAN_POINT('Origin',(0.,1.73472347597681E-15,8.75721825406948));
#378123=CARTESIAN_POINT('Origin',(-2.08502255686687,1.70736710371821,8.75693427654714));
#378124=CARTESIAN_POINT('Origin',(-2.02618074143595,1.78865266061619,8.76059769038451));
#378125=CARTESIAN_POINT('Origin',(0.,1.73472347597681E-15,8.75721825406948));
#378126=CARTESIAN_POINT('Origin',(-1.97134726848383,1.83744698877462,8.75693427654807));
#378127=CARTESIAN_POINT('Origin',(-1.90741836636232,1.91479552771773,8.76059769038511));
#378128=CARTESIAN_POINT('Origin',(0.,1.73472347597681E-15,8.75721825406948));
#378129=CARTESIAN_POINT('Origin',(-1.84957129132086,1.95997641002116,8.75693427654829));
#378130=CARTESIAN_POINT('Origin',(-1.78081800007809,2.03307008927213,8.76059769038453));
#378131=CARTESIAN_POINT('Origin',(0.,1.73472347597681E-15,8.75721825406948));
#378132=CARTESIAN_POINT('Origin',(-1.72019502898981,2.07445186778464,8.75693427654814));
#378133=CARTESIAN_POINT('Origin',(-1.64689987064938,2.14299032973853,8.76059769038468));
#378134=CARTESIAN_POINT('Origin',(0.,1.73472347597681E-15,8.75721825406948));
#378135=CARTESIAN_POINT('Origin',(-1.58375011630461,2.18040295785744,8.75693427654917));
#378136=CARTESIAN_POINT('Origin',(-1.50621427639386,2.24410456327052,8.76059769038516));
#378137=CARTESIAN_POINT('Origin',(0.,1.73472347597681E-15,8.75721825406948));
#378138=CARTESIAN_POINT('Origin',(-1.44079723467693,2.2773943044761,8.75693427654786));
#378139=CARTESIAN_POINT('Origin',(-1.35933932459167,2.33599728979102,8.7605976903843));
#378140=CARTESIAN_POINT('Origin',(0.,1.73472347597681E-15,8.75721825406948));
#378141=CARTESIAN_POINT('Origin',(-1.29192380816264,2.36502734940097,8.75693427654784));
#378142=CARTESIAN_POINT('Origin',(-1.20687855592903,2.41829090237895,8.76059769038412));
#378143=CARTESIAN_POINT('Origin',(0.,1.73472347597681E-15,8.75721825406948));
#378144=CARTESIAN_POINT('Origin',(-1.13774158960372,2.44294198964755,8.75693427654679));
#378145=CARTESIAN_POINT('Origin',(-1.04945846440719,2.49064723892892,8.7605976903849));
#378146=CARTESIAN_POINT('Origin',(0.,1.73472347597681E-15,8.75721825406948));
#378147=CARTESIAN_POINT('Origin',(-0.978884146808645,2.51081805725174,8.75693427654652));
#378148=CARTESIAN_POINT('Origin',(-0.887725922945521,2.55276897173071,8.76059769038493));
#378149=CARTESIAN_POINT('Origin',(0.,1.73472347597681E-15,8.75721825406948));
#378150=CARTESIAN_POINT('Origin',(-0.816004259084113,2.56837663489343,8.75693427654765));
#378151=CARTESIAN_POINT('Origin',(-0.722345525249641,2.60440082926018,8.76059769038479));
#378152=CARTESIAN_POINT('Origin',(0.,1.73472347597681E-15,8.75721825406948));
#378153=CARTESIAN_POINT('Origin',(-0.649771234826602,2.61538120202488,8.75693427654794));
#378154=CARTESIAN_POINT('Origin',(-0.55399685484881,2.64533064514131,8.76059769038531));
#378155=CARTESIAN_POINT('Origin',(0.,1.73472347597681E-15,8.75721825406948));
#378156=CARTESIAN_POINT('Origin',(-0.480868161189849,2.6516386067986,8.75693427654777));
#378157=CARTESIAN_POINT('Origin',(-0.383371692537824,2.67539022997746,8.76059769038473));
#378158=CARTESIAN_POINT('Origin',(0.,1.73472347597681E-15,8.75721825406948));
#378159=CARTESIAN_POINT('Origin',(2.4136141691684,-1.21620449748085,8.76059769038497));
#378160=CARTESIAN_POINT('Origin',(2.44991310085381,-1.1226518996461,8.75693427654797));
#378161=CARTESIAN_POINT('Origin',(0.,1.73472347597681E-15,8.75721825406948));
#378162=CARTESIAN_POINT('Origin',(2.48657762969223,-1.05906488413604,8.76059769038456));
#378163=CARTESIAN_POINT('Origin',(2.51680804580673,-0.96337881960785,8.75693427654744));
#378164=CARTESIAN_POINT('Origin',(0.,1.73472347597681E-15,8.75721825406948));
#378165=CARTESIAN_POINT('Origin',(2.5493232093696,-0.89757334601363,8.76059769038528));
#378166=CARTESIAN_POINT('Origin',(2.5733608866487,-0.800147009358387,8.75693427654833));
#378167=CARTESIAN_POINT('Origin',(0.,1.73472347597681E-15,8.75721825406948));
#378168=CARTESIAN_POINT('Origin',(2.60159307314759,-0.732393486483826,8.76059769038438));
#378169=CARTESIAN_POINT('Origin',(2.61933923561983,-0.633627223413621,8.75693427654751));
#378170=CARTESIAN_POINT('Origin',(0.,1.73472347597681E-15,8.75721825406948));
#378171=CARTESIAN_POINT('Origin',(2.64317243294954,-0.564204065020162,8.76059769038412));
#378172=CARTESIAN_POINT('Origin',(2.65455415782731,-0.464503727296811,8.75693427654779));
#378173=CARTESIAN_POINT('Origin',(0.,1.73472347597681E-15,8.75721825406948));
#378174=CARTESIAN_POINT('Origin',(2.67389043026933,-0.393696208031149,8.76059769038518));
#378175=CARTESIAN_POINT('Origin',(2.6788609475996,-0.293471485728388,8.75693427654779));
#378176=CARTESIAN_POINT('Origin',(0.,1.73472347597681E-15,8.75721825406948));
#378177=CARTESIAN_POINT('Origin',(2.69362083826087,-0.221570568876215,8.76059769038522));
#378178=CARTESIAN_POINT('Origin',(2.69215972312383,-0.121233306875485,8.75693427654745));
#378179=CARTESIAN_POINT('Origin',(0.,1.73472347597681E-15,8.75721825406948));
#378180=CARTESIAN_POINT('Origin',(2.69984006387324,0.124701109882108,8.76059769038496));
#378181=CARTESIAN_POINT('Origin',(2.68556010019784,0.224027761092042,8.75693427654803));
#378182=CARTESIAN_POINT('Origin',(0.,1.73472347597681E-15,8.75721825406948));
#378183=CARTESIAN_POINT('Origin',(2.6863033253636,0.297424244883076,8.76059769038514));
#378184=CARTESIAN_POINT('Origin',(2.66568882101331,0.39563189842066,8.75693427654874));
#378185=CARTESIAN_POINT('Origin',(0.,1.73472347597681E-15,8.75721825406948));
#378186=CARTESIAN_POINT('Origin',(2.66172799027848,0.468925199863798,8.76059769038476));
#378187=CARTESIAN_POINT('Origin',(2.63486365467144,0.565610299416714,8.75693427654806));
#378188=CARTESIAN_POINT('Origin',(0.,1.73472347597681E-15,8.75721825406948));
#378189=CARTESIAN_POINT('Origin',(2.62621504394336,0.638499240614644,8.76059769038486));
#378190=CARTESIAN_POINT('Origin',(2.59321126839706,0.733264486369107,8.7569342765479));
#378191=CARTESIAN_POINT('Origin',(0.,1.73472347597681E-15,8.75721825406948));
#378192=CARTESIAN_POINT('Origin',(2.57991041667163,0.805449551028446,8.76059769038508));
#378193=CARTESIAN_POINT('Origin',(2.54090282077683,0.897905532262281,8.75693427654695));
#378194=CARTESIAN_POINT('Origin',(0.,1.73472347597681E-15,8.75721825406948));
#378195=CARTESIAN_POINT('Origin',(2.52300438410802,0.969090096468083,8.76059769038486));
#378196=CARTESIAN_POINT('Origin',(2.4781532584484,1.05885689172299,8.75693427654758));
#378197=CARTESIAN_POINT('Origin',(0.,1.73472347597681E-15,8.75721825406948));
#378198=CARTESIAN_POINT('Origin',(2.4557307853478,1.12874844283258,8.760597690385));
#378199=CARTESIAN_POINT('Origin',(2.40522043281718,1.21545718109162,8.75693427654765));
#378200=CARTESIAN_POINT('Origin',(0.,1.73472347597681E-15,8.75721825406948));
#378201=CARTESIAN_POINT('Origin',(2.37836606203801,1.28376851972975,8.7605976903851));
#378202=CARTESIAN_POINT('Origin',(2.32240404051429,1.36706289618913,8.75693427654954));
#378203=CARTESIAN_POINT('Origin',(0.,1.73472347597681E-15,8.75721825406948));
#378204=CARTESIAN_POINT('Origin',(2.29122812242146,1.433513316412,8.76059769038528));
#378205=CARTESIAN_POINT('Origin',(2.23004439184453,1.51305105661064,8.75693427654751));
#378206=CARTESIAN_POINT('Origin',(0.,1.73472347597681E-15,8.75721825406948));
#378207=CARTESIAN_POINT('Origin',(2.19467503498184,1.57736749938779,8.76059769038468));
#378208=CARTESIAN_POINT('Origin',(2.12852101243191,1.65282176569313,8.75693427654792));
#378209=CARTESIAN_POINT('Origin',(0.,1.73472347597681E-15,8.75721825406948));
#378210=CARTESIAN_POINT('Origin',(2.08910355706757,1.71473994096463,8.76059769038429));
#378211=CARTESIAN_POINT('Origin',(2.01825108361135,1.78580067561086,8.75693427654768));
#378212=CARTESIAN_POINT('Origin',(0.,1.73472347597681E-15,8.75721825406948));
#378213=CARTESIAN_POINT('Origin',(1.9749475045275,1.8450661483164,8.76059769038504));
#378214=CARTESIAN_POINT('Origin',(1.899687728176,1.9114413474999,8.75693427654803));
#378215=CARTESIAN_POINT('Origin',(0.,1.73472347597681E-15,8.75721825406948));
#378216=CARTESIAN_POINT('Origin',(1.85267596906484,1.96781058309591,8.76059769038447));
#378217=CARTESIAN_POINT('Origin',(1.77331814838245,2.02922749688863,8.75693427654777));
#378218=CARTESIAN_POINT('Origin',(0.,1.73472347597681E-15,8.75721825406948));
#378219=CARTESIAN_POINT('Origin',(1.72279139064826,2.08246886209715,8.76059769038466));
#378220=CARTESIAN_POINT('Origin',(1.63966162394417,2.13867511522607,8.75693427654865));
#378221=CARTESIAN_POINT('Origin',(0.,1.73472347597681E-15,8.75721825406948));
#378222=CARTESIAN_POINT('Origin',(1.58582749286989,2.18856982985588,8.76059769038467));
#378223=CARTESIAN_POINT('Origin',(1.49926737818233,2.23933445876803,8.75693427654753));
#378224=CARTESIAN_POINT('Origin',(0.,1.73472347597681E-15,8.75721825406948));
#378225=CARTESIAN_POINT('Origin',(1.44234708976436,2.285677494737,8.7605976903848));
#378226=CARTESIAN_POINT('Origin',(1.35271232117604,2.33079189668602,8.75693427654834));
#378227=CARTESIAN_POINT('Origin',(0.,1.73472347597681E-15,8.75721825406948));
#378228=CARTESIAN_POINT('Origin',(1.29293977308441,2.37339282051545,8.76059769038473));
#378229=CARTESIAN_POINT('Origin',(1.20059867908477,2.41267161074641,8.75693427654861));
#378230=CARTESIAN_POINT('Origin',(0.,1.73472347597681E-15,8.75721825406948));
#378231=CARTESIAN_POINT('Origin',(1.13821948954226,2.45135536610491,8.76059769038536));
#378232=CARTESIAN_POINT('Origin',(1.04355151949228,2.48463713964067,8.75693427654822));
#378233=CARTESIAN_POINT('Origin',(0.,1.73472347597681E-15,8.75721825406948));
#378234=CARTESIAN_POINT('Origin',(0.978822017970095,2.51924476667868,8.76059769038497));
#378235=CARTESIAN_POINT('Origin',(0.882216182867039,2.54639276157716,8.75693427654885));
#378236=CARTESIAN_POINT('Origin',(0.,1.73472347597681E-15,8.75721825406948));
#378237=CARTESIAN_POINT('Origin',(0.815402356769505,2.57678205013041,8.7605976903849));
#378238=CARTESIAN_POINT('Origin',(0.717255630708937,2.59768470945367,8.75693427654799));
#378239=CARTESIAN_POINT('Origin',(0.,1.73472347597681E-15,8.75721825406948));
#378240=CARTESIAN_POINT('Origin',(0.648632032381852,2.6237307834193,8.76059769038445));
#378241=CARTESIAN_POINT('Origin',(0.549347721316237,2.63830221366104,8.75693427654871));
#378242=CARTESIAN_POINT('Origin',(0.,1.73472347597681E-15,8.75721825406948));
#378243=CARTESIAN_POINT('Origin',(0.479196339841701,2.65989804413279,8.76059769038473));
#378244=CARTESIAN_POINT('Origin',(0.379182424298648,2.66807836815341,8.75693427654746));
#378245=CARTESIAN_POINT('Origin',(0.,1.73472347597681E-15,8.75721825406948));
#378246=CARTESIAN_POINT('Origin',(0.30779152675381,2.6851352132362,8.76059769038509));
#378247=CARTESIAN_POINT('Origin',(0.207458985368901,2.68689081633622,8.75693427654862));
#378248=CARTESIAN_POINT('Origin',(0.,1.73472347597681E-15,8.75721825406948));
#378249=CARTESIAN_POINT('Origin',(0.135121932261841,2.69933858578726,8.76059769038467));
#378250=CARTESIAN_POINT('Origin',(0.0348830529663535,2.69466225381449,8.7569342765482));
#378251=CARTESIAN_POINT('Origin',(0.,1.73472347597681E-15,8.75721825406948));
#378252=CARTESIAN_POINT('Origin',(-0.30998909713224,2.67699985976471,8.75693427654847));
#378253=CARTESIAN_POINT('Origin',(-0.211171173710815,2.69445606249195,8.76059769038534));
#378254=CARTESIAN_POINT('Origin',(0.,2.67103869055211,7.5));
#378255=CARTESIAN_POINT('',(-0.00603856833113048,2.66775215476039,7.59394543036555));
#378256=CARTESIAN_POINT('',(-0.00603856833113048,2.66775215476039,8.85049129520029));
#378257=CARTESIAN_POINT('',(-0.00603856833113048,2.66775215476039,7.5));
#378258=CARTESIAN_POINT('',(0.00603856833113048,2.66775215476039,8.85049129520029));
#378259=CARTESIAN_POINT('Ctrl Pts',(-0.0060385683311304,2.66775215476039,
8.85049129520029));
#378260=CARTESIAN_POINT('Ctrl Pts',(-0.0059459900808512,2.66758205465325,
8.85097269580139));
#378261=CARTESIAN_POINT('Ctrl Pts',(-0.00584719181995321,2.66741812167859,
8.85143669361005));
#378262=CARTESIAN_POINT('Ctrl Pts',(-0.00573687539919907,2.6672532585408,
8.8519052845931));
#378263=CARTESIAN_POINT('Ctrl Pts',(-0.00552110347621796,2.66693079669851,
8.85282181883899));
#378264=CARTESIAN_POINT('Ctrl Pts',(-0.00526665369920735,2.66661318098465,
8.85372622499635));
#378265=CARTESIAN_POINT('Ctrl Pts',(-0.00495749990689061,2.66630506772301,
8.8546225773507));
#378266=CARTESIAN_POINT('Ctrl Pts',(-0.00470085140861172,2.66604928303633,
8.85536669723986));
#378267=CARTESIAN_POINT('Ctrl Pts',(-0.00440646616566121,2.66579996647417,
8.85610498449051));
#378268=CARTESIAN_POINT('Ctrl Pts',(-0.00405997820836668,2.66556586768779,
8.85681338218371));
#378269=CARTESIAN_POINT('Ctrl Pts',(-0.00374553984295258,2.66535342267149,
8.85745625420284));
#378270=CARTESIAN_POINT('Ctrl Pts',(-0.00338458256238873,2.66515034957616,
8.85808743050666));
#378271=CARTESIAN_POINT('Ctrl Pts',(-0.00295369827383558,2.66497307725867,
8.85866804508411));
#378272=CARTESIAN_POINT('Ctrl Pts',(-0.00275489760352519,2.66489128765418,
8.85893592806396));
#378273=CARTESIAN_POINT('Ctrl Pts',(-0.00254103122291519,2.6648151521707,
8.85919241173849));
#378274=CARTESIAN_POINT('Ctrl Pts',(-0.00230877295597377,2.66474750603832,
8.85943017985535));
#378275=CARTESIAN_POINT('Ctrl Pts',(-0.00199515553979517,2.66465616373421,
8.85975123720001));
#378276=CARTESIAN_POINT('Ctrl Pts',(-0.00163984270799643,2.66457859015688,
8.86004599534706));
#378277=CARTESIAN_POINT('Ctrl Pts',(-0.00124488186767327,2.66452589273075,
8.86026130871721));
#378278=CARTESIAN_POINT('Ctrl Pts',(-0.00110027556890578,2.66450659871735,
8.86034014101236));
#378279=CARTESIAN_POINT('Ctrl Pts',(-0.000948183946098822,2.66449033731455,
8.86040910639693));
#378280=CARTESIAN_POINT('Ctrl Pts',(-0.000792714888868764,2.6644778860275,
8.86046313645507));
#378281=CARTESIAN_POINT('Ctrl Pts',(-0.000550106727103745,2.66445845589833,
8.8605474499083));
#378282=CARTESIAN_POINT('Ctrl Pts',(-0.000292639848427733,2.66444792009911,
8.86059655985668));
#378283=CARTESIAN_POINT('Ctrl Pts',(-3.68383656842663E-5,2.66444666161026,
8.86059725258816));
#378284=CARTESIAN_POINT('Ctrl Pts',(0.000219554120677806,2.6644454002138,
8.86059794692011));
#378285=CARTESIAN_POINT('Ctrl Pts',(0.000477129998147651,2.66445610179498,
8.86056369958366));
#378286=CARTESIAN_POINT('Ctrl Pts',(0.000721997165140026,2.66447442282945,
8.86048590497774));
#378287=CARTESIAN_POINT('Ctrl Pts',(0.000785900205151045,2.66447920407396,
8.86046560290182));
#378288=CARTESIAN_POINT('Ctrl Pts',(0.000849762296446932,2.66448465677257,
8.86044257503091));
#378289=CARTESIAN_POINT('Ctrl Pts',(0.000911612840154663,2.66449057972519,
8.86041778462583));
#378290=CARTESIAN_POINT('Ctrl Pts',(0.00132779024918037,2.66453043384658,
8.860250975962));
#378291=CARTESIAN_POINT('Ctrl Pts',(0.0017087062830535,2.6645972575501,
8.8599848982295));
#378292=CARTESIAN_POINT('Ctrl Pts',(0.00204470696718254,2.6646807553764,
8.85968173251462));
#378293=CARTESIAN_POINT('Ctrl Pts',(0.00222243207854282,2.66472492094265,
8.85952137522077));
#378294=CARTESIAN_POINT('Ctrl Pts',(0.00239106259016765,2.6647744176014,
8.85934740853961));
#378295=CARTESIAN_POINT('Ctrl Pts',(0.00254865826271333,2.66482705571598,
8.8591675900182));
#378296=CARTESIAN_POINT('Ctrl Pts',(0.00318148680458622,2.66503842510675,
8.85844552518695));
#378297=CARTESIAN_POINT('Ctrl Pts',(0.00367310982058979,2.665309524653,
8.85759444184124));
#378298=CARTESIAN_POINT('Ctrl Pts',(0.0040540988240094,2.66556656868577,
8.85683498915139));
#378299=CARTESIAN_POINT('Ctrl Pts',(0.00409396830856038,2.66559346765924,
8.85675551444998));
#378300=CARTESIAN_POINT('Ctrl Pts',(0.00413261203991475,2.66562022675649,
8.85667699793651));
#378301=CARTESIAN_POINT('Ctrl Pts',(0.00417005525354386,2.66564677016415,
8.85659965593547));
#378302=CARTESIAN_POINT('Ctrl Pts',(0.00467546566173685,2.66600505443517,
8.85555568965886));
#378303=CARTESIAN_POINT('Ctrl Pts',(0.00510945303863149,2.66642237908077,
8.85434650606346));
#378304=CARTESIAN_POINT('Ctrl Pts',(0.00547847041769397,2.6668963274801,
8.85297329937117));
#378305=CARTESIAN_POINT('Ctrl Pts',(0.00568602020885762,2.66716289457662,
8.85220095427747));
#378306=CARTESIAN_POINT('Ctrl Pts',(0.00587285370781608,2.66744767638566,
8.85137579139183));
#378307=CARTESIAN_POINT('Ctrl Pts',(0.00603856833113047,2.66775215476039,
8.85049129520029));
#378308=CARTESIAN_POINT('',(0.00603856833113048,2.66775215476039,7.59394543036555));
#378309=CARTESIAN_POINT('',(0.00603856833113048,2.66775215476039,7.5));
#378310=CARTESIAN_POINT('Origin',(2.28698895758661E-17,2.67103869055211,
7.59394543036555));
#378311=CARTESIAN_POINT('Origin',(-0.1375,2.90929488800561,7.5));
#378312=CARTESIAN_POINT('',(-0.0469183093502055,2.74286319116668,8.75721825406948));
#378313=CARTESIAN_POINT('',(-0.0402149326548299,2.73054663635347,8.78727029226991));
#378314=CARTESIAN_POINT('Origin',(-0.0231992623667671,2.69928262639098,
8.75658640621021));
#378315=CARTESIAN_POINT('Ctrl Pts',(-0.04021493265483,2.73054663635347,
8.78727029226991));
#378316=CARTESIAN_POINT('Ctrl Pts',(-0.0288389699333486,2.7096448319675,
8.80838212259896));
#378317=CARTESIAN_POINT('Ctrl Pts',(-0.017447249324145,2.68871407457819,
8.82945686509571));
#378318=CARTESIAN_POINT('Ctrl Pts',(-0.00603856833113064,2.66775215476039,
8.85049129520029));
#378319=CARTESIAN_POINT('',(-0.0469183093502055,2.74286319116668,7.51860402984325));
#378320=CARTESIAN_POINT('Ctrl Pts',(-0.00603856833112958,2.66775215476039,
7.59394543036555));
#378321=CARTESIAN_POINT('Ctrl Pts',(-0.0144064330001523,2.68312698278351,
7.57858609112103));
#378322=CARTESIAN_POINT('Ctrl Pts',(-0.022764934078714,2.69848460646616,
7.56320440326857));
#378323=CARTESIAN_POINT('Ctrl Pts',(-0.031114562299379,2.71382592746348,
7.54780169004651));
#378324=CARTESIAN_POINT('Ctrl Pts',(-0.0363859720948704,2.72351143532608,
7.53807742314383));
#378325=CARTESIAN_POINT('Ctrl Pts',(-0.0416538495282657,2.73319045294751,
7.52834476460825));
#378326=CARTESIAN_POINT('Ctrl Pts',(-0.0469183093502052,2.74286319116668,
7.51860402984325));
#378327=CARTESIAN_POINT('',(-0.0469183093502055,2.74286319116668,7.5));
#378328=CARTESIAN_POINT('Origin',(0.00603856833113048,2.66775215476039,
7.5));
#378329=CARTESIAN_POINT('',(0.0402149326548299,2.73054663635347,8.78727029226991));
#378330=CARTESIAN_POINT('Ctrl Pts',(0.00603856833113057,2.66775215476039,
8.85049129520029));
#378331=CARTESIAN_POINT('Ctrl Pts',(0.0174472493241456,2.68871407457819,
8.82945686509571));
#378332=CARTESIAN_POINT('Ctrl Pts',(0.0288389699333437,2.70964483196749,
8.80838212259895));
#378333=CARTESIAN_POINT('Ctrl Pts',(0.0402149326548299,2.73054663635347,
8.78727029226991));
#378334=CARTESIAN_POINT('',(0.0469183093502055,2.74286319116668,8.75721825406948));
#378335=CARTESIAN_POINT('Origin',(0.0267453462054665,2.70579850156065,8.75937679713102));
#378336=CARTESIAN_POINT('',(0.0469183093502055,2.74286319116668,7.51860402984325));
#378337=CARTESIAN_POINT('',(0.0469183093502055,2.74286319116668,7.5));
#378338=CARTESIAN_POINT('Ctrl Pts',(0.0469183093502053,2.74286319116668,
7.51860402984325));
#378339=CARTESIAN_POINT('Ctrl Pts',(0.041653849528267,2.73319045294751,
7.52834476460825));
#378340=CARTESIAN_POINT('Ctrl Pts',(0.0363859720949718,2.72351143532627,
7.53807742314407));
#378341=CARTESIAN_POINT('Ctrl Pts',(0.0311145622994817,2.71382592746367,
7.54780169004674));
#378342=CARTESIAN_POINT('Ctrl Pts',(0.0227649340788154,2.69848460646635,
7.5632044032688));
#378343=CARTESIAN_POINT('Ctrl Pts',(0.0144064330001542,2.68312698278351,
7.57858609112103));
#378344=CARTESIAN_POINT('Ctrl Pts',(0.00603856833113041,2.66775215476039,
7.59394543036555));
#378345=CARTESIAN_POINT('Origin',(0.,1.25,7.5));
#378346=CARTESIAN_POINT('',(-1.25,0.721687836487033,7.5));
#378347=CARTESIAN_POINT('',(-1.25,0.721687836487033,7.5));
#378348=CARTESIAN_POINT('',(0.,1.44337567297406,7.5));
#378349=CARTESIAN_POINT('Origin',(0.,1.25,7.5));
#378350=CARTESIAN_POINT('',(0.,1.44337567297406,7.5));
#378351=CARTESIAN_POINT('',(0.,1.44337567297406,7.5));
#378352=CARTESIAN_POINT('',(1.25,0.721687836487032,7.5));
#378353=CARTESIAN_POINT('Origin',(0.,1.25,7.5));
#378354=CARTESIAN_POINT('',(1.25,0.721687836487032,7.5));
#378355=CARTESIAN_POINT('',(1.25,0.721687836487032,7.5));
#378356=CARTESIAN_POINT('',(1.25,-0.721687836487032,7.5));
#378357=CARTESIAN_POINT('Origin',(0.,1.25,7.5));
#378358=CARTESIAN_POINT('',(1.25,-0.721687836487032,7.5));
#378359=CARTESIAN_POINT('',(1.25,-0.721687836487032,7.5));
#378360=CARTESIAN_POINT('',(-2.19962454627626E-16,-1.44337567297406,7.5));
#378361=CARTESIAN_POINT('Origin',(0.,1.25,7.5));
#378362=CARTESIAN_POINT('',(-2.19962454627626E-16,-1.44337567297406,7.5));
#378363=CARTESIAN_POINT('',(-2.19962454627626E-16,-1.44337567297406,7.5));
#378364=CARTESIAN_POINT('',(-1.25,-0.721687836487031,7.5));
#378365=CARTESIAN_POINT('Origin',(0.,2.50721825406948,9.));
#378366=CARTESIAN_POINT('',(-2.16840434497101E-16,1.44337567297406,9.));
#378367=CARTESIAN_POINT('',(-1.25,0.721687836487033,9.));
#378368=CARTESIAN_POINT('Origin',(0.,-7.70371977754894E-31,9.));
#378369=CARTESIAN_POINT('Origin',(0.,-7.70371977754894E-31,9.));
#378370=CARTESIAN_POINT('',(5.42101086242752E-16,-1.44337567297406,9.));
#378371=CARTESIAN_POINT('Origin',(0.,-7.70371977754894E-31,9.));
#378372=CARTESIAN_POINT('',(-1.25,-0.721687836487032,9.));
#378373=CARTESIAN_POINT('Origin',(0.,-7.70371977754894E-31,9.));
#378374=CARTESIAN_POINT('Origin',(0.,-7.70371977754894E-31,9.));
#378375=CARTESIAN_POINT('Origin',(0.,1.73472347597681E-15,8.75721825406948));
#378376=CARTESIAN_POINT('Origin',(-0.137836221382471,2.69136074609044,8.75693427654847));
#378377=CARTESIAN_POINT('Origin',(-0.0381029072335807,2.70244979708389,
8.76059769038479));
#378378=CARTESIAN_POINT('Origin',(1.25,0.721687836487032,7.5));
#378379=CARTESIAN_POINT('',(1.25,0.721687836487032,7.5));
#378380=CARTESIAN_POINT('Ctrl Pts',(2.83368599028168E-16,1.44337567297406,
9.));
#378381=CARTESIAN_POINT('Ctrl Pts',(0.624999999999998,1.08253175473055,
8.63915608175649));
#378382=CARTESIAN_POINT('Ctrl Pts',(1.25,0.721687836487034,9.));
#378383=CARTESIAN_POINT('',(0.,1.44337567297406,7.5));
#378384=CARTESIAN_POINT('Origin',(1.25,-0.721687836487032,7.5));
#378385=CARTESIAN_POINT('',(1.25,-0.721687836487032,7.5));
#378386=CARTESIAN_POINT('Origin',(-2.19962454627626E-16,-1.44337567297406,
7.5));
#378387=CARTESIAN_POINT('',(-2.19962454627626E-16,-1.44337567297406,7.5));
#378388=CARTESIAN_POINT('Ctrl Pts',(1.25,-0.721687836487033,9.));
#378389=CARTESIAN_POINT('Ctrl Pts',(0.625,-1.08253175473055,8.63915608175649));
#378390=CARTESIAN_POINT('Ctrl Pts',(3.68379178736618E-15,-1.44337567297406,
9.));
#378391=CARTESIAN_POINT('Origin',(-1.25,-0.721687836487031,7.5));
#378392=CARTESIAN_POINT('',(-1.25,-0.721687836487031,7.5));
#378393=CARTESIAN_POINT('',(-1.25,-0.721687836487031,7.5));
#378394=CARTESIAN_POINT('Ctrl Pts',(-7.04373374727159E-15,-1.44337567297406,
8.99999999999999));
#378395=CARTESIAN_POINT('Ctrl Pts',(-0.625000000000001,-1.08253175473055,
8.63915608175649));
#378396=CARTESIAN_POINT('Ctrl Pts',(-1.25,-0.721687836487034,9.));
#378397=CARTESIAN_POINT('',(-1.25,-0.721687836487031,7.5));
#378398=CARTESIAN_POINT('Origin',(-1.25,0.721687836487033,7.5));
#378399=CARTESIAN_POINT('',(-1.25,0.721687836487033,7.5));
#378400=CARTESIAN_POINT('Ctrl Pts',(-1.25,-0.721687836487028,9.));
#378401=CARTESIAN_POINT('Ctrl Pts',(-1.25,2.4980018054066E-16,8.63915608175649));
#378402=CARTESIAN_POINT('Ctrl Pts',(-1.25,0.721687836487029,9.));
#378403=CARTESIAN_POINT('',(-1.25,0.721687836487033,7.5));
#378404=CARTESIAN_POINT('Origin',(0.,1.44337567297406,7.5));
#378405=CARTESIAN_POINT('Ctrl Pts',(-1.24999999999999,0.721687836487037,
9.));
#378406=CARTESIAN_POINT('Ctrl Pts',(-0.624999999999999,1.08253175473055,
8.63915608175649));
#378407=CARTESIAN_POINT('Ctrl Pts',(-4.49341635601809E-15,1.44337567297406,
9.));
#378408=CARTESIAN_POINT('Origin',(0.,1.25,7.5));
#378409=CARTESIAN_POINT('Origin',(0.,-7.70371977754894E-31,9.));
#378410=CARTESIAN_POINT('Origin',(0.,-7.70371977754894E-31,9.));
#378411=CARTESIAN_POINT('Origin',(0.,-7.70371977754894E-31,9.));
#378412=CARTESIAN_POINT('Origin',(0.,-7.70371977754894E-31,9.));
#378413=CARTESIAN_POINT('Origin',(0.,-7.70371977754894E-31,9.));
#378414=CARTESIAN_POINT('Origin',(2.50721825406948,1.84795814293585E-15,
6.));
#378415=CARTESIAN_POINT('Origin',(0.,1.84795814293585E-15,-9.));
#378416=CARTESIAN_POINT('Origin',(6.93889390390723E-17,9.71445146547012E-16,
-9.21875));
#378417=CARTESIAN_POINT('Ctrl Pts',(-1.43925448419919E-16,-1.17524047358083,
5.));
#378418=CARTESIAN_POINT('Ctrl Pts',(0.678525403784437,-1.17524047358083,
5.04166666666667));
#378419=CARTESIAN_POINT('Ctrl Pts',(1.01778810567666,-0.587620236790417,
5.08333333333333));
#378420=CARTESIAN_POINT('Ctrl Pts',(1.35705080756888,2.7065942666714E-16,
5.125));
#378421=CARTESIAN_POINT('Ctrl Pts',(1.01778810567666,0.587620236790417,
5.16666666666667));
#378422=CARTESIAN_POINT('Ctrl Pts',(0.983895352085429,0.646324208018836,
5.1708292169807));
#378423=CARTESIAN_POINT('Ctrl Pts',(0.943477955795688,0.700742119235096,
5.17524047358083));
#378424=CARTESIAN_POINT('Ctrl Pts',(-1.43925448419919E-16,-1.17524047358083,
5.0625));
#378425=CARTESIAN_POINT('Ctrl Pts',(0.678525403784437,-1.17524047358083,
5.10416666666667));
#378426=CARTESIAN_POINT('Ctrl Pts',(1.01778810567666,-0.587620236790417,
5.14583333333333));
#378427=CARTESIAN_POINT('Ctrl Pts',(1.12956523348519,-0.394016572301912,
5.15956128014086));
#378428=CARTESIAN_POINT('Ctrl Pts',(1.16245326511946,-0.172894699616898,
5.17524047358083));
#378429=CARTESIAN_POINT('Ctrl Pts',(0.,1.17524047358083,-9.25));
#378430=CARTESIAN_POINT('Ctrl Pts',(-0.678525403784438,1.17524047358083,
-9.20833333333333));
#378431=CARTESIAN_POINT('Ctrl Pts',(-1.01778810567666,0.587620236790418,
-9.16666666666667));
#378432=CARTESIAN_POINT('Ctrl Pts',(-1.35705080756888,6.0304101222105E-16,
-9.125));
#378433=CARTESIAN_POINT('Ctrl Pts',(-1.01778810567666,-0.587620236790416,
-9.08333333333333));
#378434=CARTESIAN_POINT('Ctrl Pts',(-0.678525403784438,-1.17524047358083,
-9.04166666666667));
#378435=CARTESIAN_POINT('Ctrl Pts',(-1.43925448419919E-16,-1.17524047358083,
-9.));
#378436=CARTESIAN_POINT('Ctrl Pts',(0.678525403784437,-1.17524047358083,
-8.95833333333333));
#378437=CARTESIAN_POINT('Ctrl Pts',(1.01778810567666,-0.587620236790417,
-8.91666666666667));
#378438=CARTESIAN_POINT('Ctrl Pts',(1.35705080756888,2.70659426667139E-16,
-8.875));
#378439=CARTESIAN_POINT('Ctrl Pts',(1.01778810567666,0.587620236790417,
-8.83333333333333));
#378440=CARTESIAN_POINT('Ctrl Pts',(0.678525403784439,1.17524047358083,
-8.79166666666667));
#378441=CARTESIAN_POINT('Ctrl Pts',(0.,1.17524047358083,-8.75));
#378442=CARTESIAN_POINT('Ctrl Pts',(-0.678525403784438,1.17524047358083,
-8.70833333333333));
#378443=CARTESIAN_POINT('Ctrl Pts',(-1.01778810567666,0.587620236790418,
-8.66666666666667));
#378444=CARTESIAN_POINT('Ctrl Pts',(-1.35705080756888,6.0304101222105E-16,
-8.625));
#378445=CARTESIAN_POINT('Ctrl Pts',(-1.01778810567666,-0.587620236790416,
-8.58333333333333));
#378446=CARTESIAN_POINT('Ctrl Pts',(-0.678525403784438,-1.17524047358083,
-8.54166666666667));
#378447=CARTESIAN_POINT('Ctrl Pts',(-1.43925448419919E-16,-1.17524047358083,
-8.5));
#378448=CARTESIAN_POINT('Ctrl Pts',(0.678525403784437,-1.17524047358083,
-8.45833333333333));
#378449=CARTESIAN_POINT('Ctrl Pts',(1.01778810567666,-0.587620236790417,
-8.41666666666667));
#378450=CARTESIAN_POINT('Ctrl Pts',(1.35705080756888,2.70659426667139E-16,
-8.375));
#378451=CARTESIAN_POINT('Ctrl Pts',(1.01778810567666,0.587620236790417,
-8.33333333333334));
#378452=CARTESIAN_POINT('Ctrl Pts',(0.678525403784439,1.17524047358083,
-8.29166666666667));
#378453=CARTESIAN_POINT('Ctrl Pts',(0.,1.17524047358083,-8.25));
#378454=CARTESIAN_POINT('Ctrl Pts',(-0.678525403784438,1.17524047358083,
-8.20833333333333));
#378455=CARTESIAN_POINT('Ctrl Pts',(-1.01778810567666,0.587620236790418,
-8.16666666666667));
#378456=CARTESIAN_POINT('Ctrl Pts',(-1.35705080756888,6.0304101222105E-16,
-8.125));
#378457=CARTESIAN_POINT('Ctrl Pts',(-1.01778810567666,-0.587620236790416,
-8.08333333333333));
#378458=CARTESIAN_POINT('Ctrl Pts',(-0.678525403784438,-1.17524047358083,
-8.04166666666667));
#378459=CARTESIAN_POINT('Ctrl Pts',(-1.43925448419919E-16,-1.17524047358083,
-8.));
#378460=CARTESIAN_POINT('Ctrl Pts',(0.678525403784437,-1.17524047358083,
-7.95833333333333));
#378461=CARTESIAN_POINT('Ctrl Pts',(1.01778810567666,-0.587620236790417,
-7.91666666666667));
#378462=CARTESIAN_POINT('Ctrl Pts',(1.35705080756888,2.7065942666714E-16,
-7.875));
#378463=CARTESIAN_POINT('Ctrl Pts',(1.01778810567666,0.587620236790417,
-7.83333333333333));
#378464=CARTESIAN_POINT('Ctrl Pts',(0.678525403784439,1.17524047358083,
-7.79166666666667));
#378465=CARTESIAN_POINT('Ctrl Pts',(0.,1.17524047358083,-7.75));
#378466=CARTESIAN_POINT('Ctrl Pts',(-0.678525403784438,1.17524047358083,
-7.70833333333333));
#378467=CARTESIAN_POINT('Ctrl Pts',(-1.01778810567666,0.587620236790418,
-7.66666666666667));
#378468=CARTESIAN_POINT('Ctrl Pts',(-1.35705080756888,6.0304101222105E-16,
-7.625));
#378469=CARTESIAN_POINT('Ctrl Pts',(-1.01778810567666,-0.587620236790416,
-7.58333333333333));
#378470=CARTESIAN_POINT('Ctrl Pts',(-0.678525403784438,-1.17524047358083,
-7.54166666666667));
#378471=CARTESIAN_POINT('Ctrl Pts',(-1.43925448419919E-16,-1.17524047358083,
-7.5));
#378472=CARTESIAN_POINT('Ctrl Pts',(0.678525403784437,-1.17524047358083,
-7.45833333333333));
#378473=CARTESIAN_POINT('Ctrl Pts',(1.01778810567666,-0.587620236790417,
-7.41666666666667));
#378474=CARTESIAN_POINT('Ctrl Pts',(1.35705080756888,2.7065942666714E-16,
-7.375));
#378475=CARTESIAN_POINT('Ctrl Pts',(1.01778810567666,0.587620236790417,
-7.33333333333333));
#378476=CARTESIAN_POINT('Ctrl Pts',(0.678525403784439,1.17524047358083,
-7.29166666666667));
#378477=CARTESIAN_POINT('Ctrl Pts',(0.,1.17524047358083,-7.25));
#378478=CARTESIAN_POINT('Ctrl Pts',(-0.678525403784438,1.17524047358083,
-7.20833333333333));
#378479=CARTESIAN_POINT('Ctrl Pts',(-1.01778810567666,0.587620236790418,
-7.16666666666667));
#378480=CARTESIAN_POINT('Ctrl Pts',(-1.35705080756888,6.0304101222105E-16,
-7.125));
#378481=CARTESIAN_POINT('Ctrl Pts',(-1.01778810567666,-0.587620236790416,
-7.08333333333333));
#378482=CARTESIAN_POINT('Ctrl Pts',(-0.678525403784438,-1.17524047358083,
-7.04166666666667));
#378483=CARTESIAN_POINT('Ctrl Pts',(-1.43925448419919E-16,-1.17524047358083,
-7.));
#378484=CARTESIAN_POINT('Ctrl Pts',(0.678525403784437,-1.17524047358083,
-6.95833333333333));
#378485=CARTESIAN_POINT('Ctrl Pts',(1.01778810567666,-0.587620236790417,
-6.91666666666667));
#378486=CARTESIAN_POINT('Ctrl Pts',(1.35705080756888,2.7065942666714E-16,
-6.875));
#378487=CARTESIAN_POINT('Ctrl Pts',(1.01778810567666,0.587620236790417,
-6.83333333333333));
#378488=CARTESIAN_POINT('Ctrl Pts',(0.678525403784439,1.17524047358083,
-6.79166666666667));
#378489=CARTESIAN_POINT('Ctrl Pts',(0.,1.17524047358083,-6.75));
#378490=CARTESIAN_POINT('Ctrl Pts',(-0.678525403784438,1.17524047358083,
-6.70833333333333));
#378491=CARTESIAN_POINT('Ctrl Pts',(-1.01778810567666,0.587620236790418,
-6.66666666666667));
#378492=CARTESIAN_POINT('Ctrl Pts',(-1.35705080756888,6.0304101222105E-16,
-6.625));
#378493=CARTESIAN_POINT('Ctrl Pts',(-1.01778810567666,-0.587620236790416,
-6.58333333333333));
#378494=CARTESIAN_POINT('Ctrl Pts',(-0.678525403784438,-1.17524047358083,
-6.54166666666667));
#378495=CARTESIAN_POINT('Ctrl Pts',(-1.43925448419919E-16,-1.17524047358083,
-6.5));
#378496=CARTESIAN_POINT('Ctrl Pts',(0.678525403784437,-1.17524047358083,
-6.45833333333333));
#378497=CARTESIAN_POINT('Ctrl Pts',(1.01778810567666,-0.587620236790417,
-6.41666666666667));
#378498=CARTESIAN_POINT('Ctrl Pts',(1.35705080756888,2.7065942666714E-16,
-6.375));
#378499=CARTESIAN_POINT('Ctrl Pts',(1.01778810567666,0.587620236790417,
-6.33333333333333));
#378500=CARTESIAN_POINT('Ctrl Pts',(0.678525403784439,1.17524047358083,
-6.29166666666667));
#378501=CARTESIAN_POINT('Ctrl Pts',(0.,1.17524047358083,-6.25));
#378502=CARTESIAN_POINT('Ctrl Pts',(-0.678525403784438,1.17524047358083,
-6.20833333333333));
#378503=CARTESIAN_POINT('Ctrl Pts',(-1.01778810567666,0.587620236790418,
-6.16666666666667));
#378504=CARTESIAN_POINT('Ctrl Pts',(-1.35705080756888,6.0304101222105E-16,
-6.125));
#378505=CARTESIAN_POINT('Ctrl Pts',(-1.01778810567666,-0.587620236790416,
-6.08333333333333));
#378506=CARTESIAN_POINT('Ctrl Pts',(-0.678525403784438,-1.17524047358083,
-6.04166666666667));
#378507=CARTESIAN_POINT('Ctrl Pts',(-1.43925448419919E-16,-1.17524047358083,
-6.));
#378508=CARTESIAN_POINT('Ctrl Pts',(0.678525403784437,-1.17524047358083,
-5.95833333333333));
#378509=CARTESIAN_POINT('Ctrl Pts',(1.01778810567666,-0.587620236790417,
-5.91666666666667));
#378510=CARTESIAN_POINT('Ctrl Pts',(1.35705080756888,2.7065942666714E-16,
-5.875));
#378511=CARTESIAN_POINT('Ctrl Pts',(1.01778810567666,0.587620236790417,
-5.83333333333333));
#378512=CARTESIAN_POINT('Ctrl Pts',(0.678525403784439,1.17524047358083,
-5.79166666666667));
#378513=CARTESIAN_POINT('Ctrl Pts',(0.,1.17524047358083,-5.75));
#378514=CARTESIAN_POINT('Ctrl Pts',(-0.678525403784438,1.17524047358083,
-5.70833333333333));
#378515=CARTESIAN_POINT('Ctrl Pts',(-1.01778810567666,0.587620236790418,
-5.66666666666667));
#378516=CARTESIAN_POINT('Ctrl Pts',(-1.35705080756888,6.0304101222105E-16,
-5.625));
#378517=CARTESIAN_POINT('Ctrl Pts',(-1.01778810567666,-0.587620236790416,
-5.58333333333333));
#378518=CARTESIAN_POINT('Ctrl Pts',(-0.678525403784438,-1.17524047358083,
-5.54166666666667));
#378519=CARTESIAN_POINT('Ctrl Pts',(-1.43925448419919E-16,-1.17524047358083,
-5.5));
#378520=CARTESIAN_POINT('Ctrl Pts',(0.678525403784437,-1.17524047358083,
-5.45833333333333));
#378521=CARTESIAN_POINT('Ctrl Pts',(1.01778810567666,-0.587620236790417,
-5.41666666666667));
#378522=CARTESIAN_POINT('Ctrl Pts',(1.35705080756888,2.7065942666714E-16,
-5.375));
#378523=CARTESIAN_POINT('Ctrl Pts',(1.01778810567666,0.587620236790417,
-5.33333333333333));
#378524=CARTESIAN_POINT('Ctrl Pts',(0.678525403784439,1.17524047358083,
-5.29166666666667));
#378525=CARTESIAN_POINT('Ctrl Pts',(0.,1.17524047358083,-5.25));
#378526=CARTESIAN_POINT('Ctrl Pts',(-0.678525403784438,1.17524047358083,
-5.20833333333333));
#378527=CARTESIAN_POINT('Ctrl Pts',(-1.01778810567666,0.587620236790418,
-5.16666666666667));
#378528=CARTESIAN_POINT('Ctrl Pts',(-1.35705080756888,6.0304101222105E-16,
-5.125));
#378529=CARTESIAN_POINT('Ctrl Pts',(-1.01778810567666,-0.587620236790416,
-5.08333333333333));
#378530=CARTESIAN_POINT('Ctrl Pts',(-0.678525403784438,-1.17524047358083,
-5.04166666666667));
#378531=CARTESIAN_POINT('Ctrl Pts',(-1.43925448419919E-16,-1.17524047358083,
-5.));
#378532=CARTESIAN_POINT('Ctrl Pts',(0.678525403784437,-1.17524047358083,
-4.95833333333333));
#378533=CARTESIAN_POINT('Ctrl Pts',(1.01778810567666,-0.587620236790417,
-4.91666666666667));
#378534=CARTESIAN_POINT('Ctrl Pts',(1.35705080756888,2.7065942666714E-16,
-4.875));
#378535=CARTESIAN_POINT('Ctrl Pts',(1.01778810567666,0.587620236790417,
-4.83333333333333));
#378536=CARTESIAN_POINT('Ctrl Pts',(0.678525403784439,1.17524047358083,
-4.79166666666667));
#378537=CARTESIAN_POINT('Ctrl Pts',(0.,1.17524047358083,-4.75));
#378538=CARTESIAN_POINT('Ctrl Pts',(-0.678525403784438,1.17524047358083,
-4.70833333333333));
#378539=CARTESIAN_POINT('Ctrl Pts',(-1.01778810567666,0.587620236790418,
-4.66666666666667));
#378540=CARTESIAN_POINT('Ctrl Pts',(-1.35705080756888,6.03041012221051E-16,
-4.625));
#378541=CARTESIAN_POINT('Ctrl Pts',(-1.01778810567666,-0.587620236790416,
-4.58333333333333));
#378542=CARTESIAN_POINT('Ctrl Pts',(-0.678525403784438,-1.17524047358083,
-4.54166666666667));
#378543=CARTESIAN_POINT('Ctrl Pts',(-1.43925448419919E-16,-1.17524047358083,
-4.5));
#378544=CARTESIAN_POINT('Ctrl Pts',(0.678525403784437,-1.17524047358083,
-4.45833333333333));
#378545=CARTESIAN_POINT('Ctrl Pts',(1.01778810567666,-0.587620236790417,
-4.41666666666667));
#378546=CARTESIAN_POINT('Ctrl Pts',(1.35705080756888,2.7065942666714E-16,
-4.375));
#378547=CARTESIAN_POINT('Ctrl Pts',(1.01778810567666,0.587620236790417,
-4.33333333333333));
#378548=CARTESIAN_POINT('Ctrl Pts',(0.678525403784439,1.17524047358083,
-4.29166666666667));
#378549=CARTESIAN_POINT('Ctrl Pts',(0.,1.17524047358083,-4.25));
#378550=CARTESIAN_POINT('Ctrl Pts',(-0.678525403784438,1.17524047358083,
-4.20833333333333));
#378551=CARTESIAN_POINT('Ctrl Pts',(-1.01778810567666,0.587620236790418,
-4.16666666666667));
#378552=CARTESIAN_POINT('Ctrl Pts',(-1.35705080756888,6.03041012221051E-16,
-4.125));
#378553=CARTESIAN_POINT('Ctrl Pts',(-1.01778810567666,-0.587620236790416,
-4.08333333333333));
#378554=CARTESIAN_POINT('Ctrl Pts',(-0.678525403784438,-1.17524047358083,
-4.04166666666667));
#378555=CARTESIAN_POINT('Ctrl Pts',(-1.43925448419919E-16,-1.17524047358083,
-4.));
#378556=CARTESIAN_POINT('Ctrl Pts',(0.678525403784437,-1.17524047358083,
-3.95833333333333));
#378557=CARTESIAN_POINT('Ctrl Pts',(1.01778810567666,-0.587620236790417,
-3.91666666666667));
#378558=CARTESIAN_POINT('Ctrl Pts',(1.35705080756888,2.7065942666714E-16,
-3.875));
#378559=CARTESIAN_POINT('Ctrl Pts',(1.01778810567666,0.587620236790417,
-3.83333333333333));
#378560=CARTESIAN_POINT('Ctrl Pts',(0.678525403784439,1.17524047358083,
-3.79166666666667));
#378561=CARTESIAN_POINT('Ctrl Pts',(0.,1.17524047358083,-3.75));
#378562=CARTESIAN_POINT('Ctrl Pts',(-0.678525403784438,1.17524047358083,
-3.70833333333333));
#378563=CARTESIAN_POINT('Ctrl Pts',(-1.01778810567666,0.587620236790418,
-3.66666666666667));
#378564=CARTESIAN_POINT('Ctrl Pts',(-1.35705080756888,6.03041012221051E-16,
-3.625));
#378565=CARTESIAN_POINT('Ctrl Pts',(-1.01778810567666,-0.587620236790416,
-3.58333333333333));
#378566=CARTESIAN_POINT('Ctrl Pts',(-0.678525403784438,-1.17524047358083,
-3.54166666666667));
#378567=CARTESIAN_POINT('Ctrl Pts',(-1.43925448419919E-16,-1.17524047358083,
-3.5));
#378568=CARTESIAN_POINT('Ctrl Pts',(0.678525403784437,-1.17524047358083,
-3.45833333333333));
#378569=CARTESIAN_POINT('Ctrl Pts',(1.01778810567666,-0.587620236790417,
-3.41666666666667));
#378570=CARTESIAN_POINT('Ctrl Pts',(1.35705080756888,2.7065942666714E-16,
-3.375));
#378571=CARTESIAN_POINT('Ctrl Pts',(1.01778810567666,0.587620236790417,
-3.33333333333333));
#378572=CARTESIAN_POINT('Ctrl Pts',(0.678525403784439,1.17524047358083,
-3.29166666666667));
#378573=CARTESIAN_POINT('Ctrl Pts',(0.,1.17524047358083,-3.25));
#378574=CARTESIAN_POINT('Ctrl Pts',(-0.678525403784438,1.17524047358083,
-3.20833333333333));
#378575=CARTESIAN_POINT('Ctrl Pts',(-1.01778810567666,0.587620236790418,
-3.16666666666667));
#378576=CARTESIAN_POINT('Ctrl Pts',(-1.35705080756888,6.03041012221051E-16,
-3.125));
#378577=CARTESIAN_POINT('Ctrl Pts',(-1.01778810567666,-0.587620236790416,
-3.08333333333333));
#378578=CARTESIAN_POINT('Ctrl Pts',(-0.678525403784438,-1.17524047358083,
-3.04166666666667));
#378579=CARTESIAN_POINT('Ctrl Pts',(-1.43925448419919E-16,-1.17524047358083,
-3.));
#378580=CARTESIAN_POINT('Ctrl Pts',(0.678525403784437,-1.17524047358083,
-2.95833333333333));
#378581=CARTESIAN_POINT('Ctrl Pts',(1.01778810567666,-0.587620236790417,
-2.91666666666667));
#378582=CARTESIAN_POINT('Ctrl Pts',(1.35705080756888,2.7065942666714E-16,
-2.875));
#378583=CARTESIAN_POINT('Ctrl Pts',(1.01778810567666,0.587620236790417,
-2.83333333333333));
#378584=CARTESIAN_POINT('Ctrl Pts',(0.678525403784439,1.17524047358083,
-2.79166666666667));
#378585=CARTESIAN_POINT('Ctrl Pts',(0.,1.17524047358083,-2.75));
#378586=CARTESIAN_POINT('Ctrl Pts',(-0.678525403784438,1.17524047358083,
-2.70833333333333));
#378587=CARTESIAN_POINT('Ctrl Pts',(-1.01778810567666,0.587620236790418,
-2.66666666666667));
#378588=CARTESIAN_POINT('Ctrl Pts',(-1.35705080756888,6.03041012221051E-16,
-2.625));
#378589=CARTESIAN_POINT('Ctrl Pts',(-1.01778810567666,-0.587620236790416,
-2.58333333333333));
#378590=CARTESIAN_POINT('Ctrl Pts',(-0.678525403784438,-1.17524047358083,
-2.54166666666667));
#378591=CARTESIAN_POINT('Ctrl Pts',(-1.43925448419919E-16,-1.17524047358083,
-2.5));
#378592=CARTESIAN_POINT('Ctrl Pts',(0.678525403784437,-1.17524047358083,
-2.45833333333333));
#378593=CARTESIAN_POINT('Ctrl Pts',(1.01778810567666,-0.587620236790417,
-2.41666666666667));
#378594=CARTESIAN_POINT('Ctrl Pts',(1.35705080756888,2.7065942666714E-16,
-2.375));
#378595=CARTESIAN_POINT('Ctrl Pts',(1.01778810567666,0.587620236790417,
-2.33333333333333));
#378596=CARTESIAN_POINT('Ctrl Pts',(0.678525403784439,1.17524047358083,
-2.29166666666667));
#378597=CARTESIAN_POINT('Ctrl Pts',(0.,1.17524047358083,-2.25));
#378598=CARTESIAN_POINT('Ctrl Pts',(-0.678525403784438,1.17524047358083,
-2.20833333333333));
#378599=CARTESIAN_POINT('Ctrl Pts',(-1.01778810567666,0.587620236790418,
-2.16666666666667));
#378600=CARTESIAN_POINT('Ctrl Pts',(-1.35705080756888,6.03041012221051E-16,
-2.125));
#378601=CARTESIAN_POINT('Ctrl Pts',(-1.01778810567666,-0.587620236790416,
-2.08333333333333));
#378602=CARTESIAN_POINT('Ctrl Pts',(-0.678525403784438,-1.17524047358083,
-2.04166666666667));
#378603=CARTESIAN_POINT('Ctrl Pts',(-1.43925448419919E-16,-1.17524047358083,
-2.));
#378604=CARTESIAN_POINT('Ctrl Pts',(0.678525403784437,-1.17524047358083,
-1.95833333333333));
#378605=CARTESIAN_POINT('Ctrl Pts',(1.01778810567666,-0.587620236790417,
-1.91666666666667));
#378606=CARTESIAN_POINT('Ctrl Pts',(1.35705080756888,2.7065942666714E-16,
-1.875));
#378607=CARTESIAN_POINT('Ctrl Pts',(1.01778810567666,0.587620236790417,
-1.83333333333333));
#378608=CARTESIAN_POINT('Ctrl Pts',(0.678525403784439,1.17524047358083,
-1.79166666666667));
#378609=CARTESIAN_POINT('Ctrl Pts',(0.,1.17524047358083,-1.75));
#378610=CARTESIAN_POINT('Ctrl Pts',(-0.678525403784438,1.17524047358083,
-1.70833333333333));
#378611=CARTESIAN_POINT('Ctrl Pts',(-1.01778810567666,0.587620236790418,
-1.66666666666667));
#378612=CARTESIAN_POINT('Ctrl Pts',(-1.35705080756888,6.03041012221051E-16,
-1.625));
#378613=CARTESIAN_POINT('Ctrl Pts',(-1.01778810567666,-0.587620236790416,
-1.58333333333333));
#378614=CARTESIAN_POINT('Ctrl Pts',(-0.678525403784438,-1.17524047358083,
-1.54166666666667));
#378615=CARTESIAN_POINT('Ctrl Pts',(-1.43925448419919E-16,-1.17524047358083,
-1.5));
#378616=CARTESIAN_POINT('Ctrl Pts',(0.678525403784437,-1.17524047358083,
-1.45833333333333));
#378617=CARTESIAN_POINT('Ctrl Pts',(1.01778810567666,-0.587620236790417,
-1.41666666666667));
#378618=CARTESIAN_POINT('Ctrl Pts',(1.35705080756888,2.7065942666714E-16,
-1.375));
#378619=CARTESIAN_POINT('Ctrl Pts',(1.01778810567666,0.587620236790417,
-1.33333333333333));
#378620=CARTESIAN_POINT('Ctrl Pts',(0.678525403784439,1.17524047358083,
-1.29166666666667));
#378621=CARTESIAN_POINT('Ctrl Pts',(0.,1.17524047358083,-1.25));
#378622=CARTESIAN_POINT('Ctrl Pts',(-0.678525403784438,1.17524047358083,
-1.20833333333333));
#378623=CARTESIAN_POINT('Ctrl Pts',(-1.01778810567666,0.587620236790418,
-1.16666666666667));
#378624=CARTESIAN_POINT('Ctrl Pts',(-1.35705080756888,6.03041012221051E-16,
-1.125));
#378625=CARTESIAN_POINT('Ctrl Pts',(-1.01778810567666,-0.587620236790416,
-1.08333333333333));
#378626=CARTESIAN_POINT('Ctrl Pts',(-0.678525403784438,-1.17524047358083,
-1.04166666666667));
#378627=CARTESIAN_POINT('Ctrl Pts',(-1.43925448419919E-16,-1.17524047358083,
-0.999999999999999));
#378628=CARTESIAN_POINT('Ctrl Pts',(0.678525403784437,-1.17524047358083,
-0.958333333333334));
#378629=CARTESIAN_POINT('Ctrl Pts',(1.01778810567666,-0.587620236790417,
-0.916666666666666));
#378630=CARTESIAN_POINT('Ctrl Pts',(1.35705080756888,2.7065942666714E-16,
-0.874999999999999));
#378631=CARTESIAN_POINT('Ctrl Pts',(1.01778810567666,0.587620236790417,
-0.833333333333334));
#378632=CARTESIAN_POINT('Ctrl Pts',(0.678525403784439,1.17524047358083,
-0.791666666666666));
#378633=CARTESIAN_POINT('Ctrl Pts',(0.,1.17524047358083,-0.750000000000001));
#378634=CARTESIAN_POINT('Ctrl Pts',(-0.678525403784438,1.17524047358083,
-0.708333333333333));
#378635=CARTESIAN_POINT('Ctrl Pts',(-1.01778810567666,0.587620236790418,
-0.666666666666666));
#378636=CARTESIAN_POINT('Ctrl Pts',(-1.35705080756888,6.03041012221051E-16,
-0.625000000000001));
#378637=CARTESIAN_POINT('Ctrl Pts',(-1.01778810567666,-0.587620236790416,
-0.583333333333333));
#378638=CARTESIAN_POINT('Ctrl Pts',(-0.678525403784438,-1.17524047358083,
-0.541666666666666));
#378639=CARTESIAN_POINT('Ctrl Pts',(-1.43925448419919E-16,-1.17524047358083,
-0.5));
#378640=CARTESIAN_POINT('Ctrl Pts',(0.678525403784437,-1.17524047358083,
-0.458333333333333));
#378641=CARTESIAN_POINT('Ctrl Pts',(1.01778810567666,-0.587620236790417,
-0.416666666666666));
#378642=CARTESIAN_POINT('Ctrl Pts',(1.35705080756888,2.7065942666714E-16,
-0.375));
#378643=CARTESIAN_POINT('Ctrl Pts',(1.01778810567666,0.587620236790417,
-0.333333333333333));
#378644=CARTESIAN_POINT('Ctrl Pts',(0.678525403784439,1.17524047358083,
-0.291666666666666));
#378645=CARTESIAN_POINT('Ctrl Pts',(0.,1.17524047358083,-0.25));
#378646=CARTESIAN_POINT('Ctrl Pts',(-0.678525403784438,1.17524047358083,
-0.208333333333333));
#378647=CARTESIAN_POINT('Ctrl Pts',(-1.01778810567666,0.587620236790418,
-0.166666666666666));
#378648=CARTESIAN_POINT('Ctrl Pts',(-1.35705080756888,6.03041012221051E-16,
-0.125));
#378649=CARTESIAN_POINT('Ctrl Pts',(-1.01778810567666,-0.587620236790416,
-0.0833333333333328));
#378650=CARTESIAN_POINT('Ctrl Pts',(-0.678525403784438,-1.17524047358083,
-0.0416666666666673));
#378651=CARTESIAN_POINT('Ctrl Pts',(-1.43925448419919E-16,-1.17524047358083,
0.));
#378652=CARTESIAN_POINT('Ctrl Pts',(0.678525403784437,-1.17524047358083,
0.0416666666666673));
#378653=CARTESIAN_POINT('Ctrl Pts',(1.01778810567666,-0.587620236790417,
0.0833333333333328));
#378654=CARTESIAN_POINT('Ctrl Pts',(1.35705080756888,2.7065942666714E-16,
0.125));
#378655=CARTESIAN_POINT('Ctrl Pts',(1.01778810567666,0.587620236790417,
0.166666666666667));
#378656=CARTESIAN_POINT('Ctrl Pts',(0.678525403784439,1.17524047358083,
0.208333333333333));
#378657=CARTESIAN_POINT('Ctrl Pts',(0.,1.17524047358083,0.25));
#378658=CARTESIAN_POINT('Ctrl Pts',(-0.678525403784438,1.17524047358083,
0.291666666666668));
#378659=CARTESIAN_POINT('Ctrl Pts',(-1.01778810567666,0.587620236790418,
0.333333333333333));
#378660=CARTESIAN_POINT('Ctrl Pts',(-1.35705080756888,6.03041012221051E-16,
0.375));
#378661=CARTESIAN_POINT('Ctrl Pts',(-1.01778810567666,-0.587620236790416,
0.416666666666668));
#378662=CARTESIAN_POINT('Ctrl Pts',(-0.678525403784438,-1.17524047358083,
0.458333333333333));
#378663=CARTESIAN_POINT('Ctrl Pts',(-1.43925448419919E-16,-1.17524047358083,
0.5));
#378664=CARTESIAN_POINT('Ctrl Pts',(0.678525403784437,-1.17524047358083,
0.541666666666666));
#378665=CARTESIAN_POINT('Ctrl Pts',(1.01778810567666,-0.587620236790417,
0.583333333333333));
#378666=CARTESIAN_POINT('Ctrl Pts',(1.35705080756888,2.7065942666714E-16,
0.625000000000001));
#378667=CARTESIAN_POINT('Ctrl Pts',(1.01778810567666,0.587620236790417,
0.666666666666666));
#378668=CARTESIAN_POINT('Ctrl Pts',(0.678525403784439,1.17524047358083,
0.708333333333333));
#378669=CARTESIAN_POINT('Ctrl Pts',(0.,1.17524047358083,0.750000000000001));
#378670=CARTESIAN_POINT('Ctrl Pts',(-0.678525403784438,1.17524047358083,
0.791666666666666));
#378671=CARTESIAN_POINT('Ctrl Pts',(-1.01778810567666,0.587620236790418,
0.833333333333334));
#378672=CARTESIAN_POINT('Ctrl Pts',(-1.35705080756888,6.03041012221051E-16,
0.875000000000001));
#378673=CARTESIAN_POINT('Ctrl Pts',(-1.01778810567666,-0.587620236790416,
0.916666666666666));
#378674=CARTESIAN_POINT('Ctrl Pts',(-0.678525403784438,-1.17524047358083,
0.958333333333334));
#378675=CARTESIAN_POINT('Ctrl Pts',(-1.43925448419919E-16,-1.17524047358083,
1.));
#378676=CARTESIAN_POINT('Ctrl Pts',(0.678525403784437,-1.17524047358083,
1.04166666666667));
#378677=CARTESIAN_POINT('Ctrl Pts',(1.01778810567666,-0.587620236790417,
1.08333333333333));
#378678=CARTESIAN_POINT('Ctrl Pts',(1.35705080756888,2.7065942666714E-16,
1.125));
#378679=CARTESIAN_POINT('Ctrl Pts',(1.01778810567666,0.587620236790417,
1.16666666666667));
#378680=CARTESIAN_POINT('Ctrl Pts',(0.678525403784439,1.17524047358083,
1.20833333333333));
#378681=CARTESIAN_POINT('Ctrl Pts',(0.,1.17524047358083,1.25));
#378682=CARTESIAN_POINT('Ctrl Pts',(-0.678525403784438,1.17524047358083,
1.29166666666667));
#378683=CARTESIAN_POINT('Ctrl Pts',(-1.01778810567666,0.587620236790418,
1.33333333333333));
#378684=CARTESIAN_POINT('Ctrl Pts',(-1.35705080756888,6.03041012221051E-16,
1.375));
#378685=CARTESIAN_POINT('Ctrl Pts',(-1.01778810567666,-0.587620236790416,
1.41666666666667));
#378686=CARTESIAN_POINT('Ctrl Pts',(-0.678525403784438,-1.17524047358083,
1.45833333333333));
#378687=CARTESIAN_POINT('Ctrl Pts',(-1.43925448419919E-16,-1.17524047358083,
1.5));
#378688=CARTESIAN_POINT('Ctrl Pts',(0.678525403784437,-1.17524047358083,
1.54166666666667));
#378689=CARTESIAN_POINT('Ctrl Pts',(1.01778810567666,-0.587620236790417,
1.58333333333333));
#378690=CARTESIAN_POINT('Ctrl Pts',(1.35705080756888,2.7065942666714E-16,
1.625));
#378691=CARTESIAN_POINT('Ctrl Pts',(1.01778810567666,0.587620236790417,
1.66666666666667));
#378692=CARTESIAN_POINT('Ctrl Pts',(0.678525403784439,1.17524047358083,
1.70833333333333));
#378693=CARTESIAN_POINT('Ctrl Pts',(0.,1.17524047358083,1.75));
#378694=CARTESIAN_POINT('Ctrl Pts',(-0.678525403784438,1.17524047358083,
1.79166666666667));
#378695=CARTESIAN_POINT('Ctrl Pts',(-1.01778810567666,0.587620236790418,
1.83333333333333));
#378696=CARTESIAN_POINT('Ctrl Pts',(-1.35705080756888,6.03041012221051E-16,
1.875));
#378697=CARTESIAN_POINT('Ctrl Pts',(-1.01778810567666,-0.587620236790416,
1.91666666666667));
#378698=CARTESIAN_POINT('Ctrl Pts',(-0.678525403784438,-1.17524047358083,
1.95833333333333));
#378699=CARTESIAN_POINT('Ctrl Pts',(-1.43925448419919E-16,-1.17524047358083,
2.));
#378700=CARTESIAN_POINT('Ctrl Pts',(0.678525403784437,-1.17524047358083,
2.04166666666667));
#378701=CARTESIAN_POINT('Ctrl Pts',(1.01778810567666,-0.587620236790417,
2.08333333333333));
#378702=CARTESIAN_POINT('Ctrl Pts',(1.35705080756888,2.7065942666714E-16,
2.125));
#378703=CARTESIAN_POINT('Ctrl Pts',(1.01778810567666,0.587620236790417,
2.16666666666667));
#378704=CARTESIAN_POINT('Ctrl Pts',(0.678525403784439,1.17524047358083,
2.20833333333333));
#378705=CARTESIAN_POINT('Ctrl Pts',(0.,1.17524047358083,2.25));
#378706=CARTESIAN_POINT('Ctrl Pts',(-0.678525403784438,1.17524047358083,
2.29166666666667));
#378707=CARTESIAN_POINT('Ctrl Pts',(-1.01778810567666,0.587620236790418,
2.33333333333333));
#378708=CARTESIAN_POINT('Ctrl Pts',(-1.35705080756888,6.03041012221051E-16,
2.375));
#378709=CARTESIAN_POINT('Ctrl Pts',(-1.01778810567666,-0.587620236790416,
2.41666666666667));
#378710=CARTESIAN_POINT('Ctrl Pts',(-0.678525403784438,-1.17524047358083,
2.45833333333333));
#378711=CARTESIAN_POINT('Ctrl Pts',(-1.43925448419919E-16,-1.17524047358083,
2.5));
#378712=CARTESIAN_POINT('Ctrl Pts',(0.678525403784437,-1.17524047358083,
2.54166666666667));
#378713=CARTESIAN_POINT('Ctrl Pts',(1.01778810567666,-0.587620236790417,
2.58333333333333));
#378714=CARTESIAN_POINT('Ctrl Pts',(1.35705080756888,2.7065942666714E-16,
2.625));
#378715=CARTESIAN_POINT('Ctrl Pts',(1.01778810567666,0.587620236790417,
2.66666666666667));
#378716=CARTESIAN_POINT('Ctrl Pts',(0.678525403784439,1.17524047358083,
2.70833333333333));
#378717=CARTESIAN_POINT('Ctrl Pts',(0.,1.17524047358083,2.75));
#378718=CARTESIAN_POINT('Ctrl Pts',(-0.678525403784438,1.17524047358083,
2.79166666666667));
#378719=CARTESIAN_POINT('Ctrl Pts',(-1.01778810567666,0.587620236790418,
2.83333333333333));
#378720=CARTESIAN_POINT('Ctrl Pts',(-1.35705080756888,6.03041012221051E-16,
2.875));
#378721=CARTESIAN_POINT('Ctrl Pts',(-1.01778810567666,-0.587620236790416,
2.91666666666667));
#378722=CARTESIAN_POINT('Ctrl Pts',(-0.678525403784438,-1.17524047358083,
2.95833333333333));
#378723=CARTESIAN_POINT('Ctrl Pts',(-1.43925448419919E-16,-1.17524047358083,
3.));
#378724=CARTESIAN_POINT('Ctrl Pts',(0.678525403784437,-1.17524047358083,
3.04166666666667));
#378725=CARTESIAN_POINT('Ctrl Pts',(1.01778810567666,-0.587620236790417,
3.08333333333333));
#378726=CARTESIAN_POINT('Ctrl Pts',(1.35705080756888,2.7065942666714E-16,
3.125));
#378727=CARTESIAN_POINT('Ctrl Pts',(1.01778810567666,0.587620236790417,
3.16666666666667));
#378728=CARTESIAN_POINT('Ctrl Pts',(0.678525403784439,1.17524047358083,
3.20833333333333));
#378729=CARTESIAN_POINT('Ctrl Pts',(0.,1.17524047358083,3.25));
#378730=CARTESIAN_POINT('Ctrl Pts',(-0.678525403784438,1.17524047358083,
3.29166666666667));
#378731=CARTESIAN_POINT('Ctrl Pts',(-1.01778810567666,0.587620236790418,
3.33333333333333));
#378732=CARTESIAN_POINT('Ctrl Pts',(-1.35705080756888,6.03041012221051E-16,
3.375));
#378733=CARTESIAN_POINT('Ctrl Pts',(-1.01778810567666,-0.587620236790416,
3.41666666666667));
#378734=CARTESIAN_POINT('Ctrl Pts',(-0.678525403784438,-1.17524047358083,
3.45833333333333));
#378735=CARTESIAN_POINT('Ctrl Pts',(-1.43925448419919E-16,-1.17524047358083,
3.5));
#378736=CARTESIAN_POINT('Ctrl Pts',(0.678525403784437,-1.17524047358083,
3.54166666666667));
#378737=CARTESIAN_POINT('Ctrl Pts',(1.01778810567666,-0.587620236790417,
3.58333333333333));
#378738=CARTESIAN_POINT('Ctrl Pts',(1.35705080756888,2.7065942666714E-16,
3.625));
#378739=CARTESIAN_POINT('Ctrl Pts',(1.01778810567666,0.587620236790417,
3.66666666666667));
#378740=CARTESIAN_POINT('Ctrl Pts',(0.678525403784439,1.17524047358083,
3.70833333333333));
#378741=CARTESIAN_POINT('Ctrl Pts',(0.,1.17524047358083,3.75));
#378742=CARTESIAN_POINT('Ctrl Pts',(-0.678525403784438,1.17524047358083,
3.79166666666667));
#378743=CARTESIAN_POINT('Ctrl Pts',(-1.01778810567666,0.587620236790418,
3.83333333333333));
#378744=CARTESIAN_POINT('Ctrl Pts',(-1.35705080756888,6.03041012221051E-16,
3.875));
#378745=CARTESIAN_POINT('Ctrl Pts',(-1.01778810567666,-0.587620236790416,
3.91666666666667));
#378746=CARTESIAN_POINT('Ctrl Pts',(-0.678525403784438,-1.17524047358083,
3.95833333333333));
#378747=CARTESIAN_POINT('Ctrl Pts',(-1.43925448419919E-16,-1.17524047358083,
4.));
#378748=CARTESIAN_POINT('Ctrl Pts',(0.678525403784437,-1.17524047358083,
4.04166666666667));
#378749=CARTESIAN_POINT('Ctrl Pts',(1.01778810567666,-0.587620236790417,
4.08333333333333));
#378750=CARTESIAN_POINT('Ctrl Pts',(1.35705080756888,2.7065942666714E-16,
4.125));
#378751=CARTESIAN_POINT('Ctrl Pts',(1.01778810567666,0.587620236790417,
4.16666666666667));
#378752=CARTESIAN_POINT('Ctrl Pts',(0.678525403784439,1.17524047358083,
4.20833333333333));
#378753=CARTESIAN_POINT('Ctrl Pts',(0.,1.17524047358083,4.25));
#378754=CARTESIAN_POINT('Ctrl Pts',(-0.678525403784438,1.17524047358083,
4.29166666666667));
#378755=CARTESIAN_POINT('Ctrl Pts',(-1.01778810567666,0.587620236790418,
4.33333333333333));
#378756=CARTESIAN_POINT('Ctrl Pts',(-1.35705080756888,6.03041012221051E-16,
4.375));
#378757=CARTESIAN_POINT('Ctrl Pts',(-1.01778810567666,-0.587620236790416,
4.41666666666667));
#378758=CARTESIAN_POINT('Ctrl Pts',(-0.678525403784438,-1.17524047358083,
4.45833333333333));
#378759=CARTESIAN_POINT('Ctrl Pts',(-1.43925448419919E-16,-1.17524047358083,
4.5));
#378760=CARTESIAN_POINT('Ctrl Pts',(0.678525403784437,-1.17524047358083,
4.54166666666667));
#378761=CARTESIAN_POINT('Ctrl Pts',(1.01778810567666,-0.587620236790417,
4.58333333333333));
#378762=CARTESIAN_POINT('Ctrl Pts',(1.35705080756888,2.7065942666714E-16,
4.625));
#378763=CARTESIAN_POINT('Ctrl Pts',(1.01778810567666,0.587620236790417,
4.66666666666667));
#378764=CARTESIAN_POINT('Ctrl Pts',(0.678525403784439,1.17524047358083,
4.70833333333333));
#378765=CARTESIAN_POINT('Ctrl Pts',(0.,1.17524047358083,4.75));
#378766=CARTESIAN_POINT('Ctrl Pts',(-0.678525403784438,1.17524047358083,
4.79166666666667));
#378767=CARTESIAN_POINT('Ctrl Pts',(-1.01778810567666,0.587620236790418,
4.83333333333333));
#378768=CARTESIAN_POINT('Ctrl Pts',(-1.35705080756888,6.03041012221051E-16,
4.875));
#378769=CARTESIAN_POINT('Ctrl Pts',(-1.01778810567666,-0.587620236790416,
4.91666666666667));
#378770=CARTESIAN_POINT('Ctrl Pts',(-0.678525403784438,-1.17524047358083,
4.95833333333333));
#378771=CARTESIAN_POINT('Ctrl Pts',(-1.43925448419919E-16,-1.17524047358083,
5.));
#378772=CARTESIAN_POINT('Ctrl Pts',(0.678525403784437,-1.17524047358083,
5.04166666666667));
#378773=CARTESIAN_POINT('Ctrl Pts',(1.01778810567666,-0.587620236790417,
5.08333333333333));
#378774=CARTESIAN_POINT('Ctrl Pts',(1.35705080756888,2.7065942666714E-16,
5.125));
#378775=CARTESIAN_POINT('Ctrl Pts',(1.01778810567666,0.587620236790417,
5.16666666666667));
#378776=CARTESIAN_POINT('Ctrl Pts',(0.678525403784439,1.17524047358083,
5.20833333333333));
#378777=CARTESIAN_POINT('Ctrl Pts',(0.,1.17524047358083,5.25));
#378778=CARTESIAN_POINT('Ctrl Pts',(-0.678525403784438,1.17524047358083,
5.29166666666667));
#378779=CARTESIAN_POINT('Ctrl Pts',(-1.01778810567666,0.587620236790418,
5.33333333333333));
#378780=CARTESIAN_POINT('Ctrl Pts',(-1.35705080756888,6.03041012221051E-16,
5.375));
#378781=CARTESIAN_POINT('Ctrl Pts',(-1.01778810567666,-0.587620236790416,
5.41666666666667));
#378782=CARTESIAN_POINT('Ctrl Pts',(-0.678525403784438,-1.17524047358083,
5.45833333333333));
#378783=CARTESIAN_POINT('Ctrl Pts',(-1.43925448419919E-16,-1.17524047358083,
5.5));
#378784=CARTESIAN_POINT('Ctrl Pts',(0.678525403784437,-1.17524047358083,
5.54166666666667));
#378785=CARTESIAN_POINT('Ctrl Pts',(1.01778810567666,-0.587620236790417,
5.58333333333333));
#378786=CARTESIAN_POINT('Ctrl Pts',(1.35705080756888,2.7065942666714E-16,
5.625));
#378787=CARTESIAN_POINT('Ctrl Pts',(1.01778810567666,0.587620236790417,
5.66666666666667));
#378788=CARTESIAN_POINT('Ctrl Pts',(0.678525403784439,1.17524047358083,
5.70833333333333));
#378789=CARTESIAN_POINT('Ctrl Pts',(0.,1.17524047358083,5.75));
#378790=CARTESIAN_POINT('Ctrl Pts',(-0.678525403784438,1.17524047358083,
5.79166666666667));
#378791=CARTESIAN_POINT('Ctrl Pts',(-1.01778810567666,0.587620236790418,
5.83333333333333));
#378792=CARTESIAN_POINT('Ctrl Pts',(-1.35705080756888,6.03041012221051E-16,
5.875));
#378793=CARTESIAN_POINT('Ctrl Pts',(-1.01778810567666,-0.587620236790416,
5.91666666666667));
#378794=CARTESIAN_POINT('Ctrl Pts',(-0.678525403784438,-1.17524047358083,
5.95833333333333));
#378795=CARTESIAN_POINT('Ctrl Pts',(-1.43925448419919E-16,-1.17524047358083,
6.));
#378796=CARTESIAN_POINT('Ctrl Pts',(0.678525403784437,-1.17524047358083,
6.04166666666667));
#378797=CARTESIAN_POINT('Ctrl Pts',(1.01778810567666,-0.587620236790417,
6.08333333333333));
#378798=CARTESIAN_POINT('Ctrl Pts',(1.35705080756888,2.7065942666714E-16,
6.125));
#378799=CARTESIAN_POINT('Ctrl Pts',(1.01778810567666,0.587620236790417,
6.16666666666667));
#378800=CARTESIAN_POINT('Ctrl Pts',(0.678525403784439,1.17524047358083,
6.20833333333333));
#378801=CARTESIAN_POINT('Ctrl Pts',(0.,1.17524047358083,6.25));
#378802=CARTESIAN_POINT('Ctrl Pts',(0.,1.52706329386826,-9.453125));
#378803=CARTESIAN_POINT('Ctrl Pts',(-0.881650403784438,1.52706329386826,
-9.41145833333334));
#378804=CARTESIAN_POINT('Ctrl Pts',(-1.32247560567666,0.763531646934132,
-9.36979166666667));
#378805=CARTESIAN_POINT('Ctrl Pts',(-1.76330080756888,6.27916650328731E-16,
-9.328125));
#378806=CARTESIAN_POINT('Ctrl Pts',(-1.32247560567666,-0.76353164693413,
-9.28645833333333));
#378807=CARTESIAN_POINT('Ctrl Pts',(-0.881650403784439,-1.52706329386826,
-9.24479166666667));
#378808=CARTESIAN_POINT('Ctrl Pts',(-1.87011317493118E-16,-1.52706329386826,
-9.203125));
#378809=CARTESIAN_POINT('Ctrl Pts',(0.881650403784437,-1.52706329386826,
-9.16145833333333));
#378810=CARTESIAN_POINT('Ctrl Pts',(1.32247560567666,-0.763531646934131,
-9.11979166666667));
#378811=CARTESIAN_POINT('Ctrl Pts',(1.76330080756888,1.96032512344098E-16,
-9.078125));
#378812=CARTESIAN_POINT('Ctrl Pts',(1.32247560567666,0.763531646934131,
-9.03645833333334));
#378813=CARTESIAN_POINT('Ctrl Pts',(0.881650403784439,1.52706329386826,
-8.99479166666667));
#378814=CARTESIAN_POINT('Ctrl Pts',(0.,1.52706329386826,-8.953125));
#378815=CARTESIAN_POINT('Ctrl Pts',(-0.881650403784438,1.52706329386826,
-8.91145833333334));
#378816=CARTESIAN_POINT('Ctrl Pts',(-1.32247560567666,0.763531646934132,
-8.86979166666667));
#378817=CARTESIAN_POINT('Ctrl Pts',(-1.76330080756888,6.27916650328731E-16,
-8.828125));
#378818=CARTESIAN_POINT('Ctrl Pts',(-1.32247560567666,-0.76353164693413,
-8.78645833333334));
#378819=CARTESIAN_POINT('Ctrl Pts',(-0.881650403784439,-1.52706329386826,
-8.74479166666667));
#378820=CARTESIAN_POINT('Ctrl Pts',(-1.87011317493118E-16,-1.52706329386826,
-8.703125));
#378821=CARTESIAN_POINT('Ctrl Pts',(0.881650403784437,-1.52706329386826,
-8.66145833333333));
#378822=CARTESIAN_POINT('Ctrl Pts',(1.32247560567666,-0.763531646934131,
-8.61979166666667));
#378823=CARTESIAN_POINT('Ctrl Pts',(1.76330080756888,1.96032512344098E-16,
-8.578125));
#378824=CARTESIAN_POINT('Ctrl Pts',(1.32247560567666,0.763531646934131,
-8.53645833333334));
#378825=CARTESIAN_POINT('Ctrl Pts',(0.881650403784439,1.52706329386826,
-8.49479166666667));
#378826=CARTESIAN_POINT('Ctrl Pts',(0.,1.52706329386826,-8.453125));
#378827=CARTESIAN_POINT('Ctrl Pts',(-0.881650403784438,1.52706329386826,
-8.41145833333334));
#378828=CARTESIAN_POINT('Ctrl Pts',(-1.32247560567666,0.763531646934132,
-8.36979166666667));
#378829=CARTESIAN_POINT('Ctrl Pts',(-1.76330080756888,6.27916650328731E-16,
-8.328125));
#378830=CARTESIAN_POINT('Ctrl Pts',(-1.32247560567666,-0.76353164693413,
-8.28645833333334));
#378831=CARTESIAN_POINT('Ctrl Pts',(-0.881650403784439,-1.52706329386826,
-8.24479166666667));
#378832=CARTESIAN_POINT('Ctrl Pts',(-1.87011317493118E-16,-1.52706329386826,
-8.203125));
#378833=CARTESIAN_POINT('Ctrl Pts',(0.881650403784437,-1.52706329386826,
-8.16145833333333));
#378834=CARTESIAN_POINT('Ctrl Pts',(1.32247560567666,-0.763531646934131,
-8.11979166666667));
#378835=CARTESIAN_POINT('Ctrl Pts',(1.76330080756888,1.96032512344098E-16,
-8.078125));
#378836=CARTESIAN_POINT('Ctrl Pts',(1.32247560567666,0.763531646934131,
-8.03645833333333));
#378837=CARTESIAN_POINT('Ctrl Pts',(0.881650403784439,1.52706329386826,
-7.99479166666667));
#378838=CARTESIAN_POINT('Ctrl Pts',(0.,1.52706329386826,-7.953125));
#378839=CARTESIAN_POINT('Ctrl Pts',(-0.881650403784438,1.52706329386826,
-7.91145833333334));
#378840=CARTESIAN_POINT('Ctrl Pts',(-1.32247560567666,0.763531646934132,
-7.86979166666667));
#378841=CARTESIAN_POINT('Ctrl Pts',(-1.76330080756888,6.27916650328731E-16,
-7.828125));
#378842=CARTESIAN_POINT('Ctrl Pts',(-1.32247560567666,-0.76353164693413,
-7.78645833333333));
#378843=CARTESIAN_POINT('Ctrl Pts',(-0.881650403784439,-1.52706329386826,
-7.74479166666667));
#378844=CARTESIAN_POINT('Ctrl Pts',(-1.87011317493118E-16,-1.52706329386826,
-7.703125));
#378845=CARTESIAN_POINT('Ctrl Pts',(0.881650403784437,-1.52706329386826,
-7.66145833333333));
#378846=CARTESIAN_POINT('Ctrl Pts',(1.32247560567666,-0.763531646934131,
-7.61979166666667));
#378847=CARTESIAN_POINT('Ctrl Pts',(1.76330080756888,1.96032512344098E-16,
-7.578125));
#378848=CARTESIAN_POINT('Ctrl Pts',(1.32247560567666,0.763531646934131,
-7.53645833333334));
#378849=CARTESIAN_POINT('Ctrl Pts',(0.881650403784439,1.52706329386826,
-7.49479166666667));
#378850=CARTESIAN_POINT('Ctrl Pts',(0.,1.52706329386826,-7.453125));
#378851=CARTESIAN_POINT('Ctrl Pts',(-0.881650403784438,1.52706329386826,
-7.41145833333334));
#378852=CARTESIAN_POINT('Ctrl Pts',(-1.32247560567666,0.763531646934132,
-7.36979166666667));
#378853=CARTESIAN_POINT('Ctrl Pts',(-1.76330080756888,6.27916650328731E-16,
-7.328125));
#378854=CARTESIAN_POINT('Ctrl Pts',(-1.32247560567666,-0.76353164693413,
-7.28645833333334));
#378855=CARTESIAN_POINT('Ctrl Pts',(-0.881650403784439,-1.52706329386826,
-7.24479166666667));
#378856=CARTESIAN_POINT('Ctrl Pts',(-1.87011317493118E-16,-1.52706329386826,
-7.203125));
#378857=CARTESIAN_POINT('Ctrl Pts',(0.881650403784437,-1.52706329386826,
-7.16145833333333));
#378858=CARTESIAN_POINT('Ctrl Pts',(1.32247560567666,-0.763531646934131,
-7.11979166666667));
#378859=CARTESIAN_POINT('Ctrl Pts',(1.76330080756888,1.96032512344098E-16,
-7.078125));
#378860=CARTESIAN_POINT('Ctrl Pts',(1.32247560567666,0.763531646934131,
-7.03645833333334));
#378861=CARTESIAN_POINT('Ctrl Pts',(0.881650403784439,1.52706329386826,
-6.99479166666667));
#378862=CARTESIAN_POINT('Ctrl Pts',(0.,1.52706329386826,-6.953125));
#378863=CARTESIAN_POINT('Ctrl Pts',(-0.881650403784438,1.52706329386826,
-6.91145833333334));
#378864=CARTESIAN_POINT('Ctrl Pts',(-1.32247560567666,0.763531646934132,
-6.86979166666667));
#378865=CARTESIAN_POINT('Ctrl Pts',(-1.76330080756888,6.27916650328731E-16,
-6.828125));
#378866=CARTESIAN_POINT('Ctrl Pts',(-1.32247560567666,-0.76353164693413,
-6.78645833333334));
#378867=CARTESIAN_POINT('Ctrl Pts',(-0.881650403784439,-1.52706329386826,
-6.74479166666667));
#378868=CARTESIAN_POINT('Ctrl Pts',(-1.87011317493118E-16,-1.52706329386826,
-6.703125));
#378869=CARTESIAN_POINT('Ctrl Pts',(0.881650403784437,-1.52706329386826,
-6.66145833333334));
#378870=CARTESIAN_POINT('Ctrl Pts',(1.32247560567666,-0.763531646934131,
-6.61979166666667));
#378871=CARTESIAN_POINT('Ctrl Pts',(1.76330080756888,1.96032512344098E-16,
-6.578125));
#378872=CARTESIAN_POINT('Ctrl Pts',(1.32247560567666,0.763531646934131,
-6.53645833333333));
#378873=CARTESIAN_POINT('Ctrl Pts',(0.881650403784439,1.52706329386826,
-6.49479166666667));
#378874=CARTESIAN_POINT('Ctrl Pts',(0.,1.52706329386826,-6.453125));
#378875=CARTESIAN_POINT('Ctrl Pts',(-0.881650403784438,1.52706329386826,
-6.41145833333334));
#378876=CARTESIAN_POINT('Ctrl Pts',(-1.32247560567666,0.763531646934132,
-6.36979166666667));
#378877=CARTESIAN_POINT('Ctrl Pts',(-1.76330080756888,6.27916650328731E-16,
-6.328125));
#378878=CARTESIAN_POINT('Ctrl Pts',(-1.32247560567666,-0.76353164693413,
-6.28645833333334));
#378879=CARTESIAN_POINT('Ctrl Pts',(-0.881650403784439,-1.52706329386826,
-6.24479166666667));
#378880=CARTESIAN_POINT('Ctrl Pts',(-1.87011317493118E-16,-1.52706329386826,
-6.203125));
#378881=CARTESIAN_POINT('Ctrl Pts',(0.881650403784437,-1.52706329386826,
-6.16145833333333));
#378882=CARTESIAN_POINT('Ctrl Pts',(1.32247560567666,-0.763531646934131,
-6.11979166666667));
#378883=CARTESIAN_POINT('Ctrl Pts',(1.76330080756888,1.96032512344098E-16,
-6.078125));
#378884=CARTESIAN_POINT('Ctrl Pts',(1.32247560567666,0.763531646934131,
-6.03645833333334));
#378885=CARTESIAN_POINT('Ctrl Pts',(0.881650403784439,1.52706329386826,
-5.99479166666667));
#378886=CARTESIAN_POINT('Ctrl Pts',(0.,1.52706329386826,-5.953125));
#378887=CARTESIAN_POINT('Ctrl Pts',(-0.881650403784438,1.52706329386826,
-5.91145833333334));
#378888=CARTESIAN_POINT('Ctrl Pts',(-1.32247560567666,0.763531646934132,
-5.86979166666667));
#378889=CARTESIAN_POINT('Ctrl Pts',(-1.76330080756888,6.27916650328731E-16,
-5.828125));
#378890=CARTESIAN_POINT('Ctrl Pts',(-1.32247560567666,-0.76353164693413,
-5.78645833333334));
#378891=CARTESIAN_POINT('Ctrl Pts',(-0.881650403784439,-1.52706329386826,
-5.74479166666667));
#378892=CARTESIAN_POINT('Ctrl Pts',(-1.87011317493118E-16,-1.52706329386826,
-5.703125));
#378893=CARTESIAN_POINT('Ctrl Pts',(0.881650403784437,-1.52706329386826,
-5.66145833333333));
#378894=CARTESIAN_POINT('Ctrl Pts',(1.32247560567666,-0.763531646934131,
-5.61979166666667));
#378895=CARTESIAN_POINT('Ctrl Pts',(1.76330080756888,1.96032512344098E-16,
-5.578125));
#378896=CARTESIAN_POINT('Ctrl Pts',(1.32247560567666,0.763531646934131,
-5.53645833333333));
#378897=CARTESIAN_POINT('Ctrl Pts',(0.881650403784439,1.52706329386826,
-5.49479166666667));
#378898=CARTESIAN_POINT('Ctrl Pts',(0.,1.52706329386826,-5.453125));
#378899=CARTESIAN_POINT('Ctrl Pts',(-0.881650403784438,1.52706329386826,
-5.41145833333334));
#378900=CARTESIAN_POINT('Ctrl Pts',(-1.32247560567666,0.763531646934132,
-5.36979166666667));
#378901=CARTESIAN_POINT('Ctrl Pts',(-1.76330080756888,6.27916650328731E-16,
-5.328125));
#378902=CARTESIAN_POINT('Ctrl Pts',(-1.32247560567666,-0.76353164693413,
-5.28645833333333));
#378903=CARTESIAN_POINT('Ctrl Pts',(-0.881650403784439,-1.52706329386826,
-5.24479166666667));
#378904=CARTESIAN_POINT('Ctrl Pts',(-1.87011317493118E-16,-1.52706329386826,
-5.203125));
#378905=CARTESIAN_POINT('Ctrl Pts',(0.881650403784437,-1.52706329386826,
-5.16145833333333));
#378906=CARTESIAN_POINT('Ctrl Pts',(1.32247560567666,-0.763531646934131,
-5.11979166666667));
#378907=CARTESIAN_POINT('Ctrl Pts',(1.76330080756888,1.96032512344098E-16,
-5.078125));
#378908=CARTESIAN_POINT('Ctrl Pts',(1.32247560567666,0.763531646934131,
-5.03645833333333));
#378909=CARTESIAN_POINT('Ctrl Pts',(0.881650403784439,1.52706329386826,
-4.99479166666667));
#378910=CARTESIAN_POINT('Ctrl Pts',(0.,1.52706329386826,-4.953125));
#378911=CARTESIAN_POINT('Ctrl Pts',(-0.881650403784438,1.52706329386826,
-4.91145833333333));
#378912=CARTESIAN_POINT('Ctrl Pts',(-1.32247560567666,0.763531646934132,
-4.86979166666667));
#378913=CARTESIAN_POINT('Ctrl Pts',(-1.76330080756888,6.27916650328731E-16,
-4.828125));
#378914=CARTESIAN_POINT('Ctrl Pts',(-1.32247560567666,-0.76353164693413,
-4.78645833333334));
#378915=CARTESIAN_POINT('Ctrl Pts',(-0.881650403784439,-1.52706329386826,
-4.74479166666667));
#378916=CARTESIAN_POINT('Ctrl Pts',(-1.87011317493118E-16,-1.52706329386826,
-4.703125));
#378917=CARTESIAN_POINT('Ctrl Pts',(0.881650403784437,-1.52706329386826,
-4.66145833333333));
#378918=CARTESIAN_POINT('Ctrl Pts',(1.32247560567666,-0.763531646934131,
-4.61979166666667));
#378919=CARTESIAN_POINT('Ctrl Pts',(1.76330080756888,1.96032512344098E-16,
-4.578125));
#378920=CARTESIAN_POINT('Ctrl Pts',(1.32247560567666,0.763531646934131,
-4.53645833333334));
#378921=CARTESIAN_POINT('Ctrl Pts',(0.881650403784439,1.52706329386826,
-4.49479166666667));
#378922=CARTESIAN_POINT('Ctrl Pts',(0.,1.52706329386826,-4.453125));
#378923=CARTESIAN_POINT('Ctrl Pts',(-0.881650403784438,1.52706329386826,
-4.41145833333333));
#378924=CARTESIAN_POINT('Ctrl Pts',(-1.32247560567666,0.763531646934132,
-4.36979166666667));
#378925=CARTESIAN_POINT('Ctrl Pts',(-1.76330080756888,6.27916650328731E-16,
-4.328125));
#378926=CARTESIAN_POINT('Ctrl Pts',(-1.32247560567666,-0.76353164693413,
-4.28645833333333));
#378927=CARTESIAN_POINT('Ctrl Pts',(-0.881650403784439,-1.52706329386826,
-4.24479166666667));
#378928=CARTESIAN_POINT('Ctrl Pts',(-1.87011317493118E-16,-1.52706329386826,
-4.203125));
#378929=CARTESIAN_POINT('Ctrl Pts',(0.881650403784437,-1.52706329386826,
-4.16145833333333));
#378930=CARTESIAN_POINT('Ctrl Pts',(1.32247560567666,-0.763531646934131,
-4.11979166666667));
#378931=CARTESIAN_POINT('Ctrl Pts',(1.76330080756888,1.96032512344098E-16,
-4.078125));
#378932=CARTESIAN_POINT('Ctrl Pts',(1.32247560567666,0.763531646934131,
-4.03645833333333));
#378933=CARTESIAN_POINT('Ctrl Pts',(0.881650403784439,1.52706329386826,
-3.99479166666667));
#378934=CARTESIAN_POINT('Ctrl Pts',(0.,1.52706329386826,-3.953125));
#378935=CARTESIAN_POINT('Ctrl Pts',(-0.881650403784438,1.52706329386826,
-3.91145833333334));
#378936=CARTESIAN_POINT('Ctrl Pts',(-1.32247560567666,0.763531646934132,
-3.86979166666667));
#378937=CARTESIAN_POINT('Ctrl Pts',(-1.76330080756888,6.27916650328731E-16,
-3.828125));
#378938=CARTESIAN_POINT('Ctrl Pts',(-1.32247560567666,-0.76353164693413,
-3.78645833333334));
#378939=CARTESIAN_POINT('Ctrl Pts',(-0.881650403784439,-1.52706329386826,
-3.74479166666667));
#378940=CARTESIAN_POINT('Ctrl Pts',(-1.87011317493118E-16,-1.52706329386826,
-3.703125));
#378941=CARTESIAN_POINT('Ctrl Pts',(0.881650403784437,-1.52706329386826,
-3.66145833333334));
#378942=CARTESIAN_POINT('Ctrl Pts',(1.32247560567666,-0.763531646934131,
-3.61979166666667));
#378943=CARTESIAN_POINT('Ctrl Pts',(1.76330080756888,1.96032512344098E-16,
-3.578125));
#378944=CARTESIAN_POINT('Ctrl Pts',(1.32247560567666,0.763531646934131,
-3.53645833333333));
#378945=CARTESIAN_POINT('Ctrl Pts',(0.881650403784439,1.52706329386826,
-3.49479166666667));
#378946=CARTESIAN_POINT('Ctrl Pts',(0.,1.52706329386826,-3.453125));
#378947=CARTESIAN_POINT('Ctrl Pts',(-0.881650403784438,1.52706329386826,
-3.41145833333334));
#378948=CARTESIAN_POINT('Ctrl Pts',(-1.32247560567666,0.763531646934132,
-3.36979166666667));
#378949=CARTESIAN_POINT('Ctrl Pts',(-1.76330080756888,6.27916650328731E-16,
-3.328125));
#378950=CARTESIAN_POINT('Ctrl Pts',(-1.32247560567666,-0.76353164693413,
-3.28645833333334));
#378951=CARTESIAN_POINT('Ctrl Pts',(-0.881650403784439,-1.52706329386826,
-3.24479166666667));
#378952=CARTESIAN_POINT('Ctrl Pts',(-1.87011317493118E-16,-1.52706329386826,
-3.203125));
#378953=CARTESIAN_POINT('Ctrl Pts',(0.881650403784437,-1.52706329386826,
-3.16145833333334));
#378954=CARTESIAN_POINT('Ctrl Pts',(1.32247560567666,-0.763531646934131,
-3.11979166666667));
#378955=CARTESIAN_POINT('Ctrl Pts',(1.76330080756888,1.96032512344098E-16,
-3.078125));
#378956=CARTESIAN_POINT('Ctrl Pts',(1.32247560567666,0.763531646934131,
-3.03645833333333));
#378957=CARTESIAN_POINT('Ctrl Pts',(0.881650403784439,1.52706329386826,
-2.99479166666667));
#378958=CARTESIAN_POINT('Ctrl Pts',(0.,1.52706329386826,-2.953125));
#378959=CARTESIAN_POINT('Ctrl Pts',(-0.881650403784438,1.52706329386826,
-2.91145833333334));
#378960=CARTESIAN_POINT('Ctrl Pts',(-1.32247560567666,0.763531646934132,
-2.86979166666667));
#378961=CARTESIAN_POINT('Ctrl Pts',(-1.76330080756888,6.27916650328731E-16,
-2.828125));
#378962=CARTESIAN_POINT('Ctrl Pts',(-1.32247560567666,-0.76353164693413,
-2.78645833333334));
#378963=CARTESIAN_POINT('Ctrl Pts',(-0.881650403784439,-1.52706329386826,
-2.74479166666667));
#378964=CARTESIAN_POINT('Ctrl Pts',(-1.87011317493118E-16,-1.52706329386826,
-2.703125));
#378965=CARTESIAN_POINT('Ctrl Pts',(0.881650403784437,-1.52706329386826,
-2.66145833333334));
#378966=CARTESIAN_POINT('Ctrl Pts',(1.32247560567666,-0.763531646934131,
-2.61979166666667));
#378967=CARTESIAN_POINT('Ctrl Pts',(1.76330080756888,1.96032512344098E-16,
-2.578125));
#378968=CARTESIAN_POINT('Ctrl Pts',(1.32247560567666,0.763531646934131,
-2.53645833333334));
#378969=CARTESIAN_POINT('Ctrl Pts',(0.881650403784439,1.52706329386826,
-2.49479166666667));
#378970=CARTESIAN_POINT('Ctrl Pts',(0.,1.52706329386826,-2.453125));
#378971=CARTESIAN_POINT('Ctrl Pts',(-0.881650403784438,1.52706329386826,
-2.41145833333334));
#378972=CARTESIAN_POINT('Ctrl Pts',(-1.32247560567666,0.763531646934132,
-2.36979166666667));
#378973=CARTESIAN_POINT('Ctrl Pts',(-1.76330080756888,6.27916650328731E-16,
-2.328125));
#378974=CARTESIAN_POINT('Ctrl Pts',(-1.32247560567666,-0.76353164693413,
-2.28645833333333));
#378975=CARTESIAN_POINT('Ctrl Pts',(-0.881650403784439,-1.52706329386826,
-2.24479166666667));
#378976=CARTESIAN_POINT('Ctrl Pts',(-1.87011317493118E-16,-1.52706329386826,
-2.203125));
#378977=CARTESIAN_POINT('Ctrl Pts',(0.881650403784437,-1.52706329386826,
-2.16145833333333));
#378978=CARTESIAN_POINT('Ctrl Pts',(1.32247560567666,-0.763531646934131,
-2.11979166666667));
#378979=CARTESIAN_POINT('Ctrl Pts',(1.76330080756888,1.96032512344098E-16,
-2.078125));
#378980=CARTESIAN_POINT('Ctrl Pts',(1.32247560567666,0.763531646934131,
-2.03645833333334));
#378981=CARTESIAN_POINT('Ctrl Pts',(0.881650403784439,1.52706329386826,
-1.99479166666667));
#378982=CARTESIAN_POINT('Ctrl Pts',(0.,1.52706329386826,-1.953125));
#378983=CARTESIAN_POINT('Ctrl Pts',(-0.881650403784438,1.52706329386826,
-1.91145833333334));
#378984=CARTESIAN_POINT('Ctrl Pts',(-1.32247560567666,0.763531646934132,
-1.86979166666667));
#378985=CARTESIAN_POINT('Ctrl Pts',(-1.76330080756888,6.27916650328731E-16,
-1.828125));
#378986=CARTESIAN_POINT('Ctrl Pts',(-1.32247560567666,-0.76353164693413,
-1.78645833333334));
#378987=CARTESIAN_POINT('Ctrl Pts',(-0.881650403784439,-1.52706329386826,
-1.74479166666667));
#378988=CARTESIAN_POINT('Ctrl Pts',(-1.87011317493118E-16,-1.52706329386826,
-1.703125));
#378989=CARTESIAN_POINT('Ctrl Pts',(0.881650403784437,-1.52706329386826,
-1.66145833333334));
#378990=CARTESIAN_POINT('Ctrl Pts',(1.32247560567666,-0.763531646934131,
-1.61979166666667));
#378991=CARTESIAN_POINT('Ctrl Pts',(1.76330080756888,1.96032512344098E-16,
-1.578125));
#378992=CARTESIAN_POINT('Ctrl Pts',(1.32247560567666,0.763531646934131,
-1.53645833333334));
#378993=CARTESIAN_POINT('Ctrl Pts',(0.881650403784439,1.52706329386826,
-1.49479166666667));
#378994=CARTESIAN_POINT('Ctrl Pts',(0.,1.52706329386826,-1.453125));
#378995=CARTESIAN_POINT('Ctrl Pts',(-0.881650403784438,1.52706329386826,
-1.41145833333334));
#378996=CARTESIAN_POINT('Ctrl Pts',(-1.32247560567666,0.763531646934132,
-1.36979166666667));
#378997=CARTESIAN_POINT('Ctrl Pts',(-1.76330080756888,6.27916650328731E-16,
-1.328125));
#378998=CARTESIAN_POINT('Ctrl Pts',(-1.32247560567666,-0.76353164693413,
-1.28645833333334));
#378999=CARTESIAN_POINT('Ctrl Pts',(-0.881650403784439,-1.52706329386826,
-1.24479166666667));
#379000=CARTESIAN_POINT('Ctrl Pts',(-1.87011317493118E-16,-1.52706329386826,
-1.203125));
#379001=CARTESIAN_POINT('Ctrl Pts',(0.881650403784437,-1.52706329386826,
-1.16145833333334));
#379002=CARTESIAN_POINT('Ctrl Pts',(1.32247560567666,-0.763531646934131,
-1.11979166666667));
#379003=CARTESIAN_POINT('Ctrl Pts',(1.76330080756888,1.96032512344098E-16,
-1.078125));
#379004=CARTESIAN_POINT('Ctrl Pts',(1.32247560567666,0.763531646934131,
-1.03645833333334));
#379005=CARTESIAN_POINT('Ctrl Pts',(0.881650403784439,1.52706329386826,
-0.994791666666668));
#379006=CARTESIAN_POINT('Ctrl Pts',(0.,1.52706329386826,-0.953125000000003));
#379007=CARTESIAN_POINT('Ctrl Pts',(-0.881650403784438,1.52706329386826,
-0.911458333333335));
#379008=CARTESIAN_POINT('Ctrl Pts',(-1.32247560567666,0.763531646934132,
-0.869791666666668));
#379009=CARTESIAN_POINT('Ctrl Pts',(-1.76330080756888,6.27916650328731E-16,
-0.828125000000002));
#379010=CARTESIAN_POINT('Ctrl Pts',(-1.32247560567666,-0.76353164693413,
-0.786458333333335));
#379011=CARTESIAN_POINT('Ctrl Pts',(-0.881650403784439,-1.52706329386826,
-0.744791666666668));
#379012=CARTESIAN_POINT('Ctrl Pts',(-1.87011317493118E-16,-1.52706329386826,
-0.703125000000002));
#379013=CARTESIAN_POINT('Ctrl Pts',(0.881650403784437,-1.52706329386826,
-0.661458333333335));
#379014=CARTESIAN_POINT('Ctrl Pts',(1.32247560567666,-0.763531646934131,
-0.619791666666668));
#379015=CARTESIAN_POINT('Ctrl Pts',(1.76330080756888,1.96032512344098E-16,
-0.578125000000002));
#379016=CARTESIAN_POINT('Ctrl Pts',(1.32247560567666,0.763531646934131,
-0.536458333333335));
#379017=CARTESIAN_POINT('Ctrl Pts',(0.881650403784439,1.52706329386826,
-0.494791666666668));
#379018=CARTESIAN_POINT('Ctrl Pts',(0.,1.52706329386826,-0.453125000000002));
#379019=CARTESIAN_POINT('Ctrl Pts',(-0.881650403784438,1.52706329386826,
-0.411458333333335));
#379020=CARTESIAN_POINT('Ctrl Pts',(-1.32247560567666,0.763531646934132,
-0.369791666666668));
#379021=CARTESIAN_POINT('Ctrl Pts',(-1.76330080756888,6.27916650328731E-16,
-0.328125000000002));
#379022=CARTESIAN_POINT('Ctrl Pts',(-1.32247560567666,-0.76353164693413,
-0.286458333333335));
#379023=CARTESIAN_POINT('Ctrl Pts',(-0.881650403784439,-1.52706329386826,
-0.244791666666669));
#379024=CARTESIAN_POINT('Ctrl Pts',(-1.87011317493118E-16,-1.52706329386826,
-0.203125000000002));
#379025=CARTESIAN_POINT('Ctrl Pts',(0.881650403784437,-1.52706329386826,
-0.161458333333335));
#379026=CARTESIAN_POINT('Ctrl Pts',(1.32247560567666,-0.763531646934131,
-0.119791666666669));
#379027=CARTESIAN_POINT('Ctrl Pts',(1.76330080756888,1.96032512344098E-16,
-0.0781250000000018));
#379028=CARTESIAN_POINT('Ctrl Pts',(1.32247560567666,0.763531646934131,
-0.0364583333333345));
#379029=CARTESIAN_POINT('Ctrl Pts',(0.881650403784439,1.52706329386826,
0.00520833333333102));
#379030=CARTESIAN_POINT('Ctrl Pts',(0.,1.52706329386826,0.0468749999999983));
#379031=CARTESIAN_POINT('Ctrl Pts',(-0.881650403784438,1.52706329386826,
0.0885416666666656));
#379032=CARTESIAN_POINT('Ctrl Pts',(-1.32247560567666,0.763531646934132,
0.130208333333331));
#379033=CARTESIAN_POINT('Ctrl Pts',(-1.76330080756888,6.27916650328731E-16,
0.171874999999998));
#379034=CARTESIAN_POINT('Ctrl Pts',(-1.32247560567666,-0.76353164693413,
0.213541666666666));
#379035=CARTESIAN_POINT('Ctrl Pts',(-0.881650403784439,-1.52706329386826,
0.255208333333331));
#379036=CARTESIAN_POINT('Ctrl Pts',(-1.87011317493118E-16,-1.52706329386826,
0.296874999999999));
#379037=CARTESIAN_POINT('Ctrl Pts',(0.881650403784437,-1.52706329386826,
0.338541666666664));
#379038=CARTESIAN_POINT('Ctrl Pts',(1.32247560567666,-0.763531646934131,
0.380208333333331));
#379039=CARTESIAN_POINT('Ctrl Pts',(1.76330080756888,1.96032512344098E-16,
0.421874999999999));
#379040=CARTESIAN_POINT('Ctrl Pts',(1.32247560567666,0.763531646934131,
0.463541666666664));
#379041=CARTESIAN_POINT('Ctrl Pts',(0.881650403784439,1.52706329386826,
0.505208333333331));
#379042=CARTESIAN_POINT('Ctrl Pts',(0.,1.52706329386826,0.546874999999999));
#379043=CARTESIAN_POINT('Ctrl Pts',(-0.881650403784438,1.52706329386826,
0.588541666666664));
#379044=CARTESIAN_POINT('Ctrl Pts',(-1.32247560567666,0.763531646934132,
0.630208333333332));
#379045=CARTESIAN_POINT('Ctrl Pts',(-1.76330080756888,6.27916650328732E-16,
0.671874999999999));
#379046=CARTESIAN_POINT('Ctrl Pts',(-1.32247560567666,-0.76353164693413,
0.713541666666664));
#379047=CARTESIAN_POINT('Ctrl Pts',(-0.881650403784439,-1.52706329386826,
0.755208333333332));
#379048=CARTESIAN_POINT('Ctrl Pts',(-1.87011317493118E-16,-1.52706329386826,
0.796874999999999));
#379049=CARTESIAN_POINT('Ctrl Pts',(0.881650403784437,-1.52706329386826,
0.838541666666665));
#379050=CARTESIAN_POINT('Ctrl Pts',(1.32247560567666,-0.763531646934131,
0.880208333333332));
#379051=CARTESIAN_POINT('Ctrl Pts',(1.76330080756888,1.96032512344098E-16,
0.921874999999997));
#379052=CARTESIAN_POINT('Ctrl Pts',(1.32247560567666,0.763531646934131,
0.963541666666665));
#379053=CARTESIAN_POINT('Ctrl Pts',(0.881650403784439,1.52706329386826,
1.00520833333333));
#379054=CARTESIAN_POINT('Ctrl Pts',(0.,1.52706329386826,1.046875));
#379055=CARTESIAN_POINT('Ctrl Pts',(-0.881650403784438,1.52706329386826,
1.08854166666666));
#379056=CARTESIAN_POINT('Ctrl Pts',(-1.32247560567666,0.763531646934132,
1.13020833333333));
#379057=CARTESIAN_POINT('Ctrl Pts',(-1.76330080756888,6.27916650328732E-16,
1.171875));
#379058=CARTESIAN_POINT('Ctrl Pts',(-1.32247560567666,-0.76353164693413,
1.21354166666666));
#379059=CARTESIAN_POINT('Ctrl Pts',(-0.881650403784439,-1.52706329386826,
1.25520833333333));
#379060=CARTESIAN_POINT('Ctrl Pts',(-1.87011317493118E-16,-1.52706329386826,
1.296875));
#379061=CARTESIAN_POINT('Ctrl Pts',(0.881650403784437,-1.52706329386826,
1.33854166666667));
#379062=CARTESIAN_POINT('Ctrl Pts',(1.32247560567666,-0.763531646934131,
1.38020833333333));
#379063=CARTESIAN_POINT('Ctrl Pts',(1.76330080756888,1.96032512344098E-16,
1.421875));
#379064=CARTESIAN_POINT('Ctrl Pts',(1.32247560567666,0.763531646934131,
1.46354166666667));
#379065=CARTESIAN_POINT('Ctrl Pts',(0.881650403784439,1.52706329386826,
1.50520833333333));
#379066=CARTESIAN_POINT('Ctrl Pts',(0.,1.52706329386826,1.546875));
#379067=CARTESIAN_POINT('Ctrl Pts',(-0.881650403784438,1.52706329386826,
1.58854166666667));
#379068=CARTESIAN_POINT('Ctrl Pts',(-1.32247560567666,0.763531646934132,
1.63020833333333));
#379069=CARTESIAN_POINT('Ctrl Pts',(-1.76330080756888,6.27916650328732E-16,
1.671875));
#379070=CARTESIAN_POINT('Ctrl Pts',(-1.32247560567666,-0.76353164693413,
1.71354166666667));
#379071=CARTESIAN_POINT('Ctrl Pts',(-0.881650403784439,-1.52706329386826,
1.75520833333333));
#379072=CARTESIAN_POINT('Ctrl Pts',(-1.87011317493118E-16,-1.52706329386826,
1.796875));
#379073=CARTESIAN_POINT('Ctrl Pts',(0.881650403784437,-1.52706329386826,
1.83854166666667));
#379074=CARTESIAN_POINT('Ctrl Pts',(1.32247560567666,-0.763531646934131,
1.88020833333333));
#379075=CARTESIAN_POINT('Ctrl Pts',(1.76330080756888,1.96032512344098E-16,
1.921875));
#379076=CARTESIAN_POINT('Ctrl Pts',(1.32247560567666,0.763531646934131,
1.96354166666667));
#379077=CARTESIAN_POINT('Ctrl Pts',(0.881650403784439,1.52706329386826,
2.00520833333333));
#379078=CARTESIAN_POINT('Ctrl Pts',(0.,1.52706329386826,2.046875));
#379079=CARTESIAN_POINT('Ctrl Pts',(-0.881650403784438,1.52706329386826,
2.08854166666667));
#379080=CARTESIAN_POINT('Ctrl Pts',(-1.32247560567666,0.763531646934132,
2.13020833333333));
#379081=CARTESIAN_POINT('Ctrl Pts',(-1.76330080756888,6.27916650328732E-16,
2.171875));
#379082=CARTESIAN_POINT('Ctrl Pts',(-1.32247560567666,-0.76353164693413,
2.21354166666666));
#379083=CARTESIAN_POINT('Ctrl Pts',(-0.881650403784439,-1.52706329386826,
2.25520833333333));
#379084=CARTESIAN_POINT('Ctrl Pts',(-1.87011317493118E-16,-1.52706329386826,
2.296875));
#379085=CARTESIAN_POINT('Ctrl Pts',(0.881650403784437,-1.52706329386826,
2.33854166666666));
#379086=CARTESIAN_POINT('Ctrl Pts',(1.32247560567666,-0.763531646934131,
2.38020833333333));
#379087=CARTESIAN_POINT('Ctrl Pts',(1.76330080756888,1.96032512344098E-16,
2.421875));
#379088=CARTESIAN_POINT('Ctrl Pts',(1.32247560567666,0.763531646934131,
2.46354166666666));
#379089=CARTESIAN_POINT('Ctrl Pts',(0.881650403784439,1.52706329386826,
2.50520833333333));
#379090=CARTESIAN_POINT('Ctrl Pts',(0.,1.52706329386826,2.546875));
#379091=CARTESIAN_POINT('Ctrl Pts',(-0.881650403784438,1.52706329386826,
2.58854166666666));
#379092=CARTESIAN_POINT('Ctrl Pts',(-1.32247560567666,0.763531646934132,
2.63020833333333));
#379093=CARTESIAN_POINT('Ctrl Pts',(-1.76330080756888,6.27916650328732E-16,
2.671875));
#379094=CARTESIAN_POINT('Ctrl Pts',(-1.32247560567666,-0.76353164693413,
2.71354166666666));
#379095=CARTESIAN_POINT('Ctrl Pts',(-0.881650403784439,-1.52706329386826,
2.75520833333333));
#379096=CARTESIAN_POINT('Ctrl Pts',(-1.87011317493118E-16,-1.52706329386826,
2.796875));
#379097=CARTESIAN_POINT('Ctrl Pts',(0.881650403784437,-1.52706329386826,
2.83854166666666));
#379098=CARTESIAN_POINT('Ctrl Pts',(1.32247560567666,-0.763531646934131,
2.88020833333333));
#379099=CARTESIAN_POINT('Ctrl Pts',(1.76330080756888,1.96032512344098E-16,
2.921875));
#379100=CARTESIAN_POINT('Ctrl Pts',(1.32247560567666,0.763531646934131,
2.96354166666666));
#379101=CARTESIAN_POINT('Ctrl Pts',(0.881650403784439,1.52706329386826,
3.00520833333333));
#379102=CARTESIAN_POINT('Ctrl Pts',(0.,1.52706329386826,3.046875));
#379103=CARTESIAN_POINT('Ctrl Pts',(-0.881650403784438,1.52706329386826,
3.08854166666666));
#379104=CARTESIAN_POINT('Ctrl Pts',(-1.32247560567666,0.763531646934132,
3.13020833333333));
#379105=CARTESIAN_POINT('Ctrl Pts',(-1.76330080756888,6.27916650328732E-16,
3.171875));
#379106=CARTESIAN_POINT('Ctrl Pts',(-1.32247560567666,-0.76353164693413,
3.21354166666667));
#379107=CARTESIAN_POINT('Ctrl Pts',(-0.881650403784439,-1.52706329386826,
3.25520833333333));
#379108=CARTESIAN_POINT('Ctrl Pts',(-1.87011317493118E-16,-1.52706329386826,
3.296875));
#379109=CARTESIAN_POINT('Ctrl Pts',(0.881650403784437,-1.52706329386826,
3.33854166666667));
#379110=CARTESIAN_POINT('Ctrl Pts',(1.32247560567666,-0.763531646934131,
3.38020833333333));
#379111=CARTESIAN_POINT('Ctrl Pts',(1.76330080756888,1.96032512344098E-16,
3.421875));
#379112=CARTESIAN_POINT('Ctrl Pts',(1.32247560567666,0.763531646934131,
3.46354166666667));
#379113=CARTESIAN_POINT('Ctrl Pts',(0.881650403784439,1.52706329386826,
3.50520833333333));
#379114=CARTESIAN_POINT('Ctrl Pts',(0.,1.52706329386826,3.546875));
#379115=CARTESIAN_POINT('Ctrl Pts',(-0.881650403784438,1.52706329386826,
3.58854166666667));
#379116=CARTESIAN_POINT('Ctrl Pts',(-1.32247560567666,0.763531646934132,
3.63020833333333));
#379117=CARTESIAN_POINT('Ctrl Pts',(-1.76330080756888,6.27916650328732E-16,
3.671875));
#379118=CARTESIAN_POINT('Ctrl Pts',(-1.32247560567666,-0.76353164693413,
3.71354166666667));
#379119=CARTESIAN_POINT('Ctrl Pts',(-0.881650403784439,-1.52706329386826,
3.75520833333333));
#379120=CARTESIAN_POINT('Ctrl Pts',(-1.87011317493118E-16,-1.52706329386826,
3.796875));
#379121=CARTESIAN_POINT('Ctrl Pts',(0.881650403784437,-1.52706329386826,
3.83854166666667));
#379122=CARTESIAN_POINT('Ctrl Pts',(1.32247560567666,-0.763531646934131,
3.88020833333333));
#379123=CARTESIAN_POINT('Ctrl Pts',(1.76330080756888,1.96032512344098E-16,
3.921875));
#379124=CARTESIAN_POINT('Ctrl Pts',(1.32247560567666,0.763531646934131,
3.96354166666667));
#379125=CARTESIAN_POINT('Ctrl Pts',(0.881650403784439,1.52706329386826,
4.00520833333333));
#379126=CARTESIAN_POINT('Ctrl Pts',(0.,1.52706329386826,4.046875));
#379127=CARTESIAN_POINT('Ctrl Pts',(-0.881650403784438,1.52706329386826,
4.08854166666666));
#379128=CARTESIAN_POINT('Ctrl Pts',(-1.32247560567666,0.763531646934132,
4.13020833333333));
#379129=CARTESIAN_POINT('Ctrl Pts',(-1.76330080756888,6.27916650328732E-16,
4.171875));
#379130=CARTESIAN_POINT('Ctrl Pts',(-1.32247560567666,-0.76353164693413,
4.21354166666666));
#379131=CARTESIAN_POINT('Ctrl Pts',(-0.881650403784439,-1.52706329386826,
4.25520833333333));
#379132=CARTESIAN_POINT('Ctrl Pts',(-1.87011317493118E-16,-1.52706329386826,
4.296875));
#379133=CARTESIAN_POINT('Ctrl Pts',(0.881650403784437,-1.52706329386826,
4.33854166666666));
#379134=CARTESIAN_POINT('Ctrl Pts',(1.32247560567666,-0.763531646934131,
4.38020833333333));
#379135=CARTESIAN_POINT('Ctrl Pts',(1.76330080756888,1.96032512344098E-16,
4.421875));
#379136=CARTESIAN_POINT('Ctrl Pts',(1.32247560567666,0.763531646934131,
4.46354166666666));
#379137=CARTESIAN_POINT('Ctrl Pts',(0.881650403784439,1.52706329386826,
4.50520833333333));
#379138=CARTESIAN_POINT('Ctrl Pts',(0.,1.52706329386826,4.546875));
#379139=CARTESIAN_POINT('Ctrl Pts',(-0.881650403784438,1.52706329386826,
4.58854166666666));
#379140=CARTESIAN_POINT('Ctrl Pts',(-1.32247560567666,0.763531646934132,
4.63020833333333));
#379141=CARTESIAN_POINT('Ctrl Pts',(-1.76330080756888,6.27916650328732E-16,
4.671875));
#379142=CARTESIAN_POINT('Ctrl Pts',(-1.32247560567666,-0.76353164693413,
4.71354166666666));
#379143=CARTESIAN_POINT('Ctrl Pts',(-0.881650403784439,-1.52706329386826,
4.75520833333333));
#379144=CARTESIAN_POINT('Ctrl Pts',(-1.87011317493118E-16,-1.52706329386826,
4.796875));
#379145=CARTESIAN_POINT('Ctrl Pts',(0.881650403784437,-1.52706329386826,
4.83854166666667));
#379146=CARTESIAN_POINT('Ctrl Pts',(1.32247560567666,-0.763531646934131,
4.88020833333333));
#379147=CARTESIAN_POINT('Ctrl Pts',(1.76330080756888,1.96032512344098E-16,
4.921875));
#379148=CARTESIAN_POINT('Ctrl Pts',(1.32247560567666,0.763531646934131,
4.96354166666666));
#379149=CARTESIAN_POINT('Ctrl Pts',(0.881650403784439,1.52706329386826,
5.00520833333333));
#379150=CARTESIAN_POINT('Ctrl Pts',(0.,1.52706329386826,5.046875));
#379151=CARTESIAN_POINT('Ctrl Pts',(-0.881650403784438,1.52706329386826,
5.08854166666667));
#379152=CARTESIAN_POINT('Ctrl Pts',(-1.32247560567666,0.763531646934132,
5.13020833333333));
#379153=CARTESIAN_POINT('Ctrl Pts',(-1.76330080756888,6.27916650328732E-16,
5.171875));
#379154=CARTESIAN_POINT('Ctrl Pts',(-1.32247560567666,-0.76353164693413,
5.21354166666667));
#379155=CARTESIAN_POINT('Ctrl Pts',(-0.881650403784439,-1.52706329386826,
5.25520833333333));
#379156=CARTESIAN_POINT('Ctrl Pts',(-1.87011317493118E-16,-1.52706329386826,
5.296875));
#379157=CARTESIAN_POINT('Ctrl Pts',(0.881650403784437,-1.52706329386826,
5.33854166666667));
#379158=CARTESIAN_POINT('Ctrl Pts',(1.32247560567666,-0.763531646934131,
5.38020833333333));
#379159=CARTESIAN_POINT('Ctrl Pts',(1.76330080756888,1.96032512344098E-16,
5.421875));
#379160=CARTESIAN_POINT('Ctrl Pts',(1.32247560567666,0.763531646934131,
5.46354166666667));
#379161=CARTESIAN_POINT('Ctrl Pts',(0.881650403784439,1.52706329386826,
5.50520833333333));
#379162=CARTESIAN_POINT('Ctrl Pts',(0.,1.52706329386826,5.546875));
#379163=CARTESIAN_POINT('Ctrl Pts',(-0.881650403784438,1.52706329386826,
5.58854166666667));
#379164=CARTESIAN_POINT('Ctrl Pts',(-1.32247560567666,0.763531646934132,
5.63020833333333));
#379165=CARTESIAN_POINT('Ctrl Pts',(-1.76330080756888,6.27916650328732E-16,
5.671875));
#379166=CARTESIAN_POINT('Ctrl Pts',(-1.32247560567666,-0.76353164693413,
5.71354166666667));
#379167=CARTESIAN_POINT('Ctrl Pts',(-0.881650403784439,-1.52706329386826,
5.75520833333333));
#379168=CARTESIAN_POINT('Ctrl Pts',(-1.87011317493118E-16,-1.52706329386826,
5.796875));
#379169=CARTESIAN_POINT('Ctrl Pts',(0.881650403784437,-1.52706329386826,
5.83854166666667));
#379170=CARTESIAN_POINT('Ctrl Pts',(1.32247560567666,-0.763531646934131,
5.88020833333333));
#379171=CARTESIAN_POINT('Ctrl Pts',(1.76330080756888,1.96032512344098E-16,
5.921875));
#379172=CARTESIAN_POINT('Ctrl Pts',(1.32247560567666,0.763531646934131,
5.96354166666666));
#379173=CARTESIAN_POINT('Ctrl Pts',(0.881650403784439,1.52706329386826,
6.00520833333333));
#379174=CARTESIAN_POINT('Ctrl Pts',(0.,1.52706329386826,6.046875));
#379175=CARTESIAN_POINT('Ctrl Pts',(0.,1.52706329386826,-8.984375));
#379176=CARTESIAN_POINT('Ctrl Pts',(-0.881650403784438,1.52706329386826,
-8.94270833333333));
#379177=CARTESIAN_POINT('Ctrl Pts',(-1.32247560567666,0.763531646934132,
-8.90104166666666));
#379178=CARTESIAN_POINT('Ctrl Pts',(-1.76330080756888,6.27916650328731E-16,
-8.859375));
#379179=CARTESIAN_POINT('Ctrl Pts',(-1.32247560567666,-0.76353164693413,
-8.81770833333333));
#379180=CARTESIAN_POINT('Ctrl Pts',(-0.881650403784439,-1.52706329386826,
-8.77604166666666));
#379181=CARTESIAN_POINT('Ctrl Pts',(-1.87011317493118E-16,-1.52706329386826,
-8.734375));
#379182=CARTESIAN_POINT('Ctrl Pts',(0.881650403784437,-1.52706329386826,
-8.69270833333333));
#379183=CARTESIAN_POINT('Ctrl Pts',(1.32247560567666,-0.763531646934131,
-8.65104166666666));
#379184=CARTESIAN_POINT('Ctrl Pts',(1.76330080756888,1.96032512344098E-16,
-8.609375));
#379185=CARTESIAN_POINT('Ctrl Pts',(1.32247560567666,0.763531646934131,
-8.56770833333333));
#379186=CARTESIAN_POINT('Ctrl Pts',(0.881650403784439,1.52706329386826,
-8.52604166666666));
#379187=CARTESIAN_POINT('Ctrl Pts',(0.,1.52706329386826,-8.484375));
#379188=CARTESIAN_POINT('Ctrl Pts',(-0.881650403784438,1.52706329386826,
-8.44270833333333));
#379189=CARTESIAN_POINT('Ctrl Pts',(-1.32247560567666,0.763531646934132,
-8.40104166666666));
#379190=CARTESIAN_POINT('Ctrl Pts',(-1.76330080756888,6.27916650328731E-16,
-8.359375));
#379191=CARTESIAN_POINT('Ctrl Pts',(-1.32247560567666,-0.76353164693413,
-8.31770833333333));
#379192=CARTESIAN_POINT('Ctrl Pts',(-0.881650403784439,-1.52706329386826,
-8.27604166666666));
#379193=CARTESIAN_POINT('Ctrl Pts',(-1.87011317493118E-16,-1.52706329386826,
-8.234375));
#379194=CARTESIAN_POINT('Ctrl Pts',(0.881650403784437,-1.52706329386826,
-8.19270833333333));
#379195=CARTESIAN_POINT('Ctrl Pts',(1.32247560567666,-0.763531646934131,
-8.15104166666666));
#379196=CARTESIAN_POINT('Ctrl Pts',(1.76330080756888,1.96032512344098E-16,
-8.109375));
#379197=CARTESIAN_POINT('Ctrl Pts',(1.32247560567666,0.763531646934131,
-8.06770833333333));
#379198=CARTESIAN_POINT('Ctrl Pts',(0.881650403784439,1.52706329386826,
-8.02604166666666));
#379199=CARTESIAN_POINT('Ctrl Pts',(0.,1.52706329386826,-7.984375));
#379200=CARTESIAN_POINT('Ctrl Pts',(-0.881650403784438,1.52706329386826,
-7.94270833333333));
#379201=CARTESIAN_POINT('Ctrl Pts',(-1.32247560567666,0.763531646934132,
-7.90104166666667));
#379202=CARTESIAN_POINT('Ctrl Pts',(-1.76330080756888,6.27916650328731E-16,
-7.859375));
#379203=CARTESIAN_POINT('Ctrl Pts',(-1.32247560567666,-0.76353164693413,
-7.81770833333333));
#379204=CARTESIAN_POINT('Ctrl Pts',(-0.881650403784439,-1.52706329386826,
-7.77604166666666));
#379205=CARTESIAN_POINT('Ctrl Pts',(-1.87011317493118E-16,-1.52706329386826,
-7.734375));
#379206=CARTESIAN_POINT('Ctrl Pts',(0.881650403784437,-1.52706329386826,
-7.69270833333333));
#379207=CARTESIAN_POINT('Ctrl Pts',(1.32247560567666,-0.763531646934131,
-7.65104166666666));
#379208=CARTESIAN_POINT('Ctrl Pts',(1.76330080756888,1.96032512344098E-16,
-7.609375));
#379209=CARTESIAN_POINT('Ctrl Pts',(1.32247560567666,0.763531646934131,
-7.56770833333333));
#379210=CARTESIAN_POINT('Ctrl Pts',(0.881650403784439,1.52706329386826,
-7.52604166666667));
#379211=CARTESIAN_POINT('Ctrl Pts',(0.,1.52706329386826,-7.484375));
#379212=CARTESIAN_POINT('Ctrl Pts',(-0.881650403784438,1.52706329386826,
-7.44270833333333));
#379213=CARTESIAN_POINT('Ctrl Pts',(-1.32247560567666,0.763531646934132,
-7.40104166666666));
#379214=CARTESIAN_POINT('Ctrl Pts',(-1.76330080756888,6.27916650328731E-16,
-7.359375));
#379215=CARTESIAN_POINT('Ctrl Pts',(-1.32247560567666,-0.76353164693413,
-7.31770833333333));
#379216=CARTESIAN_POINT('Ctrl Pts',(-0.881650403784439,-1.52706329386826,
-7.27604166666667));
#379217=CARTESIAN_POINT('Ctrl Pts',(-1.87011317493118E-16,-1.52706329386826,
-7.234375));
#379218=CARTESIAN_POINT('Ctrl Pts',(0.881650403784437,-1.52706329386826,
-7.19270833333333));
#379219=CARTESIAN_POINT('Ctrl Pts',(1.32247560567666,-0.763531646934131,
-7.15104166666666));
#379220=CARTESIAN_POINT('Ctrl Pts',(1.76330080756888,1.96032512344098E-16,
-7.109375));
#379221=CARTESIAN_POINT('Ctrl Pts',(1.32247560567666,0.763531646934131,
-7.06770833333333));
#379222=CARTESIAN_POINT('Ctrl Pts',(0.881650403784439,1.52706329386826,
-7.02604166666667));
#379223=CARTESIAN_POINT('Ctrl Pts',(0.,1.52706329386826,-6.984375));
#379224=CARTESIAN_POINT('Ctrl Pts',(-0.881650403784438,1.52706329386826,
-6.94270833333333));
#379225=CARTESIAN_POINT('Ctrl Pts',(-1.32247560567666,0.763531646934132,
-6.90104166666667));
#379226=CARTESIAN_POINT('Ctrl Pts',(-1.76330080756888,6.27916650328731E-16,
-6.859375));
#379227=CARTESIAN_POINT('Ctrl Pts',(-1.32247560567666,-0.76353164693413,
-6.81770833333333));
#379228=CARTESIAN_POINT('Ctrl Pts',(-0.881650403784439,-1.52706329386826,
-6.77604166666667));
#379229=CARTESIAN_POINT('Ctrl Pts',(-1.87011317493118E-16,-1.52706329386826,
-6.734375));
#379230=CARTESIAN_POINT('Ctrl Pts',(0.881650403784437,-1.52706329386826,
-6.69270833333333));
#379231=CARTESIAN_POINT('Ctrl Pts',(1.32247560567666,-0.763531646934131,
-6.65104166666667));
#379232=CARTESIAN_POINT('Ctrl Pts',(1.76330080756888,1.96032512344098E-16,
-6.609375));
#379233=CARTESIAN_POINT('Ctrl Pts',(1.32247560567666,0.763531646934131,
-6.56770833333333));
#379234=CARTESIAN_POINT('Ctrl Pts',(0.881650403784439,1.52706329386826,
-6.52604166666666));
#379235=CARTESIAN_POINT('Ctrl Pts',(0.,1.52706329386826,-6.484375));
#379236=CARTESIAN_POINT('Ctrl Pts',(-0.881650403784438,1.52706329386826,
-6.44270833333333));
#379237=CARTESIAN_POINT('Ctrl Pts',(-1.32247560567666,0.763531646934132,
-6.40104166666666));
#379238=CARTESIAN_POINT('Ctrl Pts',(-1.76330080756888,6.27916650328731E-16,
-6.359375));
#379239=CARTESIAN_POINT('Ctrl Pts',(-1.32247560567666,-0.76353164693413,
-6.31770833333333));
#379240=CARTESIAN_POINT('Ctrl Pts',(-0.881650403784439,-1.52706329386826,
-6.27604166666667));
#379241=CARTESIAN_POINT('Ctrl Pts',(-1.87011317493118E-16,-1.52706329386826,
-6.234375));
#379242=CARTESIAN_POINT('Ctrl Pts',(0.881650403784437,-1.52706329386826,
-6.19270833333333));
#379243=CARTESIAN_POINT('Ctrl Pts',(1.32247560567666,-0.763531646934131,
-6.15104166666666));
#379244=CARTESIAN_POINT('Ctrl Pts',(1.76330080756888,1.96032512344098E-16,
-6.109375));
#379245=CARTESIAN_POINT('Ctrl Pts',(1.32247560567666,0.763531646934131,
-6.06770833333333));
#379246=CARTESIAN_POINT('Ctrl Pts',(0.881650403784439,1.52706329386826,
-6.02604166666666));
#379247=CARTESIAN_POINT('Ctrl Pts',(0.,1.52706329386826,-5.984375));
#379248=CARTESIAN_POINT('Ctrl Pts',(-0.881650403784438,1.52706329386826,
-5.94270833333333));
#379249=CARTESIAN_POINT('Ctrl Pts',(-1.32247560567666,0.763531646934132,
-5.90104166666666));
#379250=CARTESIAN_POINT('Ctrl Pts',(-1.76330080756888,6.27916650328731E-16,
-5.859375));
#379251=CARTESIAN_POINT('Ctrl Pts',(-1.32247560567666,-0.76353164693413,
-5.81770833333333));
#379252=CARTESIAN_POINT('Ctrl Pts',(-0.881650403784439,-1.52706329386826,
-5.77604166666666));
#379253=CARTESIAN_POINT('Ctrl Pts',(-1.87011317493118E-16,-1.52706329386826,
-5.734375));
#379254=CARTESIAN_POINT('Ctrl Pts',(0.881650403784437,-1.52706329386826,
-5.69270833333333));
#379255=CARTESIAN_POINT('Ctrl Pts',(1.32247560567666,-0.763531646934131,
-5.65104166666666));
#379256=CARTESIAN_POINT('Ctrl Pts',(1.76330080756888,1.96032512344098E-16,
-5.609375));
#379257=CARTESIAN_POINT('Ctrl Pts',(1.32247560567666,0.763531646934131,
-5.56770833333333));
#379258=CARTESIAN_POINT('Ctrl Pts',(0.881650403784439,1.52706329386826,
-5.52604166666666));
#379259=CARTESIAN_POINT('Ctrl Pts',(0.,1.52706329386826,-5.484375));
#379260=CARTESIAN_POINT('Ctrl Pts',(-0.881650403784438,1.52706329386826,
-5.44270833333333));
#379261=CARTESIAN_POINT('Ctrl Pts',(-1.32247560567666,0.763531646934132,
-5.40104166666667));
#379262=CARTESIAN_POINT('Ctrl Pts',(-1.76330080756888,6.27916650328731E-16,
-5.359375));
#379263=CARTESIAN_POINT('Ctrl Pts',(-1.32247560567666,-0.76353164693413,
-5.31770833333333));
#379264=CARTESIAN_POINT('Ctrl Pts',(-0.881650403784439,-1.52706329386826,
-5.27604166666666));
#379265=CARTESIAN_POINT('Ctrl Pts',(-1.87011317493118E-16,-1.52706329386826,
-5.234375));
#379266=CARTESIAN_POINT('Ctrl Pts',(0.881650403784437,-1.52706329386826,
-5.19270833333333));
#379267=CARTESIAN_POINT('Ctrl Pts',(1.32247560567666,-0.763531646934131,
-5.15104166666667));
#379268=CARTESIAN_POINT('Ctrl Pts',(1.76330080756888,1.96032512344098E-16,
-5.109375));
#379269=CARTESIAN_POINT('Ctrl Pts',(1.32247560567666,0.763531646934131,
-5.06770833333333));
#379270=CARTESIAN_POINT('Ctrl Pts',(0.881650403784439,1.52706329386826,
-5.02604166666667));
#379271=CARTESIAN_POINT('Ctrl Pts',(0.,1.52706329386826,-4.984375));
#379272=CARTESIAN_POINT('Ctrl Pts',(-0.881650403784438,1.52706329386826,
-4.94270833333333));
#379273=CARTESIAN_POINT('Ctrl Pts',(-1.32247560567666,0.763531646934132,
-4.90104166666666));
#379274=CARTESIAN_POINT('Ctrl Pts',(-1.76330080756888,6.27916650328731E-16,
-4.859375));
#379275=CARTESIAN_POINT('Ctrl Pts',(-1.32247560567666,-0.76353164693413,
-4.81770833333333));
#379276=CARTESIAN_POINT('Ctrl Pts',(-0.881650403784439,-1.52706329386826,
-4.77604166666667));
#379277=CARTESIAN_POINT('Ctrl Pts',(-1.87011317493118E-16,-1.52706329386826,
-4.734375));
#379278=CARTESIAN_POINT('Ctrl Pts',(0.881650403784437,-1.52706329386826,
-4.69270833333333));
#379279=CARTESIAN_POINT('Ctrl Pts',(1.32247560567666,-0.763531646934131,
-4.65104166666666));
#379280=CARTESIAN_POINT('Ctrl Pts',(1.76330080756888,1.96032512344098E-16,
-4.609375));
#379281=CARTESIAN_POINT('Ctrl Pts',(1.32247560567666,0.763531646934131,
-4.56770833333333));
#379282=CARTESIAN_POINT('Ctrl Pts',(0.881650403784439,1.52706329386826,
-4.52604166666666));
#379283=CARTESIAN_POINT('Ctrl Pts',(0.,1.52706329386826,-4.484375));
#379284=CARTESIAN_POINT('Ctrl Pts',(-0.881650403784438,1.52706329386826,
-4.44270833333333));
#379285=CARTESIAN_POINT('Ctrl Pts',(-1.32247560567666,0.763531646934132,
-4.40104166666666));
#379286=CARTESIAN_POINT('Ctrl Pts',(-1.76330080756888,6.27916650328731E-16,
-4.359375));
#379287=CARTESIAN_POINT('Ctrl Pts',(-1.32247560567666,-0.76353164693413,
-4.31770833333333));
#379288=CARTESIAN_POINT('Ctrl Pts',(-0.881650403784439,-1.52706329386826,
-4.27604166666666));
#379289=CARTESIAN_POINT('Ctrl Pts',(-1.87011317493118E-16,-1.52706329386826,
-4.234375));
#379290=CARTESIAN_POINT('Ctrl Pts',(0.881650403784437,-1.52706329386826,
-4.19270833333333));
#379291=CARTESIAN_POINT('Ctrl Pts',(1.32247560567666,-0.763531646934131,
-4.15104166666666));
#379292=CARTESIAN_POINT('Ctrl Pts',(1.76330080756888,1.96032512344098E-16,
-4.109375));
#379293=CARTESIAN_POINT('Ctrl Pts',(1.32247560567666,0.763531646934131,
-4.06770833333333));
#379294=CARTESIAN_POINT('Ctrl Pts',(0.881650403784439,1.52706329386826,
-4.02604166666666));
#379295=CARTESIAN_POINT('Ctrl Pts',(0.,1.52706329386826,-3.984375));
#379296=CARTESIAN_POINT('Ctrl Pts',(-0.881650403784438,1.52706329386826,
-3.94270833333333));
#379297=CARTESIAN_POINT('Ctrl Pts',(-1.32247560567666,0.763531646934132,
-3.90104166666666));
#379298=CARTESIAN_POINT('Ctrl Pts',(-1.76330080756888,6.27916650328731E-16,
-3.859375));
#379299=CARTESIAN_POINT('Ctrl Pts',(-1.32247560567666,-0.76353164693413,
-3.81770833333333));
#379300=CARTESIAN_POINT('Ctrl Pts',(-0.881650403784439,-1.52706329386826,
-3.77604166666667));
#379301=CARTESIAN_POINT('Ctrl Pts',(-1.87011317493118E-16,-1.52706329386826,
-3.734375));
#379302=CARTESIAN_POINT('Ctrl Pts',(0.881650403784437,-1.52706329386826,
-3.69270833333333));
#379303=CARTESIAN_POINT('Ctrl Pts',(1.32247560567666,-0.763531646934131,
-3.65104166666666));
#379304=CARTESIAN_POINT('Ctrl Pts',(1.76330080756888,1.96032512344098E-16,
-3.609375));
#379305=CARTESIAN_POINT('Ctrl Pts',(1.32247560567666,0.763531646934131,
-3.56770833333333));
#379306=CARTESIAN_POINT('Ctrl Pts',(0.881650403784439,1.52706329386826,
-3.52604166666666));
#379307=CARTESIAN_POINT('Ctrl Pts',(0.,1.52706329386826,-3.484375));
#379308=CARTESIAN_POINT('Ctrl Pts',(-0.881650403784438,1.52706329386826,
-3.44270833333333));
#379309=CARTESIAN_POINT('Ctrl Pts',(-1.32247560567666,0.763531646934132,
-3.40104166666666));
#379310=CARTESIAN_POINT('Ctrl Pts',(-1.76330080756888,6.27916650328731E-16,
-3.359375));
#379311=CARTESIAN_POINT('Ctrl Pts',(-1.32247560567666,-0.76353164693413,
-3.31770833333333));
#379312=CARTESIAN_POINT('Ctrl Pts',(-0.881650403784439,-1.52706329386826,
-3.27604166666666));
#379313=CARTESIAN_POINT('Ctrl Pts',(-1.87011317493118E-16,-1.52706329386826,
-3.234375));
#379314=CARTESIAN_POINT('Ctrl Pts',(0.881650403784437,-1.52706329386826,
-3.19270833333333));
#379315=CARTESIAN_POINT('Ctrl Pts',(1.32247560567666,-0.763531646934131,
-3.15104166666667));
#379316=CARTESIAN_POINT('Ctrl Pts',(1.76330080756888,1.96032512344098E-16,
-3.109375));
#379317=CARTESIAN_POINT('Ctrl Pts',(1.32247560567666,0.763531646934131,
-3.06770833333333));
#379318=CARTESIAN_POINT('Ctrl Pts',(0.881650403784439,1.52706329386826,
-3.02604166666667));
#379319=CARTESIAN_POINT('Ctrl Pts',(0.,1.52706329386826,-2.984375));
#379320=CARTESIAN_POINT('Ctrl Pts',(-0.881650403784438,1.52706329386826,
-2.94270833333333));
#379321=CARTESIAN_POINT('Ctrl Pts',(-1.32247560567666,0.763531646934132,
-2.90104166666667));
#379322=CARTESIAN_POINT('Ctrl Pts',(-1.76330080756888,6.27916650328731E-16,
-2.859375));
#379323=CARTESIAN_POINT('Ctrl Pts',(-1.32247560567666,-0.76353164693413,
-2.81770833333333));
#379324=CARTESIAN_POINT('Ctrl Pts',(-0.881650403784439,-1.52706329386826,
-2.77604166666666));
#379325=CARTESIAN_POINT('Ctrl Pts',(-1.87011317493118E-16,-1.52706329386826,
-2.734375));
#379326=CARTESIAN_POINT('Ctrl Pts',(0.881650403784437,-1.52706329386826,
-2.69270833333333));
#379327=CARTESIAN_POINT('Ctrl Pts',(1.32247560567666,-0.763531646934131,
-2.65104166666666));
#379328=CARTESIAN_POINT('Ctrl Pts',(1.76330080756888,1.96032512344098E-16,
-2.609375));
#379329=CARTESIAN_POINT('Ctrl Pts',(1.32247560567666,0.763531646934131,
-2.56770833333333));
#379330=CARTESIAN_POINT('Ctrl Pts',(0.881650403784439,1.52706329386826,
-2.52604166666666));
#379331=CARTESIAN_POINT('Ctrl Pts',(0.,1.52706329386826,-2.484375));
#379332=CARTESIAN_POINT('Ctrl Pts',(-0.881650403784438,1.52706329386826,
-2.44270833333333));
#379333=CARTESIAN_POINT('Ctrl Pts',(-1.32247560567666,0.763531646934132,
-2.40104166666666));
#379334=CARTESIAN_POINT('Ctrl Pts',(-1.76330080756888,6.27916650328731E-16,
-2.359375));
#379335=CARTESIAN_POINT('Ctrl Pts',(-1.32247560567666,-0.76353164693413,
-2.31770833333333));
#379336=CARTESIAN_POINT('Ctrl Pts',(-0.881650403784439,-1.52706329386826,
-2.27604166666666));
#379337=CARTESIAN_POINT('Ctrl Pts',(-1.87011317493118E-16,-1.52706329386826,
-2.234375));
#379338=CARTESIAN_POINT('Ctrl Pts',(0.881650403784437,-1.52706329386826,
-2.19270833333333));
#379339=CARTESIAN_POINT('Ctrl Pts',(1.32247560567666,-0.763531646934131,
-2.15104166666666));
#379340=CARTESIAN_POINT('Ctrl Pts',(1.76330080756888,1.96032512344098E-16,
-2.109375));
#379341=CARTESIAN_POINT('Ctrl Pts',(1.32247560567666,0.763531646934131,
-2.06770833333333));
#379342=CARTESIAN_POINT('Ctrl Pts',(0.881650403784439,1.52706329386826,
-2.02604166666666));
#379343=CARTESIAN_POINT('Ctrl Pts',(0.,1.52706329386826,-1.984375));
#379344=CARTESIAN_POINT('Ctrl Pts',(-0.881650403784438,1.52706329386826,
-1.94270833333333));
#379345=CARTESIAN_POINT('Ctrl Pts',(-1.32247560567666,0.763531646934132,
-1.90104166666666));
#379346=CARTESIAN_POINT('Ctrl Pts',(-1.76330080756888,6.27916650328731E-16,
-1.859375));
#379347=CARTESIAN_POINT('Ctrl Pts',(-1.32247560567666,-0.76353164693413,
-1.81770833333333));
#379348=CARTESIAN_POINT('Ctrl Pts',(-0.881650403784439,-1.52706329386826,
-1.77604166666666));
#379349=CARTESIAN_POINT('Ctrl Pts',(-1.87011317493118E-16,-1.52706329386826,
-1.734375));
#379350=CARTESIAN_POINT('Ctrl Pts',(0.881650403784437,-1.52706329386826,
-1.69270833333333));
#379351=CARTESIAN_POINT('Ctrl Pts',(1.32247560567666,-0.763531646934131,
-1.65104166666666));
#379352=CARTESIAN_POINT('Ctrl Pts',(1.76330080756888,1.96032512344098E-16,
-1.609375));
#379353=CARTESIAN_POINT('Ctrl Pts',(1.32247560567666,0.763531646934131,
-1.56770833333333));
#379354=CARTESIAN_POINT('Ctrl Pts',(0.881650403784439,1.52706329386826,
-1.52604166666666));
#379355=CARTESIAN_POINT('Ctrl Pts',(0.,1.52706329386826,-1.484375));
#379356=CARTESIAN_POINT('Ctrl Pts',(-0.881650403784438,1.52706329386826,
-1.44270833333333));
#379357=CARTESIAN_POINT('Ctrl Pts',(-1.32247560567666,0.763531646934132,
-1.40104166666666));
#379358=CARTESIAN_POINT('Ctrl Pts',(-1.76330080756888,6.27916650328731E-16,
-1.359375));
#379359=CARTESIAN_POINT('Ctrl Pts',(-1.32247560567666,-0.76353164693413,
-1.31770833333333));
#379360=CARTESIAN_POINT('Ctrl Pts',(-0.881650403784439,-1.52706329386826,
-1.27604166666666));
#379361=CARTESIAN_POINT('Ctrl Pts',(-1.87011317493118E-16,-1.52706329386826,
-1.234375));
#379362=CARTESIAN_POINT('Ctrl Pts',(0.881650403784437,-1.52706329386826,
-1.19270833333333));
#379363=CARTESIAN_POINT('Ctrl Pts',(1.32247560567666,-0.763531646934131,
-1.15104166666666));
#379364=CARTESIAN_POINT('Ctrl Pts',(1.76330080756888,1.96032512344098E-16,
-1.109375));
#379365=CARTESIAN_POINT('Ctrl Pts',(1.32247560567666,0.763531646934131,
-1.06770833333333));
#379366=CARTESIAN_POINT('Ctrl Pts',(0.881650403784439,1.52706329386826,
-1.02604166666666));
#379367=CARTESIAN_POINT('Ctrl Pts',(0.,1.52706329386826,-0.984374999999997));
#379368=CARTESIAN_POINT('Ctrl Pts',(-0.881650403784438,1.52706329386826,
-0.942708333333332));
#379369=CARTESIAN_POINT('Ctrl Pts',(-1.32247560567666,0.763531646934132,
-0.901041666666665));
#379370=CARTESIAN_POINT('Ctrl Pts',(-1.76330080756888,6.27916650328731E-16,
-0.859374999999997));
#379371=CARTESIAN_POINT('Ctrl Pts',(-1.32247560567666,-0.76353164693413,
-0.817708333333332));
#379372=CARTESIAN_POINT('Ctrl Pts',(-0.881650403784439,-1.52706329386826,
-0.776041666666665));
#379373=CARTESIAN_POINT('Ctrl Pts',(-1.87011317493118E-16,-1.52706329386826,
-0.734374999999997));
#379374=CARTESIAN_POINT('Ctrl Pts',(0.881650403784437,-1.52706329386826,
-0.692708333333332));
#379375=CARTESIAN_POINT('Ctrl Pts',(1.32247560567666,-0.763531646934131,
-0.651041666666664));
#379376=CARTESIAN_POINT('Ctrl Pts',(1.76330080756888,1.96032512344098E-16,
-0.609374999999997));
#379377=CARTESIAN_POINT('Ctrl Pts',(1.32247560567666,0.763531646934131,
-0.567708333333331));
#379378=CARTESIAN_POINT('Ctrl Pts',(0.881650403784439,1.52706329386826,
-0.526041666666664));
#379379=CARTESIAN_POINT('Ctrl Pts',(0.,1.52706329386826,-0.484374999999999));
#379380=CARTESIAN_POINT('Ctrl Pts',(-0.881650403784438,1.52706329386826,
-0.442708333333331));
#379381=CARTESIAN_POINT('Ctrl Pts',(-1.32247560567666,0.763531646934132,
-0.401041666666664));
#379382=CARTESIAN_POINT('Ctrl Pts',(-1.76330080756888,6.27916650328731E-16,
-0.359374999999999));
#379383=CARTESIAN_POINT('Ctrl Pts',(-1.32247560567666,-0.76353164693413,
-0.317708333333331));
#379384=CARTESIAN_POINT('Ctrl Pts',(-0.881650403784439,-1.52706329386826,
-0.276041666666664));
#379385=CARTESIAN_POINT('Ctrl Pts',(-1.87011317493118E-16,-1.52706329386826,
-0.234374999999998));
#379386=CARTESIAN_POINT('Ctrl Pts',(0.881650403784437,-1.52706329386826,
-0.192708333333331));
#379387=CARTESIAN_POINT('Ctrl Pts',(1.32247560567666,-0.763531646934131,
-0.151041666666664));
#379388=CARTESIAN_POINT('Ctrl Pts',(1.76330080756888,1.96032512344098E-16,
-0.109374999999998));
#379389=CARTESIAN_POINT('Ctrl Pts',(1.32247560567666,0.763531646934131,
-0.0677083333333311));
#379390=CARTESIAN_POINT('Ctrl Pts',(0.881650403784439,1.52706329386826,
-0.0260416666666638));
#379391=CARTESIAN_POINT('Ctrl Pts',(0.,1.52706329386826,0.0156250000000017));
#379392=CARTESIAN_POINT('Ctrl Pts',(-0.881650403784438,1.52706329386826,
0.057291666666669));
#379393=CARTESIAN_POINT('Ctrl Pts',(-1.32247560567666,0.763531646934132,
0.0989583333333363));
#379394=CARTESIAN_POINT('Ctrl Pts',(-1.76330080756888,6.27916650328731E-16,
0.140625000000002));
#379395=CARTESIAN_POINT('Ctrl Pts',(-1.32247560567666,-0.76353164693413,
0.182291666666669));
#379396=CARTESIAN_POINT('Ctrl Pts',(-0.881650403784439,-1.52706329386826,
0.223958333333335));
#379397=CARTESIAN_POINT('Ctrl Pts',(-1.87011317493118E-16,-1.52706329386826,
0.265625000000002));
#379398=CARTESIAN_POINT('Ctrl Pts',(0.881650403784437,-1.52706329386826,
0.307291666666669));
#379399=CARTESIAN_POINT('Ctrl Pts',(1.32247560567666,-0.763531646934131,
0.348958333333335));
#379400=CARTESIAN_POINT('Ctrl Pts',(1.76330080756888,1.96032512344098E-16,
0.390625000000002));
#379401=CARTESIAN_POINT('Ctrl Pts',(1.32247560567666,0.763531646934131,
0.432291666666669));
#379402=CARTESIAN_POINT('Ctrl Pts',(0.881650403784439,1.52706329386826,
0.473958333333335));
#379403=CARTESIAN_POINT('Ctrl Pts',(0.,1.52706329386826,0.515625000000002));
#379404=CARTESIAN_POINT('Ctrl Pts',(-0.881650403784438,1.52706329386826,
0.55729166666667));
#379405=CARTESIAN_POINT('Ctrl Pts',(-1.32247560567666,0.763531646934132,
0.598958333333335));
#379406=CARTESIAN_POINT('Ctrl Pts',(-1.76330080756888,6.27916650328731E-16,
0.640625000000002));
#379407=CARTESIAN_POINT('Ctrl Pts',(-1.32247560567666,-0.76353164693413,
0.68229166666667));
#379408=CARTESIAN_POINT('Ctrl Pts',(-0.881650403784439,-1.52706329386826,
0.723958333333335));
#379409=CARTESIAN_POINT('Ctrl Pts',(-1.87011317493118E-16,-1.52706329386826,
0.765625000000003));
#379410=CARTESIAN_POINT('Ctrl Pts',(0.881650403784437,-1.52706329386826,
0.807291666666668));
#379411=CARTESIAN_POINT('Ctrl Pts',(1.32247560567666,-0.763531646934131,
0.848958333333335));
#379412=CARTESIAN_POINT('Ctrl Pts',(1.76330080756888,1.96032512344098E-16,
0.890625000000003));
#379413=CARTESIAN_POINT('Ctrl Pts',(1.32247560567666,0.763531646934131,
0.932291666666668));
#379414=CARTESIAN_POINT('Ctrl Pts',(0.881650403784439,1.52706329386826,
0.973958333333336));
#379415=CARTESIAN_POINT('Ctrl Pts',(0.,1.52706329386826,1.015625));
#379416=CARTESIAN_POINT('Ctrl Pts',(-0.881650403784438,1.52706329386826,
1.05729166666667));
#379417=CARTESIAN_POINT('Ctrl Pts',(-1.32247560567666,0.763531646934132,
1.09895833333334));
#379418=CARTESIAN_POINT('Ctrl Pts',(-1.76330080756888,6.27916650328732E-16,
1.140625));
#379419=CARTESIAN_POINT('Ctrl Pts',(-1.32247560567666,-0.76353164693413,
1.18229166666667));
#379420=CARTESIAN_POINT('Ctrl Pts',(-0.881650403784439,-1.52706329386826,
1.22395833333334));
#379421=CARTESIAN_POINT('Ctrl Pts',(-1.87011317493118E-16,-1.52706329386826,
1.265625));
#379422=CARTESIAN_POINT('Ctrl Pts',(0.881650403784437,-1.52706329386826,
1.30729166666667));
#379423=CARTESIAN_POINT('Ctrl Pts',(1.32247560567666,-0.763531646934131,
1.34895833333334));
#379424=CARTESIAN_POINT('Ctrl Pts',(1.76330080756888,1.96032512344098E-16,
1.390625));
#379425=CARTESIAN_POINT('Ctrl Pts',(1.32247560567666,0.763531646934131,
1.43229166666667));
#379426=CARTESIAN_POINT('Ctrl Pts',(0.881650403784439,1.52706329386826,
1.47395833333334));
#379427=CARTESIAN_POINT('Ctrl Pts',(0.,1.52706329386826,1.515625));
#379428=CARTESIAN_POINT('Ctrl Pts',(-0.881650403784438,1.52706329386826,
1.55729166666667));
#379429=CARTESIAN_POINT('Ctrl Pts',(-1.32247560567666,0.763531646934132,
1.59895833333334));
#379430=CARTESIAN_POINT('Ctrl Pts',(-1.76330080756888,6.27916650328732E-16,
1.640625));
#379431=CARTESIAN_POINT('Ctrl Pts',(-1.32247560567666,-0.76353164693413,
1.68229166666667));
#379432=CARTESIAN_POINT('Ctrl Pts',(-0.881650403784439,-1.52706329386826,
1.72395833333334));
#379433=CARTESIAN_POINT('Ctrl Pts',(-1.87011317493118E-16,-1.52706329386826,
1.765625));
#379434=CARTESIAN_POINT('Ctrl Pts',(0.881650403784437,-1.52706329386826,
1.80729166666667));
#379435=CARTESIAN_POINT('Ctrl Pts',(1.32247560567666,-0.763531646934131,
1.84895833333334));
#379436=CARTESIAN_POINT('Ctrl Pts',(1.76330080756888,1.96032512344098E-16,
1.890625));
#379437=CARTESIAN_POINT('Ctrl Pts',(1.32247560567666,0.763531646934131,
1.93229166666667));
#379438=CARTESIAN_POINT('Ctrl Pts',(0.881650403784439,1.52706329386826,
1.97395833333334));
#379439=CARTESIAN_POINT('Ctrl Pts',(0.,1.52706329386826,2.015625));
#379440=CARTESIAN_POINT('Ctrl Pts',(-0.881650403784438,1.52706329386826,
2.05729166666667));
#379441=CARTESIAN_POINT('Ctrl Pts',(-1.32247560567666,0.763531646934132,
2.09895833333333));
#379442=CARTESIAN_POINT('Ctrl Pts',(-1.76330080756888,6.27916650328732E-16,
2.140625));
#379443=CARTESIAN_POINT('Ctrl Pts',(-1.32247560567666,-0.76353164693413,
2.18229166666667));
#379444=CARTESIAN_POINT('Ctrl Pts',(-0.881650403784439,-1.52706329386826,
2.22395833333333));
#379445=CARTESIAN_POINT('Ctrl Pts',(-1.87011317493118E-16,-1.52706329386826,
2.265625));
#379446=CARTESIAN_POINT('Ctrl Pts',(0.881650403784437,-1.52706329386826,
2.30729166666667));
#379447=CARTESIAN_POINT('Ctrl Pts',(1.32247560567666,-0.763531646934131,
2.34895833333333));
#379448=CARTESIAN_POINT('Ctrl Pts',(1.76330080756888,1.96032512344098E-16,
2.390625));
#379449=CARTESIAN_POINT('Ctrl Pts',(1.32247560567666,0.763531646934131,
2.43229166666667));
#379450=CARTESIAN_POINT('Ctrl Pts',(0.881650403784439,1.52706329386826,
2.47395833333333));
#379451=CARTESIAN_POINT('Ctrl Pts',(0.,1.52706329386826,2.515625));
#379452=CARTESIAN_POINT('Ctrl Pts',(-0.881650403784438,1.52706329386826,
2.55729166666667));
#379453=CARTESIAN_POINT('Ctrl Pts',(-1.32247560567666,0.763531646934132,
2.59895833333334));
#379454=CARTESIAN_POINT('Ctrl Pts',(-1.76330080756888,6.27916650328732E-16,
2.640625));
#379455=CARTESIAN_POINT('Ctrl Pts',(-1.32247560567666,-0.76353164693413,
2.68229166666667));
#379456=CARTESIAN_POINT('Ctrl Pts',(-0.881650403784439,-1.52706329386826,
2.72395833333334));
#379457=CARTESIAN_POINT('Ctrl Pts',(-1.87011317493118E-16,-1.52706329386826,
2.765625));
#379458=CARTESIAN_POINT('Ctrl Pts',(0.881650403784437,-1.52706329386826,
2.80729166666667));
#379459=CARTESIAN_POINT('Ctrl Pts',(1.32247560567666,-0.763531646934131,
2.84895833333334));
#379460=CARTESIAN_POINT('Ctrl Pts',(1.76330080756888,1.96032512344098E-16,
2.890625));
#379461=CARTESIAN_POINT('Ctrl Pts',(1.32247560567666,0.763531646934131,
2.93229166666667));
#379462=CARTESIAN_POINT('Ctrl Pts',(0.881650403784439,1.52706329386826,
2.97395833333334));
#379463=CARTESIAN_POINT('Ctrl Pts',(0.,1.52706329386826,3.015625));
#379464=CARTESIAN_POINT('Ctrl Pts',(-0.881650403784438,1.52706329386826,
3.05729166666667));
#379465=CARTESIAN_POINT('Ctrl Pts',(-1.32247560567666,0.763531646934132,
3.09895833333334));
#379466=CARTESIAN_POINT('Ctrl Pts',(-1.76330080756888,6.27916650328732E-16,
3.140625));
#379467=CARTESIAN_POINT('Ctrl Pts',(-1.32247560567666,-0.76353164693413,
3.18229166666667));
#379468=CARTESIAN_POINT('Ctrl Pts',(-0.881650403784439,-1.52706329386826,
3.22395833333334));
#379469=CARTESIAN_POINT('Ctrl Pts',(-1.87011317493118E-16,-1.52706329386826,
3.265625));
#379470=CARTESIAN_POINT('Ctrl Pts',(0.881650403784437,-1.52706329386826,
3.30729166666667));
#379471=CARTESIAN_POINT('Ctrl Pts',(1.32247560567666,-0.763531646934131,
3.34895833333334));
#379472=CARTESIAN_POINT('Ctrl Pts',(1.76330080756888,1.96032512344098E-16,
3.390625));
#379473=CARTESIAN_POINT('Ctrl Pts',(1.32247560567666,0.763531646934131,
3.43229166666667));
#379474=CARTESIAN_POINT('Ctrl Pts',(0.881650403784439,1.52706329386826,
3.47395833333334));
#379475=CARTESIAN_POINT('Ctrl Pts',(0.,1.52706329386826,3.515625));
#379476=CARTESIAN_POINT('Ctrl Pts',(-0.881650403784438,1.52706329386826,
3.55729166666667));
#379477=CARTESIAN_POINT('Ctrl Pts',(-1.32247560567666,0.763531646934132,
3.59895833333334));
#379478=CARTESIAN_POINT('Ctrl Pts',(-1.76330080756888,6.27916650328732E-16,
3.640625));
#379479=CARTESIAN_POINT('Ctrl Pts',(-1.32247560567666,-0.76353164693413,
3.68229166666667));
#379480=CARTESIAN_POINT('Ctrl Pts',(-0.881650403784439,-1.52706329386826,
3.72395833333334));
#379481=CARTESIAN_POINT('Ctrl Pts',(-1.87011317493118E-16,-1.52706329386826,
3.765625));
#379482=CARTESIAN_POINT('Ctrl Pts',(0.881650403784437,-1.52706329386826,
3.80729166666667));
#379483=CARTESIAN_POINT('Ctrl Pts',(1.32247560567666,-0.763531646934131,
3.84895833333334));
#379484=CARTESIAN_POINT('Ctrl Pts',(1.76330080756888,1.96032512344098E-16,
3.890625));
#379485=CARTESIAN_POINT('Ctrl Pts',(1.32247560567666,0.763531646934131,
3.93229166666667));
#379486=CARTESIAN_POINT('Ctrl Pts',(0.881650403784439,1.52706329386826,
3.97395833333333));
#379487=CARTESIAN_POINT('Ctrl Pts',(0.,1.52706329386826,4.015625));
#379488=CARTESIAN_POINT('Ctrl Pts',(-0.881650403784438,1.52706329386826,
4.05729166666667));
#379489=CARTESIAN_POINT('Ctrl Pts',(-1.32247560567666,0.763531646934132,
4.09895833333333));
#379490=CARTESIAN_POINT('Ctrl Pts',(-1.76330080756888,6.27916650328732E-16,
4.140625));
#379491=CARTESIAN_POINT('Ctrl Pts',(-1.32247560567666,-0.76353164693413,
4.18229166666667));
#379492=CARTESIAN_POINT('Ctrl Pts',(-0.881650403784439,-1.52706329386826,
4.22395833333334));
#379493=CARTESIAN_POINT('Ctrl Pts',(-1.87011317493118E-16,-1.52706329386826,
4.265625));
#379494=CARTESIAN_POINT('Ctrl Pts',(0.881650403784437,-1.52706329386826,
4.30729166666667));
#379495=CARTESIAN_POINT('Ctrl Pts',(1.32247560567666,-0.763531646934131,
4.34895833333333));
#379496=CARTESIAN_POINT('Ctrl Pts',(1.76330080756888,1.96032512344098E-16,
4.390625));
#379497=CARTESIAN_POINT('Ctrl Pts',(1.32247560567666,0.763531646934131,
4.43229166666667));
#379498=CARTESIAN_POINT('Ctrl Pts',(0.881650403784439,1.52706329386826,
4.47395833333333));
#379499=CARTESIAN_POINT('Ctrl Pts',(0.,1.52706329386826,4.515625));
#379500=CARTESIAN_POINT('Ctrl Pts',(-0.881650403784438,1.52706329386826,
4.55729166666667));
#379501=CARTESIAN_POINT('Ctrl Pts',(-1.32247560567666,0.763531646934132,
4.59895833333333));
#379502=CARTESIAN_POINT('Ctrl Pts',(-1.76330080756888,6.27916650328732E-16,
4.640625));
#379503=CARTESIAN_POINT('Ctrl Pts',(-1.32247560567666,-0.76353164693413,
4.68229166666667));
#379504=CARTESIAN_POINT('Ctrl Pts',(-0.881650403784439,-1.52706329386826,
4.72395833333334));
#379505=CARTESIAN_POINT('Ctrl Pts',(-1.87011317493118E-16,-1.52706329386826,
4.765625));
#379506=CARTESIAN_POINT('Ctrl Pts',(0.881650403784437,-1.52706329386826,
4.80729166666667));
#379507=CARTESIAN_POINT('Ctrl Pts',(1.32247560567666,-0.763531646934131,
4.84895833333334));
#379508=CARTESIAN_POINT('Ctrl Pts',(1.76330080756888,1.96032512344098E-16,
4.890625));
#379509=CARTESIAN_POINT('Ctrl Pts',(1.32247560567666,0.763531646934131,
4.93229166666667));
#379510=CARTESIAN_POINT('Ctrl Pts',(0.881650403784439,1.52706329386826,
4.97395833333334));
#379511=CARTESIAN_POINT('Ctrl Pts',(0.,1.52706329386826,5.015625));
#379512=CARTESIAN_POINT('Ctrl Pts',(-0.881650403784438,1.52706329386826,
5.05729166666667));
#379513=CARTESIAN_POINT('Ctrl Pts',(-1.32247560567666,0.763531646934132,
5.09895833333334));
#379514=CARTESIAN_POINT('Ctrl Pts',(-1.76330080756888,6.27916650328732E-16,
5.140625));
#379515=CARTESIAN_POINT('Ctrl Pts',(-1.32247560567666,-0.76353164693413,
5.18229166666667));
#379516=CARTESIAN_POINT('Ctrl Pts',(-0.881650403784439,-1.52706329386826,
5.22395833333334));
#379517=CARTESIAN_POINT('Ctrl Pts',(-1.87011317493118E-16,-1.52706329386826,
5.265625));
#379518=CARTESIAN_POINT('Ctrl Pts',(0.881650403784437,-1.52706329386826,
5.30729166666667));
#379519=CARTESIAN_POINT('Ctrl Pts',(1.32247560567666,-0.763531646934131,
5.34895833333334));
#379520=CARTESIAN_POINT('Ctrl Pts',(1.76330080756888,1.96032512344098E-16,
5.390625));
#379521=CARTESIAN_POINT('Ctrl Pts',(1.32247560567666,0.763531646934131,
5.43229166666667));
#379522=CARTESIAN_POINT('Ctrl Pts',(0.881650403784439,1.52706329386826,
5.47395833333334));
#379523=CARTESIAN_POINT('Ctrl Pts',(0.,1.52706329386826,5.515625));
#379524=CARTESIAN_POINT('Ctrl Pts',(-0.881650403784438,1.52706329386826,
5.55729166666667));
#379525=CARTESIAN_POINT('Ctrl Pts',(-1.32247560567666,0.763531646934132,
5.59895833333334));
#379526=CARTESIAN_POINT('Ctrl Pts',(-1.76330080756888,6.27916650328732E-16,
5.640625));
#379527=CARTESIAN_POINT('Ctrl Pts',(-1.32247560567666,-0.76353164693413,
5.68229166666667));
#379528=CARTESIAN_POINT('Ctrl Pts',(-0.881650403784439,-1.52706329386826,
5.72395833333334));
#379529=CARTESIAN_POINT('Ctrl Pts',(-1.87011317493118E-16,-1.52706329386826,
5.765625));
#379530=CARTESIAN_POINT('Ctrl Pts',(0.881650403784437,-1.52706329386826,
5.80729166666667));
#379531=CARTESIAN_POINT('Ctrl Pts',(1.32247560567666,-0.763531646934131,
5.84895833333333));
#379532=CARTESIAN_POINT('Ctrl Pts',(1.76330080756888,1.96032512344098E-16,
5.890625));
#379533=CARTESIAN_POINT('Ctrl Pts',(1.32247560567666,0.763531646934131,
5.93229166666667));
#379534=CARTESIAN_POINT('Ctrl Pts',(0.881650403784439,1.52706329386826,
5.97395833333333));
#379535=CARTESIAN_POINT('Ctrl Pts',(0.,1.52706329386826,6.015625));
#379536=CARTESIAN_POINT('Ctrl Pts',(-0.881650403784438,1.52706329386826,
6.05729166666667));
#379537=CARTESIAN_POINT('Ctrl Pts',(-1.32247560567666,0.763531646934132,
6.09895833333334));
#379538=CARTESIAN_POINT('Ctrl Pts',(-1.76330080756888,6.27916650328732E-16,
6.140625));
#379539=CARTESIAN_POINT('Ctrl Pts',(-1.32247560567666,-0.76353164693413,
6.18229166666667));
#379540=CARTESIAN_POINT('Ctrl Pts',(-0.881650403784439,-1.52706329386826,
6.22395833333333));
#379541=CARTESIAN_POINT('Ctrl Pts',(-1.87011317493118E-16,-1.52706329386826,
6.265625));
#379542=CARTESIAN_POINT('Ctrl Pts',(0.881650403784437,-1.52706329386826,
6.30729166666667));
#379543=CARTESIAN_POINT('Ctrl Pts',(1.32247560567666,-0.763531646934131,
6.34895833333334));
#379544=CARTESIAN_POINT('Ctrl Pts',(1.76330080756888,1.96032512344098E-16,
6.390625));
#379545=CARTESIAN_POINT('Ctrl Pts',(1.32247560567666,0.763531646934131,
6.43229166666667));
#379546=CARTESIAN_POINT('Ctrl Pts',(0.881650403784439,1.52706329386826,
6.47395833333333));
#379547=CARTESIAN_POINT('Ctrl Pts',(0.,1.52706329386826,6.515625));
#379548=CARTESIAN_POINT('Ctrl Pts',(0.,1.17523182375213,-9.18750499398093));
#379549=CARTESIAN_POINT('Ctrl Pts',(-0.678520409803505,1.17523182375213,
-9.14583832731426));
#379550=CARTESIAN_POINT('Ctrl Pts',(-1.01778061470526,0.587615911876064,
-9.1041716606476));
#379551=CARTESIAN_POINT('Ctrl Pts',(-1.35704081960701,6.03040400634774E-16,
-9.06250499398093));
#379552=CARTESIAN_POINT('Ctrl Pts',(-1.01778061470526,-0.587615911876062,
-9.02083832731427));
#379553=CARTESIAN_POINT('Ctrl Pts',(-0.678520409803505,-1.17523182375213,
-8.9791716606476));
#379554=CARTESIAN_POINT('Ctrl Pts',(-1.43924389121415E-16,-1.17523182375213,
-8.93750499398093));
#379555=CARTESIAN_POINT('Ctrl Pts',(0.678520409803504,-1.17523182375213,
-8.89583832731427));
#379556=CARTESIAN_POINT('Ctrl Pts',(1.01778061470526,-0.587615911876063,
-8.8541716606476));
#379557=CARTESIAN_POINT('Ctrl Pts',(1.35704081960701,2.70661261425969E-16,
-8.81250499398093));
#379558=CARTESIAN_POINT('Ctrl Pts',(1.01778061470526,0.587615911876063,
-8.77083832731427));
#379559=CARTESIAN_POINT('Ctrl Pts',(0.678520409803506,1.17523182375213,
-8.7291716606476));
#379560=CARTESIAN_POINT('Ctrl Pts',(0.,1.17523182375213,-8.68750499398093));
#379561=CARTESIAN_POINT('Ctrl Pts',(-0.678520409803505,1.17523182375213,
-8.64583832731427));
#379562=CARTESIAN_POINT('Ctrl Pts',(-1.01778061470526,0.587615911876064,
-8.6041716606476));
#379563=CARTESIAN_POINT('Ctrl Pts',(-1.35704081960701,6.03040400634774E-16,
-8.56250499398093));
#379564=CARTESIAN_POINT('Ctrl Pts',(-1.01778061470526,-0.587615911876062,
-8.52083832731427));
#379565=CARTESIAN_POINT('Ctrl Pts',(-0.678520409803505,-1.17523182375213,
-8.4791716606476));
#379566=CARTESIAN_POINT('Ctrl Pts',(-1.43924389121415E-16,-1.17523182375213,
-8.43750499398093));
#379567=CARTESIAN_POINT('Ctrl Pts',(0.678520409803504,-1.17523182375213,
-8.39583832731427));
#379568=CARTESIAN_POINT('Ctrl Pts',(1.01778061470526,-0.587615911876063,
-8.3541716606476));
#379569=CARTESIAN_POINT('Ctrl Pts',(1.35704081960701,2.70661261425969E-16,
-8.31250499398093));
#379570=CARTESIAN_POINT('Ctrl Pts',(1.01778061470526,0.587615911876063,
-8.27083832731427));
#379571=CARTESIAN_POINT('Ctrl Pts',(0.678520409803506,1.17523182375213,
-8.2291716606476));
#379572=CARTESIAN_POINT('Ctrl Pts',(0.,1.17523182375213,-8.18750499398093));
#379573=CARTESIAN_POINT('Ctrl Pts',(-0.678520409803505,1.17523182375213,
-8.14583832731427));
#379574=CARTESIAN_POINT('Ctrl Pts',(-1.01778061470526,0.587615911876064,
-8.1041716606476));
#379575=CARTESIAN_POINT('Ctrl Pts',(-1.35704081960701,6.03040400634774E-16,
-8.06250499398093));
#379576=CARTESIAN_POINT('Ctrl Pts',(-1.01778061470526,-0.587615911876062,
-8.02083832731427));
#379577=CARTESIAN_POINT('Ctrl Pts',(-0.678520409803505,-1.17523182375213,
-7.9791716606476));
#379578=CARTESIAN_POINT('Ctrl Pts',(-1.43924389121415E-16,-1.17523182375213,
-7.93750499398093));
#379579=CARTESIAN_POINT('Ctrl Pts',(0.678520409803504,-1.17523182375213,
-7.89583832731427));
#379580=CARTESIAN_POINT('Ctrl Pts',(1.01778061470526,-0.587615911876063,
-7.8541716606476));
#379581=CARTESIAN_POINT('Ctrl Pts',(1.35704081960701,2.70661261425969E-16,
-7.81250499398093));
#379582=CARTESIAN_POINT('Ctrl Pts',(1.01778061470526,0.587615911876063,
-7.77083832731427));
#379583=CARTESIAN_POINT('Ctrl Pts',(0.678520409803506,1.17523182375213,
-7.7291716606476));
#379584=CARTESIAN_POINT('Ctrl Pts',(0.,1.17523182375213,-7.68750499398093));
#379585=CARTESIAN_POINT('Ctrl Pts',(-0.678520409803505,1.17523182375213,
-7.64583832731426));
#379586=CARTESIAN_POINT('Ctrl Pts',(-1.01778061470526,0.587615911876064,
-7.6041716606476));
#379587=CARTESIAN_POINT('Ctrl Pts',(-1.35704081960701,6.03040400634774E-16,
-7.56250499398093));
#379588=CARTESIAN_POINT('Ctrl Pts',(-1.01778061470526,-0.587615911876062,
-7.52083832731427));
#379589=CARTESIAN_POINT('Ctrl Pts',(-0.678520409803505,-1.17523182375213,
-7.4791716606476));
#379590=CARTESIAN_POINT('Ctrl Pts',(-1.43924389121415E-16,-1.17523182375213,
-7.43750499398093));
#379591=CARTESIAN_POINT('Ctrl Pts',(0.678520409803504,-1.17523182375213,
-7.39583832731426));
#379592=CARTESIAN_POINT('Ctrl Pts',(1.01778061470526,-0.587615911876063,
-7.3541716606476));
#379593=CARTESIAN_POINT('Ctrl Pts',(1.35704081960701,2.70661261425969E-16,
-7.31250499398093));
#379594=CARTESIAN_POINT('Ctrl Pts',(1.01778061470526,0.587615911876063,
-7.27083832731427));
#379595=CARTESIAN_POINT('Ctrl Pts',(0.678520409803506,1.17523182375213,
-7.2291716606476));
#379596=CARTESIAN_POINT('Ctrl Pts',(0.,1.17523182375213,-7.18750499398093));
#379597=CARTESIAN_POINT('Ctrl Pts',(-0.678520409803505,1.17523182375213,
-7.14583832731427));
#379598=CARTESIAN_POINT('Ctrl Pts',(-1.01778061470526,0.587615911876064,
-7.1041716606476));
#379599=CARTESIAN_POINT('Ctrl Pts',(-1.35704081960701,6.03040400634774E-16,
-7.06250499398093));
#379600=CARTESIAN_POINT('Ctrl Pts',(-1.01778061470526,-0.587615911876062,
-7.02083832731427));
#379601=CARTESIAN_POINT('Ctrl Pts',(-0.678520409803505,-1.17523182375213,
-6.9791716606476));
#379602=CARTESIAN_POINT('Ctrl Pts',(-1.43924389121415E-16,-1.17523182375213,
-6.93750499398093));
#379603=CARTESIAN_POINT('Ctrl Pts',(0.678520409803504,-1.17523182375213,
-6.89583832731427));
#379604=CARTESIAN_POINT('Ctrl Pts',(1.01778061470526,-0.587615911876063,
-6.8541716606476));
#379605=CARTESIAN_POINT('Ctrl Pts',(1.35704081960701,2.70661261425969E-16,
-6.81250499398093));
#379606=CARTESIAN_POINT('Ctrl Pts',(1.01778061470526,0.587615911876063,
-6.77083832731427));
#379607=CARTESIAN_POINT('Ctrl Pts',(0.678520409803506,1.17523182375213,
-6.7291716606476));
#379608=CARTESIAN_POINT('Ctrl Pts',(0.,1.17523182375213,-6.68750499398093));
#379609=CARTESIAN_POINT('Ctrl Pts',(-0.678520409803505,1.17523182375213,
-6.64583832731427));
#379610=CARTESIAN_POINT('Ctrl Pts',(-1.01778061470526,0.587615911876064,
-6.6041716606476));
#379611=CARTESIAN_POINT('Ctrl Pts',(-1.35704081960701,6.03040400634774E-16,
-6.56250499398093));
#379612=CARTESIAN_POINT('Ctrl Pts',(-1.01778061470526,-0.587615911876062,
-6.52083832731427));
#379613=CARTESIAN_POINT('Ctrl Pts',(-0.678520409803505,-1.17523182375213,
-6.4791716606476));
#379614=CARTESIAN_POINT('Ctrl Pts',(-1.43924389121415E-16,-1.17523182375213,
-6.43750499398093));
#379615=CARTESIAN_POINT('Ctrl Pts',(0.678520409803504,-1.17523182375213,
-6.39583832731427));
#379616=CARTESIAN_POINT('Ctrl Pts',(1.01778061470526,-0.587615911876063,
-6.3541716606476));
#379617=CARTESIAN_POINT('Ctrl Pts',(1.35704081960701,2.70661261425969E-16,
-6.31250499398093));
#379618=CARTESIAN_POINT('Ctrl Pts',(1.01778061470526,0.587615911876063,
-6.27083832731427));
#379619=CARTESIAN_POINT('Ctrl Pts',(0.678520409803506,1.17523182375213,
-6.2291716606476));
#379620=CARTESIAN_POINT('Ctrl Pts',(0.,1.17523182375213,-6.18750499398093));
#379621=CARTESIAN_POINT('Ctrl Pts',(-0.678520409803505,1.17523182375213,
-6.14583832731427));
#379622=CARTESIAN_POINT('Ctrl Pts',(-1.01778061470526,0.587615911876064,
-6.1041716606476));
#379623=CARTESIAN_POINT('Ctrl Pts',(-1.35704081960701,6.03040400634774E-16,
-6.06250499398093));
#379624=CARTESIAN_POINT('Ctrl Pts',(-1.01778061470526,-0.587615911876062,
-6.02083832731427));
#379625=CARTESIAN_POINT('Ctrl Pts',(-0.678520409803505,-1.17523182375213,
-5.9791716606476));
#379626=CARTESIAN_POINT('Ctrl Pts',(-1.43924389121415E-16,-1.17523182375213,
-5.93750499398093));
#379627=CARTESIAN_POINT('Ctrl Pts',(0.678520409803504,-1.17523182375213,
-5.89583832731427));
#379628=CARTESIAN_POINT('Ctrl Pts',(1.01778061470526,-0.587615911876063,
-5.8541716606476));
#379629=CARTESIAN_POINT('Ctrl Pts',(1.35704081960701,2.70661261425969E-16,
-5.81250499398093));
#379630=CARTESIAN_POINT('Ctrl Pts',(1.01778061470526,0.587615911876063,
-5.77083832731426));
#379631=CARTESIAN_POINT('Ctrl Pts',(0.678520409803506,1.17523182375213,
-5.7291716606476));
#379632=CARTESIAN_POINT('Ctrl Pts',(0.,1.17523182375213,-5.68750499398093));
#379633=CARTESIAN_POINT('Ctrl Pts',(-0.678520409803505,1.17523182375213,
-5.64583832731427));
#379634=CARTESIAN_POINT('Ctrl Pts',(-1.01778061470526,0.587615911876064,
-5.6041716606476));
#379635=CARTESIAN_POINT('Ctrl Pts',(-1.35704081960701,6.03040400634774E-16,
-5.56250499398093));
#379636=CARTESIAN_POINT('Ctrl Pts',(-1.01778061470526,-0.587615911876062,
-5.52083832731427));
#379637=CARTESIAN_POINT('Ctrl Pts',(-0.678520409803505,-1.17523182375213,
-5.4791716606476));
#379638=CARTESIAN_POINT('Ctrl Pts',(-1.43924389121415E-16,-1.17523182375213,
-5.43750499398093));
#379639=CARTESIAN_POINT('Ctrl Pts',(0.678520409803504,-1.17523182375213,
-5.39583832731426));
#379640=CARTESIAN_POINT('Ctrl Pts',(1.01778061470526,-0.587615911876063,
-5.3541716606476));
#379641=CARTESIAN_POINT('Ctrl Pts',(1.35704081960701,2.70661261425969E-16,
-5.31250499398093));
#379642=CARTESIAN_POINT('Ctrl Pts',(1.01778061470526,0.587615911876063,
-5.27083832731427));
#379643=CARTESIAN_POINT('Ctrl Pts',(0.678520409803506,1.17523182375213,
-5.2291716606476));
#379644=CARTESIAN_POINT('Ctrl Pts',(0.,1.17523182375213,-5.18750499398093));
#379645=CARTESIAN_POINT('Ctrl Pts',(-0.678520409803505,1.17523182375213,
-5.14583832731427));
#379646=CARTESIAN_POINT('Ctrl Pts',(-1.01778061470526,0.587615911876064,
-5.1041716606476));
#379647=CARTESIAN_POINT('Ctrl Pts',(-1.35704081960701,6.03040400634774E-16,
-5.06250499398093));
#379648=CARTESIAN_POINT('Ctrl Pts',(-1.01778061470526,-0.587615911876062,
-5.02083832731427));
#379649=CARTESIAN_POINT('Ctrl Pts',(-0.678520409803505,-1.17523182375213,
-4.9791716606476));
#379650=CARTESIAN_POINT('Ctrl Pts',(-1.43924389121415E-16,-1.17523182375213,
-4.93750499398093));
#379651=CARTESIAN_POINT('Ctrl Pts',(0.678520409803504,-1.17523182375213,
-4.89583832731427));
#379652=CARTESIAN_POINT('Ctrl Pts',(1.01778061470526,-0.587615911876063,
-4.8541716606476));
#379653=CARTESIAN_POINT('Ctrl Pts',(1.35704081960701,2.70661261425969E-16,
-4.81250499398093));
#379654=CARTESIAN_POINT('Ctrl Pts',(1.01778061470526,0.587615911876063,
-4.77083832731427));
#379655=CARTESIAN_POINT('Ctrl Pts',(0.678520409803506,1.17523182375213,
-4.7291716606476));
#379656=CARTESIAN_POINT('Ctrl Pts',(0.,1.17523182375213,-4.68750499398093));
#379657=CARTESIAN_POINT('Ctrl Pts',(-0.678520409803505,1.17523182375213,
-4.64583832731427));
#379658=CARTESIAN_POINT('Ctrl Pts',(-1.01778061470526,0.587615911876064,
-4.6041716606476));
#379659=CARTESIAN_POINT('Ctrl Pts',(-1.35704081960701,6.03040400634774E-16,
-4.56250499398093));
#379660=CARTESIAN_POINT('Ctrl Pts',(-1.01778061470526,-0.587615911876062,
-4.52083832731427));
#379661=CARTESIAN_POINT('Ctrl Pts',(-0.678520409803505,-1.17523182375213,
-4.4791716606476));
#379662=CARTESIAN_POINT('Ctrl Pts',(-1.43924389121415E-16,-1.17523182375213,
-4.43750499398093));
#379663=CARTESIAN_POINT('Ctrl Pts',(0.678520409803504,-1.17523182375213,
-4.39583832731427));
#379664=CARTESIAN_POINT('Ctrl Pts',(1.01778061470526,-0.587615911876063,
-4.3541716606476));
#379665=CARTESIAN_POINT('Ctrl Pts',(1.35704081960701,2.70661261425969E-16,
-4.31250499398093));
#379666=CARTESIAN_POINT('Ctrl Pts',(1.01778061470526,0.587615911876063,
-4.27083832731427));
#379667=CARTESIAN_POINT('Ctrl Pts',(0.678520409803506,1.17523182375213,
-4.2291716606476));
#379668=CARTESIAN_POINT('Ctrl Pts',(0.,1.17523182375213,-4.18750499398093));
#379669=CARTESIAN_POINT('Ctrl Pts',(-0.678520409803505,1.17523182375213,
-4.14583832731427));
#379670=CARTESIAN_POINT('Ctrl Pts',(-1.01778061470526,0.587615911876064,
-4.1041716606476));
#379671=CARTESIAN_POINT('Ctrl Pts',(-1.35704081960701,6.03040400634774E-16,
-4.06250499398093));
#379672=CARTESIAN_POINT('Ctrl Pts',(-1.01778061470526,-0.587615911876062,
-4.02083832731427));
#379673=CARTESIAN_POINT('Ctrl Pts',(-0.678520409803505,-1.17523182375213,
-3.9791716606476));
#379674=CARTESIAN_POINT('Ctrl Pts',(-1.43924389121415E-16,-1.17523182375213,
-3.93750499398093));
#379675=CARTESIAN_POINT('Ctrl Pts',(0.678520409803504,-1.17523182375213,
-3.89583832731427));
#379676=CARTESIAN_POINT('Ctrl Pts',(1.01778061470526,-0.587615911876063,
-3.8541716606476));
#379677=CARTESIAN_POINT('Ctrl Pts',(1.35704081960701,2.70661261425969E-16,
-3.81250499398093));
#379678=CARTESIAN_POINT('Ctrl Pts',(1.01778061470526,0.587615911876063,
-3.77083832731427));
#379679=CARTESIAN_POINT('Ctrl Pts',(0.678520409803506,1.17523182375213,
-3.7291716606476));
#379680=CARTESIAN_POINT('Ctrl Pts',(0.,1.17523182375213,-3.68750499398093));
#379681=CARTESIAN_POINT('Ctrl Pts',(-0.678520409803505,1.17523182375213,
-3.64583832731427));
#379682=CARTESIAN_POINT('Ctrl Pts',(-1.01778061470526,0.587615911876064,
-3.6041716606476));
#379683=CARTESIAN_POINT('Ctrl Pts',(-1.35704081960701,6.03040400634774E-16,
-3.56250499398093));
#379684=CARTESIAN_POINT('Ctrl Pts',(-1.01778061470526,-0.587615911876062,
-3.52083832731427));
#379685=CARTESIAN_POINT('Ctrl Pts',(-0.678520409803505,-1.17523182375213,
-3.4791716606476));
#379686=CARTESIAN_POINT('Ctrl Pts',(-1.43924389121415E-16,-1.17523182375213,
-3.43750499398093));
#379687=CARTESIAN_POINT('Ctrl Pts',(0.678520409803504,-1.17523182375213,
-3.39583832731427));
#379688=CARTESIAN_POINT('Ctrl Pts',(1.01778061470526,-0.587615911876063,
-3.3541716606476));
#379689=CARTESIAN_POINT('Ctrl Pts',(1.35704081960701,2.70661261425969E-16,
-3.31250499398093));
#379690=CARTESIAN_POINT('Ctrl Pts',(1.01778061470526,0.587615911876063,
-3.27083832731427));
#379691=CARTESIAN_POINT('Ctrl Pts',(0.678520409803506,1.17523182375213,
-3.2291716606476));
#379692=CARTESIAN_POINT('Ctrl Pts',(0.,1.17523182375213,-3.18750499398093));
#379693=CARTESIAN_POINT('Ctrl Pts',(-0.678520409803505,1.17523182375213,
-3.14583832731427));
#379694=CARTESIAN_POINT('Ctrl Pts',(-1.01778061470526,0.587615911876064,
-3.1041716606476));
#379695=CARTESIAN_POINT('Ctrl Pts',(-1.35704081960701,6.03040400634774E-16,
-3.06250499398093));
#379696=CARTESIAN_POINT('Ctrl Pts',(-1.01778061470526,-0.587615911876062,
-3.02083832731427));
#379697=CARTESIAN_POINT('Ctrl Pts',(-0.678520409803505,-1.17523182375213,
-2.9791716606476));
#379698=CARTESIAN_POINT('Ctrl Pts',(-1.43924389121415E-16,-1.17523182375213,
-2.93750499398093));
#379699=CARTESIAN_POINT('Ctrl Pts',(0.678520409803504,-1.17523182375213,
-2.89583832731427));
#379700=CARTESIAN_POINT('Ctrl Pts',(1.01778061470526,-0.587615911876063,
-2.8541716606476));
#379701=CARTESIAN_POINT('Ctrl Pts',(1.35704081960701,2.70661261425969E-16,
-2.81250499398093));
#379702=CARTESIAN_POINT('Ctrl Pts',(1.01778061470526,0.587615911876063,
-2.77083832731427));
#379703=CARTESIAN_POINT('Ctrl Pts',(0.678520409803506,1.17523182375213,
-2.7291716606476));
#379704=CARTESIAN_POINT('Ctrl Pts',(0.,1.17523182375213,-2.68750499398093));
#379705=CARTESIAN_POINT('Ctrl Pts',(-0.678520409803505,1.17523182375213,
-2.64583832731427));
#379706=CARTESIAN_POINT('Ctrl Pts',(-1.01778061470526,0.587615911876064,
-2.6041716606476));
#379707=CARTESIAN_POINT('Ctrl Pts',(-1.35704081960701,6.03040400634774E-16,
-2.56250499398093));
#379708=CARTESIAN_POINT('Ctrl Pts',(-1.01778061470526,-0.587615911876062,
-2.52083832731427));
#379709=CARTESIAN_POINT('Ctrl Pts',(-0.678520409803505,-1.17523182375213,
-2.4791716606476));
#379710=CARTESIAN_POINT('Ctrl Pts',(-1.43924389121415E-16,-1.17523182375213,
-2.43750499398093));
#379711=CARTESIAN_POINT('Ctrl Pts',(0.678520409803504,-1.17523182375213,
-2.39583832731427));
#379712=CARTESIAN_POINT('Ctrl Pts',(1.01778061470526,-0.587615911876063,
-2.3541716606476));
#379713=CARTESIAN_POINT('Ctrl Pts',(1.35704081960701,2.70661261425969E-16,
-2.31250499398093));
#379714=CARTESIAN_POINT('Ctrl Pts',(1.01778061470526,0.587615911876063,
-2.27083832731427));
#379715=CARTESIAN_POINT('Ctrl Pts',(0.678520409803506,1.17523182375213,
-2.2291716606476));
#379716=CARTESIAN_POINT('Ctrl Pts',(0.,1.17523182375213,-2.18750499398093));
#379717=CARTESIAN_POINT('Ctrl Pts',(-0.678520409803505,1.17523182375213,
-2.14583832731427));
#379718=CARTESIAN_POINT('Ctrl Pts',(-1.01778061470526,0.587615911876064,
-2.1041716606476));
#379719=CARTESIAN_POINT('Ctrl Pts',(-1.35704081960701,6.03040400634774E-16,
-2.06250499398093));
#379720=CARTESIAN_POINT('Ctrl Pts',(-1.01778061470526,-0.587615911876062,
-2.02083832731427));
#379721=CARTESIAN_POINT('Ctrl Pts',(-0.678520409803505,-1.17523182375213,
-1.9791716606476));
#379722=CARTESIAN_POINT('Ctrl Pts',(-1.43924389121415E-16,-1.17523182375213,
-1.93750499398093));
#379723=CARTESIAN_POINT('Ctrl Pts',(0.678520409803504,-1.17523182375213,
-1.89583832731427));
#379724=CARTESIAN_POINT('Ctrl Pts',(1.01778061470526,-0.587615911876063,
-1.8541716606476));
#379725=CARTESIAN_POINT('Ctrl Pts',(1.35704081960701,2.70661261425969E-16,
-1.81250499398093));
#379726=CARTESIAN_POINT('Ctrl Pts',(1.01778061470526,0.587615911876063,
-1.77083832731427));
#379727=CARTESIAN_POINT('Ctrl Pts',(0.678520409803506,1.17523182375213,
-1.7291716606476));
#379728=CARTESIAN_POINT('Ctrl Pts',(0.,1.17523182375213,-1.68750499398093));
#379729=CARTESIAN_POINT('Ctrl Pts',(-0.678520409803505,1.17523182375213,
-1.64583832731427));
#379730=CARTESIAN_POINT('Ctrl Pts',(-1.01778061470526,0.587615911876064,
-1.6041716606476));
#379731=CARTESIAN_POINT('Ctrl Pts',(-1.35704081960701,6.03040400634774E-16,
-1.56250499398093));
#379732=CARTESIAN_POINT('Ctrl Pts',(-1.01778061470526,-0.587615911876062,
-1.52083832731427));
#379733=CARTESIAN_POINT('Ctrl Pts',(-0.678520409803505,-1.17523182375213,
-1.4791716606476));
#379734=CARTESIAN_POINT('Ctrl Pts',(-1.43924389121415E-16,-1.17523182375213,
-1.43750499398093));
#379735=CARTESIAN_POINT('Ctrl Pts',(0.678520409803504,-1.17523182375213,
-1.39583832731427));
#379736=CARTESIAN_POINT('Ctrl Pts',(1.01778061470526,-0.587615911876063,
-1.3541716606476));
#379737=CARTESIAN_POINT('Ctrl Pts',(1.35704081960701,2.70661261425969E-16,
-1.31250499398093));
#379738=CARTESIAN_POINT('Ctrl Pts',(1.01778061470526,0.587615911876063,
-1.27083832731427));
#379739=CARTESIAN_POINT('Ctrl Pts',(0.678520409803506,1.17523182375213,
-1.2291716606476));
#379740=CARTESIAN_POINT('Ctrl Pts',(0.,1.17523182375213,-1.18750499398093));
#379741=CARTESIAN_POINT('Ctrl Pts',(-0.678520409803505,1.17523182375213,
-1.14583832731427));
#379742=CARTESIAN_POINT('Ctrl Pts',(-1.01778061470526,0.587615911876064,
-1.1041716606476));
#379743=CARTESIAN_POINT('Ctrl Pts',(-1.35704081960701,6.03040400634774E-16,
-1.06250499398093));
#379744=CARTESIAN_POINT('Ctrl Pts',(-1.01778061470526,-0.587615911876062,
-1.02083832731427));
#379745=CARTESIAN_POINT('Ctrl Pts',(-0.678520409803505,-1.17523182375213,
-0.9791716606476));
#379746=CARTESIAN_POINT('Ctrl Pts',(-1.43924389121415E-16,-1.17523182375213,
-0.937504993980932));
#379747=CARTESIAN_POINT('Ctrl Pts',(0.678520409803504,-1.17523182375213,
-0.895838327314267));
#379748=CARTESIAN_POINT('Ctrl Pts',(1.01778061470526,-0.587615911876063,
-0.854171660647599));
#379749=CARTESIAN_POINT('Ctrl Pts',(1.35704081960701,2.70661261425969E-16,
-0.812504993980932));
#379750=CARTESIAN_POINT('Ctrl Pts',(1.01778061470526,0.587615911876063,
-0.770838327314266));
#379751=CARTESIAN_POINT('Ctrl Pts',(0.678520409803506,1.17523182375213,
-0.729171660647599));
#379752=CARTESIAN_POINT('Ctrl Pts',(0.,1.17523182375213,-0.687504993980934));
#379753=CARTESIAN_POINT('Ctrl Pts',(-0.678520409803505,1.17523182375213,
-0.645838327314266));
#379754=CARTESIAN_POINT('Ctrl Pts',(-1.01778061470526,0.587615911876064,
-0.604171660647599));
#379755=CARTESIAN_POINT('Ctrl Pts',(-1.35704081960701,6.03040400634774E-16,
-0.562504993980934));
#379756=CARTESIAN_POINT('Ctrl Pts',(-1.01778061470526,-0.587615911876062,
-0.520838327314266));
#379757=CARTESIAN_POINT('Ctrl Pts',(-0.678520409803505,-1.17523182375213,
-0.479171660647599));
#379758=CARTESIAN_POINT('Ctrl Pts',(-1.43924389121415E-16,-1.17523182375213,
-0.437504993980933));
#379759=CARTESIAN_POINT('Ctrl Pts',(0.678520409803504,-1.17523182375213,
-0.395838327314266));
#379760=CARTESIAN_POINT('Ctrl Pts',(1.01778061470526,-0.587615911876063,
-0.354171660647599));
#379761=CARTESIAN_POINT('Ctrl Pts',(1.35704081960701,2.70661261425969E-16,
-0.312504993980933));
#379762=CARTESIAN_POINT('Ctrl Pts',(1.01778061470526,0.587615911876063,
-0.270838327314266));
#379763=CARTESIAN_POINT('Ctrl Pts',(0.678520409803506,1.17523182375213,
-0.229171660647599));
#379764=CARTESIAN_POINT('Ctrl Pts',(0.,1.17523182375213,-0.187504993980933));
#379765=CARTESIAN_POINT('Ctrl Pts',(-0.678520409803505,1.17523182375213,
-0.145838327314266));
#379766=CARTESIAN_POINT('Ctrl Pts',(-1.01778061470526,0.587615911876064,
-0.104171660647599));
#379767=CARTESIAN_POINT('Ctrl Pts',(-1.35704081960701,6.03040400634774E-16,
-0.0625049939809331));
#379768=CARTESIAN_POINT('Ctrl Pts',(-1.01778061470526,-0.587615911876062,
-0.0208383273142658));
#379769=CARTESIAN_POINT('Ctrl Pts',(-0.678520409803505,-1.17523182375213,
0.0208283393523997));
#379770=CARTESIAN_POINT('Ctrl Pts',(-1.43924389121415E-16,-1.17523182375213,
0.062495006019067));
#379771=CARTESIAN_POINT('Ctrl Pts',(0.678520409803504,-1.17523182375213,
0.104161672685734));
#379772=CARTESIAN_POINT('Ctrl Pts',(1.01778061470526,-0.587615911876063,
0.1458283393524));
#379773=CARTESIAN_POINT('Ctrl Pts',(1.35704081960701,2.70661261425969E-16,
0.187495006019067));
#379774=CARTESIAN_POINT('Ctrl Pts',(1.01778061470526,0.587615911876063,
0.229161672685734));
#379775=CARTESIAN_POINT('Ctrl Pts',(0.678520409803506,1.17523182375213,
0.2708283393524));
#379776=CARTESIAN_POINT('Ctrl Pts',(0.,1.17523182375213,0.312495006019067));
#379777=CARTESIAN_POINT('Ctrl Pts',(-0.678520409803505,1.17523182375213,
0.354161672685734));
#379778=CARTESIAN_POINT('Ctrl Pts',(-1.01778061470526,0.587615911876064,
0.3958283393524));
#379779=CARTESIAN_POINT('Ctrl Pts',(-1.35704081960701,6.03040400634774E-16,
0.437495006019067));
#379780=CARTESIAN_POINT('Ctrl Pts',(-1.01778061470526,-0.587615911876062,
0.479161672685735));
#379781=CARTESIAN_POINT('Ctrl Pts',(-0.678520409803505,-1.17523182375213,
0.5208283393524));
#379782=CARTESIAN_POINT('Ctrl Pts',(-1.43924389121415E-16,-1.17523182375213,
0.562495006019067));
#379783=CARTESIAN_POINT('Ctrl Pts',(0.678520409803504,-1.17523182375213,
0.604161672685733));
#379784=CARTESIAN_POINT('Ctrl Pts',(1.01778061470526,-0.587615911876063,
0.6458283393524));
#379785=CARTESIAN_POINT('Ctrl Pts',(1.35704081960701,2.70661261425969E-16,
0.687495006019068));
#379786=CARTESIAN_POINT('Ctrl Pts',(1.01778061470526,0.587615911876063,
0.729161672685733));
#379787=CARTESIAN_POINT('Ctrl Pts',(0.678520409803506,1.17523182375213,
0.770828339352401));
#379788=CARTESIAN_POINT('Ctrl Pts',(0.,1.17523182375213,0.812495006019068));
#379789=CARTESIAN_POINT('Ctrl Pts',(-0.678520409803505,1.17523182375213,
0.854161672685734));
#379790=CARTESIAN_POINT('Ctrl Pts',(-1.01778061470526,0.587615911876064,
0.8958283393524));
#379791=CARTESIAN_POINT('Ctrl Pts',(-1.35704081960701,6.03040400634774E-16,
0.937495006019068));
#379792=CARTESIAN_POINT('Ctrl Pts',(-1.01778061470526,-0.587615911876062,
0.979161672685733));
#379793=CARTESIAN_POINT('Ctrl Pts',(-0.678520409803505,-1.17523182375213,
1.0208283393524));
#379794=CARTESIAN_POINT('Ctrl Pts',(-1.43924389121415E-16,-1.17523182375213,
1.06249500601907));
#379795=CARTESIAN_POINT('Ctrl Pts',(0.678520409803504,-1.17523182375213,
1.10416167268573));
#379796=CARTESIAN_POINT('Ctrl Pts',(1.01778061470526,-0.587615911876063,
1.1458283393524));
#379797=CARTESIAN_POINT('Ctrl Pts',(1.35704081960701,2.70661261425969E-16,
1.18749500601907));
#379798=CARTESIAN_POINT('Ctrl Pts',(1.01778061470526,0.587615911876063,
1.22916167268573));
#379799=CARTESIAN_POINT('Ctrl Pts',(0.678520409803506,1.17523182375213,
1.2708283393524));
#379800=CARTESIAN_POINT('Ctrl Pts',(0.,1.17523182375213,1.31249500601907));
#379801=CARTESIAN_POINT('Ctrl Pts',(-0.678520409803505,1.17523182375213,
1.35416167268573));
#379802=CARTESIAN_POINT('Ctrl Pts',(-1.01778061470526,0.587615911876064,
1.3958283393524));
#379803=CARTESIAN_POINT('Ctrl Pts',(-1.35704081960701,6.03040400634774E-16,
1.43749500601907));
#379804=CARTESIAN_POINT('Ctrl Pts',(-1.01778061470526,-0.587615911876062,
1.47916167268573));
#379805=CARTESIAN_POINT('Ctrl Pts',(-0.678520409803505,-1.17523182375213,
1.5208283393524));
#379806=CARTESIAN_POINT('Ctrl Pts',(-1.43924389121415E-16,-1.17523182375213,
1.56249500601907));
#379807=CARTESIAN_POINT('Ctrl Pts',(0.678520409803504,-1.17523182375213,
1.60416167268573));
#379808=CARTESIAN_POINT('Ctrl Pts',(1.01778061470526,-0.587615911876063,
1.6458283393524));
#379809=CARTESIAN_POINT('Ctrl Pts',(1.35704081960701,2.70661261425969E-16,
1.68749500601907));
#379810=CARTESIAN_POINT('Ctrl Pts',(1.01778061470526,0.587615911876063,
1.72916167268573));
#379811=CARTESIAN_POINT('Ctrl Pts',(0.678520409803506,1.17523182375213,
1.7708283393524));
#379812=CARTESIAN_POINT('Ctrl Pts',(0.,1.17523182375213,1.81249500601907));
#379813=CARTESIAN_POINT('Ctrl Pts',(-0.678520409803505,1.17523182375213,
1.85416167268573));
#379814=CARTESIAN_POINT('Ctrl Pts',(-1.01778061470526,0.587615911876064,
1.8958283393524));
#379815=CARTESIAN_POINT('Ctrl Pts',(-1.35704081960701,6.03040400634774E-16,
1.93749500601907));
#379816=CARTESIAN_POINT('Ctrl Pts',(-1.01778061470526,-0.587615911876062,
1.97916167268573));
#379817=CARTESIAN_POINT('Ctrl Pts',(-0.678520409803505,-1.17523182375213,
2.0208283393524));
#379818=CARTESIAN_POINT('Ctrl Pts',(-1.43924389121415E-16,-1.17523182375213,
2.06249500601907));
#379819=CARTESIAN_POINT('Ctrl Pts',(0.678520409803504,-1.17523182375213,
2.10416167268574));
#379820=CARTESIAN_POINT('Ctrl Pts',(1.01778061470526,-0.587615911876063,
2.1458283393524));
#379821=CARTESIAN_POINT('Ctrl Pts',(1.35704081960701,2.70661261425969E-16,
2.18749500601907));
#379822=CARTESIAN_POINT('Ctrl Pts',(1.01778061470526,0.587615911876063,
2.22916167268573));
#379823=CARTESIAN_POINT('Ctrl Pts',(0.678520409803506,1.17523182375213,
2.2708283393524));
#379824=CARTESIAN_POINT('Ctrl Pts',(0.,1.17523182375213,2.31249500601907));
#379825=CARTESIAN_POINT('Ctrl Pts',(-0.678520409803505,1.17523182375213,
2.35416167268573));
#379826=CARTESIAN_POINT('Ctrl Pts',(-1.01778061470526,0.587615911876064,
2.3958283393524));
#379827=CARTESIAN_POINT('Ctrl Pts',(-1.35704081960701,6.03040400634774E-16,
2.43749500601907));
#379828=CARTESIAN_POINT('Ctrl Pts',(-1.01778061470526,-0.587615911876062,
2.47916167268573));
#379829=CARTESIAN_POINT('Ctrl Pts',(-0.678520409803505,-1.17523182375213,
2.5208283393524));
#379830=CARTESIAN_POINT('Ctrl Pts',(-1.43924389121415E-16,-1.17523182375213,
2.56249500601907));
#379831=CARTESIAN_POINT('Ctrl Pts',(0.678520409803504,-1.17523182375213,
2.60416167268573));
#379832=CARTESIAN_POINT('Ctrl Pts',(1.01778061470526,-0.587615911876063,
2.6458283393524));
#379833=CARTESIAN_POINT('Ctrl Pts',(1.35704081960701,2.70661261425969E-16,
2.68749500601907));
#379834=CARTESIAN_POINT('Ctrl Pts',(1.01778061470526,0.587615911876063,
2.72916167268573));
#379835=CARTESIAN_POINT('Ctrl Pts',(0.678520409803506,1.17523182375213,
2.7708283393524));
#379836=CARTESIAN_POINT('Ctrl Pts',(0.,1.17523182375213,2.81249500601907));
#379837=CARTESIAN_POINT('Ctrl Pts',(-0.678520409803505,1.17523182375213,
2.85416167268573));
#379838=CARTESIAN_POINT('Ctrl Pts',(-1.01778061470526,0.587615911876064,
2.8958283393524));
#379839=CARTESIAN_POINT('Ctrl Pts',(-1.35704081960701,6.03040400634774E-16,
2.93749500601907));
#379840=CARTESIAN_POINT('Ctrl Pts',(-1.01778061470526,-0.587615911876062,
2.97916167268573));
#379841=CARTESIAN_POINT('Ctrl Pts',(-0.678520409803505,-1.17523182375213,
3.0208283393524));
#379842=CARTESIAN_POINT('Ctrl Pts',(-1.43924389121415E-16,-1.17523182375213,
3.06249500601907));
#379843=CARTESIAN_POINT('Ctrl Pts',(0.678520409803504,-1.17523182375213,
3.10416167268573));
#379844=CARTESIAN_POINT('Ctrl Pts',(1.01778061470526,-0.587615911876063,
3.1458283393524));
#379845=CARTESIAN_POINT('Ctrl Pts',(1.35704081960701,2.70661261425969E-16,
3.18749500601907));
#379846=CARTESIAN_POINT('Ctrl Pts',(1.01778061470526,0.587615911876063,
3.22916167268573));
#379847=CARTESIAN_POINT('Ctrl Pts',(0.678520409803506,1.17523182375213,
3.2708283393524));
#379848=CARTESIAN_POINT('Ctrl Pts',(0.,1.17523182375213,3.31249500601907));
#379849=CARTESIAN_POINT('Ctrl Pts',(-0.678520409803505,1.17523182375213,
3.35416167268573));
#379850=CARTESIAN_POINT('Ctrl Pts',(-1.01778061470526,0.587615911876064,
3.3958283393524));
#379851=CARTESIAN_POINT('Ctrl Pts',(-1.35704081960701,6.03040400634774E-16,
3.43749500601907));
#379852=CARTESIAN_POINT('Ctrl Pts',(-1.01778061470526,-0.587615911876062,
3.47916167268573));
#379853=CARTESIAN_POINT('Ctrl Pts',(-0.678520409803505,-1.17523182375213,
3.5208283393524));
#379854=CARTESIAN_POINT('Ctrl Pts',(-1.43924389121415E-16,-1.17523182375213,
3.56249500601907));
#379855=CARTESIAN_POINT('Ctrl Pts',(0.678520409803504,-1.17523182375213,
3.60416167268574));
#379856=CARTESIAN_POINT('Ctrl Pts',(1.01778061470526,-0.587615911876063,
3.6458283393524));
#379857=CARTESIAN_POINT('Ctrl Pts',(1.35704081960701,2.7066126142597E-16,
3.68749500601907));
#379858=CARTESIAN_POINT('Ctrl Pts',(1.01778061470526,0.587615911876063,
3.72916167268573));
#379859=CARTESIAN_POINT('Ctrl Pts',(0.678520409803506,1.17523182375213,
3.7708283393524));
#379860=CARTESIAN_POINT('Ctrl Pts',(0.,1.17523182375213,3.81249500601907));
#379861=CARTESIAN_POINT('Ctrl Pts',(-0.678520409803505,1.17523182375213,
3.85416167268573));
#379862=CARTESIAN_POINT('Ctrl Pts',(-1.01778061470526,0.587615911876064,
3.8958283393524));
#379863=CARTESIAN_POINT('Ctrl Pts',(-1.35704081960701,6.03040400634774E-16,
3.93749500601907));
#379864=CARTESIAN_POINT('Ctrl Pts',(-1.01778061470526,-0.587615911876062,
3.97916167268573));
#379865=CARTESIAN_POINT('Ctrl Pts',(-0.678520409803505,-1.17523182375213,
4.0208283393524));
#379866=CARTESIAN_POINT('Ctrl Pts',(-1.43924389121415E-16,-1.17523182375213,
4.06249500601907));
#379867=CARTESIAN_POINT('Ctrl Pts',(0.678520409803504,-1.17523182375213,
4.10416167268574));
#379868=CARTESIAN_POINT('Ctrl Pts',(1.01778061470526,-0.587615911876063,
4.1458283393524));
#379869=CARTESIAN_POINT('Ctrl Pts',(1.35704081960701,2.7066126142597E-16,
4.18749500601907));
#379870=CARTESIAN_POINT('Ctrl Pts',(1.01778061470526,0.587615911876063,
4.22916167268574));
#379871=CARTESIAN_POINT('Ctrl Pts',(0.678520409803506,1.17523182375213,
4.2708283393524));
#379872=CARTESIAN_POINT('Ctrl Pts',(0.,1.17523182375213,4.31249500601907));
#379873=CARTESIAN_POINT('Ctrl Pts',(-0.678520409803505,1.17523182375213,
4.35416167268573));
#379874=CARTESIAN_POINT('Ctrl Pts',(-1.01778061470526,0.587615911876064,
4.3958283393524));
#379875=CARTESIAN_POINT('Ctrl Pts',(-1.35704081960701,6.03040400634775E-16,
4.43749500601907));
#379876=CARTESIAN_POINT('Ctrl Pts',(-1.01778061470526,-0.587615911876062,
4.47916167268573));
#379877=CARTESIAN_POINT('Ctrl Pts',(-0.678520409803505,-1.17523182375213,
4.5208283393524));
#379878=CARTESIAN_POINT('Ctrl Pts',(-1.43924389121415E-16,-1.17523182375213,
4.56249500601907));
#379879=CARTESIAN_POINT('Ctrl Pts',(0.678520409803504,-1.17523182375213,
4.60416167268573));
#379880=CARTESIAN_POINT('Ctrl Pts',(1.01778061470526,-0.587615911876063,
4.6458283393524));
#379881=CARTESIAN_POINT('Ctrl Pts',(1.35704081960701,2.7066126142597E-16,
4.68749500601907));
#379882=CARTESIAN_POINT('Ctrl Pts',(1.01778061470526,0.587615911876063,
4.72916167268573));
#379883=CARTESIAN_POINT('Ctrl Pts',(0.678520409803506,1.17523182375213,
4.7708283393524));
#379884=CARTESIAN_POINT('Ctrl Pts',(0.,1.17523182375213,4.81249500601907));
#379885=CARTESIAN_POINT('Ctrl Pts',(-0.678520409803505,1.17523182375213,
4.85416167268573));
#379886=CARTESIAN_POINT('Ctrl Pts',(-1.01778061470526,0.587615911876064,
4.8958283393524));
#379887=CARTESIAN_POINT('Ctrl Pts',(-1.35704081960701,6.03040400634775E-16,
4.93749500601907));
#379888=CARTESIAN_POINT('Ctrl Pts',(-1.01778061470526,-0.587615911876062,
4.97916167268573));
#379889=CARTESIAN_POINT('Ctrl Pts',(-0.678520409803505,-1.17523182375213,
5.0208283393524));
#379890=CARTESIAN_POINT('Ctrl Pts',(-1.43924389121415E-16,-1.17523182375213,
5.06249500601907));
#379891=CARTESIAN_POINT('Ctrl Pts',(0.678520409803504,-1.17523182375213,
5.10416167268573));
#379892=CARTESIAN_POINT('Ctrl Pts',(1.01778061470526,-0.587615911876063,
5.1458283393524));
#379893=CARTESIAN_POINT('Ctrl Pts',(1.35704081960701,2.7066126142597E-16,
5.18749500601907));
#379894=CARTESIAN_POINT('Ctrl Pts',(1.01778061470526,0.587615911876063,
5.22916167268573));
#379895=CARTESIAN_POINT('Ctrl Pts',(0.678520409803506,1.17523182375213,
5.2708283393524));
#379896=CARTESIAN_POINT('Ctrl Pts',(0.,1.17523182375213,5.31249500601907));
#379897=CARTESIAN_POINT('Ctrl Pts',(-0.678520409803505,1.17523182375213,
5.35416167268573));
#379898=CARTESIAN_POINT('Ctrl Pts',(-1.01778061470526,0.587615911876064,
5.3958283393524));
#379899=CARTESIAN_POINT('Ctrl Pts',(-1.35704081960701,6.03040400634775E-16,
5.43749500601907));
#379900=CARTESIAN_POINT('Ctrl Pts',(-1.01778061470526,-0.587615911876062,
5.47916167268573));
#379901=CARTESIAN_POINT('Ctrl Pts',(-0.678520409803505,-1.17523182375213,
5.5208283393524));
#379902=CARTESIAN_POINT('Ctrl Pts',(-1.43924389121415E-16,-1.17523182375213,
5.56249500601907));
#379903=CARTESIAN_POINT('Ctrl Pts',(0.678520409803504,-1.17523182375213,
5.60416167268573));
#379904=CARTESIAN_POINT('Ctrl Pts',(1.01778061470526,-0.587615911876063,
5.6458283393524));
#379905=CARTESIAN_POINT('Ctrl Pts',(1.35704081960701,2.7066126142597E-16,
5.68749500601907));
#379906=CARTESIAN_POINT('Ctrl Pts',(1.01778061470526,0.587615911876063,
5.72916167268573));
#379907=CARTESIAN_POINT('Ctrl Pts',(0.678520409803506,1.17523182375213,
5.7708283393524));
#379908=CARTESIAN_POINT('Ctrl Pts',(0.,1.17523182375213,5.81249500601907));
#379909=CARTESIAN_POINT('Ctrl Pts',(-0.678520409803505,1.17523182375213,
5.85416167268574));
#379910=CARTESIAN_POINT('Ctrl Pts',(-1.01778061470526,0.587615911876064,
5.8958283393524));
#379911=CARTESIAN_POINT('Ctrl Pts',(-1.35704081960701,6.03040400634775E-16,
5.93749500601907));
#379912=CARTESIAN_POINT('Ctrl Pts',(-1.01778061470526,-0.587615911876062,
5.97916167268573));
#379913=CARTESIAN_POINT('Ctrl Pts',(-0.678520409803505,-1.17523182375213,
6.0208283393524));
#379914=CARTESIAN_POINT('Ctrl Pts',(-1.43924389121415E-16,-1.17523182375213,
6.06249500601907));
#379915=CARTESIAN_POINT('Ctrl Pts',(0.678520409803504,-1.17523182375213,
6.10416167268574));
#379916=CARTESIAN_POINT('Ctrl Pts',(1.01778061470526,-0.587615911876063,
6.1458283393524));
#379917=CARTESIAN_POINT('Ctrl Pts',(1.35704081960701,2.7066126142597E-16,
6.18749500601907));
#379918=CARTESIAN_POINT('Ctrl Pts',(1.01778061470526,0.587615911876063,
6.22916167268573));
#379919=CARTESIAN_POINT('Ctrl Pts',(0.678520409803506,1.17523182375213,
6.2708283393524));
#379920=CARTESIAN_POINT('Ctrl Pts',(0.,1.17523182375213,6.31249500601907));
#379921=CARTESIAN_POINT('Origin',(0.,0.,7.5));
#379922=CARTESIAN_POINT('',(-0.0391111754616882,2.74606032550115,7.50366116523517));
#379923=CARTESIAN_POINT('',(1.95335088339909E-13,2.67396661573471,7.57603338622103));
#379924=CARTESIAN_POINT('Ctrl Pts',(-0.039111175493625,2.74606032554878,
7.50366116529969));
#379925=CARTESIAN_POINT('Ctrl Pts',(-0.0260946561062611,2.72206870155541,
7.52783573079709));
#379926=CARTESIAN_POINT('Ctrl Pts',(-0.0130581974131689,2.69803860815066,
7.55196141284069));
#379927=CARTESIAN_POINT('Ctrl Pts',(-8.83381775932182E-10,2.67396661662181,
7.57603338728831));
#379928=CARTESIAN_POINT('',(0.0391111754616882,2.74606032550115,7.50366116523517));
#379929=CARTESIAN_POINT('Ctrl Pts',(8.84014432836477E-10,2.673966616623,
7.57603338728985));
#379930=CARTESIAN_POINT('Ctrl Pts',(0.0130581974166911,2.69803860815728,
7.55196141284922));
#379931=CARTESIAN_POINT('Ctrl Pts',(0.0260946561203838,2.72206870158194,
7.52783573083105));
#379932=CARTESIAN_POINT('Ctrl Pts',(0.0391111754945677,2.74606032555036,
7.50366116530176));
#379933=CARTESIAN_POINT('Origin',(0.,0.,7.50366116523517));
#379934=CARTESIAN_POINT('Ctrl Pts',(-0.00576978243959104,2.66725829676663,
7.59443877723642));
#379935=CARTESIAN_POINT('Ctrl Pts',(-0.00300154637558126,2.66217203460837,
7.58783886950016));
#379936=CARTESIAN_POINT('Ctrl Pts',(0.00519220816616302,2.66439499840616,
7.58559994247159));
#379937=CARTESIAN_POINT('Ctrl Pts',(-0.02088150189643,2.69502405266403,
7.56670252222137));
#379938=CARTESIAN_POINT('Ctrl Pts',(-0.0181172667194093,2.68994514159859,
7.56004874999026));
#379939=CARTESIAN_POINT('Ctrl Pts',(-0.00986936707313795,2.69216065704217,
7.55786368756704));
#379940=CARTESIAN_POINT('Ctrl Pts',(-0.0359650017270119,2.72273795878639,
7.53888913333556));
#379941=CARTESIAN_POINT('Ctrl Pts',(-0.0331843385650257,2.71762886350384,
7.53222002137276));
#379942=CARTESIAN_POINT('Ctrl Pts',(-0.0249043752016816,2.71987489365092,
7.53005029815326));
#379943=CARTESIAN_POINT('Ctrl Pts',(-0.0510195993927981,2.75039876106078,
7.51101258149734));
#379944=CARTESIAN_POINT('Ctrl Pts',(-0.0482052295407062,2.74522773425994,
7.5043616886572));
#379945=CARTESIAN_POINT('Ctrl Pts',(-0.0399120007351545,2.74753637834759,
7.50217374673251));
#379946=CARTESIAN_POINT('Ctrl Pts',(-0.0469183093502058,2.74286319116668,
7.51860402984325));
#379947=CARTESIAN_POINT('Ctrl Pts',(-0.047129417868931,2.74325107473053,
7.51734760759494));
#379948=CARTESIAN_POINT('Ctrl Pts',(-0.0472679263427277,2.74363002494186,
7.51608817408573));
#379949=CARTESIAN_POINT('Ctrl Pts',(-0.0473209740766783,2.74400375441725,
7.5148100591312));
#379950=CARTESIAN_POINT('Ctrl Pts',(-0.0473690259817077,2.74434228750662,
7.51365231206384));
#379951=CARTESIAN_POINT('Ctrl Pts',(-0.0473472713218901,2.74467697892738,
7.51247773061043));
#379952=CARTESIAN_POINT('Ctrl Pts',(-0.0472192392491731,2.74499964227536,
7.51129758471022));
#379953=CARTESIAN_POINT('Ctrl Pts',(-0.047060110004601,2.74540067596735,
7.50983079813402));
#379954=CARTESIAN_POINT('Ctrl Pts',(-0.0467297792999064,2.74576552647934,
7.50839324291155));
#379955=CARTESIAN_POINT('Ctrl Pts',(-0.0461647233399476,2.7460415258142,
7.50715379678855));
#379956=CARTESIAN_POINT('Ctrl Pts',(-0.045903683768143,2.74616902955418,
7.50658120839351));
#379957=CARTESIAN_POINT('Ctrl Pts',(-0.0455512704078027,2.74628715902903,
7.50598221009429));
#379958=CARTESIAN_POINT('Ctrl Pts',(-0.045108640875781,2.74637153582515,
7.50545747549611));
#379959=CARTESIAN_POINT('Ctrl Pts',(-0.0448724400568288,2.74641656189527,
7.50517746087247));
#379960=CARTESIAN_POINT('Ctrl Pts',(-0.0446080257594691,2.74645266364665,
7.50491486231392));
#379961=CARTESIAN_POINT('Ctrl Pts',(-0.0443221744710907,2.74647723236113,
7.50468370960992));
#379962=CARTESIAN_POINT('Ctrl Pts',(-0.043894736628288,2.74651397033903,
7.50433806340447));
#379963=CARTESIAN_POINT('Ctrl Pts',(-0.0434065014443661,2.74652546781193,
7.50405484070984));
#379964=CARTESIAN_POINT('Ctrl Pts',(-0.042890333785409,2.74651023424991,
7.50385766036131));
#379965=CARTESIAN_POINT('Ctrl Pts',(-0.0428351376773461,2.74650860525723,
7.50383657498791));
#379966=CARTESIAN_POINT('Ctrl Pts',(-0.0427796461468639,2.7465066857332,
7.50381643264937));
#379967=CARTESIAN_POINT('Ctrl Pts',(-0.0427239166342629,2.74650448512403,
7.50379723213559));
#379968=CARTESIAN_POINT('Ctrl Pts',(-0.0423519039072553,2.74648979533795,
7.50366906242519));
#379969=CARTESIAN_POINT('Ctrl Pts',(-0.041961222930374,2.74646154237284,
7.50358235568538));
#379970=CARTESIAN_POINT('Ctrl Pts',(-0.041585309161405,2.74642525806308,
7.5035341175365));
#379971=CARTESIAN_POINT('Ctrl Pts',(-0.0410216690100585,2.74637085384718,
7.50346178989176));
#379972=CARTESIAN_POINT('Ctrl Pts',(-0.0404176336735107,2.74628836196342,
7.50346967198527));
#379973=CARTESIAN_POINT('Ctrl Pts',(-0.0398271499193936,2.74618913461648,
7.50354272648692));
#379974=CARTESIAN_POINT('Ctrl Pts',(-0.0395842717290364,2.74614832035481,
7.50357277531559));
#379975=CARTESIAN_POINT('Ctrl Pts',(-0.0393439854661266,2.74610486877363,
7.50361331098761));
#379976=CARTESIAN_POINT('Ctrl Pts',(-0.0391111754617084,2.74606032550257,
7.50366116523658));
#379977=CARTESIAN_POINT('Origin',(2.85317610332501E-6,2.68280355420138,
7.58486873427628));
#379978=CARTESIAN_POINT('Origin',(-0.0578975244977156,2.73688767154537,
9.));
#379979=CARTESIAN_POINT('Origin',(-0.0578975244977155,2.73688767154537,
8.75721825406948));
#379980=CARTESIAN_POINT('Origin',(-0.0578975244977156,2.73688767154537,
7.51860402984325));
#379981=CARTESIAN_POINT('Ctrl Pts',(-0.00637576431677354,2.66873949177856,
7.59639677331371));
#379982=CARTESIAN_POINT('Ctrl Pts',(-0.000286090908296224,2.6515061579884,
7.59959882295465));
#379983=CARTESIAN_POINT('Ctrl Pts',(0.00631291894862653,2.66856962426893,
7.59642833564546));
#379984=CARTESIAN_POINT('Ctrl Pts',(-0.00568422544926916,2.66490062761342,
7.58707626057423));
#379985=CARTESIAN_POINT('Ctrl Pts',(-9.68314384630046E-5,2.66106744105337,
7.58809943920598));
#379986=CARTESIAN_POINT('Ctrl Pts',(0.0055389809656482,2.66480268125159,
7.58710240504252));
#379987=CARTESIAN_POINT('Ctrl Pts',(-0.00215341460009478,2.66984623243071,
7.58015376756929));
#379988=CARTESIAN_POINT('Ctrl Pts',(-3.20712293815052E-5,2.66794119340239,
7.58205880659761));
#379989=CARTESIAN_POINT('Ctrl Pts',(0.00209070701379044,2.66979075755872,
7.58020924244128));
#379990=CARTESIAN_POINT('Ctrl Pts',(-7.55734230502141E-15,2.67396661490714,
7.57603338509286));
#379991=CARTESIAN_POINT('Ctrl Pts',(-7.55734230502141E-15,2.67396661490714,
7.57603338509286));
#379992=CARTESIAN_POINT('Ctrl Pts',(-7.55734230502141E-15,2.67396661490714,
7.57603338509286));
#379993=CARTESIAN_POINT('Origin',(-2.85317609963331E-6,2.68280355420132,
7.58486873427623));
#379994=CARTESIAN_POINT('Ctrl Pts',(-0.0469178037552555,2.74286226211022,
7.51860402984325));
#379995=CARTESIAN_POINT('Ctrl Pts',(-0.0505546378370145,2.74954580337902,
7.51860402984325));
#379996=CARTESIAN_POINT('Ctrl Pts',(-0.0581618967556967,2.74938487552503,
7.51860402984325));
#379997=CARTESIAN_POINT('Ctrl Pts',(-0.0482681861850447,2.74534390598683,
7.51041458714366));
#379998=CARTESIAN_POINT('Ctrl Pts',(-0.0523568843976852,2.74950766782993,
7.51004642900442));
#379999=CARTESIAN_POINT('Ctrl Pts',(-0.0581639947473825,2.74938483114304,
7.50729136483008));
#380000=CARTESIAN_POINT('Ctrl Pts',(-0.0464115390694411,2.74745970339853,
7.50215815450138));
#380001=CARTESIAN_POINT('Ctrl Pts',(-0.0486873335340281,2.74958545597972,
7.49877163671531));
#380002=CARTESIAN_POINT('Ctrl Pts',(-0.0521371901874483,2.74953633709117,
7.49481588533172));
#380003=CARTESIAN_POINT('Ctrl Pts',(-0.0391111676211739,2.74605977503896,
7.50366171572174));
#380004=CARTESIAN_POINT('Ctrl Pts',(-0.0391633148674429,2.7497211194535,
7.50000045605858));
#380005=CARTESIAN_POINT('Ctrl Pts',(-0.0391633148675675,2.7497211194535,
7.49482233047317));
#380006=CARTESIAN_POINT('Origin',(-0.0389852998002483,2.73722238709234,
7.49482233047033));
#380007=CARTESIAN_POINT('Ctrl Pts',(-0.0389349646546055,2.72819480378047,
8.78942910404912));
#380008=CARTESIAN_POINT('Ctrl Pts',(-0.0415810698404549,2.73309894040653,
8.7967269950169));
#380009=CARTESIAN_POINT('Ctrl Pts',(-0.0500812990341607,2.73037504803777,
8.79893251111267));
#380010=CARTESIAN_POINT('Ctrl Pts',(-0.0441907101996744,2.7378515401601,
8.78111911759583));
#380011=CARTESIAN_POINT('Ctrl Pts',(-0.0473342496199769,2.74366191622698,
8.78644465894812));
#380012=CARTESIAN_POINT('Ctrl Pts',(-0.0554049987396861,2.74290131092718,
8.78817647674132));
#380013=CARTESIAN_POINT('Ctrl Pts',(-0.047466216212685,2.7438698485916,
8.76780923932029));
#380014=CARTESIAN_POINT('Ctrl Pts',(-0.0511815136631339,2.75072632739817,
8.76988516158374));
#380015=CARTESIAN_POINT('Ctrl Pts',(-0.0587403725670999,2.75072062947551,
8.77093053738833));
#380016=CARTESIAN_POINT('Ctrl Pts',(-0.0468275373701205,2.74269636081296,
8.75371302330492));
#380017=CARTESIAN_POINT('Ctrl Pts',(-0.0504509795361613,2.74938492330704,
8.75300828287559));
#380018=CARTESIAN_POINT('Ctrl Pts',(-0.0580902600704512,2.74919536526138,
8.75267964240738));
#380019=CARTESIAN_POINT('Origin',(-0.0511941478023398,2.72457111673216,
8.78727029226991));
#380020=CARTESIAN_POINT('Ctrl Pts',(0.0510325618244046,2.75042257778878,
7.51098857897448));
#380021=CARTESIAN_POINT('Ctrl Pts',(0.0482181791375388,2.74525152740576,
7.50433767179956));
#380022=CARTESIAN_POINT('Ctrl Pts',(0.0399249227228591,2.74756019566318,
7.50214974420965));
#380023=CARTESIAN_POINT('Ctrl Pts',(0.0359736340692041,2.72275381955636,
7.53887321589169));
#380024=CARTESIAN_POINT('Ctrl Pts',(0.0331929726815447,2.71764472753391,
7.53220407452065));
#380025=CARTESIAN_POINT('Ctrl Pts',(0.0249129797891101,2.71989075460921,
7.53003438070911));
#380026=CARTESIAN_POINT('Ctrl Pts',(0.0208857876177118,2.69503192710157,
7.56669465659234));
#380027=CARTESIAN_POINT('Ctrl Pts',(0.0181215594219111,2.68995302886307,
7.56004085833303));
#380028=CARTESIAN_POINT('Ctrl Pts',(0.00987363856813336,2.6921685314508,
7.55785582193789));
#380029=CARTESIAN_POINT('Ctrl Pts',(0.00576970483280572,2.66725815417458,
7.59443891967696));
#380030=CARTESIAN_POINT('Ctrl Pts',(0.00300146885025822,2.66217189216599,
7.58783901202978));
#380031=CARTESIAN_POINT('Ctrl Pts',(-0.00519228551543038,2.66439485581461,
7.58560008491213));
#380032=CARTESIAN_POINT('Ctrl Pts',(0.0391111754616935,2.74606032550152,
7.50366116523554));
#380033=CARTESIAN_POINT('Ctrl Pts',(0.0398554269668709,2.74620254791117,
7.50350835821027));
#380034=CARTESIAN_POINT('Ctrl Pts',(0.0405442017937646,2.74630907137797,
7.50345484956));
#380035=CARTESIAN_POINT('Ctrl Pts',(0.0411978859975111,2.74638365637749,
7.50349758195598));
#380036=CARTESIAN_POINT('Ctrl Pts',(0.0415332744725173,2.74642192401361,
7.50351950684424));
#380037=CARTESIAN_POINT('Ctrl Pts',(0.0418924680760451,2.74645568442726,
7.50357029184312));
#380038=CARTESIAN_POINT('Ctrl Pts',(0.0422397292057554,2.74647871828665,
7.50365515313923));
#380039=CARTESIAN_POINT('Ctrl Pts',(0.0427739574431695,2.74651415368973,
7.50378570417639));
#380040=CARTESIAN_POINT('Ctrl Pts',(0.0432956039785114,2.74652558920171,
7.50400001621911));
#380041=CARTESIAN_POINT('Ctrl Pts',(0.0437650136951304,2.7465098845443,
7.50428903009635));
#380042=CARTESIAN_POINT('Ctrl Pts',(0.0438171145622515,2.74650814144815,
7.50432110841318));
#380043=CARTESIAN_POINT('Ctrl Pts',(0.04386859742804,2.7465060803685,7.50435406373354));
#380044=CARTESIAN_POINT('Ctrl Pts',(0.0439194270703296,2.7465037088339,
7.50438785222352));
#380045=CARTESIAN_POINT('Ctrl Pts',(0.0442297664683503,2.74648922947526,
7.50459414719561));
#380046=CARTESIAN_POINT('Ctrl Pts',(0.0445206726054137,2.74646243160482,
7.50483629897752));
#380047=CARTESIAN_POINT('Ctrl Pts',(0.0447811216729627,2.74642565232408,
7.5050991045531));
#380048=CARTESIAN_POINT('Ctrl Pts',(0.0453556984756082,2.74634451353664,
7.50567888004914));
#380049=CARTESIAN_POINT('Ctrl Pts',(0.0458047587608243,2.74621211426885,
7.50637912803144));
#380050=CARTESIAN_POINT('Ctrl Pts',(0.0461444808270324,2.74605479234556,
7.50710440483569));
#380051=CARTESIAN_POINT('Ctrl Pts',(0.0462277874220944,2.74601621388668,
7.50728225710685));
#380052=CARTESIAN_POINT('Ctrl Pts',(0.0463062389178228,2.74597550121701,
7.50746498566954));
#380053=CARTESIAN_POINT('Ctrl Pts',(0.0463781958941233,2.74593397446876,
7.50764697238949));
#380054=CARTESIAN_POINT('Ctrl Pts',(0.0467650167956208,2.74571073809862,
7.50862528291182));
#380055=CARTESIAN_POINT('Ctrl Pts',(0.047001339897482,2.74544729614725,
7.50965856837422));
#380056=CARTESIAN_POINT('Ctrl Pts',(0.0471465970325937,2.74517302978349,
7.51067959873202));
#380057=CARTESIAN_POINT('Ctrl Pts',(0.0472265322172639,2.74502210065757,
7.51124147302579));
#380058=CARTESIAN_POINT('Ctrl Pts',(0.0472785253772168,2.74486765340863,
7.51180065547253));
#380059=CARTESIAN_POINT('Ctrl Pts',(0.0473100357766603,2.74471340164584,
7.51235175716501));
#380060=CARTESIAN_POINT('Ctrl Pts',(0.0474189167589901,2.7441804003588,
7.51425603304535));
#380061=CARTESIAN_POINT('Ctrl Pts',(0.0472902783286506,2.74358496893378,
7.51626900505179));
#380062=CARTESIAN_POINT('Ctrl Pts',(0.0469717238008028,2.74296420982058,
7.51827788969242));
#380063=CARTESIAN_POINT('Ctrl Pts',(0.0469544830277703,2.7429306131643,
7.51838661432544));
#380064=CARTESIAN_POINT('Ctrl Pts',(0.0469366766840814,2.74289693867703,
7.51849533314856));
#380065=CARTESIAN_POINT('Ctrl Pts',(0.0469183093502092,2.74286319116668,
7.51860402984325));
#380066=CARTESIAN_POINT('Origin',(0.,9.23979071467924E-16,7.49482233047033));
#380067=CARTESIAN_POINT('Origin',(0.0389852998002483,2.73722238709234,7.49482233047033));
#380068=CARTESIAN_POINT('Ctrl Pts',(-0.00603856833113048,2.66775215476039,
8.85049129520029));
#380069=CARTESIAN_POINT('Ctrl Pts',(-0.00883014741545966,2.67288130658491,
8.85711686593484));
#380070=CARTESIAN_POINT('Ctrl Pts',(-0.0170742924659647,2.67061528926368,
8.85933012996512));
#380071=CARTESIAN_POINT('Ctrl Pts',(-0.0174472646350165,2.68871410270986,
8.82945683644723));
#380072=CARTESIAN_POINT('Ctrl Pts',(-0.0202620155135629,2.69388582959568,
8.8360746990239));
#380073=CARTESIAN_POINT('Ctrl Pts',(-0.0285204257242725,2.69157699801036,
8.8382956714852));
#380074=CARTESIAN_POINT('Ctrl Pts',(-0.0288389553570734,2.70964480518555,
8.80838214965002));
#380075=CARTESIAN_POINT('Ctrl Pts',(-0.0316648145567818,2.71483694212032,
8.81501364461994));
#380076=CARTESIAN_POINT('Ctrl Pts',(-0.0399486090321783,2.71250722933019,
8.81722098428721));
#380077=CARTESIAN_POINT('Ctrl Pts',(-0.04021493265483,2.73054663635347,
8.78727029226991));
#380078=CARTESIAN_POINT('Ctrl Pts',(-0.0430412612390256,2.73573963571921,
8.79393457792714));
#380079=CARTESIAN_POINT('Ctrl Pts',(-0.0513601984344042,2.73340839160553,
8.79610912703474));
#380080=CARTESIAN_POINT('Origin',(-0.0170177834786405,2.66177663513908,
8.85049129520029));
#380081=CARTESIAN_POINT('Ctrl Pts',(0.0391111642587046,2.74605953891717,
7.50366195182966));
#380082=CARTESIAN_POINT('Ctrl Pts',(0.0391633148679688,2.74972111945349,
7.50000065167735));
#380083=CARTESIAN_POINT('Ctrl Pts',(0.0391633148680856,2.74972111945349,
7.49482233047108));
#380084=CARTESIAN_POINT('Ctrl Pts',(0.0464182127131564,2.74745983977445,
7.50215800491337));
#380085=CARTESIAN_POINT('Ctrl Pts',(0.0486957095368234,2.74958532922222,
7.49877273257267));
#380086=CARTESIAN_POINT('Ctrl Pts',(0.0521474832453746,2.74953619049074,
7.49481816995647));
#380087=CARTESIAN_POINT('Ctrl Pts',(0.0482654124422666,2.74533902165334,
7.51043025814041));
#380088=CARTESIAN_POINT('Ctrl Pts',(0.0523537600593804,2.74950773497384,
7.51006209594513));
#380089=CARTESIAN_POINT('Ctrl Pts',(0.0581644280551635,2.74938482197663,
7.50731281821699));
#380090=CARTESIAN_POINT('Ctrl Pts',(0.0469175869148853,2.74286186359761,
7.51860402984325));
#380091=CARTESIAN_POINT('Ctrl Pts',(0.0505543270057753,2.74954580995451,
7.51860402984325));
#380092=CARTESIAN_POINT('Ctrl Pts',(0.0581618967557014,2.74938487552503,
7.51860402984325));
#380093=CARTESIAN_POINT('Origin',(0.0578975244977155,2.73688767154537,7.51860402984325));
#380094=CARTESIAN_POINT('Ctrl Pts',(0.00603856833113047,2.66775215476039,
8.85049129520029));
#380095=CARTESIAN_POINT('Ctrl Pts',(0.00883014741545964,2.67288130658491,
8.85711686593484));
#380096=CARTESIAN_POINT('Ctrl Pts',(0.0170742924659647,2.67061528926368,
8.85933012996512));
#380097=CARTESIAN_POINT('Ctrl Pts',(0.0035688986120927,2.66321446818132,
8.86332496987232));
#380098=CARTESIAN_POINT('Ctrl Pts',(0.00818107962988514,2.66349674576787,
8.86648636486738));
#380099=CARTESIAN_POINT('Ctrl Pts',(0.0101502424853851,2.65792911615186,
8.87206031107457));
#380100=CARTESIAN_POINT('Ctrl Pts',(-0.00355211642776816,2.66318363317047,
8.86341338519876));
#380101=CARTESIAN_POINT('Ctrl Pts',(-0.0081791237408215,2.6634371562646,
8.86654584966058));
#380102=CARTESIAN_POINT('Ctrl Pts',(-0.0100991546002723,2.65783022891655,
8.87215952290714));
#380103=CARTESIAN_POINT('Ctrl Pts',(-0.0060385683311304,2.66775215476039,
8.85049129520029));
#380104=CARTESIAN_POINT('Ctrl Pts',(-0.00883014741545944,2.67288130658491,
8.85711686593484));
#380105=CARTESIAN_POINT('Ctrl Pts',(-0.0170742924659645,2.67061528926368,
8.85933012996512));
#380106=CARTESIAN_POINT('Origin',(0.0170177834786405,2.66177663513908,8.85049129520029));
#380107=CARTESIAN_POINT('Origin',(0.0578975244977156,2.73688767154537,9.));
#380108=CARTESIAN_POINT('Origin',(0.0578975244977156,2.73688767154537,8.75721825406948));
#380109=CARTESIAN_POINT('Ctrl Pts',(0.0402149326548301,2.73054663635347,
8.78727029226991));
#380110=CARTESIAN_POINT('Ctrl Pts',(0.0430412612390258,2.73573963571921,
8.79393457792714));
#380111=CARTESIAN_POINT('Ctrl Pts',(0.0513601984344043,2.73340839160553,
8.79610912703474));
#380112=CARTESIAN_POINT('Ctrl Pts',(0.0288389553570644,2.70964480518553,
8.80838214965001));
#380113=CARTESIAN_POINT('Ctrl Pts',(0.0316648145567926,2.71483694212031,
8.81501364461994));
#380114=CARTESIAN_POINT('Ctrl Pts',(0.0399486090321813,2.71250722933019,
8.81722098428722));
#380115=CARTESIAN_POINT('Ctrl Pts',(0.0174472646350206,2.68871410270986,
8.82945683644722));
#380116=CARTESIAN_POINT('Ctrl Pts',(0.0202620155135602,2.69388582959568,
8.8360746990239));
#380117=CARTESIAN_POINT('Ctrl Pts',(0.0285204257242735,2.69157699801037,
8.83829567148519));
#380118=CARTESIAN_POINT('Ctrl Pts',(0.00603856833113056,2.66775215476039,
8.85049129520029));
#380119=CARTESIAN_POINT('Ctrl Pts',(0.00883014741545973,2.67288130658491,
8.85711686593484));
#380120=CARTESIAN_POINT('Ctrl Pts',(0.0170742924659648,2.67061528926368,
8.85933012996512));
#380121=CARTESIAN_POINT('Origin',(0.05119414780234,2.72457111673216,8.78727029226991));
#380122=CARTESIAN_POINT('Ctrl Pts',(0.0468298108357679,2.74270054843764,
8.75374538247848));
#380123=CARTESIAN_POINT('Ctrl Pts',(0.0504509039511556,2.74938127167972,
8.75304829418601));
#380124=CARTESIAN_POINT('Ctrl Pts',(0.0580822141425596,2.74919756546978,
8.75272238421917));
#380125=CARTESIAN_POINT('Ctrl Pts',(0.0474608175312104,2.7438599394262,
8.7676940844502));
#380126=CARTESIAN_POINT('Ctrl Pts',(0.0511736401317078,2.75070845045484,
8.76974318093969));
#380127=CARTESIAN_POINT('Ctrl Pts',(0.0587246898268686,2.7507060460072,
8.77077869880429));
#380128=CARTESIAN_POINT('Ctrl Pts',(0.0442266366581527,2.73791756168736,
8.78108014887991));
#380129=CARTESIAN_POINT('Ctrl Pts',(0.0473697799404577,2.74372323887499,
8.78639403366324));
#380130=CARTESIAN_POINT('Ctrl Pts',(0.0554304751827418,2.74298346327396,
8.78812224174742));
#380131=CARTESIAN_POINT('Ctrl Pts',(0.0389265281907873,2.72817931634984,
8.78944554828685));
#380132=CARTESIAN_POINT('Ctrl Pts',(0.041570530208704,2.73307479088723,
8.79673892988686));
#380133=CARTESIAN_POINT('Ctrl Pts',(0.0500624819120103,2.73035627831871,
8.79894799272499));
#380134=CARTESIAN_POINT('Origin',(-0.16489730596466,2.66265786424426,7.5));
#380135=CARTESIAN_POINT('',(-0.16489730596466,2.66265786424426,7.59394543036555));
#380136=CARTESIAN_POINT('',(-0.16489730596466,2.66265786424426,8.85049129520029));
#380137=CARTESIAN_POINT('',(-0.16489730596466,2.66265786424426,7.5));
#380138=CARTESIAN_POINT('',(-0.13481441689611,2.72751301502058,8.78727029226991));
#380139=CARTESIAN_POINT('Ctrl Pts',(-0.16489730596466,2.66265786424426,
8.85049129520029));
#380140=CARTESIAN_POINT('Ctrl Pts',(-0.154855100144266,2.68430767225054,
8.82945686509571));
#380141=CARTESIAN_POINT('Ctrl Pts',(-0.144827823277113,2.70592529519936,
8.80838212259895));
#380142=CARTESIAN_POINT('Ctrl Pts',(-0.13481441689611,2.72751301502058,
8.78727029226991));
#380143=CARTESIAN_POINT('',(-0.128913937383377,2.74023375097047,8.75721825406948));
#380144=CARTESIAN_POINT('Origin',(-0.146670710194622,2.70195272855935,8.75937679713156));
#380145=CARTESIAN_POINT('',(-0.128913937383377,2.74023375097047,7.51860402984325));
#380146=CARTESIAN_POINT('',(-0.128913937383377,2.74023375097047,7.5));
#380147=CARTESIAN_POINT('Ctrl Pts',(-0.128913937383377,2.74023375097047,
7.51860402984325));
#380148=CARTESIAN_POINT('Ctrl Pts',(-0.133547846342482,2.73024359133049,
7.52834476460825));
#380149=CARTESIAN_POINT('Ctrl Pts',(-0.138184763568422,2.72024694622305,
7.53807742314407));
#380150=CARTESIAN_POINT('Ctrl Pts',(-0.142824790067749,2.71024359788991,
7.54780169004674));
#380151=CARTESIAN_POINT('Ctrl Pts',(-0.150174341270648,2.69439883476507,
7.5632044032688));
#380152=CARTESIAN_POINT('Ctrl Pts',(-0.157531702584656,2.67853723396437,
7.57858609112103));
#380153=CARTESIAN_POINT('Ctrl Pts',(-0.16489730596466,2.66265786424426,
7.59394543036555));
#380154=CARTESIAN_POINT('Origin',(-0.323616654966455,2.89450777438995,7.5));
#380155=CARTESIAN_POINT('',(-0.222557758686723,2.73422161816809,8.75721825406948));
#380156=CARTESIAN_POINT('',(-0.215079030421415,2.72235985585717,8.78727029226991));
#380157=CARTESIAN_POINT('Origin',(-0.196095228656818,2.69225027889422,8.75658640621001));
#380158=CARTESIAN_POINT('',(-0.176949628854379,2.66188407944157,8.85049129520029));
#380159=CARTESIAN_POINT('Ctrl Pts',(-0.215079030421415,2.72235985585717,
8.78727029226991));
#380160=CARTESIAN_POINT('Ctrl Pts',(-0.202387257630408,2.70222985690407,
8.80838212259895));
#380161=CARTESIAN_POINT('Ctrl Pts',(-0.189677904302661,2.68207197404603,
8.82945686509571));
#380162=CARTESIAN_POINT('Ctrl Pts',(-0.176949628854379,2.66188407944157,
8.85049129520029));
#380163=CARTESIAN_POINT('',(-0.176949628854379,2.66188407944157,7.59394543036555));
#380164=CARTESIAN_POINT('',(-0.176949628854379,2.66188407944157,7.5));
#380165=CARTESIAN_POINT('',(-0.222557758686723,2.73422161816809,7.51860402984325));
#380166=CARTESIAN_POINT('Ctrl Pts',(-0.176949628854379,2.66188407944157,
7.59394543036555));
#380167=CARTESIAN_POINT('Ctrl Pts',(-0.186285369461595,2.67669118730146,
7.57858609112103));
#380168=CARTESIAN_POINT('Ctrl Pts',(-0.195610663430972,2.69148172609634,
7.56320440326857));
#380169=CARTESIAN_POINT('Ctrl Pts',(-0.204926058256057,2.70625656418747,
7.54780169004651));
#380170=CARTESIAN_POINT('Ctrl Pts',(-0.210807189994148,2.71558443175019,
7.53807742314383));
#380171=CARTESIAN_POINT('Ctrl Pts',(-0.216684380796579,2.72490604872585,
7.52834476460825));
#380172=CARTESIAN_POINT('Ctrl Pts',(-0.222557758686721,2.73422161816808,
7.51860402984324));
#380173=CARTESIAN_POINT('',(-0.222557758686723,2.73422161816809,7.5));
#380174=CARTESIAN_POINT('Origin',(-0.17113403648067,2.66555075509437,7.5));
#380175=CARTESIAN_POINT('Ctrl Pts',(-0.176949628854379,2.66188407944157,
8.85049129520029));
#380176=CARTESIAN_POINT('Ctrl Pts',(-0.176846342464761,2.6617202603322,
8.85097269580138));
#380177=CARTESIAN_POINT('Ctrl Pts',(-0.176737243973737,2.66156299420173,
8.85143669361005));
#380178=CARTESIAN_POINT('Ctrl Pts',(-0.176616591392395,2.66140553779028,
8.8519052845931));
#380179=CARTESIAN_POINT('Ctrl Pts',(-0.1763806025948,2.66109756303501,8.85282181883899));
#380180=CARTESIAN_POINT('Ctrl Pts',(-0.176106325903489,2.66079690254988,
8.85372622499636));
#380181=CARTESIAN_POINT('Ctrl Pts',(-0.175778066416341,2.66050922989146,
8.85462257735071));
#380182=CARTESIAN_POINT('Ctrl Pts',(-0.175505557048785,2.6602704142676,
8.85536669723986));
#380183=CARTESIAN_POINT('Ctrl Pts',(-0.175195802884907,2.66004047128033,
8.85610498449051));
#380184=CARTESIAN_POINT('Ctrl Pts',(-0.174835028063543,2.65982905303466,
8.85681338218371));
#380185=CARTESIAN_POINT('Ctrl Pts',(-0.174507624346547,2.65963719064467,
8.85745625420284));
#380186=CARTESIAN_POINT('Ctrl Pts',(-0.174134397753541,2.65945766139716,
8.85808743050666));
#380187=CARTESIAN_POINT('Ctrl Pts',(-0.173693040886597,2.65930836015582,
8.8586680450841));
#380188=CARTESIAN_POINT('Ctrl Pts',(-0.17348940839563,2.65923947579952,
8.85893592806395));
#380189=CARTESIAN_POINT('Ctrl Pts',(-0.17327110340926,2.65917719921061,
8.85919241173848));
#380190=CARTESIAN_POINT('Ctrl Pts',(-0.173034988239252,2.65912457290272,
8.85943017985534));
#380191=CARTESIAN_POINT('Ctrl Pts',(-0.172716162862172,2.65905351180801,
8.8597512372));
#380192=CARTESIAN_POINT('Ctrl Pts',(-0.172356609902529,2.65899886258521,
8.86004599534706));
#380193=CARTESIAN_POINT('Ctrl Pts',(-0.171959084215928,2.65897157865952,
8.86026130871721));
#380194=CARTESIAN_POINT('Ctrl Pts',(-0.171813538854627,2.65896158924511,
8.86034014101235));
#380195=CARTESIAN_POINT('Ctrl Pts',(-0.171660717848717,2.65895510579684,
8.86040910639693));
#380196=CARTESIAN_POINT('Ctrl Pts',(-0.171504770462638,2.65895264102899,
8.86046313645507));
#380197=CARTESIAN_POINT('Ctrl Pts',(-0.171261415872711,2.6589487947794,
8.8605474499083));
#380198=CARTESIAN_POINT('Ctrl Pts',(-0.171003802956377,2.65895477658666,
8.86059655985669));
#380199=CARTESIAN_POINT('Ctrl Pts',(-0.170748446413557,2.65896990994078,
8.86059725258816));
#380200=CARTESIAN_POINT('Ctrl Pts',(-0.170492499895108,2.658985078259,8.86059794692011));
#380201=CARTESIAN_POINT('Ctrl Pts',(-0.170236138887563,2.65901226079576,
8.86056369958366));
#380202=CARTESIAN_POINT('Ctrl Pts',(-0.169992948659137,2.65904623288096,
8.86048590497774));
#380203=CARTESIAN_POINT('Ctrl Pts',(-0.169929483250163,2.65905509858373,
8.86046560290182));
#380204=CARTESIAN_POINT('Ctrl Pts',(-0.169866101725982,2.65906463173742,
8.86044257503091));
#380205=CARTESIAN_POINT('Ctrl Pts',(-0.169804757745728,2.65907450529864,
8.86041778462583));
#380206=CARTESIAN_POINT('Ctrl Pts',(-0.169391988880148,2.65914094211361,
8.86025097596201));
#380207=CARTESIAN_POINT('Ctrl Pts',(-0.169016136888504,2.65923203389475,
8.8599848982295));
#380208=CARTESIAN_POINT('Ctrl Pts',(-0.168686176277915,2.65933688780355,
8.85968173251461));
#380209=CARTESIAN_POINT('Ctrl Pts',(-0.168511646019403,2.65939234951389,
8.85952137522076));
#380210=CARTESIAN_POINT('Ctrl Pts',(-0.168346533239064,2.65945254867042,
8.85934740853961));
#380211=CARTESIAN_POINT('Ctrl Pts',(-0.16819263389931,2.65951517582375,
8.8591675900182));
#380212=CARTESIAN_POINT('Ctrl Pts',(-0.16757464805491,2.65976665639733,
8.85844552518695));
#380213=CARTESIAN_POINT('Ctrl Pts',(-0.167101404538683,2.66006869733527,
8.85759444184124));
#380214=CARTESIAN_POINT('Ctrl Pts',(-0.166737667185756,2.66034962329277,
8.85683498915138));
#380215=CARTESIAN_POINT('Ctrl Pts',(-0.166699603040485,2.66037902144606,
8.85675551444998));
#380216=CARTESIAN_POINT('Ctrl Pts',(-0.166662753168069,2.66040820147624,
8.85667699793651));
#380217=CARTESIAN_POINT('Ctrl Pts',(-0.166627087527507,2.66043708934255,
8.85659965593547));
#380218=CARTESIAN_POINT('Ctrl Pts',(-0.166145670891262,2.66082701923615,
8.85555568965886));
#380219=CARTESIAN_POINT('Ctrl Pts',(-0.165739313269825,2.66127129211021,
8.85434650606346));
#380220=CARTESIAN_POINT('Ctrl Pts',(-0.165401420054749,2.66176790975638,
8.85297329937117));
#380221=CARTESIAN_POINT('Ctrl Pts',(-0.165211375709405,2.66204722692299,
8.85220095427747));
#380222=CARTESIAN_POINT('Ctrl Pts',(-0.165043172113059,2.66234339408063,
8.85137579139183));
#380223=CARTESIAN_POINT('Ctrl Pts',(-0.16489730596466,2.66265786424426,
8.85049129520029));
#380224=CARTESIAN_POINT('Origin',(-0.171134036480669,2.66555075509437,7.59394543036555));
#380225=CARTESIAN_POINT('Ctrl Pts',(-0.176649753621982,2.66140845730323,
7.59443877723642));
#380226=CARTESIAN_POINT('Ctrl Pts',(-0.173561327260499,2.65651000690965,
7.58783886950016));
#380227=CARTESIAN_POINT('Ctrl Pts',(-0.165526833445772,2.65925337904586,
7.58559994247159));
#380228=CARTESIAN_POINT('Ctrl Pts',(-0.193509382518731,2.68814895428735,
7.56670252222133));
#380229=CARTESIAN_POINT('Ctrl Pts',(-0.190425419810154,2.68325758354529,
7.56004874999026));
#380230=CARTESIAN_POINT('Ctrl Pts',(-0.18233641492009,2.68599699171951,
7.55786368756704));
#380231=CARTESIAN_POINT('Ctrl Pts',(-0.210337527743017,2.71483951606509,
7.53888913333558));
#380232=CARTESIAN_POINT('Ctrl Pts',(-0.207235236893081,2.70991907566721,
7.53222002137277));
#380233=CARTESIAN_POINT('Ctrl Pts',(-0.199116189248093,2.7126909901786,
7.53005029815326));
#380234=CARTESIAN_POINT('Ctrl Pts',(-0.227133427809856,2.74147893487042,
7.51101258149734));
#380235=CARTESIAN_POINT('Ctrl Pts',(-0.223993531557809,2.73649884979426,
7.5043616886572));
#380236=CARTESIAN_POINT('Ctrl Pts',(-0.215865257414837,2.73933409951895,
7.50217374673251));
#380237=CARTESIAN_POINT('',(-0.214971506492209,2.73791238843283,7.50366116523517));
#380238=CARTESIAN_POINT('Ctrl Pts',(-0.222557758686723,2.73422161816808,
7.51860402984325));
#380239=CARTESIAN_POINT('Ctrl Pts',(-0.222793285245618,2.73459517901432,
7.51734760759493));
#380240=CARTESIAN_POINT('Ctrl Pts',(-0.222955788562301,2.7349644763634,
7.51608817408572));
#380241=CARTESIAN_POINT('Ctrl Pts',(-0.223032672233694,2.73533403919153,
7.51481005913119));
#380242=CARTESIAN_POINT('Ctrl Pts',(-0.223102315300436,2.73566879803223,
7.51365231206383));
#380243=CARTESIAN_POINT('Ctrl Pts',(-0.223102049090854,2.73600419561941,
7.51247773061042));
#380244=CARTESIAN_POINT('Ctrl Pts',(-0.222994953185447,2.736334399064,7.51129758471022));
#380245=CARTESIAN_POINT('Ctrl Pts',(-0.222861845205841,2.73674480423496,
7.50983079813402));
#380246=CARTESIAN_POINT('Ctrl Pts',(-0.222555569253571,2.73713006948336,
7.50839324291155));
#380247=CARTESIAN_POINT('Ctrl Pts',(-0.222009357599783,2.73744170500765,
7.50715379678855));
#380248=CARTESIAN_POINT('Ctrl Pts',(-0.221757023554444,2.73758567164031,
7.50658120839351));
#380249=CARTESIAN_POINT('Ctrl Pts',(-0.221412902846589,2.73772613760701,
7.50598221009429));
#380250=CARTESIAN_POINT('Ctrl Pts',(-0.220976588784301,2.73783870041343,
7.50545747549611));
#380251=CARTESIAN_POINT('Ctrl Pts',(-0.220743758095481,2.73789876741109,
7.50517746087247));
#380252=CARTESIAN_POINT('Ctrl Pts',(-0.220482200112806,2.73795173606974,
7.50491486231392));
#380253=CARTESIAN_POINT('Ctrl Pts',(-0.220198510259498,2.73799456886009,
7.50468370960992));
#380254=CARTESIAN_POINT('Ctrl Pts',(-0.219774304443913,2.7380586173925,
7.50433806340446));
#380255=CARTESIAN_POINT('Ctrl Pts',(-0.219287809037159,2.73810137257825,
7.50405484070984));
#380256=CARTESIAN_POINT('Ctrl Pts',(-0.218771725882347,2.73811924129067,
7.50385766036131));
#380257=CARTESIAN_POINT('Ctrl Pts',(-0.218716538810688,2.73812115207172,
7.50383657498791));
#380258=CARTESIAN_POINT('Ctrl Pts',(-0.218661038309179,2.73812279184612,
7.50381643264937));
#380259=CARTESIAN_POINT('Ctrl Pts',(-0.218605282305324,2.73812416636047,
7.50379723213559));
#380260=CARTESIAN_POINT('Ctrl Pts',(-0.218233092740536,2.73813334169338,
7.50366906242519));
#380261=CARTESIAN_POINT('Ctrl Pts',(-0.217841404285933,2.73813017779315,
7.50358235568538));
#380262=CARTESIAN_POINT('Ctrl Pts',(-0.217463938128411,2.73811805291127,
7.5035341175365));
#380263=CARTESIAN_POINT('Ctrl Pts',(-0.216897970346127,2.73809987302315,
7.50346178989176));
#380264=CARTESIAN_POINT('Ctrl Pts',(-0.216289890791823,2.7380562513047,
7.50346967198527));
#380265=CARTESIAN_POINT('Ctrl Pts',(-0.215694262731964,2.73799506025502,
7.50354272648692));
#380266=CARTESIAN_POINT('Ctrl Pts',(-0.215449268582172,2.7379698911097,
7.50357277531559));
#380267=CARTESIAN_POINT('Ctrl Pts',(-0.215206692060793,2.73794192399818,
7.50361331098761));
#380268=CARTESIAN_POINT('Ctrl Pts',(-0.21497150649232,2.73791238843424,
7.50366116523659));
#380269=CARTESIAN_POINT('',(-0.171321629291009,2.66847266454068,7.57603338622103));
#380270=CARTESIAN_POINT('Origin',(-0.171884966568795,2.677291629373,7.58486873427628));
#380271=CARTESIAN_POINT('Ctrl Pts',(-0.214971506527132,2.73791238847831,
7.50366116529969));
#380272=CARTESIAN_POINT('Ctrl Pts',(-0.200444582347927,2.71480402911006,
7.52783573079709));
#380273=CARTESIAN_POINT('Ctrl Pts',(-0.185895295086754,2.69165855688567,
7.55196141284068));
#380274=CARTESIAN_POINT('Ctrl Pts',(-0.171321630229604,2.66847266536934,
7.57603338728831));
#380275=CARTESIAN_POINT('Ctrl Pts',(-0.177349390934668,2.662847783649,7.59639677331371));
#380276=CARTESIAN_POINT('Ctrl Pts',(-0.170168085926414,2.64604002430609,
7.59959882295466));
#380277=CARTESIAN_POINT('Ctrl Pts',(-0.16467589448117,2.66349123187844,
7.59642833564546));
#380278=CARTESIAN_POINT('Ctrl Pts',(-0.176413316036416,2.65906111388935,
7.58707626057422));
#380279=CARTESIAN_POINT('Ctrl Pts',(-0.170591808819725,2.65559378858556,
7.58809943920599));
#380280=CARTESIAN_POINT('Ctrl Pts',(-0.165206893457788,2.65968244207271,
7.58710240504253));
#380281=CARTESIAN_POINT('Ctrl Pts',(-0.173206625605347,2.66422277725894,
7.5801537675693));
#380282=CARTESIAN_POINT('Ctrl Pts',(-0.170967584492428,2.66245756727403,
7.58205880659761));
#380283=CARTESIAN_POINT('Ctrl Pts',(-0.168967669707232,2.66443933817145,
7.58020924244127));
#380284=CARTESIAN_POINT('Ctrl Pts',(-0.171321629238191,2.66847266371479,
7.57603338509286));
#380285=CARTESIAN_POINT('Ctrl Pts',(-0.171321629238191,2.66847266371479,
7.57603338509286));
#380286=CARTESIAN_POINT('Ctrl Pts',(-0.171321629238191,2.6684726637148,
7.57603338509286));
#380287=CARTESIAN_POINT('Origin',(-0.171890661196598,2.67729126376561,7.58486873427622));
#380288=CARTESIAN_POINT('Ctrl Pts',(-0.125292469645935,2.74804120708308,
7.51098857897448));
#380289=CARTESIAN_POINT('Ctrl Pts',(-0.127769759546158,2.74270046305981,
7.50433767179957));
#380290=CARTESIAN_POINT('Ctrl Pts',(-0.1361938934592,2.74447303714785,7.50214974420965));
#380291=CARTESIAN_POINT('Ctrl Pts',(-0.138547713792453,2.71946446846797,
7.53887321589168));
#380292=CARTESIAN_POINT('Ctrl Pts',(-0.140995321363277,2.71418771603619,
7.5322040745206));
#380293=CARTESIAN_POINT('Ctrl Pts',(-0.149402205571103,2.71589862744196,
7.53003438070911));
#380294=CARTESIAN_POINT('Ctrl Pts',(-0.151828412897386,2.6908328519732,
7.56669465659235));
#380295=CARTESIAN_POINT('Ctrl Pts',(-0.154261555562458,2.68558728416726,
7.56004085833303));
#380296=CARTESIAN_POINT('Ctrl Pts',(-0.162634477916442,2.68726978866384,
7.55785582193789));
#380297=CARTESIAN_POINT('Ctrl Pts',(-0.165133966327888,2.66214765249215,
7.59443891967696));
#380298=CARTESIAN_POINT('Ctrl Pts',(-0.167570636746948,2.656894479266,7.58783901202978));
#380299=CARTESIAN_POINT('Ctrl Pts',(-0.17588998193549,2.65858789995271,
7.58560008491213));
#380300=CARTESIAN_POINT('',(-0.136909871778125,2.74292411166389,7.50366116523517));
#380301=CARTESIAN_POINT('Ctrl Pts',(-0.136909871778144,2.74292411166427,
7.50366116523554));
#380302=CARTESIAN_POINT('Ctrl Pts',(-0.136176261638576,2.74311372622038,
7.50350835821027));
#380303=CARTESIAN_POINT('Ctrl Pts',(-0.135495726955387,2.74326416077797,
7.50345484956));
#380304=CARTESIAN_POINT('Ctrl Pts',(-0.134848164493271,2.74338047422534,
7.50349758195598));
#380305=CARTESIAN_POINT('Ctrl Pts',(-0.134515916925721,2.74344015164987,
7.50351950684424));
#380306=CARTESIAN_POINT('Ctrl Pts',(-0.134159624361105,2.74349685631232,
7.50357029184312));
#380307=CARTESIAN_POINT('Ctrl Pts',(-0.133814552501067,2.74354209194315,
7.50365515313923));
#380308=CARTESIAN_POINT('Ctrl Pts',(-0.133283692246939,2.74361168266108,
7.50378570417639));
#380309=CARTESIAN_POINT('Ctrl Pts',(-0.132763850166124,2.74365651668585,
7.50400001621911));
#380310=CARTESIAN_POINT('Ctrl Pts',(-0.132294398701261,2.74367091947915,
7.50428903009634));
#380311=CARTESIAN_POINT('Ctrl Pts',(-0.1322422932004,2.74367251807839,7.50432110841318));
#380312=CARTESIAN_POINT('Ctrl Pts',(-0.132190784057849,2.74367375975199,
7.50435406373354));
#380313=CARTESIAN_POINT('Ctrl Pts',(-0.132139906905762,2.74367464975632,
7.50438785222352));
#380314=CARTESIAN_POINT('Ctrl Pts',(-0.131829277437625,2.74368008366058,
7.50459414719561));
#380315=CARTESIAN_POINT('Ctrl Pts',(-0.131537252052967,2.74367197926943,
7.50483629897752));
#380316=CARTESIAN_POINT('Ctrl Pts',(-0.131274981649352,2.74365196258472,
7.5050991045531));
#380317=CARTESIAN_POINT('Ctrl Pts',(-0.130696386796411,2.74360780376776,
7.50567888004914));
#380318=CARTESIAN_POINT('Ctrl Pts',(-0.130239766303498,2.74350444791973,
7.50637912803145));
#380319=CARTESIAN_POINT('Ctrl Pts',(-0.129890662582477,2.74336921529871,
7.50710440483569));
#380320=CARTESIAN_POINT('Ctrl Pts',(-0.129805055419403,2.74333605357529,
7.50728225710685));
#380321=CARTESIAN_POINT('Ctrl Pts',(-0.129724156640984,2.74330045095875,
7.50746498566955));
#380322=CARTESIAN_POINT('Ctrl Pts',(-0.129649686880113,2.74326361983096,
7.50764697238949));
#380323=CARTESIAN_POINT('Ctrl Pts',(-0.129249357940303,2.74306562582414,
7.50862528291182));
#380324=CARTESIAN_POINT('Ctrl Pts',(-0.128996641605824,2.74281786641564,
7.50965856837422));
#380325=CARTESIAN_POINT('Ctrl Pts',(-0.128834110610815,2.74255347021813,
7.51067959873202));
#380326=CARTESIAN_POINT('Ctrl Pts',(-0.128744669599255,2.74240797265715,
7.51124147302578));
#380327=CARTESIAN_POINT('Ctrl Pts',(-0.128682887795611,2.74225717394985,
7.51180065547253));
#380328=CARTESIAN_POINT('Ctrl Pts',(-0.128641559193288,2.74210525799208,
7.51235175716501));
#380329=CARTESIAN_POINT('Ctrl Pts',(-0.128498752408904,2.74158032784183,
7.51425603304536));
#380330=CARTESIAN_POINT('Ctrl Pts',(-0.128588977115408,2.74097787790201,
7.5162690050518));
#380331=CARTESIAN_POINT('Ctrl Pts',(-0.128867104965876,2.7403379843463,
7.51827788969243));
#380332=CARTESIAN_POINT('Ctrl Pts',(-0.128882157770732,2.74030335209784,
7.51838661432545));
#380333=CARTESIAN_POINT('Ctrl Pts',(-0.128897769997571,2.74026860594206,
7.51849533314856));
#380334=CARTESIAN_POINT('Ctrl Pts',(-0.128913937383373,2.74023375097047,
7.51860402984325));
#380335=CARTESIAN_POINT('Ctrl Pts',(-0.171321628465918,2.66847266548377,
7.57603338728985));
#380336=CARTESIAN_POINT('Ctrl Pts',(-0.159832559191475,2.69333184005413,
7.55196141284922));
#380337=CARTESIAN_POINT('Ctrl Pts',(-0.148362498662232,2.71814780985154,
7.52783573083104));
#380338=CARTESIAN_POINT('Ctrl Pts',(-0.136909871748466,2.74292411171511,
7.50366116530176));
#380339=CARTESIAN_POINT('Origin',(-5.91995423665249E-17,9.22080657369149E-16,
7.49482233047033));
#380340=CARTESIAN_POINT('Origin',(-0.214279640797787,2.72910067339766,7.49482233047033));
#380341=CARTESIAN_POINT('Origin',(0.,0.,7.50366116523517));
#380342=CARTESIAN_POINT('Origin',(-0.13646924015649,2.7340962668661,7.49482233047033));
#380343=CARTESIAN_POINT('Ctrl Pts',(-0.222557194605718,2.73422072341404,
7.51860402984325));
#380344=CARTESIAN_POINT('Ctrl Pts',(-0.226614772381148,2.74065751987086,
7.51860402984325));
#380345=CARTESIAN_POINT('Ctrl Pts',(-0.234196090687502,2.74000952390803,
7.51860402984325));
#380346=CARTESIAN_POINT('Ctrl Pts',(-0.224063801999056,2.73661074918781,
7.51041458714366));
#380347=CARTESIAN_POINT('Ctrl Pts',(-0.228410872679949,2.74050399234172,
7.51004642900444));
#380348=CARTESIAN_POINT('Ctrl Pts',(-0.234198181525068,2.74000934519844,
7.50729136483011));
#380349=CARTESIAN_POINT('Ctrl Pts',(-0.22234652916969,2.73884115525596,
7.50215815450137));
#380350=CARTESIAN_POINT('Ctrl Pts',(-0.224753845205969,2.74081672959849,
7.49877163671527));
#380351=CARTESIAN_POINT('Ctrl Pts',(-0.228193466700913,2.74054667855528,
7.49481588533168));
#380352=CARTESIAN_POINT('Ctrl Pts',(-0.21497146339957,2.73791183960396,
7.50366171572174));
#380353=CARTESIAN_POINT('Ctrl Pts',(-0.215258086645794,2.74156232030819,
7.50000045605858));
#380354=CARTESIAN_POINT('Ctrl Pts',(-0.215258086645918,2.74156232030818,
7.49482233047317));
#380355=CARTESIAN_POINT('Origin',(-0.233131563002558,2.72755493516299,7.51860402984325));
#380356=CARTESIAN_POINT('Origin',(-0.233131563002558,2.72755493516299,9.));
#380357=CARTESIAN_POINT('Origin',(-0.233131563002558,2.72755493516299,8.75721825406948));
#380358=CARTESIAN_POINT('Ctrl Pts',(-0.213651009822412,2.72009486320776,
8.78942910404912));
#380359=CARTESIAN_POINT('Ctrl Pts',(-0.21660588741381,2.7248193872178,8.7967269950169));
#380360=CARTESIAN_POINT('Ctrl Pts',(-0.22491413159172,2.72155647982373,
8.79893251111266));
#380361=CARTESIAN_POINT('Ctrl Pts',(-0.219514666098731,2.7293950220136,
8.78111911759582));
#380362=CARTESIAN_POINT('Ctrl Pts',(-0.223024018852928,2.73499205277751,
8.78644465894816));
#380363=CARTESIAN_POINT('Ctrl Pts',(-0.231029453604107,2.73371591555135,
8.78817647674133));
#380364=CARTESIAN_POINT('Ctrl Pts',(-0.223169036578443,2.73519110279414,
8.76780923932031));
#380365=CARTESIAN_POINT('Ctrl Pts',(-0.227315996657256,2.74179545430471,
8.76988516158372));
#380366=CARTESIAN_POINT('Ctrl Pts',(-0.23485896000775,2.74130547033627,
8.77093053738832));
#380367=CARTESIAN_POINT('Ctrl Pts',(-0.222456484349946,2.73406094636595,
8.75371302330492));
#380368=CARTESIAN_POINT('Ctrl Pts',(-0.226501019435791,2.74050361175437,
8.7530082828756));
#380369=CARTESIAN_POINT('Ctrl Pts',(-0.23411245922323,2.73982499279172,
8.75267964240738));
#380370=CARTESIAN_POINT('Origin',(-0.225652834737251,2.71569317285207,8.78727029226991));
#380371=CARTESIAN_POINT('Ctrl Pts',(-0.176949628854379,2.66188407944157,
8.85049129520029));
#380372=CARTESIAN_POINT('Ctrl Pts',(-0.180064098225795,2.66682383578754,
8.85711686593484));
#380373=CARTESIAN_POINT('Ctrl Pts',(-0.188146120567861,2.66403427005499,
8.85933012996512));
#380374=CARTESIAN_POINT('Ctrl Pts',(-0.18967792138448,2.68207200113893,
8.82945683644722));
#380375=CARTESIAN_POINT('Ctrl Pts',(-0.192818242734717,2.68705276044922,
8.83607469902389));
#380376=CARTESIAN_POINT('Ctrl Pts',(-0.200911757808369,2.68421955444711,
8.8382956714852));
#380377=CARTESIAN_POINT('Ctrl Pts',(-0.202387241368152,2.70222983111105,
8.80838214965002));
#380378=CARTESIAN_POINT('Ctrl Pts',(-0.205539955892616,2.70723024682303,
8.81501364461987));
#380379=CARTESIAN_POINT('Ctrl Pts',(-0.213657465212923,2.70437457614343,
8.81722098428721));
#380380=CARTESIAN_POINT('Ctrl Pts',(-0.215079030421415,2.72235985585717,
8.78727029226991));
#380381=CARTESIAN_POINT('Ctrl Pts',(-0.218232268622135,2.72736110215464,
8.79393457792714));
#380382=CARTESIAN_POINT('Ctrl Pts',(-0.22638475034565,2.7245016516959,8.79610912703474));
#380383=CARTESIAN_POINT('Origin',(-0.187523433170215,2.65521739643647,8.85049129520029));
#380384=CARTESIAN_POINT('Ctrl Pts',(-0.16489730596466,2.66265786424426,
8.85049129520029));
#380385=CARTESIAN_POINT('Ctrl Pts',(-0.162440088364667,2.66795533476228,
8.85711686593484));
#380386=CARTESIAN_POINT('Ctrl Pts',(-0.154067697566098,2.66622217740361,
8.85933012996512));
#380387=CARTESIAN_POINT('Ctrl Pts',(-0.167071170905058,2.65797126854676,
8.86332496987231));
#380388=CARTESIAN_POINT('Ctrl Pts',(-0.162486551694886,2.65854846961614,
8.86648636486737));
#380389=CARTESIAN_POINT('Ctrl Pts',(-0.160164715441403,2.65311844398962,
8.87206031107457));
#380390=CARTESIAN_POINT('Ctrl Pts',(-0.174175579449871,2.65748425188965,
8.86341338519877));
#380391=CARTESIAN_POINT('Ctrl Pts',(-0.178809323360565,2.65744080071697,
8.86654584966058));
#380392=CARTESIAN_POINT('Ctrl Pts',(-0.180366172242092,2.65172237660299,
8.87215952290714));
#380393=CARTESIAN_POINT('Ctrl Pts',(-0.176949628854379,2.66188407944157,
8.85049129520029));
#380394=CARTESIAN_POINT('Ctrl Pts',(-0.180064098225795,2.66682383578754,
8.85711686593484));
#380395=CARTESIAN_POINT('Ctrl Pts',(-0.188146120567861,2.66403427005499,
8.85933012996512));
#380396=CARTESIAN_POINT('Origin',(-0.153557795935551,2.6573980626986,8.85049129520029));
#380397=CARTESIAN_POINT('Ctrl Pts',(-0.13481441689611,2.72751301502058,
8.78727029226991));
#380398=CARTESIAN_POINT('Ctrl Pts',(-0.132326611918836,2.7328764283063,
8.79393457792714));
#380399=CARTESIAN_POINT('Ctrl Pts',(-0.123875403548937,2.73108297011979,
8.79610912703474));
#380400=CARTESIAN_POINT('Ctrl Pts',(-0.144827836107518,2.70592526753853,
8.80838214965002));
#380401=CARTESIAN_POINT('Ctrl Pts',(-0.142340444294179,2.71128779009166,
8.81501364461991));
#380402=CARTESIAN_POINT('Ctrl Pts',(-0.133924404552004,2.70949360848066,
8.81722098428721));
#380403=CARTESIAN_POINT('Ctrl Pts',(-0.154855086667246,2.6843077013054,
8.82945683644723));
#380404=CARTESIAN_POINT('Ctrl Pts',(-0.152377472675517,2.68964914403163,
8.8360746990239));
#380405=CARTESIAN_POINT('Ctrl Pts',(-0.143988102906735,2.68787417434732,
8.8382956714852));
#380406=CARTESIAN_POINT('Ctrl Pts',(-0.16489730596466,2.66265786424426,
8.85049129520029));
#380407=CARTESIAN_POINT('Ctrl Pts',(-0.162440088364667,2.66795533476228,
8.85711686593484));
#380408=CARTESIAN_POINT('Ctrl Pts',(-0.154067697566098,2.66622217740361,
8.85933012996512));
#380409=CARTESIAN_POINT('Origin',(-0.123474906867001,2.72225321347492,8.78727029226991));
#380410=CARTESIAN_POINT('Ctrl Pts',(-0.128991833512702,2.74006577228906,
8.75374538247847));
#380411=CARTESIAN_POINT('Ctrl Pts',(-0.125806215729227,2.74696477350121,
8.75304829418601));
#380412=CARTESIAN_POINT('Ctrl Pts',(-0.118178814785787,2.74727038445809,
8.75272238421917));
#380413=CARTESIAN_POINT('Ctrl Pts',(-0.128436405723859,2.7412632099223,
8.76769408445022));
#380414=CARTESIAN_POINT('Ctrl Pts',(-0.125169997123756,2.74833553131128,
8.7697431809397));
#380415=CARTESIAN_POINT('Ctrl Pts',(-0.117634307816532,2.74881692921888,
8.7707786988043));
#380416=CARTESIAN_POINT('Ctrl Pts',(-0.131283212176532,2.73512582675581,
8.78108014887987));
#380417=CARTESIAN_POINT('Ctrl Pts',(-0.128518497833744,2.74112095743854,
8.78639403366324));
#380418=CARTESIAN_POINT('Ctrl Pts',(-0.120426966568854,2.74089915230321,
8.78812224174741));
#380419=CARTESIAN_POINT('Ctrl Pts',(-0.135948499481602,2.72506801057236,
8.78944554828685));
#380420=CARTESIAN_POINT('Ctrl Pts',(-0.133623583979923,2.7301228286232,
8.79673892988686));
#380421=CARTESIAN_POINT('Ctrl Pts',(-0.12497490420386,2.72795398274399,
8.79894799272499));
#380422=CARTESIAN_POINT('Origin',(-0.117574427354269,2.73497394942481,8.75721825406948));
#380423=CARTESIAN_POINT('Origin',(-0.117574427354269,2.73497394942481,9.));
#380424=CARTESIAN_POINT('Origin',(-0.117574427354269,2.73497394942481,7.51860402984325));
#380425=CARTESIAN_POINT('Ctrl Pts',(-0.136909832561483,2.74292332597826,
7.50366195182966));
#380426=CARTESIAN_POINT('Ctrl Pts',(-0.137092387371678,2.74658072470567,
7.50000065167735));
#380427=CARTESIAN_POINT('Ctrl Pts',(-0.137092387371561,2.74658072470568,
7.49482233047108));
#380428=CARTESIAN_POINT('Ctrl Pts',(-0.129707514805723,2.74478891396913,
7.50215800491337));
#380429=CARTESIAN_POINT('Ctrl Pts',(-0.127570877920018,2.74705595609337,
7.49877273257264));
#380430=CARTESIAN_POINT('Ctrl Pts',(-0.124123047921427,2.74722807422352,
7.49481816995647));
#380431=CARTESIAN_POINT('Ctrl Pts',(-0.127728229063016,2.74279080378929,
7.51043025814042));
#380432=CARTESIAN_POINT('Ctrl Pts',(-0.123915371774049,2.74721289337236,
7.51006209594515));
#380433=CARTESIAN_POINT('Ctrl Pts',(-0.118108767356067,2.74746252368982,
7.50731281821699));
#380434=CARTESIAN_POINT('Ctrl Pts',(-0.128914573276736,2.74023237984244,
7.51860402984325));
#380435=CARTESIAN_POINT('Ctrl Pts',(-0.125713547171829,2.74713560005233,
7.51860402984325));
#380436=CARTESIAN_POINT('Ctrl Pts',(-0.118111296885561,2.7474624149473,
7.51860402984325));
#380437=CARTESIAN_POINT('Origin',(0.,0.,7.5));
#380438=CARTESIAN_POINT('Origin',(0.176949628854341,2.66188407944157,7.5));
#380439=CARTESIAN_POINT('',(0.176949628854341,2.66188407944157,7.59394543036555));
#380440=CARTESIAN_POINT('',(0.176949628854341,2.66188407944157,8.85049129520029));
#380441=CARTESIAN_POINT('',(0.176949628854341,2.66188407944157,7.5));
#380442=CARTESIAN_POINT('',(0.215079030421376,2.72235985585717,8.78727029226991));
#380443=CARTESIAN_POINT('Ctrl Pts',(0.176949628854341,2.66188407944157,
8.85049129520029));
#380444=CARTESIAN_POINT('Ctrl Pts',(0.189677904302623,2.68207197404603,
8.82945686509571));
#380445=CARTESIAN_POINT('Ctrl Pts',(0.202387257630373,2.70222985690408,
8.80838212259896));
#380446=CARTESIAN_POINT('Ctrl Pts',(0.215079030421377,2.72235985585717,
8.78727029226991));
#380447=CARTESIAN_POINT('',(0.222557758686683,2.73422161816809,8.75721825406948));
#380448=CARTESIAN_POINT('Origin',(0.200051500241714,2.6985255681284,8.75937679713107));
#380449=CARTESIAN_POINT('',(0.222557758686683,2.73422161816809,7.51860402984325));
#380450=CARTESIAN_POINT('',(0.222557758686684,2.73422161816809,7.5));
#380451=CARTESIAN_POINT('Ctrl Pts',(0.222557758686683,2.73422161816809,
7.51860402984325));
#380452=CARTESIAN_POINT('Ctrl Pts',(0.216684380796542,2.72490604872586,
7.52834476460825));
#380453=CARTESIAN_POINT('Ctrl Pts',(0.210807189994223,2.71558443175037,
7.53807742314407));
#380454=CARTESIAN_POINT('Ctrl Pts',(0.204926058256133,2.70625656418765,
7.54780169004674));
#380455=CARTESIAN_POINT('Ctrl Pts',(0.195610663431048,2.69148172609652,
7.5632044032688));
#380456=CARTESIAN_POINT('Ctrl Pts',(0.186285369461558,2.67669118730146,
7.57858609112103));
#380457=CARTESIAN_POINT('Ctrl Pts',(0.176949628854341,2.66188407944157,
7.59394543036555));
#380458=CARTESIAN_POINT('Origin',(0.0491816719600702,2.91212708488465,7.5));
#380459=CARTESIAN_POINT('',(0.128913937383338,2.74023375097047,8.75721825406948));
#380460=CARTESIAN_POINT('',(0.134814416896071,2.72751301502058,8.78727029226991));
#380461=CARTESIAN_POINT('Origin',(0.149792034669353,2.69522304258,8.75658640620967));
#380462=CARTESIAN_POINT('',(0.164897305964621,2.66265786424426,8.85049129520029));
#380463=CARTESIAN_POINT('Ctrl Pts',(0.134814416896071,2.72751301502058,
8.78727029226991));
#380464=CARTESIAN_POINT('Ctrl Pts',(0.144827823277063,2.70592529519939,
8.80838212259898));
#380465=CARTESIAN_POINT('Ctrl Pts',(0.154855100144228,2.68430767225054,
8.82945686509571));
#380466=CARTESIAN_POINT('Ctrl Pts',(0.164897305964621,2.66265786424426,
8.85049129520029));
#380467=CARTESIAN_POINT('',(0.164897305964621,2.66265786424426,7.59394543036555));
#380468=CARTESIAN_POINT('',(0.164897305964621,2.66265786424426,7.5));
#380469=CARTESIAN_POINT('',(0.128913937383338,2.74023375097047,7.51860402984325));
#380470=CARTESIAN_POINT('Ctrl Pts',(0.164897305964622,2.66265786424426,
7.59394543036555));
#380471=CARTESIAN_POINT('Ctrl Pts',(0.157531702584619,2.67853723396437,
7.57858609112103));
#380472=CARTESIAN_POINT('Ctrl Pts',(0.150174341270698,2.69439883476488,
7.56320440326857));
#380473=CARTESIAN_POINT('Ctrl Pts',(0.1428247900678,2.71024359788972,7.54780169004651));
#380474=CARTESIAN_POINT('Ctrl Pts',(0.138184763568473,2.72024694622285,
7.53807742314383));
#380475=CARTESIAN_POINT('Ctrl Pts',(0.133547846342444,2.73024359133049,
7.52834476460825));
#380476=CARTESIAN_POINT('Ctrl Pts',(0.128913937383338,2.74023375097047,
7.51860402984325));
#380477=CARTESIAN_POINT('',(0.128913937383338,2.74023375097047,7.5));
#380478=CARTESIAN_POINT('Origin',(0.171134036480631,2.66555075509437,7.5));
#380479=CARTESIAN_POINT('Ctrl Pts',(0.164897305964622,2.66265786424426,
8.85049129520029));
#380480=CARTESIAN_POINT('Ctrl Pts',(0.164978795651674,2.66248218211717,
8.85097269580138));
#380481=CARTESIAN_POINT('Ctrl Pts',(0.1650668876992,2.66231225593408,8.85143669361005));
#380482=CARTESIAN_POINT('Ctrl Pts',(0.165166414645531,2.66214066352794,
8.8519052845931));
#380483=CARTESIAN_POINT('Ctrl Pts',(0.165361083040785,2.66180503966352,
8.85282181883899));
#380484=CARTESIAN_POINT('Ctrl Pts',(0.165594660314783,2.66147177387202,
8.85372622499636));
#380485=CARTESIAN_POINT('Ctrl Pts',(0.165883438033025,2.66114448611063,
8.85462257735071));
#380486=CARTESIAN_POINT('Ctrl Pts',(0.166123171038294,2.66087278343529,
8.85536669723986));
#380487=CARTESIAN_POINT('Ctrl Pts',(0.166400977668207,2.66060511779347,
8.85610498449051));
#380488=CARTESIAN_POINT('Ctrl Pts',(0.16673175496809,2.66034930042851,8.85681338218371));
#380489=CARTESIAN_POINT('Ctrl Pts',(0.167031935887229,2.66011714576804,
8.85745625420285));
#380490=CARTESIAN_POINT('Ctrl Pts',(0.167379140604456,2.65989136329579,
8.85808743050666));
#380491=CARTESIAN_POINT('Ctrl Pts',(0.167797781718648,2.65968684835214,
8.85866804508411));
#380492=CARTESIAN_POINT('Ctrl Pts',(0.167990933653708,2.65959248959048,
8.85893592806396));
#380493=CARTESIAN_POINT('Ctrl Pts',(0.168199482605728,2.65950280806947,
8.85919241173848));
#380494=CARTESIAN_POINT('Ctrl Pts',(0.168426929570569,2.65942042008506,
8.85943017985534));
#380495=CARTESIAN_POINT('Ctrl Pts',(0.168734050304612,2.65930917191666,
8.8597512372));
#380496=CARTESIAN_POINT('Ctrl Pts',(0.169083662951928,2.65920899275127,
8.86004599534706));
#380497=CARTESIAN_POINT('Ctrl Pts',(0.169474435967161,2.65913109836974,
8.86026130871721));
#380498=CARTESIAN_POINT('Ctrl Pts',(0.169617508985096,2.65910257904058,
8.86034014101236));
#380499=CARTESIAN_POINT('Ctrl Pts',(0.169768246247698,2.65907660650484,
8.86040910639692));
#380500=CARTESIAN_POINT('Ctrl Pts',(0.169922598120376,2.6590542198636,8.86046313645507));
#380501=CARTESIAN_POINT('Ctrl Pts',(0.170163462925003,2.65901928569743,
8.8605474499083));
#380502=CARTESIAN_POINT('Ctrl Pts',(0.17041972577939,2.65899227558558,8.86059655985669));
#380503=CARTESIAN_POINT('Ctrl Pts',(0.170674921058896,2.65897463042516,
8.86059725258816));
#380504=CARTESIAN_POINT('Ctrl Pts',(0.170930705941449,2.65895694449737,
8.86059794692012));
#380505=CARTESIAN_POINT('Ctrl Pts',(0.171188438254314,2.65895112114787,
8.86056369958366));
#380506=CARTESIAN_POINT('Ctrl Pts',(0.171433976148159,2.65895371584656,
8.86048590497774));
#380507=CARTESIAN_POINT('Ctrl Pts',(0.171498054227909,2.65895439298566,
8.86046560290182));
#380508=CARTESIAN_POINT('Ctrl Pts',(0.171562134463288,2.65895574282288,
8.86044257503091));
#380509=CARTESIAN_POINT('Ctrl Pts',(0.171624237413298,2.65895769082822,
8.86041778462583));
#380510=CARTESIAN_POINT('Ctrl Pts',(0.172042113203527,2.65897079848689,
8.86025097596201));
#380511=CARTESIAN_POINT('Ctrl Pts',(0.17242652801394,2.65901307951986,8.8599848982295));
#380512=CARTESIAN_POINT('Ctrl Pts',(0.172767188072727,2.65907487815317,
8.85968173251462));
#380513=CARTESIAN_POINT('Ctrl Pts',(0.17294737772633,2.65910756608955,8.85952137522077));
#380514=CARTESIAN_POINT('Ctrl Pts',(0.173118833030298,2.65914615685814,
8.85934740853961));
#380515=CARTESIAN_POINT('Ctrl Pts',(0.173279477441213,2.65918858963265,
8.85916759001821));
#380516=CARTESIAN_POINT('Ctrl Pts',(0.173924548252338,2.65935897927845,
8.85844552518696));
#380517=CARTESIAN_POINT('Ctrl Pts',(0.174432530583691,2.65959802342683,
8.85759444184125));
#380518=CARTESIAN_POINT('Ctrl Pts',(0.174829205672066,2.65983012928581,
8.8568349891514));
#380519=CARTESIAN_POINT('Ctrl Pts',(0.174870716663634,2.6598544185458,8.85675551444999));
#380520=CARTESIAN_POINT('Ctrl Pts',(0.174910995458546,2.65987864675125,
8.85667699793651));
#380521=CARTESIAN_POINT('Ctrl Pts',(0.174950062383047,2.6599027366277,8.85659965593547));
#380522=CARTESIAN_POINT('Ctrl Pts',(0.17547738972341,2.66022790300923,8.85555568965886));
#380523=CARTESIAN_POINT('Ctrl Pts',(0.17593722350854,2.66061656454988,8.85434650606346));
#380524=CARTESIAN_POINT('Ctrl Pts',(0.176335848680025,2.66106589614674,
8.85297329937117));
#380525=CARTESIAN_POINT('Ctrl Pts',(0.176560051050397,2.6613186177918,8.85220095427747));
#380526=CARTESIAN_POINT('Ctrl Pts',(0.176764746713045,2.66159084402269,
8.85137579139183));
#380527=CARTESIAN_POINT('Ctrl Pts',(0.176949628854341,2.66188407944157,
8.85049129520029));
#380528=CARTESIAN_POINT('Origin',(0.171134036480631,2.66555075509437,7.59394543036555));
#380529=CARTESIAN_POINT('Ctrl Pts',(0.16513389801642,2.66214779976352,7.59443877723642));
#380530=CARTESIAN_POINT('Ctrl Pts',(0.167570568507185,2.65689462638278,
7.58783886950016));
#380531=CARTESIAN_POINT('Ctrl Pts',(0.175889913880979,2.65858804720708,
7.58559994247159));
#380532=CARTESIAN_POINT('Ctrl Pts',(0.151832185296215,2.69082471912743,
7.56670252222135));
#380533=CARTESIAN_POINT('Ctrl Pts',(0.154265334106333,2.68557913807364,
7.56004874999028));
#380534=CARTESIAN_POINT('Ctrl Pts',(0.162638236120083,2.68726165675841,
7.55786368756704));
#380535=CARTESIAN_POINT('Ctrl Pts',(0.138555312195495,2.71944808720963,
7.53888913333562));
#380536=CARTESIAN_POINT('Ctrl Pts',(0.141002921328123,2.71417133141078,
7.5322200213728));
#380537=CARTESIAN_POINT('Ctrl Pts',(0.149409776264335,2.7158822477739,7.53005029815327));
#380538=CARTESIAN_POINT('Ctrl Pts',(0.125303879501795,2.74801660878327,
7.51101258149734));
#380539=CARTESIAN_POINT('Ctrl Pts',(0.127781158104529,2.74267588911605,
7.5043616886572));
#380540=CARTESIAN_POINT('Ctrl Pts',(0.136205262916607,2.74444844085289,
7.50217374673251));
#380541=CARTESIAN_POINT('',(0.136909871778086,2.7429241116639,7.50366116523517));
#380542=CARTESIAN_POINT('Ctrl Pts',(0.128913937383338,2.74023375097047,
7.51860402984325));
#380543=CARTESIAN_POINT('Ctrl Pts',(0.128728114394968,2.74063436335517,
7.51734760759493));
#380544=CARTESIAN_POINT('Ctrl Pts',(0.128614169925088,2.74102140924103,
7.51608817408572));
#380545=CARTESIAN_POINT('Ctrl Pts',(0.128585176113098,2.74139776962912,
7.51481005913119));
#380546=CARTESIAN_POINT('Ctrl Pts',(0.128558912825369,2.74173868586207,
7.51365231206383));
#380547=CARTESIAN_POINT('Ctrl Pts',(0.128602066540858,2.74207129579757,
7.51247773061042));
#380548=CARTESIAN_POINT('Ctrl Pts',(0.128750508669634,2.74238509315603,
7.51129758471022));
#380549=CARTESIAN_POINT('Ctrl Pts',(0.128935005282971,2.74277510743559,
7.50983079813402));
#380550=CARTESIAN_POINT('Ctrl Pts',(0.129288033340368,2.74311804396216,
7.50839324291155));
#380551=CARTESIAN_POINT('Ctrl Pts',(0.129869611670354,2.74335727296713,
7.50715379678855));
#380552=CARTESIAN_POINT('Ctrl Pts',(0.13013828410103,2.74346778987421,7.50658120839351));
#380553=CARTESIAN_POINT('Ctrl Pts',(0.130497541971766,2.74356309743786,
7.50598221009429));
#380554=CARTESIAN_POINT('Ctrl Pts',(0.130944668113831,2.74361894150132,
7.50545747549611));
#380555=CARTESIAN_POINT('Ctrl Pts',(0.131183268463085,2.74364874162212,
7.50517746087247));
#380556=CARTESIAN_POINT('Ctrl Pts',(0.131449452540065,2.74366782811638,
7.50491486231392));
#380557=CARTESIAN_POINT('Ctrl Pts',(0.131736290639255,2.74367403179687,
7.50468370960992));
#380558=CARTESIAN_POINT('Ctrl Pts',(0.132165204075493,2.74368330825604,
7.50433806340447));
#380559=CARTESIAN_POINT('Ctrl Pts',(0.132653172773484,2.74366350077052,
7.50405484070984));
#380560=CARTESIAN_POINT('Ctrl Pts',(0.133167303892957,2.74361522753202,
7.50385766036131));
#380561=CARTESIAN_POINT('Ctrl Pts',(0.133222282224778,2.7436100654595,7.50383657498791));
#380562=CARTESIAN_POINT('Ctrl Pts',(0.133277536757632,2.74360459452477,
7.50381643264937));
#380563=CARTESIAN_POINT('Ctrl Pts',(0.13333301077446,2.74359882783486,7.50379723213559));
#380564=CARTESIAN_POINT('Ctrl Pts',(0.133703317983596,2.74356033329326,
7.50366906242519));
#380565=CARTESIAN_POINT('Ctrl Pts',(0.13409138609082,2.74350710736077,7.50358235568538));
#380566=CARTESIAN_POINT('Ctrl Pts',(0.134464202760926,2.74344681272314,
7.5035341175365));
#380567=CARTESIAN_POINT('Ctrl Pts',(0.13502319916305,2.74335640773805,7.50346178989176));
#380568=CARTESIAN_POINT('Ctrl Pts',(0.135620708171075,2.74323538466582,
7.50346967198527));
#380569=CARTESIAN_POINT('Ctrl Pts',(0.136203621195044,2.7430985287681,7.50354272648692));
#380570=CARTESIAN_POINT('Ctrl Pts',(0.136443385387387,2.74304223710461,
7.50357277531559));
#380571=CARTESIAN_POINT('Ctrl Pts',(0.136680394004036,2.74298347960564,
7.50361331098761));
#380572=CARTESIAN_POINT('Ctrl Pts',(0.136909871778157,2.74292411166531,
7.50366116523658));
#380573=CARTESIAN_POINT('',(0.171321629291362,2.66847266454066,7.57603338622103));
#380574=CARTESIAN_POINT('Origin',(0.17189066119661,2.67729126376579,7.58486873427626));
#380575=CARTESIAN_POINT('Ctrl Pts',(0.136909871749266,2.74292411171347,
7.50366116529968));
#380576=CARTESIAN_POINT('Ctrl Pts',(0.148362498674568,2.71814780982416,
7.52783573079709));
#380577=CARTESIAN_POINT('Ctrl Pts',(0.159832559194538,2.6933318400473,7.55196141284068));
#380578=CARTESIAN_POINT('Ctrl Pts',(0.171321628466439,2.66847266548254,
7.57603338728831));
#380579=CARTESIAN_POINT('Ctrl Pts',(0.164624061684221,2.6636647768937,7.5963967733137));
#380580=CARTESIAN_POINT('Ctrl Pts',(0.169597079718486,2.64607668412072,
7.59959882295472));
#380581=CARTESIAN_POINT('Ctrl Pts',(0.177275791240311,2.66268229166692,
7.59642833564546));
#380582=CARTESIAN_POINT('Ctrl Pts',(0.165068222839356,2.6597894930393,7.5870762605742));
#380583=CARTESIAN_POINT('Ctrl Pts',(0.170398543843799,2.65560619660867,
7.58809943920599));
#380584=CARTESIAN_POINT('Ctrl Pts',(0.176262094528132,2.65897267461483,
7.58710240504253));
#380585=CARTESIAN_POINT('Ctrl Pts',(0.168908645247665,2.66449871675321,
7.58015376756929));
#380586=CARTESIAN_POINT('Ctrl Pts',(0.170903573821348,2.66246167689546,
7.58205880659762));
#380587=CARTESIAN_POINT('Ctrl Pts',(0.173140492571299,2.66417143405488,
7.58020924244126));
#380588=CARTESIAN_POINT('Ctrl Pts',(0.171321629238138,2.6684726637148,7.57603338509286));
#380589=CARTESIAN_POINT('Ctrl Pts',(0.171321629238138,2.6684726637148,7.57603338509286));
#380590=CARTESIAN_POINT('Ctrl Pts',(0.171321629238137,2.6684726637148,7.57603338509286));
#380591=CARTESIAN_POINT('Origin',(0.171884966568783,2.6772916293728,7.58486873427623));
#380592=CARTESIAN_POINT('Ctrl Pts',(0.227147889551719,2.74150187215855,
7.51098857897448));
#380593=CARTESIAN_POINT('Ctrl Pts',(0.224007978980353,2.73652176437099,
7.50433767179956));
#380594=CARTESIAN_POINT('Ctrl Pts',(0.215879678833542,2.73935703998472,
7.50214974420965));
#380595=CARTESIAN_POINT('Ctrl Pts',(0.210347158552135,2.71485479117137,
7.53887321589173));
#380596=CARTESIAN_POINT('Ctrl Pts',(0.207244869681733,2.70993435391323,
7.53220407452068));
#380597=CARTESIAN_POINT('Ctrl Pts',(0.199125792371518,2.71270626725104,
7.53003438070911));
#380598=CARTESIAN_POINT('Ctrl Pts',(0.193514163951452,2.68815653795892,
7.56669465659233));
#380599=CARTESIAN_POINT('Ctrl Pts',(0.19043020903154,2.68326517957014,7.560040858333));
#380600=CARTESIAN_POINT('Ctrl Pts',(0.182341182153904,2.6860045762737,7.55785582193789));
#380601=CARTESIAN_POINT('Ctrl Pts',(0.176649667038706,2.66140831997643,
7.59443891967696));
#380602=CARTESIAN_POINT('Ctrl Pts',(0.173561240768107,2.656509869727,7.58783901202978));
#380603=CARTESIAN_POINT('Ctrl Pts',(0.165526747119516,2.65925324170307,
7.58560008491213));
#380604=CARTESIAN_POINT('',(0.21497150649217,2.73791238843283,7.50366116523517));
#380605=CARTESIAN_POINT('Ctrl Pts',(0.214971506492199,2.7379123884332,7.50366116523554));
#380606=CARTESIAN_POINT('Ctrl Pts',(0.21572334107391,2.73800663427399,7.50350835821027));
#380607=CARTESIAN_POINT('Ctrl Pts',(0.216417525721002,2.73806880892224,
7.50345484956));
#380608=CARTESIAN_POINT('Ctrl Pts',(0.217074645537771,2.73810135898814,
7.50349758195598));
#380609=CARTESIAN_POINT('Ctrl Pts',(0.21741179673705,2.73811805958593,7.50351950684424));
#380610=CARTESIAN_POINT('Ctrl Pts',(0.217772415375925,2.73812873702199,
7.50357029184312));
#380611=CARTESIAN_POINT('Ctrl Pts',(0.218120438804839,2.73812947445888,
7.50365515313923));
#380612=CARTESIAN_POINT('Ctrl Pts',(0.218655839767117,2.73813060893543,
7.50378570417639));
#380613=CARTESIAN_POINT('Ctrl Pts',(0.219177147199477,2.73810859894365,
7.50400001621911));
#380614=CARTESIAN_POINT('Ctrl Pts',(0.219644586262636,2.73806285136934,
7.50428903009635));
#380615=CARTESIAN_POINT('Ctrl Pts',(0.219696468402382,2.73805777374055,
7.50432110841318));
#380616=CARTESIAN_POINT('Ctrl Pts',(0.219747713437272,2.73805241837707,
7.50435406373354));
#380617=CARTESIAN_POINT('Ctrl Pts',(0.219798286699864,2.73804679504868,
7.50438785222351));
#380618=CARTESIAN_POINT('Ctrl Pts',(0.220107060776615,2.73801246192593,
7.50459414719561));
#380619=CARTESIAN_POINT('Ctrl Pts',(0.220395652270365,2.7379670806944,7.50483629897752));
#380620=CARTESIAN_POINT('Ctrl Pts',(0.220653209760764,2.73791368995158,
7.50509910455309));
#380621=CARTESIAN_POINT('Ctrl Pts',(0.221221407453785,2.73779590461034,
7.50567888004914));
#380622=CARTESIAN_POINT('Ctrl Pts',(0.221661062246274,2.73763500597979,
7.50637912803144));
#380623=CARTESIAN_POINT('Ctrl Pts',(0.221990006666829,2.73745624122374,
7.50710440483569));
#380624=CARTESIAN_POINT('Ctrl Pts',(0.22207067036921,2.73741240455658,7.50728225710685));
#380625=CARTESIAN_POINT('Ctrl Pts',(0.222146352208224,2.73736674913086,
7.50746498566954));
#380626=CARTESIAN_POINT('Ctrl Pts',(0.222215500713304,2.73732069740447,
7.50764697238949));
#380627=CARTESIAN_POINT('Ctrl Pts',(0.222587224046429,2.73707313599715,
7.50862528291181));
#380628=CARTESIAN_POINT('Ctrl Pts',(0.222806182813355,2.7367950940424,7.50965856837421));
#380629=CARTESIAN_POINT('Ctrl Pts',(0.222933569195844,2.7365120845317,7.51067959873201));
#380630=CARTESIAN_POINT('Ctrl Pts',(0.223003670082806,2.73635634404099,
7.51124147302577));
#380631=CARTESIAN_POINT('Ctrl Pts',(0.223045660948021,2.73619888290729,
7.51180065547252));
#380632=CARTESIAN_POINT('Ctrl Pts',(0.223067223661595,2.73604292919307,
7.512351757165));
#380633=CARTESIAN_POINT('Ctrl Pts',(0.223141731426557,2.73550404698585,
7.51425603304534));
#380634=CARTESIAN_POINT('Ctrl Pts',(0.222975207875285,2.73491808083108,
7.51626900505178));
#380635=CARTESIAN_POINT('Ctrl Pts',(0.222617535678944,2.73431900699274,
7.5182778896924));
#380636=CARTESIAN_POINT('Ctrl Pts',(0.222598177783769,2.73428658398451,
7.51838661432543));
#380637=CARTESIAN_POINT('Ctrl Pts',(0.222578250493315,2.73425411954144,
7.51849533314855));
#380638=CARTESIAN_POINT('Ctrl Pts',(0.222557758686687,2.73422161816809,
7.51860402984325));
#380639=CARTESIAN_POINT('Ctrl Pts',(0.171321630230276,2.66847266537049,
7.57603338728985));
#380640=CARTESIAN_POINT('Ctrl Pts',(0.18589529509066,2.69165855689206,7.55196141284922));
#380641=CARTESIAN_POINT('Ctrl Pts',(0.20044458236368,2.71480402913563,7.52783573083105));
#380642=CARTESIAN_POINT('Ctrl Pts',(0.214971506528135,2.73791238847983,
7.50366116530176));
#380643=CARTESIAN_POINT('Origin',(5.91995423665117E-17,9.2208065736915E-16,
7.49482233047033));
#380644=CARTESIAN_POINT('Origin',(0.136469240156451,2.7340962668661,7.49482233047033));
#380645=CARTESIAN_POINT('Origin',(0.,0.,7.50366116523517));
#380646=CARTESIAN_POINT('Origin',(0.214279640797748,2.72910067339767,7.49482233047033));
#380647=CARTESIAN_POINT('Ctrl Pts',(0.128914382414638,2.74023279142927,
7.51860402984325));
#380648=CARTESIAN_POINT('Ctrl Pts',(0.125713236557893,2.74713561340539,
7.51860402984325));
#380649=CARTESIAN_POINT('Ctrl Pts',(0.118111296885526,2.7474624149473,7.51860402984325));
#380650=CARTESIAN_POINT('Ctrl Pts',(0.127725773959473,2.7427958558017,7.51041458714366));
#380651=CARTESIAN_POINT('Ctrl Pts',(0.123912249553058,2.74721302654345,
7.51004642900442));
#380652=CARTESIAN_POINT('Ctrl Pts',(0.118109200360832,2.74746250507528,
7.5072913648301));
#380653=CARTESIAN_POINT('Ctrl Pts',(0.129714166000048,2.7447883502916,7.50215815450137));
#380654=CARTESIAN_POINT('Ctrl Pts',(0.127579244834765,2.7470555459381,7.49877163671529));
#380655=CARTESIAN_POINT('Ctrl Pts',(0.124133329223839,2.74722756104425,
7.4948158853317));
#380656=CARTESIAN_POINT('Ctrl Pts',(0.136909844334258,2.74292356183035,
7.50366171572174));
#380657=CARTESIAN_POINT('Ctrl Pts',(0.137092387372164,2.74658072470565,
7.50000045605858));
#380658=CARTESIAN_POINT('Ctrl Pts',(0.137092387372039,2.74658072470566,
7.49482233047317));
#380659=CARTESIAN_POINT('Origin',(0.117574427354229,2.73497394942481,7.51860402984325));
#380660=CARTESIAN_POINT('Origin',(0.117574427354229,2.73497394942481,9.));
#380661=CARTESIAN_POINT('Origin',(0.117574427354229,2.73497394942481,8.75721825406948));
#380662=CARTESIAN_POINT('Ctrl Pts',(0.135941072634455,2.72508400670848,
8.78942910404913));
#380663=CARTESIAN_POINT('Ctrl Pts',(0.13361461326795,2.73014760380123,8.79672699501692));
#380664=CARTESIAN_POINT('Ctrl Pts',(0.124957328323498,2.72797391951581,
8.79893251111267));
#380665=CARTESIAN_POINT('Ctrl Pts',(0.131314834806412,2.7350576390608,8.78111911759581));
#380666=CARTESIAN_POINT('Ctrl Pts',(0.128550026197774,2.74105748434908,
8.78644465894811));
#380667=CARTESIAN_POINT('Ctrl Pts',(0.120447127148838,2.74081553646592,
8.78817647674132));
#380668=CARTESIAN_POINT('Ctrl Pts',(0.128431653016943,2.74127344462292,
8.76780923932031));
#380669=CARTESIAN_POINT('Ctrl Pts',(0.125163285148986,2.74835387598335,
8.76988516158376));
#380670=CARTESIAN_POINT('Ctrl Pts',(0.117619591664174,2.74883248752051,
8.77093053738832));
#380671=CARTESIAN_POINT('Ctrl Pts',(0.128993834005189,2.74006144760687,
8.75371302330492));
#380672=CARTESIAN_POINT('Ctrl Pts',(0.125806374260045,2.74696842246863,
8.75300828287559));
#380673=CARTESIAN_POINT('Ctrl Pts',(0.118170644421235,2.74726870427462,
8.75267964240737));
#380674=CARTESIAN_POINT('Origin',(0.123474906866962,2.72225321347492,8.78727029226991));
#380675=CARTESIAN_POINT('Ctrl Pts',(0.164897305964621,2.66265786424426,
8.85049129520029));
#380676=CARTESIAN_POINT('Ctrl Pts',(0.162440088364629,2.66795533476229,
8.85711686593484));
#380677=CARTESIAN_POINT('Ctrl Pts',(0.15406769756606,2.66622217740361,8.85933012996512));
#380678=CARTESIAN_POINT('Ctrl Pts',(0.154855086667218,2.68430770130538,
8.82945683644722));
#380679=CARTESIAN_POINT('Ctrl Pts',(0.152377472675456,2.68964914403161,
8.83607469902389));
#380680=CARTESIAN_POINT('Ctrl Pts',(0.143988102906681,2.68787417434732,
8.8382956714852));
#380681=CARTESIAN_POINT('Ctrl Pts',(0.144827836107466,2.70592526753856,
8.80838214965004));
#380682=CARTESIAN_POINT('Ctrl Pts',(0.142340444294155,2.71128779009166,
8.8150136446199));
#380683=CARTESIAN_POINT('Ctrl Pts',(0.13392440455196,2.70949360848066,8.81722098428721));
#380684=CARTESIAN_POINT('Ctrl Pts',(0.134814416896071,2.72751301502058,
8.78727029226991));
#380685=CARTESIAN_POINT('Ctrl Pts',(0.132326611918797,2.7328764283063,8.79393457792714));
#380686=CARTESIAN_POINT('Ctrl Pts',(0.123875403548898,2.7310829701198,8.79610912703474));
#380687=CARTESIAN_POINT('Origin',(0.153557795935513,2.6573980626986,8.85049129520029));
#380688=CARTESIAN_POINT('Ctrl Pts',(0.176949628854341,2.66188407944157,
8.85049129520029));
#380689=CARTESIAN_POINT('Ctrl Pts',(0.180064098225757,2.66682383578755,
8.85711686593484));
#380690=CARTESIAN_POINT('Ctrl Pts',(0.188146120567823,2.66403427005499,
8.85933012996512));
#380691=CARTESIAN_POINT('Ctrl Pts',(0.174194302759283,2.65751394830841,
8.86332496987232));
#380692=CARTESIAN_POINT('Ctrl Pts',(0.178815093143597,2.65750014247301,
8.86648636486738));
#380693=CARTESIAN_POINT('Ctrl Pts',(0.180423490888535,2.65181778745183,
8.87206031107457));
#380694=CARTESIAN_POINT('Ctrl Pts',(0.167085943002636,2.65793942165148,
8.86341338519874));
#380695=CARTESIAN_POINT('Ctrl Pts',(0.162484685652754,2.6584888772316,8.86654584966055));
#380696=CARTESIAN_POINT('Ctrl Pts',(0.160209362634033,2.65301648671671,
8.87215952290714));
#380697=CARTESIAN_POINT('Ctrl Pts',(0.164897305964622,2.66265786424426,
8.85049129520029));
#380698=CARTESIAN_POINT('Ctrl Pts',(0.162440088364629,2.66795533476229,
8.85711686593484));
#380699=CARTESIAN_POINT('Ctrl Pts',(0.15406769756606,2.66622217740361,8.85933012996512));
#380700=CARTESIAN_POINT('Origin',(0.187523433170177,2.65521739643648,8.85049129520029));
#380701=CARTESIAN_POINT('Ctrl Pts',(0.215079030421377,2.72235985585717,
8.78727029226991));
#380702=CARTESIAN_POINT('Ctrl Pts',(0.218232268622096,2.72736110215464,
8.79393457792714));
#380703=CARTESIAN_POINT('Ctrl Pts',(0.226384750345611,2.72450165169591,
8.79610912703474));
#380704=CARTESIAN_POINT('Ctrl Pts',(0.202387241368117,2.70222983111106,
8.80838214965003));
#380705=CARTESIAN_POINT('Ctrl Pts',(0.205539955892618,2.70723024682311,
8.81501364461995));
#380706=CARTESIAN_POINT('Ctrl Pts',(0.213657465212887,2.70437457614343,
8.81722098428721));
#380707=CARTESIAN_POINT('Ctrl Pts',(0.189677921384441,2.68207200113894,
8.82945683644722));
#380708=CARTESIAN_POINT('Ctrl Pts',(0.192818242734668,2.68705276044921,
8.83607469902389));
#380709=CARTESIAN_POINT('Ctrl Pts',(0.200911757808326,2.68421955444713,
8.8382956714852));
#380710=CARTESIAN_POINT('Ctrl Pts',(0.176949628854341,2.66188407944157,
8.85049129520029));
#380711=CARTESIAN_POINT('Ctrl Pts',(0.180064098225757,2.66682383578755,
8.85711686593484));
#380712=CARTESIAN_POINT('Ctrl Pts',(0.188146120567823,2.66403427005499,
8.85933012996512));
#380713=CARTESIAN_POINT('Origin',(0.225652834737212,2.71569317285208,8.78727029226991));
#380714=CARTESIAN_POINT('Ctrl Pts',(0.222459021446504,2.73406497972526,
8.75374538247847));
#380715=CARTESIAN_POINT('Ctrl Pts',(0.226500710045474,2.74049997247247,
8.75304829418603));
#380716=CARTESIAN_POINT('Ctrl Pts',(0.234104570794356,2.73982770398394,
8.75272238421917));
#380717=CARTESIAN_POINT('Ctrl Pts',(0.2231630141067,2.73518155988291,8.76769408445022));
#380718=CARTESIAN_POINT('Ctrl Pts',(0.227306993923109,2.74177811855038,
8.76974318093965));
#380719=CARTESIAN_POINT('Ctrl Pts',(0.234842375123338,2.74129192162787,
8.77077869880429));
#380720=CARTESIAN_POINT('Ctrl Pts',(0.219554748756163,2.72945860607643,
8.78108014887987));
#380721=CARTESIAN_POINT('Ctrl Pts',(0.223063405128047,2.73505097299612,
8.78639403366329));
#380722=CARTESIAN_POINT('Ctrl Pts',(0.231060141221959,2.73379626682602,
8.78812224174742));
#380723=CARTESIAN_POINT('Ctrl Pts',(0.21364159840909,2.72007994812382,8.78944554828686));
#380724=CARTESIAN_POINT('Ctrl Pts',(0.216593822171808,2.72479596259282,
8.79673892988685));
#380725=CARTESIAN_POINT('Ctrl Pts',(0.2248941505513,2.72153895428624,8.79894799272499));
#380726=CARTESIAN_POINT('Origin',(0.233131563002519,2.727554935163,8.75721825406948));
#380727=CARTESIAN_POINT('Origin',(0.233131563002519,2.727554935163,9.));
#380728=CARTESIAN_POINT('Origin',(0.233131563002519,2.727554935163,7.51860402984325));
#380729=CARTESIAN_POINT('Ctrl Pts',(0.214971444915595,2.73791160418275,
7.50366195182965));
#380730=CARTESIAN_POINT('Ctrl Pts',(0.215258086646279,2.74156232030815,
7.50000065167735));
#380731=CARTESIAN_POINT('Ctrl Pts',(0.215258086646395,2.74156232030814,
7.49482233047108));
#380732=CARTESIAN_POINT('Ctrl Pts',(0.222353197839296,2.73884086376983,
7.50215800491338));
#380733=CARTESIAN_POINT('Ctrl Pts',(0.224762195877964,2.74081606644905,
7.49877273257268));
#380734=CARTESIAN_POINT('Ctrl Pts',(0.228203729217893,2.74054587277758,
7.49481816995649));
#380735=CARTESIAN_POINT('Ctrl Pts',(0.224060721014884,2.73660605260403,
7.51043025814041));
#380736=CARTESIAN_POINT('Ctrl Pts',(0.228407759062819,2.74050425952474,
7.51006209594512));
#380737=CARTESIAN_POINT('Ctrl Pts',(0.234198613355249,2.74000930828873,
7.50731281821699));
#380738=CARTESIAN_POINT('Ctrl Pts',(0.222556952678043,2.73422033961324,
7.51860402984326));
#380739=CARTESIAN_POINT('Ctrl Pts',(0.226614462609803,2.74065754634786,
7.51860402984326));
#380740=CARTESIAN_POINT('Ctrl Pts',(0.234196090687468,2.74000952390803,
7.51860402984327));
#380741=CARTESIAN_POINT('Origin',(0.,0.,7.5));
#380742=CARTESIAN_POINT('Origin',(0.34713356539705,2.64507775146798,7.5));
#380743=CARTESIAN_POINT('',(0.34713356539705,2.64507775146798,7.59394543036555));
#380744=CARTESIAN_POINT('',(0.34713356539705,2.64507775146798,8.85049129520029));
#380745=CARTESIAN_POINT('',(0.34713356539705,2.64507775146798,7.5));
#380746=CARTESIAN_POINT('',(0.389059322317652,2.7029863147688,8.78727029226991));
#380747=CARTESIAN_POINT('Ctrl Pts',(0.34713356539705,2.64507775146798,8.85049129520029));
#380748=CARTESIAN_POINT('Ctrl Pts',(0.361129132086575,2.66440866446989,
8.82945686509571));
#380749=CARTESIAN_POINT('Ctrl Pts',(0.375103892673901,2.68371083973216,
8.80838212259896));
#380750=CARTESIAN_POINT('Ctrl Pts',(0.389059322317652,2.7029863147688,8.78727029226991));
#380751=CARTESIAN_POINT('',(0.397282670454267,2.71434454205174,8.75721825406948));
#380752=CARTESIAN_POINT('Origin',(0.372535599753802,2.68016381430646,8.75937679713185));
#380753=CARTESIAN_POINT('',(0.397282670454267,2.71434454205174,7.51860402984325));
#380754=CARTESIAN_POINT('',(0.397282670454267,2.71434454205174,7.5));
#380755=CARTESIAN_POINT('Ctrl Pts',(0.397282670454266,2.71434454205174,
7.51860402984325));
#380756=CARTESIAN_POINT('Ctrl Pts',(0.390824509465509,2.70542442105947,
7.52834476460825));
#380757=CARTESIAN_POINT('Ctrl Pts',(0.384362155931824,2.69649850925338,
7.53807742314407));
#380758=CARTESIAN_POINT('Ctrl Pts',(0.377895469082945,2.68756661219917,
7.54780169004674));
#380759=CARTESIAN_POINT('Ctrl Pts',(0.367652586608923,2.67341896999315,
7.5632044032688));
#380760=CARTESIAN_POINT('Ctrl Pts',(0.357398819381796,2.65925629358233,
7.57858609112103));
#380761=CARTESIAN_POINT('Ctrl Pts',(0.34713356539705,2.64507775146798,7.59394543036555));
#380762=CARTESIAN_POINT('Origin',(0.235661245880662,2.9029927269226,7.5));
#380763=CARTESIAN_POINT('',(0.304216449096259,2.72634410251322,8.75721825406948));
#380764=CARTESIAN_POINT('',(0.309289785090383,2.71327145765926,8.78727029226991));
#380765=CARTESIAN_POINT('Origin',(0.322167804103539,2.68008820916626,8.75658640621033));
#380766=CARTESIAN_POINT('',(0.335155581859841,2.64662214142563,8.85049129520029));
#380767=CARTESIAN_POINT('Ctrl Pts',(0.309289785090383,2.71327145765926,
8.78727029226991));
#380768=CARTESIAN_POINT('Ctrl Pts',(0.317899487896211,2.69108653097412,
8.80838212259896));
#380769=CARTESIAN_POINT('Ctrl Pts',(0.326521116789831,2.66887087391543,
8.82945686509571));
#380770=CARTESIAN_POINT('Ctrl Pts',(0.335155581859841,2.64662214142563,
8.85049129520029));
#380771=CARTESIAN_POINT('',(0.335155581859841,2.64662214142563,7.59394543036555));
#380772=CARTESIAN_POINT('',(0.335155581859841,2.64662214142563,7.5));
#380773=CARTESIAN_POINT('',(0.304216449096259,2.72634410251322,7.51860402984325));
#380774=CARTESIAN_POINT('Ctrl Pts',(0.335155581859841,2.64662214142563,
7.59394543036555));
#380775=CARTESIAN_POINT('Ctrl Pts',(0.328822506613063,2.66294080110644,
7.57858609112103));
#380776=CARTESIAN_POINT('Ctrl Pts',(0.322496518039572,2.67924120030481,
7.56320440326857));
#380777=CARTESIAN_POINT('Ctrl Pts',(0.316177244736808,2.69552429602679,
7.54780169004651));
#380778=CARTESIAN_POINT('Ctrl Pts',(0.312187668397812,2.70580437892645,
7.53807742314383));
#380779=CARTESIAN_POINT('Ctrl Pts',(0.308200765466647,2.71607757316129,
7.52834476460825));
#380780=CARTESIAN_POINT('Ctrl Pts',(0.304216449096259,2.72634410251322,
7.51860402984325));
#380781=CARTESIAN_POINT('',(0.304216449096259,2.72634410251322,7.5));
#380782=CARTESIAN_POINT('Origin',(0.341564846497265,2.64910949982511,7.5));
#380783=CARTESIAN_POINT('Ctrl Pts',(0.335155581859841,2.64662214142563,
8.85049129520029));
#380784=CARTESIAN_POINT('Ctrl Pts',(0.335225648125062,2.64644159919414,
8.85097269580138));
#380785=CARTESIAN_POINT('Ctrl Pts',(0.335302671970097,2.64626637806575,
8.85143669361005));
#380786=CARTESIAN_POINT('Ctrl Pts',(0.335391000464435,2.64608876150127,
8.8519052845931));
#380787=CARTESIAN_POINT('Ctrl Pts',(0.335563765397768,2.64574135476517,
8.85282181883899));
#380788=CARTESIAN_POINT('Ctrl Pts',(0.335775510349633,2.64539380835665,
8.85372622499636));
#380789=CARTESIAN_POINT('Ctrl Pts',(0.336042725344213,2.64504869099114,
8.85462257735071));
#380790=CARTESIAN_POINT('Ctrl Pts',(0.336264557742135,2.6447621868117,8.85536669723986));
#380791=CARTESIAN_POINT('Ctrl Pts',(0.33652464419198,2.64447727198576,8.85610498449051));
#380792=CARTESIAN_POINT('Ctrl Pts',(0.336838351599578,2.64420078725064,
8.85681338218371));
#380793=CARTESIAN_POINT('Ctrl Pts',(0.337123041564658,2.64394987691929,
8.85745625420284));
#380794=CARTESIAN_POINT('Ctrl Pts',(0.337455066979889,2.64370231285874,
8.85808743050665));
#380795=CARTESIAN_POINT('Ctrl Pts',(0.33785974463358,2.6434713956847,8.85866804508409));
#380796=CARTESIAN_POINT('Ctrl Pts',(0.338046454130659,2.64336485550627,
8.85893592806395));
#380797=CARTESIAN_POINT('Ctrl Pts',(0.338248828681714,2.64326199646833,
8.85919241173848));
#380798=CARTESIAN_POINT('Ctrl Pts',(0.33847052971609,2.6431652051818,8.85943017985534));
#380799=CARTESIAN_POINT('Ctrl Pts',(0.338769891743025,2.6430345082917,8.8597512372));
#380800=CARTESIAN_POINT('Ctrl Pts',(0.339112367572496,2.64291213519593,
8.86004599534705));
#380801=CARTESIAN_POINT('Ctrl Pts',(0.339497346992498,2.64280936394371,
8.86026130871721));
#380802=CARTESIAN_POINT('Ctrl Pts',(0.339638298811881,2.64277173649084,
8.86034014101235));
#380803=CARTESIAN_POINT('Ctrl Pts',(0.339787062302531,2.64273615954889,
8.86040910639692));
#380804=CARTESIAN_POINT('Ctrl Pts',(0.339939662725702,2.64270392954497,
8.86046313645506));
#380805=CARTESIAN_POINT('Ctrl Pts',(0.340177794408044,2.64265363489377,
8.86054744990829));
#380806=CARTESIAN_POINT('Ctrl Pts',(0.340431800199104,2.64261026145964,
8.86059655985669));
#380807=CARTESIAN_POINT('Ctrl Pts',(0.340685340623228,2.6425763021354,8.86059725258816));
#380808=CARTESIAN_POINT('Ctrl Pts',(0.340939466827023,2.64254226435155,
8.86059794692011));
#380809=CARTESIAN_POINT('Ctrl Pts',(0.341196296497925,2.64251994000076,
8.86056369958366));
#380810=CARTESIAN_POINT('Ctrl Pts',(0.341441496150749,2.64250679770149,
8.86048590497774));
#380811=CARTESIAN_POINT('Ctrl Pts',(0.341505485959662,2.64250336795268,
8.86046560290182));
#380812=CARTESIAN_POINT('Ctrl Pts',(0.341569521019693,2.64250060938173,
8.86044257503091));
#380813=CARTESIAN_POINT('Ctrl Pts',(0.341631621181662,2.64249857443501,
8.86041778462583));
#380814=CARTESIAN_POINT('Ctrl Pts',(0.342049478211836,2.64248488176879,
8.86025097596201));
#380815=CARTESIAN_POINT('Ctrl Pts',(0.342435812155876,2.64250244638938,
8.8599848982295));
#380816=CARTESIAN_POINT('Ctrl Pts',(0.342779731744066,2.64254229188586,
8.85968173251461));
#380817=CARTESIAN_POINT('Ctrl Pts',(0.342961645501975,2.64256336787063,
8.85952137522076));
#380818=CARTESIAN_POINT('Ctrl Pts',(0.343135221051665,2.6425908941713,8.85934740853961));
#380819=CARTESIAN_POINT('Ctrl Pts',(0.343298254078606,2.64262294724038,
8.8591675900182));
#380820=CARTESIAN_POINT('Ctrl Pts',(0.343952916424662,2.64275165697361,
8.85844552518695));
#380821=CARTESIAN_POINT('Ctrl Pts',(0.344475170663011,2.64295766344042,
8.85759444184123));
#380822=CARTESIAN_POINT('Ctrl Pts',(0.34488590181332,2.64316387735285,8.85683498915137));
#380823=CARTESIAN_POINT('Ctrl Pts',(0.34492888373433,2.6431854570896,8.85675551444997));
#380824=CARTESIAN_POINT('Ctrl Pts',(0.344970632078586,2.64320705484434,
8.85667699793651));
#380825=CARTESIAN_POINT('Ctrl Pts',(0.345011162179579,2.64322859219911,
8.85659965593547));
#380826=CARTESIAN_POINT('Ctrl Pts',(0.345558239550962,2.64351930451273,
8.85555568965886));
#380827=CARTESIAN_POINT('Ctrl Pts',(0.346042030188672,2.64387770585479,
8.85434650606346));
#380828=CARTESIAN_POINT('Ctrl Pts',(0.346468625116245,2.64430057424927,
8.85297329937117));
#380829=CARTESIAN_POINT('Ctrl Pts',(0.346708558770194,2.64453841195541,
8.85220095427747));
#380830=CARTESIAN_POINT('Ctrl Pts',(0.346930275458148,2.64479696397218,
8.85137579139184));
#380831=CARTESIAN_POINT('Ctrl Pts',(0.34713356539705,2.64507775146798,8.85049129520029));
#380832=CARTESIAN_POINT('Origin',(0.341564846497265,2.64910949982511,7.59394543036555));
#380833=CARTESIAN_POINT('Ctrl Pts',(0.335359007864409,2.64609796642226,
7.59443877723642));
#380834=CARTESIAN_POINT('Ctrl Pts',(0.337454099980217,2.64069946823527,
7.58783886950016));
#380835=CARTESIAN_POINT('Ctrl Pts',(0.345864850211427,2.64185638745667,
7.58559994247159));
#380836=CARTESIAN_POINT('Ctrl Pts',(0.323921961471611,2.67556820963984,
7.56670252222135));
#380837=CARTESIAN_POINT('Ctrl Pts',(0.326014025584496,2.67017751381545,
7.56004874999031));
#380838=CARTESIAN_POINT('Ctrl Pts',(0.334477523915324,2.67132012191119,
7.55786368756705));
#380839=CARTESIAN_POINT('Ctrl Pts',(0.312506272620235,2.70498342012269,
7.53888913333558));
#380840=CARTESIAN_POINT('Ctrl Pts',(0.314610769972604,2.69956068712902,
7.53222002137279));
#380841=CARTESIAN_POINT('Ctrl Pts',(0.323109970911448,2.70072945918588,
7.53005029815326));
#380842=CARTESIAN_POINT('Ctrl Pts',(0.301112457877955,2.73434226681255,
7.51101258149734));
#380843=CARTESIAN_POINT('Ctrl Pts',(0.303242465562179,2.72885380044164,
7.5043616886572));
#380844=CARTESIAN_POINT('Ctrl Pts',(0.311762829927145,2.73008297603239,
7.50217374673251));
#380845=CARTESIAN_POINT('',(0.312368326987687,2.72851663429644,7.50366116523517));
#380846=CARTESIAN_POINT('Ctrl Pts',(0.304216449096259,2.72634410251322,
7.51860402984325));
#380847=CARTESIAN_POINT('Ctrl Pts',(0.304056675224763,2.72675579751655,
7.51734760759493));
#380848=CARTESIAN_POINT('Ctrl Pts',(0.303967762981066,2.72714934862238,
7.51608817408573));
#380849=CARTESIAN_POINT('Ctrl Pts',(0.30396294223283,2.7275267933776,7.5148100591312));
#380850=CARTESIAN_POINT('Ctrl Pts',(0.303958575483881,2.72786869185621,
7.51365231206384));
#380851=CARTESIAN_POINT('Ctrl Pts',(0.30402295092717,2.72819785354088,7.51247773061043));
#380852=CARTESIAN_POINT('Ctrl Pts',(0.304191193131457,2.72850149544917,
7.51129758471022));
#380853=CARTESIAN_POINT('Ctrl Pts',(0.304400298977402,2.72887888766396,
7.50983079813402));
#380854=CARTESIAN_POINT('Ctrl Pts',(0.30477457371949,2.72919850100536,7.50839324291155));
#380855=CARTESIAN_POINT('Ctrl Pts',(0.305370284589398,2.72939997663714,
7.50715379678855));
#380856=CARTESIAN_POINT('Ctrl Pts',(0.305645485846298,2.72949305257365,
7.50658120839351));
#380857=CARTESIAN_POINT('Ctrl Pts',(0.306010111959777,2.72956514658689,
7.50598221009429));
#380858=CARTESIAN_POINT('Ctrl Pts',(0.306459897374659,2.72959222844244,
7.50545747549611));
#380859=CARTESIAN_POINT('Ctrl Pts',(0.306699916794201,2.72960668015883,
7.50517746087247));
#380860=CARTESIAN_POINT('Ctrl Pts',(0.306966776843333,2.72960867296547,
7.50491486231392));
#380861=CARTESIAN_POINT('Ctrl Pts',(0.307253423074059,2.72959648611972,
7.50468370960993));
#380862=CARTESIAN_POINT('Ctrl Pts',(0.307682049606423,2.72957826294121,
7.50433806340447));
#380863=CARTESIAN_POINT('Ctrl Pts',(0.308167746650436,2.72952723189046,
7.50405484070984));
#380864=CARTESIAN_POINT('Ctrl Pts',(0.308677728555375,2.72944611734059,
7.50385766036131));
#380865=CARTESIAN_POINT('Ctrl Pts',(0.308732263193193,2.72943744340029,
7.50383657498791));
#380866=CARTESIAN_POINT('Ctrl Pts',(0.308787053675691,2.7294284435361,7.50381643264937));
#380867=CARTESIAN_POINT('Ctrl Pts',(0.308842044242109,2.72941913446201,
7.50379723213559));
#380868=CARTESIAN_POINT('Ctrl Pts',(0.30920912426162,2.72935699334723,7.50366906242519));
#380869=CARTESIAN_POINT('Ctrl Pts',(0.309592984844094,2.72927901316413,
7.50358235568538));
#380870=CARTESIAN_POINT('Ctrl Pts',(0.30996117243167,2.72919495596223,7.5035341175365));
#380871=CARTESIAN_POINT('Ctrl Pts',(0.310513228048452,2.72906892170143,
7.50346178989176));
#380872=CARTESIAN_POINT('Ctrl Pts',(0.311101755435278,2.72890986475049,
7.50346967198527));
#380873=CARTESIAN_POINT('Ctrl Pts',(0.311674702414449,2.72873594267221,
7.50354272648692));
#380874=CARTESIAN_POINT('Ctrl Pts',(0.311910367366282,2.72866440492144,
7.50357277531559));
#380875=CARTESIAN_POINT('Ctrl Pts',(0.312143124417423,2.72859058295185,
7.50361331098761));
#380876=CARTESIAN_POINT('Ctrl Pts',(0.312368326987848,2.72851663429785,
7.50366116523659));
#380877=CARTESIAN_POINT('',(0.341939261259435,2.65201338678241,7.57603338622103));
#380878=CARTESIAN_POINT('Origin',(0.343072133619939,2.66077740925045,7.58486873427624));
#380879=CARTESIAN_POINT('Ctrl Pts',(0.312368326962103,2.72851663434776,
7.50366116529969));
#380880=CARTESIAN_POINT('Ctrl Pts',(0.32221000012475,2.70305746570147,7.52783573079709));
#380881=CARTESIAN_POINT('Ctrl Pts',(0.332066529532574,2.67755759369531,
7.55196141284068));
#380882=CARTESIAN_POINT('Ctrl Pts',(0.341939260496553,2.65201338777521,
7.57603338728831));
#380883=CARTESIAN_POINT('Ctrl Pts',(0.334947412104083,2.64764449208613,
7.59639677331371));
#380884=CARTESIAN_POINT('Ctrl Pts',(0.338963550211397,2.62893435951653,
7.59974925422225));
#380885=CARTESIAN_POINT('Ctrl Pts',(0.347594250863814,2.64601386279729,
7.59639677331372));
#380886=CARTESIAN_POINT('Ctrl Pts',(0.3351423703935,2.64374871291513,7.58707626057423));
#380887=CARTESIAN_POINT('Ctrl Pts',(0.340281256478474,2.63915422911306,
7.58811717123965));
#380888=CARTESIAN_POINT('Ctrl Pts',(0.346417486467306,2.64229494768145,
7.58707626057423));
#380889=CARTESIAN_POINT('Ctrl Pts',(0.339276623241288,2.64820220431539,
7.58015376756929));
#380890=CARTESIAN_POINT('Ctrl Pts',(0.341165064355264,2.6460088684777,7.58208760766041));
#380891=CARTESIAN_POINT('Ctrl Pts',(0.343548093433272,2.64765145922139,
7.5801537675693));
#380892=CARTESIAN_POINT('Ctrl Pts',(0.341939261153406,2.65201338596166,
7.57603338509286));
#380893=CARTESIAN_POINT('Ctrl Pts',(0.341939261153406,2.65201338596166,
7.57603338509286));
#380894=CARTESIAN_POINT('Ctrl Pts',(0.341939261153406,2.65201338596166,
7.57603338509286));
#380895=CARTESIAN_POINT('Origin',(0.343066474116786,2.6607781389623,7.58486873427623));
#380896=CARTESIAN_POINT('Ctrl Pts',(0.402329817877834,2.72131574728531,
7.51098857897448));
#380897=CARTESIAN_POINT('Ctrl Pts',(0.398877281988015,2.71654704642435,
7.50433767179956));
#380898=CARTESIAN_POINT('Ctrl Pts',(0.390947339037891,2.71989727863872,
7.50214974420965));
#380899=CARTESIAN_POINT('Ctrl Pts',(0.383856321441241,2.69579984211485,
7.53887321589168));
#380900=CARTESIAN_POINT('Ctrl Pts',(0.380445153058535,2.69108827875312,
7.53220407452063));
#380901=CARTESIAN_POINT('Ctrl Pts',(0.372520354360726,2.69437468796706,
7.53003438070911));
#380902=CARTESIAN_POINT('Ctrl Pts',(0.365347349076903,2.67023493699404,
7.56669465659233));
#380903=CARTESIAN_POINT('Ctrl Pts',(0.361956340065153,2.6655512180958,7.560040858333));
#380904=CARTESIAN_POINT('Ctrl Pts',(0.354059446710206,2.66880325214652,
7.55785582193789));
#380905=CARTESIAN_POINT('Ctrl Pts',(0.346803737871547,2.6446221881212,7.59443891967696));
#380906=CARTESIAN_POINT('Ctrl Pts',(0.343407812318908,2.63993167841372,
7.58783901202978));
#380907=CARTESIAN_POINT('Ctrl Pts',(0.33556559484521,2.64318418561333,7.58560008491213));
#380908=CARTESIAN_POINT('',(0.389948473491269,2.71851378208007,7.50366116523517));
#380909=CARTESIAN_POINT('Ctrl Pts',(0.389948473491322,2.71851378208044,
7.50366116523554));
#380910=CARTESIAN_POINT('Ctrl Pts',(0.390704801700004,2.71855966407601,
7.50350835821027));
#380911=CARTESIAN_POINT('Ctrl Pts',(0.391401543613678,2.71857723441672,
7.50345484956));
#380912=CARTESIAN_POINT('Ctrl Pts',(0.39205939879719,2.71856761579381,7.50349758195599));
#380913=CARTESIAN_POINT('Ctrl Pts',(0.392396927294144,2.71856268072692,
7.50351950684424));
#380914=CARTESIAN_POINT('Ctrl Pts',(0.392757489109026,2.71855023130953,
7.50357029184312));
#380915=CARTESIAN_POINT('Ctrl Pts',(0.393104844734224,2.71852866929362,
7.50365515313924));
#380916=CARTESIAN_POINT('Ctrl Pts',(0.393639218343962,2.71849549818184,
7.50378570417639));
#380917=CARTESIAN_POINT('Ctrl Pts',(0.394158044509274,2.71844013313008,
7.50400001621911));
#380918=CARTESIAN_POINT('Ctrl Pts',(0.394621592111593,2.71836453062546,
7.50428903009635));
#380919=CARTESIAN_POINT('Ctrl Pts',(0.394673042329127,2.7183561393291,7.50432110841318));
#380920=CARTESIAN_POINT('Ctrl Pts',(0.394723838956284,2.71834751168814,
7.50435406373355));
#380921=CARTESIAN_POINT('Ctrl Pts',(0.3947739480228,2.71833865967342,7.50438785222352));
#380922=CARTESIAN_POINT('Ctrl Pts',(0.395079887959366,2.71828461386873,
7.50459414719562));
#380923=CARTESIAN_POINT('Ctrl Pts',(0.395364978925454,2.71822083575731,
7.50483629897752));
#380924=CARTESIAN_POINT('Ctrl Pts',(0.395618586479729,2.71815105294644,
7.5050991045531));
#380925=CARTESIAN_POINT('Ctrl Pts',(0.396178070216927,2.71799710505663,
7.50567888004914));
#380926=CARTESIAN_POINT('Ctrl Pts',(0.396606512880836,2.7178083682303,7.50637912803145));
#380927=CARTESIAN_POINT('Ctrl Pts',(0.396923327952554,2.71760889522423,
7.50710440483569));
#380928=CARTESIAN_POINT('Ctrl Pts',(0.3970010172978,2.71755998048305,7.50728225710686));
#380929=CARTESIAN_POINT('Ctrl Pts',(0.39707361848719,2.71750956990922,7.50746498566955));
#380930=CARTESIAN_POINT('Ctrl Pts',(0.397139674375009,2.71745918244111,
7.50764697238949));
#380931=CARTESIAN_POINT('Ctrl Pts',(0.397494772648854,2.71718831327952,
7.50862528291182));
#380932=CARTESIAN_POINT('Ctrl Pts',(0.397695467332306,2.71689681385543,
7.50965856837422));
#380933=CARTESIAN_POINT('Ctrl Pts',(0.397804459504203,2.71660622414456,
7.51067959873202));
#380934=CARTESIAN_POINT('Ctrl Pts',(0.397864438033874,2.71644631226014,
7.51124147302578));
#380935=CARTESIAN_POINT('Ctrl Pts',(0.397896254054879,2.71628648428327,
7.51180065547253));
#380936=CARTESIAN_POINT('Ctrl Pts',(0.397907780476768,2.71612946946488,
7.51235175716501));
#380937=CARTESIAN_POINT('Ctrl Pts',(0.397947608855977,2.71558692072005,
7.51425603304536));
#380938=CARTESIAN_POINT('Ctrl Pts',(0.397743884464762,2.71501282769615,
7.51626900505181));
#380939=CARTESIAN_POINT('Ctrl Pts',(0.397348564351696,2.71443790085555,
7.51827788969244));
#380940=CARTESIAN_POINT('Ctrl Pts',(0.397327168880126,2.71440678472847,
7.51838661432546));
#380941=CARTESIAN_POINT('Ctrl Pts',(0.397305202528421,2.71437566373297,
7.51849533314857));
#380942=CARTESIAN_POINT('Ctrl Pts',(0.39728267045427,2.71434454205174,7.51860402984325));
#380943=CARTESIAN_POINT('Ctrl Pts',(0.341939262249588,2.65201338755038,
7.57603338728985));
#380944=CARTESIAN_POINT('Ctrl Pts',(0.357968509122732,2.67421790325761,
7.55196141284922));
#380945=CARTESIAN_POINT('Ctrl Pts',(0.373970838822828,2.69638364460998,
7.52783573083104));
#380946=CARTESIAN_POINT('Ctrl Pts',(0.389948473530171,2.71851378212467,
7.50366116530176));
#380947=CARTESIAN_POINT('Origin',(1.1815582111519E-16,9.16393216063564E-16,
7.49482233047033));
#380948=CARTESIAN_POINT('Origin',(0.311362998732826,2.71973515861749,7.49482233047033));
#380949=CARTESIAN_POINT('Origin',(0.,0.,7.50366116523517));
#380950=CARTESIAN_POINT('Origin',(0.388693460788409,2.70976449964574,7.49482233047033));
#380951=CARTESIAN_POINT('Ctrl Pts',(0.304216831735178,2.72634311643025,
7.51860402984325));
#380952=CARTESIAN_POINT('Ctrl Pts',(0.301464528298415,2.73343685393752,
7.51860402984325));
#380953=CARTESIAN_POINT('Ctrl Pts',(0.293899145873092,2.73425004197771,
7.51860402984325));
#380954=CARTESIAN_POINT('Ctrl Pts',(0.303194881501727,2.72897706911724,
7.51041458714366));
#380955=CARTESIAN_POINT('Ctrl Pts',(0.299672201491318,2.73362949765557,
7.51004642900443));
#380956=CARTESIAN_POINT('Ctrl Pts',(0.29389705943045,2.73425026624531,7.5072913648301));
#380957=CARTESIAN_POINT('Ctrl Pts',(0.305306847737879,2.73083807309806,
7.50215815450138));
#380958=CARTESIAN_POINT('Ctrl Pts',(0.303321572720914,2.73323739541665,
7.49877163671529));
#380959=CARTESIAN_POINT('Ctrl Pts',(0.299893758158875,2.73362983767055,
7.4948158853317));
#380960=CARTESIAN_POINT('Ctrl Pts',(0.312368264372289,2.72851608735092,
7.50366171572174));
#380961=CARTESIAN_POINT('Ctrl Pts',(0.312784747585871,2.73215404062027,
7.50000045605858));
#380962=CARTESIAN_POINT('Ctrl Pts',(0.312784747585747,2.73215404062028,
7.49482233047317));
#380963=CARTESIAN_POINT('Origin',(0.292563240664578,2.72182163269599,7.51860402984325));
#380964=CARTESIAN_POINT('Origin',(0.292563240664578,2.72182163269599,9.));
#380965=CARTESIAN_POINT('Origin',(0.292563240664578,2.72182163269599,8.75721825406948));
#380966=CARTESIAN_POINT('Ctrl Pts',(0.310258498896826,2.71077525492426,
8.78942910404912));
#380967=CARTESIAN_POINT('Ctrl Pts',(0.308261245270224,2.71597750507709,
8.79672699501689));
#380968=CARTESIAN_POINT('Ctrl Pts',(0.299482479215855,2.71436296100999,
8.79893251111267));
#380969=CARTESIAN_POINT('Ctrl Pts',(0.306280778989386,2.72102479945456,
8.78111911759584));
#380970=CARTESIAN_POINT('Ctrl Pts',(0.303906062384031,2.72718945931294,
8.78644465894816));
#380971=CARTESIAN_POINT('Ctrl Pts',(0.295804309956124,2.72746716306224,
8.78817647674132));
#380972=CARTESIAN_POINT('Ctrl Pts',(0.303801769035835,2.72741256006903,
8.76780923932029));
#380973=CARTESIAN_POINT('Ctrl Pts',(0.300993761175014,2.73468784897217,
8.76988516158371));
#380974=CARTESIAN_POINT('Ctrl Pts',(0.293496231764001,2.73564880325158,
8.77093053738832));
#380975=CARTESIAN_POINT('Ctrl Pts',(0.304285142047523,2.72616703417123,
8.75371302330492));
#380976=CARTESIAN_POINT('Ctrl Pts',(0.301546762679073,2.7332640391594,8.7530082828756));
#380977=CARTESIAN_POINT('Ctrl Pts',(0.293945960387518,2.73405292689471,
8.75267964240738));
#380978=CARTESIAN_POINT('Origin',(0.297636576658702,2.70874898784203,8.78727029226991));
#380979=CARTESIAN_POINT('Ctrl Pts',(0.335155581859841,2.64662214142563,
8.85049129520029));
#380980=CARTESIAN_POINT('Ctrl Pts',(0.333042822978375,2.6520661621945,8.85711686593484));
#380981=CARTESIAN_POINT('Ctrl Pts',(0.324576590381406,2.65087298671372,
8.85933012996512));
#380982=CARTESIAN_POINT('Ctrl Pts',(0.326521105202062,2.66887090377405,
8.82945683644721));
#380983=CARTESIAN_POINT('Ctrl Pts',(0.324390809144477,2.67436011320681,
8.83607469902387));
#380984=CARTESIAN_POINT('Ctrl Pts',(0.315904953537504,2.67312629915468,
8.8382956714852));
#380985=CARTESIAN_POINT('Ctrl Pts',(0.317899498928018,2.69108650254807,
8.80838214965002));
#380986=CARTESIAN_POINT('Ctrl Pts',(0.31576079572757,2.69659737496415,8.81501364461992));
#380987=CARTESIAN_POINT('Ctrl Pts',(0.307247094031156,2.69534609720933,
8.81722098428721));
#380988=CARTESIAN_POINT('Ctrl Pts',(0.309289785090383,2.71327145765926,
8.78727029226991));
#380989=CARTESIAN_POINT('Ctrl Pts',(0.307150726644314,2.71878324544933,
8.79393457792714));
#380990=CARTESIAN_POINT('Ctrl Pts',(0.298601974927864,2.71753494289438,
8.79610912703474));
#380991=CARTESIAN_POINT('Origin',(0.32350237342816,2.64209967160839,8.85049129520029));
#380992=CARTESIAN_POINT('Ctrl Pts',(0.34713356539705,2.64507775146798,8.85049129520029));
#380993=CARTESIAN_POINT('Ctrl Pts',(0.350558127032854,2.64980781381701,
8.85711686593484));
#380994=CARTESIAN_POINT('Ctrl Pts',(0.358444815903088,2.64650616259708,
8.85933012996512));
#380995=CARTESIAN_POINT('Ctrl Pts',(0.344103905151925,2.64089313358697,
8.86332496987232));
#380996=CARTESIAN_POINT('Ctrl Pts',(0.34871431708389,2.64058330106072,8.86648636486737));
#380997=CARTESIAN_POINT('Ctrl Pts',(0.349955340466956,2.63480957065002,
8.87206031107457));
#380998=CARTESIAN_POINT('Ctrl Pts',(0.33703741045343,2.64177316692275,8.86341338519876));
#380999=CARTESIAN_POINT('Ctrl Pts',(0.332480810620154,2.64261629715804,
8.86654584966058));
#381000=CARTESIAN_POINT('Ctrl Pts',(0.329859545232487,2.6373009307027,8.87215952290714));
#381001=CARTESIAN_POINT('Ctrl Pts',(0.335155581859841,2.64662214142563,
8.85049129520029));
#381002=CARTESIAN_POINT('Ctrl Pts',(0.333042822978374,2.6520661621945,8.85711686593484));
#381003=CARTESIAN_POINT('Ctrl Pts',(0.324576590381406,2.65087298671372,
8.85933012996512));
#381004=CARTESIAN_POINT('Origin',(0.357258508851204,2.63774729990957,8.85049129520029));
#381005=CARTESIAN_POINT('Ctrl Pts',(0.389059322317652,2.7029863147688,8.78727029226991));
#381006=CARTESIAN_POINT('Ctrl Pts',(0.392526512802761,2.7077752568042,8.79393457792714));
#381007=CARTESIAN_POINT('Ctrl Pts',(0.40047903875831,2.70439935009569,8.79610912703474));
#381008=CARTESIAN_POINT('Ctrl Pts',(0.375103874792494,2.68371081503406,
8.80838214965003));
#381009=CARTESIAN_POINT('Ctrl Pts',(0.378570489461518,2.68849896174254,
8.81501364461987));
#381010=CARTESIAN_POINT('Ctrl Pts',(0.38648835703967,2.68512906773677,8.81722098428722));
#381011=CARTESIAN_POINT('Ctrl Pts',(0.361129150869144,2.66440869041269,
8.82945683644722));
#381012=CARTESIAN_POINT('Ctrl Pts',(0.364582138437037,2.66917801513908,
8.83607469902391));
#381013=CARTESIAN_POINT('Ctrl Pts',(0.372477500384153,2.66583207697138,
8.8382956714852));
#381014=CARTESIAN_POINT('Ctrl Pts',(0.34713356539705,2.64507775146798,8.85049129520029));
#381015=CARTESIAN_POINT('Ctrl Pts',(0.350558127032854,2.64980781381701,
8.85711686593484));
#381016=CARTESIAN_POINT('Ctrl Pts',(0.358444815903088,2.64650616259708,
8.85933012996512));
#381017=CARTESIAN_POINT('Origin',(0.399184265771806,2.69565586321039,8.78727029226991));
#381018=CARTESIAN_POINT('Ctrl Pts',(0.397174100220844,2.71419455155609,
8.75374538247847));
#381019=CARTESIAN_POINT('Ctrl Pts',(0.401619776138006,2.72035737104292,
8.75304829418601));
#381020=CARTESIAN_POINT('Ctrl Pts',(0.409164941549523,2.71919930277122,
8.75272238421917));
#381021=CARTESIAN_POINT('Ctrl Pts',(0.397948185988952,2.71526373261546,
8.76769408445021));
#381022=CARTESIAN_POINT('Ctrl Pts',(0.402506294519329,2.72158123224723,
8.76974318093972));
#381023=CARTESIAN_POINT('Ctrl Pts',(0.409995042726933,2.7206132407373,8.7707786988043));
#381024=CARTESIAN_POINT('Ctrl Pts',(0.393980663297225,2.70978371958609,
8.78108014887987));
#381025=CARTESIAN_POINT('Ctrl Pts',(0.397840414937049,2.71513979600258,
8.78639403366322));
#381026=CARTESIAN_POINT('Ctrl Pts',(0.405740331578681,2.71337531512024,
8.78812224174741));
#381027=CARTESIAN_POINT('Ctrl Pts',(0.387478769473589,2.70080318793564,
8.78944554828686));
#381028=CARTESIAN_POINT('Ctrl Pts',(0.390727083660423,2.70532036322122,
8.79673892988687));
#381029=CARTESIAN_POINT('Ctrl Pts',(0.398801680886371,2.70153824292232,
8.79894799272499));
#381030=CARTESIAN_POINT('Origin',(0.407407613908421,2.70701409049334,8.75721825406948));
#381031=CARTESIAN_POINT('Origin',(0.407407613908421,2.70701409049334,9.));
#381032=CARTESIAN_POINT('Origin',(0.40740761390842,2.70701409049334,7.51860402984325));
#381033=CARTESIAN_POINT('Ctrl Pts',(0.389948361794135,2.71851300338654,
7.50366195182966));
#381034=CARTESIAN_POINT('Ctrl Pts',(0.390468316773883,2.72213785352538,
7.50000065167736));
#381035=CARTESIAN_POINT('Ctrl Pts',(0.390468316773998,2.72213785352537,
7.49482233047108));
#381036=CARTESIAN_POINT('Ctrl Pts',(0.397374485980921,2.7189674031765,7.50215800491337));
#381037=CARTESIAN_POINT('Ctrl Pts',(0.399905086144918,2.7207842025557,7.49877273257266));
#381038=CARTESIAN_POINT('Ctrl Pts',(0.403322237117531,2.72029406422793,
7.49481816995647));
#381039=CARTESIAN_POINT('Ctrl Pts',(0.398935316024003,2.71662778228441,
7.51043025814043));
#381040=CARTESIAN_POINT('Ctrl Pts',(0.403523181590999,2.72023946423693,
7.51006209594515));
#381041=CARTESIAN_POINT('Ctrl Pts',(0.409270426317654,2.71937450862293,
7.50731281821701));
#381042=CARTESIAN_POINT('Ctrl Pts',(0.397281784184358,2.71434331776496,
7.51860402984326));
#381043=CARTESIAN_POINT('Ctrl Pts',(0.401743390778344,2.72050733301407,
7.51860402984326));
#381044=CARTESIAN_POINT('Ctrl Pts',(0.409267922647734,2.71937488542709,
7.51860402984327));
#381045=CARTESIAN_POINT('Origin',(0.,0.,7.5));
#381046=CARTESIAN_POINT('Origin',(0.515891055659628,2.61740223164621,7.5));
#381047=CARTESIAN_POINT('',(0.515891055659628,2.61740223164621,7.59394543036555));
#381048=CARTESIAN_POINT('',(0.515891055659628,2.61740223164621,8.85049129520029));
#381049=CARTESIAN_POINT('',(0.515891055659628,2.61740223164621,7.5));
#381050=CARTESIAN_POINT('',(0.561440886005564,2.67250562312429,8.78727029226991));
#381051=CARTESIAN_POINT('Ctrl Pts',(0.515891055659628,2.61740223164621,
8.85049129520029));
#381052=CARTESIAN_POINT('Ctrl Pts',(0.531096402804831,2.63579672817757,
8.82945686509571));
#381053=CARTESIAN_POINT('Ctrl Pts',(0.546279145362893,2.6541638790656,8.80838212259895));
#381054=CARTESIAN_POINT('Ctrl Pts',(0.561440886005564,2.67250562312429,
8.78727029226991));
#381055=CARTESIAN_POINT('',(0.57037506251209,2.68331364198703,8.75721825406948));
#381056=CARTESIAN_POINT('Origin',(0.543488870575911,2.65078869247541,8.75937679713127));
#381057=CARTESIAN_POINT('',(0.57037506251209,2.68331364198703,7.51860402984325));
#381058=CARTESIAN_POINT('',(0.57037506251209,2.68331364198703,7.5));
#381059=CARTESIAN_POINT('Ctrl Pts',(0.57037506251209,2.68331364198703,7.51860402984325));
#381060=CARTESIAN_POINT('Ctrl Pts',(0.563358656393491,2.67482562413524,
7.52834476460825));
#381061=CARTESIAN_POINT('Ctrl Pts',(0.556337695325281,2.66633209598475,
7.53807742314407));
#381062=CARTESIAN_POINT('Ctrl Pts',(0.549312026368974,2.65783287251993,
7.54780169004674));
#381063=CARTESIAN_POINT('Ctrl Pts',(0.538183746447192,2.6443705618955,7.5632044032688));
#381064=CARTESIAN_POINT('Ctrl Pts',(0.52704364089139,2.63089394534418,7.57858609112103));
#381065=CARTESIAN_POINT('Ctrl Pts',(0.515891055659629,2.61740223164621,
7.59394543036555));
#381066=CARTESIAN_POINT('Origin',(0.421172437192753,2.88192934915565,7.5));
#381067=CARTESIAN_POINT('',(0.478268870165622,2.70125132133977,8.75721825406948));
#381068=CARTESIAN_POINT('',(0.482494215215309,2.68788048588352,8.78727029226991));
#381069=CARTESIAN_POINT('Origin',(0.493219716926182,2.65394031842374,8.75658640621087));
#381070=CARTESIAN_POINT('',(0.504036631578554,2.61971088052921,8.85049129520029));
#381071=CARTESIAN_POINT('Ctrl Pts',(0.482494215215309,2.68788048588352,
8.78727029226991));
#381072=CARTESIAN_POINT('Ctrl Pts',(0.489664835330364,2.66518951495684,
8.80838212259895));
#381073=CARTESIAN_POINT('Ctrl Pts',(0.496845388127988,2.6424671126884,8.82945686509571));
#381074=CARTESIAN_POINT('Ctrl Pts',(0.504036631578554,2.61971088052921,
8.85049129520029));
#381075=CARTESIAN_POINT('',(0.504036631578554,2.61971088052921,7.59394543036555));
#381076=CARTESIAN_POINT('',(0.504036631578554,2.61971088052921,7.5));
#381077=CARTESIAN_POINT('',(0.478268870165622,2.70125132133977,7.51860402984325));
#381078=CARTESIAN_POINT('Ctrl Pts',(0.504036631578554,2.61971088052921,
7.59394543036555));
#381079=CARTESIAN_POINT('Ctrl Pts',(0.498762108429631,2.63640177329775,
7.57858609112103));
#381080=CARTESIAN_POINT('Ctrl Pts',(0.493493487440537,2.65307398905726,
7.56320440326857));
#381081=CARTESIAN_POINT('Ctrl Pts',(0.488230459287388,2.66972850664335,
7.54780169004651));
#381082=CARTESIAN_POINT('Ctrl Pts',(0.484907727133662,2.68024308104383,
7.53807742314383));
#381083=CARTESIAN_POINT('Ctrl Pts',(0.481587221536694,2.69075060964715,
7.52834476460825));
#381084=CARTESIAN_POINT('Ctrl Pts',(0.478268870165622,2.70125132133977,
7.51860402984325));
#381085=CARTESIAN_POINT('',(0.478268870165622,2.70125132133977,7.5));
#381086=CARTESIAN_POINT('Origin',(0.510592093294214,2.62178248538886,7.5));
#381087=CARTESIAN_POINT('Ctrl Pts',(0.504036631578554,2.61971088052921,
8.85049129520029));
#381088=CARTESIAN_POINT('Ctrl Pts',(0.504094986504631,2.61952622008007,
8.85097269580138));
#381089=CARTESIAN_POINT('Ctrl Pts',(0.504160625639675,2.61934642402759,
8.85143669361005));
#381090=CARTESIAN_POINT('Ctrl Pts',(0.504237392721289,2.61916351316932,
8.8519052845931));
#381091=CARTESIAN_POINT('Ctrl Pts',(0.504387544264533,2.61880575113034,
8.85282181883899));
#381092=CARTESIAN_POINT('Ctrl Pts',(0.504576586788838,2.61844535224755,
8.85372622499636));
#381093=CARTESIAN_POINT('Ctrl Pts',(0.504821141016025,2.61808382343919,
8.85462257735071));
#381094=CARTESIAN_POINT('Ctrl Pts',(0.505024161249691,2.61778369506278,
8.85536669723986));
#381095=CARTESIAN_POINT('Ctrl Pts',(0.505265458768457,2.61748270182885,
8.85610498449051));
#381096=CARTESIAN_POINT('Ctrl Pts',(0.50556080719274,2.61718668585866,8.85681338218371));
#381097=CARTESIAN_POINT('Ctrl Pts',(0.50582883635163,2.61691805090081,8.85745625420285));
#381098=CARTESIAN_POINT('Ctrl Pts',(0.506144318101219,2.61664972254578,
8.85808743050666));
#381099=CARTESIAN_POINT('Ctrl Pts',(0.506533369387132,2.61639335202954,
8.8586680450841));
#381100=CARTESIAN_POINT('Ctrl Pts',(0.506712869216856,2.61627506823078,
8.85893592806395));
#381101=CARTESIAN_POINT('Ctrl Pts',(0.506908237766501,2.61615945434576,
8.85919241173848));
#381102=CARTESIAN_POINT('Ctrl Pts',(0.507123281853302,2.61604865749327,
8.85943017985534));
#381103=CARTESIAN_POINT('Ctrl Pts',(0.507413655030347,2.61589904894304,
8.8597512372));
#381104=CARTESIAN_POINT('Ctrl Pts',(0.507747586735331,2.61575498477418,
8.86004599534705));
#381105=CARTESIAN_POINT('Ctrl Pts',(0.508125190597089,2.61562775896039,
8.86026130871721));
#381106=CARTESIAN_POINT('Ctrl Pts',(0.508263442016658,2.61558117800309,
8.86034014101235));
#381107=CARTESIAN_POINT('Ctrl Pts',(0.508409620434265,2.61553614284821,
8.86040910639692));
#381108=CARTESIAN_POINT('Ctrl Pts',(0.50855984234006,2.6154942019216,8.86046313645506));
#381109=CARTESIAN_POINT('Ctrl Pts',(0.508794262365954,2.61542875345688,
8.86054744990829));
#381110=CARTESIAN_POINT('Ctrl Pts',(0.509044967329408,2.61536919493122,
8.86059655985668));
#381111=CARTESIAN_POINT('Ctrl Pts',(0.509295811046165,2.6153190609893,8.86059725258815));
#381112=CARTESIAN_POINT('Ctrl Pts',(0.50954723431212,2.61526881121795,8.86059794692011));
#381113=CARTESIAN_POINT('Ctrl Pts',(0.509802105972853,2.61523007760143,
8.86056369958366));
#381114=CARTESIAN_POINT('Ctrl Pts',(0.510045959806687,2.61520125230873,
8.86048590497774));
#381115=CARTESIAN_POINT('Ctrl Pts',(0.510109598396914,2.61519372976556,
8.86046560290182));
#381116=CARTESIAN_POINT('Ctrl Pts',(0.510173325147798,2.61518687412201,
8.86044257503091));
#381117=CARTESIAN_POINT('Ctrl Pts',(0.510235167338841,2.61518086458528,
8.86041778462583));
#381118=CARTESIAN_POINT('Ctrl Pts',(0.510651288544795,2.61514042786026,
8.860250975962));
#381119=CARTESIAN_POINT('Ctrl Pts',(0.511037954093418,2.61513320389167,
8.8599848982295));
#381120=CARTESIAN_POINT('Ctrl Pts',(0.511383719971653,2.61515093251764,
8.85968173251461));
#381121=CARTESIAN_POINT('Ctrl Pts',(0.511566610311217,2.61516030994504,
8.85952137522076));
#381122=CARTESIAN_POINT('Ctrl Pts',(0.511741592847463,2.61517665866632,
8.85934740853961));
#381123=CARTESIAN_POINT('Ctrl Pts',(0.511906344552753,2.61519820031704,
8.8591675900182));
#381124=CARTESIAN_POINT('Ctrl Pts',(0.512567908285739,2.61528470124179,
8.85844552518694));
#381125=CARTESIAN_POINT('Ctrl Pts',(0.513102288376397,2.6154568235023,8.8575944418412));
#381126=CARTESIAN_POINT('Ctrl Pts',(0.513525387806243,2.61563629809098,
8.85683498915133));
#381127=CARTESIAN_POINT('Ctrl Pts',(0.513569664034758,2.6156550796287,8.85675551444994));
#381128=CARTESIAN_POINT('Ctrl Pts',(0.513612710375454,2.61567395818294,
8.85667699793649));
#381129=CARTESIAN_POINT('Ctrl Pts',(0.513654537106058,2.61569285451441,
8.85659965593547));
#381130=CARTESIAN_POINT('Ctrl Pts',(0.514219116450193,2.61594791816087,
8.85555568965886));
#381131=CARTESIAN_POINT('Ctrl Pts',(0.514724875940979,2.61627458655636,
8.85434650606346));
#381132=CARTESIAN_POINT('Ctrl Pts',(0.515177687654578,2.61666925409151,
8.85297329937117));
#381133=CARTESIAN_POINT('Ctrl Pts',(0.515432366653254,2.61689123053259,
8.85220095427747));
#381134=CARTESIAN_POINT('Ctrl Pts',(0.515670193285084,2.61713504588954,
8.85137579139183));
#381135=CARTESIAN_POINT('Ctrl Pts',(0.515891055659628,2.61740223164621,
8.85049129520029));
#381136=CARTESIAN_POINT('Origin',(0.510592093294214,2.62178248538886,7.59394543036555));
#381137=CARTESIAN_POINT('Ctrl Pts',(0.504206055614804,2.61917474895075,
7.59443877723642));
#381138=CARTESIAN_POINT('Ctrl Pts',(0.505950960172756,2.61365310954453,
7.58783886950015));
#381139=CARTESIAN_POINT('Ctrl Pts',(0.514418553684581,2.61426877313379,
7.58559994247159));
#381140=CARTESIAN_POINT('Ctrl Pts',(0.494680672826266,2.6493172164713,7.56670252222138));
#381141=CARTESIAN_POINT('Ctrl Pts',(0.496423055501803,2.64380355740166,
7.56004874999028));
#381142=CARTESIAN_POINT('Ctrl Pts',(0.504942371819573,2.64440155968669,
7.55786368756704));
#381143=CARTESIAN_POINT('Ctrl Pts',(0.485173077738388,2.67940339594535,
7.53888913333558));
#381144=CARTESIAN_POINT('Ctrl Pts',(0.486925815479428,2.67385696892987,
7.53222002137275));
#381145=CARTESIAN_POINT('Ctrl Pts',(0.495482437381201,2.67447879394539,
7.53005029815327));
#381146=CARTESIAN_POINT('Ctrl Pts',(0.475683700576278,2.70943192595292,
7.51101258149734));
#381147=CARTESIAN_POINT('Ctrl Pts',(0.477457684683531,2.70381826616392,
7.5043616886572));
#381148=CARTESIAN_POINT('Ctrl Pts',(0.486039296596597,2.70449901466241,
7.50217374673251));
#381149=CARTESIAN_POINT('',(0.486543193738902,2.70289709681368,7.50366116523517));
#381150=CARTESIAN_POINT('Ctrl Pts',(0.478268870165621,2.70125132133977,
7.51860402984325));
#381151=CARTESIAN_POINT('Ctrl Pts',(0.478135801956109,2.70167240721866,
7.51734760759494));
#381152=CARTESIAN_POINT('Ctrl Pts',(0.478072287298077,2.70207084635854,
7.51608817408573));
#381153=CARTESIAN_POINT('Ctrl Pts',(0.478091659423082,2.70244782447943,
7.5148100591312));
#381154=CARTESIAN_POINT('Ctrl Pts',(0.478109207156824,2.70278930026952,
7.51365231206384));
#381155=CARTESIAN_POINT('Ctrl Pts',(0.478194539795407,2.70311366110739,
7.51247773061043));
#381156=CARTESIAN_POINT('Ctrl Pts',(0.478381890731902,2.70340589983578,
7.51129758471022));
#381157=CARTESIAN_POINT('Ctrl Pts',(0.47861474654968,2.70376911920024,7.50983079813402));
#381158=CARTESIAN_POINT('Ctrl Pts',(0.479008730001262,2.70406409599669,
7.50839324291155));
#381159=CARTESIAN_POINT('Ctrl Pts',(0.479616125507346,2.7042269903487,7.50715379678855));
#381160=CARTESIAN_POINT('Ctrl Pts',(0.479896724729476,2.70430224284564,
7.50658120839351));
#381161=CARTESIAN_POINT('Ctrl Pts',(0.480265220758786,2.7043508270587,7.50598221009429));
#381162=CARTESIAN_POINT('Ctrl Pts',(0.480715817181737,2.7043490354212,7.50545747549611));
#381163=CARTESIAN_POINT('Ctrl Pts',(0.480956269380287,2.70434807934798,
7.50517746087247));
#381164=CARTESIAN_POINT('Ctrl Pts',(0.481222708816388,2.70433297027813,
7.50491486231392));
#381165=CARTESIAN_POINT('Ctrl Pts',(0.481507985287802,2.70430244298451,
7.50468370960993));
#381166=CARTESIAN_POINT('Ctrl Pts',(0.481934563597929,2.70425679505125,
7.50433806340447));
#381167=CARTESIAN_POINT('Ctrl Pts',(0.482415993154627,2.70417475013281,
7.50405484070984));
#381168=CARTESIAN_POINT('Ctrl Pts',(0.482919730219993,2.70406112758865,
7.50385766036131));
#381169=CARTESIAN_POINT('Ctrl Pts',(0.482973597069285,2.70404897742364,
7.50383657498791));
#381170=CARTESIAN_POINT('Ctrl Pts',(0.483027698355582,2.70403648561238,
7.50381643264937));
#381171=CARTESIAN_POINT('Ctrl Pts',(0.483081979503558,2.70402367240709,
7.50379723213559));
#381172=CARTESIAN_POINT('Ctrl Pts',(0.483444323922905,2.70393814007029,
7.50366906242519));
#381173=CARTESIAN_POINT('Ctrl Pts',(0.483822399615159,2.70383572607388,
7.50358235568538));
#381174=CARTESIAN_POINT('Ctrl Pts',(0.484184445158432,2.70372825171679,
7.5035341175365));
#381175=CARTESIAN_POINT('Ctrl Pts',(0.484727291474926,2.70356710608208,
7.50346178989176));
#381176=CARTESIAN_POINT('Ctrl Pts',(0.485304418855281,2.70337066885157,
7.50346967198527));
#381177=CARTESIAN_POINT('Ctrl Pts',(0.48586504542762,2.70316039527586,7.50354272648692));
#381178=CARTESIAN_POINT('Ctrl Pts',(0.486095642741106,2.70307390540177,
7.50357277531559));
#381179=CARTESIAN_POINT('Ctrl Pts',(0.486323191778091,2.70298532231186,
7.50361331098761));
#381180=CARTESIAN_POINT('Ctrl Pts',(0.486543193739153,2.70289709681507,
7.50366116523659));
#381181=CARTESIAN_POINT('',(0.511151791457249,2.62465641716279,7.57603338622103));
#381182=CARTESIAN_POINT('Origin',(0.512843849057291,2.63332984962507,7.58486873427626));
#381183=CARTESIAN_POINT('Ctrl Pts',(0.486543193716658,2.70289709686654,
7.50366116529969));
#381184=CARTESIAN_POINT('Ctrl Pts',(0.494733471570576,2.67685967864821,
7.52783573079709));
#381185=CARTESIAN_POINT('Ctrl Pts',(0.502935967272698,2.65078068885653,
7.55196141284069));
#381186=CARTESIAN_POINT('Ctrl Pts',(0.511151790759542,2.62465641820243,
7.57603338728831));
#381187=CARTESIAN_POINT('Ctrl Pts',(0.503894391761599,2.62074446814269,
7.59639677331371));
#381188=CARTESIAN_POINT('Ctrl Pts',(0.506703515972806,2.60181546269511,
7.59974925422224));
#381189=CARTESIAN_POINT('Ctrl Pts',(0.516410771457479,2.61830690341518,
7.59639677331372));
#381190=CARTESIAN_POINT('Ctrl Pts',(0.503839346059811,2.61684420224733,
7.58707626057421));
#381191=CARTESIAN_POINT('Ctrl Pts',(0.508673304164263,2.61192990874306,
7.58811717123965));
#381192=CARTESIAN_POINT('Ctrl Pts',(0.514998153140065,2.61467102476307,
7.58707626057424));
#381193=CARTESIAN_POINT('Ctrl Pts',(0.508250440815437,2.62102366098245,
7.58015376756929));
#381194=CARTESIAN_POINT('Ctrl Pts',(0.509994474415054,2.61871383875087,
7.5820876076604));
#381195=CARTESIAN_POINT('Ctrl Pts',(0.512477848454474,2.62020037341847,
7.5801537675693));
#381196=CARTESIAN_POINT('Ctrl Pts',(0.511151791298856,2.62465641635052,
7.57603338509286));
#381197=CARTESIAN_POINT('Ctrl Pts',(0.511151791298856,2.62465641635052,
7.57603338509286));
#381198=CARTESIAN_POINT('Ctrl Pts',(0.511151791298856,2.62465641635052,
7.57603338509286));
#381199=CARTESIAN_POINT('Origin',(0.512838247935124,2.63333094044375,7.58486873427622));
#381200=CARTESIAN_POINT('Ctrl Pts',(0.575858486682816,2.68994715228608,
7.51098857897448));
#381201=CARTESIAN_POINT('Ctrl Pts',(0.572107512685082,2.68540945396643,
7.50433767179956));
#381202=CARTESIAN_POINT('Ctrl Pts',(0.564408512768194,2.68926087595866,
7.50214974420965));
#381203=CARTESIAN_POINT('Ctrl Pts',(0.555788136368668,2.6656672732599,7.53887321589171));
#381204=CARTESIAN_POINT('Ctrl Pts',(0.552082105696194,2.66118394461906,
7.53220407452063));
#381205=CARTESIAN_POINT('Ctrl Pts',(0.544384150308548,2.66497134514866,
7.53003438070911));
#381206=CARTESIAN_POINT('Ctrl Pts',(0.535679243578228,2.64134076790945,
7.56669465659231));
#381207=CARTESIAN_POINT('Ctrl Pts',(0.531995114858024,2.63688393490738,
7.56004085833299));
#381208=CARTESIAN_POINT('Ctrl Pts',(0.524322805054424,2.64063524299977,
7.55785582193788));
#381209=CARTESIAN_POINT('Ctrl Pts',(0.515532717756307,2.61696873642531,
7.59443891967696));
#381210=CARTESIAN_POINT('Ctrl Pts',(0.511843247508148,2.61250544157026,
7.58783901202978));
#381211=CARTESIAN_POINT('Ctrl Pts',(0.504225531563093,2.61625371874368,
7.58560008491213));
#381212=CARTESIAN_POINT('',(0.563323058569111,2.68794421947737,7.50366116523517));
#381213=CARTESIAN_POINT('Ctrl Pts',(0.563323058569187,2.68794421947773,
7.50366116523554));
#381214=CARTESIAN_POINT('Ctrl Pts',(0.564080772489997,2.68794154908911,
7.50350835821027));
#381215=CARTESIAN_POINT('Ctrl Pts',(0.564777208608279,2.687914442922,7.50345484956));
#381216=CARTESIAN_POINT('Ctrl Pts',(0.565433095890476,2.68786269513526,
7.50349758195598));
#381217=CARTESIAN_POINT('Ctrl Pts',(0.565769614708112,2.68783614468294,
7.50351950684424));
#381218=CARTESIAN_POINT('Ctrl Pts',(0.566128638073164,2.68780061956941,
7.50357029184312));
#381219=CARTESIAN_POINT('Ctrl Pts',(0.566473898535874,2.68775684670367,
7.50365515313924));
#381220=CARTESIAN_POINT('Ctrl Pts',(0.56700504893729,2.68768950631076,7.50378570417639));
#381221=CARTESIAN_POINT('Ctrl Pts',(0.567519261867555,2.6876010137059,7.50400001621911));
#381222=CARTESIAN_POINT('Ctrl Pts',(0.567977013192507,2.68749586693788,
7.50428903009635));
#381223=CARTESIAN_POINT('Ctrl Pts',(0.568027820067849,2.68748419645558,
7.50432110841318));
#381224=CARTESIAN_POINT('Ctrl Pts',(0.568077959553033,2.68747233198995,
7.50435406373354));
#381225=CARTESIAN_POINT('Ctrl Pts',(0.568127398514568,2.68746028766373,
7.50438785222352));
#381226=CARTESIAN_POINT('Ctrl Pts',(0.568429247138127,2.68738675126291,
7.50459414719561));
#381227=CARTESIAN_POINT('Ctrl Pts',(0.568709666076621,2.68730483834955,
7.50483629897752));
#381228=CARTESIAN_POINT('Ctrl Pts',(0.568958281566933,2.68721895022316,
7.5050991045531));
#381229=CARTESIAN_POINT('Ctrl Pts',(0.569506752309622,2.68702947238968,
7.50567888004914));
#381230=CARTESIAN_POINT('Ctrl Pts',(0.569922222282148,2.68681367292768,
7.50637912803145));
#381231=CARTESIAN_POINT('Ctrl Pts',(0.570225606143944,2.68659431134895,
7.50710440483569));
#381232=CARTESIAN_POINT('Ctrl Pts',(0.570300001889869,2.68654051953491,
7.50728225710685));
#381233=CARTESIAN_POINT('Ctrl Pts',(0.570369224095775,2.68648556096084,
7.50746498566954));
#381234=CARTESIAN_POINT('Ctrl Pts',(0.570431915928522,2.68643104480392,
7.50764697238949));
#381235=CARTESIAN_POINT('Ctrl Pts',(0.570768929968109,2.68613798094756,
7.50862528291181));
#381236=CARTESIAN_POINT('Ctrl Pts',(0.570950535870584,2.68583422188778,
7.50965856837421));
#381237=CARTESIAN_POINT('Ctrl Pts',(0.571040685959675,2.68553724607221,
7.51067959873201));
#381238=CARTESIAN_POINT('Ctrl Pts',(0.571090295667412,2.68537381990632,
7.51124147302578));
#381239=CARTESIAN_POINT('Ctrl Pts',(0.571111806105353,2.6852122818537,7.51180065547252));
#381240=CARTESIAN_POINT('Ctrl Pts',(0.571113248871017,2.6850548511387,7.51235175716501));
#381241=CARTESIAN_POINT('Ctrl Pts',(0.571118234201117,2.68451086530544,
7.51425603304536));
#381242=CARTESIAN_POINT('Ctrl Pts',(0.570878146117182,2.68395100448379,
7.51626900505181));
#381243=CARTESIAN_POINT('Ctrl Pts',(0.570446802542537,2.68340258713866,
7.51827788969244));
#381244=CARTESIAN_POINT('Ctrl Pts',(0.570423457413152,2.68337290575557,
7.51838661432546));
#381245=CARTESIAN_POINT('Ctrl Pts',(0.570399542264644,2.68334325609048,
7.51849533314857));
#381246=CARTESIAN_POINT('Ctrl Pts',(0.570375062512093,2.68331364198703,
7.51860402984325));
#381247=CARTESIAN_POINT('Ctrl Pts',(0.511151792494568,2.62465641786575,
7.57603338728984));
#381248=CARTESIAN_POINT('Ctrl Pts',(0.528570753766796,2.64578831464074,
7.55196141284921));
#381249=CARTESIAN_POINT('Ctrl Pts',(0.545960368888797,2.66688324131613,
7.52783573083105));
#381250=CARTESIAN_POINT('Ctrl Pts',(0.563323058610791,2.68794421951938,
7.50366116530176));
#381251=CARTESIAN_POINT('Origin',(1.76626572250563E-16,9.06940118467445E-16,
7.49482233047033));
#381252=CARTESIAN_POINT('Origin',(0.484977299960256,2.69419807522076,7.49482233047033));
#381253=CARTESIAN_POINT('Origin',(0.,0.,7.50366116523517));
#381254=CARTESIAN_POINT('Origin',(0.561510055974207,2.67929332232211,7.49482233047033));
#381255=CARTESIAN_POINT('Ctrl Pts',(0.478269188839816,2.70125031276705,
7.51860402984325));
#381256=CARTESIAN_POINT('Ctrl Pts',(0.475977037628223,2.70850581611646,
7.51860402984325));
#381257=CARTESIAN_POINT('Ctrl Pts',(0.468479300229098,2.70980204909083,
7.51860402984325));
#381258=CARTESIAN_POINT('Ctrl Pts',(0.477418096240793,2.70394433029203,
7.51041458714366));
#381259=CARTESIAN_POINT('Ctrl Pts',(0.474200736074164,2.70881289880015,
7.5100464290044));
#381260=CARTESIAN_POINT('Ctrl Pts',(0.468477232442144,2.7098024065765,7.50729136483009));
#381261=CARTESIAN_POINT('Ctrl Pts',(0.47964495815025,2.70566619649923,7.50215815450137));
#381262=CARTESIAN_POINT('Ctrl Pts',(0.477817487202485,2.70818778615986,
7.49877163671533));
#381263=CARTESIAN_POINT('Ctrl Pts',(0.474421859314631,2.70879904293209,
7.49481588533172));
#381264=CARTESIAN_POINT('Ctrl Pts',(0.486543096209234,2.7028965550037,7.50366171572174));
#381265=CARTESIAN_POINT('Ctrl Pts',(0.487191808179633,2.70650034953677,
7.50000045605858));
#381266=CARTESIAN_POINT('Ctrl Pts',(0.48719180817951,2.7065003495368,7.49482233047317));
#381267=CARTESIAN_POINT('Origin',(0.466349848864421,2.69748476704951,7.51860402984325));
#381268=CARTESIAN_POINT('Origin',(0.466349848864421,2.69748476704951,9.));
#381269=CARTESIAN_POINT('Origin',(0.466349848864421,2.69748476704951,8.75721825406948));
#381270=CARTESIAN_POINT('Ctrl Pts',(0.483301006436993,2.68532734615808,
8.78942910404912));
#381271=CARTESIAN_POINT('Ctrl Pts',(0.481641165693858,2.69064687220925,
8.7967269950169));
#381272=CARTESIAN_POINT('Ctrl Pts',(0.472776992362322,2.68959810286835,
8.79893251111267));
#381273=CARTESIAN_POINT('Ctrl Pts',(0.479988149754479,2.69581068528935,
8.78111911759585));
#381274=CARTESIAN_POINT('Ctrl Pts',(0.478013283372308,2.70211482780821,
8.78644465894814));
#381275=CARTESIAN_POINT('Ctrl Pts',(0.46994596940398,2.70291104204566,8.78817647674132));
#381276=CARTESIAN_POINT('Ctrl Pts',(0.477923498420489,2.70234415227765,
8.76780923932028));
#381277=CARTESIAN_POINT('Ctrl Pts',(0.475587389273433,2.7097844030008,8.76988516158372));
#381278=CARTESIAN_POINT('Ctrl Pts',(0.468166832892768,2.71122375125526,
8.77093053738833));
#381279=CARTESIAN_POINT('Ctrl Pts',(0.478326077172229,2.70107021563117,
8.75371302330493));
#381280=CARTESIAN_POINT('Ctrl Pts',(0.476048030768675,2.70832808762997,
8.75300828287559));
#381281=CARTESIAN_POINT('Ctrl Pts',(0.468513389351356,2.70960233958568,
8.75267964240738));
#381282=CARTESIAN_POINT('Origin',(0.470575193914108,2.68411393159326,8.78727029226991));
#381283=CARTESIAN_POINT('Ctrl Pts',(0.504036631578554,2.61971088052921,
8.85049129520029));
#381284=CARTESIAN_POINT('Ctrl Pts',(0.502277013195043,2.62527908089984,
8.85711686593484));
#381285=CARTESIAN_POINT('Ctrl Pts',(0.493751728365416,2.62463079031095,
8.85933012996512));
#381286=CARTESIAN_POINT('Ctrl Pts',(0.496845378477071,2.64246714322811,
8.82945683644722));
#381287=CARTESIAN_POINT('Ctrl Pts',(0.495071154197079,2.64808156302842,
8.83607469902389));
#381288=CARTESIAN_POINT('Ctrl Pts',(0.486523682952831,2.64739397461503,
8.8382956714852));
#381289=CARTESIAN_POINT('Ctrl Pts',(0.489664844518242,2.66518948588238,
8.80838214965002));
#381290=CARTESIAN_POINT('Ctrl Pts',(0.48788361832088,2.67082606280458,8.81501364461995));
#381291=CARTESIAN_POINT('Ctrl Pts',(0.479307239296681,2.67012283067464,
8.81722098428721));
#381292=CARTESIAN_POINT('Ctrl Pts',(0.482494215215309,2.68788048588352,
8.78727029226991));
#381293=CARTESIAN_POINT('Ctrl Pts',(0.480712693150428,2.69351799905963,
8.79393457792714));
#381294=CARTESIAN_POINT('Ctrl Pts',(0.472101526741932,2.69281998167919,
8.79610912703474));
#381295=CARTESIAN_POINT('Origin',(0.492117610277352,2.61594432623895,8.85049129520029));
#381296=CARTESIAN_POINT('Ctrl Pts',(0.515891055659628,2.61740223164621,
8.85049129520029));
#381297=CARTESIAN_POINT('Ctrl Pts',(0.519611637301493,2.6219031631575,8.85711686593484));
#381298=CARTESIAN_POINT('Ctrl Pts',(0.527270584603639,2.61810299364327,
8.85933012996512));
#381299=CARTESIAN_POINT('Ctrl Pts',(0.512599510788232,2.61342032250981,
8.86332496987232));
#381300=CARTESIAN_POINT('Ctrl Pts',(0.517180599096309,2.61281573646103,
8.86648636486738));
#381301=CARTESIAN_POINT('Ctrl Pts',(0.518049148486212,2.60697435615754,
8.87206031107457));
#381302=CARTESIAN_POINT('Ctrl Pts',(0.505603918890392,2.61475129959255,
8.86341338519876));
#381303=CARTESIAN_POINT('Ctrl Pts',(0.501110700619808,2.61588463988004,
8.86654584966058));
#381304=CARTESIAN_POINT('Ctrl Pts',(0.498154264204941,2.61074813946514,
8.87215952290714));
#381305=CARTESIAN_POINT('Ctrl Pts',(0.504036631578554,2.61971088052921,
8.85049129520029));
#381306=CARTESIAN_POINT('Ctrl Pts',(0.502277013195043,2.62527908089984,
8.85711686593484));
#381307=CARTESIAN_POINT('Ctrl Pts',(0.493751728365416,2.62463079031095,
8.85933012996512));
#381308=CARTESIAN_POINT('Origin',(0.525525532687654,2.60943813393232,8.85049129520029));
#381309=CARTESIAN_POINT('Ctrl Pts',(0.561440886005564,2.67250562312429,
8.78727029226991));
#381310=CARTESIAN_POINT('Ctrl Pts',(0.565207781345649,2.67706258210757,
8.79393457792714));
#381311=CARTESIAN_POINT('Ctrl Pts',(0.572927672898268,2.67318409147409,
8.79610912703474));
#381312=CARTESIAN_POINT('Ctrl Pts',(0.546279125935812,2.65416385556391,
8.80838214965001));
#381313=CARTESIAN_POINT('Ctrl Pts',(0.550045395686141,2.65872005774707,
8.81501364461993));
#381314=CARTESIAN_POINT('Ctrl Pts',(0.557731085305871,2.6548497880324,8.81722098428722));
#381315=CARTESIAN_POINT('Ctrl Pts',(0.531096423210977,2.63579675286367,
8.82945683644723));
#381316=CARTESIAN_POINT('Ctrl Pts',(0.534847887929955,2.64033504482784,
8.8360746990239));
#381317=CARTESIAN_POINT('Ctrl Pts',(0.542512653014727,2.63649012367217,
8.83829567148519));
#381318=CARTESIAN_POINT('Ctrl Pts',(0.515891055659628,2.61740223164621,
8.85049129520029));
#381319=CARTESIAN_POINT('Ctrl Pts',(0.519611637301494,2.6219031631575,8.85711686593484));
#381320=CARTESIAN_POINT('Ctrl Pts',(0.527270584603639,2.61810299364327,
8.85933012996512));
#381321=CARTESIAN_POINT('Origin',(0.57107536303359,2.6645415254104,8.78727029226991));
#381322=CARTESIAN_POINT('Ctrl Pts',(0.570257105423809,2.68317091578168,
8.75374538247848));
#381323=CARTESIAN_POINT('Ctrl Pts',(0.575088500423227,2.68903623766094,
8.75304829418602));
#381324=CARTESIAN_POINT('Ctrl Pts',(0.582543965794262,2.68739712835699,
8.75272238421917));
#381325=CARTESIAN_POINT('Ctrl Pts',(0.571098103415353,2.68418830424844,
8.76769408445019));
#381326=CARTESIAN_POINT('Ctrl Pts',(0.576051610414024,2.69020078488341,
8.76974318093968));
#381327=CARTESIAN_POINT('Ctrl Pts',(0.583462952756301,2.68875497647084,
8.7707786988043));
#381328=CARTESIAN_POINT('Ctrl Pts',(0.566787626784243,2.67897375054523,
8.78108014887991));
#381329=CARTESIAN_POINT('Ctrl Pts',(0.570982613144604,2.68407152719165,
8.78639403366325));
#381330=CARTESIAN_POINT('Ctrl Pts',(0.578753247881939,2.68180452222744,
8.78812224174741));
#381331=CARTESIAN_POINT('Ctrl Pts',(0.559723707160385,2.67042824812776,
8.78944554828685));
#381332=CARTESIAN_POINT('Ctrl Pts',(0.563254763751582,2.67472802218773,
8.79673892988685));
#381333=CARTESIAN_POINT('Ctrl Pts',(0.571070449571984,2.6704363314401,8.79894799272499));
#381334=CARTESIAN_POINT('Origin',(0.580009539540115,2.67534954427314,8.75721825406948));
#381335=CARTESIAN_POINT('Origin',(0.580009539540115,2.67534954427314,9.));
#381336=CARTESIAN_POINT('Origin',(0.580009539540115,2.67534954427314,7.51860402984325));
#381337=CARTESIAN_POINT('Ctrl Pts',(0.563322897210404,2.68794344954021,
7.50366195182966));
#381338=CARTESIAN_POINT('Ctrl Pts',(0.564074028832674,2.69152753840575,
7.50000065167736));
#381339=CARTESIAN_POINT('Ctrl Pts',(0.564074028832788,2.69152753840572,
7.49482233047108));
#381340=CARTESIAN_POINT('Ctrl Pts',(0.5707628771231,2.68792112230681,7.50215800491337));
#381341=CARTESIAN_POINT('Ctrl Pts',(0.57340468063354,2.68957205276766,7.49877273257266));
#381342=CARTESIAN_POINT('Ctrl Pts',(0.576783407432508,2.68886398386711,
7.49481816995649));
#381343=CARTESIAN_POINT('Ctrl Pts',(0.572170600248225,2.68548630569255,
7.51043025814042));
#381344=CARTESIAN_POINT('Ctrl Pts',(0.576980440810566,2.68879662150103,
7.51006209594513));
#381345=CARTESIAN_POINT('Ctrl Pts',(0.58266045931007,2.68756521579719,7.50731281821697));
#381346=CARTESIAN_POINT('Ctrl Pts',(0.570374099622798,2.68331247699919,
7.51860402984325));
#381347=CARTESIAN_POINT('Ctrl Pts',(0.575221469180506,2.68917797150193,
7.51860402984324));
#381348=CARTESIAN_POINT('Ctrl Pts',(0.582657984926149,2.68756575223785,
7.51860402984325));
#381349=CARTESIAN_POINT('Origin',(0.,0.,7.5));
#381350=CARTESIAN_POINT('Origin',(0.682528638916215,2.57897124462359,7.5));
#381351=CARTESIAN_POINT('',(0.682528638916215,2.57897124462359,7.59394543036555));
#381352=CARTESIAN_POINT('',(0.682528638916215,2.57897124462359,8.85049129520029));
#381353=CARTESIAN_POINT('',(0.682528638916215,2.57897124462359,7.5));
#381354=CARTESIAN_POINT('',(0.731515368664185,2.63104303262371,8.78727029226991));
#381355=CARTESIAN_POINT('Ctrl Pts',(0.682528638916215,2.57897124462359,
8.85049129520029));
#381356=CARTESIAN_POINT('Ctrl Pts',(0.698881284484137,2.59635373775255,
8.82945686509571));
#381357=CARTESIAN_POINT('Ctrl Pts',(0.715209619867097,2.61371038970361,
8.80838212259897));
#381358=CARTESIAN_POINT('Ctrl Pts',(0.731515368664185,2.63104303262371,
8.78727029226991));
#381359=CARTESIAN_POINT('',(0.741123661092981,2.64125643059842,8.75721825406948));
#381360=CARTESIAN_POINT('Origin',(0.712208829051163,2.61052091131519,8.75937679713107));
#381361=CARTESIAN_POINT('',(0.741123661092981,2.64125643059842,7.51860402984325));
#381362=CARTESIAN_POINT('',(0.741123661092981,2.64125643059842,7.5));
#381363=CARTESIAN_POINT('Ctrl Pts',(0.741123661092982,2.64125643059842,
7.51860402984325));
#381364=CARTESIAN_POINT('Ctrl Pts',(0.733577841762296,2.63323539497314,
7.52834476460825));
#381365=CARTESIAN_POINT('Ctrl Pts',(0.726027123794582,2.62520915220727,
7.53807742314407));
#381366=CARTESIAN_POINT('Ctrl Pts',(0.718471342711591,2.61717752746415,
7.54780169004674));
#381367=CARTESIAN_POINT('Ctrl Pts',(0.706503393831256,2.60445586794331,
7.5632044032688));
#381368=CARTESIAN_POINT('Ctrl Pts',(0.694522727030052,2.59172068955964,
7.57858609112103));
#381369=CARTESIAN_POINT('Ctrl Pts',(0.682528638916215,2.57897124462359,
7.59394543036555));
#381370=CARTESIAN_POINT('Origin',(0.604952940619213,2.8490235055211,7.5));
#381371=CARTESIAN_POINT('',(0.650355981859121,2.66505851907035,8.75721825406948));
#381372=CARTESIAN_POINT('',(0.653715973115229,2.65144443664273,8.78727029226991));
#381373=CARTESIAN_POINT('Origin',(0.66224488413743,2.6168868176421,8.75658640621054));
#381374=CARTESIAN_POINT('',(0.670846486662589,2.58203466569848,8.85049129520029));
#381375=CARTESIAN_POINT('Ctrl Pts',(0.653715973115229,2.65144443664273,
8.78727029226991));
#381376=CARTESIAN_POINT('Ctrl Pts',(0.659418044923361,2.62834066354125,
8.80838212259896));
#381377=CARTESIAN_POINT('Ctrl Pts',(0.665128015193322,2.60520488728791,
8.82945686509571));
#381378=CARTESIAN_POINT('Ctrl Pts',(0.670846486662589,2.58203466569848,
8.85049129520029));
#381379=CARTESIAN_POINT('',(0.670846486662589,2.58203466569848,7.59394543036555));
#381380=CARTESIAN_POINT('',(0.670846486662589,2.58203466569848,7.5));
#381381=CARTESIAN_POINT('',(0.650355981859121,2.66505851907035,7.51860402984325));
#381382=CARTESIAN_POINT('Ctrl Pts',(0.670846486662589,2.58203466569848,
7.59394543036555));
#381383=CARTESIAN_POINT('Ctrl Pts',(0.666652189758522,2.59902920509618,
7.57858609112103));
#381384=CARTESIAN_POINT('Ctrl Pts',(0.662462586247585,2.61600472770608,
7.56320440326857));
#381385=CARTESIAN_POINT('Ctrl Pts',(0.658277430155648,2.63296223017114,
7.54780169004651));
#381386=CARTESIAN_POINT('Ctrl Pts',(0.655635196006337,2.64366808943085,
7.53807742314383));
#381387=CARTESIAN_POINT('Ctrl Pts',(0.652994732413309,2.65436677471377,
7.52834476460825));
#381388=CARTESIAN_POINT('Ctrl Pts',(0.650355981859121,2.66505851907035,
7.51860402984325));
#381389=CARTESIAN_POINT('',(0.650355981859121,2.66505851907035,7.5));
#381390=CARTESIAN_POINT('Origin',(0.677521207658155,2.58368200434956,7.5));
#381391=CARTESIAN_POINT('Ctrl Pts',(0.670846486662589,2.58203466569848,
8.85049129520029));
#381392=CARTESIAN_POINT('Ctrl Pts',(0.670892890456614,2.58184664584109,
8.85097269580138));
#381393=CARTESIAN_POINT('Ctrl Pts',(0.670946875156382,2.58166301368506,
8.85143669361005));
#381394=CARTESIAN_POINT('Ctrl Pts',(0.671011765372867,2.58147556015296,
8.8519052845931));
#381395=CARTESIAN_POINT('Ctrl Pts',(0.671138686521124,2.58110891293205,
8.85282181883899));
#381396=CARTESIAN_POINT('Ctrl Pts',(0.671304249801585,2.5807371425313,8.85372622499636));
#381397=CARTESIAN_POINT('Ctrl Pts',(0.671525138335603,2.58036068787951,
8.85462257735071));
#381398=CARTESIAN_POINT('Ctrl Pts',(0.671708512151326,2.58004816859801,
8.85536669723986));
#381399=CARTESIAN_POINT('Ctrl Pts',(0.67193002919575,2.57973233380186,8.85610498449051));
#381400=CARTESIAN_POINT('Ctrl Pts',(0.67220580498669,2.57941800298971,8.85681338218371));
#381401=CARTESIAN_POINT('Ctrl Pts',(0.672456071950082,2.57913274728402,
8.85745625420284));
#381402=CARTESIAN_POINT('Ctrl Pts',(0.672753713651846,2.57884475725327,
8.85808743050665));
#381403=CARTESIAN_POINT('Ctrl Pts',(0.673125539874794,2.57856398687628,
8.85866804508409));
#381404=CARTESIAN_POINT('Ctrl Pts',(0.67329709243386,2.5784344455107,8.85893592806395));
#381405=CARTESIAN_POINT('Ctrl Pts',(0.673484652170822,2.57830655186085,
8.85919241173848));
#381406=CARTESIAN_POINT('Ctrl Pts',(0.673692155647773,2.57818220473043,
8.85943017985534));
#381407=CARTESIAN_POINT('Ctrl Pts',(0.673972346769258,2.57801429929367,
8.8597512372));
#381408=CARTESIAN_POINT('Ctrl Pts',(0.67429636215275,2.57784913604231,8.86004599534706));
#381409=CARTESIAN_POINT('Ctrl Pts',(0.674665038801,2.57769797846511,8.86026130871721));
#381410=CARTESIAN_POINT('Ctrl Pts',(0.674800021716019,2.57764263541452,
8.86034014101236));
#381411=CARTESIAN_POINT('Ctrl Pts',(0.67494301438211,2.57758832710582,8.86040910639693));
#381412=CARTESIAN_POINT('Ctrl Pts',(0.675090240476494,2.57753684760079,
8.86046313645507));
#381413=CARTESIAN_POINT('Ctrl Pts',(0.675319985563772,2.57745651426434,
8.8605474499083));
#381414=CARTESIAN_POINT('Ctrl Pts',(0.67556635949915,2.57738101538589,8.86059655985669));
#381415=CARTESIAN_POINT('Ctrl Pts',(0.6758134757379,2.57731491283742,8.86059725258816));
#381416=CARTESIAN_POINT('Ctrl Pts',(0.676061162913886,2.57724865756566,
8.86059794692012));
#381417=CARTESIAN_POINT('Ctrl Pts',(0.676313029242126,2.57719367384813,
8.86056369958366));
#381418=CARTESIAN_POINT('Ctrl Pts',(0.676554535209261,2.57714928401131,
8.86048590497774));
#381419=CARTESIAN_POINT('Ctrl Pts',(0.676617561076184,2.57713769958554,
8.86046560290182));
#381420=CARTESIAN_POINT('Ctrl Pts',(0.676680717651033,2.5771267750407,8.86044257503091));
#381421=CARTESIAN_POINT('Ctrl Pts',(0.676742047748321,2.57711681560842,
8.86041778462584));
#381422=CARTESIAN_POINT('Ctrl Pts',(0.677154723198763,2.57704980098779,
8.86025097596201));
#381423=CARTESIAN_POINT('Ctrl Pts',(0.67754013146029,2.57701781811486,8.8599848982295));
#381424=CARTESIAN_POINT('Ctrl Pts',(0.677886322802411,2.57701335701958,
8.85968173251461));
#381425=CARTESIAN_POINT('Ctrl Pts',(0.678069438187994,2.57701099735577,
8.85952137522076));
#381426=CARTESIAN_POINT('Ctrl Pts',(0.678245108670022,2.57701610131726,
8.85934740853961));
#381427=CARTESIAN_POINT('Ctrl Pts',(0.678410902053563,2.57702704303034,
8.85916759001821));
#381428=CARTESIAN_POINT('Ctrl Pts',(0.679076648666176,2.57707097969576,
8.85844552518695));
#381429=CARTESIAN_POINT('Ctrl Pts',(0.679620958726714,2.57720851046266,
8.85759444184122));
#381430=CARTESIAN_POINT('Ctrl Pts',(0.680054687829779,2.577360508228,8.85683498915136));
#381431=CARTESIAN_POINT('Ctrl Pts',(0.680100076425294,2.57737641438934,
8.85675551444996));
#381432=CARTESIAN_POINT('Ctrl Pts',(0.680144243875795,2.57739249616705,
8.8566769979365));
#381433=CARTESIAN_POINT('Ctrl Pts',(0.680187195361015,2.57740867382615,
8.85659965593547));
#381434=CARTESIAN_POINT('Ctrl Pts',(0.680766956700275,2.57762704069423,
8.85555568965886));
#381435=CARTESIAN_POINT('Ctrl Pts',(0.681292606769904,2.57792063379263,
8.85434650606346));
#381436=CARTESIAN_POINT('Ctrl Pts',(0.68176977456907,2.5782854786949,8.85297329937117));
#381437=CARTESIAN_POINT('Ctrl Pts',(0.682038152381839,2.57849068172211,
8.85220095427747));
#381438=CARTESIAN_POINT('Ctrl Pts',(0.682291111676902,2.57871875852964,
8.85137579139183));
#381439=CARTESIAN_POINT('Ctrl Pts',(0.682528638916215,2.57897124462359,
8.85049129520029));
#381440=CARTESIAN_POINT('Origin',(0.677521207658155,2.58368200434956,7.59394543036555));
#381441=CARTESIAN_POINT('Ctrl Pts',(0.670981212530816,2.58148878062457,
7.59443877723642));
#381442=CARTESIAN_POINT('Ctrl Pts',(0.672368759343803,2.57586668959983,
7.58783886950016));
#381443=CARTESIAN_POINT('Ctrl Pts',(0.680858400978209,2.57593856766321,
7.58559994247159));
#381444=CARTESIAN_POINT('Ctrl Pts',(0.663406635187616,2.61217961058349,
7.56670252222136));
#381445=CARTESIAN_POINT('Ctrl Pts',(0.664792176601528,2.60656564507644,
7.5600487499903));
#381446=CARTESIAN_POINT('Ctrl Pts',(0.673332303208251,2.60661658423106,
7.55786368756705));
#381447=CARTESIAN_POINT('Ctrl Pts',(0.655846202610808,2.64281312848387,
7.53888913333561));
#381448=CARTESIAN_POINT('Ctrl Pts',(0.657239978365199,2.63716579890492,
7.53222002137279));
#381449=CARTESIAN_POINT('Ctrl Pts',(0.6658188602351,2.63723812166669,7.53005029815326));
#381450=CARTESIAN_POINT('Ctrl Pts',(0.648300256915097,2.67338794813823,
7.51101258149734));
#381451=CARTESIAN_POINT('Ctrl Pts',(0.649710927764165,2.66767216266333,
7.5043616886572));
#381452=CARTESIAN_POINT('Ctrl Pts',(0.658318523541229,2.66780168672796,
7.50217374673251));
#381453=CARTESIAN_POINT('',(0.658718750143853,2.6661707753905,7.50366116523517));
#381454=CARTESIAN_POINT('Ctrl Pts',(0.650355981859121,2.66505851907035,
7.51860402984325));
#381455=CARTESIAN_POINT('Ctrl Pts',(0.650250166117407,2.66548726549259,
7.51734760759493));
#381456=CARTESIAN_POINT('Ctrl Pts',(0.650212310040393,2.66588895539464,
7.51608817408573));
#381457=CARTESIAN_POINT('Ctrl Pts',(0.650255795434424,2.66626391779724,
7.51481005913119));
#381458=CARTESIAN_POINT('Ctrl Pts',(0.650295185543453,2.66660356770153,
7.51365231206383));
#381459=CARTESIAN_POINT('Ctrl Pts',(0.650401124727213,2.66692179482435,
7.51247773061042));
#381460=CARTESIAN_POINT('Ctrl Pts',(0.65060681453073,2.66720142950121,7.51129758471022));
#381461=CARTESIAN_POINT('Ctrl Pts',(0.650862463465839,2.66754898346906,
7.50983079813402));
#381462=CARTESIAN_POINT('Ctrl Pts',(0.651274536664403,2.66781811159763,
7.50839324291155));
#381463=CARTESIAN_POINT('Ctrl Pts',(0.651891120888244,2.66794175530204,
7.50715379678855));
#381464=CARTESIAN_POINT('Ctrl Pts',(0.652175965033211,2.66799887513076,
7.50658120839351));
#381465=CARTESIAN_POINT('Ctrl Pts',(0.652546816749126,2.66802374990068,
7.50598221009429));
#381466=CARTESIAN_POINT('Ctrl Pts',(0.652996372582791,2.66799309213236,
7.50545747549611));
#381467=CARTESIAN_POINT('Ctrl Pts',(0.653236269490689,2.66797673219823,
7.50517746087247));
#381468=CARTESIAN_POINT('Ctrl Pts',(0.653501193456964,2.66794458333831,
7.50491486231392));
#381469=CARTESIAN_POINT('Ctrl Pts',(0.653783927906854,2.66789584104001,
7.50468370960993));
#381470=CARTESIAN_POINT('Ctrl Pts',(0.654206705092963,2.66782295592915,
7.50433806340447));
#381471=CARTESIAN_POINT('Ctrl Pts',(0.654681888865027,2.6677102342832,7.50405484070984));
#381472=CARTESIAN_POINT('Ctrl Pts',(0.655177311127163,2.66756457064415,
7.50385766036131));
#381473=CARTESIAN_POINT('Ctrl Pts',(0.655230288837496,2.66754899418208,
7.50383657498791));
#381474=CARTESIAN_POINT('Ctrl Pts',(0.655283478613807,2.66753306175527,
7.50381643264937));
#381475=CARTESIAN_POINT('Ctrl Pts',(0.655336827290465,2.66751679707099,
7.50379723213559));
#381476=CARTESIAN_POINT('Ctrl Pts',(0.655692947158707,2.66740822498289,
7.50366906242519));
#381477=CARTESIAN_POINT('Ctrl Pts',(0.656063684366623,2.66728179801425,
7.50358235568538));
#381478=CARTESIAN_POINT('Ctrl Pts',(0.656418100142797,2.66715134813715,
7.5035341175365));
#381479=CARTESIAN_POINT('Ctrl Pts',(0.656949506487048,2.66695575331052,
7.50346178989176));
#381480=CARTESIAN_POINT('Ctrl Pts',(0.657512862320731,2.66672274300315,
7.50346967198527));
#381481=CARTESIAN_POINT('Ctrl Pts',(0.658058864751397,2.66647698198924,
7.50354272648692));
#381482=CARTESIAN_POINT('Ctrl Pts',(0.658283446852712,2.66637589539727,
7.50357277531559));
#381483=CARTESIAN_POINT('Ctrl Pts',(0.658504852827741,2.66627291519396,
7.50361331098761));
#381484=CARTESIAN_POINT('Ctrl Pts',(0.658718750144193,2.66617077539188,
7.50366116523658));
#381485=CARTESIAN_POINT('',(0.678263889302254,2.58651417133801,7.57603338622103));
#381486=CARTESIAN_POINT('Origin',(0.680508179114277,2.59506137280035,7.58486873427628));
#381487=CARTESIAN_POINT('Ctrl Pts',(0.658718750125042,2.66617077544467,
7.50366116529969));
#381488=CARTESIAN_POINT('Ctrl Pts',(0.665223977061721,2.63966210099077,
7.52783573079709));
#381489=CARTESIAN_POINT('Ctrl Pts',(0.671738733243894,2.61311115757656,
7.55196141284069));
#381490=CARTESIAN_POINT('Ctrl Pts',(0.678263888672591,2.58651417242021,
7.57603338728831));
#381491=CARTESIAN_POINT('Ctrl Pts',(0.67077076127836,2.58307524303169,7.59639677331372));
#381492=CARTESIAN_POINT('Ctrl Pts',(0.672289956972022,2.5648608542088,7.59959882295464));
#381493=CARTESIAN_POINT('Ctrl Pts',(0.683001371747239,2.57969238838817,
7.59642833564546));
#381494=CARTESIAN_POINT('Ctrl Pts',(0.670465937779987,2.57918651744114,
7.58707626057422));
#381495=CARTESIAN_POINT('Ctrl Pts',(0.674898289962463,2.57406142766957,
7.58809943920599));
#381496=CARTESIAN_POINT('Ctrl Pts',(0.681297243148316,2.57624495667518,
7.58710240504253));
#381497=CARTESIAN_POINT('Ctrl Pts',(0.675135748308881,2.58307476921871,
7.58015376756929));
#381498=CARTESIAN_POINT('Ctrl Pts',(0.676704490972113,2.5806939462827,7.5820588065976));
#381499=CARTESIAN_POINT('Ctrl Pts',(0.67922699388854,2.58194456775798,7.58020924244128));
#381500=CARTESIAN_POINT('Ctrl Pts',(0.678263889092142,2.58651417053755,
7.57603338509286));
#381501=CARTESIAN_POINT('Ctrl Pts',(0.678263889092142,2.58651417053755,
7.57603338509286));
#381502=CARTESIAN_POINT('Ctrl Pts',(0.678263889092142,2.58651417053755,
7.57603338509286));
#381503=CARTESIAN_POINT('Origin',(0.680502659389257,2.59506282024303,7.58486873427621));
#381504=CARTESIAN_POINT('Ctrl Pts',(0.747020829444758,2.64752498744625,
7.51098857897448));
#381505=CARTESIAN_POINT('Ctrl Pts',(0.742986830895846,2.64323693804364,
7.50433767179956));
#381506=CARTESIAN_POINT('Ctrl Pts',(0.735550410854283,2.64757372349463,
7.50214974420965));
#381507=CARTESIAN_POINT('Ctrl Pts',(0.725436098627537,2.62458090579523,
7.53887321589168));
#381508=CARTESIAN_POINT('Ctrl Pts',(0.721450434540296,2.62034423483437,
7.53220407452061));
#381509=CARTESIAN_POINT('Ctrl Pts',(0.714010955012692,2.62461706343849,
7.53003438070911));
#381510=CARTESIAN_POINT('Ctrl Pts',(0.703809917164866,2.60159276304372,
7.56669465659231));
#381511=CARTESIAN_POINT('Ctrl Pts',(0.699847807611444,2.59738113002056,
7.56004085833304));
#381512=CARTESIAN_POINT('Ctrl Pts',(0.692431608525831,2.60161629722504,
7.55785582193789));
#381513=CARTESIAN_POINT('Ctrl Pts',(0.682143263122383,2.5785615988534,7.59443891967696));
#381514=CARTESIAN_POINT('Ctrl Pts',(0.678175409003342,2.57434385948674,
7.58783901202978));
#381515=CARTESIAN_POINT('Ctrl Pts',(0.670813497415743,2.57857250415905,
7.58560008491213));
#381516=CARTESIAN_POINT('',(0.734382828366872,2.64632931751461,7.50366116523517));
#381517=CARTESIAN_POINT('Ctrl Pts',(0.734382828366971,2.64632931751497,
7.50366116523554));
#381518=CARTESIAN_POINT('Ctrl Pts',(0.73513881439088,2.64627810571536,7.50350835821027));
#381519=CARTESIAN_POINT('Ctrl Pts',(0.735832082908374,2.64620643442547,
7.50345484956));
#381520=CARTESIAN_POINT('Ctrl Pts',(0.736483307107726,2.64611277011765,
7.50349758195598));
#381521=CARTESIAN_POINT('Ctrl Pts',(0.73681743341804,2.64606471338142,7.50351950684424));
#381522=CARTESIAN_POINT('Ctrl Pts',(0.737173443029245,2.64600625855207,
7.50357029184312));
#381523=CARTESIAN_POINT('Ctrl Pts',(0.737515189580167,2.64594045470857,
7.50365515313924));
#381524=CARTESIAN_POINT('Ctrl Pts',(0.738040934162335,2.64583922175066,
7.50378570417639));
#381525=CARTESIAN_POINT('Ctrl Pts',(0.738548420846329,2.64571796522779,
7.50400001621911));
#381526=CARTESIAN_POINT('Ctrl Pts',(0.738998494895536,2.64558370626699,
7.50428903009635));
#381527=CARTESIAN_POINT('Ctrl Pts',(0.739048449652331,2.64556880455527,
7.50432110841318));
#381528=CARTESIAN_POINT('Ctrl Pts',(0.739097725961639,2.64555375201862,
7.50435406373354));
#381529=CARTESIAN_POINT('Ctrl Pts',(0.739146291662892,2.64553856487362,
7.50438785222351));
#381530=CARTESIAN_POINT('Ctrl Pts',(0.739442808612704,2.6454458400535,7.50459414719561));
#381531=CARTESIAN_POINT('Ctrl Pts',(0.739717403222036,2.64534612893594,
7.50483629897752));
#381532=CARTESIAN_POINT('Ctrl Pts',(0.739960005034007,2.64524448842675,
7.5050991045531));
#381533=CARTESIAN_POINT('Ctrl Pts',(0.74049520899826,2.64502025925467,7.50567888004914));
#381534=CARTESIAN_POINT('Ctrl Pts',(0.740895999024166,2.64477828392327,
7.50637912803144));
#381535=CARTESIAN_POINT('Ctrl Pts',(0.741184705006676,2.64453993517567,
7.50710440483569));
#381536=CARTESIAN_POINT('Ctrl Pts',(0.741255501445204,2.64448148733087,
7.50728225710685));
#381537=CARTESIAN_POINT('Ctrl Pts',(0.741321060218732,2.64442220659313,
7.50746498566954));
#381538=CARTESIAN_POINT('Ctrl Pts',(0.741380130382219,2.64436378576598,
7.50764697238949));
#381539=CARTESIAN_POINT('Ctrl Pts',(0.741697675324574,2.64404973147709,
7.50862528291182));
#381540=CARTESIAN_POINT('Ctrl Pts',(0.741859446188464,2.64373496099275,
7.50965856837422));
#381541=CARTESIAN_POINT('Ctrl Pts',(0.741930383748696,2.64343281940981,
7.51067959873203));
#381542=CARTESIAN_POINT('Ctrl Pts',(0.741969420777567,2.64326655051562,
7.51124147302579));
#381543=CARTESIAN_POINT('Ctrl Pts',(0.741980537241439,2.64310396618176,
7.51180065547253));
#381544=CARTESIAN_POINT('Ctrl Pts',(0.741971890422245,2.64294676648674,
7.51235175716501));
#381545=CARTESIAN_POINT('Ctrl Pts',(0.741942012217447,2.64240357891953,
7.51425603304535));
#381546=CARTESIAN_POINT('Ctrl Pts',(0.74166654701423,2.64186025088833,7.51626900505179));
#381547=CARTESIAN_POINT('Ctrl Pts',(0.741200952461279,2.64134059660317,
7.51827788969242));
#381548=CARTESIAN_POINT('Ctrl Pts',(0.74117575360422,2.64131247193124,7.51838661432544));
#381549=CARTESIAN_POINT('Ctrl Pts',(0.741149987931383,2.64128441543339,
7.51849533314856));
#381550=CARTESIAN_POINT('Ctrl Pts',(0.741123661092985,2.64125643059842,
7.51860402984325));
#381551=CARTESIAN_POINT('Ctrl Pts',(0.678263890382482,2.58651417197306,
7.57603338728985));
#381552=CARTESIAN_POINT('Ctrl Pts',(0.697000987805591,2.60648661431919,
7.55196141284922));
#381553=CARTESIAN_POINT('Ctrl Pts',(0.715706430690848,2.62642404273906,
7.52783573083105));
#381554=CARTESIAN_POINT('Ctrl Pts',(0.734382828411158,2.64632931755387,
7.50366116530176));
#381555=CARTESIAN_POINT('Origin',(2.34371526914277E-16,8.93760209386499E-16,
7.49482233047033));
#381556=CARTESIAN_POINT('Origin',(0.656598725434842,2.65758995402928,7.49482233047033));
#381557=CARTESIAN_POINT('Origin',(0.,0.,7.50366116523517));
#381558=CARTESIAN_POINT('Origin',(0.732019285896476,2.63781235403044,7.49482233047033));
#381559=CARTESIAN_POINT('Ctrl Pts',(0.65035623525909,2.66505749215232,7.51860402984325));
#381560=CARTESIAN_POINT('Ctrl Pts',(0.648533655213662,2.6724449469243,7.51860402984325));
#381561=CARTESIAN_POINT('Ctrl Pts',(0.641134372651965,2.67421889833353,
7.51860402984325));
#381562=CARTESIAN_POINT('Ctrl Pts',(0.649679497616552,2.6678005042194,7.51041458714366));
#381563=CARTESIAN_POINT('Ctrl Pts',(0.646780678116749,2.67286520670502,
7.51004642900441));
#381564=CARTESIAN_POINT('Ctrl Pts',(0.64113233201769,2.67421938756826,7.5072913648301));
#381565=CARTESIAN_POINT('Ctrl Pts',(0.652012104546052,2.66937615713541,
7.50215815450137));
#381566=CARTESIAN_POINT('Ctrl Pts',(0.650349947137605,2.67200965238525,
7.49877163671531));
#381567=CARTESIAN_POINT('Ctrl Pts',(0.647000459287285,2.67283721189065,
7.49481588533171));
#381568=CARTESIAN_POINT('Ctrl Pts',(0.658718618100686,2.66617024094247,
7.50366171572174));
#381569=CARTESIAN_POINT('Ctrl Pts',(0.659596893131267,2.66972506797453,
7.50000045605858));
#381570=CARTESIAN_POINT('Ctrl Pts',(0.659596893131146,2.66972506797456,
7.49482233047317));
#381571=CARTESIAN_POINT('Origin',(0.638220125503548,2.66206335788656,7.51860402984325));
#381572=CARTESIAN_POINT('Origin',(0.638220125503548,2.66206335788656,9.));
#381573=CARTESIAN_POINT('Origin',(0.638220125503548,2.66206335788656,8.75721825406948));
#381574=CARTESIAN_POINT('Ctrl Pts',(0.654357526473971,2.64884485132562,
8.78942910404912));
#381575=CARTESIAN_POINT('Ctrl Pts',(0.653041919255957,2.65425979420155,
8.7967269950169));
#381576=CARTESIAN_POINT('Ctrl Pts',(0.64412876343682,2.65378110920504,8.79893251111267));
#381577=CARTESIAN_POINT('Ctrl Pts',(0.651723146255084,2.65951890676874,
8.78111911759583));
#381578=CARTESIAN_POINT('Ctrl Pts',(0.650156245245669,2.6659366268742,8.78644465894814));
#381579=CARTESIAN_POINT('Ctrl Pts',(0.642156520060452,2.66724807978472,
8.78817647674132));
#381580=CARTESIAN_POINT('Ctrl Pts',(0.650081337635878,2.66617123271352,
8.76780923932029));
#381581=CARTESIAN_POINT('Ctrl Pts',(0.648226726776164,2.67374587167056,
8.76988516158373));
#381582=CARTESIAN_POINT('Ctrl Pts',(0.640913636083721,2.67565769930935,
8.77093053738833));
#381583=CARTESIAN_POINT('Ctrl Pts',(0.650401467845208,2.66487412019735,
8.75371302330493));
#381584=CARTESIAN_POINT('Ctrl Pts',(0.648593115387865,2.67226303505393,
8.75300828287559));
#381585=CARTESIAN_POINT('Ctrl Pts',(0.641155596302533,2.67401741505541,
8.75267964240738));
#381586=CARTESIAN_POINT('Origin',(0.641580116759656,2.64844927545894,8.78727029226991));
#381587=CARTESIAN_POINT('Ctrl Pts',(0.670846486662589,2.58203466569848,
8.85049129520029));
#381588=CARTESIAN_POINT('Ctrl Pts',(0.669447239426409,2.58770416474117,
8.85711686593484));
#381589=CARTESIAN_POINT('Ctrl Pts',(0.660897934588157,2.58760342300926,
8.85933012996512));
#381590=CARTESIAN_POINT('Ctrl Pts',(0.665128007518924,2.60520491838319,
8.82945683644722));
#381591=CARTESIAN_POINT('Ctrl Pts',(0.663717145684686,2.6109214776958,8.83607469902388));
#381592=CARTESIAN_POINT('Ctrl Pts',(0.655143182195917,2.61078294036945,
8.8382956714852));
#381593=CARTESIAN_POINT('Ctrl Pts',(0.659418052229554,2.62834063393786,
8.80838214965002));
#381594=CARTESIAN_POINT('Ctrl Pts',(0.658001622475789,2.63407975346251,
8.81501364461989));
#381595=CARTESIAN_POINT('Ctrl Pts',(0.649397808304859,2.63392745668916,
8.81722098428721));
#381596=CARTESIAN_POINT('Ctrl Pts',(0.653715973115229,2.65144443664273,
8.78727029226991));
#381597=CARTESIAN_POINT('Ctrl Pts',(0.652299308087835,2.65718450945399,
8.79393457792714));
#381598=CARTESIAN_POINT('Ctrl Pts',(0.643661112117155,2.6570396455512,8.79610912703474));
#381599=CARTESIAN_POINT('Origin',(0.658710630307015,2.57903950451469,8.85049129520029));
#381600=CARTESIAN_POINT('Ctrl Pts',(0.682528638916215,2.57897124462359,
8.85049129520029));
#381601=CARTESIAN_POINT('Ctrl Pts',(0.686529951896112,2.58322455000412,
8.85711686593484));
#381602=CARTESIAN_POINT('Ctrl Pts',(0.693929685372865,2.57894147790726,
8.85933012996512));
#381603=CARTESIAN_POINT('Ctrl Pts',(0.678988735082457,2.57520840675055,
8.86332496987231));
#381604=CARTESIAN_POINT('Ctrl Pts',(0.683521675092151,2.574311551553,8.86648636486737));
#381605=CARTESIAN_POINT('Ctrl Pts',(0.684014181433137,2.56842652484136,
8.87206031107457));
#381606=CARTESIAN_POINT('Ctrl Pts',(0.672092792372933,2.57698485830991,
8.86341338519876));
#381607=CARTESIAN_POINT('Ctrl Pts',(0.667681419262718,2.57840375151122,
8.86654584966056));
#381608=CARTESIAN_POINT('Ctrl Pts',(0.66440196045203,2.57346722411881,8.87215952290714));
#381609=CARTESIAN_POINT('Ctrl Pts',(0.670846486662589,2.58203466569848,
8.85049129520029));
#381610=CARTESIAN_POINT('Ctrl Pts',(0.669447239426409,2.58770416474117,
8.85711686593484));
#381611=CARTESIAN_POINT('Ctrl Pts',(0.660897934588157,2.58760342300926,
8.85933012996512));
#381612=CARTESIAN_POINT('Origin',(0.691633059385415,2.57040622694002,8.85049129520029));
#381613=CARTESIAN_POINT('Ctrl Pts',(0.731515368664185,2.63104303262371,
8.78727029226991));
#381614=CARTESIAN_POINT('Ctrl Pts',(0.735566489878297,2.63534928303294,
8.79393457792714));
#381615=CARTESIAN_POINT('Ctrl Pts',(0.743022024337685,2.63098414602443,
8.79610912703474));
#381616=CARTESIAN_POINT('Ctrl Pts',(0.715209598974175,2.61371036749491,
8.80838214965003));
#381617=CARTESIAN_POINT('Ctrl Pts',(0.719260047395476,2.61801590274056,
8.81501364461988));
#381618=CARTESIAN_POINT('Ctrl Pts',(0.726681976909626,2.61366116108552,
8.81722098428721));
#381619=CARTESIAN_POINT('Ctrl Pts',(0.698881306429992,2.59635376108049,
8.82945683644723));
#381620=CARTESIAN_POINT('Ctrl Pts',(0.702915832726861,2.60064237146729,
8.83607469902389));
#381621=CARTESIAN_POINT('Ctrl Pts',(0.710318504785448,2.59631426692943,
8.8382956714852));
#381622=CARTESIAN_POINT('Ctrl Pts',(0.682528638916215,2.57897124462359,
8.85049129520029));
#381623=CARTESIAN_POINT('Ctrl Pts',(0.686529951896112,2.58322455000412,
8.85711686593484));
#381624=CARTESIAN_POINT('Ctrl Pts',(0.693929685372865,2.57894147790726,
8.85933012996512));
#381625=CARTESIAN_POINT('Origin',(0.740619789133384,2.62247801494013,8.78727029226991));
#381626=CARTESIAN_POINT('Ctrl Pts',(0.740996801860814,2.64112155517596,
8.75374538247849));
#381627=CARTESIAN_POINT('Ctrl Pts',(0.7461940627041,2.64666527758192,8.75304829418602));
#381628=CARTESIAN_POINT('Ctrl Pts',(0.753529191928262,2.64455186269746,
8.75272238421917));
#381629=CARTESIAN_POINT('Ctrl Pts',(0.741901256234672,2.64208297038269,
8.76769408445017));
#381630=CARTESIAN_POINT('Ctrl Pts',(0.747229806678867,2.64776572544832,
8.76974318093968));
#381631=CARTESIAN_POINT('Ctrl Pts',(0.754533288360377,2.64584804126992,
8.77077869880429));
#381632=CARTESIAN_POINT('Ctrl Pts',(0.737265538337212,2.63715530372528,
8.78108014887992));
#381633=CARTESIAN_POINT('Ctrl Pts',(0.741778521319331,2.64197383274391,
8.78639403366327));
#381634=CARTESIAN_POINT('Ctrl Pts',(0.749387942947455,2.63921361930754,
8.78812224174741));
#381635=CARTESIAN_POINT('Ctrl Pts',(0.729668620074102,2.62907994584327,
8.78944554828685));
#381636=CARTESIAN_POINT('Ctrl Pts',(0.733467909200717,2.63314464998372,
8.79673892988685));
#381637=CARTESIAN_POINT('Ctrl Pts',(0.740992567286079,2.62836102426519,
8.79894799272499));
#381638=CARTESIAN_POINT('Origin',(0.750228081562181,2.63269141291484,8.75721825406948));
#381639=CARTESIAN_POINT('Origin',(0.750228081562181,2.63269141291484,9.));
#381640=CARTESIAN_POINT('Origin',(0.750228081562181,2.63269141291484,7.51860402984325));
#381641=CARTESIAN_POINT('Ctrl Pts',(0.734382618009651,2.64632855949765,
7.50366195182966));
#381642=CARTESIAN_POINT('Ctrl Pts',(0.735361839713489,2.64985715929995,
7.50000065167735));
#381643=CARTESIAN_POINT('Ctrl Pts',(0.735361839713602,2.64985715929992,
7.49482233047108));
#381644=CARTESIAN_POINT('Ctrl Pts',(0.741805881174924,2.64582959698829,
7.50215800491337));
#381645=CARTESIAN_POINT('Ctrl Pts',(0.744548032294523,2.6473078745034,7.49877273257265));
#381646=CARTESIAN_POINT('Ctrl Pts',(0.747874451006687,2.64638478463708,
7.49481816995647));
#381647=CARTESIAN_POINT('Ctrl Pts',(0.743054712745831,2.64330958983561,
7.51043025814041));
#381648=CARTESIAN_POINT('Ctrl Pts',(0.74806676363693,2.64630493670232,7.51006209594514));
#381649=CARTESIAN_POINT('Ctrl Pts',(0.753656215494924,2.64471214101881,
7.50731281821699));
#381650=CARTESIAN_POINT('Ctrl Pts',(0.741122625541025,2.6412553296967,7.51860402984325));
#381651=CARTESIAN_POINT('Ctrl Pts',(0.746335839181183,2.64679820087802,
7.51860402984325));
#381652=CARTESIAN_POINT('Ctrl Pts',(0.753653780564754,2.64471283489162,
7.51860402984325));
#381653=CARTESIAN_POINT('Origin',(0.,0.,7.5));
#381654=CARTESIAN_POINT('Origin',(0.846361565593563,2.52994271156922,7.5));
#381655=CARTESIAN_POINT('',(0.846361565593563,2.52994271156922,7.59394543036555));
#381656=CARTESIAN_POINT('',(0.846361565593563,2.52994271156922,8.85049129520029));
#381657=CARTESIAN_POINT('',(0.846361565593563,2.52994271156922,7.5));
#381658=CARTESIAN_POINT('',(0.898583897763412,2.57876892194512,8.78727029226991));
#381659=CARTESIAN_POINT('Ctrl Pts',(0.846361565593563,2.52994271156922,
8.85049129520029));
#381660=CARTESIAN_POINT('Ctrl Pts',(0.863794313055935,2.54624177290297,
8.82945686509571));
#381661=CARTESIAN_POINT('Ctrl Pts',(0.881201144631272,2.56251660371119,
8.80838212259896));
#381662=CARTESIAN_POINT('Ctrl Pts',(0.898583897763412,2.57876892194512,
8.78727029226991));
#381663=CARTESIAN_POINT('',(0.908826823579918,2.58834572998875,8.75721825406948));
#381664=CARTESIAN_POINT('Origin',(0.878002168680578,2.55952593977649,8.75937679713143));
#381665=CARTESIAN_POINT('',(0.908826823579918,2.58834572998875,7.51860402984325));
#381666=CARTESIAN_POINT('',(0.908826823579918,2.58834572998875,7.5));
#381667=CARTESIAN_POINT('Ctrl Pts',(0.908826823579918,2.58834572998875,
7.51860402984325));
#381668=CARTESIAN_POINT('Ctrl Pts',(0.900782598427349,2.58082463674587,
7.52834476460825));
#381669=CARTESIAN_POINT('Ctrl Pts',(0.892733151079883,2.57329866091778,
7.53807742314407));
#381670=CARTESIAN_POINT('Ctrl Pts',(0.884678306195387,2.56576763856519,
7.54780169004674));
#381671=CARTESIAN_POINT('Ctrl Pts',(0.871919867225566,2.55383890617572,
7.5632044032688));
#381672=CARTESIAN_POINT('Ctrl Pts',(0.859147870308693,2.54189749753934,
7.57858609112102));
#381673=CARTESIAN_POINT('Ctrl Pts',(0.846361565593563,2.52994271156922,
7.59394543036555));
#381674=CARTESIAN_POINT('Origin',(0.786247562650672,2.80441041318874,7.5));
#381675=CARTESIAN_POINT('',(0.819770641322243,2.6179144196928,8.75721825406948));
#381676=CARTESIAN_POINT('',(0.822251471859985,2.60411303347873,8.78727029226991));
#381677=CARTESIAN_POINT('Origin',(0.828548745068344,2.56907996760748,8.75658640621073));
#381678=CARTESIAN_POINT('',(0.83489968963681,2.53374831658169,8.85049129520029));
#381679=CARTESIAN_POINT('Ctrl Pts',(0.822251471859985,2.60411303347873,
8.78727029226991));
#381680=CARTESIAN_POINT('Ctrl Pts',(0.826461564325047,2.58069139656185,
8.80838212259895));
#381681=CARTESIAN_POINT('Ctrl Pts',(0.830677488574718,2.55723731619086,
8.82945686509571));
#381682=CARTESIAN_POINT('Ctrl Pts',(0.834899689636811,2.53374831658169,
8.85049129520029));
#381683=CARTESIAN_POINT('',(0.83489968963681,2.53374831658169,7.59394543036555));
#381684=CARTESIAN_POINT('',(0.83489968963681,2.53374831658169,7.5));
#381685=CARTESIAN_POINT('',(0.819770641322243,2.6179144196928,7.51860402984325));
#381686=CARTESIAN_POINT('Ctrl Pts',(0.834899689636811,2.53374831658169,
7.59394543036555));
#381687=CARTESIAN_POINT('Ctrl Pts',(0.831802854243252,2.55097666840085,
7.57858609112103));
#381688=CARTESIAN_POINT('Ctrl Pts',(0.828709484189966,2.56818574179751,
7.56320440326857));
#381689=CARTESIAN_POINT('Ctrl Pts',(0.825619397863336,2.58537654712653,
7.54780169004651));
#381690=CARTESIAN_POINT('Ctrl Pts',(0.823668519225315,2.59622969857338,
7.53807742314383));
#381691=CARTESIAN_POINT('Ctrl Pts',(0.82171894786751,2.60707557734321,7.52834476460825));
#381692=CARTESIAN_POINT('Ctrl Pts',(0.819770641322244,2.6179144196928,7.51860402984325));
#381693=CARTESIAN_POINT('',(0.819770641322243,2.6179144196928,7.5));
#381694=CARTESIAN_POINT('Origin',(0.841666242051987,2.53496461975634,7.5));
#381695=CARTESIAN_POINT('Ctrl Pts',(0.83489968963681,2.53374831658169,8.85049129520029));
#381696=CARTESIAN_POINT('Ctrl Pts',(0.83493395161564,2.53355770992997,8.85097269580138));
#381697=CARTESIAN_POINT('Ctrl Pts',(0.83497606004542,2.53337099625431,8.85143669361005));
#381698=CARTESIAN_POINT('Ctrl Pts',(0.835028806748958,2.53317977033515,
8.8519052845931));
#381699=CARTESIAN_POINT('Ctrl Pts',(0.835131975956005,2.53280574456439,
8.85282181883899));
#381700=CARTESIAN_POINT('Ctrl Pts',(0.835273379657592,2.53242413033,8.85372622499635));
#381701=CARTESIAN_POINT('Ctrl Pts',(0.835469694820074,2.53203429676771,
8.85462257735071));
#381702=CARTESIAN_POINT('Ctrl Pts',(0.835632668695512,2.53171067078987,
8.85536669723986));
#381703=CARTESIAN_POINT('Ctrl Pts',(0.835833495004543,2.53138129226441,
8.85610498449051));
#381704=CARTESIAN_POINT('Ctrl Pts',(0.836088564940264,2.53104993826304,
8.85681338218371));
#381705=CARTESIAN_POINT('Ctrl Pts',(0.836320041307526,2.53074923398639,
8.85745625420284));
#381706=CARTESIAN_POINT('Ctrl Pts',(0.836598619887871,2.53044276569274,
8.85808743050666));
#381707=CARTESIAN_POINT('Ctrl Pts',(0.83695169313415,2.53013874920071,8.85866804508411));
#381708=CARTESIAN_POINT('Ctrl Pts',(0.837114593476293,2.52999848258155,
8.85893592806396));
#381709=CARTESIAN_POINT('Ctrl Pts',(0.837293573677378,2.52985883470932,
8.85919241173848));
#381710=CARTESIAN_POINT('Ctrl Pts',(0.837492683868179,2.52972144827001,
8.85943017985534));
#381711=CARTESIAN_POINT('Ctrl Pts',(0.837761541568687,2.52953593590619,
8.8597512372));
#381712=CARTESIAN_POINT('Ctrl Pts',(0.838074309181975,2.52935035226354,
8.86004599534706));
#381713=CARTESIAN_POINT('Ctrl Pts',(0.838432543645287,2.52917588406184,
8.86026130871721));
#381714=CARTESIAN_POINT('Ctrl Pts',(0.838563703382005,2.52911200633442,
8.86034014101235));
#381715=CARTESIAN_POINT('Ctrl Pts',(0.838702922709042,2.52904864803639,
8.86040910639693));
#381716=CARTESIAN_POINT('Ctrl Pts',(0.838846548008413,2.52898784149328,
8.86046313645507));
#381717=CARTESIAN_POINT('Ctrl Pts',(0.839070674085231,2.528892953392,8.8605474499083));
#381718=CARTESIAN_POINT('Ctrl Pts',(0.839311704589184,2.52880182440186,
8.86059655985668));
#381719=CARTESIAN_POINT('Ctrl Pts',(0.839554077896298,2.52872002487639,
8.86059725258816));
#381720=CARTESIAN_POINT('Ctrl Pts',(0.839797011182579,2.52863803636134,
8.86059794692011));
#381721=CARTESIAN_POINT('Ctrl Pts',(0.840044837205558,2.5285670284827,8.86056369958366));
#381722=CARTESIAN_POINT('Ctrl Pts',(0.840283002906171,2.52850725650911,
8.86048590497774));
#381723=CARTESIAN_POINT('Ctrl Pts',(0.840345157062984,2.52849165780363,
8.86046560290182));
#381724=CARTESIAN_POINT('Ctrl Pts',(0.840407483937885,2.52847670924879,
8.86044257503091));
#381725=CARTESIAN_POINT('Ctrl Pts',(0.840468049922893,2.52846284084641,
8.86041778462583));
#381726=CARTESIAN_POINT('Ctrl Pts',(0.840875583845876,2.52836952370761,
8.860250975962));
#381727=CARTESIAN_POINT('Ctrl Pts',(0.841258151095091,2.52831291335483,
8.8599848982295));
#381728=CARTESIAN_POINT('Ctrl Pts',(0.841603345326615,2.5282862808699,8.85968173251461));
#381729=CARTESIAN_POINT('Ctrl Pts',(0.841785933297819,2.52827219381124,
8.85952137522076));
#381730=CARTESIAN_POINT('Ctrl Pts',(0.841961569857936,2.52826603203966,
8.85934740853961));
#381731=CARTESIAN_POINT('Ctrl Pts',(0.842127723639154,2.52826632885327,
8.85916759001821));
#381732=CARTESIAN_POINT('Ctrl Pts',(0.842794917435776,2.52826752071418,
8.85844552518694));
#381733=CARTESIAN_POINT('Ctrl Pts',(0.843346920779412,2.52836989484405,
8.8575944418412));
#381734=CARTESIAN_POINT('Ctrl Pts',(0.843789497269782,2.52849379119464,
8.85683498915133));
#381735=CARTESIAN_POINT('Ctrl Pts',(0.84383581172081,2.52850675661776,8.85675551444995));
#381736=CARTESIAN_POINT('Ctrl Pts',(0.843880918787578,2.52851997553546,
8.85667699793649));
#381737=CARTESIAN_POINT('Ctrl Pts',(0.843924818530538,2.52853336804472,
8.85659965593547));
#381738=CARTESIAN_POINT('Ctrl Pts',(0.844517379501221,2.5287141408181,8.85555568965886));
#381739=CARTESIAN_POINT('Ctrl Pts',(0.845060760140805,2.5289734521824,8.85434650606345));
#381740=CARTESIAN_POINT('Ctrl Pts',(0.8455603232407,2.52930697522583,8.85297329937117));
#381741=CARTESIAN_POINT('Ctrl Pts',(0.845841297045563,2.52949456161591,
8.85220095427747));
#381742=CARTESIAN_POINT('Ctrl Pts',(0.846108349539856,2.52970596265749,
8.85137579139183));
#381743=CARTESIAN_POINT('Ctrl Pts',(0.846361565593563,2.52994271156922,
8.85049129520029));
#381744=CARTESIAN_POINT('Origin',(0.841666242051987,2.53496461975634,7.59394543036555));
#381745=CARTESIAN_POINT('Ctrl Pts',(0.834999163719523,2.5331949211712,7.59443877723642));
#381746=CARTESIAN_POINT('Ctrl Pts',(0.836023651060061,2.52749548090589,
7.58783886950016));
#381747=CARTESIAN_POINT('Ctrl Pts',(0.844500455058551,2.52702327808101,
7.58559994247159));
#381748=CARTESIAN_POINT('Ctrl Pts',(0.829406517384706,2.56430799836501,
7.56670252222135));
#381749=CARTESIAN_POINT('Ctrl Pts',(0.830429524050183,2.55861679540903,
7.5600487499903));
#381750=CARTESIAN_POINT('Ctrl Pts',(0.838955367733707,2.55812046211334,
7.55786368756704));
#381751=CARTESIAN_POINT('Ctrl Pts',(0.823824314758139,2.59536297499579,
7.53888913333561));
#381752=CARTESIAN_POINT('Ctrl Pts',(0.824853401202298,2.58963794894194,
7.53222002137279));
#381753=CARTESIAN_POINT('Ctrl Pts',(0.833419290574609,2.58916047226025,
7.53005029815327));
#381754=CARTESIAN_POINT('Ctrl Pts',(0.818252808438286,2.62635844580471,
7.51101258149734));
#381755=CARTESIAN_POINT('Ctrl Pts',(0.81929436928006,2.62056402203247,7.5043616886572));
#381756=CARTESIAN_POINT('Ctrl Pts',(0.827892578463753,2.62014178942108,
7.50217374673251));
#381757=CARTESIAN_POINT('',(0.828187489909737,2.61848858635941,7.50366116523517));
#381758=CARTESIAN_POINT('Ctrl Pts',(0.819770641322243,2.6179144196928,7.51860402984325));
#381759=CARTESIAN_POINT('Ctrl Pts',(0.819692512867909,2.61834906484739,
7.51734760759493));
#381760=CARTESIAN_POINT('Ctrl Pts',(0.819680470930653,2.61875235488163,
7.51608817408572));
#381761=CARTESIAN_POINT('Ctrl Pts',(0.819747890902897,2.619123760765,7.51481005913119));
#381762=CARTESIAN_POINT('Ctrl Pts',(0.819808961524808,2.61946018908918,
7.51365231206383));
#381763=CARTESIAN_POINT('Ctrl Pts',(0.819935071926916,2.61977097483344,
7.51247773061042));
#381764=CARTESIAN_POINT('Ctrl Pts',(0.820158255373932,2.62003685637991,
7.51129758471022));
#381765=CARTESIAN_POINT('Ctrl Pts',(0.820435646910061,2.62036731677735,
7.50983079813402));
#381766=CARTESIAN_POINT('Ctrl Pts',(0.820864116558444,2.62060949033284,
7.50839324291155));
#381767=CARTESIAN_POINT('Ctrl Pts',(0.82148735582321,2.62069337531113,7.50715379678855));
#381768=CARTESIAN_POINT('Ctrl Pts',(0.821775274405323,2.62073212775402,
7.50658120839351));
#381769=CARTESIAN_POINT('Ctrl Pts',(0.822146957898595,2.62073319086503,
7.50598221009429));
#381770=CARTESIAN_POINT('Ctrl Pts',(0.822593625821624,2.62067379294523,
7.50545747549611));
#381771=CARTESIAN_POINT('Ctrl Pts',(0.822831981651018,2.62064209637668,
7.50517746087247));
#381772=CARTESIAN_POINT('Ctrl Pts',(0.823094301518063,2.62059303983324,
7.50491486231392));
#381773=CARTESIAN_POINT('Ctrl Pts',(0.823373332129928,2.62052628282281,
7.50468370960993));
#381774=CARTESIAN_POINT('Ctrl Pts',(0.823790570909882,2.62042646003492,
7.50433806340447));
#381775=CARTESIAN_POINT('Ctrl Pts',(0.824257556265273,2.62028352485887,
7.50405484070984));
#381776=CARTESIAN_POINT('Ctrl Pts',(0.824742627927844,2.62010641868807,
7.50385766036131));
#381777=CARTESIAN_POINT('Ctrl Pts',(0.824794498802434,2.62008747993595,
7.50383657498791));
#381778=CARTESIAN_POINT('Ctrl Pts',(0.824846558500551,2.62006817236335,
7.50381643264937));
#381779=CARTESIAN_POINT('Ctrl Pts',(0.824898755484729,2.62004852303516,
7.50379723213559));
#381780=CARTESIAN_POINT('Ctrl Pts',(0.82524718742894,2.61991735734177,7.50366906242519));
#381781=CARTESIAN_POINT('Ctrl Pts',(0.825609062713809,2.61976743691642,
7.50358235568538));
#381782=CARTESIAN_POINT('Ctrl Pts',(0.825954392352437,2.61961454756585,
7.5035341175365));
#381783=CARTESIAN_POINT('Ctrl Pts',(0.826472175061791,2.61938530728839,
7.50346178989176));
#381784=CARTESIAN_POINT('Ctrl Pts',(0.827019444398843,2.6191166813935,7.50346967198527));
#381785=CARTESIAN_POINT('Ctrl Pts',(0.827548579046732,2.61883644282611,
7.50354272648692));
#381786=CARTESIAN_POINT('Ctrl Pts',(0.827766223079849,2.61872117490274,
7.50357277531559));
#381787=CARTESIAN_POINT('Ctrl Pts',(0.827980576188277,2.61860422075378,
7.50361331098761));
#381788=CARTESIAN_POINT('Ctrl Pts',(0.828187489910165,2.61848858636076,
7.50366116523658));
#381789=CARTESIAN_POINT('',(0.842588855338968,2.53774338397765,7.57603338622103));
#381790=CARTESIAN_POINT('Origin',(0.845376155095215,2.54612923215661,7.58486873427626));
#381791=CARTESIAN_POINT('Ctrl Pts',(0.828187489894435,2.61848858641467,
7.50366116529969));
#381792=CARTESIAN_POINT('Ctrl Pts',(0.832980934541032,2.59161758555463,
7.52783573079709));
#381793=CARTESIAN_POINT('Ctrl Pts',(0.83778118067268,2.56470379203953,7.55196141284068));
#381794=CARTESIAN_POINT('Ctrl Pts',(0.842588854779936,2.53774338509797,
7.57603338728831));
#381795=CARTESIAN_POINT('Ctrl Pts',(0.83489078985715,2.53479160767929,7.5963967733137));
#381796=CARTESIAN_POINT('Ctrl Pts',(0.83525626370703,2.51565878627385,7.59974925422225));
#381797=CARTESIAN_POINT('Ctrl Pts',(0.846992701389922,2.53077349621429,
7.59639677331373));
#381798=CARTESIAN_POINT('Ctrl Pts',(0.834337441147242,2.53093040200112,
7.5870762605742));
#381799=CARTESIAN_POINT('Ctrl Pts',(0.838503286617428,2.52543830193646,
7.58811717123965));
#381800=CARTESIAN_POINT('Ctrl Pts',(0.845126734807065,2.52734810969667,
7.58707626057426));
#381801=CARTESIAN_POINT('Ctrl Pts',(0.839246778196414,2.53451146916045,
7.58015376756929));
#381802=CARTESIAN_POINT('Ctrl Pts',(0.840681119793326,2.53199758847086,
7.58208760766041));
#381803=CARTESIAN_POINT('Ctrl Pts',(0.843334199200238,2.53315435188583,
7.58015376756931));
#381804=CARTESIAN_POINT('Ctrl Pts',(0.842588855078002,2.5377433831923,7.57603338509286));
#381805=CARTESIAN_POINT('Ctrl Pts',(0.842588855078001,2.5377433831923,7.57603338509286));
#381806=CARTESIAN_POINT('Ctrl Pts',(0.842588855078001,2.5377433831923,7.57603338509286));
#381807=CARTESIAN_POINT('Origin',(0.845370739448622,2.54613103027501,7.5848687342762));
#381808=CARTESIAN_POINT('Ctrl Pts',(0.915113503383049,2.59422357454068,
7.51098857897448));
#381809=CARTESIAN_POINT('Ctrl Pts',(0.910813056848287,2.59020279456989,
7.50433767179956));
#381810=CARTESIAN_POINT('Ctrl Pts',(0.903669774527107,2.59500712269798,
7.50214974420965));
#381811=CARTESIAN_POINT('Ctrl Pts',(0.89210308835161,2.57270957241784,7.53887321589169));
#381812=CARTESIAN_POINT('Ctrl Pts',(0.887854168798255,2.56873696852669,
7.53220407452062));
#381813=CARTESIAN_POINT('Ctrl Pts',(0.880703735547808,2.57347766723606,
7.53003438070911));
#381814=CARTESIAN_POINT('Ctrl Pts',(0.869048484835129,2.55115425547475,
7.56669465659233));
#381815=CARTESIAN_POINT('Ctrl Pts',(0.864824675606408,2.547205128934,7.56004085833301));
#381816=CARTESIAN_POINT('Ctrl Pts',(0.857695061991681,2.55190675204007,
7.55785582193789));
#381817=CARTESIAN_POINT('Ctrl Pts',(0.845950735501021,2.52955859857208,
7.59443891967696));
#381818=CARTESIAN_POINT('Ctrl Pts',(0.841720802274774,2.52560374628956,
7.58783901202978));
#381819=CARTESIAN_POINT('Ctrl Pts',(0.83464494671847,2.53029538205277,7.58560008491213));
#381820=CARTESIAN_POINT('',(0.902424861598253,2.59384008075032,7.50366116523517));
#381821=CARTESIAN_POINT('Ctrl Pts',(0.902424861598376,2.59384008075068,
7.50366116523554));
#381822=CARTESIAN_POINT('Ctrl Pts',(0.903176013216653,2.59374053798035,
7.50350835821027));
#381823=CARTESIAN_POINT('Ctrl Pts',(0.903863265344316,2.59362459608039,
7.50345484956));
#381824=CARTESIAN_POINT('Ctrl Pts',(0.904507150440901,2.59348940013823,
7.50349758195598));
#381825=CARTESIAN_POINT('Ctrl Pts',(0.904837511247212,2.59342003459351,
7.50351950684424));
#381826=CARTESIAN_POINT('Ctrl Pts',(0.905189044184713,2.59333889025177,
7.50357029184312));
#381827=CARTESIAN_POINT('Ctrl Pts',(0.905525872513966,2.59325132583263,
7.50365515313924));
#381828=CARTESIAN_POINT('Ctrl Pts',(0.906044050879611,2.59311661629766,
7.50378570417639));
#381829=CARTESIAN_POINT('Ctrl Pts',(0.906542725945682,2.59296309412584,
7.50400001621911));
#381830=CARTESIAN_POINT('Ctrl Pts',(0.906983273268325,2.59280027467114,
7.50428903009634));
#381831=CARTESIAN_POINT('Ctrl Pts',(0.907032170631776,2.59278220296433,
7.50432110841318));
#381832=CARTESIAN_POINT('Ctrl Pts',(0.907080381278296,2.59276402421074,
7.50435406373354));
#381833=CARTESIAN_POINT('Ctrl Pts',(0.907127874152393,2.59274575665419,
7.50438785222352));
#381834=CARTESIAN_POINT('Ctrl Pts',(0.907417840976708,2.59263422444096,
7.50459414719561));
#381835=CARTESIAN_POINT('Ctrl Pts',(0.907685482888729,2.59251712485356,
7.50483629897752));
#381836=CARTESIAN_POINT('Ctrl Pts',(0.907921074119476,2.59240014962424,
7.5050991045531));
#381837=CARTESIAN_POINT('Ctrl Pts',(0.908440812037402,2.59214209051931,
7.50567888004914));
#381838=CARTESIAN_POINT('Ctrl Pts',(0.908825275184502,2.59187493364706,
7.50637912803145));
#381839=CARTESIAN_POINT('Ctrl Pts',(0.909098116932917,2.59161857715672,
7.50710440483569));
#381840=CARTESIAN_POINT('Ctrl Pts',(0.909165023146295,2.5915557134559,7.50728225710685));
#381841=CARTESIAN_POINT('Ctrl Pts',(0.909226649092385,2.59149235415174,
7.50746498566955));
#381842=CARTESIAN_POINT('Ctrl Pts',(0.909281854854638,2.59143026871808,
7.50764697238949));
#381843=CARTESIAN_POINT('Ctrl Pts',(0.909578625839476,2.5910965145131,7.50862528291182));
#381844=CARTESIAN_POINT('Ctrl Pts',(0.909719896913601,2.59077202606365,
7.50965856837421));
#381845=CARTESIAN_POINT('Ctrl Pts',(0.909771330447324,2.5904659602779,7.51067959873202));
#381846=CARTESIAN_POINT('Ctrl Pts',(0.909799634385806,2.59029753188996,
7.51124147302578));
#381847=CARTESIAN_POINT('Ctrl Pts',(0.909800311195675,2.59013456936877,
7.51180065547253));
#381848=CARTESIAN_POINT('Ctrl Pts',(0.909781610323258,2.58997824666099,
7.512351757165));
#381849=CARTESIAN_POINT('Ctrl Pts',(0.909716991359514,2.58943808943404,
7.51425603304535));
#381850=CARTESIAN_POINT('Ctrl Pts',(0.90940728098262,2.58891352684472,7.51626900505179));
#381851=CARTESIAN_POINT('Ctrl Pts',(0.908909348679248,2.58842477099045,
7.51827788969242));
#381852=CARTESIAN_POINT('Ctrl Pts',(0.908882399642027,2.58839831859999,
7.51838661432544));
#381853=CARTESIAN_POINT('Ctrl Pts',(0.908854889321539,2.58837197055955,
7.51849533314856));
#381854=CARTESIAN_POINT('Ctrl Pts',(0.908826823579921,2.58834572998875,
7.51860402984325));
#381855=CARTESIAN_POINT('Ctrl Pts',(0.842588856457665,2.53774338454218,
7.57603338728985));
#381856=CARTESIAN_POINT('Ctrl Pts',(0.862567095279239,2.55647430140978,
7.55196141284922));
#381857=CARTESIAN_POINT('Ctrl Pts',(0.882511501250637,2.57517230440419,
7.52783573083105));
#381858=CARTESIAN_POINT('Ctrl Pts',(0.902424861644963,2.59384008078666,
7.50366116530176));
#381859=CARTESIAN_POINT('Origin',(2.91153398701365E-16,8.76907647894219E-16,
7.49482233047033));
#381860=CARTESIAN_POINT('Origin',(0.825522045906634,2.61006122566543,7.49482233047033));
#381861=CARTESIAN_POINT('Origin',(0.,0.,7.50366116523517));
#381862=CARTESIAN_POINT('Origin',(0.899520491555354,2.58549204896709,7.49482233047033));
#381863=CARTESIAN_POINT('Ctrl Pts',(0.819770828406711,2.61791337864929,
7.51860402984325));
#381864=CARTESIAN_POINT('Ctrl Pts',(0.818425308899797,2.62540242820759,
7.51860402984325));
#381865=CARTESIAN_POINT('Ctrl Pts',(0.811154886414717,2.62764680850482,
7.51860402984325));
#381866=CARTESIAN_POINT('Ctrl Pts',(0.819271226580787,2.62069411363351,
7.51041458714367));
#381867=CARTESIAN_POINT('Ctrl Pts',(0.816702859618942,2.62593413814772,
7.51004642900443));
#381868=CARTESIAN_POINT('Ctrl Pts',(0.811152881318522,2.62764742747825,
7.50729136483011));
#381869=CARTESIAN_POINT('Ctrl Pts',(0.821699993348124,2.62211707856253,
7.50215815450136));
#381870=CARTESIAN_POINT('Ctrl Pts',(0.820209979640308,2.62485165780475,
7.49877163671529));
#381871=CARTESIAN_POINT('Ctrl Pts',(0.816920395591568,2.62589211942377,
7.49481588533168));
#381872=CARTESIAN_POINT('Ctrl Pts',(0.828187323895664,2.61848806146949,
7.50366171572174));
#381873=CARTESIAN_POINT('Ctrl Pts',(0.829291552965938,2.62197931345374,
7.50000045605858));
#381874=CARTESIAN_POINT('Ctrl Pts',(0.829291552965819,2.62197931345378,
7.49482233047317));
#381875=CARTESIAN_POINT('Origin',(0.807467818749196,2.61570295937525,7.51860402984325));
#381876=CARTESIAN_POINT('Origin',(0.807467818749196,2.61570295937525,9.));
#381877=CARTESIAN_POINT('Origin',(0.807467818749196,2.61570295937525,8.75721825406948));
#381878=CARTESIAN_POINT('Ctrl Pts',(0.822725151075418,2.60147768482363,
8.78942910404913));
#381879=CARTESIAN_POINT('Ctrl Pts',(0.82175918349478,2.60696579336254,8.79672699501691));
#381880=CARTESIAN_POINT('Ctrl Pts',(0.812833671257172,2.60705915972975,
8.79893251111267));
#381881=CARTESIAN_POINT('Ctrl Pts',(0.820780072553557,2.61229859459517,
8.78111911759577));
#381882=CARTESIAN_POINT('Ctrl Pts',(0.819627575649247,2.61880352049876,
8.78644465894812));
#381883=CARTESIAN_POINT('Ctrl Pts',(0.811728311833866,2.62062482304101,
8.78817647674132));
#381884=CARTESIAN_POINT('Ctrl Pts',(0.819567853192906,2.61904244366226,
8.76780923932034));
#381885=CARTESIAN_POINT('Ctrl Pts',(0.818202361614361,2.62672034503694,
8.76988516158374));
#381886=CARTESIAN_POINT('Ctrl Pts',(0.81102678766845,2.62909679595021,8.77093053738833));
#381887=CARTESIAN_POINT('Ctrl Pts',(0.819804219376137,2.61772748538993,
8.75371302330491));
#381888=CARTESIAN_POINT('Ctrl Pts',(0.818472991773145,2.62521708046822,
8.75300828287559));
#381889=CARTESIAN_POINT('Ctrl Pts',(0.811163157381067,2.62744437939174,
8.75267964240737));
#381890=CARTESIAN_POINT('Origin',(0.809948649286937,2.60190157316117,8.78727029226991));
#381891=CARTESIAN_POINT('Ctrl Pts',(0.834899689636811,2.53374831658169,
8.85049129520029));
#381892=CARTESIAN_POINT('Ctrl Pts',(0.833866563354992,2.53949581710878,
8.85711686593484));
#381893=CARTESIAN_POINT('Ctrl Pts',(0.825328369435516,2.53994303820323,
8.85933012996512));
#381894=CARTESIAN_POINT('Ctrl Pts',(0.830677482908367,2.55723734771397,
8.82945683644722));
#381895=CARTESIAN_POINT('Ctrl Pts',(0.829635781053761,2.56303255597043,
8.83607469902389));
#381896=CARTESIAN_POINT('Ctrl Pts',(0.821070557575562,2.56344363901072,
8.83829567148519));
#381897=CARTESIAN_POINT('Ctrl Pts',(0.826461569719534,2.58069136655117,
8.80838214965001));
#381898=CARTESIAN_POINT('Ctrl Pts',(0.825415756823051,2.58650944540522,
8.81501364461994));
#381899=CARTESIAN_POINT('Ctrl Pts',(0.816819862423319,2.58690870980847,
8.81722098428721));
#381900=CARTESIAN_POINT('Ctrl Pts',(0.822251471859985,2.60411303347873,
8.78727029226991));
#381901=CARTESIAN_POINT('Ctrl Pts',(0.82120548525055,2.60993207873472,8.79393457792714));
#381902=CARTESIAN_POINT('Ctrl Pts',(0.812575755917816,2.61034096358643,
8.79610912703474));
#381903=CARTESIAN_POINT('Origin',(0.822596867063763,2.53153685626414,8.85049129520029));
#381904=CARTESIAN_POINT('Ctrl Pts',(0.846361565593563,2.52994271156922,
8.85049129520029));
#381905=CARTESIAN_POINT('Ctrl Pts',(0.850627167658178,2.53393091307484,
8.85711686593484));
#381906=CARTESIAN_POINT('Ctrl Pts',(0.857737280217445,2.5291825384573,8.85933012996512));
#381907=CARTESIAN_POINT('Ctrl Pts',(0.842587849021616,2.52641440726749,
8.86332496987231));
#381908=CARTESIAN_POINT('Ctrl Pts',(0.84705401391008,2.52522896829157,8.86648636486737));
#381909=CARTESIAN_POINT('Ctrl Pts',(0.847168453387979,2.51932447800885,
8.87206031107457));
#381910=CARTESIAN_POINT('Ctrl Pts',(0.835819892408161,2.52862903348297,
8.86341338519877));
#381911=CARTESIAN_POINT('Ctrl Pts',(0.831508491736653,2.53032764906163,
8.86654584966059));
#381912=CARTESIAN_POINT('Ctrl Pts',(0.827919486529833,2.52561137994158,
8.87215952290715));
#381913=CARTESIAN_POINT('Ctrl Pts',(0.83489968963681,2.53374831658169,8.85049129520029));
#381914=CARTESIAN_POINT('Ctrl Pts',(0.833866563354992,2.53949581710878,
8.85711686593484));
#381915=CARTESIAN_POINT('Ctrl Pts',(0.825328369435516,2.53994303820323,
8.85933012996512));
#381916=CARTESIAN_POINT('Origin',(0.854898517487337,2.52081196941081,8.85049129520029));
#381917=CARTESIAN_POINT('Ctrl Pts',(0.898583897763412,2.57876892194512,
8.78727029226991));
#381918=CARTESIAN_POINT('Ctrl Pts',(0.90290259792552,2.58280676847368,8.79393457792714));
#381919=CARTESIAN_POINT('Ctrl Pts',(0.910063138901376,2.57797292237443,
8.79610912703474));
#381920=CARTESIAN_POINT('Ctrl Pts',(0.881201122358356,2.56251658288673,
8.80838214965003));
#381921=CARTESIAN_POINT('Ctrl Pts',(0.885519105289311,2.5665537588271,8.81501364461989));
#381922=CARTESIAN_POINT('Ctrl Pts',(0.892646776397471,2.56173243979916,
8.81722098428722));
#381923=CARTESIAN_POINT('Ctrl Pts',(0.86379433645133,2.54624179477691,8.82945683644722));
#381924=CARTESIAN_POINT('Ctrl Pts',(0.868095345592108,2.55026310076635,
8.83607469902389));
#381925=CARTESIAN_POINT('Ctrl Pts',(0.87520550545719,2.54546959795622,8.83829567148519));
#381926=CARTESIAN_POINT('Ctrl Pts',(0.846361565593563,2.52994271156922,
8.85049129520029));
#381927=CARTESIAN_POINT('Ctrl Pts',(0.850627167658178,2.53393091307484,
8.85711686593484));
#381928=CARTESIAN_POINT('Ctrl Pts',(0.857737280217445,2.5291825384573,8.85933012996512));
#381929=CARTESIAN_POINT('Origin',(0.907120849657186,2.56963817978671,8.78727029226991));
#381930=CARTESIAN_POINT('Ctrl Pts',(0.908691583495659,2.58821925958122,
8.75374538247847));
#381931=CARTESIAN_POINT('Ctrl Pts',(0.9142333535232,2.59341860216942,8.75304829418601));
#381932=CARTESIAN_POINT('Ctrl Pts',(0.921418004981125,2.59083956617952,
8.75272238421917));
#381933=CARTESIAN_POINT('Ctrl Pts',(0.90965577765479,2.5891207508666,8.76769408445022));
#381934=CARTESIAN_POINT('Ctrl Pts',(0.915337475387768,2.59445042870331,
8.76974318093972));
#381935=CARTESIAN_POINT('Ctrl Pts',(0.922503084835704,2.5920687489348,8.77077869880429));
#381936=CARTESIAN_POINT('Ctrl Pts',(0.904713867650191,2.58450022009428,
8.78108014887987));
#381937=CARTESIAN_POINT('Ctrl Pts',(0.90952630243896,2.58901970111584,8.78639403366323));
#381938=CARTESIAN_POINT('Ctrl Pts',(0.916943242212184,2.58577762151637,
8.78812224174741));
#381939=CARTESIAN_POINT('Ctrl Pts',(0.896615168114507,2.57692819012542,
8.78944554828686));
#381940=CARTESIAN_POINT('Ctrl Pts',(0.900667077682575,2.58074112160516,
8.79673892988686));
#381941=CARTESIAN_POINT('Ctrl Pts',(0.907869787598794,2.57548521785991,
8.79894799272499));
#381942=CARTESIAN_POINT('Origin',(0.917363775473692,2.57921498783034,8.75721825406948));
#381943=CARTESIAN_POINT('Origin',(0.917363775473692,2.57921498783034,9.));
#381944=CARTESIAN_POINT('Origin',(0.917363775473692,2.57921498783034,7.51860402984325));
#381945=CARTESIAN_POINT('Ctrl Pts',(0.902424603106922,2.59383933776843,
7.50366195182966));
#381946=CARTESIAN_POINT('Ctrl Pts',(0.903627891060305,2.59729794873402,
7.50000065167735));
#381947=CARTESIAN_POINT('Ctrl Pts',(0.903627891060415,2.59729794873398,
7.49482233047108));
#381948=CARTESIAN_POINT('Ctrl Pts',(0.909800645744139,2.59286579032708,
7.50215800491337));
#381949=CARTESIAN_POINT('Ctrl Pts',(0.912631876385749,2.59416534033702,
7.49877273257265));
#381950=CARTESIAN_POINT('Ctrl Pts',(0.915892318043124,2.59303102267921,
7.49481816995647));
#381951=CARTESIAN_POINT('Ctrl Pts',(0.910885454044027,2.5902709478859,7.51043025814041));
#381952=CARTESIAN_POINT('Ctrl Pts',(0.916079119671698,2.59293901728806,
7.51006209594514));
#381953=CARTESIAN_POINT('Ctrl Pts',(0.921555036631549,2.59099137676401,
7.50731281821699));
#381954=CARTESIAN_POINT('Ctrl Pts',(0.9088257196206,2.588344697697,7.51860402984325));
#381955=CARTESIAN_POINT('Ctrl Pts',(0.91438335513013,2.59354216871027,7.51860402984325));
#381956=CARTESIAN_POINT('Ctrl Pts',(0.921552651160791,2.59099222521769,
7.51860402984325));
#381957=CARTESIAN_POINT('Origin',(0.,0.,7.5));
#381958=CARTESIAN_POINT('Origin',(1.0067166110539,2.47051810124199,7.5));
#381959=CARTESIAN_POINT('',(1.0067166110539,2.47051810124199,7.59394543036555));
#381960=CARTESIAN_POINT('',(1.0067166110539,2.47051810124199,8.85049129520029));
#381961=CARTESIAN_POINT('',(1.0067166110539,2.47051810124199,7.5));
#381962=CARTESIAN_POINT('',(1.06195995288109,2.51589809662206,8.78727029226991));
#381963=CARTESIAN_POINT('Ctrl Pts',(1.0067166110539,2.47051810124199,8.85049129520029));
#381964=CARTESIAN_POINT('Ctrl Pts',(1.02515782551208,2.48566675444138,8.82945686509571));
#381965=CARTESIAN_POINT('Ctrl Pts',(1.0435716248751,2.50079288733604,8.80838212259895));
#381966=CARTESIAN_POINT('Ctrl Pts',(1.06195995288109,2.51589809662206,8.78727029226991));
#381967=CARTESIAN_POINT('',(1.07279542170602,2.52479896157614,8.75721825406948));
#381968=CARTESIAN_POINT('Origin',(1.04018760906799,2.49801332713449,8.75937679713162));
#381969=CARTESIAN_POINT('',(1.07279542170602,2.52479896157614,7.51860402984325));
#381970=CARTESIAN_POINT('',(1.07279542170602,2.52479896157614,7.5));
#381971=CARTESIAN_POINT('Ctrl Pts',(1.07279542170602,2.52479896157614,7.51860402984325));
#381972=CARTESIAN_POINT('Ctrl Pts',(1.0642858461782,2.51780871650106,7.52834476460825));
#381973=CARTESIAN_POINT('Ctrl Pts',(1.05577074635674,2.51081393345975,7.53807742314407));
#381974=CARTESIAN_POINT('Ctrl Pts',(1.04724993675612,2.50381446008394,7.54780169004674));
#381975=CARTESIAN_POINT('Ctrl Pts',(1.03375343485922,2.49272767254592,7.5632044032688));
#381976=CARTESIAN_POINT('Ctrl Pts',(1.02024259070159,2.48162910346636,7.57858609112103));
#381977=CARTESIAN_POINT('Ctrl Pts',(1.0067166110539,2.47051810124199,7.59394543036555));
#381978=CARTESIAN_POINT('Origin',(0.964311324797623,2.74827339692444,7.5));
#381979=CARTESIAN_POINT('',(0.985816687379919,2.56001274842385,8.75721825406948));
#381980=CARTESIAN_POINT('',(0.987408162934477,2.54608077127966,8.78727029226991));
#381981=CARTESIAN_POINT('Origin',(0.99144792148259,2.51071621692061,8.75658640621085));
#381982=CARTESIAN_POINT('',(0.99552211070089,2.47505025214476,8.85049129520029));
#381983=CARTESIAN_POINT('Ctrl Pts',(0.987408162934478,2.54608077127966,
8.78727029226991));
#381984=CARTESIAN_POINT('Ctrl Pts',(0.990108975883465,2.52243751507743,
8.80838212259896));
#381985=CARTESIAN_POINT('Ctrl Pts',(0.992813529975795,2.49876150843589,
8.82945686509571));
#381986=CARTESIAN_POINT('Ctrl Pts',(0.99552211070089,2.47505025214476,8.85049129520029));
#381987=CARTESIAN_POINT('',(0.99552211070089,2.47505025214476,7.59394543036555));
#381988=CARTESIAN_POINT('',(0.99552211070089,2.47505025214476,7.5));
#381989=CARTESIAN_POINT('',(0.985816687379919,2.56001274842385,7.51860402984325));
#381990=CARTESIAN_POINT('Ctrl Pts',(0.99552211070089,2.47505025214476,7.59394543036555));
#381991=CARTESIAN_POINT('Ctrl Pts',(0.99353546237874,2.49244162139228,7.57858609112103));
#381992=CARTESIAN_POINT('Ctrl Pts',(0.99155103710418,2.50981352980178,7.56320440326857));
#381993=CARTESIAN_POINT('Ctrl Pts',(0.989568718370395,2.52716699728825,
7.54780169004651));
#381994=CARTESIAN_POINT('Ctrl Pts',(0.98831721182245,2.53812284299494,7.53807742314383));
#381995=CARTESIAN_POINT('Ctrl Pts',(0.987066543906758,2.54907134720939,
7.52834476460825));
#381996=CARTESIAN_POINT('Ctrl Pts',(0.985816687379919,2.56001274842385,
7.51860402984325));
#381997=CARTESIAN_POINT('',(0.985816687379919,2.56001274842385,7.5));
#381998=CARTESIAN_POINT('Origin',(1.00235268932038,2.47583052179234,7.5));
#381999=CARTESIAN_POINT('Ctrl Pts',(0.99552211070089,2.47505025214476,8.85049129520029));
#382000=CARTESIAN_POINT('Ctrl Pts',(0.995544090074704,2.47485784194233,
8.85097269580138));
#382001=CARTESIAN_POINT('Ctrl Pts',(0.995574149201926,2.47466881399358,
8.85143669361005));
#382002=CARTESIAN_POINT('Ctrl Pts',(0.995614535644998,2.47447460147568,
8.8519052845931));
#382003=CARTESIAN_POINT('Ctrl Pts',(0.995693528966433,2.47409473410719,
8.85282181883899));
#382004=CARTESIAN_POINT('Ctrl Pts',(0.995810192031005,2.4737048441739,8.85372622499636));
#382005=CARTESIAN_POINT('Ctrl Pts',(0.99598112712084,2.47330323361083,8.85462257735071));
#382006=CARTESIAN_POINT('Ctrl Pts',(0.99612303136138,2.47296983078523,8.85536669723987));
#382007=CARTESIAN_POINT('Ctrl Pts',(0.996302341696638,2.47262826201748,
8.85610498449051));
#382008=CARTESIAN_POINT('Ctrl Pts',(0.996535657640059,2.47228124643155,
8.85681338218371));
#382009=CARTESIAN_POINT('Ctrl Pts',(0.996747392225142,2.47196632924232,
8.85745625420284));
#382010=CARTESIAN_POINT('Ctrl Pts',(0.997005762944923,2.47164264202972,
8.85808743050664));
#382011=CARTESIAN_POINT('Ctrl Pts',(0.997338632360824,2.47131662869162,
8.85866804508408));
#382012=CARTESIAN_POINT('Ctrl Pts',(0.9974922110936,2.47116621320452,8.85893592806394));
#382013=CARTESIAN_POINT('Ctrl Pts',(0.997661876290776,2.47101538495296,
8.85919241173847));
#382014=CARTESIAN_POINT('Ctrl Pts',(0.99785177500895,2.47086552375509,8.85943017985534));
#382015=CARTESIAN_POINT('Ctrl Pts',(0.998108194494517,2.4706631667743,8.8597512372));
#382016=CARTESIAN_POINT('Ctrl Pts',(0.998408429108391,2.47045792534337,
8.86004599534706));
#382017=CARTESIAN_POINT('Ctrl Pts',(0.998754749324516,2.47026086344443,
8.86026130871721));
#382018=CARTESIAN_POINT('Ctrl Pts',(0.99888154691944,2.47018871352747,8.86034014101235));
#382019=CARTESIAN_POINT('Ctrl Pts',(0.999016420825345,2.47011656559295,
8.86040910639693));
#382020=CARTESIAN_POINT('Ctrl Pts',(0.999155855142542,2.47004668187887,
8.86046313645507));
#382021=CARTESIAN_POINT('Ctrl Pts',(0.999373441226775,2.46993762892833,
8.8605474499083));
#382022=CARTESIAN_POINT('Ctrl Pts',(0.999608137853262,2.46983124429506,
8.86059655985668));
#382023=CARTESIAN_POINT('Ctrl Pts',(0.99984477226483,2.46973408392439,8.86059725258816));
#382024=CARTESIAN_POINT('Ctrl Pts',(1.00008195339643,2.46963669907444,8.86059794692011));
#382025=CARTESIAN_POINT('Ctrl Pts',(1.00032472074386,2.46954995882129,8.86056369958366));
#382026=CARTESIAN_POINT('Ctrl Pts',(1.000558567504,2.46947505032681,8.86048590497774));
#382027=CARTESIAN_POINT('Ctrl Pts',(1.00061959454594,2.46945550144004,8.86046560290182));
#382028=CARTESIAN_POINT('Ctrl Pts',(1.00068083560639,2.46943659030203,8.86044257503091));
#382029=CARTESIAN_POINT('Ctrl Pts',(1.0007403886005,2.46941886991778,8.86041778462583));
#382030=CARTESIAN_POINT('Ctrl Pts',(1.00114110635172,2.46929963372096,8.860250975962));
#382031=CARTESIAN_POINT('Ctrl Pts',(1.00151926053773,2.4692186285124,8.8599848982295));
#382032=CARTESIAN_POINT('Ctrl Pts',(1.00186203918152,2.46916993407642,8.85968173251462));
#382033=CARTESIAN_POINT('Ctrl Pts',(1.0020433494452,2.46914417750965,8.85952137522077));
#382034=CARTESIAN_POINT('Ctrl Pts',(1.00221823035511,2.46912677532505,8.85934740853961));
#382035=CARTESIAN_POINT('Ctrl Pts',(1.00238406177248,2.46911642601951,8.8591675900182));
#382036=CARTESIAN_POINT('Ctrl Pts',(1.00304996111067,2.46907486817829,8.85844552518694));
#382037=CARTESIAN_POINT('Ctrl Pts',(1.00360738943725,2.46914166499387,8.85759444184123));
#382038=CARTESIAN_POINT('Ctrl Pts',(1.00405699467319,2.46923695081303,8.85683498915136));
#382039=CARTESIAN_POINT('Ctrl Pts',(1.00410404466373,2.46924692222023,8.85675551444997));
#382040=CARTESIAN_POINT('Ctrl Pts',(1.00414990599216,2.46925722395856,8.85667699793651));
#382041=CARTESIAN_POINT('Ctrl Pts',(1.00419457359941,2.46926777628528,8.85659965593547));
#382042=CARTESIAN_POINT('Ctrl Pts',(1.00479749924139,2.46941021212987,8.85555568965886));
#382043=CARTESIAN_POINT('Ctrl Pts',(1.00535637758332,2.46963417619405,8.85434650606346));
#382044=CARTESIAN_POINT('Ctrl Pts',(1.00587628317201,2.46993500686091,8.85297329937118));
#382045=CARTESIAN_POINT('Ctrl Pts',(1.00616869838734,2.47010420578114,8.85220095427748));
#382046=CARTESIAN_POINT('Ctrl Pts',(1.00644874670488,2.47029806236456,8.85137579139183));
#382047=CARTESIAN_POINT('Ctrl Pts',(1.0067166110539,2.47051810124199,8.85049129520029));
#382048=CARTESIAN_POINT('Origin',(1.00235268932038,2.47583052179234,7.59394543036555));
#382049=CARTESIAN_POINT('Ctrl Pts',(0.995585924237744,2.47449162041813,
7.59443877723642));
#382050=CARTESIAN_POINT('Ctrl Pts',(0.9962431422676,2.46873825113483,7.58783886950016));
#382051=CARTESIAN_POINT('Ctrl Pts',(1.00467227562428,2.46772390780438,7.58559994247159));
#382052=CARTESIAN_POINT('Ctrl Pts',(0.991998190294714,2.50589909453895,
7.56670252222137));
#382053=CARTESIAN_POINT('Ctrl Pts',(0.992654458457978,2.50015404050766,
7.56004874999027));
#382054=CARTESIAN_POINT('Ctrl Pts',(1.00113098469779,2.49911247430167,7.55786368756704));
#382055=CARTESIAN_POINT('Ctrl Pts',(0.988417156086367,2.53724791833982,
7.53888913333559));
#382056=CARTESIAN_POINT('Ctrl Pts',(0.989077324483416,2.53146872117116,
7.53222002137277));
#382057=CARTESIAN_POINT('Ctrl Pts',(0.997595022281273,2.53044340710011,
7.53005029815327));
#382058=CARTESIAN_POINT('Ctrl Pts',(0.984842983656921,2.56853667326527,
7.51101258149734));
#382059=CARTESIAN_POINT('Ctrl Pts',(0.985511154494491,2.56268742172587,
7.5043616886572));
#382060=CARTESIAN_POINT('Ctrl Pts',(0.994064645198965,2.56171516748282,
7.50217374673251));
#382061=CARTESIAN_POINT('',(0.99425302963392,2.56004646606292,7.50366116523517));
#382062=CARTESIAN_POINT('Ctrl Pts',(0.985816687379918,2.56001274842385,
7.51860402984325));
#382063=CARTESIAN_POINT('Ctrl Pts',(0.98576656725954,2.56045150626061,7.51734760759493));
#382064=CARTESIAN_POINT('Ctrl Pts',(0.985780388944946,2.5608547392218,7.51608817408572));
#382065=CARTESIAN_POINT('Ctrl Pts',(0.985871466452276,2.56122106239949,
7.51481005913119));
#382066=CARTESIAN_POINT('Ctrl Pts',(0.985953966634782,2.56155288668742,
7.51365231206383));
#382067=CARTESIAN_POINT('Ctrl Pts',(0.986099730040545,2.56185495396783,
7.51247773061042));
#382068=CARTESIAN_POINT('Ctrl Pts',(0.986339490022403,2.5621059898196,7.51129758471022));
#382069=CARTESIAN_POINT('Ctrl Pts',(0.98663748429823,2.56241799871397,7.50983079813402));
#382070=CARTESIAN_POINT('Ctrl Pts',(0.987080589722741,2.56263222255329,
7.50839324291155));
#382071=CARTESIAN_POINT('Ctrl Pts',(0.987707923004607,2.5626760041041,7.50715379678855));
#382072=CARTESIAN_POINT('Ctrl Pts',(0.987997732904655,2.56269622991905,
7.50658120839351));
#382073=CARTESIAN_POINT('Ctrl Pts',(0.988368720848084,2.56267347700261,
7.50598221009429));
#382074=CARTESIAN_POINT('Ctrl Pts',(0.988810665406172,2.56258558301011,
7.50545747549611));
#382075=CARTESIAN_POINT('Ctrl Pts',(0.989046500701831,2.56253868005514,
7.50517746087247));
#382076=CARTESIAN_POINT('Ctrl Pts',(0.989305138541046,2.56247291741205,
7.50491486231392));
#382077=CARTESIAN_POINT('Ctrl Pts',(0.98957931871825,2.56238842000837,7.50468370960993));
#382078=CARTESIAN_POINT('Ctrl Pts',(0.989989304568402,2.56226206973669,
7.50433806340447));
#382079=CARTESIAN_POINT('Ctrl Pts',(0.990446172564123,2.56208950838184,
7.50405484070984));
#382080=CARTESIAN_POINT('Ctrl Pts',(0.990918900363615,2.56188168744653,
7.50385766036131));
#382081=CARTESIAN_POINT('Ctrl Pts',(0.990969451253917,2.56185946422777,
7.50383657498791));
#382082=CARTESIAN_POINT('Ctrl Pts',(0.991020166949378,2.56183686084834,
7.50381643264937));
#382083=CARTESIAN_POINT('Ctrl Pts',(0.991070997752475,2.56181390761954,
7.50379723213559));
#382084=CARTESIAN_POINT('Ctrl Pts',(0.991410309991058,2.56166068730882,
7.50366906242519));
#382085=CARTESIAN_POINT('Ctrl Pts',(0.991761836329712,2.56148788948196,
7.50358235568538));
#382086=CARTESIAN_POINT('Ctrl Pts',(0.992096660797237,2.56131318891304,
7.5035341175365));
#382087=CARTESIAN_POINT('Ctrl Pts',(0.992598692191478,2.56105124518222,
7.50346178989176));
#382088=CARTESIAN_POINT('Ctrl Pts',(0.993127626184805,2.56074810754123,
7.50346967198527));
#382089=CARTESIAN_POINT('Ctrl Pts',(0.99363771872215,2.56043454298074,7.50354272648692));
#382090=CARTESIAN_POINT('Ctrl Pts',(0.993847530341052,2.56030556738661,
7.50357277531559));
#382091=CARTESIAN_POINT('Ctrl Pts',(0.994053949759978,2.56017511988168,
7.50361331098761));
#382092=CARTESIAN_POINT('Ctrl Pts',(0.994253029634434,2.56004646606424,
7.50366116523659));
#382093=CARTESIAN_POINT('',(1.00345144303435,2.47854446470828,7.57603338622103));
#382094=CARTESIAN_POINT('Origin',(1.00677029912172,2.48673450035404,7.58486873427626));
#382095=CARTESIAN_POINT('Ctrl Pts',(0.994253029622191,2.56004646611905,
7.50366116529969));
#382096=CARTESIAN_POINT('Ctrl Pts',(0.997314994686469,2.53292355755921,
7.52783573079709));
#382097=CARTESIAN_POINT('Ctrl Pts',(1.00038100552659,2.50575750849376,7.55196141284068));
#382098=CARTESIAN_POINT('Ctrl Pts',(1.00345144254825,2.47854446586212,7.57603338728831));
#382099=CARTESIAN_POINT('Ctrl Pts',(0.995580073096902,2.47609196989964,
7.59639677331372));
#382100=CARTESIAN_POINT('Ctrl Pts',(0.994718951965599,2.45697504293773,
7.59974925422226));
#382101=CARTESIAN_POINT('Ctrl Pts',(1.00739967866912,2.4713067419417,7.5963967733137));
#382102=CARTESIAN_POINT('Ctrl Pts',(0.994780473004155,2.47227415065622,
7.58707626057422));
#382103=CARTESIAN_POINT('Ctrl Pts',(0.998585879238804,2.46652642806453,
7.58811717123965));
#382104=CARTESIAN_POINT('Ctrl Pts',(1.00531808064709,2.46800794613741,7.58707626057424));
#382105=CARTESIAN_POINT('Ctrl Pts',(0.999909163054375,2.47553331782442,
7.5801537675693));
#382106=CARTESIAN_POINT('Ctrl Pts',(1.00117949275383,2.47293270359069,7.58208760766041));
#382107=CARTESIAN_POINT('Ctrl Pts',(1.00390123521105,2.47391710692994,7.58015376756929));
#382108=CARTESIAN_POINT('Ctrl Pts',(1.0034514427236,2.47854446394126,7.57603338509286));
#382109=CARTESIAN_POINT('Ctrl Pts',(1.0034514427236,2.47854446394126,7.57603338509286));
#382110=CARTESIAN_POINT('Ctrl Pts',(1.0034514427236,2.47854446394126,7.57603338509286));
#382111=CARTESIAN_POINT('Origin',(1.0067650098081,2.48673664175957,7.58486873427622));
#382112=CARTESIAN_POINT('Ctrl Pts',(1.07944577964471,2.53026194050811,7.51098857897448));
#382113=CARTESIAN_POINT('Ctrl Pts',(1.07489655658135,2.52652495221649,7.50433767179956));
#382114=CARTESIAN_POINT('Ctrl Pts',(1.06807576525984,2.53177708100688,7.50214974420965));
#382115=CARTESIAN_POINT('Ctrl Pts',(1.0551042351301,2.51026642356289,7.53887321589164));
#382116=CARTESIAN_POINT('Ctrl Pts',(1.05060951983246,2.50657421102296,7.53220407452058));
#382117=CARTESIAN_POINT('Ctrl Pts',(1.04377751552321,2.51176329928973,7.53003438070911));
#382118=CARTESIAN_POINT('Ctrl Pts',(1.03071594587084,2.49023250784912,7.56669465659229));
#382119=CARTESIAN_POINT('Ctrl Pts',(1.02624779350493,2.48656211559886,7.56004085833293));
#382120=CARTESIAN_POINT('Ctrl Pts',(1.01943406247276,2.4917108746287,7.55785582193788));
#382121=CARTESIAN_POINT('Ctrl Pts',(1.00628201485162,2.47016109942061,7.59443891967696));
#382122=CARTESIAN_POINT('Ctrl Pts',(1.00180738422111,2.46648538555857,7.58783901202978));
#382123=CARTESIAN_POINT('Ctrl Pts',(0.99504666090435,2.47162073347497,7.58560008491213));
#382124=CARTESIAN_POINT('',(1.0667586375038,2.53069219871728,7.50366116523517));
#382125=CARTESIAN_POINT('Ctrl Pts',(1.06675863750394,2.53069219871762,7.50366116523554));
#382126=CARTESIAN_POINT('Ctrl Pts',(1.06750186807347,2.53054473401917,7.50350835821027));
#382127=CARTESIAN_POINT('Ctrl Pts',(1.06818027974489,2.53038499793928,7.50345484955999));
#382128=CARTESIAN_POINT('Ctrl Pts',(1.06881417987673,2.5302088259119,7.50349758195598));
#382129=CARTESIAN_POINT('Ctrl Pts',(1.06913941765563,2.5301184365966,7.50351950684424));
#382130=CARTESIAN_POINT('Ctrl Pts',(1.06948502939518,2.53001493618197,7.50357029184312));
#382131=CARTESIAN_POINT('Ctrl Pts',(1.06981555540291,2.52990597100817,7.50365515313923));
#382132=CARTESIAN_POINT('Ctrl Pts',(1.070324038246,2.52973833844652,7.50378570417639));
#382133=CARTESIAN_POINT('Ctrl Pts',(1.07081185253134,2.52955318148128,7.50400001621911));
#382134=CARTESIAN_POINT('Ctrl Pts',(1.07124106282399,2.52936247059274,7.50428903009634));
#382135=CARTESIAN_POINT('Ctrl Pts',(1.07128870186433,2.52934130315135,7.50432110841318));
#382136=CARTESIAN_POINT('Ctrl Pts',(1.07133564874016,2.52932007288124,7.50435406373354));
#382137=CARTESIAN_POINT('Ctrl Pts',(1.07138187362868,2.52929879997845,7.50438785222352));
#382138=CARTESIAN_POINT('Ctrl Pts',(1.07166409879162,2.5291689186819,7.50459414719561));
#382139=CARTESIAN_POINT('Ctrl Pts',(1.0719236882083,2.52903491181198,7.50483629897752));
#382140=CARTESIAN_POINT('Ctrl Pts',(1.07215130076292,2.52890308253883,7.5050991045531));
#382141=CARTESIAN_POINT('Ctrl Pts',(1.07265343691994,2.52861225392128,7.50567888004914));
#382142=CARTESIAN_POINT('Ctrl Pts',(1.07301999334669,2.52832101331307,7.50637912803144));
#382143=CARTESIAN_POINT('Ctrl Pts',(1.07327584969574,2.52804770250378,7.50710440483569));
#382144=CARTESIAN_POINT('Ctrl Pts',(1.07333859075199,2.52798068126737,7.50728225710685));
#382145=CARTESIAN_POINT('Ctrl Pts',(1.07339603063641,2.52791350375378,7.50746498566954));
#382146=CARTESIAN_POINT('Ctrl Pts',(1.07344714514511,2.52784800883597,7.50764697238949));
#382147=CARTESIAN_POINT('Ctrl Pts',(1.0737219226768,2.52749592618251,7.50862528291181));
#382148=CARTESIAN_POINT('Ctrl Pts',(1.07384211344801,2.52716305316058,7.50965856837422));
#382149=CARTESIAN_POINT('Ctrl Pts',(1.0738738316038,2.526854320862,7.51067959873202));
#382150=CARTESIAN_POINT('Ctrl Pts',(1.07389128614494,2.52668442508868,7.51124147302578));
#382151=CARTESIAN_POINT('Ctrl Pts',(1.07388152051965,2.52652175402811,7.51180065547253));
#382152=CARTESIAN_POINT('Ctrl Pts',(1.07385284243991,2.52636695067111,7.51235175716501));
#382153=CARTESIAN_POINT('Ctrl Pts',(1.0737537482504,2.52583204340633,7.51425603304536));
#382154=CARTESIAN_POINT('Ctrl Pts',(1.0734110653662,2.52532840179909,7.5162690050518));
#382155=CARTESIAN_POINT('Ctrl Pts',(1.07288284142304,2.52487255277835,7.51827788969244));
#382156=CARTESIAN_POINT('Ctrl Pts',(1.07285425294504,2.52484788136791,7.51838661432545));
#382157=CARTESIAN_POINT('Ctrl Pts',(1.07282511102271,2.52482335005463,7.51849533314857));
#382158=CARTESIAN_POINT('Ctrl Pts',(1.07279542170602,2.52479896157614,7.51860402984325));
#382159=CARTESIAN_POINT('Ctrl Pts',(1.00345144418691,2.47854446519998,7.57603338728984));
#382160=CARTESIAN_POINT('Ctrl Pts',(1.0245887295383,2.49595688723387,7.55196141284921));
#382161=CARTESIAN_POINT('Ctrl Pts',(1.04569014275367,2.51333863069779,7.52783573083105));
#382162=CARTESIAN_POINT('Ctrl Pts',(1.06675863755274,2.53069219875055,7.50366116530176));
#382163=CARTESIAN_POINT('Origin',(3.46738858720981E-16,8.56451684780641E-16,
7.49482233047033));
#382164=CARTESIAN_POINT('Origin',(0.99105311921787,2.55180719586895,7.49482233047033));
#382165=CARTESIAN_POINT('Origin',(0.,0.,7.50366116523517));
#382166=CARTESIAN_POINT('Origin',(1.06332537456789,2.52254740248822,7.49482233047033));
#382167=CARTESIAN_POINT('Ctrl Pts',(0.985816807380114,2.56001169753274,
7.51860402984325));
#382168=CARTESIAN_POINT('Ctrl Pts',(0.98495387743998,2.56757156776632,7.51860402984325));
#382169=CARTESIAN_POINT('Ctrl Pts',(0.97784219075701,2.57027715431148,7.51860402984325));
#382170=CARTESIAN_POINT('Ctrl Pts',(0.985496394341871,2.56281872879759,
7.51041458714366));
#382171=CARTESIAN_POINT('Ctrl Pts',(0.983269033888734,2.56821254295569,
7.51004642900443));
#382172=CARTESIAN_POINT('Ctrl Pts',(0.977840229438259,2.57027790048013,
7.5072913648301));
#382173=CARTESIAN_POINT('Ctrl Pts',(0.988011340623422,2.56408315847148,
7.50215815450137));
#382174=CARTESIAN_POINT('Ctrl Pts',(0.986699593402179,2.5669075847334,7.4987716367153));
#382175=CARTESIAN_POINT('Ctrl Pts',(0.983483430761492,2.56815667298609,
7.49481588533169));
#382176=CARTESIAN_POINT('Ctrl Pts',(0.994252830331128,2.56004595288801,
7.50366171572174));
#382177=CARTESIAN_POINT('Ctrl Pts',(0.995578475926988,2.56345928352118,
7.50000045605858));
#382178=CARTESIAN_POINT('Ctrl Pts',(0.995578475926872,2.56345928352122,
7.49482233047317));
#382179=CARTESIAN_POINT('Origin',(0.973397453526297,2.55859407633734,7.51860402984325));
#382180=CARTESIAN_POINT('Origin',(0.973397453526297,2.55859407633734,9.));
#382181=CARTESIAN_POINT('Origin',(0.973397453526297,2.55859407633734,8.75721825406948));
#382182=CARTESIAN_POINT('Ctrl Pts',(0.987712021557103,2.54342048849949,
8.78942910404912));
#382183=CARTESIAN_POINT('Ctrl Pts',(0.987099662981816,2.54895921088619,
8.79672699501691));
#382184=CARTESIAN_POINT('Ctrl Pts',(0.978198471170056,2.54962424495469,
8.79893251111267));
#382185=CARTESIAN_POINT('Ctrl Pts',(0.986464237477126,2.55434378716015,
8.78111911759583));
#382186=CARTESIAN_POINT('Ctrl Pts',(0.985730880534924,2.560909188726,8.78644465894813));
#382187=CARTESIAN_POINT('Ctrl Pts',(0.977964537858769,2.56323285677718,
8.78817647674132));
#382188=CARTESIAN_POINT('Ctrl Pts',(0.985686588644408,2.56115144742715,
8.76780923932029));
#382189=CARTESIAN_POINT('Ctrl Pts',(0.984815827444813,2.56890106107581,
8.76988516158374));
#382190=CARTESIAN_POINT('Ctrl Pts',(0.977807256217952,2.57173236991702,
8.77093053738833));
#382191=CARTESIAN_POINT('Ctrl Pts',(0.985838219522192,2.55982404684426,
8.75371302330492));
#382192=CARTESIAN_POINT('Ctrl Pts',(0.984989587073317,2.56738354579158,
8.75300828287559));
#382193=CARTESIAN_POINT('Ctrl Pts',(0.97783747505197,2.5700746111881,8.75267964240738));
#382194=CARTESIAN_POINT('Origin',(0.974988929080856,2.54466209919315,8.78727029226991));
#382195=CARTESIAN_POINT('Ctrl Pts',(0.99552211070089,2.47505025214476,8.85049129520029));
#382196=CARTESIAN_POINT('Ctrl Pts',(0.99485935071093,2.48085213644374,8.85711686593484));
#382197=CARTESIAN_POINT('Ctrl Pts',(0.986367352980481,2.48184548263715,
8.85933012996512));
#382198=CARTESIAN_POINT('Ctrl Pts',(0.992813526340779,2.49876154025728,
8.82945683644722));
#382199=CARTESIAN_POINT('Ctrl Pts',(0.992145265042191,2.50461158370381,
8.83607469902387));
#382200=CARTESIAN_POINT('Ctrl Pts',(0.98362397791506,2.50557059788235,8.83829567148519));
#382201=CARTESIAN_POINT('Ctrl Pts',(0.990108979344078,2.52243748478279,
8.80838214965003));
#382202=CARTESIAN_POINT('Ctrl Pts',(0.989438080774401,2.52831061523211,
8.81501364461989));
#382203=CARTESIAN_POINT('Ctrl Pts',(0.980885428519758,2.529259800149,8.81722098428721));
#382204=CARTESIAN_POINT('Ctrl Pts',(0.987408162934478,2.54608077127966,
8.78727029226991));
#382205=CARTESIAN_POINT('Ctrl Pts',(0.986737152926342,2.55195487727525,
8.79393457792714));
#382206=CARTESIAN_POINT('Ctrl Pts',(0.978151351640454,2.55291583068591,
8.79610912703474));
#382207=CARTESIAN_POINT('Origin',(0.983102876847268,2.47363158005825,8.85049129520029));
#382208=CARTESIAN_POINT('Ctrl Pts',(1.0067166110539,2.47051810124199,8.85049129520029));
#382209=CARTESIAN_POINT('Ctrl Pts',(1.01122897392938,2.47422481049726,8.85711686593484));
#382210=CARTESIAN_POINT('Ctrl Pts',(1.01802024859354,2.46903064544887,8.85933012996512));
#382211=CARTESIAN_POINT('Ctrl Pts',(1.00272458875461,2.46723882907078,8.86332496987232));
#382212=CARTESIAN_POINT('Ctrl Pts',(1.00710562609236,2.46576967753949,8.86648636486738));
#382213=CARTESIAN_POINT('Ctrl Pts',(1.00684152845079,2.45986998650278,8.87206031107457));
#382214=CARTESIAN_POINT('Ctrl Pts',(0.996112429222676,2.46988252956821,
8.86341338519875));
#382215=CARTESIAN_POINT('Ctrl Pts',(0.991918717460033,2.47185388754846,
8.86654584966059));
#382216=CARTESIAN_POINT('Ctrl Pts',(0.988034913849316,2.46737725686224,
8.87215952290715));
#382217=CARTESIAN_POINT('Ctrl Pts',(0.99552211070089,2.47505025214476,8.85049129520029));
#382218=CARTESIAN_POINT('Ctrl Pts',(0.99485935071093,2.48085213644374,8.85711686593484));
#382219=CARTESIAN_POINT('Ctrl Pts',(0.986367352980481,2.48184548263715,
8.85933012996512));
#382220=CARTESIAN_POINT('Origin',(1.01465101420574,2.46085915478682,8.85049129520029));
#382221=CARTESIAN_POINT('Ctrl Pts',(1.06195995288109,2.51589809662206,8.78727029226991));
#382222=CARTESIAN_POINT('Ctrl Pts',(1.06652848552586,2.51965094689245,8.79393457792714));
#382223=CARTESIAN_POINT('Ctrl Pts',(1.07336460881939,2.51436825501293,8.79610912703474));
#382224=CARTESIAN_POINT('Ctrl Pts',(1.04357160131372,2.50079286798139,8.80838214965002));
#382225=CARTESIAN_POINT('Ctrl Pts',(1.04813937523626,2.5045450949946,8.81501364461995));
#382226=CARTESIAN_POINT('Ctrl Pts',(1.05494349880895,2.4992770104278,8.81722098428721));
#382227=CARTESIAN_POINT('Ctrl Pts',(1.02515785026088,2.48566677477144,8.82945683644722));
#382228=CARTESIAN_POINT('Ctrl Pts',(1.02970766847646,2.48940425195465,8.83607469902389));
#382229=CARTESIAN_POINT('Ctrl Pts',(1.036496098976,2.48416504840349,8.83829567148519));
#382230=CARTESIAN_POINT('Ctrl Pts',(1.0067166110539,2.47051810124199,8.85049129520029));
#382231=CARTESIAN_POINT('Ctrl Pts',(1.01122897392938,2.47422481049726,8.85711686593484));
#382232=CARTESIAN_POINT('Ctrl Pts',(1.01802024859354,2.46903064544887,8.85933012996512));
#382233=CARTESIAN_POINT('Origin',(1.06989435603293,2.50623915016688,8.78727029226991));
#382234=CARTESIAN_POINT('Ctrl Pts',(1.07265235650019,2.52468141587758,8.75374538247849));
#382235=CARTESIAN_POINT('Ctrl Pts',(1.07851586339024,2.52951501343406,8.75304829418602));
#382236=CARTESIAN_POINT('Ctrl Pts',(1.08552051380797,2.52648095415081,8.75272238421917));
#382237=CARTESIAN_POINT('Ctrl Pts',(1.07367232836398,2.52551927882055,8.76769408445016));
#382238=CARTESIAN_POINT('Ctrl Pts',(1.07968382607103,2.53047397863891,8.76974318093967));
#382239=CARTESIAN_POINT('Ctrl Pts',(1.08668211825915,2.5276380901133,8.7707786988043));
#382240=CARTESIAN_POINT('Ctrl Pts',(1.0684445336205,2.52122487068539,8.78108014887994));
#382241=CARTESIAN_POINT('Ctrl Pts',(1.07353664488911,2.52542673219291,8.78639403366327));
#382242=CARTESIAN_POINT('Ctrl Pts',(1.08073062501097,2.52171610883081,8.78812224174741));
#382243=CARTESIAN_POINT('Ctrl Pts',(1.05987733210578,2.51418728372499,8.78944554828685));
#382244=CARTESIAN_POINT('Ctrl Pts',(1.06416521194975,2.51773277439069,8.79673892988685));
#382245=CARTESIAN_POINT('Ctrl Pts',(1.0710163762168,2.5120261902546,8.79894799272499));
#382246=CARTESIAN_POINT('Origin',(1.08072982485787,2.51514001512097,8.75721825406948));
#382247=CARTESIAN_POINT('Origin',(1.08072982485787,2.51514001512097,9.));
#382248=CARTESIAN_POINT('Origin',(1.08072982485787,2.51514001512097,7.51860402984325));
#382249=CARTESIAN_POINT('Ctrl Pts',(1.06675833194055,2.53069147382352,7.50366195182966));
#382250=CARTESIAN_POINT('Ctrl Pts',(1.06818074157518,2.53406588377807,7.50000065167735));
#382251=CARTESIAN_POINT('Ctrl Pts',(1.06818074157528,2.53406588377802,7.49482233047108));
#382252=CARTESIAN_POINT('Ctrl Pts',(1.07405684430837,2.52924734196545,7.50215800491337));
#382253=CARTESIAN_POINT('Ctrl Pts',(1.07696552033799,2.5303628243405,7.49877273257266));
#382254=CARTESIAN_POINT('Ctrl Pts',(1.08014658708643,2.52902194004574,7.49481816995649));
#382255=CARTESIAN_POINT('Ctrl Pts',(1.07497317162722,2.52658832699994,7.51043025814042));
#382256=CARTESIAN_POINT('Ctrl Pts',(1.08032711010537,2.52891815526811,7.51006209594513));
#382257=CARTESIAN_POINT('Ctrl Pts',(1.08566699044973,2.52662367317617,7.50731281821698));
#382258=CARTESIAN_POINT('Ctrl Pts',(1.07279425387574,2.52479800213626,7.51860402984325));
#382259=CARTESIAN_POINT('Ctrl Pts',(1.07867347373823,2.52962871545824,7.51860402984325));
#382260=CARTESIAN_POINT('Ctrl Pts',(1.08566466424078,2.52662467272426,7.51860402984325));
#382261=CARTESIAN_POINT('Origin',(0.,0.,7.5));
#382262=CARTESIAN_POINT('Origin',(1.16293484201938,2.40094160211229,7.5));
#382263=CARTESIAN_POINT('',(1.16293484201938,2.40094160211229,7.59394543036555));
#382264=CARTESIAN_POINT('',(1.16293484201938,2.40094160211229,8.85049129520029));
#382265=CARTESIAN_POINT('',(1.16293484201938,2.40094160211229,7.5));
#382266=CARTESIAN_POINT('',(1.22097218676268,2.44268890636152,8.78727029226991));
#382267=CARTESIAN_POINT('Ctrl Pts',(1.16293484201938,2.40094160211229,8.85049129520029));
#382268=CARTESIAN_POINT('Ctrl Pts',(1.18230874456754,2.41487759811195,8.82945686509571));
#382269=CARTESIAN_POINT('Ctrl Pts',(1.20165384546692,2.42879287656844,8.80838212259896));
#382270=CARTESIAN_POINT('Ctrl Pts',(1.22097218676268,2.44268890636152,8.78727029226991));
#382271=CARTESIAN_POINT('',(1.23235567333044,2.45087725266274,8.75721825406948));
#382272=CARTESIAN_POINT('Origin',(1.19809869544952,2.42623584190851,8.75937679713156));
#382273=CARTESIAN_POINT('',(1.23235567333044,2.45087725266274,7.51860402984325));
#382274=CARTESIAN_POINT('',(1.23235567333044,2.45087725266274,7.5));
#382275=CARTESIAN_POINT('Ctrl Pts',(1.23235567333044,2.45087725266274,7.51860402984325));
#382276=CARTESIAN_POINT('Ctrl Pts',(1.22341571509851,2.44444658017187,7.52834476460825));
#382277=CARTESIAN_POINT('Ctrl Pts',(1.2144699531747,2.43801173298123,7.53807742314407));
#382278=CARTESIAN_POINT('Ctrl Pts',(1.20551819269233,2.43157257091969,7.54780169004674));
#382279=CARTESIAN_POINT('Ctrl Pts',(1.19133908788962,2.42137328622122,7.5632044032688));
#382280=CARTESIAN_POINT('Ctrl Pts',(1.17714491544795,2.41116316309945,7.57858609112103));
#382281=CARTESIAN_POINT('Ctrl Pts',(1.16293484201938,2.40094160211229,7.59394543036555));
#382282=CARTESIAN_POINT('Origin',(1.13841252486685,2.68084313576939,7.5));
#382283=CARTESIAN_POINT('',(1.14781180121214,2.49159143565062,8.75721825406948));
#382284=CARTESIAN_POINT('',(1.14850738206909,2.4775861170588,8.78727029226991));
#382285=CARTESIAN_POINT('Origin',(1.15027302572293,2.4420353947459,8.75658640620927));
#382286=CARTESIAN_POINT('',(1.15205371787328,2.40618167532515,8.85049129520029));
#382287=CARTESIAN_POINT('Ctrl Pts',(1.14850738206909,2.4775861170588,8.78727029226991));
#382288=CARTESIAN_POINT('Ctrl Pts',(1.14968781728227,2.45381839678239,8.80838212259896));
#382289=CARTESIAN_POINT('Ctrl Pts',(1.15086988762437,2.4300177536601,8.82945686509571));
#382290=CARTESIAN_POINT('Ctrl Pts',(1.15205371787328,2.40618167532515,8.85049129520029));
#382291=CARTESIAN_POINT('',(1.15205371787328,2.40618167532515,7.59394543036555));
#382292=CARTESIAN_POINT('',(1.15205371787328,2.40618167532515,7.5));
#382293=CARTESIAN_POINT('',(1.14781180121214,2.49159143565062,7.51860402984325));
#382294=CARTESIAN_POINT('Ctrl Pts',(1.15205371787328,2.40618167532515,7.59394543036555));
#382295=CARTESIAN_POINT('Ctrl Pts',(1.15118542018663,2.42366459713436,7.57858609112103));
#382296=CARTESIAN_POINT('Ctrl Pts',(1.15031809411991,2.44112795565877,7.56320440326857));
#382297=CARTESIAN_POINT('Ctrl Pts',(1.14945168875185,2.45857277618248,7.54780169004651));
#382298=CARTESIAN_POINT('Ctrl Pts',(1.14890469700283,2.469586296229,7.53807742314383));
#382299=CARTESIAN_POINT('Ctrl Pts',(1.14835807179199,2.4805924361358,7.52834476460825));
#382300=CARTESIAN_POINT('Ctrl Pts',(1.14781180121214,2.49159143565062,7.51860402984325));
#382301=CARTESIAN_POINT('',(1.14781180121214,2.49159143565062,7.5));
#382302=CARTESIAN_POINT('Origin',(1.15892025438438,2.40652270515031,7.5));
#382303=CARTESIAN_POINT('Ctrl Pts',(1.15205371787328,2.40618167532515,8.85049129520029));
#382304=CARTESIAN_POINT('Ctrl Pts',(1.15206332432412,2.4059882522268,8.85097269580138));
#382305=CARTESIAN_POINT('Ctrl Pts',(1.15208121062938,2.40579768676135,8.85143669361005));
#382306=CARTESIAN_POINT('Ctrl Pts',(1.15210907085543,2.40560128570561,8.8519052845931));
#382307=CARTESIAN_POINT('Ctrl Pts',(1.15216356369075,2.40521713769589,8.85282181883899));
#382308=CARTESIAN_POINT('Ctrl Pts',(1.15225500672475,2.40482057420507,8.85372622499636));
#382309=CARTESIAN_POINT('Ctrl Pts',(1.15239985933298,2.40440883694516,8.85462257735071));
#382310=CARTESIAN_POINT('Ctrl Pts',(1.15252011082366,2.40406702729552,8.85536669723986));
#382311=CARTESIAN_POINT('Ctrl Pts',(1.15267716836052,2.40371467186481,8.85610498449051));
#382312=CARTESIAN_POINT('Ctrl Pts',(1.15288777156639,2.40335342065579,8.8568133821837));
#382313=CARTESIAN_POINT('Ctrl Pts',(1.15307889430647,2.40302558461626,8.85745625420285));
#382314=CARTESIAN_POINT('Ctrl Pts',(1.15331599546498,2.4026860085849,8.85808743050666));
#382315=CARTESIAN_POINT('Ctrl Pts',(1.15362729321869,2.40233933805946,8.85866804508411));
#382316=CARTESIAN_POINT('Ctrl Pts',(1.15377091925414,2.40217939179392,8.85893592806396));
#382317=CARTESIAN_POINT('Ctrl Pts',(1.15393057225671,2.40201800294868,8.85919241173849));
#382318=CARTESIAN_POINT('Ctrl Pts',(1.15411047916768,2.40185628280407,8.85943017985534));
#382319=CARTESIAN_POINT('Ctrl Pts',(1.15435340675564,2.40163791273455,8.8597512372));
#382320=CARTESIAN_POINT('Ctrl Pts',(1.15463987464167,2.40141385689639,8.86004599534705));
#382321=CARTESIAN_POINT('Ctrl Pts',(1.15497285750655,2.40119501106983,8.86026130871721));
#382322=CARTESIAN_POINT('Ctrl Pts',(1.15509477192116,2.40111488544281,8.86034014101235));
#382323=CARTESIAN_POINT('Ctrl Pts',(1.15522474618013,2.40103424434314,8.86040910639692));
#382324=CARTESIAN_POINT('Ctrl Pts',(1.15535941654963,2.40095557062528,8.86046313645507));
#382325=CARTESIAN_POINT('Ctrl Pts',(1.15556956853339,2.40083280094743,8.8605474499083));
#382326=CARTESIAN_POINT('Ctrl Pts',(1.15579696686363,2.40071159782832,8.86059655985668));
#382327=CARTESIAN_POINT('Ctrl Pts',(1.1560268899981,2.40059947586524,8.86059725258816));
#382328=CARTESIAN_POINT('Ctrl Pts',(1.15625734434686,2.40048709485563,8.86059794692011));
#382329=CARTESIAN_POINT('Ctrl Pts',(1.15649405543564,2.40038497866229,8.86056369958366));
#382330=CARTESIAN_POINT('Ctrl Pts',(1.15672262232881,2.40029524146198,8.86048590497774));
#382331=CARTESIAN_POINT('Ctrl Pts',(1.15678227148268,2.40027182272449,8.86046560290182));
#382332=CARTESIAN_POINT('Ctrl Pts',(1.15684217507603,2.40024902671322,8.86044257503091));
#382333=CARTESIAN_POINT('Ctrl Pts',(1.15690047036321,2.40022752716397,8.86041778462583));
#382334=CARTESIAN_POINT('Ctrl Pts',(1.15729272530747,2.40008286187624,8.86025097596201));
#382335=CARTESIAN_POINT('Ctrl Pts',(1.15766491251362,2.39997779467968,8.8599848982295));
#382336=CARTESIAN_POINT('Ctrl Pts',(1.15800386701869,2.39990723838853,8.85968173251461));
#382337=CARTESIAN_POINT('Ctrl Pts',(1.1581831545321,2.39986991815291,8.85952137522076));
#382338=CARTESIAN_POINT('Ctrl Pts',(1.15835656116863,2.3998413470646,8.85934740853961));
#382339=CARTESIAN_POINT('Ctrl Pts',(1.15852138878528,2.39982039416742,8.8591675900182));
#382340=CARTESIAN_POINT('Ctrl Pts',(1.15918325734183,2.39973625739416,8.85844552518695));
#382341=CARTESIAN_POINT('Ctrl Pts',(1.15974382005879,2.39976720241302,8.85759444184125));
#382342=CARTESIAN_POINT('Ctrl Pts',(1.16019860651594,2.39983348615086,8.85683498915139));
#382343=CARTESIAN_POINT('Ctrl Pts',(1.16024619870749,2.3998404225675,8.85675551444999));
#382344=CARTESIAN_POINT('Ctrl Pts',(1.16029262584355,2.3998477647944,8.85667699793652));
#382345=CARTESIAN_POINT('Ctrl Pts',(1.16033787776631,2.39985543357681,8.85659965593547));
#382346=CARTESIAN_POINT('Ctrl Pts',(1.16094869052878,2.39995894719317,8.85555568965886));
#382347=CARTESIAN_POINT('Ctrl Pts',(1.16152077002208,2.40014664364084,8.85434650606346));
#382348=CARTESIAN_POINT('Ctrl Pts',(1.16205888169598,2.40041354575341,8.85297329937118));
#382349=CARTESIAN_POINT('Ctrl Pts',(1.16236153672493,2.40056366192914,8.85220095427747));
#382350=CARTESIAN_POINT('Ctrl Pts',(1.16265343008711,2.4007391774561,8.85137579139184));
#382351=CARTESIAN_POINT('Ctrl Pts',(1.16293484201938,2.40094160211229,8.85049129520029));
#382352=CARTESIAN_POINT('Origin',(1.15892025438438,2.40652270515031,7.59394543036555));
#382353=CARTESIAN_POINT('Ctrl Pts',(1.15208160864076,2.40562010281997,7.59443877723642));
#382354=CARTESIAN_POINT('Ctrl Pts',(1.15236885671008,2.39983644634717,7.58783886950016));
#382355=CARTESIAN_POINT('Ctrl Pts',(1.16071568230793,2.39828413066547,7.58559994247159));
#382356=CARTESIAN_POINT('Ctrl Pts',(1.15051352985786,2.43719291381974,7.56670252222138));
#382357=CARTESIAN_POINT('Ctrl Pts',(1.1508003627722,2.43141761637252,7.56004874999025));
#382358=CARTESIAN_POINT('Ctrl Pts',(1.15919273970381,2.42983509727515,7.55786368756704));
#382359=CARTESIAN_POINT('Ctrl Pts',(1.14894837930542,2.46870676574945,7.5388891333356));
#382360=CARTESIAN_POINT('Ctrl Pts',(1.14923691688177,2.46289714542676,7.53222002137278));
#382361=CARTESIAN_POINT('Ctrl Pts',(1.15767142205791,2.4613282072018,7.53005029815327));
#382362=CARTESIAN_POINT('Ctrl Pts',(1.14738622780756,2.50016023258599,7.51101258149734));
#382363=CARTESIAN_POINT('Ctrl Pts',(1.14767826298363,2.49428018910866,7.5043616886572));
#382364=CARTESIAN_POINT('Ctrl Pts',(1.15615188708086,2.49276190843519,7.50217374673251));
#382365=CARTESIAN_POINT('',(1.15623297039273,2.49108456570913,7.50366116523517));
#382366=CARTESIAN_POINT('Ctrl Pts',(1.14781180121214,2.49159143565062,7.51860402984325));
#382367=CARTESIAN_POINT('Ctrl Pts',(1.14778989538004,2.49203250321948,7.51734760759494));
#382368=CARTESIAN_POINT('Ctrl Pts',(1.14782952389184,2.49243402213688,7.51608817408573));
#382369=CARTESIAN_POINT('Ctrl Pts',(1.14794388467724,2.49279375730838,7.51481005913121));
#382370=CARTESIAN_POINT('Ctrl Pts',(1.14804747540939,2.49311961402289,7.51365231206384));
#382371=CARTESIAN_POINT('Ctrl Pts',(1.14821229284571,2.4934117215802,7.51247773061043));
#382372=CARTESIAN_POINT('Ctrl Pts',(1.14846764413722,2.49364688017711,7.51129758471022));
#382373=CARTESIAN_POINT('Ctrl Pts',(1.14878501663034,2.49393915545694,7.50983079813402));
#382374=CARTESIAN_POINT('Ctrl Pts',(1.14924093701575,2.49412454928838,7.50839324291155));
#382375=CARTESIAN_POINT('Ctrl Pts',(1.1498697864677,2.49412804750393,7.50715379678855));
#382376=CARTESIAN_POINT('Ctrl Pts',(1.15016029679463,2.49412966357872,7.50658120839351));
#382377=CARTESIAN_POINT('Ctrl Pts',(1.15052906471918,2.49408318813145,7.50598221009429));
#382378=CARTESIAN_POINT('Ctrl Pts',(1.15096446986735,2.49396715924153,7.50545747549611));
#382379=CARTESIAN_POINT('Ctrl Pts',(1.15119681553145,2.49390524263443,7.50517746087247));
#382380=CARTESIAN_POINT('Ctrl Pts',(1.15145070854448,2.49382304412449,7.50491486231392));
#382381=CARTESIAN_POINT('Ctrl Pts',(1.15171891162186,2.49372115354553,7.50468370960992));
#382382=CARTESIAN_POINT('Ctrl Pts',(1.15211995982241,2.49356879499042,7.50433806340447));
#382383=CARTESIAN_POINT('Ctrl Pts',(1.15256483308987,2.49336731654839,7.50405484070984));
#382384=CARTESIAN_POINT('Ctrl Pts',(1.15302327448635,2.49312963482938,7.50385766036131));
#382385=CARTESIAN_POINT('Ctrl Pts',(1.15307229766792,2.49310421846394,7.50383657498791));
#382386=CARTESIAN_POINT('Ctrl Pts',(1.15312146095905,2.49307841215981,7.50381643264937));
#382387=CARTESIAN_POINT('Ctrl Pts',(1.1531707167064,2.49305224935015,7.50379723213559));
#382388=CARTESIAN_POINT('Ctrl Pts',(1.15349951493258,2.49287760403722,7.50366906242519));
#382389=CARTESIAN_POINT('Ctrl Pts',(1.15383924782789,2.49268263887218,7.50358235568538));
#382390=CARTESIAN_POINT('Ctrl Pts',(1.15416219125876,2.49248684496703,7.5035341175365));
#382391=CARTESIAN_POINT('Ctrl Pts',(1.1546464083832,2.49219327416583,7.50346178989176));
#382392=CARTESIAN_POINT('Ctrl Pts',(1.15515483352957,2.49185687043633,7.50346967198527));
#382393=CARTESIAN_POINT('Ctrl Pts',(1.15564378787672,2.49151126838678,7.50354272648693));
#382394=CARTESIAN_POINT('Ctrl Pts',(1.15584490492046,2.49136911511026,7.50357277531559));
#382395=CARTESIAN_POINT('Ctrl Pts',(1.15604254242821,2.49122571028614,7.50361331098761));
#382396=CARTESIAN_POINT('Ctrl Pts',(1.15623297039333,2.49108456571042,7.50366116523659));
#382397=CARTESIAN_POINT('',(1.16019063351064,2.4091606745873,7.57603338622103));
#382398=CARTESIAN_POINT('Origin',(1.16402740803766,2.4171212430868,7.58486873427629));
#382399=CARTESIAN_POINT('Ctrl Pts',(1.15623297038463,2.4910845657659,7.50366116529968));
#382400=CARTESIAN_POINT('Ctrl Pts',(1.15755087359533,2.46382120335538,7.52783573079709));
#382401=CARTESIAN_POINT('Ctrl Pts',(1.15887005024772,2.4365145298623,7.55196141284069));
#382402=CARTESIAN_POINT('Ctrl Pts',(1.16019063309946,2.40916067576991,7.57603338728831));
#382403=CARTESIAN_POINT('Ctrl Pts',(1.15205371787328,2.40618167532515,7.59394543036555));
#382404=CARTESIAN_POINT('Ctrl Pts',(1.152680314397,2.39356533625318,7.59394543036555));
#382405=CARTESIAN_POINT('Ctrl Pts',(1.16293484201938,2.40094160211229,7.59394543036555));
#382406=CARTESIAN_POINT('Ctrl Pts',(1.15216945057637,2.40385143095157,7.58587155981959));
#382407=CARTESIAN_POINT('Ctrl Pts',(1.15521804482293,2.39883498778136,7.58685956158229));
#382408=CARTESIAN_POINT('Ctrl Pts',(1.16104082544615,2.39957920198036,7.58587155981959));
#382409=CARTESIAN_POINT('Ctrl Pts',(1.15683108903169,2.40656504321341,7.57982961904597));
#382410=CARTESIAN_POINT('Ctrl Pts',(1.15782736055642,2.40425328773227,7.58148017275035));
#382411=CARTESIAN_POINT('Ctrl Pts',(1.16025592890684,2.40491572725606,7.57982961904597));
#382412=CARTESIAN_POINT('Ctrl Pts',(1.16019063315139,2.40916067384177,7.57603338509286));
#382413=CARTESIAN_POINT('Ctrl Pts',(1.16019063315139,2.40916067384177,7.57603338509286));
#382414=CARTESIAN_POINT('Ctrl Pts',(1.16019063315139,2.40916067384177,7.57603338509286));
#382415=CARTESIAN_POINT('Origin',(1.16402226679187,2.4171237189801,7.5848687342762));
#382416=CARTESIAN_POINT('Ctrl Pts',(1.23934238165741,2.4559029174225,7.51098857897448));
#382417=CARTESIAN_POINT('Ctrl Pts',(1.23456307579883,2.45246507689653,7.50433767179957));
#382418=CARTESIAN_POINT('Ctrl Pts',(1.22809280357158,2.45814342422545,7.50214974420965));
#382419=CARTESIAN_POINT('Ctrl Pts',(1.21376973228735,2.4375080515231,7.53887321589168));
#382420=CARTESIAN_POINT('Ctrl Pts',(1.20904769099469,2.4341114024277,7.53220407452062));
#382421=CARTESIAN_POINT('Ctrl Pts',(1.20256218979777,2.43972755717507,7.53003438070911));
#382422=CARTESIAN_POINT('Ctrl Pts',(1.18814797399715,2.41907786069558,7.56669465659231));
#382423=CARTESIAN_POINT('Ctrl Pts',(1.18345383909063,2.41570128516482,7.56004085833298));
#382424=CARTESIAN_POINT('Ctrl Pts',(1.17698398972326,2.42127602276314,7.55785582193789));
#382425=CARTESIAN_POINT('Ctrl Pts',(1.16247826555638,2.40061317846372,7.59443891967696));
#382426=CARTESIAN_POINT('Ctrl Pts',(1.15777732473868,2.39723170731886,7.58783901202978));
#382427=CARTESIAN_POINT('Ctrl Pts',(1.15135951492374,2.40278966514234,7.58560008491213));
#382428=CARTESIAN_POINT('',(1.22670887334883,2.45714515960793,7.50366116523517));
#382429=CARTESIAN_POINT('Ctrl Pts',(1.226708873349,2.45714515960827,7.50366116523554));
#382430=CARTESIAN_POINT('Ctrl Pts',(1.22744112877594,2.45695037894577,7.50350835821027));
#382431=CARTESIAN_POINT('Ctrl Pts',(1.22810791225205,2.45674750507576,7.50345484956));
#382432=CARTESIAN_POINT('Ctrl Pts',(1.22872922258754,2.45653108089181,7.50349758195598));
#382433=CARTESIAN_POINT('Ctrl Pts',(1.22904800086722,2.45642003923501,7.50351950684424));
#382434=CARTESIAN_POINT('Ctrl Pts',(1.22938627121605,2.45629460805291,7.50357029184312));
#382435=CARTESIAN_POINT('Ctrl Pts',(1.22970913669999,2.45616468988572,7.50365515313923));
#382436=CARTESIAN_POINT('Ctrl Pts',(1.23020583455544,2.45596482313552,7.50378570417639));
#382437=CARTESIAN_POINT('Ctrl Pts',(1.23068078352653,2.45574879222656,7.50400001621911));
#382438=CARTESIAN_POINT('Ctrl Pts',(1.23109689307202,2.45553097357612,7.50428903009635));
#382439=CARTESIAN_POINT('Ctrl Pts',(1.23114307803021,2.45550679738172,7.50432110841318));
#382440=CARTESIAN_POINT('Ctrl Pts',(1.23118856822057,2.45548260283481,7.50435406373354));
#382441=CARTESIAN_POINT('Ctrl Pts',(1.23123333517554,2.45545841200072,7.50438785222351));
#382442=CARTESIAN_POINT('Ctrl Pts',(1.23150665895337,2.45531071533094,7.50459414719561));
#382443=CARTESIAN_POINT('Ctrl Pts',(1.23175712916612,2.45516035184147,7.50483629897752));
#382444=CARTESIAN_POINT('Ctrl Pts',(1.23197582773581,2.45501421023926,7.5050991045531));
#382445=CARTESIAN_POINT('Ctrl Pts',(1.23245829874673,2.45469180718626,7.50567888004914));
#382446=CARTESIAN_POINT('Ctrl Pts',(1.23280544219416,2.45437767961221,7.50637912803144));
#382447=CARTESIAN_POINT('Ctrl Pts',(1.23304326177522,2.45408853757673,7.50710440483569));
#382448=CARTESIAN_POINT('Ctrl Pts',(1.23310157985788,2.45401763420936,7.50728225710685));
#382449=CARTESIAN_POINT('Ctrl Pts',(1.23315459764782,2.45394691453315,7.50746498566954));
#382450=CARTESIAN_POINT('Ctrl Pts',(1.23320141086249,2.45387827926385,7.50764697238949));
#382451=CARTESIAN_POINT('Ctrl Pts',(1.23345306582122,2.45350931494506,7.50862528291182));
#382452=CARTESIAN_POINT('Ctrl Pts',(1.23355168239986,2.45316942519731,7.50965856837422));
#382453=CARTESIAN_POINT('Ctrl Pts',(1.23356355484101,2.45285929503312,7.51067959873204));
#382454=CARTESIAN_POINT('Ctrl Pts',(1.23357008826035,2.4526886300126,7.51124147302579));
#382455=CARTESIAN_POINT('Ctrl Pts',(1.23354992032895,2.45252691886293,7.51180065547253));
#382456=CARTESIAN_POINT('Ctrl Pts',(1.23351138288626,2.45237427097691,7.51235175716501));
#382457=CARTESIAN_POINT('Ctrl Pts',(1.23337822067027,2.451846811723,7.51425603304535));
#382458=CARTESIAN_POINT('Ctrl Pts',(1.23300397343624,2.45136616066923,7.51626900505179));
#382459=CARTESIAN_POINT('Ctrl Pts',(1.23244762843879,2.45094509166343,7.51827788969242));
#382460=CARTESIAN_POINT('Ctrl Pts',(1.23241751799618,2.45092230261312,7.51838661432544));
#382461=CARTESIAN_POINT('Ctrl Pts',(1.23238686422242,2.45089968883143,7.51849533314856));
#382462=CARTESIAN_POINT('Ctrl Pts',(1.23235567333044,2.45087725266274,7.51860402984325));
#382463=CARTESIAN_POINT('Ctrl Pts',(1.16019063469235,2.40916067500414,7.57603338728985));
#382464=CARTESIAN_POINT('Ctrl Pts',(1.18240010893414,2.42518305082722,7.55196141284922));
#382465=CARTESIAN_POINT('Ctrl Pts',(1.2045718191603,2.4411771094484,7.52783573083105));
#382466=CARTESIAN_POINT('Ctrl Pts',(1.22670887339981,2.457145159638,7.50366116530176));
#382467=CARTESIAN_POINT('Origin',(4.00899494394862E-16,8.32476377985989E-16,
7.49482233047033));
#382468=CARTESIAN_POINT('Origin',(1.15251174268201,2.48306724294371,7.49482233047033));
#382469=CARTESIAN_POINT('Origin',(0.,0.,7.50366116523517));
#382470=CARTESIAN_POINT('Origin',(1.22276082553375,2.44923706764781,7.49482233047033));
#382471=CARTESIAN_POINT('Ctrl Pts',(1.14781185363495,2.49159037923024,7.51860402984325));
#382472=CARTESIAN_POINT('Ctrl Pts',(1.14743505922582,2.49919000501072,7.51860402984325));
#382473=CARTESIAN_POINT('Ctrl Pts',(1.14051133179099,2.50234567996837,7.51860402984325));
#382474=CARTESIAN_POINT('Ctrl Pts',(1.14767194603029,2.49441217208217,7.51041458714365));
#382475=CARTESIAN_POINT('Ctrl Pts',(1.14579474478773,2.49993761154478,7.51004642900441));
#382476=CARTESIAN_POINT('Ctrl Pts',(1.14050942230917,2.50234655026605,7.50729136483008));
#382477=CARTESIAN_POINT('Ctrl Pts',(1.15026273737233,2.49551287068814,7.50215815450139));
#382478=CARTESIAN_POINT('Ctrl Pts',(1.14913464688836,2.49841553779643,7.49877163671531));
#382479=CARTESIAN_POINT('Ctrl Pts',(1.14600512155788,2.49986811991122,7.49481588533172));
#382480=CARTESIAN_POINT('Ctrl Pts',(1.1562327386202,2.49108406635797,7.50366171572174));
#382481=CARTESIAN_POINT('Ctrl Pts',(1.15777435337954,2.49440544953233,7.50000045605858));
#382482=CARTESIAN_POINT('Ctrl Pts',(1.15777435337943,2.49440544953238,7.49482233047317));
#382483=CARTESIAN_POINT('Origin',(1.13532718937376,2.49097138142306,7.51860402984325));
#382484=CARTESIAN_POINT('Origin',(1.13532718937376,2.49097138142306,9.));
#382485=CARTESIAN_POINT('Origin',(1.13532718937376,2.49097138142306,8.75721825406948));
#382486=CARTESIAN_POINT('Ctrl Pts',(1.14864017147865,2.47491183182611,8.78942910404913));
#382487=CARTESIAN_POINT('Ctrl Pts',(1.14838393822146,2.48047840826227,8.79672699501689));
#382488=CARTESIAN_POINT('Ctrl Pts',(1.13954364374199,2.48171237726442,8.79893251111266));
#382489=CARTESIAN_POINT('Ctrl Pts',(1.14809480925299,2.48589263319866,8.78111911759583));
#382490=CARTESIAN_POINT('Ctrl Pts',(1.14778360579385,2.49249153178346,8.78644465894816));
#382491=CARTESIAN_POINT('Ctrl Pts',(1.14018209782487,2.49530801689312,8.78817647674132));
#382492=CARTESIAN_POINT('Ctrl Pts',(1.14775492647406,2.49273613052929,8.76780923932029));
#382493=CARTESIAN_POINT('Ctrl Pts',(1.14738247379799,2.50052561162719,8.76988516158371));
#382494=CARTESIAN_POINT('Ctrl Pts',(1.14056970501266,2.50380014394097,8.77093053738833));
#382495=CARTESIAN_POINT('Ctrl Pts',(1.1478211989626,2.49140174220957,8.75371302330492));
#382496=CARTESIAN_POINT('Ctrl Pts',(1.1474586488806,2.49900008142322,8.75300828287559));
#382497=CARTESIAN_POINT('Ctrl Pts',(1.1404936487924,2.50214385512782,8.75267964240738));
#382498=CARTESIAN_POINT('Origin',(1.13602277023071,2.47696606283123,8.78727029226991));
#382499=CARTESIAN_POINT('Ctrl Pts',(1.15205371787328,2.40618167532515,8.85049129520029));
#382500=CARTESIAN_POINT('Ctrl Pts',(1.15176404759814,2.41201410220894,8.85711686593484));
#382501=CARTESIAN_POINT('Ctrl Pts',(1.14335314149692,2.41354949162872,8.85933012996512));
#382502=CARTESIAN_POINT('Ctrl Pts',(1.15086988603562,2.43001778564904,8.82945683644728));
#382503=CARTESIAN_POINT('Ctrl Pts',(1.15057781132205,2.43589862520232,8.83607469902393));
#382504=CARTESIAN_POINT('Ctrl Pts',(1.1421354763426,2.43740162972408,8.8382956714852));
#382505=CARTESIAN_POINT('Ctrl Pts',(1.14968781879479,2.45381836632828,8.80838214965002));
#382506=CARTESIAN_POINT('Ctrl Pts',(1.14939459141804,2.45972241442014,8.81501364461988));
#382507=CARTESIAN_POINT('Ctrl Pts',(1.14092032599117,2.46121761944619,8.81722098428721));
#382508=CARTESIAN_POINT('Ctrl Pts',(1.14850738206909,2.4775861170588,8.78727029226991));
#382509=CARTESIAN_POINT('Ctrl Pts',(1.14821410598631,2.48349114583245,8.79393457792714));
#382510=CARTESIAN_POINT('Ctrl Pts',(1.1397075136464,2.48500021903836,8.79610912703474));
#382511=CARTESIAN_POINT('Origin',(1.1395691060349,2.40556162109758,8.85049129520029));
#382512=CARTESIAN_POINT('Ctrl Pts',(1.16293484201938,2.40094160211229,8.85049129520029));
#382513=CARTESIAN_POINT('Ctrl Pts',(1.16767542343877,2.40435158745379,8.85711686593484));
#382514=CARTESIAN_POINT('Ctrl Pts',(1.17411995340351,2.39873297591288,8.85933012996512));
#382515=CARTESIAN_POINT('Ctrl Pts',(1.15874091806866,2.39792483730434,8.86332496987231));
#382516=CARTESIAN_POINT('Ctrl Pts',(1.16301882523354,2.39617801027645,8.86648636486737));
#382517=CARTESIAN_POINT('Ctrl Pts',(1.16237727570635,2.39030736158172,8.87206031107457));
#382518=CARTESIAN_POINT('Ctrl Pts',(1.15231172640007,2.40098674855133,8.86341338519877));
#382519=CARTESIAN_POINT('Ctrl Pts',(1.14825293640748,2.40322274820032,8.86654584966058));
#382520=CARTESIAN_POINT('Ctrl Pts',(1.14409029377498,2.39900415138368,8.87215952290714));
#382521=CARTESIAN_POINT('Ctrl Pts',(1.15205371787328,2.40618167532515,8.85049129520029));
#382522=CARTESIAN_POINT('Ctrl Pts',(1.15176404759814,2.41201410220894,8.85711686593484));
#382523=CARTESIAN_POINT('Ctrl Pts',(1.14335314149692,2.41354949162872,8.85933012996512));
#382524=CARTESIAN_POINT('Origin',(1.17023409226482,2.39079414204317,8.85049129520029));
#382525=CARTESIAN_POINT('Ctrl Pts',(1.22097218676268,2.44268890636152,8.78727029226991));
#382526=CARTESIAN_POINT('Ctrl Pts',(1.22577177880954,2.446141339107,8.79393457792714));
#382527=CARTESIAN_POINT('Ctrl Pts',(1.23225539332378,2.44043150916129,8.79610912703474));
#382528=CARTESIAN_POINT('Ctrl Pts',(1.20165382071389,2.42879285876314,8.80838214965003));
#382529=CARTESIAN_POINT('Ctrl Pts',(1.20645261566514,2.43224471814344,8.8150136446199));
#382530=CARTESIAN_POINT('Ctrl Pts',(1.21290523209917,2.42655151572733,8.81722098428721));
#382531=CARTESIAN_POINT('Ctrl Pts',(1.18230877056804,2.41487761681457,8.82945683644722));
#382532=CARTESIAN_POINT('Ctrl Pts',(1.18708870167942,2.4183159070961,8.83607469902387));
#382533=CARTESIAN_POINT('Ctrl Pts',(1.1935275076964,2.41265253181514,8.83829567148519));
#382534=CARTESIAN_POINT('Ctrl Pts',(1.16293484201938,2.40094160211229,8.85049129520029));
#382535=CARTESIAN_POINT('Ctrl Pts',(1.16767542343877,2.40435158745379,8.85711686593484));
#382536=CARTESIAN_POINT('Ctrl Pts',(1.17411995340351,2.39873297591288,8.85933012996512));
#382537=CARTESIAN_POINT('Origin',(1.22827143700812,2.4325414462924,8.78727029226991));
#382538=CARTESIAN_POINT('Ctrl Pts',(1.23220537088866,2.45076911469363,8.75374538247848));
#382539=CARTESIAN_POINT('Ctrl Pts',(1.23836652023368,2.45521710492923,8.75304829418602));
#382540=CARTESIAN_POINT('Ctrl Pts',(1.24516238600017,2.45174048995302,8.75272238421917));
#382541=CARTESIAN_POINT('Ctrl Pts',(1.23327692917391,2.45153990633562,8.7676940844502));
#382542=CARTESIAN_POINT('Ctrl Pts',(1.23959352432148,2.45609926821131,8.76974318093968));
#382543=CARTESIAN_POINT('Ctrl Pts',(1.24639574176609,2.45282082420285,8.7707786988043));
#382544=CARTESIAN_POINT('Ctrl Pts',(1.22778473182154,2.4475892674818,8.78108014887991));
#382545=CARTESIAN_POINT('Ctrl Pts',(1.23313559499254,2.45145624312506,8.78639403366326));
#382546=CARTESIAN_POINT('Ctrl Pts',(1.24007705385559,2.44729232374766,8.78812224174741));
#382547=CARTESIAN_POINT('Ctrl Pts',(1.21878423279645,2.44111504248424,8.78944554828685));
#382548=CARTESIAN_POINT('Ctrl Pts',(1.2232904630983,2.44437852315427,8.79673892988685));
#382549=CARTESIAN_POINT('Ctrl Pts',(1.22976192881264,2.4382447082056,8.79894799272499));
#382550=CARTESIAN_POINT('Origin',(1.23965492357588,2.44072979259362,8.75721825406948));
#382551=CARTESIAN_POINT('Origin',(1.23965492357588,2.44072979259362,9.));
#382552=CARTESIAN_POINT('Origin',(1.23965492357588,2.44072979259362,7.51860402984325));
#382553=CARTESIAN_POINT('Ctrl Pts',(1.2267085219693,2.45714445578105,7.50366195182966));
#382554=CARTESIAN_POINT('Ctrl Pts',(1.22834420829887,2.46042079855025,7.50000065167735));
#382555=CARTESIAN_POINT('Ctrl Pts',(1.22834420829897,2.4604207985502,7.49482233047108));
#382556=CARTESIAN_POINT('Ctrl Pts',(1.23389951291486,2.45523567375382,7.50215800491337));
#382557=CARTESIAN_POINT('Ctrl Pts',(1.23687368195879,2.45616250473763,7.49877273257264));
#382558=CARTESIAN_POINT('Ctrl Pts',(1.23996230211268,2.45462056378712,7.49481816995647));
#382559=CARTESIAN_POINT('Ctrl Pts',(1.23464359386721,2.45252341272686,7.51043025814041));
#382560=CARTESIAN_POINT('Ctrl Pts',(1.24013580471419,2.45450542609693,7.51006209594514));
#382561=CARTESIAN_POINT('Ctrl Pts',(1.2453177057293,2.45187353095618,7.50731281821699));
#382562=CARTESIAN_POINT('Ctrl Pts',(1.23235444642807,2.45087637001727,7.51860402984325));
#382563=CARTESIAN_POINT('Ctrl Pts',(1.23853109166801,2.45532047521073,7.51860402984325));
#382564=CARTESIAN_POINT('Ctrl Pts',(1.24531544834107,2.4518746774913,7.51860402984325));
#382565=CARTESIAN_POINT('Origin',(0.,0.,7.5));
#382566=CARTESIAN_POINT('Origin',(1.31437432427026,2.32149911893916,7.5));
#382567=CARTESIAN_POINT('',(1.31437432427026,2.32149911893916,7.59394543036555));
#382568=CARTESIAN_POINT('',(1.31437432427026,2.32149911893916,8.85049129520029));
#382569=CARTESIAN_POINT('',(1.31437432427026,2.32149911893916,7.5));
#382570=CARTESIAN_POINT('',(1.37496718403115,2.35944218342962,8.78727029226991));
#382571=CARTESIAN_POINT('Ctrl Pts',(1.31437432427026,2.32149911893916,8.85049129520029));
#382572=CARTESIAN_POINT('Ctrl Pts',(1.33460130338714,2.33416519174225,8.82945686509571));
#382573=CARTESIAN_POINT('Ctrl Pts',(1.35479821265376,2.34681243489657,8.80838212259895));
#382574=CARTESIAN_POINT('Ctrl Pts',(1.37496718403115,2.35944218342962,8.78727029226991));
#382575=CARTESIAN_POINT('',(1.38685191115367,2.36688436340662,8.75721825406948));
#382576=CARTESIAN_POINT('Origin',(1.35108653730003,2.34448843318217,8.75937679713155));
#382577=CARTESIAN_POINT('',(1.38685191115367,2.36688436340662,7.51860402984325));
#382578=CARTESIAN_POINT('',(1.38685191115367,2.36688436340662,7.5));
#382579=CARTESIAN_POINT('Ctrl Pts',(1.38685191115367,2.36688436340662,7.51860402984325));
#382580=CARTESIAN_POINT('Ctrl Pts',(1.37751830642363,2.36103968851261,7.52834476460825));
#382581=CARTESIAN_POINT('Ctrl Pts',(1.36817864245207,2.35519121934001,7.53807742314407));
#382582=CARTESIAN_POINT('Ctrl Pts',(1.35883271579191,2.34933882849084,7.54780169004674));
#382583=CARTESIAN_POINT('Ctrl Pts',(1.34402927306645,2.3400689576805,7.5632044032688));
#382584=CARTESIAN_POINT('Ctrl Pts',(1.32921009923994,2.3307892361025,7.57858609112103));
#382585=CARTESIAN_POINT('Ctrl Pts',(1.31437432427026,2.32149911893916,7.59394543036555));
#382586=CARTESIAN_POINT('Origin',(1.30783574368268,2.60239671513041,7.5));
#382587=CARTESIAN_POINT('',(1.30509031014831,2.41293163922361,8.75721825406948));
#382588=CARTESIAN_POINT('',(1.30488713801671,2.39891053004238,8.78727029226991));
#382589=CARTESIAN_POINT('Origin',(1.30437141136732,2.36331972532997,8.75658640621135));
#382590=CARTESIAN_POINT('',(1.30385128920418,2.32742558187728,8.85049129520029));
#382591=CARTESIAN_POINT('Ctrl Pts',(1.30488713801671,2.39891053004238,8.78727029226991));
#382592=CARTESIAN_POINT('Ctrl Pts',(1.3045423448326,2.37511601235258,8.80838212259895));
#382593=CARTESIAN_POINT('Ctrl Pts',(1.30419707404388,2.35128853469735,8.82945686509571));
#382594=CARTESIAN_POINT('Ctrl Pts',(1.30385128920418,2.32742558187728,8.85049129520029));
#382595=CARTESIAN_POINT('',(1.30385128920418,2.32742558187728,7.59394543036555));
#382596=CARTESIAN_POINT('',(1.30385128920418,2.32742558187728,7.5));
#382597=CARTESIAN_POINT('',(1.30509031014831,2.41293163922361,7.51860402984325));
#382598=CARTESIAN_POINT('Ctrl Pts',(1.30385128920418,2.32742558187728,7.59394543036555));
#382599=CARTESIAN_POINT('Ctrl Pts',(1.30410491017447,2.34492821517239,7.57858609112103));
#382600=CARTESIAN_POINT('Ctrl Pts',(1.30435824734443,2.36241126312566,7.56320440326857));
#382601=CARTESIAN_POINT('Ctrl Pts',(1.3046113155876,2.37987575217718,7.54780169004651));
#382602=CARTESIAN_POINT('Ctrl Pts',(1.30477108634394,2.39090168964725,7.53807742314383));
#382603=CARTESIAN_POINT('Ctrl Pts',(1.30493075003819,2.40192023865671,7.52834476460825));
#382604=CARTESIAN_POINT('Ctrl Pts',(1.30509031014831,2.41293163922361,7.51860402984325));
#382605=CARTESIAN_POINT('',(1.30509031014831,2.41293163922361,7.5));
#382606=CARTESIAN_POINT('Origin',(1.3107255675355,2.32732597051532,7.5));
#382607=CARTESIAN_POINT('Ctrl Pts',(1.30385128920418,2.32742558187728,8.85049129520029));
#382608=CARTESIAN_POINT('Ctrl Pts',(1.30384848325707,2.32723194070001,8.85097269580138));
#382609=CARTESIAN_POINT('Ctrl Pts',(1.30385412324171,2.32704062079224,8.85143669361005));
#382610=CARTESIAN_POINT('Ctrl Pts',(1.30386934276709,2.32684283825272,8.8519052845931));
#382611=CARTESIAN_POINT('Ctrl Pts',(1.30389911119355,2.32645598814833,8.85282181883899));
#382612=CARTESIAN_POINT('Ctrl Pts',(1.30396495843793,2.32605438066444,8.85372622499636));
#382613=CARTESIAN_POINT('Ctrl Pts',(1.30408313333414,2.32563420862442,8.85462257735071));
#382614=CARTESIAN_POINT('Ctrl Pts',(1.30418123793579,2.32528539671989,8.85536669723987));
#382615=CARTESIAN_POINT('Ctrl Pts',(1.30431539729113,2.32492370253027,8.85610498449051));
#382616=CARTESIAN_POINT('Ctrl Pts',(1.30450242234569,2.32454970015688,8.85681338218371));
#382617=CARTESIAN_POINT('Ctrl Pts',(1.30467214787644,2.32421029241565,8.85745625420284));
#382618=CARTESIAN_POINT('Ctrl Pts',(1.30488700517416,2.32385622295629,8.85808743050665));
#382619=CARTESIAN_POINT('Ctrl Pts',(1.30517545207641,2.32349031978707,8.85866804508409));
#382620=CARTESIAN_POINT('Ctrl Pts',(1.30530853522435,2.3233214999966,8.85893592806395));
#382621=CARTESIAN_POINT('Ctrl Pts',(1.30545751998389,2.32315021373905,8.85919241173848));
#382622=CARTESIAN_POINT('Ctrl Pts',(1.30562669581158,2.32297729919045,8.85943017985534));
#382623=CARTESIAN_POINT('Ctrl Pts',(1.30585513326037,2.32274381336167,8.8597512372));
#382624=CARTESIAN_POINT('Ctrl Pts',(1.30612665726056,2.32250186380978,8.86004599534705));
#382625=CARTESIAN_POINT('Ctrl Pts',(1.30644493447619,2.32226213334004,8.86026130871721));
#382626=CARTESIAN_POINT('Ctrl Pts',(1.30656146473801,2.32217436125635,8.86034014101235));
#382627=CARTESIAN_POINT('Ctrl Pts',(1.30668600525793,2.3220855583631,8.86040910639693));
#382628=CARTESIAN_POINT('Ctrl Pts',(1.3068153582903,2.32199841792863,8.86046313645507));
#382629=CARTESIAN_POINT('Ctrl Pts',(1.307017212614,2.32186243601043,8.8605474499083));
#382630=CARTESIAN_POINT('Ctrl Pts',(1.30723637821948,2.32172691245507,8.86059655985668));
#382631=CARTESIAN_POINT('Ctrl Pts',(1.30745864527337,2.32160028963279,8.86059725258816));
#382632=CARTESIAN_POINT('Ctrl Pts',(1.30768142585295,2.3214733742612,8.86059794692011));
#382633=CARTESIAN_POINT('Ctrl Pts',(1.30791110798644,2.321356301745,8.86056369958366));
#382634=CARTESIAN_POINT('Ctrl Pts',(1.30813345578225,2.32125210458826,8.86048590497774));
#382635=CARTESIAN_POINT('Ctrl Pts',(1.30819148193687,2.32122491223268,8.86046560290182));
#382636=CARTESIAN_POINT('Ctrl Pts',(1.30824980190641,2.32119832502185,8.86044257503091));
#382637=CARTESIAN_POINT('Ctrl Pts',(1.30830659993882,2.32117313465386,8.86041778462584));
#382638=CARTESIAN_POINT('Ctrl Pts',(1.30868878021642,2.3210036347359,8.86025097596201));
#382639=CARTESIAN_POINT('Ctrl Pts',(1.30905347104564,2.320874937295,8.8599848982295));
#382640=CARTESIAN_POINT('Ctrl Pts',(1.30938720857524,2.32078280907962,8.85968173251461));
#382641=CARTESIAN_POINT('Ctrl Pts',(1.30956373660751,2.32073407853199,8.85952137522076));
#382642=CARTESIAN_POINT('Ctrl Pts',(1.30973495640559,2.3206944559447,8.85934740853961));
#382643=CARTESIAN_POINT('Ctrl Pts',(1.3098981029095,2.32066298555584,8.8591675900182));
#382644=CARTESIAN_POINT('Ctrl Pts',(1.31055322092454,2.32053661558659,8.85844552518695));
#382645=CARTESIAN_POINT('Ctrl Pts',(1.31111461455945,2.320531581649,8.85759444184123));
#382646=CARTESIAN_POINT('Ctrl Pts',(1.31157271342272,2.32056859093144,8.85683498915138));
#382647=CARTESIAN_POINT('Ctrl Pts',(1.31162065224874,2.32057246385428,8.85675551444997));
#382648=CARTESIAN_POINT('Ctrl Pts',(1.31166745441336,2.32057681639897,8.85667699793651));
#382649=CARTESIAN_POINT('Ctrl Pts',(1.31171310470176,2.3205815701244,8.85659965593547));
#382650=CARTESIAN_POINT('Ctrl Pts',(1.31232929462408,2.32064573615287,8.85555568965886));
#382651=CARTESIAN_POINT('Ctrl Pts',(1.3129122244714,2.32079639369908,8.85434650606346));
#382652=CARTESIAN_POINT('Ctrl Pts',(1.31346633101422,2.32102827049931,8.85297329937117));
#382653=CARTESIAN_POINT('Ctrl Pts',(1.31377798218235,2.32115868707097,8.85220095427747));
#382654=CARTESIAN_POINT('Ctrl Pts',(1.31408052113673,2.32131514031054,8.85137579139183));
#382655=CARTESIAN_POINT('Ctrl Pts',(1.31437432427026,2.32149911893916,8.85049129520029));
#382656=CARTESIAN_POINT('Origin',(1.3107255675355,2.32732597051532,7.59394543036555));
#382657=CARTESIAN_POINT('Ctrl Pts',(1.30384314259315,2.32686337621543,7.59443877723642));
#382658=CARTESIAN_POINT('Ctrl Pts',(1.30375924033799,2.32107319883816,7.58783886950015));
#382659=CARTESIAN_POINT('Ctrl Pts',(1.31198945928026,2.31898928960332,7.58559994247159));
#382660=CARTESIAN_POINT('Ctrl Pts',(1.30430116254244,2.35847178464138,7.56670252222136));
#382661=CARTESIAN_POINT('Ctrl Pts',(1.30421738154988,2.35268997571431,7.56004874999032));
#382662=CARTESIAN_POINT('Ctrl Pts',(1.31249112309633,2.35057300663594,7.55786368756704));
#382663=CARTESIAN_POINT('Ctrl Pts',(1.30475832718525,2.39002116752267,7.53888913333559));
#382664=CARTESIAN_POINT('Ctrl Pts',(1.30467404827812,2.38420499702201,7.53222002137277));
#382665=CARTESIAN_POINT('Ctrl Pts',(1.31299070164157,2.38209888174684,7.53005029815327));
#382666=CARTESIAN_POINT('Ctrl Pts',(1.30521461583455,2.42151009722833,7.51101258149734));
#382667=CARTESIAN_POINT('Ctrl Pts',(1.30512931531394,2.41562342417298,7.5043616886572));
#382668=CARTESIAN_POINT('Ctrl Pts',(1.31348825286493,2.41356535601004,7.50217374673251));
#382669=CARTESIAN_POINT('',(1.31346170186501,2.41188626453889,7.50366116523517));
#382670=CARTESIAN_POINT('Ctrl Pts',(1.30509031014831,2.41293163922361,7.51860402984325));
#382671=CARTESIAN_POINT('Ctrl Pts',(1.30509670862026,2.41337320408333,7.51734760759493));
#382672=CARTESIAN_POINT('Ctrl Pts',(1.30516198111639,2.41377135902958,7.51608817408572));
#382673=CARTESIAN_POINT('Ctrl Pts',(1.30529915524687,2.41412302796592,7.51481005913119));
#382674=CARTESIAN_POINT('Ctrl Pts',(1.30542341085214,2.41444157809186,7.51365231206383));
#382675=CARTESIAN_POINT('Ctrl Pts',(1.30560660504881,2.41472252559346,7.51247773061043));
#382676=CARTESIAN_POINT('Ctrl Pts',(1.30587649835674,2.41494084061839,7.51129758471022));
#382677=CARTESIAN_POINT('Ctrl Pts',(1.30621194491551,2.41521218126186,7.50983079813402));
#382678=CARTESIAN_POINT('Ctrl Pts',(1.30667880678715,2.41536798326241,7.50839324291155));
#382679=CARTESIAN_POINT('Ctrl Pts',(1.30730658833189,2.41533118376778,7.50715379678855));
#382680=CARTESIAN_POINT('Ctrl Pts',(1.30759660531648,2.41531418346162,7.50658120839351));
#382681=CARTESIAN_POINT('Ctrl Pts',(1.30796163787564,2.41524417646109,7.50598221009429));
#382682=CARTESIAN_POINT('Ctrl Pts',(1.30838871444073,2.41510048946134,7.50545747549611));
#382683=CARTESIAN_POINT('Ctrl Pts',(1.30861661571512,2.41502381363075,7.50517746087247));
#382684=CARTESIAN_POINT('Ctrl Pts',(1.3088647206011,2.41492551702526,7.50491486231392));
#382685=CARTESIAN_POINT('Ctrl Pts',(1.30912584447469,2.41480665196125,7.50468370960993));
#382686=CARTESIAN_POINT('Ctrl Pts',(1.30951630703256,2.4146289111967,7.50433806340447));
#382687=CARTESIAN_POINT('Ctrl Pts',(1.30994735749208,2.41439934358563,7.50405484070984));
#382688=CARTESIAN_POINT('Ctrl Pts',(1.31038962865153,2.41413277776808,7.50385766036131));
#382689=CARTESIAN_POINT('Ctrl Pts',(1.31043692267758,2.41410427269727,7.50383657498791));
#382690=CARTESIAN_POINT('Ctrl Pts',(1.31048433154187,2.41407536951208,7.50381643264937));
#382691=CARTESIAN_POINT('Ctrl Pts',(1.31053180983103,2.41404610463015,7.50379723213559));
#382692=CARTESIAN_POINT('Ctrl Pts',(1.31084874294237,2.41385075197006,7.50366906242519));
#382693=CARTESIAN_POINT('Ctrl Pts',(1.311175286359,2.41363442062053,7.50358235568538));
#382694=CARTESIAN_POINT('Ctrl Pts',(1.31148502170938,2.4134183379383,7.5035341175365));
#382695=CARTESIAN_POINT('Ctrl Pts',(1.311949434812,2.41309434641212,7.50346178989176));
#382696=CARTESIAN_POINT('Ctrl Pts',(1.31243526188342,2.41272605894919,7.50346967198527));
#382697=CARTESIAN_POINT('Ctrl Pts',(1.31290106882208,2.41234983956353,7.50354272648692));
#382698=CARTESIAN_POINT('Ctrl Pts',(1.31309266485759,2.41219509274292,7.50357277531559));
#382699=CARTESIAN_POINT('Ctrl Pts',(1.31328070831926,2.4120393198808,7.50361331098761));
#382700=CARTESIAN_POINT('Ctrl Pts',(1.31346170186569,2.41188626454013,7.50366116523659));
#382701=CARTESIAN_POINT('',(1.31216235181373,2.3298771264911,7.57603338622103));
#382702=CARTESIAN_POINT('Origin',(1.31650127865085,2.3375755161608,7.58486873427629));
#382703=CARTESIAN_POINT('Ctrl Pts',(1.31346170186055,2.41188626459606,7.50366116529968));
#382704=CARTESIAN_POINT('Ctrl Pts',(1.31303012767071,2.38459447933897,7.52783573079709));
#382705=CARTESIAN_POINT('Ctrl Pts',(1.31259704935554,2.3572593903969,7.55196141284069));
#382706=CARTESIAN_POINT('Ctrl Pts',(1.31216235147917,2.32987712769763,7.57603338728831));
#382707=CARTESIAN_POINT('Ctrl Pts',(1.3040419876395,2.32845133507715,7.59639677331371));
#382708=CARTESIAN_POINT('Ctrl Pts',(1.30089133461177,2.31044729938369,7.59959882295468));
#382709=CARTESIAN_POINT('Ctrl Pts',(1.31501451773084,2.32207676674859,7.59642833564546));
#382710=CARTESIAN_POINT('Ctrl Pts',(1.30276074036375,2.32476711066729,7.58707626057421));
#382711=CARTESIAN_POINT('Ctrl Pts',(1.30574812934753,2.31868535121003,7.58809943920599));
#382712=CARTESIAN_POINT('Ctrl Pts',(1.31249166603443,2.31917434379263,7.58710240504253));
#382713=CARTESIAN_POINT('Ctrl Pts',(1.30826409698653,2.32734367779126,7.58015376756929));
#382714=CARTESIAN_POINT('Ctrl Pts',(1.30917762705492,2.32464280122792,7.58205880659761));
#382715=CARTESIAN_POINT('Ctrl Pts',(1.31193485703792,2.32521267652891,7.58020924244127));
#382716=CARTESIAN_POINT('Ctrl Pts',(1.31216235140745,2.32987712577012,7.57603338509286));
#382717=CARTESIAN_POINT('Ctrl Pts',(1.31216235140745,2.32987712577012,7.57603338509286));
#382718=CARTESIAN_POINT('Ctrl Pts',(1.31216235140745,2.32987712577012,7.57603338509286));
#382719=CARTESIAN_POINT('Origin',(1.31649630659926,2.33757831636739,7.58486873427623));
#382720=CARTESIAN_POINT('Ctrl Pts',(1.39414625998577,2.37145206245969,7.51098857897448));
#382721=CARTESIAN_POINT('Ctrl Pts',(1.3891565105249,2.3683274965235,7.50433767179956));
#382722=CARTESIAN_POINT('Ctrl Pts',(1.38306334512837,2.37440872884376,7.50214974420965));
#382723=CARTESIAN_POINT('Ctrl Pts',(1.36744758926183,2.35473343605575,7.53887321589169));
#382724=CARTESIAN_POINT('Ctrl Pts',(1.36251762585468,2.3516463079646,7.53220407452062));
#382725=CARTESIAN_POINT('Ctrl Pts',(1.35640527808564,2.35766645120807,7.53003438070911));
#382726=CARTESIAN_POINT('Ctrl Pts',(1.34069764724135,2.33798270372187,7.56669465659232));
#382727=CARTESIAN_POINT('Ctrl Pts',(1.33579681900139,2.33491381998374,7.56004085833298));
#382728=CARTESIAN_POINT('Ctrl Pts',(1.32969743729769,2.34089162835799,7.55785582193789));
#382729=CARTESIAN_POINT('Ctrl Pts',(1.31389764371716,2.32120062302662,7.59443891967696));
#382730=CARTESIAN_POINT('Ctrl Pts',(1.30898970988643,2.31812728978919,7.58783901202978));
#382731=CARTESIAN_POINT('Ctrl Pts',(1.30294118573046,2.32408501867887,7.58560008491213));
#382732=CARTESIAN_POINT('',(1.38161829930505,2.37350118398178,7.50366116523517));
#382733=CARTESIAN_POINT('Ctrl Pts',(1.38161829930524,2.3735011839821,7.50366116523554));
#382734=CARTESIAN_POINT('Ctrl Pts',(1.38233657059497,2.37325988775107,7.50350835821027));
#382735=CARTESIAN_POINT('Ctrl Pts',(1.38298898591943,2.37301470974319,7.50345484956));
#382736=CARTESIAN_POINT('Ctrl Pts',(1.38359515336113,2.37275892273607,7.50349758195598));
#382737=CARTESIAN_POINT('Ctrl Pts',(1.38390616221327,2.37262768503176,7.50351950684424));
#382738=CARTESIAN_POINT('Ctrl Pts',(1.38423570114596,2.37248083850581,7.50357029184312));
#382739=CARTESIAN_POINT('Ctrl Pts',(1.38454957938259,2.37233050120685,7.50365515313923));
#382740=CARTESIAN_POINT('Ctrl Pts',(1.38503245121237,2.37209922156347,7.50378570417639));
#382741=CARTESIAN_POINT('Ctrl Pts',(1.385492583202,2.37185320442812,7.50400001621911));
#382742=CARTESIAN_POINT('Ctrl Pts',(1.38589388211694,2.37160917307934,7.50428903009634));
#382743=CARTESIAN_POINT('Ctrl Pts',(1.38593842320909,2.37158208747709,7.50432110841318));
#382744=CARTESIAN_POINT('Ctrl Pts',(1.38598226978504,2.37155502807398,7.50435406373354));
#382745=CARTESIAN_POINT('Ctrl Pts',(1.38602539484944,2.37152801871389,7.50438785222351));
#382746=CARTESIAN_POINT('Ctrl Pts',(1.38628869409613,2.37136311358819,7.50459414719561));
#382747=CARTESIAN_POINT('Ctrl Pts',(1.38652901586912,2.371197011355,7.50483629897752));
#382748=CARTESIAN_POINT('Ctrl Pts',(1.38673790177454,2.37103715795092,7.50509910455309));
#382749=CARTESIAN_POINT('Ctrl Pts',(1.38719872506249,2.37068450528576,7.50567888004914));
#382750=CARTESIAN_POINT('Ctrl Pts',(1.38752502904371,2.37034878156346,7.50637912803144));
#382751=CARTESIAN_POINT('Ctrl Pts',(1.38774383460512,2.37004499644843,7.50710440483569));
#382752=CARTESIAN_POINT('Ctrl Pts',(1.38779749007268,2.36997050230725,7.50728225710685));
#382753=CARTESIAN_POINT('Ctrl Pts',(1.38784586790667,2.36989653107073,7.50746498566954));
#382754=CARTESIAN_POINT('Ctrl Pts',(1.38788818746177,2.369825037487,7.50764697238949));
#382755=CARTESIAN_POINT('Ctrl Pts',(1.38811568574332,2.36944070765641,7.50862528291181));
#382756=CARTESIAN_POINT('Ctrl Pts',(1.38819232289272,2.36909519786271,7.50965856837421));
#382757=CARTESIAN_POINT('Ctrl Pts',(1.38818430083282,2.36878494422429,7.51067959873202));
#382758=CARTESIAN_POINT('Ctrl Pts',(1.38817988628315,2.36861421125574,7.51124147302578));
#382759=CARTESIAN_POINT('Ctrl Pts',(1.38814939891999,2.36845412452277,7.51180065547252));
#382760=CARTESIAN_POINT('Ctrl Pts',(1.38810116047297,2.36830425937063,7.512351757165));
#382761=CARTESIAN_POINT('Ctrl Pts',(1.3879344774226,2.3677864155708,7.51425603304535));
#382762=CARTESIAN_POINT('Ctrl Pts',(1.38753020370091,2.36733073016879,7.51626900505179));
#382763=CARTESIAN_POINT('Ctrl Pts',(1.3869480237901,2.36694617144079,7.51827788969241));
#382764=CARTESIAN_POINT('Ctrl Pts',(1.38691651511316,2.36692535839572,7.51838661432544));
#382765=CARTESIAN_POINT('Ctrl Pts',(1.38688447545089,2.36690475507049,7.51849533314856));
#382766=CARTESIAN_POINT('Ctrl Pts',(1.38685191115368,2.36688436340662,7.51860402984325));
#382767=CARTESIAN_POINT('Ctrl Pts',(1.31216235301971,2.32987712683138,7.57603338728984));
#382768=CARTESIAN_POINT('Ctrl Pts',(1.33535275265831,2.34444361706461,7.55196141284921));
#382769=CARTESIAN_POINT('Ctrl Pts',(1.35850365158215,2.35898426782545,7.52783573083105));
#382770=CARTESIAN_POINT('Ctrl Pts',(1.38161829935784,2.37350118400852,7.50366116530176));
#382771=CARTESIAN_POINT('Origin',(4.53412748053601E-16,8.0508024718857E-16,
7.49482233047033));
#382772=CARTESIAN_POINT('Origin',(1.30923444818248,2.40412383410096,7.49482233047033));
#382773=CARTESIAN_POINT('Origin',(0.,0.,7.50366116523517));
#382774=CARTESIAN_POINT('Origin',(1.37717168998611,2.36586229233673,7.49482233047033));
#382775=CARTESIAN_POINT('Ctrl Pts',(1.30509029477833,2.41293058161502,7.51860402984325));
#382776=CARTESIAN_POINT('Ctrl Pts',(1.30520118422925,2.42053873444996,7.51860402984325));
#382777=CARTESIAN_POINT('Ctrl Pts',(1.29849386712373,2.4241315304748,7.51860402984325));
#382778=CARTESIAN_POINT('Ctrl Pts',(1.30513146751761,2.41575554070189,7.51041458714366));
#382779=CARTESIAN_POINT('Ctrl Pts',(1.30361213930819,2.42138990025307,7.51004642900444));
#382780=CARTESIAN_POINT('Ctrl Pts',(1.29849201732532,2.42413252132528,7.50729136483011));
#382781=CARTESIAN_POINT('Ctrl Pts',(1.30778745780281,2.41668798523335,7.50215815450137));
#382782=CARTESIAN_POINT('Ctrl Pts',(1.30684765962187,2.41965696550621,7.49877163671527));
#382783=CARTESIAN_POINT('Ctrl Pts',(1.30381763149245,2.42130707251161,7.49481588533168));
#382784=CARTESIAN_POINT('Ctrl Pts',(1.31346143857514,2.41188578106341,7.50366171572174));
#382785=CARTESIAN_POINT('Ctrl Pts',(1.31521268767224,2.41510156850307,7.50000045605858));
#382786=CARTESIAN_POINT('Ctrl Pts',(1.31521268767213,2.41510156850313,7.49482233047317));
#382787=CARTESIAN_POINT('Origin',(1.29259162227317,2.41311275079082,7.51860402984325));
#382788=CARTESIAN_POINT('Origin',(1.29259162227317,2.41311275079082,9.));
#382789=CARTESIAN_POINT('Origin',(1.29259162227317,2.41311275079082,8.75721825406948));
#382790=CARTESIAN_POINT('Ctrl Pts',(1.30484831255304,2.39623323156884,8.78942910404913));
#382791=CARTESIAN_POINT('Ctrl Pts',(1.30494925753137,2.40180478779785,8.79672699501691));
#382792=CARTESIAN_POINT('Ctrl Pts',(1.29620618705044,2.40360262109034,8.79893251111266));
#382793=CARTESIAN_POINT('Ctrl Pts',(1.30500761319207,2.40722641318505,8.78111911759576));
#382794=CARTESIAN_POINT('Ctrl Pts',(1.30511984201778,2.41383169249909,8.78644465894811));
#382795=CARTESIAN_POINT('Ctrl Pts',(1.29771440498272,2.41712942112576,8.78817647674131));
#382796=CARTESIAN_POINT('Ctrl Pts',(1.30510689311817,2.41407762618082,8.76780923932035));
#382797=CARTESIAN_POINT('Ctrl Pts',(1.30523427945354,2.42187496607927,8.76988516158375));
#382798=CARTESIAN_POINT('Ctrl Pts',(1.29864530823804,2.42557926611001,8.77093053738834));
#382799=CARTESIAN_POINT('Ctrl Pts',(1.30508753488959,2.41274173341214,8.75371302330491));
#382800=CARTESIAN_POINT('Ctrl Pts',(1.30521255697053,2.42034768968648,8.75300828287559));
#382801=CARTESIAN_POINT('Ctrl Pts',(1.29846328949482,2.42393125325864,8.75267964240737));
#382802=CARTESIAN_POINT('Origin',(1.29238845014157,2.39909164160959,8.78727029226991));
#382803=CARTESIAN_POINT('Ctrl Pts',(1.30385128920418,2.32742558187728,8.85049129520029));
#382804=CARTESIAN_POINT('Ctrl Pts',(1.30393589896115,2.33326458465276,8.85711686593484));
#382805=CARTESIAN_POINT('Ctrl Pts',(1.29564064670646,2.33533570805445,8.85933012996512));
#382806=CARTESIAN_POINT('Ctrl Pts',(1.30419707450793,2.35128856672232,8.82945683644724));
#382807=CARTESIAN_POINT('Ctrl Pts',(1.30428238657705,2.35717603675118,8.8360746990239));
#382808=CARTESIAN_POINT('Ctrl Pts',(1.29595369511061,2.35921685544825,8.83829567148519));
#382809=CARTESIAN_POINT('Ctrl Pts',(1.30454234439081,2.37511598186413,8.80838214965001));
#382810=CARTESIAN_POINT('Ctrl Pts',(1.30462799314117,2.38102668659857,8.81501364461995));
#382811=CARTESIAN_POINT('Ctrl Pts',(1.29626693711641,2.38306176761556,8.81722098428721));
#382812=CARTESIAN_POINT('Ctrl Pts',(1.30488713801671,2.39891053004238,8.78727029226991));
#382813=CARTESIAN_POINT('Ctrl Pts',(1.30497280099362,2.40482221656425,8.79393457792714));
#382814=CARTESIAN_POINT('Ctrl Pts',(1.29658037301227,2.40687320845992,8.79610912703474));
#382815=CARTESIAN_POINT('Origin',(1.29135260132903,2.32760669344449,8.85049129520029));
#382816=CARTESIAN_POINT('Ctrl Pts',(1.31437432427026,2.32149911893916,8.85049129520029));
#382817=CARTESIAN_POINT('Ctrl Pts',(1.31932364416766,2.32459836800567,8.85711686593484));
#382818=CARTESIAN_POINT('Ctrl Pts',(1.325394947477,2.31857839805226,8.85933012996512));
#382819=CARTESIAN_POINT('Ctrl Pts',(1.30999573240122,2.31875725802815,8.86332496987232));
#382820=CARTESIAN_POINT('Ctrl Pts',(1.31415293055507,2.31673993359065,8.86648636486738));
#382821=CARTESIAN_POINT('Ctrl Pts',(1.31313656540689,2.31092245099262,8.87206031107457));
#382822=CARTESIAN_POINT('Ctrl Pts',(1.3037759275236,2.32222479797461,8.86341338519876));
#382823=CARTESIAN_POINT('Ctrl Pts',(1.29986873773974,2.32471625109016,8.86654584966054));
#382824=CARTESIAN_POINT('Ctrl Pts',(1.29544436127692,2.32077302326231,8.87215952290714));
#382825=CARTESIAN_POINT('Ctrl Pts',(1.30385128920418,2.32742558187728,8.85049129520029));
#382826=CARTESIAN_POINT('Ctrl Pts',(1.30393589896115,2.33326458465277,8.85711686593484));
#382827=CARTESIAN_POINT('Ctrl Pts',(1.29564064670646,2.33533570805445,8.85933012996512));
#382828=CARTESIAN_POINT('Origin',(1.32100842742436,2.31090484334614,8.85049129520029));
#382829=CARTESIAN_POINT('Ctrl Pts',(1.37496718403115,2.35944218342962,8.78727029226991));
#382830=CARTESIAN_POINT('Ctrl Pts',(1.37997811292687,2.3625800118635,8.79393457792714));
#382831=CARTESIAN_POINT('Ctrl Pts',(1.38608257609904,2.35646650676758,8.79610912703474));
#382832=CARTESIAN_POINT('Ctrl Pts',(1.3547981868108,2.34681241871379,8.80838214965002));
#382833=CARTESIAN_POINT('Ctrl Pts',(1.35980828351299,2.34994972603061,8.81501364461989));
#382834=CARTESIAN_POINT('Ctrl Pts',(1.36588287762333,2.34385480035508,8.81722098428721));
#382835=CARTESIAN_POINT('Ctrl Pts',(1.3346013305325,2.33416520874059,8.82945683644723));
#382836=CARTESIAN_POINT('Ctrl Pts',(1.33959173277748,2.33729018344821,8.8360746990239));
#382837=CARTESIAN_POINT('Ctrl Pts',(1.34565445587684,2.3312259084612,8.8382956714852));
#382838=CARTESIAN_POINT('Ctrl Pts',(1.31437432427026,2.32149911893916,8.85049129520029));
#382839=CARTESIAN_POINT('Ctrl Pts',(1.31932364416766,2.32459836800567,8.85711686593484));
#382840=CARTESIAN_POINT('Ctrl Pts',(1.325394947477,2.31857839805226,8.85933012996512));
#382841=CARTESIAN_POINT('Origin',(1.38160128718524,2.34884790783661,8.78727029226991));
#382842=CARTESIAN_POINT('Ctrl Pts',(1.38669498910091,2.36678607752908,8.75374538247848));
#382843=CARTESIAN_POINT('Ctrl Pts',(1.39312846341669,2.37083018269781,8.75304829418602));
#382844=CARTESIAN_POINT('Ctrl Pts',(1.3996876188618,2.36692529818532,8.75272238421917));
#382845=CARTESIAN_POINT('Ctrl Pts',(1.3878137305448,2.36748663052192,8.76769408445021));
#382846=CARTESIAN_POINT('Ctrl Pts',(1.39440946688854,2.37163191905903,8.76974318093966));
#382847=CARTESIAN_POINT('Ctrl Pts',(1.40098765781904,2.36792439139735,8.77077869880429));
#382848=CARTESIAN_POINT('Ctrl Pts',(1.38207969920048,2.36389599497185,8.78108014887988));
#382849=CARTESIAN_POINT('Ctrl Pts',(1.38766732642936,2.36741219451847,8.78639403366328));
#382850=CARTESIAN_POINT('Ctrl Pts',(1.39432774009022,2.36281208956368,8.78812224174742));
#382851=CARTESIAN_POINT('Ctrl Pts',(1.37268288764616,2.3580117359164,8.78944554828686));
#382852=CARTESIAN_POINT('Ctrl Pts',(1.37738895133899,2.36097979624867,8.79673892988685));
#382853=CARTESIAN_POINT('Ctrl Pts',(1.38345412585988,2.35444395564874,8.79894799272499));
#382854=CARTESIAN_POINT('Origin',(1.39348601430777,2.35629008781361,8.75721825406948));
#382855=CARTESIAN_POINT('Origin',(1.39348601430777,2.35629008781361,9.));
#382856=CARTESIAN_POINT('Origin',(1.39348601430777,2.35629008781361,7.51860402984325));
#382857=CARTESIAN_POINT('Ctrl Pts',(1.38161790355312,2.37350050411394,7.50366195182966));
#382858=CARTESIAN_POINT('Ctrl Pts',(1.38346014519165,2.37666531650258,7.50000065167735));
#382859=CARTESIAN_POINT('Ctrl Pts',(1.38346014519175,2.37666531650252,7.49482233047108));
#382860=CARTESIAN_POINT('Ctrl Pts',(1.38867182375217,2.37113491551234,7.50215800491338));
#382861=CARTESIAN_POINT('Ctrl Pts',(1.39169926431183,2.37186928655758,7.49877273257264));
#382862=CARTESIAN_POINT('Ctrl Pts',(1.39468274606847,2.37013262511744,7.49481816995647));
#382863=CARTESIAN_POINT('Ctrl Pts',(1.38924060074975,2.36838055368624,7.5104302581404));
#382864=CARTESIAN_POINT('Ctrl Pts',(1.39484851529313,2.37000660764011,7.51006209594515));
#382865=CARTESIAN_POINT('Ctrl Pts',(1.39985114343623,2.36704811447227,7.50731281821699));
#382866=CARTESIAN_POINT('Ctrl Pts',(1.38685063022082,2.36688356118255,7.51860402984325));
#382867=CARTESIAN_POINT('Ctrl Pts',(1.39329931967803,2.370922796466,7.51860402984324));
#382868=CARTESIAN_POINT('Ctrl Pts',(1.3998489641448,2.36704940328307,7.51860402984325));
#382869=CARTESIAN_POINT('Origin',(0.,0.,7.5));
#382870=CARTESIAN_POINT('Origin',(1.46041276049031,2.2325170979263,7.5));
#382871=CARTESIAN_POINT('',(1.46041276049031,2.2325170979263,7.59394543036555));
#382872=CARTESIAN_POINT('',(1.46041276049031,2.2325170979263,8.85049129520029));
#382873=CARTESIAN_POINT('',(1.46041276049031,2.2325170979263,7.5));
#382874=CARTESIAN_POINT('',(1.5233121462109,2.26650000646725,8.78727029226991));
#382875=CARTESIAN_POINT('Ctrl Pts',(1.46041276049031,2.2325170979263,8.85049129520029));
#382876=CARTESIAN_POINT('Ctrl Pts',(1.48140969918004,2.24386119992283,8.82945686509571));
#382877=CARTESIAN_POINT('Ctrl Pts',(1.50237542338151,2.25518843754003,8.80838212259896));
#382878=CARTESIAN_POINT('Ctrl Pts',(1.5233121462109,2.26650000646725,8.78727029226991));
#382879=CARTESIAN_POINT('',(1.53564927699518,2.27316543860616,8.75721825406948));
#382880=CARTESIAN_POINT('Origin',(1.49852247476168,2.25310701859276,8.75937679713152));
#382881=CARTESIAN_POINT('',(1.53564927699518,2.27316543860616,7.51860402984325));
#382882=CARTESIAN_POINT('',(1.53564927699518,2.27316543860616,7.5));
#382883=CARTESIAN_POINT('Ctrl Pts',(1.53564927699518,2.27316543860616,7.51860402984325));
#382884=CARTESIAN_POINT('Ctrl Pts',(1.5259603795509,2.26793077833183,7.52834476460825));
#382885=CARTESIAN_POINT('Ctrl Pts',(1.51626519221421,2.26269271979159,7.53807742314407));
#382886=CARTESIAN_POINT('Ctrl Pts',(1.50656350379361,2.25745114888413,7.54780169004675));
#382887=CARTESIAN_POINT('Ctrl Pts',(1.49119655366688,2.24914878384945,7.5632044032688));
#382888=CARTESIAN_POINT('Ctrl Pts',(1.47581327361948,2.24083759618168,7.57858609112103));
#382889=CARTESIAN_POINT('Ctrl Pts',(1.46041276049031,2.2325170979263,7.59394543036555));
#382890=CARTESIAN_POINT('Origin',(1.47188478489783,2.51325648817661,7.5));
#382891=CARTESIAN_POINT('',(1.45700592305909,2.32435658911882,8.75721825406948));
#382892=CARTESIAN_POINT('',(1.45590483281682,2.31037730509333,8.78727029226991));
#382893=CARTESIAN_POINT('Origin',(1.45310985509558,2.27489266822179,8.75658640620982));
#382894=CARTESIAN_POINT('',(1.45029105591251,2.23910559748226,8.85049129520029));
#382895=CARTESIAN_POINT('Ctrl Pts',(1.45590483281682,2.31037730509333,8.78727029226991));
#382896=CARTESIAN_POINT('Ctrl Pts',(1.45403622806456,2.28665376676723,8.80838212259896));
#382897=CARTESIAN_POINT('Ctrl Pts',(1.45216503493675,2.26289736679571,8.82945686509571));
#382898=CARTESIAN_POINT('Ctrl Pts',(1.45029105591251,2.23910559748226,8.85049129520029));
#382899=CARTESIAN_POINT('',(1.45029105591251,2.23910559748226,7.59394543036555));
#382900=CARTESIAN_POINT('',(1.45029105591251,2.23910559748226,7.5));
#382901=CARTESIAN_POINT('',(1.45700592305909,2.32435658911882,7.51860402984325));
#382902=CARTESIAN_POINT('Ctrl Pts',(1.45029105591251,2.23910559748225,7.59394543036555));
#382903=CARTESIAN_POINT('Ctrl Pts',(1.45166555335678,2.25655602018875,7.57858609112103));
#382904=CARTESIAN_POINT('Ctrl Pts',(1.45303851274666,2.27398691597674,7.56320440326857));
#382905=CARTESIAN_POINT('Ctrl Pts',(1.45441001468936,2.29139930822443,7.54780169004651));
#382906=CARTESIAN_POINT('Ctrl Pts',(1.45527589141875,2.30239235517594,7.53807742314383));
#382907=CARTESIAN_POINT('Ctrl Pts',(1.45614118792571,2.31337803570671,7.52834476460825));
#382908=CARTESIAN_POINT('Ctrl Pts',(1.4570059230591,2.32435658911882,7.51860402984325));
#382909=CARTESIAN_POINT('',(1.45700592305909,2.32435658911882,7.5));
#382910=CARTESIAN_POINT('Origin',(1.45714482817987,2.23856575425762,7.5));
#382911=CARTESIAN_POINT('Ctrl Pts',(1.45029105591251,2.23910559748225,8.85049129520029));
#382912=CARTESIAN_POINT('Ctrl Pts',(1.4502758490977,2.2389125339392,8.85097269580138));
#382913=CARTESIAN_POINT('Ctrl Pts',(1.45026921958581,2.23872124576364,8.85143669361005));
#382914=CARTESIAN_POINT('Ctrl Pts',(1.45027173587022,2.23852289447122,8.8519052845931));
#382915=CARTESIAN_POINT('Ctrl Pts',(1.45027665756297,2.23813493192223,8.85282181883899));
#382916=CARTESIAN_POINT('Ctrl Pts',(1.45031663843729,2.23772993073655,8.85372622499635));
#382917=CARTESIAN_POINT('Ctrl Pts',(1.45040765001546,2.23730305049346,8.8546225773507));
#382918=CARTESIAN_POINT('Ctrl Pts',(1.45048320459523,2.23694866967699,8.85536669723986));
#382919=CARTESIAN_POINT('Ctrl Pts',(1.4505939144795,2.23657912300746,8.85610498449051));
#382920=CARTESIAN_POINT('Ctrl Pts',(1.45075659285669,2.23619390632567,8.85681338218371));
#382921=CARTESIAN_POINT('Ctrl Pts',(1.45090422373948,2.23584432158196,8.85745625420284));
#382922=CARTESIAN_POINT('Ctrl Pts',(1.4510959542817,2.23547721364194,8.85808743050665));
#382923=CARTESIAN_POINT('Ctrl Pts',(1.45136036504231,2.23509358140355,8.85866804508409));
#382924=CARTESIAN_POINT('Ctrl Pts',(1.45148235843553,2.23491658180487,8.85893592806395));
#382925=CARTESIAN_POINT('Ctrl Pts',(1.4516200627417,2.234736101987,8.85919241173848));
#382926=CARTESIAN_POINT('Ctrl Pts',(1.45177781230635,2.23455270357739,8.85943017985534));
#382927=CARTESIAN_POINT('Ctrl Pts',(1.45199082091748,2.23430506143268,8.8597512372));
#382928=CARTESIAN_POINT('Ctrl Pts',(1.45224628528148,2.23404621238968,8.86004599534705));
#382929=CARTESIAN_POINT('Ctrl Pts',(1.4525485489785,2.23378658238068,8.86026130871721));
#382930=CARTESIAN_POINT('Ctrl Pts',(1.4526592162397,2.23369152451464,8.86034014101235));
#382931=CARTESIAN_POINT('Ctrl Pts',(1.45277781125685,2.23359492473796,8.86040910639692));
#382932=CARTESIAN_POINT('Ctrl Pts',(1.45290131541274,2.23349967566561,8.86046313645506));
#382933=CARTESIAN_POINT('Ctrl Pts',(1.45309404261367,2.23335104028592,8.86054744990829));
#382934=CARTESIAN_POINT('Ctrl Pts',(1.45330407489591,2.23320175318969,8.86059655985668));
#382935=CARTESIAN_POINT('Ctrl Pts',(1.45351777252622,2.23306114982854,8.86059725258816));
#382936=CARTESIAN_POINT('Ctrl Pts',(1.45373196388343,2.23292022161745,8.86059794692011));
#382937=CARTESIAN_POINT('Ctrl Pts',(1.45395367324847,2.23278867385447,8.86056369958366));
#382938=CARTESIAN_POINT('Ctrl Pts',(1.45416888827214,2.23267044490978,8.86048590497774));
#382939=CARTESIAN_POINT('Ctrl Pts',(1.45422505298559,2.23263959067531,8.86046560290182));
#382940=CARTESIAN_POINT('Ctrl Pts',(1.45428154968206,2.23260932151749,8.86044257503091));
#382941=CARTESIAN_POINT('Ctrl Pts',(1.45433661706439,2.23258054384337,8.86041778462584));
#382942=CARTESIAN_POINT('Ctrl Pts',(1.4547071522146,2.23238690580672,8.86025097596201));
#382943=CARTESIAN_POINT('Ctrl Pts',(1.45506284807405,2.23223510696686,8.8599848982295));
#382944=CARTESIAN_POINT('Ctrl Pts',(1.45538999722907,2.23212178540184,8.85968173251461));
#382945=CARTESIAN_POINT('Ctrl Pts',(1.45556304038866,2.23206184478649,8.85952137522076));
#382946=CARTESIAN_POINT('Ctrl Pts',(1.45573136976942,2.23201133351792,8.85934740853961));
#382947=CARTESIAN_POINT('Ctrl Pts',(1.4558921647566,2.23196947495596,8.8591675900182));
#382948=CARTESIAN_POINT('Ctrl Pts',(1.45653784020969,2.23180139107203,8.85844552518695));
#382949=CARTESIAN_POINT('Ctrl Pts',(1.45709775787567,2.23176039886351,8.85759444184125));
#382950=CARTESIAN_POINT('Ctrl Pts',(1.45755728671856,2.23176798161147,8.8568349891514));
#382951=CARTESIAN_POINT('Ctrl Pts',(1.45760537518814,2.23176877512585,8.85675551444999));
#382952=CARTESIAN_POINT('Ctrl Pts',(1.45765236006119,2.23177012010279,8.85667699793651));
#382953=CARTESIAN_POINT('Ctrl Pts',(1.45769822112842,2.23177193923716,8.85659965593547));
#382954=CARTESIAN_POINT('Ctrl Pts',(1.45831725615402,2.23179649400577,8.85555568965886));
#382955=CARTESIAN_POINT('Ctrl Pts',(1.45890864097158,2.23190949356634,8.85434650606346));
#382956=CARTESIAN_POINT('Ctrl Pts',(1.45947646544067,2.23210539222272,8.85297329937117));
#382957=CARTESIAN_POINT('Ctrl Pts',(1.45979583210649,2.23221557328066,8.85220095427747));
#382958=CARTESIAN_POINT('Ctrl Pts',(1.46010777345562,2.2323523213329,8.85137579139183));
#382959=CARTESIAN_POINT('Ctrl Pts',(1.46041276049031,2.2325170979263,8.85049129520029));
#382960=CARTESIAN_POINT('Origin',(1.45714482817987,2.23856575425762,7.59394543036555));
#382961=CARTESIAN_POINT('Ctrl Pts',(1.45024690539914,2.2385450688874,7.59443877723642));
#382962=CARTESIAN_POINT('Ctrl Pts',(1.44979219759188,2.23277216368648,7.58783886950015));
#382963=CARTESIAN_POINT('Ctrl Pts',(1.45787199014354,2.23016522412854,7.58559994247159));
#382964=CARTESIAN_POINT('Ctrl Pts',(1.45272914197842,2.27005918900933,7.56670252222137));
#382965=CARTESIAN_POINT('Ctrl Pts',(1.45227509135303,2.26429462729542,7.56004874999031));
#382966=CARTESIAN_POINT('Ctrl Pts',(1.46039619893559,2.26165190731612,7.55786368756704));
#382967=CARTESIAN_POINT('Ctrl Pts',(1.45520674322889,2.30151445966059,7.53888913333558));
#382968=CARTESIAN_POINT('Ctrl Pts',(1.4547499941584,2.29571563887413,7.53222002137277));
#382969=CARTESIAN_POINT('Ctrl Pts',(1.46291462079657,2.29308100102818,7.53005029815327));
#382970=CARTESIAN_POINT('Ctrl Pts',(1.45767959703743,2.33290945746887,7.51101258149734));
#382971=CARTESIAN_POINT('Ctrl Pts',(1.45721731133828,2.32704034443777,7.5043616886572));
#382972=CARTESIAN_POINT('Ctrl Pts',(1.46542721367564,2.32445094582891,7.50217374673251));
#382973=CARTESIAN_POINT('',(1.46529313746767,2.32277700535967,7.50366116523517));
#382974=CARTESIAN_POINT('Ctrl Pts',(1.45700592305909,2.32435658911882,7.51860402984325));
#382975=CARTESIAN_POINT('Ctrl Pts',(1.45704059954239,2.32479683678467,7.51734760759494));
#382976=CARTESIAN_POINT('Ctrl Pts',(1.45713124780418,2.3251899916557,7.51608817408573));
#382977=CARTESIAN_POINT('Ctrl Pts',(1.4572906716018,2.32553214927377,7.5148100591312));
#382978=CARTESIAN_POINT('Ctrl Pts',(1.45743508148724,2.32584208382035,7.51365231206384));
#382979=CARTESIAN_POINT('Ctrl Pts',(1.45763589966002,2.3261107167927,7.51247773061043));
#382980=CARTESIAN_POINT('Ctrl Pts',(1.45791922593487,2.32631129114239,7.51129758471022));
#382981=CARTESIAN_POINT('Ctrl Pts',(1.45827136813743,2.32656058215259,7.50983079813402));
#382982=CARTESIAN_POINT('Ctrl Pts',(1.45874725305973,2.3266861520984,7.50839324291155));
#382983=CARTESIAN_POINT('Ctrl Pts',(1.45937138700825,2.32660920611061,7.50715379678855));
#382984=CARTESIAN_POINT('Ctrl Pts',(1.45965971890848,2.3265736592814,7.50658120839351));
#382985=CARTESIAN_POINT('Ctrl Pts',(1.46001951610518,2.32648040840139,7.50598221009429));
#382986=CARTESIAN_POINT('Ctrl Pts',(1.46043650913798,2.32630965373253,7.50545747549611));
#382987=CARTESIAN_POINT('Ctrl Pts',(1.46065902952742,2.32621853375587,7.50517746087247));
#382988=CARTESIAN_POINT('Ctrl Pts',(1.46090032677017,2.32610454297667,7.50491486231392));
#382989=CARTESIAN_POINT('Ctrl Pts',(1.46115329842596,2.32596919186967,7.50468370960992));
#382990=CARTESIAN_POINT('Ctrl Pts',(1.46153157084674,2.3257667992706,7.50433806340446));
#382991=CARTESIAN_POINT('Ctrl Pts',(1.46194702721951,2.32551008583305,7.50405484070984));
#382992=CARTESIAN_POINT('Ctrl Pts',(1.46237131075486,2.32521573129308,7.50385766036131));
#382993=CARTESIAN_POINT('Ctrl Pts',(1.46241668128411,2.32518425465034,7.50383657498791));
#382994=CARTESIAN_POINT('Ctrl Pts',(1.46246214090838,2.32515237335348,7.50381643264937));
#382995=CARTESIAN_POINT('Ctrl Pts',(1.46250764664087,2.32512012665496,7.50379723213559));
#382996=CARTESIAN_POINT('Ctrl Pts',(1.46281141229124,2.3249048693937,7.50366906242519));
#382997=CARTESIAN_POINT('Ctrl Pts',(1.46312342439225,2.32466806081159,7.50358235568538));
#382998=CARTESIAN_POINT('Ctrl Pts',(1.46341867889314,2.32443257728237,7.5035341175365));
#382999=CARTESIAN_POINT('Ctrl Pts',(1.46386137960088,2.32407949638188,7.50346178989176));
#383000=CARTESIAN_POINT('Ctrl Pts',(1.46432261222972,2.3236808385577,7.50346967198527));
#383001=CARTESIAN_POINT('Ctrl Pts',(1.46476335765927,2.32327554780209,7.50354272648692));
#383002=CARTESIAN_POINT('Ctrl Pts',(1.46494464537733,2.32310884332528,7.50357277531559));
#383003=CARTESIAN_POINT('Ctrl Pts',(1.465122322082,2.32294134252926,7.50361331098761));
#383004=CARTESIAN_POINT('Ctrl Pts',(1.46529313746842,2.32277700536087,7.50366116523658));
#383005=CARTESIAN_POINT('',(1.45874211355528,2.24101961352507,7.57603338622103));
#383006=CARTESIAN_POINT('Origin',(1.4635653631209,2.24842419003007,7.5848687342763));
#383007=CARTESIAN_POINT('Ctrl Pts',(1.46529313746688,2.32277700541701,7.50366116529968));
#383008=CARTESIAN_POINT('Ctrl Pts',(1.46311385930741,2.29556894511304,7.52783573079709));
#383009=CARTESIAN_POINT('Ctrl Pts',(1.46093030563638,2.26831776646581,7.55196141284069));
#383010=CARTESIAN_POINT('Ctrl Pts',(1.4587421132987,2.24101961475055,7.57603338728831));
#383011=CARTESIAN_POINT('Ctrl Pts',(1.45054708277063,2.24011702507157,7.59639677331369));
#383012=CARTESIAN_POINT('Ctrl Pts',(1.44604747589547,2.22151724109334,7.59974925422225));
#383013=CARTESIAN_POINT('Ctrl Pts',(1.46123398723744,2.23316062115794,7.59639677331374));
#383014=CARTESIAN_POINT('Ctrl Pts',(1.44903241888635,2.2365224600907,7.58707626057419));
#383015=CARTESIAN_POINT('Ctrl Pts',(1.45166892345315,2.23015329411148,7.58811717123965));
#383016=CARTESIAN_POINT('Ctrl Pts',(1.45856018235537,2.2303205733527,7.58707626057427));
#383017=CARTESIAN_POINT('Ctrl Pts',(1.45468954949523,2.23874113211159,7.58015376756928));
#383018=CARTESIAN_POINT('Ctrl Pts',(1.4554393233935,2.23594564091327,7.58208760766041));
#383019=CARTESIAN_POINT('Ctrl Pts',(1.4582990518177,2.23639160646932,7.58015376756931));
#383020=CARTESIAN_POINT('Ctrl Pts',(1.45874211310364,2.2410196128316,7.57603338509286));
#383021=CARTESIAN_POINT('Ctrl Pts',(1.45874211310364,2.2410196128316,7.57603338509286));
#383022=CARTESIAN_POINT('Ctrl Pts',(1.45874211310364,2.2410196128316,7.57603338509286));
#383023=CARTESIAN_POINT('Origin',(1.46356058069556,2.24842730304488,7.58486873427623));
#383024=CARTESIAN_POINT('Ctrl Pts',(1.54322129228843,2.27725640229735,7.51098857897448));
#383025=CARTESIAN_POINT('Ctrl Pts',(1.53804160317609,2.27445795046259,7.50433767179956));
#383026=CARTESIAN_POINT('Ctrl Pts',(1.53235058273387,2.28091707868618,7.50214974420965));
#383027=CARTESIAN_POINT('Ctrl Pts',(1.51550631077543,2.2622827158109,7.53887321589169));
#383028=CARTESIAN_POINT('Ctrl Pts',(1.51038868353094,2.25951779439551,7.53220407452062));
#383029=CARTESIAN_POINT('Ctrl Pts',(1.50467460613785,2.26591718807518,7.53003438070911));
#383030=CARTESIAN_POINT('Ctrl Pts',(1.4877381062743,2.24728027432284,7.56669465659234));
#383031=CARTESIAN_POINT('Ctrl Pts',(1.48265072325537,2.24453169307895,7.56004085833301));
#383032=CARTESIAN_POINT('Ctrl Pts',(1.47694687288308,2.25088800813224,7.55785582193788));
#383033=CARTESIAN_POINT('Ctrl Pts',(1.45991793462975,2.23224975633353,7.59443891967696));
#383034=CARTESIAN_POINT('Ctrl Pts',(1.45482317553885,2.22949718998903,7.58783901202978));
#383035=CARTESIAN_POINT('Ctrl Pts',(1.449168791725,2.23583020835897,7.58560008491213));
#383036=CARTESIAN_POINT('',(1.53085035931323,2.28010398287623,7.50366116523517));
#383037=CARTESIAN_POINT('Ctrl Pts',(1.53085035931343,2.28010398287654,7.50366116523554));
#383038=CARTESIAN_POINT('Ctrl Pts',(1.53155169493517,2.27981716261496,7.50350835821027));
#383039=CARTESIAN_POINT('Ctrl Pts',(1.53218706119348,2.27953068795824,7.50345484956));
#383040=CARTESIAN_POINT('Ctrl Pts',(1.53277559486934,2.27923658921162,7.50349758195598));
#383041=CARTESIAN_POINT('Ctrl Pts',(1.53307755629185,2.27908569474368,7.50351950684424));
#383042=CARTESIAN_POINT('Ctrl Pts',(1.53339700966224,2.27891803629775,7.50357029184312));
#383043=CARTESIAN_POINT('Ctrl Pts',(1.53370061085855,2.27874789763523,7.50365515313924));
#383044=CARTESIAN_POINT('Ctrl Pts',(1.53416767243874,2.27848615547632,7.50378570417639));
#383045=CARTESIAN_POINT('Ctrl Pts',(1.53461109666587,2.27821116305176,7.50400001621911));
#383046=CARTESIAN_POINT('Ctrl Pts',(1.53499593592695,2.27794192178181,7.50428903009635));
#383047=CARTESIAN_POINT('Ctrl Pts',(1.53503865012416,2.27791203807227,7.50432110841318));
#383048=CARTESIAN_POINT('Ctrl Pts',(1.5350806729107,2.27788222500583,7.50435406373354));
#383049=CARTESIAN_POINT('Ctrl Pts',(1.53512197887439,2.277852508107,7.50438785222352));
#383050=CARTESIAN_POINT('Ctrl Pts',(1.53537417163686,2.27767107215592,7.50459414719561));
#383051=CARTESIAN_POINT('Ctrl Pts',(1.53560335743637,2.27748991372872,7.50483629897752));
#383052=CARTESIAN_POINT('Ctrl Pts',(1.53580157232053,2.27731700539469,7.5050991045531));
#383053=CARTESIAN_POINT('Ctrl Pts',(1.53623885426378,2.27693555224282,7.50567888004914));
#383054=CARTESIAN_POINT('Ctrl Pts',(1.53654297792573,2.27657961193306,7.50637912803145));
#383055=CARTESIAN_POINT('Ctrl Pts',(1.5367418703485,2.27626243205668,7.50710440483569));
#383056=CARTESIAN_POINT('Ctrl Pts',(1.53679064271913,2.27618465325409,7.50728225710685));
#383057=CARTESIAN_POINT('Ctrl Pts',(1.53683418180228,2.27610773442094,7.50746498566955));
#383058=CARTESIAN_POINT('Ctrl Pts',(1.53687183379768,2.27603367630524,7.50764697238949));
#383059=CARTESIAN_POINT('Ctrl Pts',(1.53707424056282,2.27563556025657,7.50862528291182));
#383060=CARTESIAN_POINT('Ctrl Pts',(1.53712858336449,2.27528585019077,7.50965856837421));
#383061=CARTESIAN_POINT('Ctrl Pts',(1.53710069976791,2.27497674797687,7.51067959873202));
#383062=CARTESIAN_POINT('Ctrl Pts',(1.53708535538955,2.27480664863868,7.51124147302578));
#383063=CARTESIAN_POINT('Ctrl Pts',(1.53704467387375,2.27464884415314,7.51180065547253));
#383064=CARTESIAN_POINT('Ctrl Pts',(1.53698693264453,2.27450237756294,7.51235175716501));
#383065=CARTESIAN_POINT('Ctrl Pts',(1.5367874136962,2.27399627714843,7.51425603304537));
#383066=CARTESIAN_POINT('Ctrl Pts',(1.53635477473427,2.27356742990723,7.51626900505183));
#383067=CARTESIAN_POINT('Ctrl Pts',(1.53574915221222,2.27322096169133,7.51827788969247));
#383068=CARTESIAN_POINT('Ctrl Pts',(1.53571637477686,2.27320221017675,7.51838661432547));
#383069=CARTESIAN_POINT('Ctrl Pts',(1.53568308088394,2.27318370197148,7.51849533314857));
#383070=CARTESIAN_POINT('Ctrl Pts',(1.53564927699518,2.27316543860616,7.51860402984325));
#383071=CARTESIAN_POINT('Ctrl Pts',(1.45874211478058,2.24101961378738,7.57603338728984));
#383072=CARTESIAN_POINT('Ctrl Pts',(1.48281814548955,2.25407036159789,7.55196141284921));
#383073=CARTESIAN_POINT('Ctrl Pts',(1.50685310110153,2.26709785384546,7.52783573083104));
#383074=CARTESIAN_POINT('Ctrl Pts',(1.53085035936762,2.28010398289953,7.50366116530176));
#383075=CARTESIAN_POINT('Origin',(5.04062831473859E-16,7.74375868966282E-16,
7.49482233047033));
#383076=CARTESIAN_POINT('Origin',(1.46057722850546,2.31530136474095,7.49482233047033));
#383077=CARTESIAN_POINT('Origin',(0.,0.,7.50366116523517));
#383078=CARTESIAN_POINT('Origin',(1.52592346056192,2.27276568139057,7.49482233047033));
#383079=CARTESIAN_POINT('Ctrl Pts',(1.45700583995948,2.32435553466796,7.51860402984325));
#383080=CARTESIAN_POINT('Ctrl Pts',(1.45760395760191,2.33194095102541,7.51860402984325));
#383081=CARTESIAN_POINT('Ctrl Pts',(1.4511406126304,2.33595610454792,7.51860402984325));
#383082=CARTESIAN_POINT('Ctrl Pts',(1.45722792385509,2.32717205162695,7.51041458714365));
#383083=CARTESIAN_POINT('Ctrl Pts',(1.45607271192432,2.33289217847477,7.51004642900443));
#383084=CARTESIAN_POINT('Ctrl Pts',(1.4511388301166,2.33595721187959,7.5072913648301));
#383085=CARTESIAN_POINT('Ctrl Pts',(1.45993819904963,2.32793241046927,7.50215815450138));
#383086=CARTESIAN_POINT('Ctrl Pts',(1.45919055500405,2.33095550372991,7.49877163671529));
#383087=CARTESIAN_POINT('Ctrl Pts',(1.45627247511123,2.33279635498231,7.4948158853317));
#383088=CARTESIAN_POINT('Ctrl Pts',(1.46529284374238,2.32277653974658,7.50366171572174));
#383089=CARTESIAN_POINT('Ctrl Pts',(1.46724653091906,2.32587351709116,7.50000045605858));
#383090=CARTESIAN_POINT('Ctrl Pts',(1.46724653091895,2.32587351709123,7.49482233047317));
#383091=CARTESIAN_POINT('Origin',(1.44454451893662,2.32533812225452,7.51860402984325));
#383092=CARTESIAN_POINT('Origin',(1.44454451893662,2.32533812225452,9.));
#383093=CARTESIAN_POINT('Origin',(1.44454451893662,2.32533812225452,8.75721825406948));
#383094=CARTESIAN_POINT('Ctrl Pts',(1.45569455202207,2.30770799497264,8.78942910404913));
#383095=CARTESIAN_POINT('Ctrl Pts',(1.45615226043134,2.31326163627486,8.79672699501691));
#383096=CARTESIAN_POINT('Ctrl Pts',(1.44754234110094,2.31561594617506,8.79893251111267));
#383097=CARTESIAN_POINT('Ctrl Pts',(1.45655786092529,2.31866838349121,8.78111911759576));
#383098=CARTESIAN_POINT('Ctrl Pts',(1.45709306086352,2.32525290102493,8.78644465894812));
#383099=CARTESIAN_POINT('Ctrl Pts',(1.44991412529163,2.32901832209436,8.78817647674131));
#383100=CARTESIAN_POINT('Ctrl Pts',(1.45709589559391,2.3254991590484,8.76780923932034));
#383101=CARTESIAN_POINT('Ctrl Pts',(1.45772259748296,2.33327231680525,8.76988516158375));
#383102=CARTESIAN_POINT('Ctrl Pts',(1.45138449933332,2.3373911627895,8.77093053738833));
#383103=CARTESIAN_POINT('Ctrl Pts',(1.45699098619532,2.32416725130065,8.75371302330491));
#383104=CARTESIAN_POINT('Ctrl Pts',(1.45760306669665,2.33174957012985,8.75300828287559));
#383105=CARTESIAN_POINT('Ctrl Pts',(1.45109726602121,2.33575819793819,8.75267964240738));
#383106=CARTESIAN_POINT('Origin',(1.44344342869435,2.31135883822903,8.78727029226991));
#383107=CARTESIAN_POINT('Ctrl Pts',(1.45029105591251,2.23910559748226,8.85049129520029));
#383108=CARTESIAN_POINT('Ctrl Pts',(1.45074959802196,2.24492718243456,8.85711686593484));
#383109=CARTESIAN_POINT('Ctrl Pts',(1.44260408658464,2.24752552912785,8.85933012996512));
#383110=CARTESIAN_POINT('Ctrl Pts',(1.45216503745169,2.26289739872515,8.82945683644722));
#383111=CARTESIAN_POINT('Ctrl Pts',(1.45262738573788,2.26876730635237,8.83607469902389));
#383112=CARTESIAN_POINT('Ctrl Pts',(1.44444656216418,2.27133755306296,8.8382956714852));
#383113=CARTESIAN_POINT('Ctrl Pts',(1.45403622567028,2.28665373636973,8.80838214965002));
#383114=CARTESIAN_POINT('Ctrl Pts',(1.45450039859867,2.2925468093931,8.81501364461996));
#383115=CARTESIAN_POINT('Ctrl Pts',(1.44628690934866,2.29511340381665,8.81722098428721));
#383116=CARTESIAN_POINT('Ctrl Pts',(1.45590483281682,2.31037730509333,8.78727029226991));
#383117=CARTESIAN_POINT('Ctrl Pts',(1.45636908284586,2.31627135697544,8.79393457792714));
#383118=CARTESIAN_POINT('Ctrl Pts',(1.44812530550982,2.31885583959522,8.79610912703474));
#383119=CARTESIAN_POINT('Origin',(1.43782965179004,2.24008713061795,8.85049129520029));
#383120=CARTESIAN_POINT('Ctrl Pts',(1.46041276049031,2.2325170979263,8.85049129520029));
#383121=CARTESIAN_POINT('Ctrl Pts',(1.46555048104863,2.23529287523863,8.85711686593484));
#383122=CARTESIAN_POINT('Ctrl Pts',(1.47122360941498,2.22889628422053,8.85933012996512));
#383123=CARTESIAN_POINT('Ctrl Pts',(1.45586749327613,2.23006140780685,8.86332496987232));
#383124=CARTESIAN_POINT('Ctrl Pts',(1.45988689960006,2.22778187557852,8.86648636486736));
#383125=CARTESIAN_POINT('Ctrl Pts',(1.45849989529328,2.22204146436105,8.87206031107457));
#383126=CARTESIAN_POINT('Ctrl Pts',(1.44988263370187,2.23392032758735,8.86341338519876));
#383127=CARTESIAN_POINT('Ctrl Pts',(1.44614309960763,2.23665699625423,8.86654584966054));
#383128=CARTESIAN_POINT('Ctrl Pts',(1.44147517002643,2.23300534098411,8.87215952290714));
#383129=CARTESIAN_POINT('Ctrl Pts',(1.45029105591251,2.23910559748225,8.85049129520029));
#383130=CARTESIAN_POINT('Ctrl Pts',(1.45074959802196,2.24492718243456,8.85711686593484));
#383131=CARTESIAN_POINT('Ctrl Pts',(1.44260408658464,2.24752552912785,8.85933012996512));
#383132=CARTESIAN_POINT('Origin',(1.46635445560019,2.22151954096027,8.85049129520029));
#383133=CARTESIAN_POINT('Ctrl Pts',(1.5233121462109,2.26650000646725,8.78727029226991));
#383134=CARTESIAN_POINT('Ctrl Pts',(1.5285138209738,2.26931033657942,8.79393457792714));
#383135=CARTESIAN_POINT('Ctrl Pts',(1.53421404825534,2.26281827803709,8.79610912703474));
#383136=CARTESIAN_POINT('Ctrl Pts',(1.50237539655482,2.25518842304626,8.80838214965003));
#383137=CARTESIAN_POINT('Ctrl Pts',(1.50757620744593,2.25799828643089,8.81501364461988));
#383138=CARTESIAN_POINT('Ctrl Pts',(1.51324781742237,2.2515266828529,8.81722098428721));
#383139=CARTESIAN_POINT('Ctrl Pts',(1.48140972735871,2.24386121514703,8.82945683644723));
#383140=CARTESIAN_POINT('Ctrl Pts',(1.486590094104,2.24666003308934,8.8360746990239));
#383141=CARTESIAN_POINT('Ctrl Pts',(1.4922518212561,2.24021977780303,8.83829567148519));
#383142=CARTESIAN_POINT('Ctrl Pts',(1.46041276049031,2.2325170979263,8.85049129520029));
#383143=CARTESIAN_POINT('Ctrl Pts',(1.46555048104863,2.23529287523863,8.85711686593484));
#383144=CARTESIAN_POINT('Ctrl Pts',(1.47122360941498,2.22889628422053,8.85933012996512));
#383145=CARTESIAN_POINT('Origin',(1.52925384132078,2.25550244950121,8.78727029226991));
#383146=CARTESIAN_POINT('Ctrl Pts',(1.53548638015781,2.27307740869794,8.75374538247848));
#383147=CARTESIAN_POINT('Ctrl Pts',(1.5421657429184,2.27670101070422,8.75304829418601));
#383148=CARTESIAN_POINT('Ctrl Pts',(1.54846123506547,2.2723839026635,8.75272238421917));
#383149=CARTESIAN_POINT('Ctrl Pts',(1.53664770761177,2.2737048443191,8.76769408445021));
#383150=CARTESIAN_POINT('Ctrl Pts',(1.54349548185627,2.27741902563786,8.76974318093969));
#383151=CARTESIAN_POINT('Ctrl Pts',(1.54982261507513,2.2732976493494,8.7707786988043));
#383152=CARTESIAN_POINT('Ctrl Pts',(1.53069540464027,2.27048896676448,8.78108014887988));
#383153=CARTESIAN_POINT('Ctrl Pts',(1.53649683516816,2.27363994139629,8.78639403366325));
#383154=CARTESIAN_POINT('Ctrl Pts',(1.54284883455845,2.26862255368209,8.78812224174741));
#383155=CARTESIAN_POINT('Ctrl Pts',(1.52094089407098,2.26521885333375,8.78944554828685));
#383156=CARTESIAN_POINT('Ctrl Pts',(1.52582745292964,2.26787929693169,8.79673892988686));
#383157=CARTESIAN_POINT('Ctrl Pts',(1.53146141315399,2.26096828785146,8.79894799272499));
#383158=CARTESIAN_POINT('Origin',(1.54159097210506,2.26216788164013,8.75721825406948));
#383159=CARTESIAN_POINT('Origin',(1.54159097210506,2.26216788164013,9.));
#383160=CARTESIAN_POINT('Origin',(1.54159097210506,2.26216788164013,7.51860402984325));
#383161=CARTESIAN_POINT('Ctrl Pts',(1.53084992081512,2.28010332976117,7.50366195182967));
#383162=CARTESIAN_POINT('Ctrl Pts',(1.53289114759657,2.28314360687629,7.50000065167736));
#383163=CARTESIAN_POINT('Ctrl Pts',(1.53289114759667,2.28314360687623,7.49482233047108));
#383164=CARTESIAN_POINT('Ctrl Pts',(1.53773778419651,2.2772906552962,7.50215800491336));
#383165=CARTESIAN_POINT('Ctrl Pts',(1.54080605586926,2.2778295487147,7.49877273257261));
#383166=CARTESIAN_POINT('Ctrl Pts',(1.54367213946216,2.2759053030993,7.49481816995645));
#383167=CARTESIAN_POINT('Ctrl Pts',(1.53812892001263,2.2745055109345,7.51043025814043));
#383168=CARTESIAN_POINT('Ctrl Pts',(1.54382949412868,2.27576892366773,7.51006209594518));
#383169=CARTESIAN_POINT('Ctrl Pts',(1.54863229252764,2.27249598955576,7.50731281821701));
#383170=CARTESIAN_POINT('Ctrl Pts',(1.53564794729546,2.27316472009999,7.51860402984324));
#383171=CARTESIAN_POINT('Ctrl Pts',(1.54234218192173,2.27678248738924,7.51860402984324));
#383172=CARTESIAN_POINT('Ctrl Pts',(1.5486302002882,2.27249741534624,7.51860402984325));
#383173=CARTESIAN_POINT('Origin',(0.,0.,7.5));
#383174=CARTESIAN_POINT('Origin',(1.60045004741994,2.13436118528465,7.5));
#383175=CARTESIAN_POINT('',(1.60045004741994,2.13436118528465,7.59394543036555));
#383176=CARTESIAN_POINT('',(1.60045004741994,2.13436118528465,8.85049129520029));
#383177=CARTESIAN_POINT('',(1.60045004741994,2.13436118528465,7.5));
#383178=CARTESIAN_POINT('',(1.66539749203243,2.16424429481557,8.78727029226991));
#383179=CARTESIAN_POINT('Ctrl Pts',(1.60045004741994,2.13436118528465,8.85049129520029));
#383180=CARTESIAN_POINT('Ctrl Pts',(1.62213066475763,2.1443367011262,8.82945686509571));
#383181=CARTESIAN_POINT('Ctrl Pts',(1.64377905123605,2.15429738715723,8.80838212259895));
#383182=CARTESIAN_POINT('Ctrl Pts',(1.66539749203243,2.16424429481557,8.78727029226991));
#383183=CARTESIAN_POINT('',(1.67813633056178,2.17010558942601,8.75721825406948));
#383184=CARTESIAN_POINT('Origin',(1.6398006619417,2.15246710397366,8.75937679713116));
#383185=CARTESIAN_POINT('',(1.67813633056178,2.17010558942601,7.51860402984325));
#383186=CARTESIAN_POINT('',(1.67813633056178,2.17010558942601,7.5));
#383187=CARTESIAN_POINT('Ctrl Pts',(1.67813633056178,2.17010558942601,7.51860402984325));
#383188=CARTESIAN_POINT('Ctrl Pts',(1.66813195416113,2.16550245411326,7.52834476460825));
#383189=CARTESIAN_POINT('Ctrl Pts',(1.65812108306368,2.16089633051148,7.53807742314407));
#383190=CARTESIAN_POINT('Ctrl Pts',(1.64810349920135,2.1562871182849,7.54780169004674));
#383191=CARTESIAN_POINT('Ctrl Pts',(1.63223618776763,2.14898637522467,7.5632044032688));
#383192=CARTESIAN_POINT('Ctrl Pts',(1.61635201469676,2.14167787391999,7.57858609112103));
#383193=CARTESIAN_POINT('Ctrl Pts',(1.60045004741994,2.13436118528465,7.59394543036555));
#383194=CARTESIAN_POINT('Origin',(1.62988553581354,2.41378875122107,7.5));
#383195=CARTESIAN_POINT('',(1.60293438610524,2.22623025921642,8.75721825406948));
#383196=CARTESIAN_POINT('',(1.60093990236827,2.21235024422327,8.78727029226991));
#383197=CARTESIAN_POINT('Origin',(1.59587715873839,2.17711758918247,8.75658640621021));
#383198=CARTESIAN_POINT('',(1.59077126558564,2.14158464790053,8.85049129520029));
#383199=CARTESIAN_POINT('Ctrl Pts',(1.60093990236827,2.21235024422327,8.78727029226991));
#383200=CARTESIAN_POINT('Ctrl Pts',(1.59755516454561,2.18879517036853,8.80838212259895));
#383201=CARTESIAN_POINT('Ctrl Pts',(1.59416573821263,2.16520746822395,8.82945686509571));
#383202=CARTESIAN_POINT('Ctrl Pts',(1.59077126558564,2.14158464790053,8.85049129520029));
#383203=CARTESIAN_POINT('',(1.59077126558564,2.14158464790053,7.59394543036555));
#383204=CARTESIAN_POINT('',(1.59077126558564,2.14158464790053,7.5));
#383205=CARTESIAN_POINT('',(1.60293438610524,2.22623025921642,7.51860402984325));
#383206=CARTESIAN_POINT('Ctrl Pts',(1.59077126558564,2.14158464790053,7.59394543036555));
#383207=CARTESIAN_POINT('Ctrl Pts',(1.59326099139906,2.1589111524884,7.57858609112103));
#383208=CARTESIAN_POINT('Ctrl Pts',(1.59574793122422,2.17621826882141,7.56320440326857));
#383209=CARTESIAN_POINT('Ctrl Pts',(1.59823223107079,2.19350701301058,7.54780169004651));
#383210=CARTESIAN_POINT('Ctrl Pts',(1.59980065570001,2.2044219966556,7.53807742314383));
#383211=CARTESIAN_POINT('Ctrl Pts',(1.60136802933074,2.21532966618996,7.52834476460825));
#383212=CARTESIAN_POINT('Ctrl Pts',(1.60293438610524,2.22623025921642,7.51860402984325));
#383213=CARTESIAN_POINT('',(1.60293438610524,2.22623025921642,7.5));
#383214=CARTESIAN_POINT('Origin',(1.59757636816866,2.14060679114483,7.5));
#383215=CARTESIAN_POINT('Ctrl Pts',(1.59077126558564,2.14158464790053,8.85049129520029));
#383216=CARTESIAN_POINT('Ctrl Pts',(1.59074372039119,2.1413929553312,8.85097269580138));
#383217=CARTESIAN_POINT('Ctrl Pts',(1.59072484862485,2.141202484932,8.85143669361005));
#383218=CARTESIAN_POINT('Ctrl Pts',(1.59071465132835,2.14100437995469,8.8519052845931));
#383219=CARTESIAN_POINT('Ctrl Pts',(1.5906947060631,2.14061689918243,8.85282181883899));
#383220=CARTESIAN_POINT('Ctrl Pts',(1.59070865627737,2.14021016853171,8.85372622499635));
#383221=CARTESIAN_POINT('Ctrl Pts',(1.59077213055141,2.13977833422802,8.8546225773507));
#383222=CARTESIAN_POINT('Ctrl Pts',(1.59082482463932,2.1394198407264,8.85536669723986));
#383223=CARTESIAN_POINT('Ctrl Pts',(1.59091163012185,2.1390439601235,8.85610498449051));
#383224=CARTESIAN_POINT('Ctrl Pts',(1.59104929334132,2.13864911207128,8.8568133821837));
#383225=CARTESIAN_POINT('Ctrl Pts',(1.5911742229292,2.13829078684378,8.85745625420284));
#383226=CARTESIAN_POINT('Ctrl Pts',(1.59134203885398,2.13791214894838,8.85808743050666));
#383227=CARTESIAN_POINT('Ctrl Pts',(1.59158132695242,2.13751236406796,8.8586680450841));
#383228=CARTESIAN_POINT('Ctrl Pts',(1.59169172929391,2.13732791199041,8.85893592806395));
#383229=CARTESIAN_POINT('Ctrl Pts',(1.59181758729019,2.13713898024249,8.85919241173848));
#383230=CARTESIAN_POINT('Ctrl Pts',(1.59196326236498,2.13694585159528,8.85943017985534));
#383231=CARTESIAN_POINT('Ctrl Pts',(1.59215996684039,2.13668507074934,8.8597512372));
#383232=CARTESIAN_POINT('Ctrl Pts',(1.59239832181033,2.13641038588146,8.86004599534705));
#383233=CARTESIAN_POINT('Ctrl Pts',(1.59268332992238,2.1361319232086,8.86026130871721));
#383234=CARTESIAN_POINT('Ctrl Pts',(1.59278767942742,2.13602997017337,8.86034014101235));
#383235=CARTESIAN_POINT('Ctrl Pts',(1.59289984160946,2.13592597046245,8.86040910639693));
#383236=CARTESIAN_POINT('Ctrl Pts',(1.5930169893838,2.1358230041511,8.86046313645507));
#383237=CARTESIAN_POINT('Ctrl Pts',(1.59319979750455,2.13566232608458,8.8605474499083));
#383238=CARTESIAN_POINT('Ctrl Pts',(1.59339983339584,2.13549988890018,8.86059655985668));
#383239=CARTESIAN_POINT('Ctrl Pts',(1.59360408347317,2.13534588276953,8.86059725258816));
#383240=CARTESIAN_POINT('Ctrl Pts',(1.59380880544978,2.13519152082319,8.86059794692011));
#383241=CARTESIAN_POINT('Ctrl Pts',(1.59402163099504,2.13504603837141,8.86056369958366));
#383242=CARTESIAN_POINT('Ctrl Pts',(1.59422882888186,2.13491426346685,8.86048590497774));
#383243=CARTESIAN_POINT('Ctrl Pts',(1.5942829013613,2.13487987414017,8.86046560290182));
#383244=CARTESIAN_POINT('Ctrl Pts',(1.59433734262764,2.13484604741781,8.86044257503091));
#383245=CARTESIAN_POINT('Ctrl Pts',(1.59439045307622,2.13481380069121,8.86041778462583));
#383246=CARTESIAN_POINT('Ctrl Pts',(1.59474782049062,2.13459682023609,8.860250975962));
#383247=CARTESIAN_POINT('Ctrl Pts',(1.59509305974972,2.13442254377126,8.8599848982295));
#383248=CARTESIAN_POINT('Ctrl Pts',(1.59541227620411,2.13428849451922,8.85968173251462));
#383249=CARTESIAN_POINT('Ctrl Pts',(1.59558112341956,2.134217590145,8.85952137522077));
#383250=CARTESIAN_POINT('Ctrl Pts',(1.59574587068147,2.13415639775679,8.85934740853961));
#383251=CARTESIAN_POINT('Ctrl Pts',(1.59590365341083,2.13410432302753,8.8591675900182));
#383252=CARTESIAN_POINT('Ctrl Pts',(1.59653723308303,2.13389521592165,8.85844552518695));
#383253=CARTESIAN_POINT('Ctrl Pts',(1.5970933739583,2.133818433888,8.85759444184124));
#383254=CARTESIAN_POINT('Ctrl Pts',(1.59755244447823,2.13379655894234,8.85683498915138));
#383255=CARTESIAN_POINT('Ctrl Pts',(1.59760048498554,2.13379426978753,8.85675551444998));
#383256=CARTESIAN_POINT('Ctrl Pts',(1.59764745949609,2.13379260166991,8.85667699793651));
#383257=CARTESIAN_POINT('Ctrl Pts',(1.59769334288918,2.13379147873802,8.85659965593547));
#383258=CARTESIAN_POINT('Ctrl Pts',(1.59831267927035,2.13377632134596,8.85555568965886));
#383259=CARTESIAN_POINT('Ctrl Pts',(1.59891008893107,2.13385119858146,8.85434650606346));
#383260=CARTESIAN_POINT('Ctrl Pts',(1.59948929801391,2.13401031410439,8.85297329937117));
#383261=CARTESIAN_POINT('Ctrl Pts',(1.59981506783128,2.13409980689099,8.85220095427747));
#383262=CARTESIAN_POINT('Ctrl Pts',(1.60013512974124,2.13421628782884,8.85137579139183));
#383263=CARTESIAN_POINT('Ctrl Pts',(1.60045004741994,2.13436118528465,8.85049129520029));
#383264=CARTESIAN_POINT('Origin',(1.59757636816866,2.14060679114483,7.59394543036555));
#383265=CARTESIAN_POINT('Ctrl Pts',(1.59069129259386,2.14102809970489,7.59443877723642));
#383266=CARTESIAN_POINT('Ctrl Pts',(1.5898676477264,2.13529618878609,7.58783886950016));
#383267=CARTESIAN_POINT('Ctrl Pts',(1.59776381228676,2.13217693137888,7.58559994247159));
#383268=CARTESIAN_POINT('Ctrl Pts',(1.59518754576058,2.17231843324348,7.56670252222136));
#383269=CARTESIAN_POINT('Ctrl Pts',(1.59436509129383,2.16659480656326,7.56004874999026));
#383270=CARTESIAN_POINT('Ctrl Pts',(1.60230019353944,2.16343719518632,7.55786368756704));
#383271=CARTESIAN_POINT('Ctrl Pts',(1.59967540262374,2.20355033521047,7.53888913333559));
#383272=CARTESIAN_POINT('Ctrl Pts',(1.59884806026979,2.19779269273671,7.53222002137282));
#383273=CARTESIAN_POINT('Ctrl Pts',(1.6068271099805,2.19464035861197,7.53005029815327));
#383274=CARTESIAN_POINT('Ctrl Pts',(1.60415466010479,2.23472239234116,7.51101258149734));
#383275=CARTESIAN_POINT('Ctrl Pts',(1.60331728885819,2.22889495677869,7.5043616886572));
#383276=CARTESIAN_POINT('Ctrl Pts',(1.6113444197322,2.2257848681182,7.50217374673251));
#383277=CARTESIAN_POINT('',(1.61110336926408,2.22412295723132,7.50366116523517));
#383278=CARTESIAN_POINT('Ctrl Pts',(1.60293438610524,2.22623025921642,7.51860402984325));
#383279=CARTESIAN_POINT('Ctrl Pts',(1.60299719810678,2.22666738061631,7.51734760759494));
#383280=CARTESIAN_POINT('Ctrl Pts',(1.60311284964106,2.22705391985441,7.51608817408573));
#383281=CARTESIAN_POINT('Ctrl Pts',(1.60329386799925,2.22738516015518,7.5148100591312));
#383282=CARTESIAN_POINT('Ctrl Pts',(1.60345783875367,2.22768520553486,7.51365231206384));
#383283=CARTESIAN_POINT('Ctrl Pts',(1.60367545569761,2.22794042010746,7.51247773061043));
#383284=CARTESIAN_POINT('Ctrl Pts',(1.60397105069095,2.22812242957887,7.51129758471022));
#383285=CARTESIAN_POINT('Ctrl Pts',(1.60433844150945,2.22834864656558,7.50983079813401));
#383286=CARTESIAN_POINT('Ctrl Pts',(1.60482139396919,2.22844346846281,7.50839324291155));
#383287=CARTESIAN_POINT('Ctrl Pts',(1.60543931562121,2.22832669216943,7.50715379678855));
#383288=CARTESIAN_POINT('Ctrl Pts',(1.60572477761946,2.22827274488671,7.50658120839351));
#383289=CARTESIAN_POINT('Ctrl Pts',(1.60607786096983,2.2281566333151,7.50598221009429));
#383290=CARTESIAN_POINT('Ctrl Pts',(1.60648305695653,2.22795951264467,7.50545747549611));
#383291=CARTESIAN_POINT('Ctrl Pts',(1.60669928207701,2.22785432295347,7.50517746087247));
#383292=CARTESIAN_POINT('Ctrl Pts',(1.6069327801344,2.22772510641314,7.50491486231392));
#383293=CARTESIAN_POINT('Ctrl Pts',(1.60717656005759,2.22757382544986,7.50468370960992));
#383294=CARTESIAN_POINT('Ctrl Pts',(1.60754108793877,2.22734761269088,7.50433806340446));
#383295=CARTESIAN_POINT('Ctrl Pts',(1.60793924302545,2.22706480831742,7.50405484070984));
#383296=CARTESIAN_POINT('Ctrl Pts',(1.60834379546465,2.22674387462099,7.50385766036131));
#383297=CARTESIAN_POINT('Ctrl Pts',(1.60838705605985,2.22670955575059,7.50383657498791));
#383298=CARTESIAN_POINT('Ctrl Pts',(1.60843037964074,2.22667482734915,7.50381643264937));
#383299=CARTESIAN_POINT('Ctrl Pts',(1.60847372582376,2.22663973134264,7.50379723213559));
#383300=CARTESIAN_POINT('Ctrl Pts',(1.60876307577494,2.22640545401847,7.50366906242519));
#383301=CARTESIAN_POINT('Ctrl Pts',(1.60905927443567,2.22614914130104,7.50358235568538));
#383302=CARTESIAN_POINT('Ctrl Pts',(1.60933883482301,2.22589522457716,7.5035341175365));
#383303=CARTESIAN_POINT('Ctrl Pts',(1.6097580039837,2.22551450518752,7.50346178989176));
#383304=CARTESIAN_POINT('Ctrl Pts',(1.61019274686614,2.2250871151726,7.50346967198527));
#383305=CARTESIAN_POINT('Ctrl Pts',(1.61060661966907,2.22465441847369,7.50354272648693));
#383306=CARTESIAN_POINT('Ctrl Pts',(1.61077685411957,2.22447644136514,7.50357277531559));
#383307=CARTESIAN_POINT('Ctrl Pts',(1.61094343395555,2.22429790093191,7.50361331098761));
#383308=CARTESIAN_POINT('Ctrl Pts',(1.61110336926491,2.22412295723247,7.50366116523659));
#383309=CARTESIAN_POINT('',(1.59932759105302,2.14295327026986,7.57603338622103));
#383310=CARTESIAN_POINT('Origin',(1.60461534358149,2.15003360661828,7.58486873427626));
#383311=CARTESIAN_POINT('Ctrl Pts',(1.61110336926697,2.22412295728859,7.50366116529968));
#383312=CARTESIAN_POINT('Ctrl Pts',(1.60718534225927,2.19711042569366,7.5278357307971));
#383313=CARTESIAN_POINT('Ctrl Pts',(1.6032602859228,2.17005513827967,7.55196141284068));
#383314=CARTESIAN_POINT('Ctrl Pts',(1.59932759087549,2.14295327150927,7.57603338728831));
#383315=CARTESIAN_POINT('Ctrl Pts',(1.59109156879722,2.1425775937061,7.59639677331372));
#383316=CARTESIAN_POINT('Ctrl Pts',(1.58540951459636,2.12430431578102,7.59974925422225));
#383317=CARTESIAN_POINT('Ctrl Pts',(1.6013108175438,2.13495077015054,7.59639677331371));
#383318=CARTESIAN_POINT('Ctrl Pts',(1.5893497123834,2.13908745899276,7.58707626057423));
#383319=CARTESIAN_POINT('Ctrl Pts',(1.59157272610353,2.13256245772059,7.58811717123966));
#383320=CARTESIAN_POINT('Ctrl Pts',(1.59846054379304,2.13228786879498,7.58707626057422));
#383321=CARTESIAN_POINT('Ctrl Pts',(1.59513737061503,2.14093911891167,7.5801537675693));
#383322=CARTESIAN_POINT('Ctrl Pts',(1.59570649628631,2.13810133317129,7.58208760766041));
#383323=CARTESIAN_POINT('Ctrl Pts',(1.59858892220311,2.138363159014,7.5801537675693));
#383324=CARTESIAN_POINT('Ctrl Pts',(1.59932759055788,2.14295326960676,7.57603338509286));
#383325=CARTESIAN_POINT('Ctrl Pts',(1.59932759055788,2.14295326960676,7.57603338509286));
#383326=CARTESIAN_POINT('Ctrl Pts',(1.59932759055788,2.14295326960676,7.57603338509286));
#383327=CARTESIAN_POINT('Origin',(1.60461077043304,2.15003701964786,7.5848687342762));
#383328=CARTESIAN_POINT('Ctrl Pts',(1.68595489728113,2.17370300710801,7.51098857897448));
#383329=CARTESIAN_POINT('Ctrl Pts',(1.68060655297094,2.17124216881354,7.50433767179956));
#383330=CARTESIAN_POINT('Ctrl Pts',(1.67534106310675,2.17805265099709,7.50214974420965));
#383331=CARTESIAN_POINT('Ctrl Pts',(1.65733749178292,2.16053579062865,7.53887321589164));
#383332=CARTESIAN_POINT('Ctrl Pts',(1.65205323012916,2.15810443754413,7.53220407452056));
#383333=CARTESIAN_POINT('Ctrl Pts',(1.64676090348175,2.16485678517878,7.53003438070911));
#383334=CARTESIAN_POINT('Ctrl Pts',(1.62866513030971,2.1473432882365,7.56669465659232));
#383335=CARTESIAN_POINT('Ctrl Pts',(1.62341209765988,2.1449263039967,7.56004085833299));
#383336=CARTESIAN_POINT('Ctrl Pts',(1.61812721696367,2.1516350062671,7.55785582193789));
#383337=CARTESIAN_POINT('Ctrl Pts',(1.59993910959752,2.13412609657559,7.59443891967696));
#383338=CARTESIAN_POINT('Ctrl Pts',(1.59467846070439,2.13170560800956,7.58783901202978));
#383339=CARTESIAN_POINT('Ctrl Pts',(1.58944145230862,2.13838789212886,7.58560008491213));
#383340=CARTESIAN_POINT('',(1.67379182682861,2.17733734542427,7.50366116523517));
#383341=CARTESIAN_POINT('Ctrl Pts',(1.67379182682884,2.17733734542457,7.50366116523554));
#383342=CARTESIAN_POINT('Ctrl Pts',(1.67447334484406,2.17700617973841,7.50350835821027));
#383343=CARTESIAN_POINT('Ctrl Pts',(1.67508905117998,2.17667958561866,7.50345484955999));
#383344=CARTESIAN_POINT('Ctrl Pts',(1.67565753267889,2.17634838364738,7.50349758195598));
#383345=CARTESIAN_POINT('Ctrl Pts',(1.67594920584752,2.17617845247354,7.50351950684424));
#383346=CARTESIAN_POINT('Ctrl Pts',(1.67625726095318,2.17599067105216,7.50357029184312));
#383347=CARTESIAN_POINT('Ctrl Pts',(1.67654933754674,2.17580143016233,7.50365515313924));
#383348=CARTESIAN_POINT('Ctrl Pts',(1.67699866962112,2.17551030104257,7.50378570417639));
#383349=CARTESIAN_POINT('Ctrl Pts',(1.67742356396048,2.17520746333167,7.50400001621911));
#383350=CARTESIAN_POINT('Ctrl Pts',(1.67779036218063,2.17491411851067,7.50428903009634));
#383351=CARTESIAN_POINT('Ctrl Pts',(1.6778310739611,2.1748815594924,7.50432110841318));
#383352=CARTESIAN_POINT('Ctrl Pts',(1.6778711002776,2.17484911527092,7.50435406373354));
#383353=CARTESIAN_POINT('Ctrl Pts',(1.67791041740551,2.17481681294647,7.50438785222352));
#383354=CARTESIAN_POINT('Ctrl Pts',(1.6781504673696,2.17461959172923,7.50459414719561));
#383355=CARTESIAN_POINT('Ctrl Pts',(1.67836757542203,2.17442412152687,7.50483629897752));
#383356=CARTESIAN_POINT('Ctrl Pts',(1.67855430477745,2.17423886878032,7.5050991045531));
#383357=CARTESIAN_POINT('Ctrl Pts',(1.6789662484907,2.17383018261457,7.50567888004914));
#383358=CARTESIAN_POINT('Ctrl Pts',(1.67924694212402,2.17345548835242,7.50637912803144));
#383359=CARTESIAN_POINT('Ctrl Pts',(1.67942510411653,2.17312621707483,7.50710440483569));
#383360=CARTESIAN_POINT('Ctrl Pts',(1.6794687929741,2.17304547322062,7.50728225710685));
#383361=CARTESIAN_POINT('Ctrl Pts',(1.67950731439497,2.17296592286683,7.50746498566954));
#383362=CARTESIAN_POINT('Ctrl Pts',(1.67954014411054,2.17288960453984,7.50764697238949));
#383363=CARTESIAN_POINT('Ctrl Pts',(1.67971662762646,2.17247933821732,7.50862528291182));
#383364=CARTESIAN_POINT('Ctrl Pts',(1.67974845277417,2.1721268649131,7.50965856837423));
#383365=CARTESIAN_POINT('Ctrl Pts',(1.67970082222059,2.17182018429101,7.51067959873204));
#383366=CARTESIAN_POINT('Ctrl Pts',(1.67967461106688,2.17165141755786,7.5112414730258));
#383367=CARTESIAN_POINT('Ctrl Pts',(1.67962390256752,2.17149654377222,7.51180065547253));
#383368=CARTESIAN_POINT('Ctrl Pts',(1.67955689582719,2.1713540776066,7.51235175716501));
#383369=CARTESIAN_POINT('Ctrl Pts',(1.67932536084705,2.17086180025259,7.51425603304536));
#383370=CARTESIAN_POINT('Ctrl Pts',(1.67886613445119,2.1704615533975,7.5162690050518));
#383371=CARTESIAN_POINT('Ctrl Pts',(1.67823955795076,2.17015459940593,7.51827788969243));
#383372=CARTESIAN_POINT('Ctrl Pts',(1.67820564644649,2.17013798647584,7.51838661432545));
#383373=CARTESIAN_POINT('Ctrl Pts',(1.67817123513466,2.1701216494447,7.51849533314856));
#383374=CARTESIAN_POINT('Ctrl Pts',(1.67813633056178,2.17010558942601,7.51860402984325));
#383375=CARTESIAN_POINT('Ctrl Pts',(1.59932759229262,2.14295327045313,7.57603338728985));
#383376=CARTESIAN_POINT('Ctrl Pts',(1.62419032049748,2.15443464751878,7.55196141284922));
#383377=CARTESIAN_POINT('Ctrl Pts',(1.64901056800951,2.16589544849306,7.52783573083105));
#383378=CARTESIAN_POINT('Ctrl Pts',(1.67379182688439,2.17733734544404,7.50366116530176));
#383379=CARTESIAN_POINT('Origin',(5.52641612598452E-16,7.40489414195308E-16,
7.49482233047033));
#383380=CARTESIAN_POINT('Origin',(1.60591818370368,2.21696482544263,7.49482233047033));
#383381=CARTESIAN_POINT('Origin',(0.,0.,7.50366116523517));
#383382=CARTESIAN_POINT('Origin',(1.66840488432873,2.17032978875286,7.49482233047033));
#383383=CARTESIAN_POINT('Ctrl Pts',(1.60293423561746,2.22622921225625,7.51860402984325));
#383384=CARTESIAN_POINT('Ctrl Pts',(1.60401712365771,2.23376072203333,7.51860402984325));
#383385=CARTESIAN_POINT('Ctrl Pts',(1.59782431009108,2.23818173392644,7.51860402984325));
#383386=CARTESIAN_POINT('Ctrl Pts',(1.60333631807902,2.22902571341502,7.51041458714365));
#383387=CARTESIAN_POINT('Ctrl Pts',(1.60254996944052,2.23480810233128,7.5100464290044));
#383388=CARTESIAN_POINT('Ctrl Pts',(1.59782260218663,2.23818295318903,7.50729136483009));
#383389=CARTESIAN_POINT('Ctrl Pts',(1.60608974108079,2.22961086209063,7.50215815450138));
#383390=CARTESIAN_POINT('Ctrl Pts',(1.60553732340033,2.23267564580042,7.49877163671533));
#383391=CARTESIAN_POINT('Ctrl Pts',(1.6027431827603,2.23469967684714,7.49481588533172));
#383392=CARTESIAN_POINT('Ctrl Pts',(1.61110304631034,2.22412251139393,7.50366171572174));
#383393=CARTESIAN_POINT('Ctrl Pts',(1.61325114344693,2.22708795249922,7.50000045605858));
#383394=CARTESIAN_POINT('Ctrl Pts',(1.61325114344683,2.2270879524993,7.49482233047317));
#383395=CARTESIAN_POINT('Origin',(1.59056147231794,2.22800818059041,7.51860402984325));
#383396=CARTESIAN_POINT('Origin',(1.59056147231794,2.22800818059041,9.));
#383397=CARTESIAN_POINT('Origin',(1.59056147231794,2.22800818059041,8.75721825406948));
#383398=CARTESIAN_POINT('Ctrl Pts',(1.60055903033134,2.20969989122328,8.78942910404912));
#383399=CARTESIAN_POINT('Ctrl Pts',(1.60137162134951,2.21521279649536,8.79672699501691));
#383400=CARTESIAN_POINT('Ctrl Pts',(1.592930233175,2.21811390863888,8.79893251111267));
#383401=CARTESIAN_POINT('Ctrl Pts',(1.60212279997728,2.22058244805681,8.78111911759583));
#383402=CARTESIAN_POINT('Ctrl Pts',(1.60307877177669,2.22711914661526,8.78644465894814));
#383403=CARTESIAN_POINT('Ctrl Pts',(1.59615583745411,2.2313367872046,8.78817647674132));
#383404=CARTESIAN_POINT('Ctrl Pts',(1.60309737848857,2.22736471705347,8.76780923932029));
#383405=CARTESIAN_POINT('Ctrl Pts',(1.60422082067878,2.23508175109614,8.76988516158372));
#383406=CARTESIAN_POINT('Ctrl Pts',(1.59815964019983,2.23959821781225,8.77093053738833));
#383407=CARTESIAN_POINT('Ctrl Pts',(1.60290734901519,2.22604226742124,8.75371302330492));
#383408=CARTESIAN_POINT('Ctrl Pts',(1.60400397276683,2.23356979143084,8.75300828287559));
#383409=CARTESIAN_POINT('Ctrl Pts',(1.59776837262213,2.23798701116386,8.75267964240738));
#383410=CARTESIAN_POINT('Origin',(1.58856698858097,2.21412816559727,8.78727029226991));
#383411=CARTESIAN_POINT('Ctrl Pts',(1.59077126558564,2.14158464790053,8.85049129520029));
#383412=CARTESIAN_POINT('Ctrl Pts',(1.59160185579968,2.14736489288837,8.85711686593484));
#383413=CARTESIAN_POINT('Ctrl Pts',(1.58363955683344,2.15047978570935,8.85933012996512));
#383414=CARTESIAN_POINT('Ctrl Pts',(1.59416574276814,2.16520749992665,8.82945683644721));
#383415=CARTESIAN_POINT('Ctrl Pts',(1.59500322738313,2.17103572444269,8.83607469902388));
#383416=CARTESIAN_POINT('Ctrl Pts',(1.58700388846101,2.17412483747177,8.83829567148519));
#383417=CARTESIAN_POINT('Ctrl Pts',(1.59755516020867,2.18879514018688,8.80838214965002));
#383418=CARTESIAN_POINT('Ctrl Pts',(1.59839594992895,2.19464636559807,8.81501364461995));
#383419=CARTESIAN_POINT('Ctrl Pts',(1.59036377844284,2.19773392674117,8.81722098428721));
#383420=CARTESIAN_POINT('Ctrl Pts',(1.60093990236827,2.21235024422327,8.78727029226991));
#383421=CARTESIAN_POINT('Ctrl Pts',(1.6017808317465,2.21820244154216,8.79393457792714));
#383422=CARTESIAN_POINT('Ctrl Pts',(1.59371958050512,2.22130979469261,8.79610912703474));
#383423=CARTESIAN_POINT('Origin',(1.57839835179835,2.14336256927453,8.85049129520029));
#383424=CARTESIAN_POINT('Ctrl Pts',(1.60045004741994,2.13436118528465,8.85049129520029));
#383425=CARTESIAN_POINT('Ctrl Pts',(1.60575505664338,2.13680208457842,8.85711686593484));
#383426=CARTESIAN_POINT('Ctrl Pts',(1.61100669796541,2.13005515746019,8.85933012996512));
#383427=CARTESIAN_POINT('Ctrl Pts',(1.59575678233858,2.13220175691421,8.86332496987232));
#383428=CARTESIAN_POINT('Ctrl Pts',(1.59962188022982,2.12966938398193,8.86648636486737));
#383429=CARTESIAN_POINT('Ctrl Pts',(1.59786993626266,2.12402963272603,8.87206031107457));
#383430=CARTESIAN_POINT('Ctrl Pts',(1.59003146113941,2.13643619939961,8.86341338519876));
#383431=CARTESIAN_POINT('Ctrl Pts',(1.58647494928256,2.13940683805928,8.86654584966057));
#383432=CARTESIAN_POINT('Ctrl Pts',(1.58158264810683,2.13606176078166,8.87215952290715));
#383433=CARTESIAN_POINT('Ctrl Pts',(1.59077126558564,2.14158464790053,8.85049129520029));
#383434=CARTESIAN_POINT('Ctrl Pts',(1.59160185579968,2.14736489288837,8.85711686593484));
#383435=CARTESIAN_POINT('Ctrl Pts',(1.58363955683344,2.15047978570935,8.85933012996512));
#383436=CARTESIAN_POINT('Origin',(1.60567491878591,2.12300553826614,8.85049129520029));
#383437=CARTESIAN_POINT('Ctrl Pts',(1.66539749203243,2.16424429481557,8.78727029226991));
#383438=CARTESIAN_POINT('Ctrl Pts',(1.67076853786517,2.16671557835679,8.79393457792714));
#383439=CARTESIAN_POINT('Ctrl Pts',(1.67604110579947,2.15987164362914,8.79610912703474));
#383440=CARTESIAN_POINT('Ctrl Pts',(1.64377902353585,2.15429737441203,8.80838214965001));
#383441=CARTESIAN_POINT('Ctrl Pts',(1.64914917736843,2.15676824753312,8.81501364461993));
#383442=CARTESIAN_POINT('Ctrl Pts',(1.65439449734899,2.14994655925992,8.81722098428721));
#383443=CARTESIAN_POINT('Ctrl Pts',(1.62213069385382,2.14433671451371,8.82945683644722));
#383444=CARTESIAN_POINT('Ctrl Pts',(1.6274797378613,2.1467978747474,8.8360746990239));
#383445=CARTESIAN_POINT('Ctrl Pts',(1.63271720381481,2.1400081035522,8.8382956714852));
#383446=CARTESIAN_POINT('Ctrl Pts',(1.60045004741994,2.13436118528465,8.85049129520029));
#383447=CARTESIAN_POINT('Ctrl Pts',(1.60575505664338,2.13680208457842,8.85711686593484));
#383448=CARTESIAN_POINT('Ctrl Pts',(1.61100669796541,2.13005515746019,8.85933012996512));
#383449=CARTESIAN_POINT('Origin',(1.6706223633984,2.15288864779706,8.78727029226991));
#383450=CARTESIAN_POINT('Ctrl Pts',(1.67796812831783,2.17002817722088,8.75374538247848));
#383451=CARTESIAN_POINT('Ctrl Pts',(1.68486593258895,2.17321638590681,8.75304829418601));
#383452=CARTESIAN_POINT('Ctrl Pts',(1.69087189191036,2.16850479426082,8.75272238421917));
#383453=CARTESIAN_POINT('Ctrl Pts',(1.67916726963829,2.17057991720283,8.76769408445022));
#383454=CARTESIAN_POINT('Ctrl Pts',(1.6862389428103,2.1738477289355,8.76974318093972));
#383455=CARTESIAN_POINT('Ctrl Pts',(1.69228901876996,2.16932943963945,8.7707786988043));
#383456=CARTESIAN_POINT('Ctrl Pts',(1.67302115432923,2.16775201237431,8.78108014887987));
#383457=CARTESIAN_POINT('Ctrl Pts',(1.67901254883373,2.17052481406067,8.78639403366322));
#383458=CARTESIAN_POINT('Ctrl Pts',(1.68503003222545,2.1651107611094,8.78812224174741));
#383459=CARTESIAN_POINT('Ctrl Pts',(1.66294902812127,2.16311770059482,8.78944554828685));
#383460=CARTESIAN_POINT('Ctrl Pts',(1.66799600222723,2.16545959512505,8.79673892988687));
#383461=CARTESIAN_POINT('Ctrl Pts',(1.673175597004,2.15820181638323,8.79894799272499));
#383462=CARTESIAN_POINT('Origin',(1.68336120192775,2.1587499424075,8.75721825406948));
#383463=CARTESIAN_POINT('Origin',(1.68336120192775,2.1587499424075,9.));
#383464=CARTESIAN_POINT('Origin',(1.68336120192775,2.1587499424075,7.51860402984325));
#383465=CARTESIAN_POINT('Ctrl Pts',(1.67379134738622,2.17733672174578,7.50366195182966));
#383466=CARTESIAN_POINT('Ctrl Pts',(1.67602317147189,2.18023997043658,7.50000065167735));
#383467=CARTESIAN_POINT('Ctrl Pts',(1.67602317147199,2.18023997043651,7.49482233047108));
#383468=CARTESIAN_POINT('Ctrl Pts',(1.68048485024187,2.1740885193001,7.50215800491337));
#383469=CARTESIAN_POINT('Ctrl Pts',(1.68358134484128,2.17442972066327,7.49877273257265));
#383470=CARTESIAN_POINT('Ctrl Pts',(1.68631825291817,2.17232579801056,7.49481816995649));
#383471=CARTESIAN_POINT('Ctrl Pts',(1.68069673761558,2.17128403715843,7.51043025814042));
#383472=CARTESIAN_POINT('Ctrl Pts',(1.68646654642245,2.17217961703705,7.51006209594514));
#383473=CARTESIAN_POINT('Ctrl Pts',(1.69104977934847,2.16860569116931,7.50731281821698));
#383474=CARTESIAN_POINT('Ctrl Pts',(1.67813495755922,2.17010495759025,7.51860402984325));
#383475=CARTESIAN_POINT('Ctrl Pts',(1.68504722930856,2.17328639070348,7.51860402984324));
#383476=CARTESIAN_POINT('Ctrl Pts',(1.69104778275847,2.16860724808059,7.51860402984325));
#383477=CARTESIAN_POINT('Origin',(0.,0.,7.5));
#383478=CARTESIAN_POINT('Origin',(1.73391074180927,2.02743472471363,7.5));
#383479=CARTESIAN_POINT('',(1.73391074180927,2.02743472471363,7.59394543036555));
#383480=CARTESIAN_POINT('',(1.73391074180927,2.02743472471363,8.85049129520029));
#383481=CARTESIAN_POINT('',(1.73391074180927,2.02743472471363,7.5));
#383482=CARTESIAN_POINT('',(1.80063936233257,2.05309523912755,8.78727029226991));
#383483=CARTESIAN_POINT('Ctrl Pts',(1.73391074180927,2.02743472471362,8.85049129520029));
#383484=CARTESIAN_POINT('Ctrl Pts',(1.75618594748779,2.03600066286586,8.82945686509571));
#383485=CARTESIAN_POINT('Ctrl Pts',(1.77842803837959,2.04455386671526,8.80838212259896));
#383486=CARTESIAN_POINT('Ctrl Pts',(1.80063936233257,2.05309523912756,8.78727029226991));
#383487=CARTESIAN_POINT('',(1.81372756198698,2.05812831089272,8.75721825406948));
#383488=CARTESIAN_POINT('Origin',(1.77434055646696,2.04298224032222,8.75937679713133));
#383489=CARTESIAN_POINT('',(1.81372756198698,2.05812831089272,7.51860402984325));
#383490=CARTESIAN_POINT('',(1.81372756198698,2.05812831089272,7.5));
#383491=CARTESIAN_POINT('Ctrl Pts',(1.81372756198698,2.05812831089272,7.51860402984325));
#383492=CARTESIAN_POINT('Ctrl Pts',(1.80344881675852,2.05417561581191,7.52834476460825));
#383493=CARTESIAN_POINT('Ctrl Pts',(1.79316339871698,2.0502203546985,7.53807742314407));
#383494=CARTESIAN_POINT('Ctrl Pts',(1.78287108381379,2.04626244139451,7.54780169004674));
#383495=CARTESIAN_POINT('Ctrl Pts',(1.76656861325928,2.03999332062795,7.5632044032688));
#383496=CARTESIAN_POINT('Ctrl Pts',(1.75024881863924,2.0337175378859,7.57858609112103));
#383497=CARTESIAN_POINT('Ctrl Pts',(1.73391074180927,2.02743472471363,7.59394543036555));
#383498=CARTESIAN_POINT('Origin',(1.78118873745324,2.3044022385307,7.5));
#383499=CARTESIAN_POINT('',(1.74227604793053,2.118955871654,8.75721825406948));
#383500=CARTESIAN_POINT('',(1.73939636646036,2.10523216165206,8.78727029226991));
#383501=CARTESIAN_POINT('Origin',(1.7320866608215,2.07039626697888,8.75658640621061));
#383502=CARTESIAN_POINT('',(1.72471465490912,2.03526346763212,8.85049129520029));
#383503=CARTESIAN_POINT('Ctrl Pts',(1.73939636646036,2.10523216165206,8.78727029226991));
#383504=CARTESIAN_POINT('Ctrl Pts',(1.73450940418103,2.0819423451197,8.80838212259894));
#383505=CARTESIAN_POINT('Ctrl Pts',(1.72961567252273,2.05862026772972,8.82945686509571));
#383506=CARTESIAN_POINT('Ctrl Pts',(1.72471465490912,2.03526346763212,8.85049129520029));
#383507=CARTESIAN_POINT('',(1.72471465490912,2.03526346763212,7.59394543036555));
#383508=CARTESIAN_POINT('',(1.72471465490912,2.03526346763212,7.5));
#383509=CARTESIAN_POINT('',(1.74227604793053,2.118955871654,7.51860402984325));
#383510=CARTESIAN_POINT('Ctrl Pts',(1.72471465490912,2.03526346763212,7.59394543036555));
#383511=CARTESIAN_POINT('Ctrl Pts',(1.72830937827427,2.05239485577749,7.57858609112103));
#383512=CARTESIAN_POINT('Ctrl Pts',(1.73190007916553,2.06950707400214,7.56320440326857));
#383513=CARTESIAN_POINT('Ctrl Pts',(1.73548696839501,2.08660112697449,7.54780169004651));
#383514=CARTESIAN_POINT('Ctrl Pts',(1.73775149593084,2.09739319530396,7.53807742314383));
#383515=CARTESIAN_POINT('Ctrl Pts',(1.74001450601089,2.10817803188811,7.52834476460825));
#383516=CARTESIAN_POINT('Ctrl Pts',(1.74227604793053,2.118955871654,7.51860402984325));
#383517=CARTESIAN_POINT('',(1.74227604793053,2.118955871654,7.5));
#383518=CARTESIAN_POINT('Origin',(1.73144312418159,2.03385161556851,7.5));
#383519=CARTESIAN_POINT('Ctrl Pts',(1.72471465490912,2.03526346763211,8.85049129520029));
#383520=CARTESIAN_POINT('Ctrl Pts',(1.72467488452414,2.0350739337424,8.85097269580138));
#383521=CARTESIAN_POINT('Ctrl Pts',(1.72464384805149,2.03488506380328,8.85143669361005));
#383522=CARTESIAN_POINT('Ctrl Pts',(1.72462097907696,2.03468801919692,8.8519052845931));
#383523=CARTESIAN_POINT('Ctrl Pts',(1.72457624881307,2.034302612443,8.85282181883899));
#383524=CARTESIAN_POINT('Ctrl Pts',(1.72456411104286,2.03389582367072,8.85372622499635));
#383525=CARTESIAN_POINT('Ctrl Pts',(1.72459978718337,2.03346080980622,8.85462257735071));
#383526=CARTESIAN_POINT('Ctrl Pts',(1.72462940424812,2.03309967674615,8.85536669723986));
#383527=CARTESIAN_POINT('Ctrl Pts',(1.72469194862655,2.0327190067839,8.85610498449051));
#383528=CARTESIAN_POINT('Ctrl Pts',(1.72480403100062,2.0323161498766,8.85681338218371));
#383529=CARTESIAN_POINT('Ctrl Pts',(1.72490574593111,2.03195055660052,8.85745625420285));
#383530=CARTESIAN_POINT('Ctrl Pts',(1.72504895764682,2.03156194465407,8.85808743050666));
#383531=CARTESIAN_POINT('Ctrl Pts',(1.72526213979697,2.03114764993346,8.85866804508411));
#383532=CARTESIAN_POINT('Ctrl Pts',(1.72536049741983,2.03095650333018,8.85893592806396));
#383533=CARTESIAN_POINT('Ctrl Pts',(1.72547399192869,2.03075989601329,8.85919241173849));
#383534=CARTESIAN_POINT('Ctrl Pts',(1.72560699390351,2.03055783073551,8.85943017985534));
#383535=CARTESIAN_POINT('Ctrl Pts',(1.72578658594231,2.03028498279279,8.8597512372));
#383536=CARTESIAN_POINT('Ctrl Pts',(1.72600685206649,2.02999559083907,8.86004599534705));
#383537=CARTESIAN_POINT('Ctrl Pts',(1.7262734334341,2.02969943976519,8.86026130871721));
#383538=CARTESIAN_POINT('Ctrl Pts',(1.7263710363885,2.02959101050767,8.86034014101235));
#383539=CARTESIAN_POINT('Ctrl Pts',(1.72647630483695,2.02948003821963,8.86040910639692));
#383540=CARTESIAN_POINT('Ctrl Pts',(1.7265866148444,2.02936977777994,8.86046313645507));
#383541=CARTESIAN_POINT('Ctrl Pts',(1.72675875268719,2.02919771728723,8.8605474499083));
#383542=CARTESIAN_POINT('Ctrl Pts',(1.72694797019715,2.02902279750388,8.86059655985668));
#383543=CARTESIAN_POINT('Ctrl Pts',(1.72714193341413,2.02885602144796,8.86059725258816));
#383544=CARTESIAN_POINT('Ctrl Pts',(1.72733634476362,2.02868886007272,8.86059794692011));
#383545=CARTESIAN_POINT('Ctrl Pts',(1.72753941194329,2.02853004075074,8.86056369958366));
#383546=CARTESIAN_POINT('Ctrl Pts',(1.72773774127271,2.02838526137767,8.86048590497774));
#383547=CARTESIAN_POINT('Ctrl Pts',(1.72778949932271,2.0283474782719,8.86046560290182));
#383548=CARTESIAN_POINT('Ctrl Pts',(1.72784166144809,2.02831023298625,8.86044257503091));
#383549=CARTESIAN_POINT('Ctrl Pts',(1.72789259672069,2.02827464971589,8.86041778462583));
#383550=CARTESIAN_POINT('Ctrl Pts',(1.72823532789991,2.02803521846153,8.86025097596201));
#383551=CARTESIAN_POINT('Ctrl Pts',(1.72856869189649,2.02783918051111,8.8599848982295));
#383552=CARTESIAN_POINT('Ctrl Pts',(1.72887866392137,2.02768495440918,8.85968173251461));
#383553=CARTESIAN_POINT('Ctrl Pts',(1.72904262136326,2.02760337763736,8.85952137522076));
#383554=CARTESIAN_POINT('Ctrl Pts',(1.72920310952447,2.02753175558217,8.85934740853961));
#383555=CARTESIAN_POINT('Ctrl Pts',(1.72935723163293,2.02746967867185,8.8591675900182));
#383556=CARTESIAN_POINT('Ctrl Pts',(1.72997611200948,2.02722040760997,8.85844552518695));
#383557=CARTESIAN_POINT('Ctrl Pts',(1.7305261907919,2.02710815126501,8.85759444184122));
#383558=CARTESIAN_POINT('Ctrl Pts',(1.73098291656963,2.02705690851458,8.85683498915136));
#383559=CARTESIAN_POINT('Ctrl Pts',(1.7310307117059,2.02705154609722,8.85675551444996));
#383560=CARTESIAN_POINT('Ctrl Pts',(1.73107748282562,2.0270468717397,8.8566769979365));
#383561=CARTESIAN_POINT('Ctrl Pts',(1.73112319999986,2.0270428113559,8.85659965593547));
#383562=CARTESIAN_POINT('Ctrl Pts',(1.73174029275056,2.02698800408814,8.85555568965886));
#383563=CARTESIAN_POINT('Ctrl Pts',(1.73234127237002,2.02702445131195,8.85434650606346));
#383564=CARTESIAN_POINT('Ctrl Pts',(1.73292948597223,2.02714612986163,8.85297329937117));
#383565=CARTESIAN_POINT('Ctrl Pts',(1.73326032028309,2.02721456663184,8.85220095427747));
#383566=CARTESIAN_POINT('Ctrl Pts',(1.73358718755085,2.02731030181013,8.85137579139183));
#383567=CARTESIAN_POINT('Ctrl Pts',(1.73391074180927,2.02743472471362,8.85049129520029));
#383568=CARTESIAN_POINT('Origin',(1.73144312418159,2.03385161556851,7.59394543036555));
#383569=CARTESIAN_POINT('Ctrl Pts',(1.7245991880651,2.03471318681161,7.59443877723642));
#383570=CARTESIAN_POINT('Ctrl Pts',(1.72340999067088,2.02904582382638,7.58783886950016));
#383571=CARTESIAN_POINT('Ctrl Pts',(1.73109008020603,2.02542706626767,7.58559994247159));
#383572=CARTESIAN_POINT('Ctrl Pts',(1.73109098175055,2.06565115507456,7.56670252222133));
#383573=CARTESIAN_POINT('Ctrl Pts',(1.72990350308422,2.05999198303783,7.56004874999025));
#383574=CARTESIAN_POINT('Ctrl Pts',(1.73761999295571,2.05633245556569,7.55786368756704));
#383575=CARTESIAN_POINT('Ctrl Pts',(1.73757065265992,2.09653134977293,7.53888913333561));
#383576=CARTESIAN_POINT('Ctrl Pts',(1.73637611674972,2.09083854499971,7.53222002137279));
#383577=CARTESIAN_POINT('Ctrl Pts',(1.7441368019062,2.08718146821334,7.53005029815327));
#383578=CARTESIAN_POINT('Ctrl Pts',(1.74403790758368,2.12735237355687,7.51101258149734));
#383579=CARTESIAN_POINT('Ctrl Pts',(1.7428288917277,2.12159056164572,7.5043616886572));
#383580=CARTESIAN_POINT('Ctrl Pts',(1.75064026593579,2.11797256295503,7.50217374673251));
#383581=CARTESIAN_POINT('',(1.7502932317356,2.11632951079883,7.50366116523517));
#383582=CARTESIAN_POINT('Ctrl Pts',(1.74227604793053,2.118955871654,7.51860402984325));
#383583=CARTESIAN_POINT('Ctrl Pts',(1.74236673734232,2.11938807056234,7.51734760759493));
#383584=CARTESIAN_POINT('Ctrl Pts',(1.74250691691214,2.11976640579488,7.51608817408573));
#383585=CARTESIAN_POINT('Ctrl Pts',(1.74270878598764,2.12008536764089,7.51481005913119));
#383586=CARTESIAN_POINT('Ctrl Pts',(1.74289164382004,2.12037429090285,7.51365231206383));
#383587=CARTESIAN_POINT('Ctrl Pts',(1.74312516530044,2.12061503834427,7.51247773061042));
#383588=CARTESIAN_POINT('Ctrl Pts',(1.74343181434903,2.12077773502146,7.51129758471022));
#383589=CARTESIAN_POINT('Ctrl Pts',(1.7438129440958,2.12097994841054,7.50983079813402));
#383590=CARTESIAN_POINT('Ctrl Pts',(1.74430097953773,2.12104363261568,7.50839324291155));
#383591=CARTESIAN_POINT('Ctrl Pts',(1.74491014972063,2.12088750587554,7.50715379678855));
#383592=CARTESIAN_POINT('Ctrl Pts',(1.74519156879232,2.12081537982028,7.50658120839351));
#383593=CARTESIAN_POINT('Ctrl Pts',(1.74553648740115,2.12067688468441,7.50598221009429));
#383594=CARTESIAN_POINT('Ctrl Pts',(1.74592822130451,2.12045420802354,7.50545747549611));
#383595=CARTESIAN_POINT('Ctrl Pts',(1.74613726264064,2.12033538086481,7.50517746087247));
#383596=CARTESIAN_POINT('Ctrl Pts',(1.74636200201907,2.12019146954181,7.50491486231392));
#383597=CARTESIAN_POINT('Ctrl Pts',(1.74659558846566,2.12002488036819,7.50468370960992));
#383598=CARTESIAN_POINT('Ctrl Pts',(1.74694487388399,2.11977577700606,7.50433806340446));
#383599=CARTESIAN_POINT('Ctrl Pts',(1.74732409157993,2.11946804380052,7.50405484070983));
#383600=CARTESIAN_POINT('Ctrl Pts',(1.74770725053022,2.119121849733,7.5038576603613));
#383601=CARTESIAN_POINT('Ctrl Pts',(1.74774822342431,2.11908482965856,7.5038365749879));
#383602=CARTESIAN_POINT('Ctrl Pts',(1.74778923293593,2.11904739685899,7.50381643264937));
#383603=CARTESIAN_POINT('Ctrl Pts',(1.74783024145071,2.11900959576151,7.50379723213559));
#383604=CARTESIAN_POINT('Ctrl Pts',(1.74810398670169,2.1187572610702,7.50366906242519));
#383605=CARTESIAN_POINT('Ctrl Pts',(1.74838315477832,2.11848249746139,7.50358235568538));
#383606=CARTESIAN_POINT('Ctrl Pts',(1.7486458722785,2.11821119094114,7.5035341175365));
#383607=CARTESIAN_POINT('Ctrl Pts',(1.74903978743615,2.11780439751998,7.50346178989176));
#383608=CARTESIAN_POINT('Ctrl Pts',(1.74944625412043,2.11735003155157,7.50346967198527));
#383609=CARTESIAN_POINT('Ctrl Pts',(1.74983155360462,2.11689170695291,7.50354272648692));
#383610=CARTESIAN_POINT('Ctrl Pts',(1.74999003525769,2.11670318855872,7.50357277531559));
#383611=CARTESIAN_POINT('Ctrl Pts',(1.75014483371269,2.11651434214922,7.50361331098761));
#383612=CARTESIAN_POINT('Ctrl Pts',(1.7502932317365,2.11632951079992,7.50366116523659));
#383613=CARTESIAN_POINT('',(1.73334108842444,2.03608107236508,7.57603338622103));
#383614=CARTESIAN_POINT('Origin',(1.73907161540509,2.04280807393504,7.58486873427629));
#383615=CARTESIAN_POINT('Ctrl Pts',(1.75029323174215,2.1163295108558,7.50366116529969));
#383616=CARTESIAN_POINT('Ctrl Pts',(1.74465255589963,2.08962350825639,7.5278357307971));
#383617=CARTESIAN_POINT('Ctrl Pts',(1.73900212579611,2.06287528805497,7.55196141284068));
#383618=CARTESIAN_POINT('Ctrl Pts',(1.73334108832669,2.03608107361332,7.57603338728831));
#383619=CARTESIAN_POINT('Ctrl Pts',(1.72471465490912,2.03526346763212,7.59394543036555));
#383620=CARTESIAN_POINT('Ctrl Pts',(1.72212056626995,2.02290080857694,7.59394543036555));
#383621=CARTESIAN_POINT('Ctrl Pts',(1.73391074180927,2.02743472471363,7.59394543036555));
#383622=CARTESIAN_POINT('Ctrl Pts',(1.72423552539132,2.03298007808928,7.58587155981959));
#383623=CARTESIAN_POINT('Ctrl Pts',(1.72591197114046,2.02735440847488,7.58685956158229));
#383624=CARTESIAN_POINT('Ctrl Pts',(1.7317330902689,2.0265973080504,7.58587155981959));
#383625=CARTESIAN_POINT('Ctrl Pts',(1.72943302451169,2.03442249532769,7.57982961904598));
#383626=CARTESIAN_POINT('Ctrl Pts',(1.72981032546514,2.03193363728709,7.58148017275035));
#383627=CARTESIAN_POINT('Ctrl Pts',(1.73232749797677,2.03195839414114,7.57982961904596));
#383628=CARTESIAN_POINT('Ctrl Pts',(1.73334108788783,2.03608107173507,7.57603338509286));
#383629=CARTESIAN_POINT('Ctrl Pts',(1.73334108788783,2.03608107173507,7.57603338509286));
#383630=CARTESIAN_POINT('Ctrl Pts',(1.73334108788783,2.03608107173507,7.57603338509286));
#383631=CARTESIAN_POINT('Origin',(1.73906727032654,2.04281177295477,7.58486873427624));
#383632=CARTESIAN_POINT('Ctrl Pts',(1.82176055196472,2.06121740000463,7.51098857897448));
#383633=CARTESIAN_POINT('Ctrl Pts',(1.81626552995066,2.05910428736284,7.50433767179956));
#383634=CARTESIAN_POINT('Ctrl Pts',(1.81144720769179,2.06623813777423,7.50214974420965));
#383635=CARTESIAN_POINT('Ctrl Pts',(1.79235831753899,2.04991076044927,7.53887321589168));
#383636=CARTESIAN_POINT('Ctrl Pts',(1.78692913564057,2.04782296664701,7.53220407452062));
#383637=CARTESIAN_POINT('Ctrl Pts',(1.78208030704416,2.05490052139172,7.53003438070912));
#383638=CARTESIAN_POINT('Ctrl Pts',(1.76289961997714,2.03858240797512,7.56669465659235));
#383639=CARTESIAN_POINT('Ctrl Pts',(1.75750252353437,2.03650695264608,7.56004085833302));
#383640=CARTESIAN_POINT('Ctrl Pts',(1.75265832922257,2.04354047463692,7.55785582193789));
#383641=CARTESIAN_POINT('Ctrl Pts',(1.7333857915781,2.02723285491821,7.59443891967696));
#383642=CARTESIAN_POINT('Ctrl Pts',(1.72798087001744,2.02515439043736,7.58783901202978));
#383643=CARTESIAN_POINT('Ctrl Pts',(1.72318275703058,2.03215848136722,7.58560008491213));
#383644=CARTESIAN_POINT('',(1.80985532470034,2.06562356178257,7.50366116523517));
#383645=CARTESIAN_POINT('Ctrl Pts',(1.80985532470058,2.06562356178285,7.50366116523554));
#383646=CARTESIAN_POINT('Ctrl Pts',(1.81051422460559,2.06524941150296,7.50350835821027));
#383647=CARTESIAN_POINT('Ctrl Pts',(1.81110774094971,2.06488403996546,7.50345484956));
#383648=CARTESIAN_POINT('Ctrl Pts',(1.81165383425925,2.06451709574947,7.50349758195598));
#383649=CARTESIAN_POINT('Ctrl Pts',(1.81193402062638,2.06432882615337,7.50351950684424));
#383650=CARTESIAN_POINT('Ctrl Pts',(1.81222941160282,2.06412169339068,7.50357029184312));
#383651=CARTESIAN_POINT('Ctrl Pts',(1.81250876338825,2.06391412790495,7.50365515313923));
#383652=CARTESIAN_POINT('Ctrl Pts',(1.81293851955495,2.06359480813634,7.50378570417639));
#383653=CARTESIAN_POINT('Ctrl Pts',(1.81334313802456,2.0632653695642,7.50400001621911));
#383654=CARTESIAN_POINT('Ctrl Pts',(1.81369038795123,2.06294912660894,7.50428903009634));
#383655=CARTESIAN_POINT('Ctrl Pts',(1.81372893002151,2.06291402607393,7.50432110841318));
#383656=CARTESIAN_POINT('Ctrl Pts',(1.81376679539123,2.06287908401769,7.50435406373354));
#383657=CARTESIAN_POINT('Ctrl Pts',(1.81380396212085,2.06284432900479,7.50438785222351));
#383658=CARTESIAN_POINT('Ctrl Pts',(1.81403088286978,2.0626321329457,7.50459414719561));
#383659=CARTESIAN_POINT('Ctrl Pts',(1.81423502103156,2.06242315419715,7.50483629897752));
#383660=CARTESIAN_POINT('Ctrl Pts',(1.81440949754727,2.06222631828136,7.50509910455309));
#383661=CARTESIAN_POINT('Ctrl Pts',(1.81479441026544,2.06179207848083,7.50567888004914));
#383662=CARTESIAN_POINT('Ctrl Pts',(1.81505052043979,2.0614001699654,7.50637912803144));
#383663=CARTESIAN_POINT('Ctrl Pts',(1.81520721989618,2.06106016033292,7.50710440483569));
#383664=CARTESIAN_POINT('Ctrl Pts',(1.81524564571381,2.06097678322089,7.50728225710685));
#383665=CARTESIAN_POINT('Ctrl Pts',(1.81527899117963,2.06089492823593,7.50746498566954));
#383666=CARTESIAN_POINT('Ctrl Pts',(1.81530686371103,2.06081666330603,7.50764697238949));
#383667=CARTESIAN_POINT('Ctrl Pts',(1.8154566987691,2.06039593258198,7.50862528291182));
#383668=CARTESIAN_POINT('Ctrl Pts',(1.81546587548649,2.06004214442775,7.50965856837422));
#383669=CARTESIAN_POINT('Ctrl Pts',(1.81539869370007,2.05973914561394,7.51067959873203));
#383670=CARTESIAN_POINT('Ctrl Pts',(1.81536172347827,2.05957240498452,7.51124147302579));
#383671=CARTESIAN_POINT('Ctrl Pts',(1.81530119636744,2.0594210983084,7.51180065547253));
#383672=CARTESIAN_POINT('Ctrl Pts',(1.81522519946108,2.05928321799139,7.51235175716501));
#383673=CARTESIAN_POINT('Ctrl Pts',(1.81496259987602,2.05880678657111,7.51425603304535));
#383674=CARTESIAN_POINT('Ctrl Pts',(1.81447867310599,2.05843678480232,7.51626900505178));
#383675=CARTESIAN_POINT('Ctrl Pts',(1.81383371736442,2.05817060637486,7.51827788969241));
#383676=CARTESIAN_POINT('Ctrl Pts',(1.81379881114089,2.05815620029535,7.51838661432543));
#383677=CARTESIAN_POINT('Ctrl Pts',(1.81376342381361,2.05814210157072,7.51849533314856));
#383678=CARTESIAN_POINT('Ctrl Pts',(1.81372756198698,2.05812831089272,7.51860402984325));
#383679=CARTESIAN_POINT('Ctrl Pts',(1.73334108967323,2.03608107246855,7.57603338728985));
#383680=CARTESIAN_POINT('Ctrl Pts',(1.75888834909077,2.04594589934822,7.55196141284923));
#383681=CARTESIAN_POINT('Ctrl Pts',(1.78439189678191,2.05579291415965,7.52783573083105));
#383682=CARTESIAN_POINT('Ctrl Pts',(1.80985532475727,2.06562356179872,7.50366116530176));
#383683=CARTESIAN_POINT('Origin',(5.98949470795624E-16,7.03560129586924E-16,
7.49482233047033));
#383684=CARTESIAN_POINT('Origin',(1.74466007661669,2.10951830213911,7.49482233047033));
#383685=CARTESIAN_POINT('Origin',(0.,0.,7.50366116523517));
#383686=CARTESIAN_POINT('Origin',(1.80403047455411,2.05897554547889,7.49482233047033));
#383687=CARTESIAN_POINT('Ctrl Pts',(1.74227583067298,2.1189548364867,7.51860402984325));
#383688=CARTESIAN_POINT('Ctrl Pts',(1.74383903929182,2.12640149109425,7.51860402984325));
#383689=CARTESIAN_POINT('Ctrl Pts',(1.73794220472936,2.13121019447179,7.51860402984325));
#383690=CARTESIAN_POINT('Ctrl Pts',(1.74285625945742,2.12171983042216,7.51041458714366));
#383691=CARTESIAN_POINT('Ctrl Pts',(1.74244200538641,2.12754072033047,7.51004642900443));
#383692=CARTESIAN_POINT('Ctrl Pts',(1.73794057845241,2.13121152065508,7.5072913648301));
#383693=CARTESIAN_POINT('Ctrl Pts',(1.7456415158607,2.12212736442965,7.50215815450137));
#383694=CARTESIAN_POINT('Ctrl Pts',(1.74528659454809,2.12522124473493,7.49877163671529));
#383695=CARTESIAN_POINT('Ctrl Pts',(1.74262787488407,2.12742013839824,7.49481588533169));
#383696=CARTESIAN_POINT('Ctrl Pts',(1.75029288088051,2.11632908656918,7.50366171572174));
#383697=CARTESIAN_POINT('Ctrl Pts',(1.7526265609851,2.1191508058016,7.50000045605858));
#383698=CARTESIAN_POINT('Ctrl Pts',(1.752626560985,2.11915080580168,7.49482233047317));
#383699=CARTESIAN_POINT('Origin',(1.73004246743514,2.121522875406,7.51860402984325));
#383700=CARTESIAN_POINT('Origin',(1.73004246743514,2.121522875406,9.));
#383701=CARTESIAN_POINT('Origin',(1.73004246743514,2.121522875406,8.75721825406948));
#383702=CARTESIAN_POINT('Ctrl Pts',(1.73884646826614,2.10261165664175,8.78942910404913));
#383703=CARTESIAN_POINT('Ctrl Pts',(1.74001060278244,2.10806117217339,8.79672699501691));
#383704=CARTESIAN_POINT('Ctrl Pts',(1.73177243323848,2.11149716526816,8.79893251111267));
#383705=CARTESIAN_POINT('Ctrl Pts',(1.74110427278991,2.11337166302988,8.78111911759576));
#383706=CARTESIAN_POINT('Ctrl Pts',(1.74247708815731,2.11983368191662,8.78644465894812));
#383707=CARTESIAN_POINT('Ctrl Pts',(1.73583860290615,2.12448621083598,8.78817647674132));
#383708=CARTESIAN_POINT('Ctrl Pts',(1.7425113903917,2.12007755566787,8.76780923932034));
#383709=CARTESIAN_POINT('Ctrl Pts',(1.74412695641817,2.1277067550482,8.76988516158375));
#383710=CARTESIAN_POINT('Ctrl Pts',(1.73836760030061,2.1326022833657,8.77093053738832));
#383711=CARTESIAN_POINT('Ctrl Pts',(1.74223702171541,2.11876999838043,8.75371302330491));
#383712=CARTESIAN_POINT('Ctrl Pts',(1.74381368245515,2.12621179535963,8.75300828287559));
#383713=CARTESIAN_POINT('Ctrl Pts',(1.7378739062597,2.13101945571394,8.75267964240738));
#383714=CARTESIAN_POINT('Origin',(1.72716278596497,2.10779916540406,8.78727029226991));
#383715=CARTESIAN_POINT('Ctrl Pts',(1.72471465490912,2.03526346763212,8.85049129520029));
#383716=CARTESIAN_POINT('Ctrl Pts',(1.72591388015439,2.04097862038897,8.85711686593484));
#383717=CARTESIAN_POINT('Ctrl Pts',(1.71816751245359,2.0445972595749,8.85933012996512));
#383718=CARTESIAN_POINT('Ctrl Pts',(1.72961567910008,2.05862029907541,8.82945683644722));
#383719=CARTESIAN_POINT('Ctrl Pts',(1.73082485863995,2.06438289105559,8.83607469902389));
#383720=CARTESIAN_POINT('Ctrl Pts',(1.72303987536886,2.06797817657509,8.8382956714852));
#383721=CARTESIAN_POINT('Ctrl Pts',(1.73450939791925,2.08194231527792,8.80838214965001));
#383722=CARTESIAN_POINT('Ctrl Pts',(1.73572334944616,2.08772764913661,8.81501364461993));
#383723=CARTESIAN_POINT('Ctrl Pts',(1.72790550163944,2.09132348954826,8.81722098428721));
#383724=CARTESIAN_POINT('Ctrl Pts',(1.73939636646036,2.10523216165206,8.78727029226991));
#383725=CARTESIAN_POINT('Ctrl Pts',(1.74061051962858,2.11101845647366,8.79393457792714));
#383726=CARTESIAN_POINT('Ctrl Pts',(1.73276491989236,2.11463591137415,8.79610912703474));
#383727=CARTESIAN_POINT('Origin',(1.71248107441373,2.03783047138412,8.85049129520029));
#383728=CARTESIAN_POINT('Ctrl Pts',(1.73391074180927,2.02743472471362,8.85049129520029));
#383729=CARTESIAN_POINT('Ctrl Pts',(1.739361240277,2.02953071581006,8.85711686593484));
#383730=CARTESIAN_POINT('Ctrl Pts',(1.74416981443404,2.02246117716244,8.85933012996512));
#383731=CARTESIAN_POINT('Ctrl Pts',(1.72908876449365,2.02558043164656,8.86332496987232));
#383732=CARTESIAN_POINT('Ctrl Pts',(1.73278367143587,2.02280562407395,8.86648636486738));
#383733=CARTESIAN_POINT('Ctrl Pts',(1.7306739869219,2.01728970772722,8.87206031107457));
#383734=CARTESIAN_POINT('Ctrl Pts',(1.72364650824246,2.03017299660443,8.86341338519876));
#383735=CARTESIAN_POINT('Ctrl Pts',(1.72028763309304,2.03336539826537,8.86654584966054));
#383736=CARTESIAN_POINT('Ctrl Pts',(1.71519106383777,2.03034064462034,8.87215952290714));
#383737=CARTESIAN_POINT('Ctrl Pts',(1.72471465490912,2.03526346763211,8.85049129520029));
#383738=CARTESIAN_POINT('Ctrl Pts',(1.72591388015439,2.04097862038897,8.85711686593484));
#383739=CARTESIAN_POINT('Ctrl Pts',(1.71816751245359,2.0445972595749,8.85933012996512));
#383740=CARTESIAN_POINT('Origin',(1.73839731931416,2.01576765043201,8.85049129520029));
#383741=CARTESIAN_POINT('Ctrl Pts',(1.80063936233257,2.05309523912756,8.78727029226991));
#383742=CARTESIAN_POINT('Ctrl Pts',(1.80615770845572,2.05521732106367,8.79393457792714));
#383743=CARTESIAN_POINT('Ctrl Pts',(1.81098095093019,2.04804963334651,8.79610912703474));
#383744=CARTESIAN_POINT('Ctrl Pts',(1.77842800991972,2.04455385577101,8.80838214965003));
#383745=CARTESIAN_POINT('Ctrl Pts',(1.78394543957967,2.04667558528085,8.81501364461987));
#383746=CARTESIAN_POINT('Ctrl Pts',(1.78874291541949,2.03953184409283,8.81722098428722));
#383747=CARTESIAN_POINT('Ctrl Pts',(1.75618597738195,2.03600067436167,8.82945683644723));
#383748=CARTESIAN_POINT('Ctrl Pts',(1.76168171828239,2.03811406345147,8.8360746990239));
#383749=CARTESIAN_POINT('Ctrl Pts',(1.7664734011663,2.0310026769736,8.83829567148519));
#383750=CARTESIAN_POINT('Ctrl Pts',(1.73391074180927,2.02743472471362,8.85049129520029));
#383751=CARTESIAN_POINT('Ctrl Pts',(1.739361240277,2.02953071581006,8.85711686593484));
#383752=CARTESIAN_POINT('Ctrl Pts',(1.74416981443404,2.02246117716244,8.85933012996512));
#383753=CARTESIAN_POINT('Origin',(1.80512593983745,2.04142816484594,8.78727029226991));
#383754=CARTESIAN_POINT('Ctrl Pts',(1.81355474551558,2.05806183449404,8.75374538247848));
#383755=CARTESIAN_POINT('Ctrl Pts',(1.82064264673988,2.06080154882625,8.75304829418602));
#383756=CARTESIAN_POINT('Ctrl Pts',(1.82633439346051,2.0557148345157,8.75272238421917));
#383757=CARTESIAN_POINT('Ctrl Pts',(1.81478677317359,2.05853561161883,8.7676940844502));
#383758=CARTESIAN_POINT('Ctrl Pts',(1.82205328625122,2.06134362562606,8.7697431809397));
#383759=CARTESIAN_POINT('Ctrl Pts',(1.82780144389181,2.05644698994232,8.77077869880429));
#383760=CARTESIAN_POINT('Ctrl Pts',(1.80847210123317,2.05610729998395,8.78108014887988));
#383761=CARTESIAN_POINT('Ctrl Pts',(1.81462883978908,2.05849053468798,8.78639403366325));
#383762=CARTESIAN_POINT('Ctrl Pts',(1.82028708005223,2.0527020640045,8.78812224174742));
#383763=CARTESIAN_POINT('Ctrl Pts',(1.79812374791355,2.05212783323686,8.78944554828686));
#383764=CARTESIAN_POINT('Ctrl Pts',(1.80331039816766,2.05414155535239,8.79673892988686));
#383765=CARTESIAN_POINT('Ctrl Pts',(1.80801434343089,2.04656683071865,8.79894799272499));
#383766=CARTESIAN_POINT('Origin',(1.81821413949186,2.04646123661111,8.75721825406948));
#383767=CARTESIAN_POINT('Origin',(1.81821413949186,2.04646123661111,9.));
#383768=CARTESIAN_POINT('Origin',(1.81821413949186,2.04646123661111,7.51860402984325));
#383769=CARTESIAN_POINT('Ctrl Pts',(1.8098548062838,2.06562297010347,7.50366195182966));
#383770=CARTESIAN_POINT('Ctrl Pts',(1.8122680566298,2.06837726029834,7.50000065167735));
#383771=CARTESIAN_POINT('Ctrl Pts',(1.81226805662989,2.06837726029826,7.49482233047108));
#383772=CARTESIAN_POINT('Ctrl Pts',(1.81632644357471,2.06195258723767,7.50215800491338));
#383773=CARTESIAN_POINT('Ctrl Pts',(1.81943843694025,2.06209469447589,7.49877273257267));
#383774=CARTESIAN_POINT('Ctrl Pts',(1.8220349229588,2.05981974025537,7.49481816995647));
#383775=CARTESIAN_POINT('Ctrl Pts',(1.81635821181535,2.05914029153471,7.5104302581404));
#383776=CARTESIAN_POINT('Ctrl Pts',(1.82217354593104,2.05966435842891,7.51006209594513));
#383777=CARTESIAN_POINT('Ctrl Pts',(1.82651837989692,2.05580412683338,7.50731281821699));
#383778=CARTESIAN_POINT('Ctrl Pts',(1.81372615132356,2.05812776832371,7.51860402984325));
#383779=CARTESIAN_POINT('Ctrl Pts',(1.82082805618866,2.06085979406985,7.51860402984324));
#383780=CARTESIAN_POINT('Ctrl Pts',(1.82651648716078,2.05580580846778,7.51860402984325));
#383781=CARTESIAN_POINT('Origin',(0.,0.,7.5));
#383782=CARTESIAN_POINT('Origin',(1.86024642503782,1.91217709997537,7.5));
#383783=CARTESIAN_POINT('',(1.86024642503782,1.91217709997537,7.59394543036555));
#383784=CARTESIAN_POINT('',(1.86024642503782,1.91217709997537,8.85049129520029));
#383785=CARTESIAN_POINT('',(1.86024642503782,1.91217709997537,7.5));
#383786=CARTESIAN_POINT('',(1.92848201925695,1.93350957471442,8.78727029226991));
#383787=CARTESIAN_POINT('Ctrl Pts',(1.86024642503782,1.91217709997537,8.85049129520029));
#383788=CARTESIAN_POINT('Ctrl Pts',(1.88302468545901,1.91929826116104,8.82945686509571));
#383789=CARTESIAN_POINT('Ctrl Pts',(1.9057690832418,1.92640883587954,8.80838212259897));
#383790=CARTESIAN_POINT('Ctrl Pts',(1.92848201925695,1.93350957471442,8.78727029226991));
#383791=CARTESIAN_POINT('',(1.94186579781664,1.93769374166284,8.75721825406948));
#383792=CARTESIAN_POINT('Origin',(1.90158930505073,1.92510232442688,8.75937679713145));
#383793=CARTESIAN_POINT('',(1.94186579781664,1.93769374166284,7.51860402984325));
#383794=CARTESIAN_POINT('',(1.94186579781664,1.93769374166284,7.5));
#383795=CARTESIAN_POINT('Ctrl Pts',(1.94186579781664,1.93769374166284,7.51860402984325));
#383796=CARTESIAN_POINT('Ctrl Pts',(1.9313549213293,1.93440772928591,7.52834476460825));
#383797=CARTESIAN_POINT('Ctrl Pts',(1.92083722133262,1.93111958367716,7.53807742314407));
#383798=CARTESIAN_POINT('Ctrl Pts',(1.91031246871818,1.9278292332105,7.54780169004674));
#383799=CARTESIAN_POINT('Ctrl Pts',(1.89364182939126,1.92261749589957,7.5632044032688));
#383800=CARTESIAN_POINT('Ctrl Pts',(1.87695347475873,1.91740022025759,7.57858609112103));
#383801=CARTESIAN_POINT('Ctrl Pts',(1.86024642503782,1.91217709997537,7.59394543036555));
#383802=CARTESIAN_POINT('Origin',(1.92517265250696,2.18554644274947,7.5));
#383803=CARTESIAN_POINT('',(1.87445832375783,2.00297423990034,8.75721825406948));
#383804=CARTESIAN_POINT('',(1.87070527778331,1.98946322855773,8.78727029226991));
#383805=CARTESIAN_POINT('Origin',(1.86117864728403,1.95516724241569,8.75658640621101));
#383806=CARTESIAN_POINT('',(1.85157082176544,1.92057895321256,8.85049129520029));
#383807=CARTESIAN_POINT('Ctrl Pts',(1.87070527778331,1.98946322855773,8.78727029226991));
#383808=CARTESIAN_POINT('Ctrl Pts',(1.86433617262357,1.96653437219954,8.80838212259895));
#383809=CARTESIAN_POINT('Ctrl Pts',(1.85795824503303,1.94357375498271,8.82945686509571));
#383810=CARTESIAN_POINT('Ctrl Pts',(1.85157082176544,1.92057895321256,8.85049129520029));
#383811=CARTESIAN_POINT('',(1.85157082176544,1.92057895321256,7.59394543036555));
#383812=CARTESIAN_POINT('',(1.85157082176544,1.92057895321256,7.5));
#383813=CARTESIAN_POINT('',(1.87445832375783,2.00297423990034,7.51860402984325));
#383814=CARTESIAN_POINT('Ctrl Pts',(1.85157082176544,1.92057895321256,7.59394543036555));
#383815=CARTESIAN_POINT('Ctrl Pts',(1.85625577119296,1.93744482836688,7.57858609112103));
#383816=CARTESIAN_POINT('Ctrl Pts',(1.86093547819014,1.95429183070791,7.56320440326857));
#383817=CARTESIAN_POINT('Ctrl Pts',(1.86561021750531,1.97112094933312,7.54780169004651));
#383818=CARTESIAN_POINT('Ctrl Pts',(1.86856154251836,1.98174575542339,7.53807742314383));
#383819=CARTESIAN_POINT('Ctrl Pts',(1.8715108898539,1.99236344185046,7.52834476460825));
#383820=CARTESIAN_POINT('Ctrl Pts',(1.87445832375783,2.00297423990034,7.51860402984325));
#383821=CARTESIAN_POINT('',(1.87445832375783,2.00297423990034,7.5));
#383822=CARTESIAN_POINT('Origin',(1.85819500900386,1.91873890744402,7.5));
#383823=CARTESIAN_POINT('Ctrl Pts',(1.85157082176544,1.92057895321256,8.85049129520029));
#383824=CARTESIAN_POINT('Ctrl Pts',(1.85151898961497,1.92039235683786,8.85097269580138));
#383825=CARTESIAN_POINT('Ctrl Pts',(1.85147591597154,1.92020586346591,8.85143669361005));
#383826=CARTESIAN_POINT('Ctrl Pts',(1.85144046929249,1.92001068892906,8.8519052845931));
#383827=CARTESIAN_POINT('Ctrl Pts',(1.85137113783622,1.91962893991249,8.85282181883899));
#383828=CARTESIAN_POINT('Ctrl Pts',(1.85133296195824,1.91922376460099,8.85372622499636));
#383829=CARTESIAN_POINT('Ctrl Pts',(1.85134069336429,1.91878735874096,8.85462257735071));
#383830=CARTESIAN_POINT('Ctrl Pts',(1.85134711170301,1.91842507009563,8.85536669723986));
#383831=CARTESIAN_POINT('Ctrl Pts',(1.85138513796909,1.91804117502856,8.85610498449051));
#383832=CARTESIAN_POINT('Ctrl Pts',(1.85147117892722,1.91763196469162,8.85681338218371));
#383833=CARTESIAN_POINT('Ctrl Pts',(1.85154926123186,1.91726060566817,8.85745625420284));
#383834=CARTESIAN_POINT('Ctrl Pts',(1.85166728025085,1.91686361656052,8.85808743050666));
#383835=CARTESIAN_POINT('Ctrl Pts',(1.85185348044152,1.91643651442559,8.8586680450841));
#383836=CARTESIAN_POINT('Ctrl Pts',(1.85193938917317,1.91623945875897,8.85893592806395));
#383837=CARTESIAN_POINT('Ctrl Pts',(1.85204005382135,1.91603598377475,8.85919241173848));
#383838=CARTESIAN_POINT('Ctrl Pts',(1.85215983616255,1.91582581219597,8.85943017985534));
#383839=CARTESIAN_POINT('Ctrl Pts',(1.85232157778254,1.91554201834717,8.8597512372));
#383840=CARTESIAN_POINT('Ctrl Pts',(1.85252284994021,1.91523910848123,8.86004599534705));
#383841=CARTESIAN_POINT('Ctrl Pts',(1.85276990912335,1.91492648595463,8.86026130871721));
#383842=CARTESIAN_POINT('Ctrl Pts',(1.85286036445564,1.91481202603389,8.86034014101235));
#383843=CARTESIAN_POINT('Ctrl Pts',(1.85295830659985,1.91469453717767,8.86040910639692));
#383844=CARTESIAN_POINT('Ctrl Pts',(1.85306132555294,1.91457743569343,8.86046313645506));
#383845=CARTESIAN_POINT('Ctrl Pts',(1.85322208576646,1.914394699808,8.86054744990829));
#383846=CARTESIAN_POINT('Ctrl Pts',(1.85339970735975,1.91420801620862,8.86059655985668));
#383847=CARTESIAN_POINT('Ctrl Pts',(1.8535825866799,1.91402915554602,8.86059725258816));
#383848=CARTESIAN_POINT('Ctrl Pts',(1.85376588852434,1.91384988164382,8.86059794692011));
#383849=CARTESIAN_POINT('Ctrl Pts',(1.85395836289181,1.91367837807429,8.86056369958366));
#383850=CARTESIAN_POINT('Ctrl Pts',(1.85414700868607,1.91352118916221,8.86048590497774));
#383851=CARTESIAN_POINT('Ctrl Pts',(1.85419623962171,1.91348016753623,8.86046560290182));
#383852=CARTESIAN_POINT('Ctrl Pts',(1.85424590826076,1.91343965673617,8.86044257503091));
#383853=CARTESIAN_POINT('Ctrl Pts',(1.85429445905343,1.91340088314134,8.86041778462583));
#383854=CARTESIAN_POINT('Ctrl Pts',(1.85462114564155,1.91313998496212,8.86025097596201));
#383855=CARTESIAN_POINT('Ctrl Pts',(1.85494126451143,1.91292299108811,8.8599848982295));
#383856=CARTESIAN_POINT('Ctrl Pts',(1.85524071836527,1.91274922188442,8.85968173251461));
#383857=CARTESIAN_POINT('Ctrl Pts',(1.85539911229729,1.91265730793145,8.85952137522076));
#383858=CARTESIAN_POINT('Ctrl Pts',(1.85555468187753,1.91257555051966,8.8593474085396));
#383859=CARTESIAN_POINT('Ctrl Pts',(1.85570451004429,1.91250372651562,8.8591675900182));
#383860=CARTESIAN_POINT('Ctrl Pts',(1.85630614801294,1.91221531580601,8.85844552518696));
#383861=CARTESIAN_POINT('Ctrl Pts',(1.85684790431078,1.91206804643516,8.85759444184128));
#383862=CARTESIAN_POINT('Ctrl Pts',(1.85730040856211,1.9119876464474,8.85683498915144));
#383863=CARTESIAN_POINT('Ctrl Pts',(1.8573477619269,1.9119792328028,8.85675551445002));
#383864=CARTESIAN_POINT('Ctrl Pts',(1.85739413746324,1.91197157141332,8.85667699793653));
#383865=CARTESIAN_POINT('Ctrl Pts',(1.85743950055697,1.9119645902626,8.85659965593547));
#383866=CARTESIAN_POINT('Ctrl Pts',(1.85805181391074,1.91187035833397,8.85555568965886));
#383867=CARTESIAN_POINT('Ctrl Pts',(1.85865389393476,1.91186822577663,8.85434650606346));
#383868=CARTESIAN_POINT('Ctrl Pts',(1.85924869496048,1.91195196734978,8.85297329937117));
#383869=CARTESIAN_POINT('Ctrl Pts',(1.85958323429569,1.91199906688223,8.85220095427747));
#383870=CARTESIAN_POINT('Ctrl Pts',(1.85991556375352,1.91207366290458,8.85137579139183));
#383871=CARTESIAN_POINT('Ctrl Pts',(1.86024642503782,1.91217709997537,8.85049129520029));
#383872=CARTESIAN_POINT('Origin',(1.85819500900386,1.91873890744402,7.59394543036555));
#383873=CARTESIAN_POINT('Ctrl Pts',(1.85142033554721,1.92003720098911,7.59443877723642));
#383874=CARTESIAN_POINT('Ctrl Pts',(1.84987047229341,1.91445767434761,7.58783886950016));
#383875=CARTESIAN_POINT('Ctrl Pts',(1.85730292766808,1.91035428688842,7.58559994247159));
#383876=CARTESIAN_POINT('Ctrl Pts',(1.85988099357867,1.95049567322872,7.56670252222138));
#383877=CARTESIAN_POINT('Ctrl Pts',(1.85833337031732,1.94492421058726,7.56004874999029));
#383878=CARTESIAN_POINT('Ctrl Pts',(1.86579953910258,1.94077780480322,7.55786368756704));
#383879=CARTESIAN_POINT('Ctrl Pts',(1.86832585217657,1.98089726731458,7.5388891333356));
#383880=CARTESIAN_POINT('Ctrl Pts',(1.86676903131436,1.97529269319786,7.53222002137279));
#383881=CARTESIAN_POINT('Ctrl Pts',(1.8742794615967,1.97114590146279,7.53005029815327));
#383882=CARTESIAN_POINT('Ctrl Pts',(1.87675452920535,2.01124060755398,7.51101258149734));
#383883=CARTESIAN_POINT('Ctrl Pts',(1.87517883684548,2.00556809581521,7.5043616886572));
#383884=CARTESIAN_POINT('Ctrl Pts',(1.88274235577549,2.001457054227,7.50217374673251));
#383885=CARTESIAN_POINT('',(1.88229076388119,1.99983961245521,7.50366116523517));
#383886=CARTESIAN_POINT('Ctrl Pts',(1.87445832375783,2.00297423990034,7.51860402984325));
#383887=CARTESIAN_POINT('Ctrl Pts',(1.87457651791763,2.00339974031911,7.51734760759494));
#383888=CARTESIAN_POINT('Ctrl Pts',(1.87474064949507,2.00376831688546,7.51608817408573));
#383889=CARTESIAN_POINT('Ctrl Pts',(1.87496253976454,2.00407368959408,7.5148100591312));
#383890=CARTESIAN_POINT('Ctrl Pts',(1.87516353327286,2.00435030349067,7.51365231206384));
#383891=CARTESIAN_POINT('Ctrl Pts',(1.87541199969986,2.00457559451803,7.51247773061043));
#383892=CARTESIAN_POINT('Ctrl Pts',(1.875728442717,2.00471830984544,7.51129758471022));
#383893=CARTESIAN_POINT('Ctrl Pts',(1.87612174524814,2.00489568869871,7.50983079813402));
#383894=CARTESIAN_POINT('Ctrl Pts',(1.87661285822995,2.0049279735197,7.50839324291155));
#383895=CARTESIAN_POINT('Ctrl Pts',(1.87721077373279,2.00473313789107,7.50715379678855));
#383896=CARTESIAN_POINT('Ctrl Pts',(1.87748699346659,2.00464312944469,7.50658120839351));
#383897=CARTESIAN_POINT('Ctrl Pts',(1.87782232998932,2.00448281985079,7.50598221009429));
#383898=CARTESIAN_POINT('Ctrl Pts',(1.87819899209072,2.00423550222564,7.50545747549611));
#383899=CARTESIAN_POINT('Ctrl Pts',(1.87839999064681,2.00410352588566,7.50517746087247));
#383900=CARTESIAN_POINT('Ctrl Pts',(1.87861504784395,2.0039455111425,7.50491486231392));
#383901=CARTESIAN_POINT('Ctrl Pts',(1.87883748095714,2.00376429830918,7.50468370960993));
#383902=CARTESIAN_POINT('Ctrl Pts',(1.8791700886239,2.00349332796303,7.50433806340447));
#383903=CARTESIAN_POINT('Ctrl Pts',(1.87952881064224,2.00316193046717,7.50405484070983));
#383904=CARTESIAN_POINT('Ctrl Pts',(1.87988900162131,2.00279189861427,7.50385766036131));
#383905=CARTESIAN_POINT('Ctrl Pts',(1.87992751844788,2.0027523294592,7.50383657498791));
#383906=CARTESIAN_POINT('Ctrl Pts',(1.87996604537337,2.0027123460809,7.50381643264937));
#383907=CARTESIAN_POINT('Ctrl Pts',(1.88000454770712,2.00267199522526,7.50379723213559));
#383908=CARTESIAN_POINT('Ctrl Pts',(1.88026156337995,2.00240264006419,7.50366906242519));
#383909=CARTESIAN_POINT('Ctrl Pts',(1.88052255371096,2.0021105546266,7.50358235568538));
#383910=CARTESIAN_POINT('Ctrl Pts',(1.88076734876143,2.00182297316666,7.5035341175365));
#383911=CARTESIAN_POINT('Ctrl Pts',(1.88113439123415,2.00139177731542,7.50346178989176));
#383912=CARTESIAN_POINT('Ctrl Pts',(1.8815109114615,2.00091230248074,7.50346967198527));
#383913=CARTESIAN_POINT('Ctrl Pts',(1.88186605434871,2.00043023333641,7.50354272648692));
#383914=CARTESIAN_POINT('Ctrl Pts',(1.88201213196924,2.0002319483191,7.50357277531559));
#383915=CARTESIAN_POINT('Ctrl Pts',(1.88215451294322,2.00003357194374,7.50361331098761));
#383916=CARTESIAN_POINT('Ctrl Pts',(1.88229076388216,1.99983961245625,7.50366116523659));
#383917=CARTESIAN_POINT('',(1.86023191546302,1.92084218059594,7.57603338622103));
#383918=CARTESIAN_POINT('Origin',(1.86638166893215,1.92718820469566,7.58486873427626));
#383919=CARTESIAN_POINT('Ctrl Pts',(1.88229076389138,1.99983961251165,7.50366116529968));
#383920=CARTESIAN_POINT('Ctrl Pts',(1.87495061796099,1.97354987960085,7.52783573079709));
#383921=CARTESIAN_POINT('Ctrl Pts',(1.86759803291971,1.9472186407863,7.55196141284068));
#383922=CARTESIAN_POINT('Ctrl Pts',(1.86023191544544,1.92084218184787,7.57603338728831));
#383923=CARTESIAN_POINT('Ctrl Pts',(1.85201547038342,1.92152278748126,7.59639677331371));
#383924=CARTESIAN_POINT('Ctrl Pts',(1.84404333085312,1.90412613787916,7.59974925422226));
#383925=CARTESIAN_POINT('Ctrl Pts',(1.86117552269004,1.91265177151733,7.59639677331372));
#383926=CARTESIAN_POINT('Ctrl Pts',(1.8498416060656,1.91828405037994,7.58707626057423));
#383927=CARTESIAN_POINT('Ctrl Pts',(1.85121197023113,1.91152834659309,7.58811717123965));
#383928=CARTESIAN_POINT('Ctrl Pts',(1.85800812538016,1.9103752174624,7.58707626057424));
#383929=CARTESIAN_POINT('Ctrl Pts',(1.85581853271803,1.91938039888898,7.58015376756929));
#383930=CARTESIAN_POINT('Ctrl Pts',(1.85602009788945,1.91649313315482,7.58208760766041));
#383931=CARTESIAN_POINT('Ctrl Pts',(1.85891234067495,1.91638421296597,7.5801537675693));
#383932=CARTESIAN_POINT('Ctrl Pts',(1.86023191488714,1.9208421800016,7.57603338509286));
#383933=CARTESIAN_POINT('Ctrl Pts',(1.86023191488714,1.9208421800016,7.57603338509286));
#383934=CARTESIAN_POINT('Ctrl Pts',(1.86023191488714,1.9208421800016,7.57603338509286));
#383935=CARTESIAN_POINT('Origin',(1.86637756977751,1.92719217450502,7.58486873427621));
#383936=CARTESIAN_POINT('Ctrl Pts',(1.95008020177387,1.94026180847488,7.51098857897448));
#383937=CARTESIAN_POINT('Ctrl Pts',(1.94446108228008,1.93850510471889,7.50433767179956));
#383938=CARTESIAN_POINT('Ctrl Pts',(1.94010972714622,1.94593300883657,7.50214974420965));
#383939=CARTESIAN_POINT('Ctrl Pts',(1.9200139585086,1.9308622072507,7.53887321589169));
#383940=CARTESIAN_POINT('Ctrl Pts',(1.91446216603848,1.92912655192328,7.53220407452063));
#383941=CARTESIAN_POINT('Ctrl Pts',(1.91007676036986,1.93650023058754,7.53003438070912));
#383942=CARTESIAN_POINT('Ctrl Pts',(1.88988997696529,1.92144455532481,7.56669465659235));
#383943=CARTESIAN_POINT('Ctrl Pts',(1.88437099455651,1.91971915739766,7.56004085833303));
#383944=CARTESIAN_POINT('Ctrl Pts',(1.87998739246264,1.92704859685844,7.55785582193789));
#383945=CARTESIAN_POINT('Ctrl Pts',(1.859709619531,1.91200927861988,7.59443891967696));
#383946=CARTESIAN_POINT('Ctrl Pts',(1.85418263528485,1.9102813790806,7.58783901202978));
#383947=CARTESIAN_POINT('Ctrl Pts',(1.84984313418236,1.91757849550901,7.58560008491213));
#383948=CARTESIAN_POINT('',(1.93848173883012,1.94542168785064,7.50366116523517));
#383949=CARTESIAN_POINT('Ctrl Pts',(1.93848173883038,1.9454216878509,7.50366116523554));
#383950=CARTESIAN_POINT('Ctrl Pts',(1.93911531306413,1.94500609044103,7.50350835821027));
#383951=CARTESIAN_POINT('Ctrl Pts',(1.93968420053048,1.94460344287582,7.50345484956));
#383952=CARTESIAN_POINT('Ctrl Pts',(1.94020566163611,1.9442022642676,7.50349758195598));
#383953=CARTESIAN_POINT('Ctrl Pts',(1.94047320985586,1.9439964298894,7.50351950684424));
#383954=CARTESIAN_POINT('Ctrl Pts',(1.94075472287819,1.94377079693834,7.50357029184312));
#383955=CARTESIAN_POINT('Ctrl Pts',(1.94102020193909,1.94354575978782,7.50365515313923));
#383956=CARTESIAN_POINT('Ctrl Pts',(1.94142861623783,1.94319956152378,7.50378570417639));
#383957=CARTESIAN_POINT('Ctrl Pts',(1.94181129617362,1.94284487582416,7.50400001621911));
#383958=CARTESIAN_POINT('Ctrl Pts',(1.94213757088235,1.94250703424478,7.50428903009635));
#383959=CARTESIAN_POINT('Ctrl Pts',(1.94217378486482,1.94246953642867,7.50432110841318));
#383960=CARTESIAN_POINT('Ctrl Pts',(1.94220933369085,1.94243224012206,7.50435406373354));
#383961=CARTESIAN_POINT('Ctrl Pts',(1.94224419729612,1.94239517523653,7.50438785222352));
#383962=CARTESIAN_POINT('Ctrl Pts',(1.94245705636384,1.94216887629469,7.50459414719561));
#383963=CARTESIAN_POINT('Ctrl Pts',(1.94264738578748,1.94194724773846,7.50483629897752));
#383964=CARTESIAN_POINT('Ctrl Pts',(1.94280889250206,1.94173963749442,7.5050991045531));
#383965=CARTESIAN_POINT('Ctrl Pts',(1.94316519253622,1.94128162844362,7.50567888004914));
#383966=CARTESIAN_POINT('Ctrl Pts',(1.94339566683995,1.94087411611105,7.50637912803144));
#383967=CARTESIAN_POINT('Ctrl Pts',(1.94353025984855,1.94052476529618,7.50710440483569));
#383968=CARTESIAN_POINT('Ctrl Pts',(1.94356326472631,1.94043909754079,7.50728225710685));
#383969=CARTESIAN_POINT('Ctrl Pts',(1.9435912972134,1.94035527428434,7.50746498566954));
#383970=CARTESIAN_POINT('Ctrl Pts',(1.94361409802642,1.94027538435891,7.50764697238949));
#383971=CARTESIAN_POINT('Ctrl Pts',(1.94373666892225,1.93984591810613,7.50862528291181));
#383972=CARTESIAN_POINT('Ctrl Pts',(1.94372315950022,1.93949226889331,7.50965856837422));
#383973=CARTESIAN_POINT('Ctrl Pts',(1.94363670254534,1.93919419697489,7.51067959873202));
#383974=CARTESIAN_POINT('Ctrl Pts',(1.94358912517401,1.93903016762222,7.51124147302579));
#383975=CARTESIAN_POINT('Ctrl Pts',(1.9435190281706,1.9388830498072,7.51180065547253));
#383976=CARTESIAN_POINT('Ctrl Pts',(1.94343435338579,1.93875032191859,7.51235175716501));
#383977=CARTESIAN_POINT('Ctrl Pts',(1.94314176827384,1.93829169419094,7.51425603304536));
#383978=CARTESIAN_POINT('Ctrl Pts',(1.94263512968854,1.93795345792508,7.5162690050518));
#383979=CARTESIAN_POINT('Ctrl Pts',(1.94197444496731,1.93772914884598,7.51827788969243));
#383980=CARTESIAN_POINT('Ctrl Pts',(1.94193868746167,1.93771700881473,7.51838661432545));
#383981=CARTESIAN_POINT('Ctrl Pts',(1.94190246953306,1.93770520633128,7.51849533314857));
#383982=CARTESIAN_POINT('Ctrl Pts',(1.94186579781664,1.93769374166283,7.51860402984325));
#383983=CARTESIAN_POINT('Ctrl Pts',(1.86023191671587,1.92084218061918,7.57603338728985));
#383984=CARTESIAN_POINT('Ctrl Pts',(1.88635872817725,1.92904992062325,7.55196141284922));
#383985=CARTESIAN_POINT('Ctrl Pts',(1.91244077649953,1.93724268577581,7.52783573083105));
#383986=CARTESIAN_POINT('Ctrl Pts',(1.93848173888797,1.94542168786311,7.50366116530176));
#383987=CARTESIAN_POINT('Origin',(6.42796117143038E-16,6.63739765492893E-16,
7.49482233047033));
#383988=CARTESIAN_POINT('Origin',(1.87623278704646,1.99340331564184,7.49482233047033));
#383989=CARTESIAN_POINT('Origin',(0.,0.,7.50366116523517));
#383990=CARTESIAN_POINT('Origin',(1.93224291659621,1.93916053003968,7.49482233047033));
#383991=CARTESIAN_POINT('Ctrl Pts',(1.87445804062326,2.00297322077965,7.51860402984325));
#383992=CARTESIAN_POINT('Ctrl Pts',(1.87649514626116,2.01030442031657,7.51860402984325));
#383993=CARTESIAN_POINT('Ctrl Pts',(1.87091852206097,2.01548105518489,7.51860402984325));
#383994=CARTESIAN_POINT('Ctrl Pts',(1.8752144306242,2.00569534553863,7.51041458714365));
#383995=CARTESIAN_POINT('Ctrl Pts',(1.87517397337952,2.0115308171538,7.51004642900439));
#383996=CARTESIAN_POINT('Ctrl Pts',(1.87091698409424,2.01548248283932,7.50729136483008));
#383997=CARTESIAN_POINT('Ctrl Pts',(1.87802007521299,2.00592359023331,7.50215815450138));
#383998=CARTESIAN_POINT('Ctrl Pts',(1.87786410871603,2.00903385371625,7.49877163671532));
#383999=CARTESIAN_POINT('Ctrl Pts',(1.87535173527745,2.01139857427046,7.49481588533172));
#384000=CARTESIAN_POINT('Ctrl Pts',(1.88229038656648,1.99983921157655,7.50366171572174));
#384001=CARTESIAN_POINT('Ctrl Pts',(1.88480006004696,2.00250561388651,7.50000045605858));
#384002=CARTESIAN_POINT('Ctrl Pts',(1.88480006004687,2.0025056138866,7.49482233047317));
#384003=CARTESIAN_POINT('Origin',(1.86241434696069,2.00631977766132,7.51860402984325));
#384004=CARTESIAN_POINT('Origin',(1.86241434696069,2.00631977766132,9.));
#384005=CARTESIAN_POINT('Origin',(1.86241434696069,2.00631977766132,8.75721825406948));
#384006=CARTESIAN_POINT('Ctrl Pts',(1.86998861308143,1.98688333975429,8.78942910404913));
#384007=CARTESIAN_POINT('Ctrl Pts',(1.87149950741741,1.99224707231727,8.79672699501689));
#384008=CARTESIAN_POINT('Ctrl Pts',(1.86349840890978,1.99620382713063,8.79893251111267));
#384009=CARTESIAN_POINT('Ctrl Pts',(1.87293117467995,1.9974765805228,8.78111911759583));
#384010=CARTESIAN_POINT('Ctrl Pts',(1.87471519242254,2.0038373659161,8.78644465894818));
#384011=CARTESIAN_POINT('Ctrl Pts',(1.86838843520261,2.00890566492618,8.78817647674132));
#384012=CARTESIAN_POINT('Ctrl Pts',(1.8747650492242,2.00407854085087,8.7678092393203));
#384013=CARTESIAN_POINT('Ctrl Pts',(1.87686610037956,2.01158855555213,8.7698851615837));
#384014=CARTESIAN_POINT('Ctrl Pts',(1.87143223505306,2.01684302869505,8.77093053738832));
#384015=CARTESIAN_POINT('Ctrl Pts',(1.87440746878473,2.00279124894155,8.75371302330492));
#384016=CARTESIAN_POINT('Ctrl Pts',(1.87645768767539,2.01011673895028,8.7530082828756));
#384017=CARTESIAN_POINT('Ctrl Pts',(1.87083814324368,2.01529508421825,8.75267964240738));
#384018=CARTESIAN_POINT('Origin',(1.85866130098617,1.99280876631871,8.78727029226991));
#384019=CARTESIAN_POINT('Ctrl Pts',(1.85157082176544,1.92057895321256,8.85049129520029));
#384020=CARTESIAN_POINT('Ctrl Pts',(1.85313375416819,1.92620552894985,8.85711686593484));
#384021=CARTESIAN_POINT('Ctrl Pts',(1.8456351492193,1.93031304473611,8.85933012996512));
#384022=CARTESIAN_POINT('Ctrl Pts',(1.85795825360519,1.9435737858426,8.82945683644724));
#384023=CARTESIAN_POINT('Ctrl Pts',(1.85953415929185,1.94924706556041,8.83607469902391));
#384024=CARTESIAN_POINT('Ctrl Pts',(1.85199552183796,1.95333374977092,8.8382956714852));
#384025=CARTESIAN_POINT('Ctrl Pts',(1.86433616446269,1.96653434282029,8.80838214965001));
#384026=CARTESIAN_POINT('Ctrl Pts',(1.86591828940897,1.97223001194863,8.81501364461985));
#384027=CARTESIAN_POINT('Ctrl Pts',(1.85834689049523,1.97631935554933,8.81722098428721));
#384028=CARTESIAN_POINT('Ctrl Pts',(1.87070527778331,1.98946322855773,8.78727029226991));
#384029=CARTESIAN_POINT('Ctrl Pts',(1.87228766552573,1.99515984375547,8.79393457792714));
#384030=CARTESIAN_POINT('Ctrl Pts',(1.86468995654684,1.99927253550788,8.79610912703474));
#384031=CARTESIAN_POINT('Origin',(1.83952684496831,1.92392449097353,8.85049129520029));
#384032=CARTESIAN_POINT('Ctrl Pts',(1.86024642503782,1.91217709997537,8.85049129520029));
#384033=CARTESIAN_POINT('Ctrl Pts',(1.86582001548251,1.91391956999747,8.85711686593484));
#384034=CARTESIAN_POINT('Ctrl Pts',(1.8701657630119,1.90655647007117,8.85933012996512));
#384035=CARTESIAN_POINT('Ctrl Pts',(1.85531555002703,1.91063556189963,8.86332496987232));
#384036=CARTESIAN_POINT('Ctrl Pts',(1.85882508285508,1.90762972196619,8.86648636486737));
#384037=CARTESIAN_POINT('Ctrl Pts',(1.85636632694048,1.90226030661207,8.87206031107457));
#384038=CARTESIAN_POINT('Ctrl Pts',(1.85017872212211,1.91556737749546,8.86341338519876));
#384039=CARTESIAN_POINT('Ctrl Pts',(1.84703128601863,1.91896842389455,8.86654584966059));
#384040=CARTESIAN_POINT('Ctrl Pts',(1.84175139158005,1.91627642324358,8.87215952290715));
#384041=CARTESIAN_POINT('Ctrl Pts',(1.85157082176544,1.92057895321256,8.85049129520029));
#384042=CARTESIAN_POINT('Ctrl Pts',(1.85313375416819,1.92620552894985,8.85711686593484));
#384043=CARTESIAN_POINT('Ctrl Pts',(1.8456351492193,1.93031304473611,8.85933012996512));
#384044=CARTESIAN_POINT('Origin',(1.86397627237228,1.90024654094146,8.85049129520029));
#384045=CARTESIAN_POINT('Ctrl Pts',(1.92848201925695,1.93350957471442,8.78727029226991));
#384046=CARTESIAN_POINT('Ctrl Pts',(1.93412498960261,1.93527373495556,8.79393457792714));
#384047=CARTESIAN_POINT('Ctrl Pts',(1.93847908687933,1.92781174781519,8.79610912703474));
#384048=CARTESIAN_POINT('Ctrl Pts',(1.9057690541392,1.9264088267812,8.80838214965004));
#384049=CARTESIAN_POINT('Ctrl Pts',(1.91141108732461,1.92817269403821,8.81501364461989));
#384050=CARTESIAN_POINT('Ctrl Pts',(1.91574100516638,1.92073625510017,8.81722098428722));
#384051=CARTESIAN_POINT('Ctrl Pts',(1.88302471602829,1.91929827071791,8.82945683644723));
#384052=CARTESIAN_POINT('Ctrl Pts',(1.88864457064353,1.92105520429471,8.8360746990239));
#384053=CARTESIAN_POINT('Ctrl Pts',(1.89297078040504,1.9136514247466,8.83829567148519));
#384054=CARTESIAN_POINT('Ctrl Pts',(1.86024642503782,1.91217709997537,8.85049129520029));
#384055=CARTESIAN_POINT('Ctrl Pts',(1.86582001548251,1.91391956999747,8.85711686593484));
#384056=CARTESIAN_POINT('Ctrl Pts',(1.8701657630119,1.90655647007117,8.85933012996512));
#384057=CARTESIAN_POINT('Origin',(1.93221186659141,1.92157901568051,8.78727029226991));
#384058=CARTESIAN_POINT('Ctrl Pts',(1.94168907725773,1.93763847423638,8.75374538247848));
#384059=CARTESIAN_POINT('Ctrl Pts',(1.94893794972874,1.93991843614102,8.75304829418601));
#384060=CARTESIAN_POINT('Ctrl Pts',(1.95429209524043,1.93447750156611,8.75272238421917));
#384061=CARTESIAN_POINT('Ctrl Pts',(1.94294892858739,1.93803234165219,8.76769408445018));
#384062=CARTESIAN_POINT('Ctrl Pts',(1.95038042190972,1.9403690192021,8.7697431809397));
#384063=CARTESIAN_POINT('Ctrl Pts',(1.95580304081852,1.93511415845703,8.77077869880429));
#384064=CARTESIAN_POINT('Ctrl Pts',(1.9364916483571,1.93601360166434,8.78108014887992));
#384065=CARTESIAN_POINT('Ctrl Pts',(1.94278843160509,1.93799747616341,8.78639403366325));
#384066=CARTESIAN_POINT('Ctrl Pts',(1.94806417781672,1.9318583738154,8.78812224174741));
#384067=CARTESIAN_POINT('Ctrl Pts',(1.92590959152933,1.93270533243209,8.78944554828686));
#384068=CARTESIAN_POINT('Ctrl Pts',(1.93121460487314,1.93438260731682,8.79673892988685));
#384069=CARTESIAN_POINT('Ctrl Pts',(1.93542357110275,1.92652206295943,8.79894799272499));
#384070=CARTESIAN_POINT('Origin',(1.9455956451511,1.92576318262893,8.75721825406948));
#384071=CARTESIAN_POINT('Origin',(1.9455956451511,1.92576318262893,9.));
#384072=CARTESIAN_POINT('Origin',(1.9455956451511,1.92576318262893,7.51860402984325));
#384073=CARTESIAN_POINT('Ctrl Pts',(1.93848118356971,1.94542113060227,7.50366195182966));
#384074=CARTESIAN_POINT('Ctrl Pts',(1.94106594361273,1.948015144332,7.50000065167735));
#384075=CARTESIAN_POINT('Ctrl Pts',(1.94106594361282,1.94801514433192,7.49482233047108));
#384076=CARTESIAN_POINT('Ctrl Pts',(1.94470436195011,1.94134364970687,7.50215800491337));
#384077=CARTESIAN_POINT('Ctrl Pts',(1.94781906623354,1.94128607887102,7.49877273257265));
#384078=CARTESIAN_POINT('Ctrl Pts',(1.95026446067572,1.93884944135754,7.49481816995649));
#384079=CARTESIAN_POINT('Ctrl Pts',(1.94455588051514,1.93853509676886,7.51043025814042));
#384080=CARTESIAN_POINT('Ctrl Pts',(1.95039284348441,1.93868549717537,7.51006209594514));
#384081=CARTESIAN_POINT('Ctrl Pts',(1.95448142463542,1.93455482237168,7.50731281821698));
#384082=CARTESIAN_POINT('Ctrl Pts',(1.94186435528905,1.9376932905901,7.51860402984325));
#384083=CARTESIAN_POINT('Ctrl Pts',(1.94912671001948,1.93996468248936,7.51860402984324));
#384084=CARTESIAN_POINT('Ctrl Pts',(1.95447964353079,1.93455662181901,7.51860402984325));
#384085=CARTESIAN_POINT('Origin',(0.,0.,7.5));
#384086=CARTESIAN_POINT('Origin',(1.97893795668428,1.78906192937261,7.5));
#384087=CARTESIAN_POINT('',(1.97893795668428,1.78906192937261,7.59394543036555));
#384088=CARTESIAN_POINT('',(1.97893795668428,1.78906192937261,8.85049129520029));
#384089=CARTESIAN_POINT('',(1.97893795668428,1.78906192937261,7.5));
#384090=CARTESIAN_POINT('',(2.0484001299061,1.80597870472227,8.78727029226991));
#384091=CARTESIAN_POINT('Ctrl Pts',(1.97893795668428,1.78906192937261,8.85049129520029));
#384092=CARTESIAN_POINT('Ctrl Pts',(2.00212567109016,1.79470905121292,8.82945686509571));
#384093=CARTESIAN_POINT('Ctrl Pts',(2.02527891415477,1.80034777792378,8.80838212259896));
#384094=CARTESIAN_POINT('Ctrl Pts',(2.0484001299061,1.80597870472227,8.78727029226991));
#384095=CARTESIAN_POINT('',(2.06202449055416,1.80929677321445,8.75721825406948));
#384096=CARTESIAN_POINT('Origin',(2.02102401528965,1.79931175014709,8.75937679713129));
#384097=CARTESIAN_POINT('',(2.06202449055416,1.80929677321445,7.51860402984325));
#384098=CARTESIAN_POINT('',(2.06202449055416,1.80929677321445,7.5));
#384099=CARTESIAN_POINT('Ctrl Pts',(2.06202449055416,1.80929677321445,7.51860402984325));
#384100=CARTESIAN_POINT('Ctrl Pts',(2.051324674254,1.80669094647111,7.52834476460825));
#384101=CARTESIAN_POINT('Ctrl Pts',(2.0406179117875,1.80408342806265,7.53807742314407));
#384102=CARTESIAN_POINT('Ctrl Pts',(2.02990396992788,1.80147416118916,7.54780169004674));
#384103=CARTESIAN_POINT('Ctrl Pts',(2.01293366506138,1.79734122348039,7.5632044032688));
#384104=CARTESIAN_POINT('Ctrl Pts',(1.99594532644518,1.79320389384319,7.57858609112103));
#384105=CARTESIAN_POINT('Ctrl Pts',(1.97893795668428,1.78906192937261,7.59394543036555));
#384106=CARTESIAN_POINT('Origin',(2.06124562018329,2.05770976783675,7.5));
#384107=CARTESIAN_POINT('',(1.99893804826276,1.87876195735831,8.75721825406948));
#384108=CARTESIAN_POINT('',(1.99432705985482,1.86551916431874,8.78727029226991));
#384109=CARTESIAN_POINT('Origin',(1.98262265146286,1.83190401626966,8.75658640621077));
#384110=CARTESIAN_POINT('',(1.97081848695443,1.79800236791135,8.85049129520029));
#384111=CARTESIAN_POINT('Ctrl Pts',(1.99432705985482,1.86551916431874,8.78727029226991));
#384112=CARTESIAN_POINT('Ctrl Pts',(1.98650198383395,1.84304548772372,8.80838212259896));
#384113=CARTESIAN_POINT('Ctrl Pts',(1.97866606858369,1.82054068078122,8.82945686509571));
#384114=CARTESIAN_POINT('Ctrl Pts',(1.97081848695443,1.79800236791135,8.85049129520029));
#384115=CARTESIAN_POINT('',(1.97081848695443,1.79800236791135,7.59394543036555));
#384116=CARTESIAN_POINT('',(1.97081848695443,1.79800236791135,7.5));
#384117=CARTESIAN_POINT('',(1.99893804826276,1.87876195735831,7.51860402984325));
#384118=CARTESIAN_POINT('Ctrl Pts',(1.97081848695443,1.79800236791135,7.59394543036555));
#384119=CARTESIAN_POINT('Ctrl Pts',(1.97657441098219,1.81453342457589,7.57858609112103));
#384120=CARTESIAN_POINT('Ctrl Pts',(1.98232389416546,1.83104598308703,7.56320440326857));
#384121=CARTESIAN_POINT('Ctrl Pts',(1.98806727405974,1.84754101290683,7.54780169004651));
#384122=CARTESIAN_POINT('Ctrl Pts',(1.99169326892248,1.85795489715066,7.53807742314383));
#384123=CARTESIAN_POINT('Ctrl Pts',(1.99531683401267,1.86836180306963,7.52834476460825));
#384124=CARTESIAN_POINT('Ctrl Pts',(1.99893804826276,1.87876195735831,7.51860402984324));
#384125=CARTESIAN_POINT('',(1.99893804826276,1.87876195735831,7.5));
#384126=CARTESIAN_POINT('Origin',(1.97731117195257,1.79574168958063,7.5));
#384127=CARTESIAN_POINT('Ctrl Pts',(1.97081848695443,1.79800236791135,8.85049129520029));
#384128=CARTESIAN_POINT('Ctrl Pts',(1.9707548060279,1.7978194758162,8.85097269580138));
#384129=CARTESIAN_POINT('Ctrl Pts',(1.97069987221252,1.7976361253527,8.85143669361005));
#384130=CARTESIAN_POINT('Ctrl Pts',(1.97065199348697,1.79744362289939,8.8519052845931));
#384131=CARTESIAN_POINT('Ctrl Pts',(1.97055834573614,1.79706710030878,8.85282181883899));
#384132=CARTESIAN_POINT('Ctrl Pts',(1.97049428862326,1.7966652034103,8.85372622499636));
#384133=CARTESIAN_POINT('Ctrl Pts',(1.97047404352485,1.79622919884003,8.85462257735071));
#384134=CARTESIAN_POINT('Ctrl Pts',(1.9704572367632,1.79586724333121,8.85536669723986));
#384135=CARTESIAN_POINT('Ctrl Pts',(1.97047058865884,1.79548170066649,8.85610498449051));
#384136=CARTESIAN_POINT('Ctrl Pts',(1.9705302346403,1.79506781843297,8.85681338218371));
#384137=CARTESIAN_POINT('Ctrl Pts',(1.97058436346214,1.79469221965602,8.85745625420285));
#384138=CARTESIAN_POINT('Ctrl Pts',(1.97067670481894,1.79428848470056,8.85808743050666));
#384139=CARTESIAN_POINT('Ctrl Pts',(1.97083515791361,1.79385033020559,8.85866804508411));
#384140=CARTESIAN_POINT('Ctrl Pts',(1.97090826473664,1.79364817521964,8.85893592806396));
#384141=CARTESIAN_POINT('Ctrl Pts',(1.97099568587151,1.79343866869044,8.85919241173848));
#384142=CARTESIAN_POINT('Ctrl Pts',(1.97110175636776,1.79322125445076,8.85943017985534));
#384143=CARTESIAN_POINT('Ctrl Pts',(1.97124498293792,1.79292768086569,8.8597512372));
#384144=CARTESIAN_POINT('Ctrl Pts',(1.97142643405861,1.79261249780914,8.86004599534705));
#384145=CARTESIAN_POINT('Ctrl Pts',(1.97165295583811,1.79228468846284,8.86026130871721));
#384146=CARTESIAN_POINT('Ctrl Pts',(1.97173589184792,1.79216466821924,8.86034014101235));
#384147=CARTESIAN_POINT('Ctrl Pts',(1.97182610522263,1.79204114558175,8.86040910639692));
#384148=CARTESIAN_POINT('Ctrl Pts',(1.97192140979438,1.79191768424809,8.86046313645506));
#384149=CARTESIAN_POINT('Ctrl Pts',(1.97207013178041,1.79172502387089,8.86054744990829));
#384150=CARTESIAN_POINT('Ctrl Pts',(1.97223542757181,1.79152734357843,8.86059655985668));
#384151=CARTESIAN_POINT('Ctrl Pts',(1.97240647150479,1.79133713328596,8.86059725258816));
#384152=CARTESIAN_POINT('Ctrl Pts',(1.97257791061758,1.79114648353173,8.86059794692011));
#384153=CARTESIAN_POINT('Ctrl Pts',(1.97275900125439,1.79096300045962,8.86056369958366));
#384154=CARTESIAN_POINT('Ctrl Pts',(1.97293718832746,1.79079404793147,8.86048590497774));
#384155=CARTESIAN_POINT('Ctrl Pts',(1.97298368984827,1.79074995635195,8.86046560290182));
#384156=CARTESIAN_POINT('Ctrl Pts',(1.9730306609019,1.79070634650504,8.86044257503091));
#384157=CARTESIAN_POINT('Ctrl Pts',(1.973076627709,1.79066454191475,8.86041778462583));
#384158=CARTESIAN_POINT('Ctrl Pts',(1.97338592728075,1.79038324889726,8.86025097596201));
#384159=CARTESIAN_POINT('Ctrl Pts',(1.97369148558684,1.79014619077402,8.8599848982295));
#384160=CARTESIAN_POINT('Ctrl Pts',(1.97397919074952,1.78995359252351,8.85968173251461));
#384161=CARTESIAN_POINT('Ctrl Pts',(1.97413137029703,1.78985171908355,8.85952137522076));
#384162=CARTESIAN_POINT('Ctrl Pts',(1.97428138202753,1.7897601622739,8.85934740853961));
#384163=CARTESIAN_POINT('Ctrl Pts',(1.97442630057651,1.78967888631637,8.8591675900182));
#384164=CARTESIAN_POINT('Ctrl Pts',(1.97500822387783,1.7893525211005,8.85844552518696));
#384165=CARTESIAN_POINT('Ctrl Pts',(1.97553943149826,1.78917084386518,8.85759444184126));
#384166=CARTESIAN_POINT('Ctrl Pts',(1.97598585478618,1.7890616170209,8.85683498915141));
#384167=CARTESIAN_POINT('Ctrl Pts',(1.97603257179434,1.78905018672254,8.85675551444999));
#384168=CARTESIAN_POINT('Ctrl Pts',(1.97607836118025,1.78903956978339,8.85667699793652));
#384169=CARTESIAN_POINT('Ctrl Pts',(1.97612318378677,1.7890296965528,8.85659965593547));
#384170=CARTESIAN_POINT('Ctrl Pts',(1.97672820161668,1.7888964271825,8.85555568965886));
#384171=CARTESIAN_POINT('Ctrl Pts',(1.97732890796931,1.78885572360714,8.85434650606346));
#384172=CARTESIAN_POINT('Ctrl Pts',(1.97792785225354,1.78890118409168,8.85297329937118));
#384173=CARTESIAN_POINT('Ctrl Pts',(1.97826472191922,1.7889267528443,8.85220095427748));
#384174=CARTESIAN_POINT('Ctrl Pts',(1.9786011479541,1.78897990317965,8.85137579139184));
#384175=CARTESIAN_POINT('Ctrl Pts',(1.97893795668428,1.78906192937261,8.85049129520029));
#384176=CARTESIAN_POINT('Origin',(1.97731117195257,1.79574168958063,7.59394543036555));
#384177=CARTESIAN_POINT('Ctrl Pts',(1.97063359974215,1.79747137046106,7.59443877723642));
#384178=CARTESIAN_POINT('Ctrl Pts',(1.96872943934931,1.79200260763506,7.58783886950016));
#384179=CARTESIAN_POINT('Ctrl Pts',(1.97588371901011,1.78743145197464,7.58559994247159));
#384180=CARTESIAN_POINT('Ctrl Pts',(1.98102835546094,1.82732518628152,7.56670252222135));
#384181=CARTESIAN_POINT('Ctrl Pts',(1.97912694712045,1.82186432737043,7.56004874999029));
#384182=CARTESIAN_POINT('Ctrl Pts',(1.98631211473056,1.81724808174526,7.55786368756704));
#384183=CARTESIAN_POINT('Ctrl Pts',(1.99140370001199,1.85712325308371,7.5388891333356));
#384184=CARTESIAN_POINT('Ctrl Pts',(1.98949099150865,1.85162994002072,7.53222002137279));
#384185=CARTESIAN_POINT('Ctrl Pts',(1.99672030494779,1.84701047339368,7.53005029815327));
#384186=CARTESIAN_POINT('Ctrl Pts',(2.00175916390393,1.8868642224849,7.51101258149734));
#384187=CARTESIAN_POINT('Ctrl Pts',(1.99982326989806,1.88130432048599,7.5043616886572));
#384188=CARTESIAN_POINT('Ctrl Pts',(2.00710785342834,1.87671712915195,7.50217374673251));
#384189=CARTESIAN_POINT('',(2.00655355952789,1.87513194417977,7.50366116523517));
#384190=CARTESIAN_POINT('Ctrl Pts',(1.99893804826276,1.87876195735831,7.51860402984325));
#384191=CARTESIAN_POINT('Ctrl Pts',(1.99908326148542,1.87917901081501,7.51734760759493));
#384192=CARTESIAN_POINT('Ctrl Pts',(1.99927067061861,1.87953631415501,7.51608817408572));
#384193=CARTESIAN_POINT('Ctrl Pts',(1.99951167028734,1.87982684288428,7.51481005913119));
#384194=CARTESIAN_POINT('Ctrl Pts',(1.99972997354615,1.88009001074965,7.51365231206383));
#384195=CARTESIAN_POINT('Ctrl Pts',(1.99999236391792,1.88029891959379,7.51247773061042));
#384196=CARTESIAN_POINT('Ctrl Pts',(2.00031730057136,1.88042106712354,7.51129758471022));
#384197=CARTESIAN_POINT('Ctrl Pts',(2.00072115972242,1.88057288255325,7.50983079813402));
#384198=CARTESIAN_POINT('Ctrl Pts',(2.00121333215551,1.88057363532483,7.50839324291155));
#384199=CARTESIAN_POINT('Ctrl Pts',(2.00179753601525,1.88034089142909,7.50715379678855));
#384200=CARTESIAN_POINT('Ctrl Pts',(2.00206742136501,1.88023337045562,7.50658120839351));
#384201=CARTESIAN_POINT('Ctrl Pts',(2.00239179783195,1.88005190515019,7.50598221009429));
#384202=CARTESIAN_POINT('Ctrl Pts',(2.00275184034601,1.87978096284193,7.50545747549612));
#384203=CARTESIAN_POINT('Ctrl Pts',(2.00294397017588,1.87963637963979,7.50517746087247));
#384204=CARTESIAN_POINT('Ctrl Pts',(2.00314846147559,1.87946491079294,7.50491486231392));
#384205=CARTESIAN_POINT('Ctrl Pts',(2.00335882723,1.87926981894233,7.50468370960993));
#384206=CARTESIAN_POINT('Ctrl Pts',(2.00367339038895,1.87897809508744,7.50433806340447));
#384207=CARTESIAN_POINT('Ctrl Pts',(2.00401014266396,1.87862439508465,7.50405484070984));
#384208=CARTESIAN_POINT('Ctrl Pts',(2.00434588556982,1.87823204598661,7.50385766036131));
#384209=CARTESIAN_POINT('Ctrl Pts',(2.00438178805498,1.87819009034906,7.50383657498791));
#384210=CARTESIAN_POINT('Ctrl Pts',(2.00441767407892,1.87814772069231,7.50381643264937));
#384211=CARTESIAN_POINT('Ctrl Pts',(2.0044535120173,1.87810498588884,7.50379723213559));
#384212=CARTESIAN_POINT('Ctrl Pts',(2.00469274197944,1.87781971709614,7.50366906242519));
#384213=CARTESIAN_POINT('Ctrl Pts',(2.00493448209958,1.87751151007149,7.50358235568538));
#384214=CARTESIAN_POINT('Ctrl Pts',(2.00516034878496,1.87720883540576,7.5035341175365));
#384215=CARTESIAN_POINT('Ctrl Pts',(2.00549901031652,1.87675500900067,7.50346178989176));
#384216=CARTESIAN_POINT('Ctrl Pts',(2.00584403688454,1.87625239556468,7.50346967198527));
#384217=CARTESIAN_POINT('Ctrl Pts',(2.00616756381648,1.8757485628002,7.50354272648692));
#384218=CARTESIAN_POINT('Ctrl Pts',(2.0063006371402,1.87554132595544,7.50357277531559));
#384219=CARTESIAN_POINT('Ctrl Pts',(2.00643001555918,1.8753342347853,7.50361331098761));
#384220=CARTESIAN_POINT('Ctrl Pts',(2.00655355952893,1.87513194418074,7.50366116523658));
#384221=CARTESIAN_POINT('',(1.97947865054246,1.79771013628737,7.57603338622103));
#384222=CARTESIAN_POINT('Origin',(1.98602235984314,1.80364910574213,7.58486873427626));
#384223=CARTESIAN_POINT('Ctrl Pts',(2.00655355954168,1.87513194423543,7.50366116529969));
#384224=CARTESIAN_POINT('Ctrl Pts',(1.99754410575749,1.84936651116493,7.5278357307971));
#384225=CARTESIAN_POINT('Ctrl Pts',(1.98851957912755,1.82356045444555,7.55196141284068));
#384226=CARTESIAN_POINT('Ctrl Pts',(1.97947865060514,1.79771013753785,7.57603338728831));
#384227=CARTESIAN_POINT('Ctrl Pts',(1.97132269366338,1.7989157742366,7.5963967733137));
#384228=CARTESIAN_POINT('Ctrl Pts',(1.96225232658171,1.7820656446504,7.59974925422226));
#384229=CARTESIAN_POINT('Ctrl Pts',(1.97989555771579,1.78947609816001,7.59639677331373));
#384230=CARTESIAN_POINT('Ctrl Pts',(1.96894578918438,1.79582297143307,7.58707626057422));
#384231=CARTESIAN_POINT('Ctrl Pts',(1.96988049836197,1.78899334843065,7.58811717123965));
#384232=CARTESIAN_POINT('Ctrl Pts',(1.97658880884429,1.78740715737198,7.58707626057425));
#384233=CARTESIAN_POINT('Ctrl Pts',(1.97498067889015,1.79653412437102,7.58015376756929));
#384234=CARTESIAN_POINT('Ctrl Pts',(1.97499684217358,1.79363987650909,7.58208760766041));
#384235=CARTESIAN_POINT('Ctrl Pts',(1.97787616399562,1.79334587347695,7.58015376756931));
#384236=CARTESIAN_POINT('Ctrl Pts',(1.97947864992969,1.79771013573114,7.57603338509286));
#384237=CARTESIAN_POINT('Ctrl Pts',(1.97947864992969,1.79771013573114,7.57603338509286));
#384238=CARTESIAN_POINT('Ctrl Pts',(1.97947864992969,1.79771013573114,7.57603338509286));
#384239=CARTESIAN_POINT('Origin',(1.98601852345785,1.80365333002931,7.58486873427623));
#384240=CARTESIAN_POINT('Ctrl Pts',(2.07038655374304,1.81133326498926,7.51098857897448));
#384241=CARTESIAN_POINT('Ctrl Pts',(2.06466642693681,1.8099401887916,7.50433767179956));
#384242=CARTESIAN_POINT('Ctrl Pts',(2.06079991957957,1.81763162376428,7.50214974420965));
#384243=CARTESIAN_POINT('Ctrl Pts',(2.03977985028099,1.8038793270739,7.53887321589169));
#384244=CARTESIAN_POINT('Ctrl Pts',(2.03412826074528,1.80250294240137,7.53220407452062));
#384245=CARTESIAN_POINT('Ctrl Pts',(2.03022429857703,1.81014244495787,7.53003438070911));
#384246=CARTESIAN_POINT('Ctrl Pts',(2.00911437065793,1.7964110748481,7.56669465659233));
#384247=CARTESIAN_POINT('Ctrl Pts',(2.00349618096567,1.79504282435304,7.56004085833301));
#384248=CARTESIAN_POINT('Ctrl Pts',(1.99959118425104,1.80263806304485,7.55785582193789));
#384249=CARTESIAN_POINT('Ctrl Pts',(1.97839150175078,1.78892884607101,7.59443891967696));
#384250=CARTESIAN_POINT('Ctrl Pts',(1.97276516638294,1.78755861178312,7.58783901202978));
#384251=CARTESIAN_POINT('Ctrl Pts',(1.96890210910568,1.79511876829347,7.58560008491213));
#384252=CARTESIAN_POINT('',(2.05914251569201,1.81722565891169,7.50366116523517));
#384253=CARTESIAN_POINT('Ctrl Pts',(2.0591425156923,1.81722565891194,7.50366116523554));
#384254=CARTESIAN_POINT('Ctrl Pts',(2.05974816076236,1.81677032215098,7.50350835821027));
#384255=CARTESIAN_POINT('Ctrl Pts',(2.06029008167032,1.81633205312326,7.50345484956));
#384256=CARTESIAN_POINT('Ctrl Pts',(2.0607847677765,1.81589828865177,7.50349758195598));
#384257=CARTESIAN_POINT('Ctrl Pts',(2.06103857843585,1.81567573530908,7.50351950684424));
#384258=CARTESIAN_POINT('Ctrl Pts',(2.06130505670667,1.81543252934385,7.50357029184312));
#384259=CARTESIAN_POINT('Ctrl Pts',(2.06155557213263,1.81519094525446,7.50365515313924));
#384260=CARTESIAN_POINT('Ctrl Pts',(2.06194096630146,1.81481929109793,7.50378570417639));
#384261=CARTESIAN_POINT('Ctrl Pts',(2.06230013518947,1.81444081575045,7.50400001621911));
#384262=CARTESIAN_POINT('Ctrl Pts',(2.06260409394752,1.81408276381047,7.50428903009635));
#384263=CARTESIAN_POINT('Ctrl Pts',(2.06263783103114,1.81404302279981,7.50432110841318));
#384264=CARTESIAN_POINT('Ctrl Pts',(2.06267091723573,1.81400352550136,7.50435406373355));
#384265=CARTESIAN_POINT('Ctrl Pts',(2.06270333445461,1.81396430305075,7.50438785222352));
#384266=CARTESIAN_POINT('Ctrl Pts',(2.06290125715757,1.81372483113706,7.50459414719562));
#384267=CARTESIAN_POINT('Ctrl Pts',(2.06307699573865,1.81349146349243,7.50483629897752));
#384268=CARTESIAN_POINT('Ctrl Pts',(2.06322486898635,1.81327393203518,7.5050991045531));
#384269=CARTESIAN_POINT('Ctrl Pts',(2.06355109222324,1.81279403579152,7.50567888004914));
#384270=CARTESIAN_POINT('Ctrl Pts',(2.063754983588,1.81237259419741,7.50637912803144));
#384271=CARTESIAN_POINT('Ctrl Pts',(2.06386691707728,1.81201533775758,7.50710440483569));
#384272=CARTESIAN_POINT('Ctrl Pts',(2.06389436539104,1.811927731386,7.50728225710685));
#384273=CARTESIAN_POINT('Ctrl Pts',(2.06391696970789,1.81184228430581,7.50746498566954));
#384274=CARTESIAN_POINT('Ctrl Pts',(2.0639346051091,1.8117610976697,7.50764697238949));
#384275=CARTESIAN_POINT('Ctrl Pts',(2.06402940817259,1.81132466065713,7.50862528291182));
#384276=CARTESIAN_POINT('Ctrl Pts',(2.06399326812426,1.81097260360619,7.50965856837422));
#384277=CARTESIAN_POINT('Ctrl Pts',(2.06388789127108,1.81068068342462,7.51067959873203));
#384278=CARTESIAN_POINT('Ctrl Pts',(2.06382990225586,1.81052003938049,7.51124147302579));
#384279=CARTESIAN_POINT('Ctrl Pts',(2.06375052340349,1.81037771496522,7.51180065547253));
#384280=CARTESIAN_POINT('Ctrl Pts',(2.06365751868708,1.81025068491239,7.512351757165));
#384281=CARTESIAN_POINT('Ctrl Pts',(2.06333615034322,1.80981174547708,7.51425603304536));
#384282=CARTESIAN_POINT('Ctrl Pts',(2.06280888182927,1.80950666459951,7.5162690050518));
#384283=CARTESIAN_POINT('Ctrl Pts',(2.06213518302361,1.8093251466029,7.51827788969244));
#384284=CARTESIAN_POINT('Ctrl Pts',(2.06209872117114,1.8093153225059,7.51838661432545));
#384285=CARTESIAN_POINT('Ctrl Pts',(2.06206182146844,1.80930586476257,7.51849533314857));
#384286=CARTESIAN_POINT('Ctrl Pts',(2.06202449055416,1.80929677321445,7.51860402984325));
#384287=CARTESIAN_POINT('Ctrl Pts',(1.97947865179423,1.79771013623029,7.57603338728985));
#384288=CARTESIAN_POINT('Ctrl Pts',(2.00607765462697,1.80422706199454,7.55196141284922));
#384289=CARTESIAN_POINT('Ctrl Pts',(2.03263102684925,1.81073191165887,7.52783573083104));
#384290=CARTESIAN_POINT('Ctrl Pts',(2.05914251575055,1.81722565892043,7.50366116530176));
#384291=CARTESIAN_POINT('Origin',(6.84001376365777E-16,6.21191952330719E-16,
7.49482233047033));
#384292=CARTESIAN_POINT('Origin',(2.0000956545036,1.86909700733692,7.49482233047033));
#384293=CARTESIAN_POINT('Origin',(0.,0.,7.50366116523517));
#384294=CARTESIAN_POINT('Origin',(2.05251535802922,1.81137708803391,7.49482233047033));
#384295=CARTESIAN_POINT('Ctrl Pts',(1.99893770041463,1.878760958472,7.51860402984325));
#384296=CARTESIAN_POINT('Ctrl Pts',(2.00144033216758,1.88594657746686,7.51860402984325));
#384297=CARTESIAN_POINT('Ctrl Pts',(1.99620683387467,1.89146987192291,7.51860402984325));
#384298=CARTESIAN_POINT('Ctrl Pts',(1.99986694346332,1.88142902825996,7.51041458714367));
#384299=CARTESIAN_POINT('Ctrl Pts',(2.00020044929247,1.88725510237742,7.51004642900443));
#384300=CARTESIAN_POINT('Ctrl Pts',(1.99620539053798,1.89147139518194,7.50729136483011));
#384301=CARTESIAN_POINT('Ctrl Pts',(2.00268144724221,1.88147704573546,7.50215815450137));
#384302=CARTESIAN_POINT('Ctrl Pts',(2.00272507646069,1.88459091165628,7.49877163671529));
#384303=CARTESIAN_POINT('Ctrl Pts',(2.00036937312888,1.88711174195736,7.49481588533168));
#384304=CARTESIAN_POINT('Ctrl Pts',(2.00655315730403,1.87513156829939,7.50366171572174));
#384305=CARTESIAN_POINT('Ctrl Pts',(2.00922851137374,1.87763169686786,7.50000045605858));
#384306=CARTESIAN_POINT('Ctrl Pts',(2.00922851137366,1.87763169686795,7.49482233047317));
#384307=CARTESIAN_POINT('Origin',(1.98713316644797,1.88287228159599,7.51860402984325));
#384308=CARTESIAN_POINT('Origin',(1.98713316644797,1.88287228159599,9.));
#384309=CARTESIAN_POINT('Origin',(1.98713316644797,1.88287228159599,8.75721825406948));
#384310=CARTESIAN_POINT('Ctrl Pts',(1.99344657357428,1.86299049303864,8.78942910404913));
#384311=CARTESIAN_POINT('Ctrl Pts',(1.99529801914104,1.86824640190533,8.7967269950169));
#384312=CARTESIAN_POINT('Ctrl Pts',(1.98756686989969,1.87270765928304,8.79893251111266));
#384313=CARTESIAN_POINT('Ctrl Pts',(1.99706180063074,1.87337343828892,8.78111911759577));
#384314=CARTESIAN_POINT('Ctrl Pts',(1.99924968983695,1.87960685235723,8.78644465894813));
#384315=CARTESIAN_POINT('Ctrl Pts',(1.99326065865079,1.88507009473028,8.78817647674132));
#384316=CARTESIAN_POINT('Ctrl Pts',(1.99931489633358,1.87984433743599,8.76780923932033));
#384317=CARTESIAN_POINT('Ctrl Pts',(2.00189279894798,1.88720430719688,8.76988516158374));
#384318=CARTESIAN_POINT('Ctrl Pts',(1.99680675333071,1.89279613340802,8.77093053738833));
#384319=CARTESIAN_POINT('Ctrl Pts',(1.99887557350567,1.87858260066337,8.75371302330491));
#384320=CARTESIAN_POINT('Ctrl Pts',(2.00139092575807,1.8857616816919,8.75300828287559));
#384321=CARTESIAN_POINT('Ctrl Pts',(1.99611470500354,1.89128943294207,8.75267964240738));
#384322=CARTESIAN_POINT('Origin',(1.98252217804003,1.86962948855642,8.78727029226991));
#384323=CARTESIAN_POINT('Ctrl Pts',(1.97081848695443,1.79800236791135,8.85049129520029));
#384324=CARTESIAN_POINT('Ctrl Pts',(1.97273870409016,1.80351724582249,8.85711686593484));
#384325=CARTESIAN_POINT('Ctrl Pts',(1.96551867526936,1.80809675954566,8.85933012996512));
#384326=CARTESIAN_POINT('Ctrl Pts',(1.97866607911544,1.82054071102848,8.82945683644722));
#384327=CARTESIAN_POINT('Ctrl Pts',(1.98060223521436,1.82610136576063,8.83607469902389));
#384328=CARTESIAN_POINT('Ctrl Pts',(1.97334092145601,1.83066265560018,8.8382956714852));
#384329=CARTESIAN_POINT('Ctrl Pts',(1.9865019738075,1.84304545892769,8.80838214965003));
#384330=CARTESIAN_POINT('Ctrl Pts',(1.98844577088237,1.84862805859969,8.81501364461993));
#384331=CARTESIAN_POINT('Ctrl Pts',(1.98115193336379,1.85319410139927,8.81722098428722));
#384332=CARTESIAN_POINT('Ctrl Pts',(1.99432705985482,1.86551916431874,8.78727029226991));
#384333=CARTESIAN_POINT('Ctrl Pts',(1.99627117980078,1.87110269127884,8.79393457792714));
#384334=CARTESIAN_POINT('Ctrl Pts',(1.98895258219513,1.87569371995059,8.79610912703474));
#384335=CARTESIAN_POINT('Origin',(1.95901360513964,1.80211269214903,8.85049129520029));
#384336=CARTESIAN_POINT('Ctrl Pts',(1.97893795668428,1.78906192937261,8.85049129520029));
#384337=CARTESIAN_POINT('Ctrl Pts',(1.98461173602726,1.7904437181373,8.85711686593484));
#384338=CARTESIAN_POINT('Ctrl Pts',(1.98847679932026,1.7828173134893,8.85933012996512));
#384339=CARTESIAN_POINT('Ctrl Pts',(1.97391844600142,1.78783948079882,8.86332496987232));
#384340=CARTESIAN_POINT('Ctrl Pts',(1.9772281832921,1.78461496014557,8.86648636486737));
#384341=CARTESIAN_POINT('Ctrl Pts',(1.97443045953233,1.77941410986349,8.87206031107457));
#384342=CARTESIAN_POINT('Ctrl Pts',(1.96910815477048,1.79309028114443,8.86341338519876));
#384343=CARTESIAN_POINT('Ctrl Pts',(1.966185091203,1.79668599665246,8.86654584966058));
#384344=CARTESIAN_POINT('Ctrl Pts',(1.9607435677999,1.79433781100371,8.87215952290714));
#384345=CARTESIAN_POINT('Ctrl Pts',(1.97081848695443,1.79800236791135,8.85049129520029));
#384346=CARTESIAN_POINT('Ctrl Pts',(1.97273870409016,1.80351724582249,8.85711686593484));
#384347=CARTESIAN_POINT('Ctrl Pts',(1.96551867526936,1.80809675954566,8.85933012996512));
#384348=CARTESIAN_POINT('Origin',(1.98189574710557,1.77691691081257,8.85049129520029));
#384349=CARTESIAN_POINT('Ctrl Pts',(2.0484001299061,1.80597870472227,8.78727029226991));
#384350=CARTESIAN_POINT('Ctrl Pts',(2.05414453629871,1.8073776939556,8.79393457792714));
#384351=CARTESIAN_POINT('Ctrl Pts',(2.05801159645803,1.79965207029777,8.79610912703474));
#384352=CARTESIAN_POINT('Ctrl Pts',(2.02527888452904,1.80034777070874,8.80838214965003));
#384353=CARTESIAN_POINT('Ctrl Pts',(2.0310223369153,1.80174652760397,8.81501364461988));
#384354=CARTESIAN_POINT('Ctrl Pts',(2.03486690419788,1.79404794883869,8.81722098428721));
#384355=CARTESIAN_POINT('Ctrl Pts',(2.00212570220894,1.79470905879157,8.82945683644723));
#384356=CARTESIAN_POINT('Ctrl Pts',(2.00784657735089,1.79610231723846,8.83607469902389));
#384357=CARTESIAN_POINT('Ctrl Pts',(2.01168953666614,1.78843656833838,8.8382956714852));
#384358=CARTESIAN_POINT('Ctrl Pts',(1.97893795668428,1.78906192937261,8.85049129520029));
#384359=CARTESIAN_POINT('Ctrl Pts',(1.98461173602726,1.7904437181373,8.85711686593484));
#384360=CARTESIAN_POINT('Ctrl Pts',(1.98847679932026,1.7828173134893,8.85933012996512));
#384361=CARTESIAN_POINT('Origin',(2.0513579203274,1.79383368616223,8.78727029226991));
#384362=CARTESIAN_POINT('Ctrl Pts',(2.06184459209041,1.80925294186594,8.75374538247847));
#384363=CARTESIAN_POINT('Ctrl Pts',(2.06922464863628,1.8110637824905,8.75304829418601));
#384364=CARTESIAN_POINT('Ctrl Pts',(2.07421919160667,1.80529098561845,8.75272238421917));
#384365=CARTESIAN_POINT('Ctrl Pts',(2.06312709009236,1.80956528108706,8.76769408445022));
#384366=CARTESIAN_POINT('Ctrl Pts',(2.07069302605927,1.81142102027039,8.76974318093972));
#384367=CARTESIAN_POINT('Ctrl Pts',(2.07576782353207,1.80582952781395,8.7707786988043));
#384368=CARTESIAN_POINT('Ctrl Pts',(2.05655373592174,1.80796440818185,8.78108014887987));
#384369=CARTESIAN_POINT('Ctrl Pts',(2.0629646890288,1.80954077031014,8.78639403366321));
#384370=CARTESIAN_POINT('Ctrl Pts',(2.0678362620161,1.80307626318599,8.78812224174741));
#384371=CARTESIAN_POINT('Ctrl Pts',(2.04578145952719,1.80534093085236,8.78944554828686));
#384372=CARTESIAN_POINT('Ctrl Pts',(2.05118303652296,1.80667486622402,8.79673892988686));
#384373=CARTESIAN_POINT('Ctrl Pts',(2.0548797281739,1.79856080280582,8.79894799272499));
#384374=CARTESIAN_POINT('Origin',(2.06498228097545,1.79715175465441,8.75721825406948));
#384375=CARTESIAN_POINT('Origin',(2.06498228097545,1.79715175465441,9.));
#384376=CARTESIAN_POINT('Origin',(2.06498228097545,1.79715175465441,7.51860402984325));
#384377=CARTESIAN_POINT('Ctrl Pts',(2.05914192586943,1.8172251383839,7.50366195182966));
#384378=CARTESIAN_POINT('Ctrl Pts',(2.06188757427602,1.81964821628966,7.50000065167735));
#384379=CARTESIAN_POINT('Ctrl Pts',(2.0618875742761,1.81964821628958,7.49482233047108));
#384380=CARTESIAN_POINT('Ctrl Pts',(2.06509107296447,1.8127573147025,7.50215800491337));
#384381=CARTESIAN_POINT('Ctrl Pts',(2.06819568917778,1.81250030236349,7.49877273257264));
#384382=CARTESIAN_POINT('Ctrl Pts',(2.07047994339331,1.80991199422326,7.49481816995649));
#384383=CARTESIAN_POINT('Ctrl Pts',(2.06476295199597,1.80996404547592,7.51043025814042));
#384384=CARTESIAN_POINT('Ctrl Pts',(2.07059755848593,1.8097401613672,7.51006209594515));
#384385=CARTESIAN_POINT('Ctrl Pts',(2.07441308596513,1.80535601718416,7.50731281821698));
#384386=CARTESIAN_POINT('Ctrl Pts',(2.06202302209007,1.80929641549156,7.51860402984325));
#384387=CARTESIAN_POINT('Ctrl Pts',(2.06941598411247,1.81109783990739,7.51860402984324));
#384388=CARTESIAN_POINT('Ctrl Pts',(2.07441142381096,1.80535792705009,7.51860402984325));
#384389=CARTESIAN_POINT('Origin',(0.,0.,7.5));
#384390=CARTESIAN_POINT('Origin',(2.08949760778586,1.65859511954948,7.5));
#384391=CARTESIAN_POINT('',(2.08949760778586,1.65859511954948,7.59394543036555));
#384392=CARTESIAN_POINT('',(2.08949760778586,1.65859511954948,8.85049129520029));
#384393=CARTESIAN_POINT('',(2.08949760778586,1.65859511954948,7.5));
#384394=CARTESIAN_POINT('',(2.15990092504103,1.6710266808512,8.78727029226991));
#384395=CARTESIAN_POINT('Ctrl Pts',(2.08949760778586,1.65859511954948,8.85049129520029));
#384396=CARTESIAN_POINT('Ctrl Pts',(2.11299949288419,1.66274499680948,8.82945686509571));
#384397=CARTESIAN_POINT('Ctrl Pts',(2.1364664395885,1.66688870477514,8.80838212259894));
#384398=CARTESIAN_POINT('Ctrl Pts',(2.15990092504103,1.67102668085121,8.78727029226991));
#384399=CARTESIAN_POINT('',(2.17370988235713,1.67346501623199,8.75721825406948));
#384400=CARTESIAN_POINT('Origin',(2.13215390434319,1.66612741793514,8.75937679713173));
#384401=CARTESIAN_POINT('',(2.17370988235713,1.67346501623199,7.51860402984325));
#384402=CARTESIAN_POINT('',(2.17370988235713,1.67346501623199,7.5));
#384403=CARTESIAN_POINT('Ctrl Pts',(2.17370988235713,1.67346501623199,7.51860402984325));
#384404=CARTESIAN_POINT('Ctrl Pts',(2.16286509408443,1.67155008302327,7.52834476460825));
#384405=CARTESIAN_POINT('Ctrl Pts',(2.15201326553168,1.66963390666755,7.53807742314407));
#384406=CARTESIAN_POINT('Ctrl Pts',(2.14115416031211,1.6677164454245,7.54780169004674));
#384407=CARTESIAN_POINT('Ctrl Pts',(2.12395392452885,1.66467929044544,7.5632044032688));
#384408=CARTESIAN_POINT('Ctrl Pts',(2.10673541065634,1.66163890798795,7.57858609112103));
#384409=CARTESIAN_POINT('Ctrl Pts',(2.08949760778586,1.65859511954948,7.59394543036555));
#384410=CARTESIAN_POINT('Origin',(2.18884848747049,1.92141752211062,7.5));
#384411=CARTESIAN_POINT('',(2.11520370755651,1.74682943894032,8.75721825406948));
#384412=CARTESIAN_POINT('',(2.10975372425558,1.73390928168096,8.78727029226991));
#384413=CARTESIAN_POINT('Origin',(2.09591963389567,1.70111310357894,8.75658640621063));
#384414=CARTESIAN_POINT('',(2.08196763624129,1.6680374052101,8.85049129520029));
#384415=CARTESIAN_POINT('Ctrl Pts',(2.10975372425558,1.73390928168096,8.78727029226991));
#384416=CARTESIAN_POINT('Ctrl Pts',(2.10050483228941,1.71198313400682,8.80838212259895));
#384417=CARTESIAN_POINT('Ctrl Pts',(2.09124312883601,1.69002661441765,8.82945686509571));
#384418=CARTESIAN_POINT('Ctrl Pts',(2.08196763624129,1.6680374052101,8.85049129520029));
#384419=CARTESIAN_POINT('',(2.08196763624129,1.6680374052101,7.59394543036555));
#384420=CARTESIAN_POINT('',(2.08196763624129,1.6680374052101,7.5));
#384421=CARTESIAN_POINT('',(2.11520370755651,1.74682943894032,7.51860402984325));
#384422=CARTESIAN_POINT('Ctrl Pts',(2.08196763624129,1.6680374052101,7.59394543036555));
#384423=CARTESIAN_POINT('Ctrl Pts',(2.08877088254282,1.68416571372712,7.57858609112103));
#384424=CARTESIAN_POINT('Ctrl Pts',(2.09556651605251,1.7002759747635,7.56320440326857));
#384425=CARTESIAN_POINT('Ctrl Pts',(2.10235493574597,1.71636913416219,7.54780169004651));
#384426=CARTESIAN_POINT('Ctrl Pts',(2.10664070046774,1.72652930367545,7.53807742314383));
#384427=CARTESIAN_POINT('Ctrl Pts',(2.11092359330636,1.73668266487763,7.52834476460825));
#384428=CARTESIAN_POINT('Ctrl Pts',(2.11520370755651,1.74682943894032,7.51860402984325));
#384429=CARTESIAN_POINT('',(2.11520370755651,1.74682943894032,7.5));
#384430=CARTESIAN_POINT('Origin',(2.0883021391638,1.66536538392937,7.5));
#384431=CARTESIAN_POINT('Ctrl Pts',(2.08196763624129,1.6680374052101,8.85049129520029));
#384432=CARTESIAN_POINT('Ctrl Pts',(2.08189236821728,1.66785896893735,8.85097269580138));
#384433=CARTESIAN_POINT('Ctrl Pts',(2.08182579996479,1.66767951480867,8.85143669361005));
#384434=CARTESIAN_POINT('Ctrl Pts',(2.08176568593668,1.66749047547278,8.8519052845931));
#384435=CARTESIAN_POINT('Ctrl Pts',(2.08164810670999,1.6671207265202,8.85282181883899));
#384436=CARTESIAN_POINT('Ctrl Pts',(2.08155843158662,1.66672375951533,8.85372622499636));
#384437=CARTESIAN_POINT('Ctrl Pts',(2.08151029317522,1.66628994787111,8.85462257735071));
#384438=CARTESIAN_POINT('Ctrl Pts',(2.08147033037578,1.66592981285162,8.85536669723987));
#384439=CARTESIAN_POINT('Ctrl Pts',(2.08145895303518,1.66554420686677,8.85610498449051));
#384440=CARTESIAN_POINT('Ctrl Pts',(2.08149195894182,1.66512735346752,8.85681338218371));
#384441=CARTESIAN_POINT('Ctrl Pts',(2.08152191185393,1.66474905835303,8.85745625420284));
#384442=CARTESIAN_POINT('Ctrl Pts',(2.0815881960981,1.66434023658329,8.85808743050666));
#384443=CARTESIAN_POINT('Ctrl Pts',(2.08171825097901,1.6638928301991,8.8586680450841));
#384444=CARTESIAN_POINT('Ctrl Pts',(2.08177825548182,1.66368640659201,8.85893592806395));
#384445=CARTESIAN_POINT('Ctrl Pts',(2.08185207387118,1.6634717294251,8.85919241173848));
#384446=CARTESIAN_POINT('Ctrl Pts',(2.08194399665605,1.66324796592627,8.85943017985534));
#384447=CARTESIAN_POINT('Ctrl Pts',(2.08206811962769,1.66294581896175,8.8597512372));
#384448=CARTESIAN_POINT('Ctrl Pts',(2.08222900408982,1.66261965786937,8.86004599534706));
#384449=CARTESIAN_POINT('Ctrl Pts',(2.08243405763911,1.66227800874229,8.86026130871721));
#384450=CARTESIAN_POINT('Ctrl Pts',(2.08250913352457,1.66215292136476,8.86034014101235));
#384451=CARTESIAN_POINT('Ctrl Pts',(2.08259124742368,1.66202387252702,8.86040910639692));
#384452=CARTESIAN_POINT('Ctrl Pts',(2.08267844598715,1.66189455867303,8.86046313645506));
#384453=CARTESIAN_POINT('Ctrl Pts',(2.08281451861517,1.66169276548687,8.86054744990829));
#384454=CARTESIAN_POINT('Ctrl Pts',(2.08296680936882,1.66148490081206,8.86059655985668));
#384455=CARTESIAN_POINT('Ctrl Pts',(2.08312531505841,1.66128412250463,8.86059725258816));
#384456=CARTESIAN_POINT('Ctrl Pts',(2.08328418695946,1.66108288031909,8.86059794692011));
#384457=CARTESIAN_POINT('Ctrl Pts',(2.08345314972534,1.66088817171569,8.86056369958366));
#384458=CARTESIAN_POINT('Ctrl Pts',(2.08362014586832,1.66070814983367,8.86048590497774));
#384459=CARTESIAN_POINT('Ctrl Pts',(2.08366372688956,1.66066116948236,8.86046560290182));
#384460=CARTESIAN_POINT('Ctrl Pts',(2.08370780734364,1.66061463979082,8.86044257503091));
#384461=CARTESIAN_POINT('Ctrl Pts',(2.08375100127771,1.6605699759891,8.86041778462583));
#384462=CARTESIAN_POINT('Ctrl Pts',(2.08404164285481,1.66026944402668,8.86025097596201));
#384463=CARTESIAN_POINT('Ctrl Pts',(2.08433138499248,1.66001329577689,8.8599848982295));
#384464=CARTESIAN_POINT('Ctrl Pts',(2.08460615922177,1.65980265990707,8.85968173251461));
#384465=CARTESIAN_POINT('Ctrl Pts',(2.08475149904637,1.65969124559994,8.85952137522076));
#384466=CARTESIAN_POINT('Ctrl Pts',(2.08489533649674,1.65959026561901,8.8593474085396));
#384467=CARTESIAN_POINT('Ctrl Pts',(2.08503474992654,1.65949987168834,8.8591675900182));
#384468=CARTESIAN_POINT('Ctrl Pts',(2.08559456731286,1.65913689307087,8.85844552518695));
#384469=CARTESIAN_POINT('Ctrl Pts',(2.08611304340984,1.65892155452182,8.85759444184124));
#384470=CARTESIAN_POINT('Ctrl Pts',(2.0865515512853,1.65878394965754,8.85683498915139));
#384471=CARTESIAN_POINT('Ctrl Pts',(2.08659743996662,1.65876954967496,8.85675551444998));
#384472=CARTESIAN_POINT('Ctrl Pts',(2.0866424550437,1.65875602081343,8.85667699793651));
#384473=CARTESIAN_POINT('Ctrl Pts',(2.0866865529773,1.65874329607419,8.85659965593547));
#384474=CARTESIAN_POINT('Ctrl Pts',(2.08728178913532,1.65857153689465,8.85555568965886));
#384475=CARTESIAN_POINT('Ctrl Pts',(2.08787865338529,1.65849242956099,8.85434650606346));
#384476=CARTESIAN_POINT('Ctrl Pts',(2.0884792797375,1.65849942215005,8.85297329937117));
#384477=CARTESIAN_POINT('Ctrl Pts',(2.08881709546393,1.65850335505533,8.85220095427747));
#384478=CARTESIAN_POINT('Ctrl Pts',(2.08915623562911,1.65853484129756,8.85137579139184));
#384479=CARTESIAN_POINT('Ctrl Pts',(2.08949760778586,1.65859511954948,8.85049129520029));
#384480=CARTESIAN_POINT('Origin',(2.0883021391638,1.66536538392937,7.59394543036555));
#384481=CARTESIAN_POINT('Ctrl Pts',(2.08174910777616,1.66751934451538,7.59443877723642));
#384482=CARTESIAN_POINT('Ctrl Pts',(2.07949847484779,1.66218381782438,7.58783886950016));
#384483=CARTESIAN_POINT('Ctrl Pts',(2.086345180325,1.65716367782185,7.58559994247159));
#384484=CARTESIAN_POINT('Ctrl Pts',(2.09403524690138,1.69664582818389,7.56670252222138));
#384485=CARTESIAN_POINT('Ctrl Pts',(2.09178786677661,1.69131801284371,7.56004874999029));
#384486=CARTESIAN_POINT('Ctrl Pts',(2.09866250781646,1.68625089652094,7.55786368756705));
#384487=CARTESIAN_POINT('Ctrl Pts',(2.1062984428893,1.72571792105421,7.53888913333558));
#384488=CARTESIAN_POINT('Ctrl Pts',(2.10403770647439,1.72035844224661,7.53222002137275));
#384489=CARTESIAN_POINT('Ctrl Pts',(2.11095619627073,1.71528528310687,7.53005029815327));
#384490=CARTESIAN_POINT('Ctrl Pts',(2.11853814082204,1.75473430759452,7.51101258149734));
#384491=CARTESIAN_POINT('Ctrl Pts',(2.11625000017389,1.74930986216538,7.5043616886572));
#384492=CARTESIAN_POINT('Ctrl Pts',(2.12322571438817,1.74426537083866,7.50217374673251));
#384493=CARTESIAN_POINT('',(2.12257099619411,1.74271895653114,7.50366116523517));
#384494=CARTESIAN_POINT('Ctrl Pts',(2.11520370755651,1.74682943894032,7.51860402984325));
#384495=CARTESIAN_POINT('Ctrl Pts',(2.11537534312975,1.74723633167284,7.51734760759494));
#384496=CARTESIAN_POINT('Ctrl Pts',(2.11558525971437,1.74758089355042,7.51608817408573));
#384497=CARTESIAN_POINT('Ctrl Pts',(2.11584437846302,1.74785538445546,7.5148100591312));
#384498=CARTESIAN_POINT('Ctrl Pts',(2.1160790944174,1.74810402487641,7.51365231206384));
#384499=CARTESIAN_POINT('Ctrl Pts',(2.11635433051561,1.74829569308609,7.51247773061043));
#384500=CARTESIAN_POINT('Ctrl Pts',(2.11668642557094,1.74839677088778,7.51129758471022));
#384501=CARTESIAN_POINT('Ctrl Pts',(2.11709918179804,1.74852239905175,7.50983079813402));
#384502=CARTESIAN_POINT('Ctrl Pts',(2.11759039124033,1.74849161668062,7.50839324291155));
#384503=CARTESIAN_POINT('Ctrl Pts',(2.11815848283798,1.74822192091238,7.50715379678855));
#384504=CARTESIAN_POINT('Ctrl Pts',(2.11842092478693,1.74809732923854,7.50658120839351));
#384505=CARTESIAN_POINT('Ctrl Pts',(2.11873300826559,1.74789545390146,7.50598221009429));
#384506=CARTESIAN_POINT('Ctrl Pts',(2.1190749517004,1.74760200027015,7.50545747549611));
#384507=CARTESIAN_POINT('Ctrl Pts',(2.11925742330135,1.74744540432924,7.50517746087247));
#384508=CARTESIAN_POINT('Ctrl Pts',(2.11945050840502,1.74726118598096,7.50491486231392));
#384509=CARTESIAN_POINT('Ctrl Pts',(2.11964794236264,1.74705301678733,7.50468370960992));
#384510=CARTESIAN_POINT('Ctrl Pts',(2.11994316840629,1.74674173817959,7.50433806340447));
#384511=CARTESIAN_POINT('Ctrl Pts',(2.12025656715065,1.74636718909905,7.50405484070984));
#384512=CARTESIAN_POINT('Ctrl Pts',(2.12056648234368,1.74595413500248,7.50385766036131));
#384513=CARTESIAN_POINT('Ctrl Pts',(2.1205996229564,1.74590996528717,7.50383657498791));
#384514=CARTESIAN_POINT('Ctrl Pts',(2.12063272061543,1.74586538345797,7.50381643264937));
#384515=CARTESIAN_POINT('Ctrl Pts',(2.12066574689267,1.74582044031314,7.50379723213559));
#384516=CARTESIAN_POINT('Ctrl Pts',(2.12088620809689,1.74552043011947,7.50366906242519));
#384517=CARTESIAN_POINT('Ctrl Pts',(2.12110770464416,1.74519736799653,7.50358235568538));
#384518=CARTESIAN_POINT('Ctrl Pts',(2.1213137148298,1.74488084388015,7.5035341175365));
#384519=CARTESIAN_POINT('Ctrl Pts',(2.12162260378731,1.74440625179125,7.50346178989176));
#384520=CARTESIAN_POINT('Ctrl Pts',(2.12193471890784,1.74388256510035,7.50346967198527));
#384521=CARTESIAN_POINT('Ctrl Pts',(2.12222530044294,1.74335903907262,7.50354272648692));
#384522=CARTESIAN_POINT('Ctrl Pts',(2.12234482264301,1.74314370198107,7.50357277531559));
#384523=CARTESIAN_POINT('Ctrl Pts',(2.12246066686333,1.74292874699818,7.50361331098761));
#384524=CARTESIAN_POINT('Ctrl Pts',(2.12257099619521,1.74271895653205,7.50366116523659));
#384525=CARTESIAN_POINT('',(2.09059128324999,1.66719091542118,7.57603338622103));
#384526=CARTESIAN_POINT('Origin',(2.09750205887771,1.67269842573194,7.58486873427627));
#384527=CARTESIAN_POINT('Ctrl Pts',(2.12257099621144,1.74271895658581,7.50366116529969));
#384528=CARTESIAN_POINT('Ctrl Pts',(2.11192925635159,1.71758369904673,7.52783573079709));
#384529=CARTESIAN_POINT('Ctrl Pts',(2.10126987184861,1.692408867045,7.55196141284069));
#384530=CARTESIAN_POINT('Ctrl Pts',(2.09059128339265,1.66719091666508,7.57603338728831));
#384531=CARTESIAN_POINT('Ctrl Pts',(2.08252932914759,1.66891663020922,7.59639677331372));
#384532=CARTESIAN_POINT('Ctrl Pts',(2.07239800659894,1.65268226143543,7.59974925422224));
#384533=CARTESIAN_POINT('Ctrl Pts',(2.0904797772088,1.65894708367398,7.59639677331371));
#384534=CARTESIAN_POINT('Ctrl Pts',(2.07995915171788,1.66598247069355,7.58707626057424));
#384535=CARTESIAN_POINT('Ctrl Pts',(2.08045436498717,1.65910699286144,7.58811717123965));
#384536=CARTESIAN_POINT('Ctrl Pts',(2.0870472649161,1.65709425787422,7.58707626057421));
#384537=CARTESIAN_POINT('Ctrl Pts',(2.08602720582062,1.66630550578071,7.5801537675693));
#384538=CARTESIAN_POINT('Ctrl Pts',(2.0858579007976,1.66341616887639,7.58208760766041));
#384539=CARTESIAN_POINT('Ctrl Pts',(2.08871246990528,1.66293829112239,7.5801537675693));
#384540=CARTESIAN_POINT('Ctrl Pts',(2.09059128260285,1.66719091490535,7.57603338509286));
#384541=CARTESIAN_POINT('Ctrl Pts',(2.09059128260285,1.66719091490535,7.57603338509286));
#384542=CARTESIAN_POINT('Ctrl Pts',(2.09059128260285,1.66719091490535,7.57603338509286));
#384543=CARTESIAN_POINT('Origin',(2.09749850102576,1.67270288713816,7.58486873427622));
#384544=CARTESIAN_POINT('Ctrl Pts',(2.18218524326636,1.67496156458802,7.51098857897448));
#384545=CARTESIAN_POINT('Ctrl Pts',(2.1763876143757,1.67393784039762,7.50433767179956));
#384546=CARTESIAN_POINT('Ctrl Pts',(2.17302184310317,1.68186120046917,7.50214974420965));
#384547=CARTESIAN_POINT('Ctrl Pts',(2.15116384911715,1.66948391981124,7.53887321589167));
#384548=CARTESIAN_POINT('Ctrl Pts',(2.14543568610953,1.66847246165342,7.5322040745206));
#384549=CARTESIAN_POINT('Ctrl Pts',(2.14202920965962,1.6763463957475,7.53003438070911));
#384550=CARTESIAN_POINT('Ctrl Pts',(2.12008288244789,1.66399575593587,7.56669465659234));
#384551=CARTESIAN_POINT('Ctrl Pts',(2.11438857181863,1.66299027530768,7.56004085833295));
#384552=CARTESIAN_POINT('Ctrl Pts',(2.1109782269524,1.67082010276554,7.55785582193789));
#384553=CARTESIAN_POINT('Ctrl Pts',(2.08894374892622,1.65849732116959,7.59443891967696));
#384554=CARTESIAN_POINT('Ctrl Pts',(2.08324118225557,1.65749038271971,7.58783901202978));
#384555=CARTESIAN_POINT('Ctrl Pts',(2.0798704429345,1.66528251300723,7.58560008491213));
#384556=CARTESIAN_POINT('',(2.17134183427225,1.68156225994659,7.50366116523517));
#384557=CARTESIAN_POINT('Ctrl Pts',(2.17134183427255,1.68156225994682,7.50366116523554));
#384558=CARTESIAN_POINT('Ctrl Pts',(2.17191706145342,1.6810690549112,7.50350835821027));
#384559=CARTESIAN_POINT('Ctrl Pts',(2.17242978893373,1.68059696536242,7.50345484956));
#384560=CARTESIAN_POINT('Ctrl Pts',(2.17289566726915,1.68013239745891,7.50349758195598));
#384561=CARTESIAN_POINT('Ctrl Pts',(2.17313469740565,1.67989403967115,7.50351950684424));
#384562=CARTESIAN_POINT('Ctrl Pts',(2.1733850459086,1.67963426007723,7.50357029184312));
#384563=CARTESIAN_POINT('Ctrl Pts',(2.17361956827799,1.67937712176982,7.50365515313924));
#384564=CARTESIAN_POINT('Ctrl Pts',(2.1739803586496,1.67898153892743,7.50378570417639));
#384565=CARTESIAN_POINT('Ctrl Pts',(2.17431454058785,1.67858082916848,7.50400001621911));
#384566=CARTESIAN_POINT('Ctrl Pts',(2.17459493436346,1.67820403818011,7.50428903009635));
#384567=CARTESIAN_POINT('Ctrl Pts',(2.17462605591534,1.67816221727926,7.50432110841318));
#384568=CARTESIAN_POINT('Ctrl Pts',(2.17465654354017,1.67812068129183,7.50435406373354));
#384569=CARTESIAN_POINT('Ctrl Pts',(2.17468638116336,1.67807946244961,7.50438785222352));
#384570=CARTESIAN_POINT('Ctrl Pts',(2.17486855419471,1.67782780160553,7.50459414719561));
#384571=CARTESIAN_POINT('Ctrl Pts',(2.17502897978569,1.67758365383021,7.50483629897752));
#384572=CARTESIAN_POINT('Ctrl Pts',(2.17516261192363,1.67735709504316,7.5050991045531));
#384573=CARTESIAN_POINT('Ctrl Pts',(2.17545741784199,1.67685728360325,7.50567888004914));
#384574=CARTESIAN_POINT('Ctrl Pts',(2.17563388843443,1.6764236445415,7.50637912803144));
#384575=CARTESIAN_POINT('Ctrl Pts',(2.17572270244566,1.67605995052007,7.50710440483569));
#384576=CARTESIAN_POINT('Ctrl Pts',(2.17574448140442,1.67597076552567,7.50728225710685));
#384577=CARTESIAN_POINT('Ctrl Pts',(2.17576156466506,1.67588404574211,7.50746498566954));
#384578=CARTESIAN_POINT('Ctrl Pts',(2.17577396218681,1.67580189600862,7.50764697238949));
#384579=CARTESIAN_POINT('Ctrl Pts',(2.17584060785183,1.67536028164957,7.50862528291181));
#384580=CARTESIAN_POINT('Ctrl Pts',(2.17578198568441,1.67501126343844,7.50965856837421));
#384581=CARTESIAN_POINT('Ctrl Pts',(2.17565812194902,1.67472669455636,7.51067959873201));
#384582=CARTESIAN_POINT('Ctrl Pts',(2.17558995957921,1.67457009594161,7.51124147302578));
#384583=CARTESIAN_POINT('Ctrl Pts',(2.17550162506261,1.67443314976765,7.51180065547252));
#384584=CARTESIAN_POINT('Ctrl Pts',(2.17540067259094,1.67431233954432,7.51235175716501));
#384585=CARTESIAN_POINT('Ctrl Pts',(2.17505184158663,1.67389489209765,7.51425603304535));
#384586=CARTESIAN_POINT('Ctrl Pts',(2.17450610980346,1.67362422025114,7.5162690050518));
#384587=CARTESIAN_POINT('Ctrl Pts',(2.17382216528628,1.6734862392334,7.51827788969243));
#384588=CARTESIAN_POINT('Ctrl Pts',(2.17378514891653,1.67347877143997,7.51838661432545));
#384589=CARTESIAN_POINT('Ctrl Pts',(2.17374771906853,1.67347169730066,7.51849533314856));
#384590=CARTESIAN_POINT('Ctrl Pts',(2.17370988235713,1.67346501623199,7.51860402984325));
#384591=CARTESIAN_POINT('Ctrl Pts',(2.09059128449553,1.66719091528402,7.57603338728984));
#384592=CARTESIAN_POINT('Ctrl Pts',(2.11755317769153,1.67199024736258,7.55196141284922));
#384593=CARTESIAN_POINT('Ctrl Pts',(2.14446876031168,1.67678045171611,7.52783573083105));
#384594=CARTESIAN_POINT('Ctrl Pts',(2.17134183433122,1.68156225995156,7.50366116530176));
#384595=CARTESIAN_POINT('Origin',(7.22395927215194E-16,5.76091528191162E-16,
7.49482233047033));
#384596=CARTESIAN_POINT('Origin',(2.1157396998972,1.73711017850881,7.49482233047033));
#384597=CARTESIAN_POINT('Origin',(0.,0.,7.50366116523517));
#384598=CARTESIAN_POINT('Origin',(2.16435357359292,1.67615030903423,7.49482233047033));
#384599=CARTESIAN_POINT('Ctrl Pts',(2.11520329642422,1.74682846439304,7.51860402984325));
#384600=CARTESIAN_POINT('Ctrl Pts',(2.11816117044151,1.75383897559608,7.51860402984325));
#384601=CARTESIAN_POINT('Ctrl Pts',(2.11329230362296,1.75968623323819,7.51860402984325));
#384602=CARTESIAN_POINT('Ctrl Pts',(2.11630157406164,1.74943151553893,7.51041458714365));
#384603=CARTESIAN_POINT('Ctrl Pts',(2.1170076725176,1.75522425157044,7.5100464290044));
#384604=CARTESIAN_POINT('Ctrl Pts',(2.1132909608473,1.75968784584242,7.50729136483009));
#384605=CARTESIAN_POINT('Ctrl Pts',(2.11911337163085,1.74929910848111,7.50215815450139));
#384606=CARTESIAN_POINT('Ctrl Pts',(2.11935641728298,1.75240378129679,7.49877163671533));
#384607=CARTESIAN_POINT('Ctrl Pts',(2.11716706414824,1.75507036271236,7.49481588533172));
#384608=CARTESIAN_POINT('Ctrl Pts',(2.12257057071393,1.74271860719363,7.50366171572174));
#384609=CARTESIAN_POINT('Ctrl Pts',(2.12540061176913,1.74504218845604,7.50000045605858));
#384610=CARTESIAN_POINT('Ctrl Pts',(2.12540061176905,1.74504218845613,7.49482233047317));
#384611=CARTESIAN_POINT('Origin',(2.10368642951558,1.75168765945074,7.51860402984325));
#384612=CARTESIAN_POINT('Origin',(2.10368642951558,1.75168765945074,9.));
#384613=CARTESIAN_POINT('Origin',(2.10368642951558,1.75168765945074,8.75721825406948));
#384614=CARTESIAN_POINT('Ctrl Pts',(2.10871303450336,1.73144221877688,8.78942910404912));
#384615=CARTESIAN_POINT('Ctrl Pts',(2.11089742331392,1.73656870629038,8.79672699501691));
#384616=CARTESIAN_POINT('Ctrl Pts',(2.10346799228943,1.74151613396893,8.79893251111267));
#384617=CARTESIAN_POINT('Ctrl Pts',(2.11298607127434,1.74157220275981,8.78111911759583));
#384618=CARTESIAN_POINT('Ctrl Pts',(2.1155688414381,1.74765263106764,8.78644465894813));
#384619=CARTESIAN_POINT('Ctrl Pts',(2.10994214649949,1.75348836716887,8.78817647674131));
#384620=CARTESIAN_POINT('Ctrl Pts',(2.11564912968224,1.74788545041325,8.76780923932029));
#384621=CARTESIAN_POINT('Ctrl Pts',(2.11869329060088,1.75506513153933,8.76988516158374));
#384622=CARTESIAN_POINT('Ctrl Pts',(2.11397596434524,1.7609713328053,8.77093053738833));
#384623=CARTESIAN_POINT('Ctrl Pts',(2.11512986973762,1.74665445352438,8.75371302330492));
#384624=CARTESIAN_POINT('Ctrl Pts',(2.11810001922979,1.75365762518884,8.75300828287559));
#384625=CARTESIAN_POINT('Ctrl Pts',(2.11318880327527,1.75951206770563,8.75267964240738));
#384626=CARTESIAN_POINT('Origin',(2.09823644621465,1.73876750219138,8.78727029226991));
#384627=CARTESIAN_POINT('Ctrl Pts',(2.08196763624129,1.6680374052101,8.85049129520029));
#384628=CARTESIAN_POINT('Ctrl Pts',(2.0842372475259,1.67341792347881,8.85711686593484));
#384629=CARTESIAN_POINT('Ctrl Pts',(2.07732546348031,1.6784506169347,8.85933012996512));
#384630=CARTESIAN_POINT('Ctrl Pts',(2.09124314128407,1.690026643928,8.82945683644723));
#384631=CARTESIAN_POINT('Ctrl Pts',(2.09353159171458,1.69545182375145,8.83607469902391));
#384632=CARTESIAN_POINT('Ctrl Pts',(2.08657743994751,1.70046897590166,8.8382956714852));
#384633=CARTESIAN_POINT('Ctrl Pts',(2.10050482043859,1.71198310591235,8.80838214965002));
#384634=CARTESIAN_POINT('Ctrl Pts',(2.10280230216297,1.7174296960284,8.81501364461992));
#384635=CARTESIAN_POINT('Ctrl Pts',(2.09581599798245,1.72245367517765,8.81722098428721));
#384636=CARTESIAN_POINT('Ctrl Pts',(2.10975372425558,1.73390928168096,8.78727029226991));
#384637=CARTESIAN_POINT('Ctrl Pts',(2.11205158759921,1.73935677649348,8.79393457792714));
#384638=CARTESIAN_POINT('Ctrl Pts',(2.10504217505419,1.74440727656298,8.79610912703474));
#384639=CARTESIAN_POINT('Origin',(2.07045035820036,1.67289562572052,8.85049129520029));
#384640=CARTESIAN_POINT('Ctrl Pts',(2.08949760778586,1.65859511954948,8.85049129520029));
#384641=CARTESIAN_POINT('Ctrl Pts',(2.09524826125079,1.65961054899033,8.85711686593484));
#384642=CARTESIAN_POINT('Ctrl Pts',(2.09861675793327,1.65175217815318,8.85933012996512));
#384643=CARTESIAN_POINT('Ctrl Pts',(2.084410087677,1.65769678378104,8.86332496987232));
#384644=CARTESIAN_POINT('Ctrl Pts',(2.08750642900989,1.654266832655,8.86648636486737));
#384645=CARTESIAN_POINT('Ctrl Pts',(2.08438123385196,1.64925591885436,8.87206031107456));
#384646=CARTESIAN_POINT('Ctrl Pts',(2.07994609963852,1.66324499221154,8.86341338519877));
#384647=CARTESIAN_POINT('Ctrl Pts',(2.07725942010221,1.6670206012622,8.86654584966059));
#384648=CARTESIAN_POINT('Ctrl Pts',(2.07167862812148,1.66502587981416,8.87215952290715));
#384649=CARTESIAN_POINT('Ctrl Pts',(2.08196763624129,1.6680374052101,8.85049129520029));
#384650=CARTESIAN_POINT('Ctrl Pts',(2.0842372475259,1.67341792347881,8.85711686593484));
#384651=CARTESIAN_POINT('Ctrl Pts',(2.07732546348031,1.6784506169347,8.85933012996512));
#384652=CARTESIAN_POINT('Origin',(2.0916711870987,1.64628554794967,8.85049129520029));
#384653=CARTESIAN_POINT('Ctrl Pts',(2.15990092504103,1.67102668085121,8.78727029226991));
#384654=CARTESIAN_POINT('Ctrl Pts',(2.16572316248255,1.67205475032988,8.79393457792714));
#384655=CARTESIAN_POINT('Ctrl Pts',(2.16908729494478,1.66409723639934,8.79610912703474));
#384656=CARTESIAN_POINT('Ctrl Pts',(2.13646640956136,1.66688869947306,8.80838214965001));
#384657=CARTESIAN_POINT('Ctrl Pts',(2.14228768007071,1.66791659821439,8.81501364461984));
#384658=CARTESIAN_POINT('Ctrl Pts',(2.14563109864245,1.65998751473334,8.81722098428721));
#384659=CARTESIAN_POINT('Ctrl Pts',(2.1129995244246,1.66274500237877,8.82945683644722));
#384660=CARTESIAN_POINT('Ctrl Pts',(2.1187979117902,1.66376886049793,8.83607469902389));
#384661=CARTESIAN_POINT('Ctrl Pts',(2.12214182911501,1.65587264245243,8.83829567148519));
#384662=CARTESIAN_POINT('Ctrl Pts',(2.08949760778586,1.65859511954948,8.85049129520029));
#384663=CARTESIAN_POINT('Ctrl Pts',(2.0952482612508,1.65961054899033,8.85711686593484));
#384664=CARTESIAN_POINT('Ctrl Pts',(2.09861675793327,1.65175217815318,8.85933012996512));
#384665=CARTESIAN_POINT('Origin',(2.16207450435387,1.6587171092514,8.78727029226991));
#384666=CARTESIAN_POINT('Ctrl Pts',(2.17352754522994,1.67343280107383,8.75374538247848));
#384667=CARTESIAN_POINT('Ctrl Pts',(2.18100845961528,1.67476707928574,8.75304829418602));
#384668=CARTESIAN_POINT('Ctrl Pts',(2.18562287639598,1.66868614177719,8.75272238421917));
#384669=CARTESIAN_POINT('Ctrl Pts',(2.17482741984481,1.67366232863142,8.76769408445018));
#384670=CARTESIAN_POINT('Ctrl Pts',(2.18249670840253,1.6750295038178,8.76974318093969));
#384671=CARTESIAN_POINT('Ctrl Pts',(2.18720283100793,1.66912435629186,8.7707786988043));
#384672=CARTESIAN_POINT('Ctrl Pts',(2.16816500305613,1.67248590113901,8.78108014887992));
#384673=CARTESIAN_POINT('Ctrl Pts',(2.17466378204077,1.67364827328636,8.78639403366325));
#384674=CARTESIAN_POINT('Ctrl Pts',(2.17911116346538,1.66688492543247,8.78812224174741));
#384675=CARTESIAN_POINT('Ctrl Pts',(2.15724677268912,1.67055799614335,8.78944554828685));
#384676=CARTESIAN_POINT('Ctrl Pts',(2.16272271709833,1.67154311057535,8.79673892988686));
#384677=CARTESIAN_POINT('Ctrl Pts',(2.16589194367167,1.66320887052341,8.79894799272499));
#384678=CARTESIAN_POINT('Origin',(2.17588346166996,1.66115544463218,8.75721825406948));
#384679=CARTESIAN_POINT('Origin',(2.17588346166996,1.66115544463218,9.));
#384680=CARTESIAN_POINT('Origin',(2.17588346166996,1.66115544463218,7.51860402984325));
#384681=CARTESIAN_POINT('Ctrl Pts',(2.17134121231119,1.68156177827834,7.50366195182966));
#384682=CARTESIAN_POINT('Ctrl Pts',(2.17423646662311,1.68380396341327,7.50000065167735));
#384683=CARTESIAN_POINT('Ctrl Pts',(2.17423646662319,1.68380396341318,7.49482233047108));
#384684=CARTESIAN_POINT('Ctrl Pts',(2.17699188179938,1.67672197105678,7.50215800491337));
#384685=CARTESIAN_POINT('Ctrl Pts',(2.18007365240861,1.67626657333344,7.49877273257267));
#384686=CARTESIAN_POINT('Ctrl Pts',(2.18218737990695,1.6735372304798,7.49481816995647));
#384687=CARTESIAN_POINT('Ctrl Pts',(2.17648546961679,1.67395546368404,7.51043025814042));
#384688=CARTESIAN_POINT('Ctrl Pts',(2.18229374397787,1.67335821504792,7.51006209594515));
#384689=CARTESIAN_POINT('Ctrl Pts',(2.18582053896441,1.66873861687436,7.507312818217));
#384690=CARTESIAN_POINT('Ctrl Pts',(2.17370839399077,1.67346475332889,7.51860402984326));
#384691=CARTESIAN_POINT('Ctrl Pts',(2.1812015840384,1.67478880782198,7.51860402984326));
#384692=CARTESIAN_POINT('Ctrl Pts',(2.18581900259084,1.66874062931087,7.51860402984327));
#384693=CARTESIAN_POINT('Origin',(0.,0.,7.5));
#384694=CARTESIAN_POINT('Origin',(2.19147106502122,1.52131278661258,7.5));
#384695=CARTESIAN_POINT('',(2.19147106502122,1.52131278661258,7.59394543036555));
#384696=CARTESIAN_POINT('',(2.19147106502122,1.52131278661258,8.85049129520029));
#384697=CARTESIAN_POINT('',(2.19147106502122,1.52131278661258,7.5));
#384698=CARTESIAN_POINT('',(2.26252622397766,1.52920804991442,8.78727029226991));
#384699=CARTESIAN_POINT('Ctrl Pts',(2.19147106502122,1.52131278661258,8.85049129520029));
#384700=CARTESIAN_POINT('Ctrl Pts',(2.21519054652499,1.52394836655647,8.82945686509571));
#384701=CARTESIAN_POINT('Ctrl Pts',(2.2388747661514,1.52658002839208,8.80838212259897));
#384702=CARTESIAN_POINT('Ctrl Pts',(2.26252622397766,1.52920804991442,8.78727029226991));
#384703=CARTESIAN_POINT('',(2.27646303399418,1.53075663254071,8.75721825406948));
#384704=CARTESIAN_POINT('Origin',(2.23452231565462,1.52609661077913,8.75937679713095));
#384705=CARTESIAN_POINT('',(2.27646303399418,1.53075663254071,7.51860402984325));
#384706=CARTESIAN_POINT('',(2.27646303399418,1.53075663254071,7.5));
#384707=CARTESIAN_POINT('Ctrl Pts',(2.27646303399418,1.53075663254071,7.51860402984325));
#384708=CARTESIAN_POINT('Ctrl Pts',(2.26551783731016,1.52954046173792,7.52834476460825));
#384709=CARTESIAN_POINT('Ctrl Pts',(2.2545655351624,1.5283235014146,7.53807742314407));
#384710=CARTESIAN_POINT('Ctrl Pts',(2.24360588897548,1.52710572506153,7.54780169004674));
#384711=CARTESIAN_POINT('Ctrl Pts',(2.22624640173374,1.52517683313347,7.5632044032688));
#384712=CARTESIAN_POINT('Ctrl Pts',(2.20886846717178,1.52324589143937,7.57858609112103));
#384713=CARTESIAN_POINT('Ctrl Pts',(2.19147106502122,1.52131278661258,7.59394543036555));
#384714=CARTESIAN_POINT('Origin',(2.30745690681614,1.77722975964338,7.5));
#384715=CARTESIAN_POINT('',(2.22277754110614,1.60771882366398,8.75721825406948));
#384716=CARTESIAN_POINT('',(2.21651095806262,1.59517439388238,8.78727029226991));
#384717=CARTESIAN_POINT('Origin',(2.20060403297873,1.56333195225666,8.75658640621012));
#384718=CARTESIAN_POINT('',(2.18456153393017,1.53121811901794,8.85049129520029));
#384719=CARTESIAN_POINT('Ctrl Pts',(2.21651095806262,1.59517439388238,8.78727029226991));
#384720=CARTESIAN_POINT('Ctrl Pts',(2.20587625583212,1.57388587437305,8.80838212259895));
#384721=CARTESIAN_POINT('Ctrl Pts',(2.19522682250169,1.55256786618587,8.82945686509571));
#384722=CARTESIAN_POINT('Ctrl Pts',(2.18456153393017,1.53121811901794,8.85049129520029));
#384723=CARTESIAN_POINT('',(2.18456153393017,1.53121811901794,7.59394543036555));
#384724=CARTESIAN_POINT('',(2.18456153393017,1.53121811901794,7.5));
#384725=CARTESIAN_POINT('',(2.22277754110614,1.60771882366398,7.51860402984325));
#384726=CARTESIAN_POINT('Ctrl Pts',(2.18456153393017,1.53121811901794,7.59394543036555));
#384727=CARTESIAN_POINT('Ctrl Pts',(2.19238414650714,1.54687740470824,7.57858609112103));
#384728=CARTESIAN_POINT('Ctrl Pts',(2.20019800562749,1.56251916775162,7.56320440326857));
#384729=CARTESIAN_POINT('Ctrl Pts',(2.20800357004749,1.57814432648526,7.54780169004651));
#384730=CARTESIAN_POINT('Ctrl Pts',(2.21293149350175,1.58800903095208,7.53807742314383));
#384731=CARTESIAN_POINT('Ctrl Pts',(2.21785611476347,1.5978671250984,7.52834476460825));
#384732=CARTESIAN_POINT('Ctrl Pts',(2.22277754110614,1.60771882366398,7.51860402984324));
#384733=CARTESIAN_POINT('',(2.22277754110614,1.60771882366398,7.5));
#384734=CARTESIAN_POINT('Origin',(2.19071182494581,1.52814573469579,7.5));
#384735=CARTESIAN_POINT('Ctrl Pts',(2.18456153393017,1.53121811901794,8.85049129520029));
#384736=CARTESIAN_POINT('Ctrl Pts',(2.18447498810114,1.5310448718005,8.85097269580138));
#384737=CARTESIAN_POINT('Ctrl Pts',(2.18439705895476,1.53087005142217,8.85143669361005));
#384738=CARTESIAN_POINT('Ctrl Pts',(2.18432495664554,1.53068525200686,8.8519052845931));
#384739=CARTESIAN_POINT('Ctrl Pts',(2.18418392910125,1.53032379607009,8.85282181883899));
#384740=CARTESIAN_POINT('Ctrl Pts',(2.18406900446171,1.52993339018138,8.85372622499635));
#384741=CARTESIAN_POINT('Ctrl Pts',(2.18399317054836,1.52950355408832,8.8546225773507));
#384742=CARTESIAN_POINT('Ctrl Pts',(2.18393021592686,1.5291467194302,8.85536669723986));
#384743=CARTESIAN_POINT('Ctrl Pts',(2.18389415610195,1.52876263466292,8.85610498449051));
#384744=CARTESIAN_POINT('Ctrl Pts',(2.18390038630543,1.52834452303799,8.85681338218371));
#384745=CARTESIAN_POINT('Ctrl Pts',(2.18390604022486,1.52796508608171,8.85745625420285));
#384746=CARTESIAN_POINT('Ctrl Pts',(2.18394599498022,1.52755285743403,8.85808743050667));
#384747=CARTESIAN_POINT('Ctrl Pts',(2.18404711722398,1.5270980376494,8.85866804508412));
#384748=CARTESIAN_POINT('Ctrl Pts',(2.18409377283519,1.52688819366007,8.85893592806397));
#384749=CARTESIAN_POINT('Ctrl Pts',(2.18415368514344,1.52666922800998,8.85919241173849));
#384750=CARTESIAN_POINT('Ctrl Pts',(2.18423108248649,1.52644003474421,8.85943017985534));
#384751=CARTESIAN_POINT('Ctrl Pts',(2.18433559181169,1.52613055598694,8.8597512372));
#384752=CARTESIAN_POINT('Ctrl Pts',(2.1844752485065,1.52579475712462,8.86004599534705));
#384753=CARTESIAN_POINT('Ctrl Pts',(2.18465799121655,1.52544067212631,8.86026130871721));
#384754=CARTESIAN_POINT('Ctrl Pts',(2.18472489847476,1.52531103162571,8.86034014101235));
#384755=CARTESIAN_POINT('Ctrl Pts',(2.18479857547463,1.52517698687706,8.86040910639693));
#384756=CARTESIAN_POINT('Ctrl Pts',(2.18487730971223,1.52504235188111,8.86046313645507));
#384757=CARTESIAN_POINT('Ctrl Pts',(2.18500017383062,1.52483225509749,8.8605474499083));
#384758=CARTESIAN_POINT('Ctrl Pts',(2.18513883375113,1.52461506020086,8.86059655985669));
#384759=CARTESIAN_POINT('Ctrl Pts',(2.18528414986346,1.52440453891959,8.86059725258816));
#384760=CARTESIAN_POINT('Ctrl Pts',(2.18542980171406,1.52419353125006,8.86059794692012));
#384761=CARTESIAN_POINT('Ctrl Pts',(2.18558594230477,1.52398839721479,8.86056369958366));
#384762=CARTESIAN_POINT('Ctrl Pts',(2.18574106129467,1.52379804572741,8.86048590497774));
#384763=CARTESIAN_POINT('Ctrl Pts',(2.18578154273259,1.52374836965665,8.86046560290182));
#384764=CARTESIAN_POINT('Ctrl Pts',(2.18582255145108,1.52369911132097,8.86044257503091));
#384765=CARTESIAN_POINT('Ctrl Pts',(2.18586279501898,1.52365177184096,8.86041778462583));
#384766=CARTESIAN_POINT('Ctrl Pts',(2.18613358429284,1.52333323588391,8.860250975962));
#384767=CARTESIAN_POINT('Ctrl Pts',(2.18640631964951,1.52305905007567,8.8599848982295));
#384768=CARTESIAN_POINT('Ctrl Pts',(2.18666703383915,1.52283124213453,8.85968173251461));
#384769=CARTESIAN_POINT('Ctrl Pts',(2.18680493670833,1.5227107447855,8.85952137522076));
#384770=CARTESIAN_POINT('Ctrl Pts',(2.18694200881964,1.52260075658168,8.85934740853961));
#384771=CARTESIAN_POINT('Ctrl Pts',(2.18707534425058,1.52250161612592,8.8591675900182));
#384772=CARTESIAN_POINT('Ctrl Pts',(2.18761075531216,1.52210351566387,8.85844552518697));
#384773=CARTESIAN_POINT('Ctrl Pts',(2.18811436935617,1.52185540067338,8.85759444184127));
#384774=CARTESIAN_POINT('Ctrl Pts',(2.18854315989624,1.52168998323701,8.85683498915143));
#384775=CARTESIAN_POINT('Ctrl Pts',(2.1885880316843,1.52167267274283,8.85675551445001));
#384776=CARTESIAN_POINT('Ctrl Pts',(2.18863208747595,1.5216562875519,8.85667699793653));
#384777=CARTESIAN_POINT('Ctrl Pts',(2.18867527952879,1.52164076359269,8.85659965593547));
#384778=CARTESIAN_POINT('Ctrl Pts',(2.18925828806186,1.52143122039922,8.85555568965886));
#384779=CARTESIAN_POINT('Ctrl Pts',(2.18984885756595,1.52131403437627,8.85434650606346));
#384780=CARTESIAN_POINT('Ctrl Pts',(2.19044869788362,1.5212825303358,8.85297329937117));
#384781=CARTESIAN_POINT('Ctrl Pts',(2.19078607151351,1.5212648112326,8.85220095427747));
#384782=CARTESIAN_POINT('Ctrl Pts',(2.19112653220932,1.52127450399798,8.85137579139184));
#384783=CARTESIAN_POINT('Ctrl Pts',(2.19147106502122,1.52131278661258,8.85049129520029));
#384784=CARTESIAN_POINT('Origin',(2.19071182494581,1.52814573469579,7.59394543036555));
#384785=CARTESIAN_POINT('Ctrl Pts',(2.18431026219254,1.53071512390131,7.59443877723642));
#384786=CARTESIAN_POINT('Ctrl Pts',(2.18172240506209,1.52553475816895,7.58783886950016));
#384787=CARTESIAN_POINT('Ctrl Pts',(2.1882334017743,1.52008626265639,7.58559994247159));
#384788=CARTESIAN_POINT('Ctrl Pts',(2.19843729834314,1.55899458844884,7.56670252222137));
#384789=CARTESIAN_POINT('Ctrl Pts',(2.19585318140098,1.55382170981567,7.56004874999025));
#384790=CARTESIAN_POINT('Ctrl Pts',(2.20238904649608,1.54832454466312,7.55786368756705));
#384791=CARTESIAN_POINT('Ctrl Pts',(2.21253795366518,1.58722124392178,7.53888913333555));
#384792=CARTESIAN_POINT('Ctrl Pts',(2.20993847918948,1.58201762261761,7.53222002137274));
#384793=CARTESIAN_POINT('Ctrl Pts',(2.2165177157845,1.57651161766423,7.53005029815326));
#384794=CARTESIAN_POINT('Ctrl Pts',(2.2266115900945,1.6153938130449,7.51101258149734));
#384795=CARTESIAN_POINT('Ctrl Pts',(2.2239806052648,1.61012711439534,7.5043616886572));
#384796=CARTESIAN_POINT('Ctrl Pts',(2.23061878545708,1.60464605197284,7.50217374673251));
#384797=CARTESIAN_POINT('',(2.22986633334691,1.60314476287809,7.50366116523517));
#384798=CARTESIAN_POINT('Ctrl Pts',(2.22277754110614,1.60771882366398,7.51860402984325));
#384799=CARTESIAN_POINT('Ctrl Pts',(2.22297489374257,1.60811388366282,7.51734760759493));
#384800=CARTESIAN_POINT('Ctrl Pts',(2.22320645518634,1.60844428819931,7.51608817408572));
#384801=CARTESIAN_POINT('Ctrl Pts',(2.22348262824041,1.60870161333811,7.51481005913119));
#384802=CARTESIAN_POINT('Ctrl Pts',(2.22373279239216,1.60893470459783,7.51365231206383));
#384803=CARTESIAN_POINT('Ctrl Pts',(2.22401974321264,1.60910834456725,7.51247773061042));
#384804=CARTESIAN_POINT('Ctrl Pts',(2.22435763202005,1.6091879372905,7.51129758471022));
#384805=CARTESIAN_POINT('Ctrl Pts',(2.22477758921932,1.60928686195567,7.50983079813402));
#384806=CARTESIAN_POINT('Ctrl Pts',(2.22526581718583,1.6092246709332,7.50839324291155));
#384807=CARTESIAN_POINT('Ctrl Pts',(2.22581546211117,1.60891913153021,7.50715379678855));
#384808=CARTESIAN_POINT('Ctrl Pts',(2.22606938222903,1.60877798112993,7.50658120839351));
#384809=CARTESIAN_POINT('Ctrl Pts',(2.22636789030146,1.60855652531024,7.50598221009429));
#384810=CARTESIAN_POINT('Ctrl Pts',(2.2266903295381,1.6082417662198,7.50545747549611));
#384811=CARTESIAN_POINT('Ctrl Pts',(2.2268623930952,1.60807380102644,7.50517746087247));
#384812=CARTESIAN_POINT('Ctrl Pts',(2.22704327857472,1.60787759016945,7.50491486231392));
#384813=CARTESIAN_POINT('Ctrl Pts',(2.22722696943706,1.60765719904465,7.50468370960993));
#384814=CARTESIAN_POINT('Ctrl Pts',(2.22750164521827,1.60732764479464,7.50433806340447));
#384815=CARTESIAN_POINT('Ctrl Pts',(2.22779040260931,1.60693378573887,7.50405484070984));
#384816=CARTESIAN_POINT('Ctrl Pts',(2.22807321658151,1.60650172397165,7.50385766036131));
#384817=CARTESIAN_POINT('Ctrl Pts',(2.22810345913991,1.6064555216814,7.50383657498791));
#384818=CARTESIAN_POINT('Ctrl Pts',(2.22813363242864,1.60640891087605,7.50381643264937));
#384819=CARTESIAN_POINT('Ctrl Pts',(2.22816371133268,1.60636194407088,7.50379723213559));
#384820=CARTESIAN_POINT('Ctrl Pts',(2.2283644978566,1.60604842528248,7.50366906242519));
#384821=CARTESIAN_POINT('Ctrl Pts',(2.22856484065418,1.60571183559281,7.50358235568538));
#384822=CARTESIAN_POINT('Ctrl Pts',(2.22875014780003,1.60538276269127,7.5035341175365));
#384823=CARTESIAN_POINT('Ctrl Pts',(2.22902799489252,1.60488935511926,7.50346178989176));
#384824=CARTESIAN_POINT('Ctrl Pts',(2.22930591601756,1.6043467471144,7.50346967198527));
#384825=CARTESIAN_POINT('Ctrl Pts',(2.22956235809398,1.60380567910417,7.50354272648692));
#384826=CARTESIAN_POINT('Ctrl Pts',(2.22966783802804,1.60358312663211,7.50357277531559));
#384827=CARTESIAN_POINT('Ctrl Pts',(2.22976967202095,1.60336119113261,7.50361331098761));
#384828=CARTESIAN_POINT('Ctrl Pts',(2.22986633334807,1.60314476287892,7.50366116523658));
#384829=CARTESIAN_POINT('',(2.19311322794422,1.52982084947219,7.57603338622103));
#384830=CARTESIAN_POINT('Origin',(2.2003626720401,1.5348742690979,7.58486873427626));
#384831=CARTESIAN_POINT('Ctrl Pts',(2.22986633336771,1.60314476293154,7.50366116529969));
#384832=CARTESIAN_POINT('Ctrl Pts',(2.21763603662394,1.5787429670886,7.52783573079709));
#384833=CARTESIAN_POINT('Ctrl Pts',(2.2053855959453,1.55430280858918,7.55196141284069));
#384834=CARTESIAN_POINT('Ctrl Pts',(2.19311322816629,1.5298208507044,7.57603338728831));
#384835=CARTESIAN_POINT('Ctrl Pts',(2.18456153393017,1.53121811901794,7.59394543036555));
#384836=CARTESIAN_POINT('Ctrl Pts',(2.17891644017658,1.51991778489476,7.59394543036555));
#384837=CARTESIAN_POINT('Ctrl Pts',(2.19147106502122,1.52131278661258,7.59394543036555));
#384838=CARTESIAN_POINT('Ctrl Pts',(2.18351888218448,1.52913094144132,7.58587155981958));
#384839=CARTESIAN_POINT('Ctrl Pts',(2.18371352266054,1.52326402197321,7.58685956158229));
#384840=CARTESIAN_POINT('Ctrl Pts',(2.18915221929746,1.52105512907139,7.5858715598196));
#384841=CARTESIAN_POINT('Ctrl Pts',(2.1889122721287,1.52920781474962,7.57982961904599));
#384842=CARTESIAN_POINT('Ctrl Pts',(2.18864592315211,1.52670465103575,7.58148017275035));
#384843=CARTESIAN_POINT('Ctrl Pts',(2.19108705088151,1.52609010586745,7.57982961904595));
#384844=CARTESIAN_POINT('Ctrl Pts',(2.19311322726536,1.52982084899889,7.57603338509286));
#384845=CARTESIAN_POINT('Ctrl Pts',(2.19311322726536,1.52982084899889,7.57603338509286));
#384846=CARTESIAN_POINT('Ctrl Pts',(2.19311322726536,1.52982084899889,7.57603338509286));
#384847=CARTESIAN_POINT('Origin',(2.20035940734063,1.53487894928969,7.58486873427622));
#384848=CARTESIAN_POINT('Ctrl Pts',(2.28501686554783,1.53170708783977,7.51098857897448));
#384849=CARTESIAN_POINT('Ctrl Pts',(2.27916555827344,1.5310569223589,7.50433767179956));
#384850=CARTESIAN_POINT('Ctrl Pts',(2.27631435376174,1.53917964874325,7.50214974420965));
#384851=CARTESIAN_POINT('Ctrl Pts',(2.25370825427413,1.52822824501891,7.53887321589169));
#384852=CARTESIAN_POINT('Ctrl Pts',(2.24792705604506,1.52758586967435,7.53220407452061));
#384853=CARTESIAN_POINT('Ctrl Pts',(2.24503206325587,1.53566187962185,7.53003438070912));
#384854=CARTESIAN_POINT('Ctrl Pts',(2.22233951891749,1.52474272153654,7.56669465659231));
#384855=CARTESIAN_POINT('Ctrl Pts',(2.21659248649519,1.52410414251075,7.56004085833303));
#384856=CARTESIAN_POINT('Ctrl Pts',(2.21369080731581,1.53213638429418,7.55785582193789));
#384857=CARTESIAN_POINT('Ctrl Pts',(2.1909120781603,1.52125067502893,7.59443891967696));
#384858=CARTESIAN_POINT('Ctrl Pts',(2.18515671325648,1.52061117014313,7.58783901202978));
#384859=CARTESIAN_POINT('Ctrl Pts',(2.18229214298249,1.52860325467307,7.58560008491213));
#384860=CARTESIAN_POINT('',(2.2746186435041,1.53898896096139,7.50366116523517));
#384861=CARTESIAN_POINT('Ctrl Pts',(2.27461864350441,1.5389889609616,7.50366116523554));
#384862=CARTESIAN_POINT('Ctrl Pts',(2.27516108906422,1.53845991433661,7.50350835821027));
#384863=CARTESIAN_POINT('Ctrl Pts',(2.27564251620969,1.53795594418399,7.50345484956));
#384864=CARTESIAN_POINT('Ctrl Pts',(2.27607767238033,1.53746248185762,7.50349758195598));
#384865=CARTESIAN_POINT('Ctrl Pts',(2.27630093976789,1.53720929908808,7.50351950684424));
#384866=CARTESIAN_POINT('Ctrl Pts',(2.27653412976725,1.53693401335554,7.50357029184312));
#384867=CARTESIAN_POINT('Ctrl Pts',(2.27675169537736,1.53666237746656,7.50365515313923));
#384868=CARTESIAN_POINT('Ctrl Pts',(2.27708639938673,1.53624449147307,7.50378570417639));
#384869=CARTESIAN_POINT('Ctrl Pts',(2.27739422114994,1.53582319390499,7.50400001621911));
#384870=CARTESIAN_POINT('Ctrl Pts',(2.27764989774496,1.53542921218324,7.50428903009635));
#384871=CARTESIAN_POINT('Ctrl Pts',(2.27767827587995,1.53538548324324,7.50432110841318));
#384872=CARTESIAN_POINT('Ctrl Pts',(2.27770603964484,1.53534207924713,7.50435406373354));
#384873=CARTESIAN_POINT('Ctrl Pts',(2.27773317506314,1.53529903339035,7.50438785222352));
#384874=CARTESIAN_POINT('Ctrl Pts',(2.27789884983481,1.53503621774428,7.50459414719561));
#384875=CARTESIAN_POINT('Ctrl Pts',(2.27804330321255,1.53478229309384,7.50483629897752));
#384876=CARTESIAN_POINT('Ctrl Pts',(2.2781621451176,1.53454763795564,7.5050991045531));
#384877=CARTESIAN_POINT('Ctrl Pts',(2.27842432229668,1.53402996515189,7.50567888004914));
#384878=CARTESIAN_POINT('Ctrl Pts',(2.27857264696128,1.53358591053843,7.50637912803144));
#384879=CARTESIAN_POINT('Ctrl Pts',(2.27863797653864,1.53321727343213,7.50710440483569));
#384880=CARTESIAN_POINT('Ctrl Pts',(2.27865399664798,1.53312687629519,7.50728225710685));
#384881=CARTESIAN_POINT('Ctrl Pts',(2.27866548865362,1.53303924015847,7.50746498566954));
#384882=CARTESIAN_POINT('Ctrl Pts',(2.27867259735184,1.53295646489846,7.50764697238949));
#384883=CARTESIAN_POINT('Ctrl Pts',(2.27871081175707,1.53251148788106,7.50862528291181));
#384884=CARTESIAN_POINT('Ctrl Pts',(2.2786299483616,1.53216694270045,7.5096585683742));
#384885=CARTESIAN_POINT('Ctrl Pts',(2.27848810672668,1.53189089447242,7.510679598732));
#384886=CARTESIAN_POINT('Ctrl Pts',(2.27841005109606,1.53173898478435,7.51124147302577));
#384887=CARTESIAN_POINT('Ctrl Pts',(2.27831312390071,1.5316079795929,7.51180065547252));
#384888=CARTESIAN_POINT('Ctrl Pts',(2.27820463850914,1.5314938856342,7.512351757165));
#384889=CARTESIAN_POINT('Ctrl Pts',(2.2778297782658,1.53109964555726,7.51425603304536));
#384890=CARTESIAN_POINT('Ctrl Pts',(2.27726782574235,1.53086449499048,7.51626900505182));
#384891=CARTESIAN_POINT('Ctrl Pts',(2.27657644598837,1.53077061794521,7.51827788969245));
#384892=CARTESIAN_POINT('Ctrl Pts',(2.27653902720956,1.53076553714212,7.51838661432546));
#384893=CARTESIAN_POINT('Ctrl Pts',(2.27650122102354,1.53076087567598,7.51849533314857));
#384894=CARTESIAN_POINT('Ctrl Pts',(2.27646303399418,1.53075663254071,7.51860402984325));
#384895=CARTESIAN_POINT('Ctrl Pts',(2.19311322917842,1.52982084925552,7.57603338728985));
#384896=CARTESIAN_POINT('Ctrl Pts',(2.22032722053522,1.53288286616343,7.55196141284922));
#384897=CARTESIAN_POINT('Ctrl Pts',(2.24749441165088,1.53593874122898,7.52783573083105));
#384898=CARTESIAN_POINT('Ctrl Pts',(2.27461864356327,1.53898896096258,7.50366116530176));
#384899=CARTESIAN_POINT('Origin',(7.57821998246243E-16,5.28623820391022E-16,
7.49482233047033));
#384900=CARTESIAN_POINT('Origin',(2.22268971703919,1.59798519134824,7.49482233047033));
#384901=CARTESIAN_POINT('Origin',(0.,0.,7.50366116523517));
#384902=CARTESIAN_POINT('Origin',(2.26729799607035,1.53403586888162,7.49482233047033));
#384903=CARTESIAN_POINT('Ctrl Pts',(2.2227770683791,1.60771787746035,7.51860402984325));
#384904=CARTESIAN_POINT('Ctrl Pts',(2.22617803012196,1.61452447317728,7.51860402984325));
#384905=CARTESIAN_POINT('Ctrl Pts',(2.22169380199588,1.62067166636957,7.51860402984325));
#384906=CARTESIAN_POINT('Ctrl Pts',(2.22403986754686,1.61024521346864,7.51041458714367));
#384907=CARTESIAN_POINT('Ctrl Pts',(2.22511565711968,1.61598080781929,7.51004642900443));
#384908=CARTESIAN_POINT('Ctrl Pts',(2.22169256529901,1.62067336169246,7.50729136483011));
#384909=CARTESIAN_POINT('Ctrl Pts',(2.22683740462711,1.60993292596655,7.50215815450136));
#384910=CARTESIAN_POINT('Ctrl Pts',(2.22727886798611,1.61301564791056,7.49877163671529));
#384911=CARTESIAN_POINT('Ctrl Pts',(2.2252648615701,1.61581702288556,7.49481588533168));
#384912=CARTESIAN_POINT('Ctrl Pts',(2.22986588635879,1.60314444151893,7.50366171572174));
#384913=CARTESIAN_POINT('Ctrl Pts',(2.23283898515375,1.60528192738148,7.50000045605858));
#384914=CARTESIAN_POINT('Ctrl Pts',(2.23283898515367,1.60528192738158,7.49482233047317));
#384915=CARTESIAN_POINT('Origin',(2.21159519380499,1.61330497697698,7.51860402984325));
#384916=CARTESIAN_POINT('Origin',(2.21159519380499,1.61330497697698,9.));
#384917=CARTESIAN_POINT('Origin',(2.21159519380499,1.61330497697698,8.75721825406948));
#384918=CARTESIAN_POINT('Ctrl Pts',(2.21531434125614,1.59277907704499,8.78942910404912));
#384919=CARTESIAN_POINT('Ctrl Pts',(2.21782269718832,1.59775507736846,8.7967269950169));
#384920=CARTESIAN_POINT('Ctrl Pts',(2.21072551350638,1.6031683453063,8.79893251111267));
#384921=CARTESIAN_POINT('Ctrl Pts',(2.22022762891697,1.60261447348346,8.78111911759584));
#384922=CARTESIAN_POINT('Ctrl Pts',(2.2231946668817,1.60851693024665,8.78644465894815));
#384923=CARTESIAN_POINT('Ctrl Pts',(2.21795342948706,1.61470117978467,8.78817647674132));
#384924=CARTESIAN_POINT('Ctrl Pts',(2.22328970695173,1.60874412715453,8.76780923932029));
#384925=CARTESIAN_POINT('Ctrl Pts',(2.2267876170644,1.61571401679599,8.76988516158372));
#384926=CARTESIAN_POINT('Ctrl Pts',(2.22245839467584,1.62191032326894,8.77093053738833));
#384927=CARTESIAN_POINT('Ctrl Pts',(2.22269264364087,1.60754892857964,8.75371302330492));
#384928=CARTESIAN_POINT('Ctrl Pts',(2.22610538539147,1.61434741334549,8.7530082828756));
#384929=CARTESIAN_POINT('Ctrl Pts',(2.22157935547677,1.62050448996882,8.75267964240738));
#384930=CARTESIAN_POINT('Origin',(2.20532861076146,1.60076054719537,8.78727029226991));
#384931=CARTESIAN_POINT('Ctrl Pts',(2.18456153393017,1.53121811901794,8.85049129520029));
#384932=CARTESIAN_POINT('Ctrl Pts',(2.18717121304407,1.53644216794053,8.85711686593484));
#384933=CARTESIAN_POINT('Ctrl Pts',(2.1805960757769,1.54190736071222,8.85933012996512));
#384934=CARTESIAN_POINT('Ctrl Pts',(2.1952268368149,1.55256789483802,8.82945683644723));
#384935=CARTESIAN_POINT('Ctrl Pts',(2.19785817784331,1.55783530652517,8.83607469902391));
#384936=CARTESIAN_POINT('Ctrl Pts',(2.19123976416882,1.5632877044317,8.8382956714852));
#384937=CARTESIAN_POINT('Ctrl Pts',(2.20587624220564,1.57388584709559,8.80838214965001));
#384938=CARTESIAN_POINT('Ctrl Pts',(2.20851796773429,1.57917404644857,8.81501364461986));
#384939=CARTESIAN_POINT('Ctrl Pts',(2.20186790511425,1.5846353173396,8.81722098428721));
#384940=CARTESIAN_POINT('Ctrl Pts',(2.21651095806262,1.59517439388238,8.78727029226991));
#384941=CARTESIAN_POINT('Ctrl Pts',(2.21915312239054,1.60046347162265,8.79393457792714));
#384942=CARTESIAN_POINT('Ctrl Pts',(2.21248169808583,1.60595268950179,8.79610912703474));
#384943=CARTESIAN_POINT('Origin',(2.17337918662901,1.53680427233094,8.85049129520029));
#384944=CARTESIAN_POINT('Ctrl Pts',(2.19147106502122,1.52131278661258,8.85049129520029));
#384945=CARTESIAN_POINT('Ctrl Pts',(2.19727496193951,1.52195768411221,8.85711686593484));
#384946=CARTESIAN_POINT('Ctrl Pts',(2.20013305013605,1.51389963881731,8.85933012996512));
#384947=CARTESIAN_POINT('Ctrl Pts',(2.18633644119775,1.52074225510386,8.86332496987232));
#384948=CARTESIAN_POINT('Ctrl Pts',(2.18920666304212,1.51712096790994,8.86648636486738));
#384949=CARTESIAN_POINT('Ctrl Pts',(2.1857668385833,1.51232058151036,8.87206031107458));
#384950=CARTESIAN_POINT('Ctrl Pts',(2.1822370998361,1.5265650728407,8.86341338519875));
#384951=CARTESIAN_POINT('Ctrl Pts',(2.17979784447348,1.53050506064651,8.86654584966054));
#384952=CARTESIAN_POINT('Ctrl Pts',(2.17410071658646,1.52887200013753,8.87215952290714));
#384953=CARTESIAN_POINT('Ctrl Pts',(2.18456153393017,1.53121811901794,8.85049129520029));
#384954=CARTESIAN_POINT('Ctrl Pts',(2.18717121304407,1.53644216794053,8.85711686593484));
#384955=CARTESIAN_POINT('Ctrl Pts',(2.1805960757769,1.54190736071222,8.85933012996512));
#384956=CARTESIAN_POINT('Origin',(2.19285150152198,1.5088892446431,8.85049129520029));
#384957=CARTESIAN_POINT('Ctrl Pts',(2.26252622397766,1.52920804991442,8.78727029226991));
#384958=CARTESIAN_POINT('Ctrl Pts',(2.26840236764558,1.52986097508044,8.79393457792714));
#384959=CARTESIAN_POINT('Ctrl Pts',(2.27124974846883,1.5217042700088,8.79610912703474));
#384960=CARTESIAN_POINT('Ctrl Pts',(2.23887473584625,1.52658002502474,8.80838214965003));
#384961=CARTESIAN_POINT('Ctrl Pts',(2.24474990362954,1.52723284175577,8.81501364461996));
#384962=CARTESIAN_POINT('Ctrl Pts',(2.24757843466629,1.51910583586372,8.81722098428721));
#384963=CARTESIAN_POINT('Ctrl Pts',(2.21519057835741,1.52394837009352,8.82945683644722));
#384964=CARTESIAN_POINT('Ctrl Pts',(2.22104265112922,1.52459862063229,8.83607469902388));
#384965=CARTESIAN_POINT('Ctrl Pts',(2.22387378559008,1.51650438069503,8.8382956714852));
#384966=CARTESIAN_POINT('Ctrl Pts',(2.19147106502122,1.52131278661258,8.85049129520029));
#384967=CARTESIAN_POINT('Ctrl Pts',(2.19727496193951,1.52195768411221,8.85711686593484));
#384968=CARTESIAN_POINT('Ctrl Pts',(2.20013305013605,1.51389963881731,8.85933012996512));
#384969=CARTESIAN_POINT('Origin',(2.26390666047842,1.51678450794494,8.78727029226991));
#384970=CARTESIAN_POINT('Ctrl Pts',(2.27627900746589,1.53073616595189,8.75374538247848));
#384971=CARTESIAN_POINT('Ctrl Pts',(2.28383003900886,1.5315883989158,8.75304829418602));
#384972=CARTESIAN_POINT('Ctrl Pts',(2.28804536797154,1.52522430864732,8.75272238421917));
#384973=CARTESIAN_POINT('Ctrl Pts',(2.27759091723008,1.53088193866798,8.76769408445019));
#384974=CARTESIAN_POINT('Ctrl Pts',(2.28533204362688,1.53175493184133,8.76974318093969));
#384975=CARTESIAN_POINT('Ctrl Pts',(2.28965015289764,1.52556039476371,8.77077869880429));
#384976=CARTESIAN_POINT('Ctrl Pts',(2.27086681512296,1.53013479078127,8.78108014887989));
#384977=CARTESIAN_POINT('Ctrl Pts',(2.2774267151084,1.53087839651125,8.78639403366324));
#384978=CARTESIAN_POINT('Ctrl Pts',(2.28143162972609,1.52384399997467,8.78812224174741));
#384979=CARTESIAN_POINT('Ctrl Pts',(2.25984749613408,1.52891038029461,8.78944554828685));
#384980=CARTESIAN_POINT('Ctrl Pts',(2.26537530612658,1.52954262574047,8.79673892988685));
#384981=CARTESIAN_POINT('Ctrl Pts',(2.26800404459052,1.52102245623483,8.79894799272499));
#384982=CARTESIAN_POINT('Origin',(2.27784347049494,1.51833309057123,8.75721825406948));
#384983=CARTESIAN_POINT('Origin',(2.27784347049494,1.51833309057123,9.));
#384984=CARTESIAN_POINT('Origin',(2.27784347049494,1.51833309057123,7.51860402984325));
#384985=CARTESIAN_POINT('Ctrl Pts',(2.27461799196033,1.53898852013197,7.50366195182966));
#384986=CARTESIAN_POINT('Ctrl Pts',(2.27765095495659,1.5410405988764,7.50000065167735));
#384987=CARTESIAN_POINT('Ctrl Pts',(2.27765095495666,1.5410405988763,7.49482233047108));
#384988=CARTESIAN_POINT('Ctrl Pts',(2.27994696402869,1.53379661717627,7.50215800491336));
#384989=CARTESIAN_POINT('Ctrl Pts',(2.28299322537737,1.53314470539553,7.49877273257267));
#384990=CARTESIAN_POINT('Ctrl Pts',(2.28492774039883,1.5302855432837,7.49481816995647));
#384991=CARTESIAN_POINT('Ctrl Pts',(2.27926434158826,1.53106823982957,7.51043025814043));
#384992=CARTESIAN_POINT('Ctrl Pts',(2.28502241637524,1.53010008088881,7.51006209594514));
#384993=CARTESIAN_POINT('Ctrl Pts',(2.28824598651204,1.52526401164453,7.50731281821701));
#384994=CARTESIAN_POINT('Ctrl Pts',(2.27646153184156,1.53075646553773,7.51860402984326));
#384995=CARTESIAN_POINT('Ctrl Pts',(2.28402415878925,1.53159770928416,7.51860402984326));
#384996=CARTESIAN_POINT('Ctrl Pts',(2.28824458223236,1.52526611838206,7.51860402984327));
#384997=CARTESIAN_POINT('Origin',(0.,0.,7.5));
#384998=CARTESIAN_POINT('Origin',(2.28443929758134,1.37777905311492,7.5));
#384999=CARTESIAN_POINT('',(2.28443929758134,1.37777905311492,7.59394543036555));
#385000=CARTESIAN_POINT('',(2.28443929758134,1.37777905311492,8.85049129520029));
#385001=CARTESIAN_POINT('',(2.28443929758134,1.37777905311492,7.5));
#385002=CARTESIAN_POINT('',(2.35585431734962,1.38110557508644,8.78727029226991));
#385003=CARTESIAN_POINT('Ctrl Pts',(2.28443929758134,1.37777905311492,8.85049129520029));
#385004=CARTESIAN_POINT('Ctrl Pts',(2.30827890705323,1.37888950557938,8.82945686509571));
#385005=CARTESIAN_POINT('Ctrl Pts',(2.332083076063,1.37999830722197,8.80838212259896));
#385006=CARTESIAN_POINT('Ctrl Pts',(2.35585431734962,1.38110557508644,8.78727029226991));
#385007=CARTESIAN_POINT('',(2.36986171072476,1.38175804150005,8.75721825406948));
#385008=CARTESIAN_POINT('Origin',(2.32770859547085,1.37979474530318,8.75937679713124));
#385009=CARTESIAN_POINT('',(2.36986171072476,1.38175804150005,7.51860402984325));
#385010=CARTESIAN_POINT('',(2.36986171072476,1.38175804150005,7.5));
#385011=CARTESIAN_POINT('Ctrl Pts',(2.36986171072476,1.38175804150005,7.51860402984325));
#385012=CARTESIAN_POINT('Ctrl Pts',(2.35886108179033,1.38124563060989,7.52834476460825));
#385013=CARTESIAN_POINT('Ctrl Pts',(2.34785331140634,1.38073288706997,7.53807742314407));
#385014=CARTESIAN_POINT('Ctrl Pts',(2.3368381597891,1.38021979971113,7.54780169004674));
#385015=CARTESIAN_POINT('Ctrl Pts',(2.31939075494555,1.37940709706474,7.5632044032688));
#385016=CARTESIAN_POINT('Ctrl Pts',(2.30192480935482,1.37859353078764,7.57858609112103));
#385017=CARTESIAN_POINT('Ctrl Pts',(2.28443929758134,1.37777905311492,7.59394543036555));
#385018=CARTESIAN_POINT('Origin',(2.41658349078373,1.62573897887917,7.5));
#385019=CARTESIAN_POINT('',(2.32121750495508,1.4620017468866,8.75721825406948));
#385020=CARTESIAN_POINT('',(2.31416007290287,1.44988459233549,8.78727029226991));
#385021=CARTESIAN_POINT('Origin',(2.29624567806382,1.41912673461211,8.75658640621071));
#385022=CARTESIAN_POINT('',(2.27817859968916,1.38810672912948,8.85049129520029));
#385023=CARTESIAN_POINT('Ctrl Pts',(2.31416007290287,1.44988459233549,8.78727029226991));
#385024=CARTESIAN_POINT('Ctrl Pts',(2.30218326068065,1.42932118008403,8.80838212259896));
#385025=CARTESIAN_POINT('Ctrl Pts',(2.29018985827904,1.40872928356716,8.82945686509571));
#385026=CARTESIAN_POINT('Ctrl Pts',(2.27817859968916,1.38810672912948,8.85049129520029));
#385027=CARTESIAN_POINT('',(2.27817859968916,1.38810672912948,7.59394543036555));
#385028=CARTESIAN_POINT('',(2.27817859968916,1.38810672912948,7.5));
#385029=CARTESIAN_POINT('',(2.32121750495508,1.4620017468866,7.51860402984325));
#385030=CARTESIAN_POINT('Ctrl Pts',(2.27817859968916,1.38810672912948,7.59394543036555));
#385031=CARTESIAN_POINT('Ctrl Pts',(2.28698843374853,1.40323264462924,7.57858609112103));
#385032=CARTESIAN_POINT('Ctrl Pts',(2.29578840965636,1.41834163432014,7.56320440326857));
#385033=CARTESIAN_POINT('Ctrl Pts',(2.30457904406442,1.43343458525991,7.54780169004651));
#385034=CARTESIAN_POINT('Ctrl Pts',(2.31012887635665,1.44296328849364,7.53807742314383));
#385035=CARTESIAN_POINT('Ctrl Pts',(2.31567498971637,1.4524856065607,7.52834476460825));
#385036=CARTESIAN_POINT('Ctrl Pts',(2.32121750495508,1.4620017468866,7.51860402984325));
#385037=CARTESIAN_POINT('',(2.32121750495508,1.4620017468866,7.5));
#385038=CARTESIAN_POINT('Origin',(2.2841194059329,1.38464660685212,7.5));
#385039=CARTESIAN_POINT('Ctrl Pts',(2.27817859968916,1.38810672912948,8.85049129520029));
#385040=CARTESIAN_POINT('Ctrl Pts',(2.27808113169048,1.38793938287733,8.85097269580138));
#385041=CARTESIAN_POINT('Ctrl Pts',(2.27799216187779,1.38776991462376,8.85143669361005));
#385042=CARTESIAN_POINT('Ctrl Pts',(2.2779083675713,1.3875901145095,8.8519052845931));
#385043=CARTESIAN_POINT('Ctrl Pts',(2.27774447122185,1.38723843688849,8.852821818839));
#385044=CARTESIAN_POINT('Ctrl Pts',(2.27760476931614,1.38685619637749,8.85372622499636));
#385045=CARTESIAN_POINT('Ctrl Pts',(2.27750155151866,1.38643210212429,8.85462257735071));
#385046=CARTESIAN_POINT('Ctrl Pts',(2.27741586376914,1.3860800341377,8.85536669723987));
#385047=CARTESIAN_POINT('Ctrl Pts',(2.27735526963748,1.38569904887468,8.85610498449051));
#385048=CARTESIAN_POINT('Ctrl Pts',(2.27733469853654,1.38528139713442,8.85681338218371));
#385049=CARTESIAN_POINT('Ctrl Pts',(2.27731603023014,1.3849023775242,8.85745625420284));
#385050=CARTESIAN_POINT('Ctrl Pts',(2.27732949131403,1.38448843593453,8.85808743050666));
#385051=CARTESIAN_POINT('Ctrl Pts',(2.27740126538764,1.38402807170153,8.8586680450841));
#385052=CARTESIAN_POINT('Ctrl Pts',(2.27743438038933,1.3838156696239,8.85893592806395));
#385053=CARTESIAN_POINT('Ctrl Pts',(2.27748014042395,1.38359331526745,8.85919241173848));
#385054=CARTESIAN_POINT('Ctrl Pts',(2.27754269428291,1.38335963403902,8.85943017985534));
#385055=CARTESIAN_POINT('Ctrl Pts',(2.27762716051043,1.3830440952036,8.8597512372));
#385056=CARTESIAN_POINT('Ctrl Pts',(2.2777450155586,1.3827000384409,8.86004599534705));
#385057=CARTESIAN_POINT('Ctrl Pts',(2.27790469650042,1.38233497258256,8.86026130871721));
#385058=CARTESIAN_POINT('Ctrl Pts',(2.27796316019511,1.38220131167952,8.86034014101235));
#385059=CARTESIAN_POINT('Ctrl Pts',(2.27802809754115,1.3820628218386,8.86040910639693));
#385060=CARTESIAN_POINT('Ctrl Pts',(2.278098043917,1.38192341894476,8.86046313645507));
#385061=CARTESIAN_POINT('Ctrl Pts',(2.27820719465073,1.38170588189642,8.8605474499083));
#385062=CARTESIAN_POINT('Ctrl Pts',(2.27833165395477,1.38148024927839,8.86059655985668));
#385063=CARTESIAN_POINT('Ctrl Pts',(2.27846318335475,1.38126085010039,8.86059725258816));
#385064=CARTESIAN_POINT('Ctrl Pts',(2.2785950166402,1.38104094402264,8.86059794692011));
#385065=CARTESIAN_POINT('Ctrl Pts',(2.27873769344055,1.38082622749525,8.86056369958366));
#385066=CARTESIAN_POINT('Ctrl Pts',(2.27888029786019,1.38062632859761,8.86048590497774));
#385067=CARTESIAN_POINT('Ctrl Pts',(2.27891751336787,1.38057416093704,8.86046560290182));
#385068=CARTESIAN_POINT('Ctrl Pts',(2.27895528183714,1.38052237637027,8.86044257503091));
#385069=CARTESIAN_POINT('Ctrl Pts',(2.27899240966942,1.38047255574005,8.86041778462583));
#385070=CARTESIAN_POINT('Ctrl Pts',(2.27924223390883,1.38013732472094,8.860250975962));
#385071=CARTESIAN_POINT('Ctrl Pts',(2.27949684175641,1.37984622804255,8.8599848982295));
#385072=CARTESIAN_POINT('Ctrl Pts',(2.27974242457589,1.37960218414178,8.85968173251461));
#385073=CARTESIAN_POINT('Ctrl Pts',(2.27987232381717,1.37947309890031,8.85952137522076));
#385074=CARTESIAN_POINT('Ctrl Pts',(2.28000206733072,1.37935455443873,8.85934740853961));
#385075=CARTESIAN_POINT('Ctrl Pts',(2.2801287768589,1.37924707484728,8.8591675900182));
#385076=CARTESIAN_POINT('Ctrl Pts',(2.28063758147686,1.37881548842082,8.85844552518696));
#385077=CARTESIAN_POINT('Ctrl Pts',(2.28112426400979,1.3785356165466,8.85759444184125));
#385078=CARTESIAN_POINT('Ctrl Pts',(2.28154157522217,1.37834306627386,8.8568349891514));
#385079=CARTESIAN_POINT('Ctrl Pts',(2.28158524572916,1.37832291640062,8.85675551444999));
#385080=CARTESIAN_POINT('Ctrl Pts',(2.28162816120066,1.37830374221057,8.85667699793652));
#385081=CARTESIAN_POINT('Ctrl Pts',(2.28167026988731,1.37828548282268,8.85659965593547));
#385082=CARTESIAN_POINT('Ctrl Pts',(2.28223865508833,1.3780390166732,8.85555568965886));
#385083=CARTESIAN_POINT('Ctrl Pts',(2.28282050306976,1.37788423350347,8.85434650606346));
#385084=CARTESIAN_POINT('Ctrl Pts',(2.28341709248037,1.37781436229031,8.85297329937118));
#385085=CARTESIAN_POINT('Ctrl Pts',(2.28375263767311,1.37777506399023,8.85220095427747));
#385086=CARTESIAN_POINT('Ctrl Pts',(2.28409301987351,1.3777629234491,8.85137579139184));
#385087=CARTESIAN_POINT('Ctrl Pts',(2.28443929758134,1.37777905311492,8.85049129520029));
#385088=CARTESIAN_POINT('Origin',(2.2841194059329,1.38464660685212,7.59394543036555));
#385089=CARTESIAN_POINT('Ctrl Pts',(2.27789561720848,1.38762086650577,7.59443877723642));
#385090=CARTESIAN_POINT('Ctrl Pts',(2.27498116993601,1.38261694896602,7.58783886950016));
#385091=CARTESIAN_POINT('Ctrl Pts',(2.28112970280111,1.3767624869802,7.58559994247159));
#385092=CARTESIAN_POINT('Ctrl Pts',(2.29380549936271,1.41493710554661,7.5667025222214));
#385093=CARTESIAN_POINT('Ctrl Pts',(2.29089526429404,1.40994042008829,7.56004874999031));
#385094=CARTESIAN_POINT('Ctrl Pts',(2.29706549617269,1.40403579513669,7.55786368756704));
#385095=CARTESIAN_POINT('Ctrl Pts',(2.30968567140157,1.44220233424022,7.5388891333356));
#385096=CARTESIAN_POINT('Ctrl Pts',(2.3067581406633,1.43717595323564,7.5322200213728));
#385097=CARTESIAN_POINT('Ctrl Pts',(2.31297108856251,1.43125972782396,7.53005029815327));
#385098=CARTESIAN_POINT('Ctrl Pts',(2.32553541473658,1.4694153188166,7.51101258149734));
#385099=CARTESIAN_POINT('Ctrl Pts',(2.32257239700633,1.46432800894107,7.5043616886572));
#385100=CARTESIAN_POINT('Ctrl Pts',(2.32884576547033,1.45843289828396,7.50217374673251));
#385101=CARTESIAN_POINT('',(2.32799867143117,1.4569829035209,7.50366116523517));
#385102=CARTESIAN_POINT('Ctrl Pts',(2.32121750495508,1.4620017468866,7.51860402984325));
#385103=CARTESIAN_POINT('Ctrl Pts',(2.32143976369038,1.46238335076547,7.51734760759494));
#385104=CARTESIAN_POINT('Ctrl Pts',(2.32169201845767,1.46269824025776,7.51608817408573));
#385105=CARTESIAN_POINT('Ctrl Pts',(2.32198411096283,1.46293734222614,7.5148100591312));
#385106=CARTESIAN_POINT('Ctrl Pts',(2.32224869533378,1.46315392650263,7.51365231206384));
#385107=CARTESIAN_POINT('Ctrl Pts',(2.32254618173406,1.46330882470793,7.51247773061043));
#385108=CARTESIAN_POINT('Ctrl Pts',(2.32288847583597,1.46336660528917,7.51129758471022));
#385109=CARTESIAN_POINT('Ctrl Pts',(2.32331390831319,1.46343841995286,7.50983079813402));
#385110=CARTESIAN_POINT('Ctrl Pts',(2.32379714857049,1.46334507583531,7.50839324291155));
#385111=CARTESIAN_POINT('Ctrl Pts',(2.32432608821462,1.46300494832451,7.50715379678855));
#385112=CARTESIAN_POINT('Ctrl Pts',(2.32457044308917,1.46284781921505,7.50658120839351));
#385113=CARTESIAN_POINT('Ctrl Pts',(2.32485414912167,1.46260769292224,7.50598221009429));
#385114=CARTESIAN_POINT('Ctrl Pts',(2.32515575918815,1.46227292178528,7.50545747549611));
#385115=CARTESIAN_POINT('Ctrl Pts',(2.32531670765533,1.46209427754447,7.50517746087247));
#385116=CARTESIAN_POINT('Ctrl Pts',(2.32548465021346,1.46188688045126,7.50491486231392));
#385117=CARTESIAN_POINT('Ctrl Pts',(2.32565384315538,1.46165517302971,7.50468370960993));
#385118=CARTESIAN_POINT('Ctrl Pts',(2.32590683997244,1.46130869734652,7.50433806340447));
#385119=CARTESIAN_POINT('Ctrl Pts',(2.32616976944411,1.46089714676686,7.50405484070984));
#385120=CARTESIAN_POINT('Ctrl Pts',(2.3264243200522,1.46044785276346,7.50385766036131));
#385121=CARTESIAN_POINT('Ctrl Pts',(2.32645154028312,1.46039980775341,7.50383657498791));
#385122=CARTESIAN_POINT('Ctrl Pts',(2.32647866521304,1.46035135950571,7.50381643264937));
#385123=CARTESIAN_POINT('Ctrl Pts',(2.3265056731432,1.46030256203688,7.50379723213559));
#385124=CARTESIAN_POINT('Ctrl Pts',(2.32668595991194,1.4599768229697,7.50366906242519));
#385125=CARTESIAN_POINT('Ctrl Pts',(2.32686432570829,1.45962808883253,7.50358235568538));
#385126=CARTESIAN_POINT('Ctrl Pts',(2.32702816834755,1.45928781937696,7.5035341175365));
#385127=CARTESIAN_POINT('Ctrl Pts',(2.3272738318417,1.45877762383939,7.50346178989177));
#385128=CARTESIAN_POINT('Ctrl Pts',(2.32751641693376,1.45821832421325,7.50346967198527));
#385129=CARTESIAN_POINT('Ctrl Pts',(2.32773766577598,1.45766193758503,7.50354272648692));
#385130=CARTESIAN_POINT('Ctrl Pts',(2.32782867000437,1.45743308424832,7.50357277531559));
#385131=CARTESIAN_POINT('Ctrl Pts',(2.32791607531214,1.45720508021277,7.50361331098761));
#385132=CARTESIAN_POINT('Ctrl Pts',(2.32799867143237,1.45698290352165,7.50366116523659));
#385133=CARTESIAN_POINT('',(2.28662319996352,1.38616442150718,7.57603338622103));
#385134=CARTESIAN_POINT('Origin',(2.29418152300578,1.39074298486225,7.5848687342763));
#385135=CARTESIAN_POINT('Ctrl Pts',(2.32799867145534,1.4569829035729,7.50366116529969));
#385136=CARTESIAN_POINT('Ctrl Pts',(2.31423007474033,1.43341484163944,7.5278357307971));
#385137=CARTESIAN_POINT('Ctrl Pts',(2.30043891757453,1.40980978649596,7.55196141284068));
#385138=CARTESIAN_POINT('Ctrl Pts',(2.28662320026408,1.38616442272263,7.57603338728831));
#385139=CARTESIAN_POINT('Ctrl Pts',(2.27884811390189,1.38890690800898,7.59639677331371));
#385140=CARTESIAN_POINT('Ctrl Pts',(2.26672396437058,1.37410138795021,7.59974925422225));
#385141=CARTESIAN_POINT('Ctrl Pts',(2.28545841158006,1.37800253058071,7.59639677331372));
#385142=CARTESIAN_POINT('Ctrl Pts',(2.2759238256025,1.38632550489715,7.58707626057422));
#385143=CARTESIAN_POINT('Ctrl Pts',(2.27553575658722,1.37944314817572,7.58811717123965));
#385144=CARTESIAN_POINT('Ctrl Pts',(2.28181714606147,1.37660385638466,7.58707626057424));
#385145=CARTESIAN_POINT('Ctrl Pts',(2.28198336987503,1.38586992233497,7.58015376756929));
#385146=CARTESIAN_POINT('Ctrl Pts',(2.28144597464152,1.38302595709235,7.5820876076604));
#385147=CARTESIAN_POINT('Ctrl Pts',(2.28421599812537,1.38218696851293,7.5801537675693));
#385148=CARTESIAN_POINT('Ctrl Pts',(2.28662319925573,1.38616442107835,7.57603338509286));
#385149=CARTESIAN_POINT('Ctrl Pts',(2.28662319925573,1.38616442107835,7.57603338509286));
#385150=CARTESIAN_POINT('Ctrl Pts',(2.28662319925573,1.38616442107835,7.57603338509286));
#385151=CARTESIAN_POINT('Origin',(2.29417856487513,1.3907478646081,7.58486873427623));
#385152=CARTESIAN_POINT('Ctrl Pts',(2.37845886339418,1.38215849811745,7.51098857897448));
#385153=CARTESIAN_POINT('Ctrl Pts',(2.37257792201276,1.38188456301553,7.50433767179956));
#385154=CARTESIAN_POINT('Ctrl Pts',(2.37025300047281,1.39017327768763,7.50214974420965));
#385155=CARTESIAN_POINT('Ctrl Pts',(2.34699168879536,1.38069275256386,7.53887321589168));
#385156=CARTESIAN_POINT('Ctrl Pts',(2.34118121152847,1.38042209969057,7.53220407452061));
#385157=CARTESIAN_POINT('Ctrl Pts',(2.33880959854635,1.38866699943437,7.53003438070912));
#385158=CARTESIAN_POINT('Ctrl Pts',(2.31546408561356,1.37922419223812,7.56669465659234));
#385159=CARTESIAN_POINT('Ctrl Pts',(2.30968794718703,1.37895513887304,7.56004085833298));
#385160=CARTESIAN_POINT('Ctrl Pts',(2.30730685731678,1.38715678877751,7.55785582193789));
#385161=CARTESIAN_POINT('Ctrl Pts',(2.28387747971605,1.37775288355733,7.59443891967696));
#385162=CARTESIAN_POINT('Ctrl Pts',(2.27809296660797,1.37748344009836,7.58783901202978));
#385163=CARTESIAN_POINT('Ctrl Pts',(2.27574633651477,1.38564263768109,7.58560008491213));
#385164=CARTESIAN_POINT('',(2.36854855682562,1.39009162622351,7.50366116523517));
#385165=CARTESIAN_POINT('Ctrl Pts',(2.36854855682595,1.3900916262237,7.50366116523554));
#385166=CARTESIAN_POINT('Ctrl Pts',(2.36905599173953,1.3895289119754,7.50350835821027));
#385167=CARTESIAN_POINT('Ctrl Pts',(2.36950414026276,1.38899513214038,7.50345484956));
#385168=CARTESIAN_POINT('Ctrl Pts',(2.36990678611857,1.38847480313371,7.50349758195598));
#385169=CARTESIAN_POINT('Ctrl Pts',(2.3701133733036,1.38820783576469,7.50351950684424));
#385170=CARTESIAN_POINT('Ctrl Pts',(2.37032844657166,1.38791817510165,7.50357029184312));
#385171=CARTESIAN_POINT('Ctrl Pts',(2.37052816139873,1.38763315784124,7.50365515313923));
#385172=CARTESIAN_POINT('Ctrl Pts',(2.37083540367528,1.38719468587983,7.50378570417639));
#385173=CARTESIAN_POINT('Ctrl Pts',(2.37111560035779,1.38675453170472,7.50400001621911));
#385174=CARTESIAN_POINT('Ctrl Pts',(2.37134550914225,1.38634497820498,7.50428903009634));
#385175=CARTESIAN_POINT('Ctrl Pts',(2.37137102724851,1.38629952091742,7.50432110841318));
#385176=CARTESIAN_POINT('Ctrl Pts',(2.37139595306619,1.38625442726895,7.50435406373354));
#385177=CARTESIAN_POINT('Ctrl Pts',(2.37142027477435,1.38620973128228,7.50438785222352));
#385178=CARTESIAN_POINT('Ctrl Pts',(2.37156877049318,1.38593684080007,7.50459414719561));
#385179=CARTESIAN_POINT('Ctrl Pts',(2.37169665806774,1.38567418270537,7.50483629897752));
#385180=CARTESIAN_POINT('Ctrl Pts',(2.37180022139303,1.38543239546432,7.5050991045531));
#385181=CARTESIAN_POINT('Ctrl Pts',(2.37202869249057,1.38489898852534,7.50567888004914));
#385182=CARTESIAN_POINT('Ctrl Pts',(2.37214826172947,1.38444634307581,7.50637912803144));
#385183=CARTESIAN_POINT('Ctrl Pts',(2.37218983841972,1.38407427769359,7.50710440483569));
#385184=CARTESIAN_POINT('Ctrl Pts',(2.37220003384958,1.38398303987534,7.50728225710685));
#385185=CARTESIAN_POINT('Ctrl Pts',(2.3722058873771,1.38389484750112,7.50746498566954));
#385186=CARTESIAN_POINT('Ctrl Pts',(2.37220767804061,1.38381178685591,7.50764697238949));
#385187=CARTESIAN_POINT('Ctrl Pts',(2.37221730415485,1.38336527568616,7.50862528291181));
#385188=CARTESIAN_POINT('Ctrl Pts',(2.37211453181639,1.3830266193461,7.50965856837421));
#385189=CARTESIAN_POINT('Ctrl Pts',(2.37195529513962,1.38276022611353,7.51067959873201));
#385190=CARTESIAN_POINT('Ctrl Pts',(2.37186766699554,1.38261362958163,7.51124147302578));
#385191=CARTESIAN_POINT('Ctrl Pts',(2.37176254541607,1.38248910370112,7.51180065547252));
#385192=CARTESIAN_POINT('Ctrl Pts',(2.37164697289434,1.3823821948436,7.51235175716501));
#385193=CARTESIAN_POINT('Ctrl Pts',(2.37124762379312,1.38201278215343,7.51425603304536));
#385194=CARTESIAN_POINT('Ctrl Pts',(2.37067175971286,1.38181411915051,7.5162690050518));
#385195=CARTESIAN_POINT('Ctrl Pts',(2.3699757857498,1.38176473183863,7.51827788969243));
#385196=CARTESIAN_POINT('Ctrl Pts',(2.36993811832371,1.38176205890398,7.51838661432545));
#385197=CARTESIAN_POINT('Ctrl Pts',(2.36990009115339,1.38175982926598,7.51849533314856));
#385198=CARTESIAN_POINT('Ctrl Pts',(2.36986171072477,1.38175804150005,7.51860402984325));
#385199=CARTESIAN_POINT('Ctrl Pts',(2.2866232011813,1.38616442121187,7.57603338728985));
#385200=CARTESIAN_POINT('Ctrl Pts',(2.31397746257105,1.38747654046485,7.55196141284922));
#385201=CARTESIAN_POINT('Ctrl Pts',(2.34128462636657,1.38878552899631,7.52783573083105));
#385202=CARTESIAN_POINT('Ctrl Pts',(2.36854855688475,1.3900916262209,7.50366116530176));
#385203=CARTESIAN_POINT('Origin',(7.90134016134189E-16,4.78983883923441E-16,
7.49482233047033));
#385204=CARTESIAN_POINT('Origin',(2.32050622536841,1.45229374026967,7.49482233047033));
#385205=CARTESIAN_POINT('Origin',(0.,0.,7.50366116523517));
#385206=CARTESIAN_POINT('Origin',(2.36092560474802,1.38561774629412,7.49482233047033));
#385207=CARTESIAN_POINT('Ctrl Pts',(2.32121697257583,1.46200083291477,7.51860402984325));
#385208=CARTESIAN_POINT('Ctrl Pts',(2.32504704676294,1.46857554338378,7.51860402984325));
#385209=CARTESIAN_POINT('Ctrl Pts',(2.32096588398457,1.47499741199086,7.51860402984325));
#385210=CARTESIAN_POINT('Ctrl Pts',(2.32263910416129,1.46444206841972,7.51041458714366));
#385211=CARTESIAN_POINT('Ctrl Pts',(2.32408016420081,1.47009695230205,7.51004642900443));
#385212=CARTESIAN_POINT('Ctrl Pts',(2.32096475844833,1.47499918306597,7.5072913648301));
#385213=CARTESIAN_POINT('Ctrl Pts',(2.3254108850726,1.46395118372964,7.50215815450137));
#385214=CARTESIAN_POINT('Ctrl Pts',(2.32604895207089,1.46699928723627,7.49877163671528));
#385215=CARTESIAN_POINT('Ctrl Pts',(2.32421856835796,1.46992394432006,7.4948158853317));
#385216=CARTESIAN_POINT('Ctrl Pts',(2.32799820477188,1.45698261146063,7.50366171572174));
#385217=CARTESIAN_POINT('Ctrl Pts',(2.33110214420591,1.45892521853541,7.50000045605858));
#385218=CARTESIAN_POINT('Ctrl Pts',(2.33110214420585,1.45892521853552,7.49482233047317));
#385219=CARTESIAN_POINT('Origin',(2.31041603905737,1.46829287829999,7.51860402984325));
#385220=CARTESIAN_POINT('Origin',(2.31041603905737,1.46829287829999,9.));
#385221=CARTESIAN_POINT('Origin',(2.31041603905737,1.46829287829999,8.75721825406948));
#385222=CARTESIAN_POINT('Ctrl Pts',(2.31281244619726,1.44757086443546,8.78942910404912));
#385223=CARTESIAN_POINT('Ctrl Pts',(2.31563446187851,1.45237593011623,8.79672699501691));
#385224=CARTESIAN_POINT('Ctrl Pts',(2.30889868938921,1.45823279403427,8.79893251111267));
#385225=CARTESIAN_POINT('Ctrl Pts',(2.31834579499506,1.45707125757588,8.78111911759583));
#385226=CARTESIAN_POINT('Ctrl Pts',(2.32168490856531,1.46277148833352,8.78644465894813));
#385227=CARTESIAN_POINT('Ctrl Pts',(2.31685066608332,1.46927883890044,8.78817647674132));
#385228=CARTESIAN_POINT('Ctrl Pts',(2.32179430992118,1.46299212920275,8.7678092393203));
#385229=CARTESIAN_POINT('Ctrl Pts',(2.32573159556495,1.46972358658803,8.76988516158374));
#385230=CARTESIAN_POINT('Ctrl Pts',(2.3218082667469,1.47618453631557,8.77093053738833));
#385231=CARTESIAN_POINT('Ctrl Pts',(2.32112189670533,1.46183764026921,8.75371302330492));
#385232=CARTESIAN_POINT('Ctrl Pts',(2.32496320702647,1.46840350170427,8.75300828287559));
#385233=CARTESIAN_POINT('Ctrl Pts',(2.32084096157934,1.47483791168561,8.75267964240738));
#385234=CARTESIAN_POINT('Origin',(2.30335860700516,1.45617572374888,8.78727029226991));
#385235=CARTESIAN_POINT('Ctrl Pts',(2.27817859968916,1.38810672912948,8.85049129520029));
#385236=CARTESIAN_POINT('Ctrl Pts',(2.28111762290109,1.39315284196837,8.85711686593484));
#385237=CARTESIAN_POINT('Ctrl Pts',(2.27490615106173,1.39902807640649,8.85933012996512));
#385238=CARTESIAN_POINT('Ctrl Pts',(2.29018987439859,1.40872931124339,8.82945683644723));
#385239=CARTESIAN_POINT('Ctrl Pts',(2.29315329328014,1.41381730986979,8.83607469902389));
#385240=CARTESIAN_POINT('Ctrl Pts',(2.28689781417967,1.4196825484601,8.8382956714852));
#385241=CARTESIAN_POINT('Ctrl Pts',(2.30218324533449,1.42932115373567,8.80838214965002));
#385242=CARTESIAN_POINT('Ctrl Pts',(2.30515835925054,1.43442923198018,8.81501364461988));
#385243=CARTESIAN_POINT('Ctrl Pts',(2.29887186472475,1.44030535307938,8.81722098428721));
#385244=CARTESIAN_POINT('Ctrl Pts',(2.31416007290287,1.44988459233549,8.78727029226991));
#385245=CARTESIAN_POINT('Ctrl Pts',(2.31713568099512,1.45499351904858,8.79393457792714));
#385246=CARTESIAN_POINT('Ctrl Pts',(2.31082965924419,1.46089889836366,8.79610912703474));
#385247=CARTESIAN_POINT('Origin',(2.26737713379144,1.39439786054287,8.85049129520029));
#385248=CARTESIAN_POINT('Ctrl Pts',(2.28443929758134,1.37777905311492,8.85049129520029));
#385249=CARTESIAN_POINT('Ctrl Pts',(2.29027258849561,1.37805076865117,8.85711686593484));
#385250=CARTESIAN_POINT('Ctrl Pts',(2.29260852370876,1.36982616113508,8.85933012996512));
#385251=CARTESIAN_POINT('Ctrl Pts',(2.27927866931394,1.37753867030226,8.86332496987232));
#385252=CARTESIAN_POINT('Ctrl Pts',(2.28191097731257,1.3737409276863,8.86648636486737));
#385253=CARTESIAN_POINT('Ctrl Pts',(2.27817065852941,1.36917079450518,8.87206031107458));
#385254=CARTESIAN_POINT('Ctrl Pts',(2.27556081970207,1.38361217013839,8.86341338519876));
#385255=CARTESIAN_POINT('Ctrl Pts',(2.27337901193666,1.3877003464444,8.86654584966059));
#385256=CARTESIAN_POINT('Ctrl Pts',(2.26758895886382,1.38643565747033,8.87215952290713));
#385257=CARTESIAN_POINT('Ctrl Pts',(2.27817859968916,1.38810672912948,8.85049129520029));
#385258=CARTESIAN_POINT('Ctrl Pts',(2.28111762290109,1.39315284196837,8.85711686593484));
#385259=CARTESIAN_POINT('Ctrl Pts',(2.27490615106173,1.39902807640649,8.85933012996512));
#385260=CARTESIAN_POINT('Origin',(2.28502091876033,1.36529259177457,8.85049129520029));
#385261=CARTESIAN_POINT('Ctrl Pts',(2.35585431734962,1.38110557508644,8.78727029226991));
#385262=CARTESIAN_POINT('Ctrl Pts',(2.36176022090917,1.38138067293023,8.79393457792714));
#385263=CARTESIAN_POINT('Ctrl Pts',(2.36407914959489,1.37305829436826,8.79610912703474));
#385264=CARTESIAN_POINT('Ctrl Pts',(2.33208304560438,1.3799983058032,8.80838214965002));
#385265=CARTESIAN_POINT('Ctrl Pts',(2.33798796833692,1.38027335795994,8.81501364461995));
#385266=CARTESIAN_POINT('Ctrl Pts',(2.340289988798,1.37198182526738,8.81722098428721));
#385267=CARTESIAN_POINT('Ctrl Pts',(2.30827893904692,1.37888950706965,8.82945683644729));
#385268=CARTESIAN_POINT('Ctrl Pts',(2.31416064980264,1.37916347800914,8.83607469902394));
#385269=CARTESIAN_POINT('Ctrl Pts',(2.31646736766072,1.37090447714819,8.8382956714852));
#385270=CARTESIAN_POINT('Ctrl Pts',(2.28443929758134,1.37777905311492,8.85049129520029));
#385271=CARTESIAN_POINT('Ctrl Pts',(2.29027258849561,1.37805076865117,8.85711686593484));
#385272=CARTESIAN_POINT('Ctrl Pts',(2.29260852370876,1.36982616113508,8.85933012996512));
#385273=CARTESIAN_POINT('Origin',(2.35643593852861,1.36861911374609,8.78727029226991));
#385274=CARTESIAN_POINT('Ctrl Pts',(2.36967675099987,1.38174940758219,8.75374538247849));
#385275=CARTESIAN_POINT('Ctrl Pts',(2.37726687089215,1.38211609329003,8.75304829418603));
#385276=CARTESIAN_POINT('Ctrl Pts',(2.38106579034591,1.37549500167362,8.75272238421917));
#385277=CARTESIAN_POINT('Ctrl Pts',(2.37099530499473,1.38181082644541,8.76769408445016));
#385278=CARTESIAN_POINT('Ctrl Pts',(2.37877645928179,1.38218605028951,8.76974318093965));
#385279=CARTESIAN_POINT('Ctrl Pts',(2.38268881118068,1.3757275783418,8.7707786988043));
#385280=CARTESIAN_POINT('Ctrl Pts',(2.3642371483471,1.38149602835534,8.78108014887993));
#385281=CARTESIAN_POINT('Ctrl Pts',(2.37083121329715,1.38181781203247,8.78639403366329));
#385282=CARTESIAN_POINT('Ctrl Pts',(2.37437720405471,1.37454127265745,8.78812224174741));
#385283=CARTESIAN_POINT('Ctrl Pts',(2.35316202148166,1.380980143743,8.78944554828684));
#385284=CARTESIAN_POINT('Ctrl Pts',(2.35871898210047,1.38125692217054,8.79673892988684));
#385285=CARTESIAN_POINT('Ctrl Pts',(2.36079643040481,1.37258583441529,8.79894799272499));
#385286=CARTESIAN_POINT('Origin',(2.37044333190375,1.3692715801597,8.75721825406948));
#385287=CARTESIAN_POINT('Origin',(2.37044333190375,1.3692715801597,9.));
#385288=CARTESIAN_POINT('Origin',(2.37044333190375,1.3692715801597,7.51860402984325));
#385289=CARTESIAN_POINT('Ctrl Pts',(2.36854787837648,1.39009122804437,7.50366195182966));
#385290=CARTESIAN_POINT('Ctrl Pts',(2.37170608696156,1.39194476796657,7.50000065167735));
#385291=CARTESIAN_POINT('Ctrl Pts',(2.37170608696162,1.39194476796647,7.49482233047108));
#385292=CARTESIAN_POINT('Ctrl Pts',(2.37353325513569,1.38456856399743,7.50215800491337));
#385293=CARTESIAN_POINT('Ctrl Pts',(2.37653148948252,1.38372281700464,7.49877273257267));
#385294=CARTESIAN_POINT('Ctrl Pts',(2.37827884268993,1.38074558454504,7.49481816995647));
#385295=CARTESIAN_POINT('Ctrl Pts',(2.37267722747951,1.38188952816453,7.51043025814041));
#385296=CARTESIAN_POINT('Ctrl Pts',(2.37836144152797,1.38055443729187,7.51006209594513));
#385297=CARTESIAN_POINT('Ctrl Pts',(2.38126854047387,1.37552176942275,7.507312818217));
#385298=CARTESIAN_POINT('Ctrl Pts',(2.36986020095857,1.38175797108345,7.51860402984325));
#385299=CARTESIAN_POINT('Ctrl Pts',(2.37746118834999,1.3821129472322,7.51860402984324));
#385300=CARTESIAN_POINT('Ctrl Pts',(2.38126727405857,1.37552396180426,7.51860402984325));
#385301=CARTESIAN_POINT('Origin',(0.,0.,7.5));
#385302=CARTESIAN_POINT('Origin',(2.36802027905701,1.22858372995534,7.5));
#385303=CARTESIAN_POINT('',(2.36802027905701,1.22858372995534,7.59394543036555));
#385304=CARTESIAN_POINT('',(2.36802027905701,1.22858372995534,8.85049129520029));
#385305=CARTESIAN_POINT('',(2.36802027905701,1.22858372995534,7.5));
#385306=CARTESIAN_POINT('',(2.43950170000241,1.22732784120422,8.78727029226991));
#385307=CARTESIAN_POINT('Ctrl Pts',(2.36802027905701,1.22858372995534,8.85049129520029));
#385308=CARTESIAN_POINT('Ctrl Pts',(2.39188205442812,1.22816449185299,8.82945686509571));
#385309=CARTESIAN_POINT('Ctrl Pts',(2.41570835638483,1.22774587699877,8.80838212259895));
#385310=CARTESIAN_POINT('Ctrl Pts',(2.43950170000242,1.22732784120422,8.78727029226991));
#385311=CARTESIAN_POINT('',(2.45352211735224,1.2270815102807,8.75721825406948));
#385312=CARTESIAN_POINT('Origin',(2.41132982137661,1.2278230072536,8.75937679713168));
#385313=CARTESIAN_POINT('',(2.45352211735224,1.2270815102807,7.51860402984325));
#385314=CARTESIAN_POINT('',(2.45352211735224,1.2270815102807,7.5));
#385315=CARTESIAN_POINT('Ctrl Pts',(2.45352211735224,1.2270815102807,7.51860402984325));
#385316=CARTESIAN_POINT('Ctrl Pts',(2.44251126011131,1.22727496490942,7.52834476460825));
#385317=CARTESIAN_POINT('Ctrl Pts',(2.43149325478075,1.2274685451261,7.53807742314407));
#385318=CARTESIAN_POINT('Ctrl Pts',(2.42046786135393,1.2276622551475,7.54780169004674));
#385319=CARTESIAN_POINT('Ctrl Pts',(2.40300423403753,1.22796908135228,7.5632044032688));
#385320=CARTESIAN_POINT('Ctrl Pts',(2.38552204873489,1.22827623361052,7.57858609112103));
#385321=CARTESIAN_POINT('Ctrl Pts',(2.36802027905701,1.22858372995534,7.59394543036555));
#385322=CARTESIAN_POINT('Origin',(2.51577981483215,1.46756768793083,7.5));
#385323=CARTESIAN_POINT('',(2.41011908817656,1.31027699133287,8.75721825406948));
#385324=CARTESIAN_POINT('',(2.40229980761778,1.29863690399944,8.78727029226991));
#385325=CARTESIAN_POINT('Origin',(2.38245155711292,1.26909002081042,8.75658640621015));
#385326=CARTESIAN_POINT('',(2.36243414091424,1.23929131094307,8.85049129520029));
#385327=CARTESIAN_POINT('Ctrl Pts',(2.40229980761778,1.29863690399944,8.78727029226991));
#385328=CARTESIAN_POINT('Ctrl Pts',(2.38903010069427,1.27888309847761,8.80838212259896));
#385329=CARTESIAN_POINT('Ctrl Pts',(2.37574201268453,1.2591019301508,8.82945686509571));
#385330=CARTESIAN_POINT('Ctrl Pts',(2.36243414091424,1.23929131094307,8.85049129520029));
#385331=CARTESIAN_POINT('',(2.36243414091424,1.23929131094307,7.59394543036555));
#385332=CARTESIAN_POINT('',(2.36243414091424,1.23929131094307,7.5));
#385333=CARTESIAN_POINT('',(2.41011908817656,1.31027699133287,7.51860402984325));
#385334=CARTESIAN_POINT('Ctrl Pts',(2.36243414091424,1.23929131094307,7.59394543036555));
#385335=CARTESIAN_POINT('Ctrl Pts',(2.37219499495816,1.25382170062101,7.57858609112103));
#385336=CARTESIAN_POINT('Ctrl Pts',(2.38194492666489,1.26833583087991,7.56320440326857));
#385337=CARTESIAN_POINT('Ctrl Pts',(2.39168450845862,1.28283455385297,7.54780169004651));
#385338=CARTESIAN_POINT('Ctrl Pts',(2.39783344413751,1.29198810036814,7.53807742314383));
#385339=CARTESIAN_POINT('Ctrl Pts',(2.4039782594258,1.30113551310847,7.52834476460825));
#385340=CARTESIAN_POINT('Ctrl Pts',(2.41011908817656,1.31027699133287,7.51860402984325));
#385341=CARTESIAN_POINT('',(2.41011908817656,1.31027699133287,7.5));
#385342=CARTESIAN_POINT('Origin',(2.36814105033893,1.23545766909512,7.5));
#385343=CARTESIAN_POINT('Ctrl Pts',(2.36243414091424,1.23929131094307,8.85049129520029));
#385344=CARTESIAN_POINT('Ctrl Pts',(2.36232615126283,1.23913055331786,8.85097269580138));
#385345=CARTESIAN_POINT('Ctrl Pts',(2.36222650637988,1.23896713357046,8.85143669361005));
#385346=CARTESIAN_POINT('Ctrl Pts',(2.36213136440491,1.23879307159446,8.8519052845931));
#385347=CARTESIAN_POINT('Ctrl Pts',(2.36194527273555,1.23845261740801,8.85282181883899));
#385348=CARTESIAN_POINT('Ctrl Pts',(2.36178136762875,1.23808011298297,8.85372622499636));
#385349=CARTESIAN_POINT('Ctrl Pts',(2.36165119009121,1.23766350326389,8.85462257735071));
#385350=CARTESIAN_POINT('Ctrl Pts',(2.36154312132302,1.23731764867169,8.85536669723986));
#385351=CARTESIAN_POINT('Ctrl Pts',(2.36145824187889,1.2369413284631,8.85610498449051));
#385352=CARTESIAN_POINT('Ctrl Pts',(2.36141095400461,1.23652585282809,8.85681338218371));
#385353=CARTESIAN_POINT('Ctrl Pts',(2.36136804018444,1.23614880803681,8.85745625420284));
#385354=CARTESIAN_POINT('Ctrl Pts',(2.36135495228238,1.23573485447993,8.85808743050665));
#385355=CARTESIAN_POINT('Ctrl Pts',(2.36139708325078,1.23527083753394,8.8586680450841));
#385356=CARTESIAN_POINT('Ctrl Pts',(2.36141652156631,1.23505675017371,8.85893592806395));
#385357=CARTESIAN_POINT('Ctrl Pts',(2.3614479412895,1.23483192081265,8.85919241173848));
#385358=CARTESIAN_POINT('Ctrl Pts',(2.36149539461713,1.23459471186786,8.85943017985534));
#385359=CARTESIAN_POINT('Ctrl Pts',(2.36155947065713,1.23427440957104,8.8597512372));
#385360=CARTESIAN_POINT('Ctrl Pts',(2.361655039767,1.233923508711,8.86004599534706));
#385361=CARTESIAN_POINT('Ctrl Pts',(2.36179100277735,1.23354896212654,8.86026130871721));
#385362=CARTESIAN_POINT('Ctrl Pts',(2.36184078266864,1.23341183006239,8.86034014101235));
#385363=CARTESIAN_POINT('Ctrl Pts',(2.36189671351936,1.23326946421365,8.86040910639692));
#385364=CARTESIAN_POINT('Ctrl Pts',(2.36195758460882,1.23312586625832,8.86046313645506));
#385365=CARTESIAN_POINT('Ctrl Pts',(2.36205257343412,1.23290178285166,8.86054744990829));
#385366=CARTESIAN_POINT('Ctrl Pts',(2.36216232069169,1.23266863968505,8.86059655985668));
#385367=CARTESIAN_POINT('Ctrl Pts',(2.36227952289682,1.2324412641686,8.86059725258816));
#385368=CARTESIAN_POINT('Ctrl Pts',(2.36239699588587,1.23221336332387,8.86059794692011));
#385369=CARTESIAN_POINT('Ctrl Pts',(2.36252562260629,1.23198994662063,8.86056369958366));
#385370=CARTESIAN_POINT('Ctrl Pts',(2.3626551264635,1.23178132174018,8.86048590497774));
#385371=CARTESIAN_POINT('Ctrl Pts',(2.36268892311444,1.2317268768579,8.86046560290182));
#385372=CARTESIAN_POINT('Ctrl Pts',(2.36272329613576,1.23167277885394,8.86044257503091));
#385373=CARTESIAN_POINT('Ctrl Pts',(2.36275715566618,1.23162068179717,8.86041778462583));
#385374=CARTESIAN_POINT('Ctrl Pts',(2.36298498828977,1.23127013325217,8.86025097596201));
#385375=CARTESIAN_POINT('Ctrl Pts',(2.36322042238999,1.23096332188232,8.8599848982295));
#385376=CARTESIAN_POINT('Ctrl Pts',(2.36344986468682,1.23070404485065,8.85968173251461));
#385377=CARTESIAN_POINT('Ctrl Pts',(2.36357122651637,1.23056690215569,8.85952137522076));
#385378=CARTESIAN_POINT('Ctrl Pts',(2.36369310828822,1.23044028856096,8.85934740853961));
#385379=CARTESIAN_POINT('Ctrl Pts',(2.36381267123702,1.23032491149051,8.8591675900182));
#385380=CARTESIAN_POINT('Ctrl Pts',(2.36429277862403,1.22986161258086,8.85844552518697));
#385381=CARTESIAN_POINT('Ctrl Pts',(2.36476052976295,1.22955113387649,8.85759444184128));
#385382=CARTESIAN_POINT('Ctrl Pts',(2.36516464682635,1.22933224199776,8.85683498915144));
#385383=CARTESIAN_POINT('Ctrl Pts',(2.36520693660079,1.2293093355456,8.85675551445001));
#385384=CARTESIAN_POINT('Ctrl Pts',(2.36524853540329,1.22928745114727,8.85667699793653));
#385385=CARTESIAN_POINT('Ctrl Pts',(2.36528938769013,1.22926653136243,8.85659965593547));
#385386=CARTESIAN_POINT('Ctrl Pts',(2.36584081394238,1.22898415503923,8.85555568965886));
#385387=CARTESIAN_POINT('Ctrl Pts',(2.36641154946299,1.22879241075995,8.85434650606346));
#385388=CARTESIAN_POINT('Ctrl Pts',(2.36700243645268,1.22868445948992,8.85297329937117));
#385389=CARTESIAN_POINT('Ctrl Pts',(2.3673347743811,1.2286237434781,8.85220095427747));
#385390=CARTESIAN_POINT('Ctrl Pts',(2.36767367938263,1.22858981951856,8.85137579139183));
#385391=CARTESIAN_POINT('Ctrl Pts',(2.36802027905701,1.22858372995534,8.85049129520029));
#385392=CARTESIAN_POINT('Origin',(2.36814105033893,1.23545766909512,7.59394543036555));
#385393=CARTESIAN_POINT('Ctrl Pts',(2.36212061052624,1.23882457732601,7.59443877723642));
#385394=CARTESIAN_POINT('Ctrl Pts',(2.35889154920072,1.23401767014939,7.58783886950016));
#385395=CARTESIAN_POINT('Ctrl Pts',(2.36465235257833,1.22778129893038,7.58559994247159));
#385396=CARTESIAN_POINT('Ctrl Pts',(2.37974796156564,1.26506534257459,7.56670252222138));
#385397=CARTESIAN_POINT('Ctrl Pts',(2.37652356715048,1.26026538274351,7.56004874999027));
#385398=CARTESIAN_POINT('Ctrl Pts',(2.38230281100646,1.25397756136337,7.55786368756705));
#385399=CARTESIAN_POINT('Ctrl Pts',(2.39734239528812,1.29125710581579,7.53888913333557));
#385400=CARTESIAN_POINT('Ctrl Pts',(2.3940988381391,1.28642861958841,7.53222002137274));
#385401=CARTESIAN_POINT('Ctrl Pts',(2.39991996700693,1.28012648475776,7.53005029815326));
#385402=CARTESIAN_POINT('Ctrl Pts',(2.41490311553372,1.31739868185468,7.51101258149734));
#385403=CARTESIAN_POINT('Ctrl Pts',(2.41162024057834,1.31251166560068,7.5043616886572));
#385404=CARTESIAN_POINT('Ctrl Pts',(2.41750301869741,1.30622673098317,7.50217374673251));
#385405=CARTESIAN_POINT('',(2.41656476362036,1.30483398889129,7.50366116523517));
#385406=CARTESIAN_POINT('Ctrl Pts',(2.41011908817656,1.31027699133287,7.51860402984325));
#385407=CARTESIAN_POINT('Ctrl Pts',(2.41036533970192,1.31064357099958,7.51734760759493));
#385408=CARTESIAN_POINT('Ctrl Pts',(2.41063725122378,1.31094165149921,7.51608817408572));
#385409=CARTESIAN_POINT('Ctrl Pts',(2.41094406290927,1.31116154777589,7.51481005913119));
#385410=CARTESIAN_POINT('Ctrl Pts',(2.41122198026549,1.31136073507791,7.51365231206383));
#385411=CARTESIAN_POINT('Ctrl Pts',(2.41152877981015,1.31149625500912,7.51247773061042));
#385412=CARTESIAN_POINT('Ctrl Pts',(2.41187407264667,1.31153198601555,7.51129758471022));
#385413=CARTESIAN_POINT('Ctrl Pts',(2.41230323220853,1.31157639557592,7.50983079813402));
#385414=CARTESIAN_POINT('Ctrl Pts',(2.41277949901876,1.31145228193427,7.50839324291155));
#385415=CARTESIAN_POINT('Ctrl Pts',(2.41328555985521,1.31107896397256,7.50715379678855));
#385416=CARTESIAN_POINT('Ctrl Pts',(2.41351934537986,1.31090650183115,7.50658120839351));
#385417=CARTESIAN_POINT('Ctrl Pts',(2.41378708356348,1.31064869179565,7.50598221009429));
#385418=CARTESIAN_POINT('Ctrl Pts',(2.41406662507935,1.31029528425859,7.50545747549612));
#385419=CARTESIAN_POINT('Ctrl Pts',(2.41421579708483,1.31010669505783,7.50517746087247));
#385420=CARTESIAN_POINT('Ctrl Pts',(2.41437010660958,1.30988896396755,7.50491486231392));
#385421=CARTESIAN_POINT('Ctrl Pts',(2.41452410638098,1.30964689238474,7.50468370960993));
#385422=CARTESIAN_POINT('Ctrl Pts',(2.41475438461571,1.30928491901128,7.50433806340446));
#385423=CARTESIAN_POINT('Ctrl Pts',(2.41499040573442,1.30885736805732,7.50405484070983));
#385424=CARTESIAN_POINT('Ctrl Pts',(2.41521564697535,1.30839268806317,7.5038576603613));
#385425=CARTESIAN_POINT('Ctrl Pts',(2.41523973302502,1.30834299776057,7.50383657498791));
#385426=CARTESIAN_POINT('Ctrl Pts',(2.41526369813397,1.30829291115477,7.50381643264937));
#385427=CARTESIAN_POINT('Ctrl Pts',(2.41528752410888,1.30824248354156,7.50379723213559));
#385428=CARTESIAN_POINT('Ctrl Pts',(2.41544657028543,1.30790586272729,7.50366906242519));
#385429=CARTESIAN_POINT('Ctrl Pts',(2.41560222613724,1.307546417166,7.50358235568538));
#385430=CARTESIAN_POINT('Ctrl Pts',(2.41574393100535,1.30719634939658,7.5035341175365));
#385431=CARTESIAN_POINT('Ctrl Pts',(2.41595640141718,1.30667146239635,7.50346178989176));
#385432=CARTESIAN_POINT('Ctrl Pts',(2.41616265364206,1.30609776943107,7.50346967198527));
#385433=CARTESIAN_POINT('Ctrl Pts',(2.41634780009115,1.30552835049685,7.50354272648692));
#385434=CARTESIAN_POINT('Ctrl Pts',(2.41642395465796,1.30529413670293,7.50357277531559));
#385435=CARTESIAN_POINT('Ctrl Pts',(2.41649657211344,1.30506100104883,7.50361331098761));
#385436=CARTESIAN_POINT('Ctrl Pts',(2.41656476362161,1.30483398889196,7.50366116523658));
#385437=CARTESIAN_POINT('',(2.37073694677503,1.23681194660286,7.57603338622103));
#385438=CARTESIAN_POINT('Origin',(2.37857308999266,1.2408968393883,7.58486873427628));
#385439=CARTESIAN_POINT('Ctrl Pts',(2.41656476364781,1.30483398894163,7.50366116529969));
#385440=CARTESIAN_POINT('Ctrl Pts',(2.40131444507885,1.28219650713941,7.52783573079709));
#385441=CARTESIAN_POINT('Ctrl Pts',(2.3860392422488,1.25952355358682,7.55196141284069));
#385442=CARTESIAN_POINT('Ctrl Pts',(2.37073694715283,1.23681194779657,7.57603338728831));
#385443=CARTESIAN_POINT('Ctrl Pts',(2.36315354717505,1.24004694984635,7.59639677331371));
#385444=CARTESIAN_POINT('Ctrl Pts',(2.35069119251653,1.22667677287986,7.59959882295466));
#385445=CARTESIAN_POINT('Ctrl Pts',(2.36887194462181,1.22871860183697,7.59642833564546));
#385446=CARTESIAN_POINT('Ctrl Pts',(2.36006987607436,1.23765821029868,7.58707626057422));
#385447=CARTESIAN_POINT('Ctrl Pts',(2.35925575920167,1.2309314350866,7.58809943920598));
#385448=CARTESIAN_POINT('Ctrl Pts',(2.36517419960408,1.22766241933318,7.58710240504253));
#385449=CARTESIAN_POINT('Ctrl Pts',(2.36608778108832,1.23681532744523,7.58015376756929));
#385450=CARTESIAN_POINT('Ctrl Pts',(2.36537997734291,1.23405339238916,7.58205880659762));
#385451=CARTESIAN_POINT('Ctrl Pts',(2.36800166586016,1.23302683291375,7.58020924244128));
#385452=CARTESIAN_POINT('Ctrl Pts',(2.37073694604121,1.23681194622026,7.57603338509286));
#385453=CARTESIAN_POINT('Ctrl Pts',(2.37073694604121,1.23681194622026,7.57603338509286));
#385454=CARTESIAN_POINT('Ctrl Pts',(2.37073694604121,1.23681194622026,7.57603338509286));
#385455=CARTESIAN_POINT('Origin',(2.37857045058671,1.24090189863631,7.58486873427622));
#385456=CARTESIAN_POINT('Ctrl Pts',(2.46212726359302,1.22693032265429,7.51098857897448));
#385457=CARTESIAN_POINT('Ctrl Pts',(2.45624085415415,1.22703374358942,7.50433767179956));
#385458=CARTESIAN_POINT('Ctrl Pts',(2.45445176918725,1.23545438644277,7.50214974420965));
#385459=CARTESIAN_POINT('Ctrl Pts',(2.43063083103921,1.22748369743086,7.53887321589169));
#385460=CARTESIAN_POINT('Ctrl Pts',(2.42481495123189,1.22758587919964,7.53220407452061));
#385461=CARTESIAN_POINT('Ctrl Pts',(2.42297646352331,1.23596578867811,7.53003438070911));
#385462=CARTESIAN_POINT('Ctrl Pts',(2.39907391371632,1.22803813489113,7.5666946565923));
#385463=CARTESIAN_POINT('Ctrl Pts',(2.39329240467737,1.22813971278464,7.56004085833293));
#385464=CARTESIAN_POINT('Ctrl Pts',(2.39144168852525,1.23647706847158,7.55785582193789));
#385465=CARTESIAN_POINT('Ctrl Pts',(2.36745793881746,1.22859360996012,7.59443891967696));
#385466=CARTESIAN_POINT('Ctrl Pts',(2.36166804731026,1.22869533512896,7.58783901202978));
#385467=CARTESIAN_POINT('Ctrl Pts',(2.35984900020426,1.23698811787147,7.58560008491213));
#385468=CARTESIAN_POINT('',(2.45274559607508,1.23548210681976,7.50366116523517));
#385469=CARTESIAN_POINT('Ctrl Pts',(2.45274559607541,1.23548210681992,7.50366116523554));
#385470=CARTESIAN_POINT('Ctrl Pts',(2.45321593518387,1.23488803726186,7.50350835821027));
#385471=CARTESIAN_POINT('Ctrl Pts',(2.45362896354644,1.2343266411603,7.50345484956));
#385472=CARTESIAN_POINT('Ctrl Pts',(2.45399744452924,1.23378158361682,7.50349758195598));
#385473=CARTESIAN_POINT('Ctrl Pts',(2.45418650260067,1.2335019286745,7.50351950684424));
#385474=CARTESIAN_POINT('Ctrl Pts',(2.45438257535524,1.23319908335876,7.50357029184312));
#385475=CARTESIAN_POINT('Ctrl Pts',(2.4545636187282,1.23290185592397,7.50365515313924));
#385476=CARTESIAN_POINT('Ctrl Pts',(2.45484213674752,1.23244459976999,7.50378570417639));
#385477=CARTESIAN_POINT('Ctrl Pts',(2.45509355696108,1.23198739767575,7.50400001621911));
#385478=CARTESIAN_POINT('Ctrl Pts',(2.45529675319046,1.2315639553412,7.50428903009635));
#385479=CARTESIAN_POINT('Ctrl Pts',(2.45531930640862,1.23151695649984,7.50432110841318));
#385480=CARTESIAN_POINT('Ctrl Pts',(2.45534129185355,1.23147035849848,7.50435406373354));
#385481=CARTESIAN_POINT('Ctrl Pts',(2.45536269990846,1.23142419604732,7.50438785222352));
#385482=CARTESIAN_POINT('Ctrl Pts',(2.45549340637369,1.2311423520945,7.50459414719561));
#385483=CARTESIAN_POINT('Ctrl Pts',(2.4556042026276,1.23087203987399,7.50483629897752));
#385484=CARTESIAN_POINT('Ctrl Pts',(2.45569206180921,1.23062411408573,7.5050991045531));
#385485=CARTESIAN_POINT('Ctrl Pts',(2.45588588798845,1.23007716489503,7.50567888004914));
#385486=CARTESIAN_POINT('Ctrl Pts',(2.45597621046601,1.22961778862668,7.50637912803145));
#385487=CARTESIAN_POINT('Ctrl Pts',(2.45599386342159,1.229243823865,7.50710440483569));
#385488=CARTESIAN_POINT('Ctrl Pts',(2.45599819227676,1.2291521202812,7.50728225710685));
#385489=CARTESIAN_POINT('Ctrl Pts',(2.45599838327277,1.22906373407088,7.50746498566954));
#385490=CARTESIAN_POINT('Ctrl Pts',(2.45599484854336,1.22898072935447,7.50764697238949));
#385491=CARTESIAN_POINT('Ctrl Pts',(2.45597584681085,1.22853451884255,7.50862528291181));
#385492=CARTESIAN_POINT('Ctrl Pts',(2.45585158784298,1.2282031429546,7.50965856837421));
#385493=CARTESIAN_POINT('Ctrl Pts',(2.45567561046202,1.22794749938439,7.51067959873201));
#385494=CARTESIAN_POINT('Ctrl Pts',(2.45557876988732,1.22780681840526,7.51124147302578));
#385495=CARTESIAN_POINT('Ctrl Pts',(2.45546588589085,1.22768928353925,7.51180065547252));
#385496=CARTESIAN_POINT('Ctrl Pts',(2.45534370115124,1.22758999909434,7.512351757165));
#385497=CARTESIAN_POINT('Ctrl Pts',(2.45492150420325,1.22724693178692,7.51425603304536));
#385498=CARTESIAN_POINT('Ctrl Pts',(2.45433409491521,1.22708557269675,7.5162690050518));
#385499=CARTESIAN_POINT('Ctrl Pts',(2.45363638664936,1.22708087806131,7.51827788969244));
#385500=CARTESIAN_POINT('Ctrl Pts',(2.45359862535953,1.22708062397877,7.51838661432545));
#385501=CARTESIAN_POINT('Ctrl Pts',(2.45356053346671,1.22708083533097,7.51849533314857));
#385502=CARTESIAN_POINT('Ctrl Pts',(2.45352211735224,1.2270815102807,7.51860402984325));
#385503=CARTESIAN_POINT('Ctrl Pts',(2.37073694797139,1.23681194623013,7.57603338728985));
#385504=CARTESIAN_POINT('Ctrl Pts',(2.39811907486655,1.23636877604874,7.55196141284922));
#385505=CARTESIAN_POINT('Ctrl Pts',(2.42545400034853,1.23592549913145,7.52783573083105));
#385506=CARTESIAN_POINT('Ctrl Pts',(2.45274559613391,1.23548210681337,7.50366116530176));
#385507=CARTESIAN_POINT('Origin',(8.19199203866625E-16,4.27375699935098E-16,
7.49482233047033));
#385508=CARTESIAN_POINT('Origin',(2.40878727587057,1.3006345026963,7.49482233047033));
#385509=CARTESIAN_POINT('Origin',(0.,0.,7.50366116523517));
#385510=CARTESIAN_POINT('Origin',(2.44485166369884,1.23150582317302,7.49482233047033));
#385511=CARTESIAN_POINT('Ctrl Pts',(2.41011849833277,1.31027611334855,7.51860402984325));
#385512=CARTESIAN_POINT('Ctrl Pts',(2.41436194636775,1.31659192167406,7.51860402984325));
#385513=CARTESIAN_POINT('Ctrl Pts',(2.41070061931035,1.32326207686033,7.51860402984325));
#385514=CARTESIAN_POINT('Ctrl Pts',(2.41169411849219,1.31262121678981,7.51041458714367));
#385515=CARTESIAN_POINT('Ctrl Pts',(2.41349452737361,1.31817215307298,7.51004642900444));
#385516=CARTESIAN_POINT('Ctrl Pts',(2.41069960955982,1.32326391640993,7.50729136483011));
#385517=CARTESIAN_POINT('Ctrl Pts',(2.41442875339228,1.31195375206225,7.50215815450137));
#385518=CARTESIAN_POINT('Ctrl Pts',(2.41526080207567,1.31495471182038,7.49877163671528));
#385519=CARTESIAN_POINT('Ctrl Pts',(2.41362156250511,1.31799063296965,7.49481588533168));
#385520=CARTESIAN_POINT('Ctrl Pts',(2.4165642792075,1.30483372733005,7.50366171572174));
#385521=CARTESIAN_POINT('Ctrl Pts',(2.4197863045277,1.30657347302791,7.50000045605858));
#385522=CARTESIAN_POINT('Ctrl Pts',(2.41978630452764,1.30657347302802,7.49482233047317));
#385523=CARTESIAN_POINT('Origin',(2.39974288922258,1.31724724923823,7.51860402984325));
#385524=CARTESIAN_POINT('Origin',(2.39974288922258,1.31724724923823,9.));
#385525=CARTESIAN_POINT('Origin',(2.39974288922258,1.31724724923823,8.75721825406948));
#385526=CARTESIAN_POINT('Ctrl Pts',(2.40080670870024,1.29641427264101,8.78942910404912));
#385527=CARTESIAN_POINT('Ctrl Pts',(2.4039307878628,1.3010286586335,8.7967269950169));
#385528=CARTESIAN_POINT('Ctrl Pts',(2.39758410530011,1.30730505142161,8.79893251111267));
#385529=CARTESIAN_POINT('Ctrl Pts',(2.4069373809179,1.3055406233301,8.78111911759584));
#385530=CARTESIAN_POINT('Ctrl Pts',(2.4106348489598,1.31101520461131,8.78644465894814));
#385531=CARTESIAN_POINT('Ctrl Pts',(2.40622746632976,1.31781891610784,8.78817647674132));
#385532=CARTESIAN_POINT('Ctrl Pts',(2.41075816204786,1.31122838278128,8.7678092393203));
#385533=CARTESIAN_POINT('Ctrl Pts',(2.41511864407147,1.31769374690809,8.76988516158373));
#385534=CARTESIAN_POINT('Ctrl Pts',(2.41161733062358,1.3243927904619,8.77093053738833));
#385535=CARTESIAN_POINT('Ctrl Pts',(2.41001316201714,1.31011934753173,8.75371302330492));
#385536=CARTESIAN_POINT('Ctrl Pts',(2.41426725614075,1.316425605103,8.75300828287559));
#385537=CARTESIAN_POINT('Ctrl Pts',(2.41056573435195,1.32311090807155,8.75267964240738));
#385538=CARTESIAN_POINT('Origin',(2.39192360866379,1.3056071619048,8.78727029226991));
#385539=CARTESIAN_POINT('Ctrl Pts',(2.36243414091424,1.23929131094307,8.85049129520029));
#385540=CARTESIAN_POINT('Ctrl Pts',(2.36569043114741,1.24413875213822,8.85711686593484));
#385541=CARTESIAN_POINT('Ctrl Pts',(2.35986814900601,1.25039988564422,8.85933012996512));
#385542=CARTESIAN_POINT('Ctrl Pts',(2.3757420305442,1.2591019567374,8.82945683644723));
#385543=CARTESIAN_POINT('Ctrl Pts',(2.37902534995512,1.26398963462527,8.83607469902391));
#385544=CARTESIAN_POINT('Ctrl Pts',(2.37315851053407,1.27024361237588,8.83829567148519));
#385545=CARTESIAN_POINT('Ctrl Pts',(2.3890300836915,1.27888307316661,8.80838214965003));
#385546=CARTESIAN_POINT('Ctrl Pts',(2.39232636061372,1.28379004011345,8.81501364461987));
#385547=CARTESIAN_POINT('Ctrl Pts',(2.38642926673663,1.29005686517883,8.81722098428721));
#385548=CARTESIAN_POINT('Ctrl Pts',(2.40229980761778,1.29863690399944,8.78727029226991));
#385549=CARTESIAN_POINT('Ctrl Pts',(2.40559663206245,1.30354468600962,8.79393457792714));
#385550=CARTESIAN_POINT('Ctrl Pts',(2.39968192566131,1.30984196029033,8.79610912703474));
#385551=CARTESIAN_POINT('Origin',(2.35205794196025,1.24626156884843,8.85049129520029));
#385552=CARTESIAN_POINT('Ctrl Pts',(2.36802027905701,1.22858372995534,8.85049129520029));
#385553=CARTESIAN_POINT('Ctrl Pts',(2.37385899372365,1.22848114699079,8.85711686593484));
#385554=CARTESIAN_POINT('Ctrl Pts',(2.37566317709457,1.22012377392995,8.85933012996512));
#385555=CARTESIAN_POINT('Ctrl Pts',(2.36285485247416,1.22867448362327,8.86332496987231));
#385556=CARTESIAN_POINT('Ctrl Pts',(2.36523842990887,1.22471589132429,8.86648636486738));
#385557=CARTESIAN_POINT('Ctrl Pts',(2.36121298657354,1.22039479101918,8.87206031107457));
#385558=CARTESIAN_POINT('Ctrl Pts',(2.35953377205362,1.23497370824509,8.86341338519876));
#385559=CARTESIAN_POINT('Ctrl Pts',(2.3576183774015,1.23919327385792,8.86654584966059));
#385560=CARTESIAN_POINT('Ctrl Pts',(2.35175919171291,1.23830215329706,8.87215952290714));
#385561=CARTESIAN_POINT('Ctrl Pts',(2.36243414091424,1.23929131094307,8.85049129520029));
#385562=CARTESIAN_POINT('Ctrl Pts',(2.36569043114741,1.24413875213822,8.85711686593484));
#385563=CARTESIAN_POINT('Ctrl Pts',(2.35986814900601,1.25039988564422,8.85933012996512));
#385564=CARTESIAN_POINT('Origin',(2.36780069490805,1.21608565879209,8.85049129520029));
#385565=CARTESIAN_POINT('Ctrl Pts',(2.43950170000242,1.22732784120422,8.78727029226991));
#385566=CARTESIAN_POINT('Ctrl Pts',(2.44541309482907,1.22722398128974,8.79393457792714));
#385567=CARTESIAN_POINT('Ctrl Pts',(2.44719404240187,1.21877012767608,8.79610912703474));
#385568=CARTESIAN_POINT('Ctrl Pts',(2.41570832589787,1.22774587753441,8.80838214965002));
#385569=CARTESIAN_POINT('Ctrl Pts',(2.4216187389855,1.22764203486855,8.81501364461988));
#385570=CARTESIAN_POINT('Ctrl Pts',(2.42338478937513,1.21922004706182,8.81722098428721));
#385571=CARTESIAN_POINT('Ctrl Pts',(2.39188208645151,1.22816449129036,8.82945683644721));
#385572=CARTESIAN_POINT('Ctrl Pts',(2.39776926598005,1.22806105682517,8.83607469902391));
#385573=CARTESIAN_POINT('Ctrl Pts',(2.39954208843694,1.2196712330467,8.83829567148519));
#385574=CARTESIAN_POINT('Ctrl Pts',(2.36802027905701,1.22858372995534,8.85049129520029));
#385575=CARTESIAN_POINT('Ctrl Pts',(2.37385899372365,1.22848114699079,8.85711686593484));
#385576=CARTESIAN_POINT('Ctrl Pts',(2.37566317709457,1.22012377392995,8.85933012996512));
#385577=CARTESIAN_POINT('Origin',(2.43928211585346,1.21482977004097,8.78727029226991));
#385578=CARTESIAN_POINT('Ctrl Pts',(2.45333698446993,1.22708474451241,8.75374538247848));
#385579=CARTESIAN_POINT('Ctrl Pts',(2.46093500328082,1.22696437617396,8.75304829418601));
#385580=CARTESIAN_POINT('Ctrl Pts',(2.46430190265074,1.22011349069529,8.75272238421917));
#385581=CARTESIAN_POINT('Ctrl Pts',(2.45465676447423,1.22706155713948,8.76769408445019));
#385582=CARTESIAN_POINT('Ctrl Pts',(2.46244597221949,1.22693746977907,8.76974318093971));
#385583=CARTESIAN_POINT('Ctrl Pts',(2.46593649005342,1.22024160220786,8.77077869880429));
#385584=CARTESIAN_POINT('Ctrl Pts',(2.44789232400142,1.22718040241893,8.78108014887992));
#385585=CARTESIAN_POINT('Ctrl Pts',(2.4544934574888,1.22707904176507,8.78639403366324));
#385586=CARTESIAN_POINT('Ctrl Pts',(2.45756595314955,1.21959026041271,8.78812224174742));
#385587=CARTESIAN_POINT('Ctrl Pts',(2.4368068993313,1.22737516356144,8.78944554828686));
#385588=CARTESIAN_POINT('Ctrl Pts',(2.44237017583327,1.22729533762874,8.79673892988686));
#385589=CARTESIAN_POINT('Ctrl Pts',(2.44388779729732,1.2185089629834,8.79894799272499));
#385590=CARTESIAN_POINT('Origin',(2.45330253320328,1.21458343911746,8.75721825406948));
#385591=CARTESIAN_POINT('Origin',(2.45330253320328,1.21458343911746,9.));
#385592=CARTESIAN_POINT('Origin',(2.45330253320328,1.21458343911746,7.51860402984325));
#385593=CARTESIAN_POINT('Ctrl Pts',(2.45274489350846,1.2354817529271,7.50366195182966));
#385594=CARTESIAN_POINT('Ctrl Pts',(2.45601536992583,1.23712913743396,7.50000065167735));
#385595=CARTESIAN_POINT('Ctrl Pts',(2.45601536992589,1.23712913743385,7.49482233047108));
#385596=CARTESIAN_POINT('Ctrl Pts',(2.45736618897607,1.2296510216001,7.50215800491337));
#385597=CARTESIAN_POINT('Ctrl Pts',(2.46030407593302,1.22861491475105,7.49877273257265));
#385598=CARTESIAN_POINT('Ctrl Pts',(2.46185708707723,1.22553184603046,7.49481816995647));
#385599=CARTESIAN_POINT('Ctrl Pts',(2.45634027370536,1.22703233601389,7.51043025814043));
#385600=CARTESIAN_POINT('Ctrl Pts',(2.46192726936052,1.22533579938413,7.51006209594516));
#385601=CARTESIAN_POINT('Ctrl Pts',(2.46450595122239,1.22012721320191,7.50731281821701));
#385602=CARTESIAN_POINT('Ctrl Pts',(2.45352060617641,1.22708153673983,7.51860402984326));
#385603=CARTESIAN_POINT('Ctrl Pts',(2.46112871992397,1.22694878661777,7.51860402984326));
#385604=CARTESIAN_POINT('Ctrl Pts',(2.46450482787544,1.22012948221845,7.51860402984327));
#385605=CARTESIAN_POINT('Origin',(0.,0.,7.5));
#385606=CARTESIAN_POINT('Origin',(2.44187055726727,1.07433989271898,7.5));
#385607=CARTESIAN_POINT('',(2.44187055726727,1.07433989271898,7.59394543036555));
#385608=CARTESIAN_POINT('',(2.44187055726727,1.07433989271898,8.85049129520029));
#385609=CARTESIAN_POINT('',(2.44187055726727,1.07433989271898,7.5));
#385610=CARTESIAN_POINT('',(2.51312464689843,1.06850675396149,8.78727029226991));
#385611=CARTESIAN_POINT('Ctrl Pts',(2.44187055726727,1.07433989271898,8.85049129520029));
#385612=CARTESIAN_POINT('Ctrl Pts',(2.46565644538428,1.07239268678912,8.82945686509571));
#385613=CARTESIAN_POINT('Ctrl Pts',(2.48940697290245,1.07044837561632,8.80838212259895));
#385614=CARTESIAN_POINT('Ctrl Pts',(2.51312464689843,1.06850675396149,8.78727029226991));
#385615=CARTESIAN_POINT('',(2.52710047532066,1.06736263792745,8.75721825406948));
#385616=CARTESIAN_POINT('Origin',(2.48504237581485,1.07080588110006,8.75937679713113));
#385617=CARTESIAN_POINT('',(2.52710047532066,1.06736263792745,7.51860402984325));
#385618=CARTESIAN_POINT('',(2.52710047532066,1.06736263792745,7.5));
#385619=CARTESIAN_POINT('Ctrl Pts',(2.52710047532066,1.06736263792745,7.51860402984325));
#385620=CARTESIAN_POINT('Ctrl Pts',(2.51612463574747,1.06826116312848,7.52834476460825));
#385621=CARTESIAN_POINT('Ctrl Pts',(2.50514167081761,1.06916027163912,7.53807742314407));
#385622=CARTESIAN_POINT('Ctrl Pts',(2.49415134128774,1.07005998304475,7.54780169004674));
#385623=CARTESIAN_POINT('Ctrl Pts',(2.47674325328906,1.071485077286,7.5632044032688));
#385624=CARTESIAN_POINT('Ctrl Pts',(2.45931666632383,1.07291168592507,7.57858609112103));
#385625=CARTESIAN_POINT('Ctrl Pts',(2.44187055726727,1.07433989271898,7.59394543036555));
#385626=CARTESIAN_POINT('Origin',(2.60463825998836,1.3033658465605,7.5));
#385627=CARTESIAN_POINT('',(2.48911697509581,1.15316802656823,8.75721825406948));
#385628=CARTESIAN_POINT('',(2.4805679771315,1.1420528380681,8.78727029226991));
#385629=CARTESIAN_POINT('Origin',(2.4588674316814,1.11383834389691,8.75658640621072));
#385630=CARTESIAN_POINT('',(2.43698193351377,1.08538337893284,8.85049129520029));
#385631=CARTESIAN_POINT('Ctrl Pts',(2.4805679771315,1.1420528380681,8.78727029226991));
#385632=CARTESIAN_POINT('Ctrl Pts',(2.4660599035788,1.12318981189998,8.80838212259896));
#385633=CARTESIAN_POINT('Ctrl Pts',(2.45153173356484,1.10430065682692,8.82945686509571));
#385634=CARTESIAN_POINT('Ctrl Pts',(2.43698193351377,1.08538337893284,8.85049129520029));
#385635=CARTESIAN_POINT('',(2.43698193351377,1.08538337893284,7.59394543036555));
#385636=CARTESIAN_POINT('',(2.43698193351377,1.08538337893284,7.5));
#385637=CARTESIAN_POINT('',(2.48911697509581,1.15316802656823,7.51860402984325));
#385638=CARTESIAN_POINT('Ctrl Pts',(2.43698193351377,1.08538337893284,7.59394543036555));
#385639=CARTESIAN_POINT('Ctrl Pts',(2.44765369809929,1.09925853430101,7.57858609112103));
#385640=CARTESIAN_POINT('Ctrl Pts',(2.45831352104416,1.11311816345342,7.56320440326857));
#385641=CARTESIAN_POINT('Ctrl Pts',(2.46896202819286,1.12696308009709,7.54780169004651));
#385642=CARTESIAN_POINT('Ctrl Pts',(2.47568479996275,1.13570385600764,7.53807742314383));
#385643=CARTESIAN_POINT('Ctrl Pts',(2.48240306681553,1.14443877474018,7.52834476460825));
#385644=CARTESIAN_POINT('Ctrl Pts',(2.48911697509581,1.15316802656823,7.51860402984325));
#385645=CARTESIAN_POINT('',(2.48911697509581,1.15316802656823,7.5));
#385646=CARTESIAN_POINT('Origin',(2.44243149520446,1.08119197077097,7.5));
#385647=CARTESIAN_POINT('Ctrl Pts',(2.43698193351377,1.08538337893284,8.85049129520029));
#385648=CARTESIAN_POINT('Ctrl Pts',(2.43686386596228,1.08522987052213,8.85097269580138));
#385649=CARTESIAN_POINT('Ctrl Pts',(2.43675395547126,1.0850731708077,8.85143669361005));
#385650=CARTESIAN_POINT('Ctrl Pts',(2.43664785678659,1.08490556222797,8.8519052845931));
#385651=CARTESIAN_POINT('Ctrl Pts',(2.4364403344879,1.08457773047535,8.85282181883899));
#385652=CARTESIAN_POINT('Ctrl Pts',(2.43625289970127,1.08421649283684,8.85372622499635));
#385653=CARTESIAN_POINT('Ctrl Pts',(2.43609629735109,1.08380907959058,8.8546225773507));
#385654=CARTESIAN_POINT('Ctrl Pts',(2.43596629164197,1.08347085958349,8.85536669723986));
#385655=CARTESIAN_POINT('Ctrl Pts',(2.43585747567321,1.08310075080978,8.85610498449051));
#385656=CARTESIAN_POINT('Ctrl Pts',(2.43578366534162,1.08268915855854,8.85681338218371));
#385657=CARTESIAN_POINT('Ctrl Pts',(2.43571668234977,1.08231563794411,8.85745625420284));
#385658=CARTESIAN_POINT('Ctrl Pts',(2.43567709924276,1.08190337344397,8.85808743050666));
#385659=CARTESIAN_POINT('Ctrl Pts',(2.43568941398076,1.08143761053014,8.85866804508411));
#385660=CARTESIAN_POINT('Ctrl Pts',(2.43569509573392,1.0812227176182,8.85893592806396));
#385661=CARTESIAN_POINT('Ctrl Pts',(2.4357120460353,1.08099633712461,8.85919241173848));
#385662=CARTESIAN_POINT('Ctrl Pts',(2.43574420383571,1.0807565752059,8.85943017985534));
#385663=CARTESIAN_POINT('Ctrl Pts',(2.43578762638599,1.08043282563852,8.8597512372));
#385664=CARTESIAN_POINT('Ctrl Pts',(2.43586051684358,1.08007652260804,8.86004599534706));
#385665=CARTESIAN_POINT('Ctrl Pts',(2.43597220322128,1.07969403438973,8.86026130871721));
#385666=CARTESIAN_POINT('Ctrl Pts',(2.43601309475293,1.07955399466952,8.86034014101235));
#385667=CARTESIAN_POINT('Ctrl Pts',(2.43605978927648,1.07940833782478,8.86040910639692));
#385668=CARTESIAN_POINT('Ctrl Pts',(2.43611133494716,1.07926113488276,8.86046313645506));
#385669=CARTESIAN_POINT('Ctrl Pts',(2.43619177153458,1.07903142592456,8.86054744990829));
#385670=CARTESIAN_POINT('Ctrl Pts',(2.43628635577067,1.07879173024466,8.86059655985668));
#385671=CARTESIAN_POINT('Ctrl Pts',(2.43638874917194,1.07855731272453,8.86059725258816));
#385672=CARTESIAN_POINT('Ctrl Pts',(2.43649137914287,1.07832235360627,8.86059794692011));
#385673=CARTESIAN_POINT('Ctrl Pts',(2.43660542722858,1.07809115479434,8.86056369958366));
#385674=CARTESIAN_POINT('Ctrl Pts',(2.43672129836424,1.07787466121546,8.86048590497774));
#385675=CARTESIAN_POINT('Ctrl Pts',(2.43675153728075,1.07781816283716,8.86046560290182));
#385676=CARTESIAN_POINT('Ctrl Pts',(2.436782373608,1.07776197369632,8.86044257503091));
#385677=CARTESIAN_POINT('Ctrl Pts',(2.4368128257005,1.07770781429098,8.86041778462583));
#385678=CARTESIAN_POINT('Ctrl Pts',(2.43701773049513,1.07734338869924,8.86025097596201));
#385679=CARTESIAN_POINT('Ctrl Pts',(2.43723302339879,1.07702212339167,8.8599848982295));
#385680=CARTESIAN_POINT('Ctrl Pts',(2.43744538234536,1.07674867865403,8.85968173251461));
#385681=CARTESIAN_POINT('Ctrl Pts',(2.43755770806138,1.07660404205434,8.85952137522076));
#385682=CARTESIAN_POINT('Ctrl Pts',(2.43767122725319,1.07646987960889,8.85934740853961));
#385683=CARTESIAN_POINT('Ctrl Pts',(2.4377831523128,1.07634707916857,8.8591675900182));
#385684=CARTESIAN_POINT('Ctrl Pts',(2.43823258960464,1.07585397157031,8.85844552518695));
#385685=CARTESIAN_POINT('Ctrl Pts',(2.4386794872598,1.07551416185936,8.85759444184124));
#385686=CARTESIAN_POINT('Ctrl Pts',(2.43906874957054,1.07526982784832,8.85683498915138));
#385687=CARTESIAN_POINT('Ctrl Pts',(2.43910948483467,1.07524425894478,8.85675551444998));
#385688=CARTESIAN_POINT('Ctrl Pts',(2.43914959602974,1.07521975426587,8.85667699793651));
#385689=CARTESIAN_POINT('Ctrl Pts',(2.43918902404595,1.07519626004797,8.85659965593547));
#385690=CARTESIAN_POINT('Ctrl Pts',(2.43972122542068,1.07487913389593,8.85555568965886));
#385691=CARTESIAN_POINT('Ctrl Pts',(2.4402785032058,1.07465121642548,8.85434650606346));
#385692=CARTESIAN_POINT('Ctrl Pts',(2.44086125969317,1.0745056286935,8.85297329937118));
#385693=CARTESIAN_POINT('Ctrl Pts',(2.44118902470945,1.07442374446505,8.85220095427747));
#385694=CARTESIAN_POINT('Ctrl Pts',(2.44152505987875,1.07436817648792,8.85137579139184));
#385695=CARTESIAN_POINT('Ctrl Pts',(2.44187055726727,1.07433989271898,8.85049129520029));
#385696=CARTESIAN_POINT('Origin',(2.44243149520446,1.08119197077097,7.59394543036555));
#385697=CARTESIAN_POINT('Ctrl Pts',(2.43663914358207,1.08493769223099,7.59443877723642));
#385698=CARTESIAN_POINT('Ctrl Pts',(2.43310873710912,1.08034754803015,7.58783886950016));
#385699=CARTESIAN_POINT('Ctrl Pts',(2.43845813862246,1.07375489416499,7.58559994247159));
#385700=CARTESIAN_POINT('Ctrl Pts',(2.45591152894015,1.10999515475426,7.56670252222136));
#385701=CARTESIAN_POINT('Ctrl Pts',(2.45238622490691,1.10541164461491,7.56004874999027));
#385702=CARTESIAN_POINT('Ctrl Pts',(2.45775073258753,1.09876646481299,7.55786368756704));
#385703=CARTESIAN_POINT('Ctrl Pts',(2.4751479250441,1.13500582496978,7.53888913333557));
#385704=CARTESIAN_POINT('Ctrl Pts',(2.47160166995631,1.13039507480532,7.53222002137274));
#385705=CARTESIAN_POINT('Ctrl Pts',(2.47700705952566,1.12373292737947,7.53005029815327));
#385706=CARTESIAN_POINT('Ctrl Pts',(2.49434746143404,1.15996857112789,7.51101258149734));
#385707=CARTESIAN_POINT('Ctrl Pts',(2.4907582192909,1.15530193029348,7.5043616886572));
#385708=CARTESIAN_POINT('Ctrl Pts',(2.49622623346789,1.14865299786,7.50217374673251));
#385709=CARTESIAN_POINT('',(2.49520067284432,1.14732323151531,7.50366116523517));
#385710=CARTESIAN_POINT('Ctrl Pts',(2.48911697509581,1.15316802656823,7.51860402984325));
#385711=CARTESIAN_POINT('Ctrl Pts',(2.48938620751088,1.15351807566829,7.51734760759493));
#385712=CARTESIAN_POINT('Ctrl Pts',(2.48967665844453,1.15379812229854,7.51608817408573));
#385713=CARTESIAN_POINT('Ctrl Pts',(2.48999692855533,1.15399790928256,7.5148100591312));
#385714=CARTESIAN_POINT('Ctrl Pts',(2.4902870368748,1.15417888110675,7.51365231206384));
#385715=CARTESIAN_POINT('Ctrl Pts',(2.49060188885869,1.15429446588341,7.51247773061043));
#385716=CARTESIAN_POINT('Ctrl Pts',(2.49094876154749,1.15430800048867,7.51129758471022));
#385717=CARTESIAN_POINT('Ctrl Pts',(2.49137988468531,1.15432482245729,7.50983079813402));
#385718=CARTESIAN_POINT('Ctrl Pts',(2.49184722096597,1.15417044930113,7.50839324291155));
#385719=CARTESIAN_POINT('Ctrl Pts',(2.49232832348223,1.1537654749321,7.50715379678855));
#385720=CARTESIAN_POINT('Ctrl Pts',(2.49255057898211,1.15357838844267,7.50658120839351));
#385721=CARTESIAN_POINT('Ctrl Pts',(2.49280124912323,1.1533039540612,7.50598221009429));
#385722=CARTESIAN_POINT('Ctrl Pts',(2.49305757339242,1.15293336235142,7.50545747549611));
#385723=CARTESIAN_POINT('Ctrl Pts',(2.49319435595644,1.15273560314419,7.50517746087247));
#385724=CARTESIAN_POINT('Ctrl Pts',(2.49333439835687,1.15250843276059,7.50491486231392));
#385725=CARTESIAN_POINT('Ctrl Pts',(2.49347257213967,1.15225699174058,7.50468370960992));
#385726=CARTESIAN_POINT('Ctrl Pts',(2.4936791855294,1.15188100810308,7.50433806340446));
#385727=CARTESIAN_POINT('Ctrl Pts',(2.49388732843373,1.15143921367341,7.50405484070983));
#385728=CARTESIAN_POINT('Ctrl Pts',(2.49408233474293,1.1509610571583,7.5038576603613));
#385729=CARTESIAN_POINT('Ctrl Pts',(2.49410318763662,1.15090992575125,7.50383657498791));
#385730=CARTESIAN_POINT('Ctrl Pts',(2.49412389444683,1.15085840660396,7.50381643264937));
#385731=CARTESIAN_POINT('Ctrl Pts',(2.49414444056045,1.15080655606423,7.50379723213559));
#385732=CARTESIAN_POINT('Ctrl Pts',(2.49428159258994,1.15046043675001,7.50366906242519));
#385733=CARTESIAN_POINT('Ctrl Pts',(2.49441389887393,1.15009175680351,7.50358235568538));
#385734=CARTESIAN_POINT('Ctrl Pts',(2.49453288367519,1.14973332922379,7.5035341175365));
#385735=CARTESIAN_POINT('Ctrl Pts',(2.49471128791821,1.14919590763417,7.50346178989176));
#385736=CARTESIAN_POINT('Ctrl Pts',(2.49488035974129,1.14861017875719,7.50346967198527));
#385737=CARTESIAN_POINT('Ctrl Pts',(2.49502864299076,1.14803006738152,7.50354272648692));
#385738=CARTESIAN_POINT('Ctrl Pts',(2.49508963496055,1.14779145556511,7.50357277531559));
#385739=CARTESIAN_POINT('Ctrl Pts',(2.49514716616304,1.14755414629688,7.50361331098761));
#385740=CARTESIAN_POINT('Ctrl Pts',(2.49520067284561,1.1473232315159,7.50366116523659));
#385741=CARTESIAN_POINT('',(2.44510882695076,1.08237714611462,7.57603338622103));
#385742=CARTESIAN_POINT('Origin',(2.45319058995184,1.0859515826301,7.58486873427627));
#385743=CARTESIAN_POINT('Ctrl Pts',(2.49520067287494,1.14732323156379,7.50366116529969));
#385744=CARTESIAN_POINT('Ctrl Pts',(2.47853129928219,1.12570935216129,7.52783573079709));
#385745=CARTESIAN_POINT('Ctrl Pts',(2.46183481987291,1.10406166822897,7.55196141284068));
#385746=CARTESIAN_POINT('Ctrl Pts',(2.44510882740428,1.08237714728166,7.57603338728831));
#385747=CARTESIAN_POINT('Ctrl Pts',(2.43774827562801,1.08609137277755,7.59639677331371));
#385748=CARTESIAN_POINT('Ctrl Pts',(2.42383037731441,1.07295780766365,7.59974925422225));
#385749=CARTESIAN_POINT('Ctrl Pts',(2.4429098820182,1.07443121403228,7.59639677331372));
#385750=CARTESIAN_POINT('Ctrl Pts',(2.43451789319204,1.08390511263724,7.58707626057422));
#385751=CARTESIAN_POINT('Ctrl Pts',(2.4332529139748,1.07712888513356,7.58811717123965));
#385752=CARTESIAN_POINT('Ctrl Pts',(2.43911965275286,1.07350965763148,7.58707626057424));
#385753=CARTESIAN_POINT('Ctrl Pts',(2.44046943008489,1.08267839307897,7.5801537675693));
#385754=CARTESIAN_POINT('Ctrl Pts',(2.43957276865562,1.07992649732891,7.58208760766041));
#385755=CARTESIAN_POINT('Ctrl Pts',(2.44221276280679,1.07874017409314,7.5801537675693));
#385756=CARTESIAN_POINT('Ctrl Pts',(2.44510882619394,1.08237714577982,7.57603338509286));
#385757=CARTESIAN_POINT('Ctrl Pts',(2.44510882619394,1.08237714577982,7.57603338509286));
#385758=CARTESIAN_POINT('Ctrl Pts',(2.44510882619394,1.08237714577982,7.57603338509286));
#385759=CARTESIAN_POINT('Origin',(2.45318828011531,1.08595680059061,7.5848687342762));
#385760=CARTESIAN_POINT('Ctrl Pts',(2.53567825474112,1.06666042731961,7.51098857897448));
#385761=CARTESIAN_POINT('Ctrl Pts',(2.52981056576382,1.06714077931299,7.50433767179956));
#385762=CARTESIAN_POINT('Ctrl Pts',(2.52856466910386,1.07565874811988,7.50214974420965));
#385763=CARTESIAN_POINT('Ctrl Pts',(2.50428198982965,1.06923064849069,7.53887321589171));
#385764=CARTESIAN_POINT('Ctrl Pts',(2.49848460617955,1.06970524501469,7.53220407452063));
#385765=CARTESIAN_POINT('Ctrl Pts',(2.49718679848483,1.07818572938232,7.53003438070912));
#385766=CARTESIAN_POINT('Ctrl Pts',(2.4728254325079,1.07180580543453,7.5666946565923));
#385767=CARTESIAN_POINT('Ctrl Pts',(2.46706231031734,1.07227759718128,7.56004085833297));
#385768=CARTESIAN_POINT('Ctrl Pts',(2.46574957287294,1.0807163986678,7.55785582193789));
#385769=CARTESIAN_POINT('Ctrl Pts',(2.44131000543014,1.07438578168709,7.59443891967696));
#385770=CARTESIAN_POINT('Ctrl Pts',(2.43553852742995,1.07485825747318,7.58783901202978));
#385771=CARTESIAN_POINT('Ctrl Pts',(2.43425453816588,1.08325054855239,7.58560008491213));
#385772=CARTESIAN_POINT('',(2.52686377755798,1.075795726429,7.50366116523517));
#385773=CARTESIAN_POINT('Ctrl Pts',(2.52686377755832,1.07579572642914,7.50366116523554));
#385774=CARTESIAN_POINT('Ctrl Pts',(2.52729508813737,1.07517274272056,7.50350835821027));
#385775=CARTESIAN_POINT('Ctrl Pts',(2.52767129911715,1.07458603724944,7.50345484956));
#385776=CARTESIAN_POINT('Ctrl Pts',(2.52800410105954,1.07401849092752,7.50349758195598));
#385777=CARTESIAN_POINT('Ctrl Pts',(2.52817485313721,1.07372729757405,7.50351950684424));
#385778=CARTESIAN_POINT('Ctrl Pts',(2.52835111967327,1.07341251206197,7.50357029184312));
#385779=CARTESIAN_POINT('Ctrl Pts',(2.52851274764608,1.07310429582409,7.50365515313923));
#385780=CARTESIAN_POINT('Ctrl Pts',(2.52876139691789,1.07263013444116,7.50378570417639));
#385781=CARTESIAN_POINT('Ctrl Pts',(2.5289830075229,1.07215776316926,7.50400001621911));
#385782=CARTESIAN_POINT('Ctrl Pts',(2.52915865622031,1.07172217201528,7.50428903009634));
#385783=CARTESIAN_POINT('Ctrl Pts',(2.52917815187436,1.07167382474843,7.50432110841318));
#385784=CARTESIAN_POINT('Ctrl Pts',(2.52919710660364,1.07162591387537,7.50435406373354));
#385785=CARTESIAN_POINT('Ctrl Pts',(2.529215513035,1.07157847465114,7.50438785222351));
#385786=CARTESIAN_POINT('Ctrl Pts',(2.52932789314572,1.07128883538497,7.50459414719561));
#385787=CARTESIAN_POINT('Ctrl Pts',(2.52942114279341,1.07101197980954,7.50483629897752));
#385788=CARTESIAN_POINT('Ctrl Pts',(2.52949293679912,1.07075893425431,7.5050991045531));
#385789=CARTESIAN_POINT('Ctrl Pts',(2.52965132158672,1.07020069034344,7.50567888004914));
#385790=CARTESIAN_POINT('Ctrl Pts',(2.52971202614849,1.0697364709319,7.50637912803144));
#385791=CARTESIAN_POINT('Ctrl Pts',(2.52970568282964,1.06936214349218,7.50710440483569));
#385792=CARTESIAN_POINT('Ctrl Pts',(2.52970412732193,1.06927035097252,7.50728225710685));
#385793=CARTESIAN_POINT('Ctrl Pts',(2.52969865500157,1.069182134124,7.50746498566954));
#385794=CARTESIAN_POINT('Ctrl Pts',(2.52968980940421,1.06909952642057,7.50764697238949));
#385795=CARTESIAN_POINT('Ctrl Pts',(2.52964225790714,1.06865545014118,7.50862528291182));
#385796=CARTESIAN_POINT('Ctrl Pts',(2.5294970229166,1.06833271639993,7.50965856837422));
#385797=CARTESIAN_POINT('Ctrl Pts',(2.52930502796027,1.06808887298637,7.51067959873202));
#385798=CARTESIAN_POINT('Ctrl Pts',(2.52919937289363,1.06795468564832,7.51124147302579));
#385799=CARTESIAN_POINT('Ctrl Pts',(2.52907919034472,1.06784462477279,7.51180065547253));
#385800=CARTESIAN_POINT('Ctrl Pts',(2.52895089547053,1.06775337272156,7.51235175716501));
#385801=CARTESIAN_POINT('Ctrl Pts',(2.52850758557361,1.06743806053406,7.51425603304536));
#385802=CARTESIAN_POINT('Ctrl Pts',(2.52791104486854,1.06731466841575,7.5162690050518));
#385803=CARTESIAN_POINT('Ctrl Pts',(2.52721446933283,1.06735468574801,7.51827788969243));
#385804=CARTESIAN_POINT('Ctrl Pts',(2.52717676934849,1.06735685156166,7.51838661432545));
#385805=CARTESIAN_POINT('Ctrl Pts',(2.52713876926093,1.06735950303556,7.51849533314856));
#385806=CARTESIAN_POINT('Ctrl Pts',(2.52710047532066,1.06736263792744,7.51860402984325));
#385807=CARTESIAN_POINT('Ctrl Pts',(2.44510882812078,1.08237714566601,7.57603338728985));
#385808=CARTESIAN_POINT('Ctrl Pts',(2.4724063014885,1.08018050713157,7.55196141284922));
#385809=CARTESIAN_POINT('Ctrl Pts',(2.49965666358481,1.07798678628545,7.52783573083105));
#385810=CARTESIAN_POINT('Ctrl Pts',(2.52686377761628,1.07579572641885,7.50366116530176));
#385811=CARTESIAN_POINT('Origin',(8.44898126352695E-16,3.74011337523921E-16,
7.49482233047033));
#385812=CARTESIAN_POINT('Origin',(2.48717010277292,1.14363067896613,7.49482233047033));
#385813=CARTESIAN_POINT('Origin',(0.,0.,7.50366116523517));
#385814=CARTESIAN_POINT('Origin',(2.51873130274447,1.07233337846732,7.49482233047033));
#385815=CARTESIAN_POINT('Ctrl Pts',(2.48911633021126,1.15316718817924,7.51860402984325));
#385816=CARTESIAN_POINT('Ctrl Pts',(2.49375571485591,1.1591981413501,7.51860402984325));
#385817=CARTESIAN_POINT('Ctrl Pts',(2.49052926869772,1.16608917401715,7.51860402984325));
#385818=CARTESIAN_POINT('Ctrl Pts',(2.49083896438344,1.15540652302375,7.51041458714366));
#385819=CARTESIAN_POINT('Ctrl Pts',(2.49299132384047,1.1608307017199,7.5100464290044));
#385820=CARTESIAN_POINT('Ctrl Pts',(2.49052837888218,1.16609107448214,7.50729136483008));
#385821=CARTESIAN_POINT('Ctrl Pts',(2.4935252160709,1.15456522101444,7.50215815450138));
#385822=CARTESIAN_POINT('Ctrl Pts',(2.49454782737291,1.1575067054367,7.49877163671533));
#385823=CARTESIAN_POINT('Ctrl Pts',(2.49310646793173,1.16064141540027,7.49481588533172));
#385824=CARTESIAN_POINT('Ctrl Pts',(2.49520017266846,1.14732300152792,7.50366171572174));
#385825=CARTESIAN_POINT('Ctrl Pts',(2.49852704388164,1.1488527368606,7.50000045605858));
#385826=CARTESIAN_POINT('Ctrl Pts',(2.49852704388159,1.14885273686071,7.49482233047317));
#385827=CARTESIAN_POINT('Origin',(2.47920868111273,1.16078876868071,7.51860402984325));
#385828=CARTESIAN_POINT('Origin',(2.47920868111273,1.16078876868071,9.));
#385829=CARTESIAN_POINT('Origin',(2.47920868111273,1.16078876868071,8.75721825406948));
#385830=CARTESIAN_POINT('Ctrl Pts',(2.47893554146575,1.13993043652028,8.78942910404912));
#385831=CARTESIAN_POINT('Ctrl Pts',(2.48234884659823,1.14433518132267,8.7967269950169));
#385832=CARTESIAN_POINT('Ctrl Pts',(2.47641733384217,1.15100531193659,8.79893251111267));
#385833=CARTESIAN_POINT('Ctrl Pts',(2.48563834485609,1.14864524262545,8.78111911759584));
#385834=CARTESIAN_POINT('Ctrl Pts',(2.48967897368032,1.15387167820146,8.78644465894814));
#385835=CARTESIAN_POINT('Ctrl Pts',(2.48571656178288,1.16094379271768,8.78817647674132));
#385836=CARTESIAN_POINT('Ctrl Pts',(2.48981569178069,1.15407651767735,8.76780923932029));
#385837=CARTESIAN_POINT('Ctrl Pts',(2.49458145202819,1.16024922097768,8.76988516158373));
#385838=CARTESIAN_POINT('Ctrl Pts',(2.49151654159843,1.16715883055087,8.77093053738833));
#385839=CARTESIAN_POINT('Ctrl Pts',(2.48900116630002,1.15301749337551,8.75371302330492));
#385840=CARTESIAN_POINT('Ctrl Pts',(2.49365056324085,1.15903823331794,8.75300828287559));
#385841=CARTESIAN_POINT('Ctrl Pts',(2.49038497545739,1.16594695792981,8.75267964240738));
#385842=CARTESIAN_POINT('Origin',(2.47065968314843,1.14967358018058,8.78727029226991));
#385843=CARTESIAN_POINT('Ctrl Pts',(2.43698193351377,1.08538337893284,8.85049129520029));
#385844=CARTESIAN_POINT('Ctrl Pts',(2.44054210997314,1.09001222930861,8.85711686593484));
#385845=CARTESIAN_POINT('Ctrl Pts',(2.4351329425359,1.0966335335419,8.85933012996512));
#385846=CARTESIAN_POINT('Ctrl Pts',(2.45153175309122,1.10430068221462,8.82945683644724));
#385847=CARTESIAN_POINT('Ctrl Pts',(2.45512148116771,1.10896795484717,8.8360746990239));
#385848=CARTESIAN_POINT('Ctrl Pts',(2.44966738952773,1.11558497282205,8.83829567148519));
#385849=CARTESIAN_POINT('Ctrl Pts',(2.46605988498928,1.12318978773036,8.80838214965002));
#385850=CARTESIAN_POINT('Ctrl Pts',(2.46966377980879,1.12787547959984,8.81501364461992));
#385851=CARTESIAN_POINT('Ctrl Pts',(2.46418031900403,1.13450725690291,8.81722098428721));
#385852=CARTESIAN_POINT('Ctrl Pts',(2.4805679771315,1.1420528380681,8.78727029226991));
#385853=CARTESIAN_POINT('Ctrl Pts',(2.48417247056978,1.14673930824638,8.79393457792714));
#385854=CARTESIAN_POINT('Ctrl Pts',(2.47867338431573,1.15340260064194,8.79610912703474));
#385855=CARTESIAN_POINT('Origin',(2.4270736395307,1.09300412104532,8.85049129520029));
#385856=CARTESIAN_POINT('Ctrl Pts',(2.44187055726727,1.07433989271898,8.85049129520029));
#385857=CARTESIAN_POINT('Ctrl Pts',(2.44769070315532,1.07386343278904,8.85711686593484));
#385858=CARTESIAN_POINT('Ctrl Pts',(2.44895572090754,1.06540763642202,8.85933012996512));
#385859=CARTESIAN_POINT('Ctrl Pts',(2.43672155821481,1.07476140994123,8.86332496987232));
#385860=CARTESIAN_POINT('Ctrl Pts',(2.43884661045462,1.0706582346641,8.86648636486738));
#385861=CARTESIAN_POINT('Ctrl Pts',(2.43455258397725,1.06660392356302,8.87206031107457));
#385862=CARTESIAN_POINT('Ctrl Pts',(2.43381089401739,1.08126047448359,8.86341338519876));
#385863=CARTESIAN_POINT('Ctrl Pts',(2.43216978324604,1.08559409030303,8.86654584966059));
#385864=CARTESIAN_POINT('Ctrl Pts',(2.42626554159248,1.08508019996091,8.87215952290714));
#385865=CARTESIAN_POINT('Ctrl Pts',(2.43698193351377,1.08538337893284,8.85049129520029));
#385866=CARTESIAN_POINT('Ctrl Pts',(2.44054210997314,1.09001222930861,8.85711686593484));
#385867=CARTESIAN_POINT('Ctrl Pts',(2.4351329425359,1.0966335335419,8.85933012996512));
#385868=CARTESIAN_POINT('Origin',(2.44085067010873,1.06188156898808,8.85049129520029));
#385869=CARTESIAN_POINT('Ctrl Pts',(2.51312464689843,1.06850675396149,8.78727029226991));
#385870=CARTESIAN_POINT('Ctrl Pts',(2.51901724180285,1.0680243630714,8.79393457792714));
#385871=CARTESIAN_POINT('Ctrl Pts',(2.52025288996714,1.05947377310391,8.79610912703474));
#385872=CARTESIAN_POINT('Ctrl Pts',(2.48940694251246,1.07044837810417,8.80838214965001));
#385873=CARTESIAN_POINT('Ctrl Pts',(2.49529855880009,1.0699660673275,8.81501364461992));
#385874=CARTESIAN_POINT('Ctrl Pts',(2.4965213820383,1.06144823216102,8.81722098428721));
#385875=CARTESIAN_POINT('Ctrl Pts',(2.46565647730582,1.07239268417589,8.82945683644723));
#385876=CARTESIAN_POINT('Ctrl Pts',(2.47152493392368,1.07191226934046,8.8360746990239));
#385877=CARTESIAN_POINT('Ctrl Pts',(2.47275657607161,1.06342609822994,8.8382956714852));
#385878=CARTESIAN_POINT('Ctrl Pts',(2.44187055726727,1.07433989271898,8.85049129520029));
#385879=CARTESIAN_POINT('Ctrl Pts',(2.44769070315532,1.07386343278904,8.85711686593484));
#385880=CARTESIAN_POINT('Ctrl Pts',(2.44895572090754,1.06540763642202,8.85933012996512));
#385881=CARTESIAN_POINT('Origin',(2.51210475973989,1.05604843023059,8.78727029226991));
#385882=CARTESIAN_POINT('Ctrl Pts',(2.52691593003165,1.06737772701857,8.75374538247848));
#385883=CARTESIAN_POINT('Ctrl Pts',(2.53449062587208,1.06677079925315,8.75304829418602));
#385884=CARTESIAN_POINT('Ctrl Pts',(2.53741166984647,1.05971827167017,8.75272238421917));
#385885=CARTESIAN_POINT('Ctrl Pts',(2.52823151278633,1.06727002869138,8.76769408445018));
#385886=CARTESIAN_POINT('Ctrl Pts',(2.53599676646445,1.06664714002805,8.76974318093966));
#385887=CARTESIAN_POINT('Ctrl Pts',(2.53905110694683,1.05974139158941,8.7707786988043));
#385888=CARTESIAN_POINT('Ctrl Pts',(2.52148858502512,1.0678220289796,8.78108014887992));
#385889=CARTESIAN_POINT('Ctrl Pts',(2.52806966157637,1.06729794050742,8.78639403366329));
#385890=CARTESIAN_POINT('Ctrl Pts',(2.53065603659667,1.05962769018665,8.78812224174741));
#385891=CARTESIAN_POINT('Ctrl Pts',(2.51043841493815,1.06872663556165,8.78944554828686));
#385892=CARTESIAN_POINT('Ctrl Pts',(2.51598514662683,1.0682905332906,8.79673892988685));
#385893=CARTESIAN_POINT('Ctrl Pts',(2.51693670501844,1.05942497685325,8.79894799272499));
#385894=CARTESIAN_POINT('Origin',(2.52608058816213,1.05490431419655,8.75721825406948));
#385895=CARTESIAN_POINT('Origin',(2.52608058816213,1.05490431419655,9.));
#385896=CARTESIAN_POINT('Origin',(2.52608058816213,1.05490431419655,7.51860402984325));
#385897=CARTESIAN_POINT('Ctrl Pts',(2.52686305376087,1.07579541827706,7.50366195182966));
#385898=CARTESIAN_POINT('Ctrl Pts',(2.53023235892144,1.07722987791225,7.50000065167736));
#385899=CARTESIAN_POINT('Ctrl Pts',(2.53023235892149,1.07722987791214,7.49482233047108));
#385900=CARTESIAN_POINT('Ctrl Pts',(2.53110127804255,1.0696805793957,7.50215800491337));
#385901=CARTESIAN_POINT('Ctrl Pts',(2.53396674520192,1.06845837027569,7.49877273257265));
#385902=CARTESIAN_POINT('Ctrl Pts',(2.53531903262702,1.0652821342848,7.49481816995649));
#385903=CARTESIAN_POINT('Ctrl Pts',(2.52990969086322,1.06713300479696,7.51043025814042));
#385904=CARTESIAN_POINT('Ctrl Pts',(2.53537650996154,1.065081993843,7.51006209594516));
#385905=CARTESIAN_POINT('Ctrl Pts',(2.53761617838247,1.05971889254556,7.50731281821699));
#385906=CARTESIAN_POINT('Ctrl Pts',(2.52709896894495,1.06736276115358,7.51860402984326));
#385907=CARTESIAN_POINT('Ctrl Pts',(2.53468294567732,1.06674283025944,7.51860402984327));
#385908=CARTESIAN_POINT('Ctrl Pts',(2.53761520271995,1.05972122887324,7.51860402984327));
#385909=CARTESIAN_POINT('Origin',(0.,0.,7.5));
#385910=CARTESIAN_POINT('Origin',(2.50568666557813,0.915681362418256,7.5));
#385911=CARTESIAN_POINT('',(2.50568666557813,0.915681362418256,7.59394543036555));
#385912=CARTESIAN_POINT('',(2.50568666557813,0.915681362418256,8.85049129520029));
#385913=CARTESIAN_POINT('',(2.50568666557813,0.915681362418256,7.5));
#385914=CARTESIAN_POINT('',(2.57642062555679,0.905294943272749,8.78727029226991));
#385915=CARTESIAN_POINT('Ctrl Pts',(2.50568666557813,0.915681362418256,
8.85049129520029));
#385916=CARTESIAN_POINT('Ctrl Pts',(2.5292989251247,0.912214190147721,8.82945686509571));
#385917=CARTESIAN_POINT('Ctrl Pts',(2.55287608219231,0.908752172248009,
8.80838212259897));
#385918=CARTESIAN_POINT('Ctrl Pts',(2.5764206255568,0.905294943272749,8.78727029226991));
#385919=CARTESIAN_POINT('',(2.59029443537465,0.903257743546384,8.75721825406948));
#385920=CARTESIAN_POINT('Origin',(2.54854335809215,0.909388583893973,8.75937679713106));
#385921=CARTESIAN_POINT('',(2.59029443537465,0.903257743546384,7.51860402984325));
#385922=CARTESIAN_POINT('',(2.59029443537465,0.903257743546384,7.5));
#385923=CARTESIAN_POINT('Ctrl Pts',(2.59029443537465,0.903257743546384,
7.51860402984325));
#385924=CARTESIAN_POINT('Ctrl Pts',(2.5793987155483,0.904857647086956,7.52834476460825));
#385925=CARTESIAN_POINT('Ctrl Pts',(2.56849592237787,0.906458589261826,
7.53807742314407));
#385926=CARTESIAN_POINT('Ctrl Pts',(2.5575858183664,0.908060604944513,7.54780169004674));
#385927=CARTESIAN_POINT('Ctrl Pts',(2.54030480325306,0.910598111204327,
7.5632044032688));
#385928=CARTESIAN_POINT('Ctrl Pts',(2.52300542420908,0.913138313983315,
7.57858609112103));
#385929=CARTESIAN_POINT('Ctrl Pts',(2.50568666557813,0.915681362418256,
7.59394543036555));
#385930=CARTESIAN_POINT('Origin',(2.68279368784111,1.13380819535556,7.5));
#385931=CARTESIAN_POINT('',(2.55788654645047,0.991320447028643,8.75721825406948));
#385932=CARTESIAN_POINT('',(2.54864296074702,0.98077583205558,8.78727029226991));
#385933=CARTESIAN_POINT('Origin',(2.5251792925462,0.954009666308747,8.75658640621048));
#385934=CARTESIAN_POINT('',(2.50151564461751,0.927015373804568,8.85049129520029));
#385935=CARTESIAN_POINT('Ctrl Pts',(2.54864296074703,0.98077583205558,8.78727029226991));
#385936=CARTESIAN_POINT('Ctrl Pts',(2.53295613735133,0.962881097461795,
8.80838212259897));
#385937=CARTESIAN_POINT('Ctrl Pts',(2.51724758470003,0.9449615752324,8.82945686509571));
#385938=CARTESIAN_POINT('Ctrl Pts',(2.50151564461751,0.927015373804568,
8.85049129520029));
#385939=CARTESIAN_POINT('',(2.50151564461751,0.927015373804568,7.59394543036555));
#385940=CARTESIAN_POINT('',(2.50151564461751,0.927015373804568,7.5));
#385941=CARTESIAN_POINT('',(2.55788654645047,0.991320447028643,7.51860402984325));
#385942=CARTESIAN_POINT('Ctrl Pts',(2.50151564461751,0.927015373804568,
7.59394543036555));
#385943=CARTESIAN_POINT('Ctrl Pts',(2.51305446717485,0.940178278873355,
7.57858609112103));
#385944=CARTESIAN_POINT('Ctrl Pts',(2.52458037785886,0.953326454730193,
7.56320440326857));
#385945=CARTESIAN_POINT('Ctrl Pts',(2.53609405336255,0.966460673312278,
7.54780169004651));
#385946=CARTESIAN_POINT('Ctrl Pts',(2.54336303591222,0.974752760895097,
7.53807742314383));
#385947=CARTESIAN_POINT('Ctrl Pts',(2.55062714752992,0.983039291965133,
7.52834476460825));
#385948=CARTESIAN_POINT('Ctrl Pts',(2.55788654645047,0.991320447028641,
7.51860402984325));
#385949=CARTESIAN_POINT('',(2.55788654645047,0.991320447028643,7.5));
#385950=CARTESIAN_POINT('Origin',(2.50668546515629,0.922483422723978,7.5));
#385951=CARTESIAN_POINT('Ctrl Pts',(2.50151564461751,0.927015373804568,
8.85049129520029));
#385952=CARTESIAN_POINT('Ctrl Pts',(2.50138798433082,0.926869745407353,
8.85097269580138));
#385953=CARTESIAN_POINT('Ctrl Pts',(2.50126825987752,0.926720409638632,
8.85143669361005));
#385954=CARTESIAN_POINT('Ctrl Pts',(2.5011516404654,0.926559943194764,8.8519052845931));
#385955=CARTESIAN_POINT('Ctrl Pts',(2.50092354029102,0.92624608100697,8.85282181883899));
#385956=CARTESIAN_POINT('Ctrl Pts',(2.5007133460343,0.925897594557944,8.85372622499636));
#385957=CARTESIAN_POINT('Ctrl Pts',(2.50053096238414,0.925501051932918,
8.85462257735071));
#385958=CARTESIAN_POINT('Ctrl Pts',(2.50037955395543,0.925171856329486,
8.85536669723987));
#385959=CARTESIAN_POINT('Ctrl Pts',(2.5002472486102,0.924809479847003,8.85610498449051));
#385960=CARTESIAN_POINT('Ctrl Pts',(2.50014721912377,0.924403462300365,
8.85681338218371));
#385961=CARTESIAN_POINT('Ctrl Pts',(2.50005644220773,0.924035000739128,
8.85745625420284));
#385962=CARTESIAN_POINT('Ctrl Pts',(2.49999052655124,0.923626119378991,
8.85808743050666));
#385963=CARTESIAN_POINT('Ctrl Pts',(2.49997297445494,0.923160524417053,
8.8586680450841));
#385964=CARTESIAN_POINT('Ctrl Pts',(2.49996487629819,0.922945708994476,
8.85893592806395));
#385965=CARTESIAN_POINT('Ctrl Pts',(2.49996728752533,0.92271870761434,8.85919241173848));
#385966=CARTESIAN_POINT('Ctrl Pts',(2.49998401765522,0.922477377954862,
8.85943017985535));
#385967=CARTESIAN_POINT('Ctrl Pts',(2.50000660828322,0.922151511473342,
8.85975123720001));
#385968=CARTESIAN_POINT('Ctrl Pts',(2.500056520566,0.921791270397994,8.86004599534705));
#385969=CARTESIAN_POINT('Ctrl Pts',(2.50014347136777,0.921402412271963,
8.86026130871721));
#385970=CARTESIAN_POINT('Ctrl Pts',(2.50017530650771,0.921260040348952,
8.86034014101235));
#385971=CARTESIAN_POINT('Ctrl Pts',(2.50021257282626,0.921111691043425,
8.86040910639692));
#385972=CARTESIAN_POINT('Ctrl Pts',(2.50025458126596,0.920961488003178,
8.86046313645506));
#385973=CARTESIAN_POINT('Ctrl Pts',(2.50032013508429,0.920727097416814,
8.86054744990829));
#385974=CARTESIAN_POINT('Ctrl Pts',(2.50039916763199,0.92048183418458,8.86059655985669));
#385975=CARTESIAN_POINT('Ctrl Pts',(2.50048633147295,0.920241337932643,
8.86059725258816));
#385976=CARTESIAN_POINT('Ctrl Pts',(2.50057369669721,0.920000286038284,
8.86059794692011));
#385977=CARTESIAN_POINT('Ctrl Pts',(2.50067269750015,0.919762255163163,
8.86056369958366));
#385978=CARTESIAN_POINT('Ctrl Pts',(2.50077445977492,0.919538782504412,
8.86048590497774));
#385979=CARTESIAN_POINT('Ctrl Pts',(2.50080101669881,0.91948046279406,8.86046560290182));
#385980=CARTESIAN_POINT('Ctrl Pts',(2.5008281896189,0.919422413409564,8.86044257503091));
#385981=CARTESIAN_POINT('Ctrl Pts',(2.5008551091393,0.919366414208263,8.86041778462584));
#385982=CARTESIAN_POINT('Ctrl Pts',(2.50103624410722,0.918989609072723,
8.86025097596201));
#385983=CARTESIAN_POINT('Ctrl Pts',(2.50123051112959,0.918655209975485,
8.85998489822951));
#385984=CARTESIAN_POINT('Ctrl Pts',(2.50142491409744,0.918368721174964,
8.85968173251462));
#385985=CARTESIAN_POINT('Ctrl Pts',(2.50152774212946,0.918217185013339,
8.85952137522077));
#385986=CARTESIAN_POINT('Ctrl Pts',(2.50163243226652,0.91807602501943,8.85934740853961));
#385987=CARTESIAN_POINT('Ctrl Pts',(2.50173625951288,0.917946305822599,
8.8591675900182));
#385988=CARTESIAN_POINT('Ctrl Pts',(2.5021531798753,0.917425415820627,8.85844552518695));
#385989=CARTESIAN_POINT('Ctrl Pts',(2.50257738764837,0.917057671454099,
8.85759444184125));
#385990=CARTESIAN_POINT('Ctrl Pts',(2.5029501956441,0.91678889933161,8.85683498915139));
#385991=CARTESIAN_POINT('Ctrl Pts',(2.50298920900799,0.916760773044789,
8.85675551444998));
#385992=CARTESIAN_POINT('Ctrl Pts',(2.50302766777014,0.91673374878028,8.85667699793651));
#385993=CARTESIAN_POINT('Ctrl Pts',(2.50306550949756,0.916707776672099,
8.85659965593547));
#385994=CARTESIAN_POINT('Ctrl Pts',(2.50357629906516,0.916357203830595,
8.85555568965886));
#385995=CARTESIAN_POINT('Ctrl Pts',(2.50411782914084,0.916094049730749,
8.85434650606346));
#385996=CARTESIAN_POINT('Ctrl Pts',(2.50469006045449,0.915911423788039,
8.85297329937117));
#385997=CARTESIAN_POINT('Ctrl Pts',(2.50501190570186,0.915808707822827,
8.85220095427747));
#385998=CARTESIAN_POINT('Ctrl Pts',(2.50534369019835,0.91573172416885,8.85137579139183));
#385999=CARTESIAN_POINT('Ctrl Pts',(2.50568666557813,0.915681362418256,
8.85049129520029));
#386000=CARTESIAN_POINT('Origin',(2.50668546515629,0.922483422723978,7.59394543036555));
#386001=CARTESIAN_POINT('Ctrl Pts',(2.50114500373946,0.926592565440176,
7.59443877723642));
#386002=CARTESIAN_POINT('Ctrl Pts',(2.49732775931655,0.922238046102233,
7.58783886950016));
#386003=CARTESIAN_POINT('Ctrl Pts',(2.50224377712737,0.91531620021978,7.58559994247159));
#386004=CARTESIAN_POINT('Ctrl Pts',(2.52198322905087,0.950363758749822,
7.56670252222133));
#386005=CARTESIAN_POINT('Ctrl Pts',(2.51817150162988,0.946015532928613,
7.56004874999025));
#386006=CARTESIAN_POINT('Ctrl Pts',(2.5230992292225,0.939040301174041,7.55786368756704));
#386007=CARTESIAN_POINT('Ctrl Pts',(2.54278254105854,0.974090561731036,
7.53888913333559));
#386008=CARTESIAN_POINT('Ctrl Pts',(2.53894816035486,0.969716494190849,
7.53222002137277));
#386009=CARTESIAN_POINT('Ctrl Pts',(2.54391559872046,0.96272171036261,7.53005029815327));
#386010=CARTESIAN_POINT('Ctrl Pts',(2.56354199857947,0.997771900729855,
7.51101258149734));
#386011=CARTESIAN_POINT('Ctrl Pts',(2.55966113821443,0.99334481154321,7.5043616886572));
#386012=CARTESIAN_POINT('Ctrl Pts',(2.5646919192062,0.986359203183337,7.50217374673251));
#386013=CARTESIAN_POINT('',(2.56358326728469,0.98509787688097,7.50366116523517));
#386014=CARTESIAN_POINT('Ctrl Pts',(2.55788654645047,0.991320447028644,
7.51860402984325));
#386015=CARTESIAN_POINT('Ctrl Pts',(2.55817765342151,0.99165252713523,7.51734760759493));
#386016=CARTESIAN_POINT('Ctrl Pts',(2.55848545024178,0.991913389124431,
7.51608817408572));
#386017=CARTESIAN_POINT('Ctrl Pts',(2.5588178627193,0.992092245848213,7.51481005913119));
#386018=CARTESIAN_POINT('Ctrl Pts',(2.5591189698847,0.992254258542534,7.51365231206383));
#386019=CARTESIAN_POINT('Ctrl Pts',(2.55944058051348,0.992349433202007,
7.51247773061042));
#386020=CARTESIAN_POINT('Ctrl Pts',(2.55978760768028,0.992340715789489,
7.51129758471022));
#386021=CARTESIAN_POINT('Ctrl Pts',(2.5602189228166,0.992329881041294,7.50983079813402));
#386022=CARTESIAN_POINT('Ctrl Pts',(2.56067540818268,0.992145882723034,
7.50839324291155));
#386023=CARTESIAN_POINT('Ctrl Pts',(2.56112957542531,0.991710916073226,
7.50715379678855));
#386024=CARTESIAN_POINT('Ctrl Pts',(2.5613393876049,0.991509974014278,7.50658120839351));
#386025=CARTESIAN_POINT('Ctrl Pts',(2.56157195964613,0.991220042996603,
7.50598221009429));
#386026=CARTESIAN_POINT('Ctrl Pts',(2.56180401337726,0.990833789954918,
7.50545747549612));
#386027=CARTESIAN_POINT('Ctrl Pts',(2.56192784443093,0.990627673376225,
7.50517746087247));
#386028=CARTESIAN_POINT('Ctrl Pts',(2.56205304424277,0.990391997191143,
7.50491486231392));
#386029=CARTESIAN_POINT('Ctrl Pts',(2.56217482425125,0.990132219959011,
7.50468370960992));
#386030=CARTESIAN_POINT('Ctrl Pts',(2.56235692377725,0.989743771054887,
7.50433806340446));
#386031=CARTESIAN_POINT('Ctrl Pts',(2.56253633316337,0.989289548577592,
7.50405484070983));
#386032=CARTESIAN_POINT('Ctrl Pts',(2.56270030321808,0.988799880389195,
7.5038576603613));
#386033=CARTESIAN_POINT('Ctrl Pts',(2.56271783726676,0.988747517987619,
7.50383657498791));
#386034=CARTESIAN_POINT('Ctrl Pts',(2.56273520068951,0.988694778002053,
7.50381643264937));
#386035=CARTESIAN_POINT('Ctrl Pts',(2.56275238251344,0.988641717600799,
7.50379723213559));
#386036=CARTESIAN_POINT('Ctrl Pts',(2.56286707680879,0.988287522065131,
7.50366906242519));
#386037=CARTESIAN_POINT('Ctrl Pts',(2.56297548985005,0.987911122718402,
7.50358235568538));
#386038=CARTESIAN_POINT('Ctrl Pts',(2.5630712656504,0.987545808184195,7.5035341175365));
#386039=CARTESIAN_POINT('Ctrl Pts',(2.56321487062329,0.986998060385773,
7.50346178989177));
#386040=CARTESIAN_POINT('Ctrl Pts',(2.56334606729218,0.986402702482696,
7.50346967198527));
#386041=CARTESIAN_POINT('Ctrl Pts',(2.56345687801436,0.985814282467652,
7.50354272648693));
#386042=CARTESIAN_POINT('Ctrl Pts',(2.56350245675804,0.985572253135891,
7.50357277531559));
#386043=CARTESIAN_POINT('Ctrl Pts',(2.56354466529948,0.985331745408197,
7.50361331098761));
#386044=CARTESIAN_POINT('Ctrl Pts',(2.56358326728602,0.985097876881478,
7.50366116523659));
#386045=CARTESIAN_POINT('',(2.50943323048235,0.923494625763825,7.57603338622103));
#386046=CARTESIAN_POINT('Origin',(2.51772740356821,0.926543917882798,7.58486873427629));
#386047=CARTESIAN_POINT('Ctrl Pts',(2.56358326731836,0.985097876927392,
7.50366116529969));
#386048=CARTESIAN_POINT('Ctrl Pts',(2.54556333673348,0.964596415991244,
7.5278357307971));
#386049=CARTESIAN_POINT('Ctrl Pts',(2.52751419016024,0.944062956655914,
7.55196141284068));
#386050=CARTESIAN_POINT('Ctrl Pts',(2.50943323100971,0.923494626899403,
7.57603338728831));
#386051=CARTESIAN_POINT('Ctrl Pts',(2.50232577352107,0.927672813292166,
7.59639677331371));
#386052=CARTESIAN_POINT('Ctrl Pts',(2.48825599434034,0.916006055835398,
7.59959882295466));
#386053=CARTESIAN_POINT('Ctrl Pts',(2.50654858601383,0.915706218428471,
7.59642833564546));
#386054=CARTESIAN_POINT('Ctrl Pts',(2.49896195408414,0.925698016371091,
7.58707626057422));
#386055=CARTESIAN_POINT('Ctrl Pts',(2.49729432017831,0.919130574845469,
7.58809943920598));
#386056=CARTESIAN_POINT('Ctrl Pts',(2.50274613781078,0.915131564305941,
7.58710240504253));
#386057=CARTESIAN_POINT('Ctrl Pts',(2.50482266671419,0.924092500961746,
7.5801537675693));
#386058=CARTESIAN_POINT('Ctrl Pts',(2.50376748561201,0.921443753288322,
7.58205880659761));
#386059=CARTESIAN_POINT('Ctrl Pts',(2.50623637659076,0.920090367765581,
7.58020924244128));
#386060=CARTESIAN_POINT('Ctrl Pts',(2.50943322970563,0.923494625478202,
7.57603338509286));
#386061=CARTESIAN_POINT('Ctrl Pts',(2.50943322970563,0.923494625478202,
7.57603338509286));
#386062=CARTESIAN_POINT('Ctrl Pts',(2.50943322970563,0.923494625478202,
7.57603338509286));
#386063=CARTESIAN_POINT('Origin',(2.51772543279328,0.926549273113992,7.58486873427622));
#386064=CARTESIAN_POINT('Ctrl Pts',(2.5988096000392,0.902007395491139,7.51098857897448));
#386065=CARTESIAN_POINT('Ctrl Pts',(2.5929847431161,0.902862704673379,7.50433767179956));
#386066=CARTESIAN_POINT('Ctrl Pts',(2.59228715441969,0.911442997272883,
7.50214974420965));
#386067=CARTESIAN_POINT('Ctrl Pts',(2.56764251675708,0.90658390146661,7.53887321589171));
#386068=CARTESIAN_POINT('Ctrl Pts',(2.56188745195716,0.907428962526944,
7.53220407452065));
#386069=CARTESIAN_POINT('Ctrl Pts',(2.56113565724649,0.915975173654399,
7.53003438070911));
#386070=CARTESIAN_POINT('Ctrl Pts',(2.53641558117792,0.911169196021767,
7.56669465659233));
#386071=CARTESIAN_POINT('Ctrl Pts',(2.53069452774099,0.912009262928332,
7.56004085833297));
#386072=CARTESIAN_POINT('Ctrl Pts',(2.52992516332406,0.920514833368955,
7.55785582193789));
#386073=CARTESIAN_POINT('Ctrl Pts',(2.50513020557114,0.915763071782075,
7.59443891967696));
#386074=CARTESIAN_POINT('Ctrl Pts',(2.49940085731905,0.91660435668108,7.58783901202978));
#386075=CARTESIAN_POINT('Ctrl Pts',(2.49865720208422,0.925061670372792,
7.58560008491213));
#386076=CARTESIAN_POINT('',(2.59059853376831,0.911688670640886,7.50366116523517));
#386077=CARTESIAN_POINT('Ctrl Pts',(2.59059853376866,0.91168867064101,7.50366116523554));
#386078=CARTESIAN_POINT('Ctrl Pts',(2.59098904347061,0.911039332755585,
7.50350835821027));
#386079=CARTESIAN_POINT('Ctrl Pts',(2.59132689113599,0.910429728813554,
7.50345484956));
#386080=CARTESIAN_POINT('Ctrl Pts',(2.5916226464834,0.909842025882762,7.50349758195598));
#386081=CARTESIAN_POINT('Ctrl Pts',(2.59177439091041,0.909540490694081,
7.50351950684424));
#386082=CARTESIAN_POINT('Ctrl Pts',(2.59193012691096,0.909215058506864,
7.50357029184312));
#386083=CARTESIAN_POINT('Ctrl Pts',(2.5920716753196,0.908897119992529,7.50365515313924));
#386084=CARTESIAN_POINT('Ctrl Pts',(2.5922894340907,0.908408001811463,7.50378570417639));
#386085=CARTESIAN_POINT('Ctrl Pts',(2.59248032444165,0.907922402436793,
7.50400001621911));
#386086=CARTESIAN_POINT('Ctrl Pts',(2.59262770382891,0.907476452400882,
7.50428903009635));
#386087=CARTESIAN_POINT('Ctrl Pts',(2.59264406180703,0.907426955377829,
7.50432110841318));
#386088=CARTESIAN_POINT('Ctrl Pts',(2.59265990793161,0.907377928509123,
7.50435406373355));
#386089=CARTESIAN_POINT('Ctrl Pts',(2.59267523710345,0.907329407449752,
7.50438785222352));
#386090=CARTESIAN_POINT('Ctrl Pts',(2.59276882906568,0.907033163060106,
7.50459414719562));
#386091=CARTESIAN_POINT('Ctrl Pts',(2.59284414892436,0.90675090178871,7.50483629897752));
#386092=CARTESIAN_POINT('Ctrl Pts',(2.59289958273718,0.906493776284968,
7.5050991045531));
#386093=CARTESIAN_POINT('Ctrl Pts',(2.59302187529608,0.905926531597902,
7.50567888004914));
#386094=CARTESIAN_POINT('Ctrl Pts',(2.593052712494,0.905459376620307,7.50637912803144));
#386095=CARTESIAN_POINT('Ctrl Pts',(2.59302239896678,0.905086224694295,
7.50710440483569));
#386096=CARTESIAN_POINT('Ctrl Pts',(2.59301496548809,0.904994720433934,
7.50728225710685));
#386097=CARTESIAN_POINT('Ctrl Pts',(2.59300385233831,0.904907035449151,
7.50746498566954));
#386098=CARTESIAN_POINT('Ctrl Pts',(2.59298973222145,0.904825164211477,
7.50764697238949));
#386099=CARTESIAN_POINT('Ctrl Pts',(2.59291382635912,0.904385046969313,
7.50862528291182));
#386100=CARTESIAN_POINT('Ctrl Pts',(2.59274821214765,0.904072281556945,
7.50965856837421));
#386101=CARTESIAN_POINT('Ctrl Pts',(2.5925409885644,0.903841240304918,7.51067959873202));
#386102=CARTESIAN_POINT('Ctrl Pts',(2.59242695316516,0.903714098012506,
7.51124147302578));
#386103=CARTESIAN_POINT('Ctrl Pts',(2.59229996591968,0.903611963391194,
7.51180065547253));
#386104=CARTESIAN_POINT('Ctrl Pts',(2.59216608810208,0.9035291187079,7.51235175716501));
#386105=CARTESIAN_POINT('Ctrl Pts',(2.59170348691166,0.903242857325715,
7.51425603304536));
#386106=CARTESIAN_POINT('Ctrl Pts',(2.59110026610329,0.903157939223945,
7.5162690050518));
#386107=CARTESIAN_POINT('Ctrl Pts',(2.590407685676,0.903242504084119,7.51827788969243));
#386108=CARTESIAN_POINT('Ctrl Pts',(2.59037020191448,0.903247080894157,
7.51838661432545));
#386109=CARTESIAN_POINT('Ctrl Pts',(2.59033244978269,0.903252161594292,
7.51849533314856));
#386110=CARTESIAN_POINT('Ctrl Pts',(2.59029443537465,0.90325774354638,7.51860402984325));
#386111=CARTESIAN_POINT('Ctrl Pts',(2.50943323162122,0.923494625241175,
7.57603338728985));
#386112=CARTESIAN_POINT('Ctrl Pts',(2.53653388028815,0.91955354481261,7.55196141284922));
#386113=CARTESIAN_POINT('Ctrl Pts',(2.56358770141575,0.915618394507179,
7.52783573083105));
#386114=CARTESIAN_POINT('Ctrl Pts',(2.59059853382585,0.911688670627024,
7.50366116530176));
#386115=CARTESIAN_POINT('Origin',(8.67125181207502E-16,3.19110082301679E-16,
7.49482233047033));
#386116=CARTESIAN_POINT('Origin',(2.55533261422667,0.981927431468074,7.49482233047033));
#386117=CARTESIAN_POINT('Origin',(0.,0.,7.50366116523517));
#386118=CARTESIAN_POINT('Origin',(2.58226093460096,0.908754485894723,7.49482233047033));
#386119=CARTESIAN_POINT('Ctrl Pts',(2.55788584917514,0.99131965168011,7.51860402984325));
#386120=CARTESIAN_POINT('Ctrl Pts',(2.56290210620281,0.997040967216104,
7.51860402984325));
#386121=CARTESIAN_POINT('Ctrl Pts',(2.56012379910316,1.00412456063259,7.51860402984325));
#386122=CARTESIAN_POINT('Ctrl Pts',(2.55974841868675,0.993444016020654,
7.51041458714366));
#386123=CARTESIAN_POINT('Ctrl Pts',(2.56224388421272,0.998719148016046,
7.51004642900443));
#386124=CARTESIAN_POINT('Ctrl Pts',(2.56012303287905,1.00412651420355,7.5072913648301));
#386125=CARTESIAN_POINT('Ctrl Pts',(2.56237524877722,0.992432333820012,
7.50215815450138));
#386126=CARTESIAN_POINT('Ctrl Pts',(2.56358422056863,0.99530225571599,7.49877163671529));
#386127=CARTESIAN_POINT('Ctrl Pts',(2.56234666411195,0.998522873298203,
7.4948158853317));
#386128=CARTESIAN_POINT('Ctrl Pts',(2.56358275340116,0.985097679412492,
7.50366171572174));
#386129=CARTESIAN_POINT('Ctrl Pts',(2.5670007996799,0.986411118369394,7.50000045605858));
#386130=CARTESIAN_POINT('Ctrl Pts',(2.56700079967986,0.986411118369511,
7.49482233047317));
#386131=CARTESIAN_POINT('Origin',(2.5484868727436,0.999560358084262,7.51860402984325));
#386132=CARTESIAN_POINT('Origin',(2.5484868727436,0.999560358084262,9.));
#386133=CARTESIAN_POINT('Origin',(2.5484868727436,0.999560358084262,8.75721825406948));
#386134=CARTESIAN_POINT('Ctrl Pts',(2.54687789636137,0.97876238172157,8.78942910404913));
#386135=CARTESIAN_POINT('Ctrl Pts',(2.55056640146082,0.982939385292657,
8.79672699501689));
#386136=CARTESIAN_POINT('Ctrl Pts',(2.54507443236962,0.989975844734957,
8.79893251111266));
#386137=CARTESIAN_POINT('Ctrl Pts',(2.55412528766752,0.987029832235237,
8.78111911759583));
#386138=CARTESIAN_POINT('Ctrl Pts',(2.55849247346355,0.991986645561208,
8.78644465894816));
#386139=CARTESIAN_POINT('Ctrl Pts',(2.55499131469909,0.999298102261577,
8.78817647674132));
#386140=CARTESIAN_POINT('Ctrl Pts',(2.55864203477219,0.992182304613644,
8.7678092393203));
#386141=CARTESIAN_POINT('Ctrl Pts',(2.56379348971243,0.998036982125591,
8.76988516158372));
#386142=CARTESIAN_POINT('Ctrl Pts',(2.56117757667523,1.00512876465032,8.77093053738832));
#386143=CARTESIAN_POINT('Ctrl Pts',(2.5577613309015,0.991177643017536,8.75371302330492));
#386144=CARTESIAN_POINT('Ctrl Pts',(2.56278692529023,0.996888124819248,
8.75300828287559));
#386145=CARTESIAN_POINT('Ctrl Pts',(2.55997069051277,1.0039918816431,8.75267964240738));
#386146=CARTESIAN_POINT('Origin',(2.53924328704016,0.989015743111198,8.78727029226991));
#386147=CARTESIAN_POINT('Ctrl Pts',(2.50151564461751,0.927015373804568,
8.85049129520029));
#386148=CARTESIAN_POINT('Ctrl Pts',(2.50536507777435,0.931406612421877,
8.85711686593484));
#386149=CARTESIAN_POINT('Ctrl Pts',(2.50039125247053,0.938360879023106,
8.85933012996512));
#386150=CARTESIAN_POINT('Ctrl Pts',(2.51724760581287,0.94496159931686,8.82945683644722));
#386151=CARTESIAN_POINT('Ctrl Pts',(2.52112899159229,0.94938928786971,8.83607469902387));
#386152=CARTESIAN_POINT('Ctrl Pts',(2.51611005976582,0.956342155322669,
8.8382956714852));
#386153=CARTESIAN_POINT('Ctrl Pts',(2.53295611725146,0.96288107453287,8.80838214965003));
#386154=CARTESIAN_POINT('Ctrl Pts',(2.53685282079135,0.967326236811966,
8.81501364461989));
#386155=CARTESIAN_POINT('Ctrl Pts',(2.5318055257756,0.974295714957373,8.81722098428721));
#386156=CARTESIAN_POINT('Ctrl Pts',(2.54864296074703,0.98077583205558,8.78727029226991));
#386157=CARTESIAN_POINT('Ctrl Pts',(2.5525403115422,0.985221732690743,8.79393457792714));
#386158=CARTESIAN_POINT('Ctrl Pts',(2.54747944236022,0.992223662303431,
8.79610912703474));
#386159=CARTESIAN_POINT('Origin',(2.49211597091065,0.935255284860186,8.85049129520029));
#386160=CARTESIAN_POINT('Ctrl Pts',(2.50568666557813,0.915681362418256,
8.85049129520029));
#386161=CARTESIAN_POINT('Ctrl Pts',(2.51146432645972,0.914832983398971,
8.85711686593484));
#386162=CARTESIAN_POINT('Ctrl Pts',(2.51218498036395,0.906313510406806,
8.85933012996512));
#386163=CARTESIAN_POINT('Ctrl Pts',(2.50057525239759,0.916431911090139,
8.86332496987232));
#386164=CARTESIAN_POINT('Ctrl Pts',(2.50243304714704,0.912201013662211,
8.86648636486736));
#386165=CARTESIAN_POINT('Ctrl Pts',(2.4978880826035,0.908430151799111,8.87206031107457));
#386166=CARTESIAN_POINT('Ctrl Pts',(2.49808696496685,0.923104109502799,
8.86341338519875));
#386167=CARTESIAN_POINT('Ctrl Pts',(2.49672688175244,0.927533967771879,
8.86654584966058));
#386168=CARTESIAN_POINT('Ctrl Pts',(2.49080184592933,0.927399419334149,
8.87215952290715));
#386169=CARTESIAN_POINT('Ctrl Pts',(2.50151564461751,0.927015373804567,
8.85049129520029));
#386170=CARTESIAN_POINT('Ctrl Pts',(2.50536507777435,0.931406612421877,
8.85711686593484));
#386171=CARTESIAN_POINT('Ctrl Pts',(2.50039125247053,0.938360879023106,
8.85933012996512));
#386172=CARTESIAN_POINT('Origin',(2.50387066634511,0.903313980044218,8.85049129520029));
#386173=CARTESIAN_POINT('Ctrl Pts',(2.5764206255568,0.905294943272749,8.78727029226991));
#386174=CARTESIAN_POINT('Ctrl Pts',(2.58227020660256,0.904436003654703,
8.79393457792714));
#386175=CARTESIAN_POINT('Ctrl Pts',(2.58295547781499,0.895823813541636,
8.79610912703474));
#386176=CARTESIAN_POINT('Ctrl Pts',(2.55287605202415,0.908752176677835,
8.80838214965003));
#386177=CARTESIAN_POINT('Ctrl Pts',(2.55872466159671,0.907893379708777,
8.81501364461997));
#386178=CARTESIAN_POINT('Ctrl Pts',(2.55939923284052,0.899314698794315,
8.81722098428721));
#386179=CARTESIAN_POINT('Ctrl Pts',(2.52929895681322,0.912214185494648,
8.82945683644722));
#386180=CARTESIAN_POINT('Ctrl Pts',(2.53512457577336,0.911358764416574,
8.83607469902387));
#386181=CARTESIAN_POINT('Ctrl Pts',(2.53580997653059,0.902811117471385,
8.83829567148519));
#386182=CARTESIAN_POINT('Ctrl Pts',(2.50568666557813,0.915681362418256,
8.85049129520029));
#386183=CARTESIAN_POINT('Ctrl Pts',(2.51146432645972,0.914832983398971,
8.85711686593484));
#386184=CARTESIAN_POINT('Ctrl Pts',(2.51218498036395,0.906313510406806,
8.85933012996512));
#386185=CARTESIAN_POINT('Origin',(2.57460462632378,0.892927560898711,8.78727029226991));
#386186=CARTESIAN_POINT('Ctrl Pts',(2.59011123601511,0.903284625492616,
8.75374538247848));
#386187=CARTESIAN_POINT('Ctrl Pts',(2.59763148283512,0.902193632296599,
8.75304829418601));
#386188=CARTESIAN_POINT('Ctrl Pts',(2.60009466821772,0.894968442957906,
8.75272238421917));
#386189=CARTESIAN_POINT('Ctrl Pts',(2.5914172155084,0.903092858766698,8.76769408445019));
#386190=CARTESIAN_POINT('Ctrl Pts',(2.59912660602631,0.901973728383564,
8.7697431809397));
#386191=CARTESIAN_POINT('Ctrl Pts',(2.60173221821703,0.894886476279139,
8.7707786988043));
#386192=CARTESIAN_POINT('Ctrl Pts',(2.58472350859536,0.904075745776096,
8.78108014887991));
#386193=CARTESIAN_POINT('Ctrl Pts',(2.59125748515533,0.903131083077539,
8.78639403366325));
#386194=CARTESIAN_POINT('Ctrl Pts',(2.59334711156538,0.895310882492175,
8.78812224174741));
#386195=CARTESIAN_POINT('Ctrl Pts',(2.57375400061066,0.905686480575195,
8.78944554828685));
#386196=CARTESIAN_POINT('Ctrl Pts',(2.57926139477576,0.904895894003568,
8.79673892988685));
#386197=CARTESIAN_POINT('Ctrl Pts',(2.57964297993741,0.895987586247271,
8.79894799272499));
#386198=CARTESIAN_POINT('Origin',(2.58847843614163,0.890890361172345,8.75721825406948));
#386199=CARTESIAN_POINT('Origin',(2.58847843614163,0.890890361172345,9.));
#386200=CARTESIAN_POINT('Origin',(2.58847843614163,0.890890361172345,7.51860402984325));
#386201=CARTESIAN_POINT('Ctrl Pts',(2.59059779171497,0.911688409495914,
7.50366195182966));
#386202=CARTESIAN_POINT('Ctrl Pts',(2.5940520804211,0.912904049757124,7.50000065167735));
#386203=CARTESIAN_POINT('Ctrl Pts',(2.59405208042114,0.912904049757014,
7.49482233047108));
#386204=CARTESIAN_POINT('Ctrl Pts',(2.59443552903803,0.905314590244799,
7.50215800491337));
#386205=CARTESIAN_POINT('Ctrl Pts',(2.5972168015806,0.903911301173251,7.49877273257264));
#386206=CARTESIAN_POINT('Ctrl Pts',(2.59836280844753,0.900654949747057,
7.49481816995649));
#386207=CARTESIAN_POINT('Ctrl Pts',(2.59308316643741,0.902848595164,7.51043025814043));
#386208=CARTESIAN_POINT('Ctrl Pts',(2.59840734464655,0.900451537929794,
7.51006209594516));
#386209=CARTESIAN_POINT('Ctrl Pts',(2.60029879634861,0.894955959650746,
7.50731281821699));
#386210=CARTESIAN_POINT('Ctrl Pts',(2.59029293998907,0.903257963033155,
7.51860402984326));
#386211=CARTESIAN_POINT('Ctrl Pts',(2.59782161551911,0.902153398795956,
7.51860402984326));
#386212=CARTESIAN_POINT('Ctrl Pts',(2.60029797237972,0.894958353689109,
7.51860402984327));
#386213=CARTESIAN_POINT('Origin',(0.,0.,7.5));
#386214=CARTESIAN_POINT('Origin',(2.55920636991202,0.753260100986319,7.5));
#386215=CARTESIAN_POINT('',(2.55920636991202,0.753260100986319,7.59394543036555));
#386216=CARTESIAN_POINT('',(2.55920636991202,0.753260100986319,8.85049129520029));
#386217=CARTESIAN_POINT('',(2.55920636991202,0.753260100986319,7.5));
#386218=CARTESIAN_POINT('',(2.62912953922426,0.738363081476946,8.78727029226991));
#386219=CARTESIAN_POINT('Ctrl Pts',(2.55920636991202,0.753260100986318,
8.85049129520029));
#386220=CARTESIAN_POINT('Ctrl Pts',(2.58254797304886,0.748287209729676,
8.82945686509571));
#386221=CARTESIAN_POINT('Ctrl Pts',(2.60585487607021,0.7433217112772,8.80838212259895));
#386222=CARTESIAN_POINT('Ctrl Pts',(2.62912953922426,0.738363081476946,
8.78727029226991));
#386223=CARTESIAN_POINT('',(2.64284431997726,0.735441169348907,8.75721825406948));
#386224=CARTESIAN_POINT('Origin',(2.60157182905073,0.744234413933357,8.75937679713113));
#386225=CARTESIAN_POINT('',(2.64284431997726,0.735441169348907,7.51860402984325));
#386226=CARTESIAN_POINT('',(2.64284431997726,0.735441169348907,7.5));
#386227=CARTESIAN_POINT('Ctrl Pts',(2.64284431997726,0.735441169348907,
7.51860402984325));
#386228=CARTESIAN_POINT('Ctrl Pts',(2.63207349274765,0.737735876882188,
7.52834476460825));
#386229=CARTESIAN_POINT('Ctrl Pts',(2.62129567325243,0.740032074106494,
7.53807742314407));
#386230=CARTESIAN_POINT('Ctrl Pts',(2.61051062671697,0.742329811040171,
7.54780169004674));
#386231=CARTESIAN_POINT('Ctrl Pts',(2.59342769588682,0.74596930216103,7.5632044032688));
#386232=CARTESIAN_POINT('Ctrl Pts',(2.57632661162329,0.74961266084185,7.57858609112103));
#386233=CARTESIAN_POINT('Ctrl Pts',(2.55920636991202,0.753260100986319,
7.59394543036555));
#386234=CARTESIAN_POINT('Origin',(2.74992494097309,0.959591483074807,7.5));
#386235=CARTESIAN_POINT('',(2.61614521332082,0.825399319134649,8.75721825406948));
#386236=CARTESIAN_POINT('',(2.60624502375464,0.815468607773385,8.78727029226991));
#386237=CARTESIAN_POINT('Origin',(2.58111465004893,0.790260758367688,8.75658640621043));
#386238=CARTESIAN_POINT('',(2.5557700913641,0.764838063661159,8.85049129520029));
#386239=CARTESIAN_POINT('Ctrl Pts',(2.60624502375464,0.815468607773385,
8.78727029226991));
#386240=CARTESIAN_POINT('Ctrl Pts',(2.58944391103809,0.798615698056782,
8.80838212259896));
#386241=CARTESIAN_POINT('Ctrl Pts',(2.57261952556176,0.781739443831623,
8.82945686509571));
#386242=CARTESIAN_POINT('Ctrl Pts',(2.5557700913641,0.764838063661159,8.85049129520029));
#386243=CARTESIAN_POINT('',(2.5557700913641,0.764838063661159,7.59394543036555));
#386244=CARTESIAN_POINT('',(2.5557700913641,0.764838063661159,7.5));
#386245=CARTESIAN_POINT('',(2.61614521332082,0.825399319134649,7.51860402984325));
#386246=CARTESIAN_POINT('Ctrl Pts',(2.5557700913641,0.764838063661158,7.59394543036555));
#386247=CARTESIAN_POINT('Ctrl Pts',(2.56812855639629,0.777234629230197,
7.57858609112103));
#386248=CARTESIAN_POINT('Ctrl Pts',(2.58047319238015,0.789617323116598,
7.56320440326857));
#386249=CARTESIAN_POINT('Ctrl Pts',(2.59280472407651,0.801986872315658,
7.54780169004651));
#386250=CARTESIAN_POINT('Ctrl Pts',(2.60059004759746,0.80979619760422,7.53807742314383));
#386251=CARTESIAN_POINT('Ctrl Pts',(2.60837015418731,0.817600289878136,
7.52834476460825));
#386252=CARTESIAN_POINT('Ctrl Pts',(2.61614521332082,0.825399319134647,
7.51860402984325));
#386253=CARTESIAN_POINT('',(2.61614521332082,0.825399319134649,7.5));
#386254=CARTESIAN_POINT('Origin',(2.56063892684944,0.759984192420934,7.5));
#386255=CARTESIAN_POINT('Ctrl Pts',(2.5557700913641,0.764838063661158,8.85049129520029));
#386256=CARTESIAN_POINT('Ctrl Pts',(2.55563336292571,0.764700913695755,
8.85097269580138));
#386257=CARTESIAN_POINT('Ctrl Pts',(2.55550431648359,0.764559555525447,
8.85143669361005));
#386258=CARTESIAN_POINT('Ctrl Pts',(2.5553776555582,0.764406890608487,8.8519052845931));
#386259=CARTESIAN_POINT('Ctrl Pts',(2.55512991482068,0.764108287712571,
8.85282181883899));
#386260=CARTESIAN_POINT('Ctrl Pts',(2.55489782482715,0.763773984458597,
8.85372622499635));
#386261=CARTESIAN_POINT('Ctrl Pts',(2.55469040933054,0.763389941933513,
8.8546225773507));
#386262=CARTESIAN_POINT('Ctrl Pts',(2.55451822035196,0.763071123469087,
8.85536669723986));
#386263=CARTESIAN_POINT('Ctrl Pts',(2.5543629693013,0.762717968360524,8.8561049844905));
#386264=CARTESIAN_POINT('Ctrl Pts',(2.55423713170265,0.762319193931679,
8.8568133821837));
#386265=CARTESIAN_POINT('Ctrl Pts',(2.55412293388424,0.761957305511216,
8.85745625420284));
#386266=CARTESIAN_POINT('Ctrl Pts',(2.55403095653984,0.761553487472297,
8.85808743050666));
#386267=CARTESIAN_POINT('Ctrl Pts',(2.55398360973458,0.761089973691814,
8.8586680450841));
#386268=CARTESIAN_POINT('Ctrl Pts',(2.55396176494498,0.760876118481245,
8.85893592806396));
#386269=CARTESIAN_POINT('Ctrl Pts',(2.55394962718963,0.760649429011939,
8.85919241173848));
#386270=CARTESIAN_POINT('Ctrl Pts',(2.5539508609013,0.760407523287027,8.85943017985534));
#386271=CARTESIAN_POINT('Ctrl Pts',(2.55395252677728,0.760080878946637,
8.8597512372));
#386272=CARTESIAN_POINT('Ctrl Pts',(2.55397925578498,0.759718180134276,
8.86004599534705));
#386273=CARTESIAN_POINT('Ctrl Pts',(2.55404111371133,0.759324550001974,
8.86026130871721));
#386274=CARTESIAN_POINT('Ctrl Pts',(2.55406376164212,0.759180430912929,
8.86034014101235));
#386275=CARTESIAN_POINT('Ctrl Pts',(2.55409144662039,0.759029998745733,
8.86040910639693));
#386276=CARTESIAN_POINT('Ctrl Pts',(2.55412374520742,0.758877412823769,
8.86046313645507));
#386277=CARTESIAN_POINT('Ctrl Pts',(2.55417414688197,0.758639303770441,
8.8605474499083));
#386278=CARTESIAN_POINT('Ctrl Pts',(2.55423730297957,0.758389480825107,
8.86059655985669));
#386279=CARTESIAN_POINT('Ctrl Pts',(2.55430887908532,0.758143894092047,
8.86059725258816));
#386280=CARTESIAN_POINT('Ctrl Pts',(2.55438062056045,0.757897739955521,
8.86059794692012));
#386281=CARTESIAN_POINT('Ctrl Pts',(2.55446416726509,0.757653855137138,
8.86056369958366));
#386282=CARTESIAN_POINT('Ctrl Pts',(2.55455140251595,0.757424321695602,
8.86048590497774));
#386283=CARTESIAN_POINT('Ctrl Pts',(2.55457416831912,0.757364420301395,
8.86046560290182));
#386284=CARTESIAN_POINT('Ctrl Pts',(2.55459756617269,0.757304749210617,
8.86044257503091));
#386285=CARTESIAN_POINT('Ctrl Pts',(2.5546208425029,0.757247140326087,8.86041778462584));
#386286=CARTESIAN_POINT('Ctrl Pts',(2.55477746332169,0.756859504019869,
8.86025097596201));
#386287=CARTESIAN_POINT('Ctrl Pts',(2.5549499061779,0.756513345250583,8.8599848982295));
#386288=CARTESIAN_POINT('Ctrl Pts',(2.55512555432353,0.756214989631114,
8.85968173251461));
#386289=CARTESIAN_POINT('Ctrl Pts',(2.55521846212913,0.756057176602153,
8.85952137522076));
#386290=CARTESIAN_POINT('Ctrl Pts',(2.55531389301721,0.755909599116478,
8.85934740853961));
#386291=CARTESIAN_POINT('Ctrl Pts',(2.55540919580187,0.755773494207136,
8.8591675900182));
#386292=CARTESIAN_POINT('Ctrl Pts',(2.55579188601969,0.755226962250202,
8.85844552518695));
#386293=CARTESIAN_POINT('Ctrl Pts',(2.55619166074993,0.754832794368578,
8.85759444184124));
#386294=CARTESIAN_POINT('Ctrl Pts',(2.55654648248264,0.754540688576943,
8.85683498915139));
#386295=CARTESIAN_POINT('Ctrl Pts',(2.556583613632,0.75451012048379,8.85675551444998));
#386296=CARTESIAN_POINT('Ctrl Pts',(2.55662026192593,0.754480687682179,
8.85667699793651));
#386297=CARTESIAN_POINT('Ctrl Pts',(2.55665636186477,0.754452344408681,
8.85659965593547));
#386298=CARTESIAN_POINT('Ctrl Pts',(2.55714364068135,0.754069765456718,
8.85555568965886));
#386299=CARTESIAN_POINT('Ctrl Pts',(2.55766719778434,0.753772456084119,
8.85434650606346));
#386300=CARTESIAN_POINT('Ctrl Pts',(2.55822655250307,0.753553542379849,
8.85297329937117));
#386301=CARTESIAN_POINT('Ctrl Pts',(2.55854115545037,0.753430416759805,
8.85220095427747));
#386302=CARTESIAN_POINT('Ctrl Pts',(2.55886732590038,0.753332333771325,
8.85137579139183));
#386303=CARTESIAN_POINT('Ctrl Pts',(2.55920636991202,0.753260100986319,
8.85049129520029));
#386304=CARTESIAN_POINT('Origin',(2.56063892684944,0.759984192420934,7.59394543036555));
#386305=CARTESIAN_POINT('Ctrl Pts',(2.55537312258256,0.764439871044488,
7.59443877723642));
#386306=CARTESIAN_POINT('Ctrl Pts',(2.55128472608583,0.760338870223441,
7.58783886950016));
#386307=CARTESIAN_POINT('Ctrl Pts',(2.55574715922245,0.753116275673151,
7.58559994247159));
#386308=CARTESIAN_POINT('Ctrl Pts',(2.57769155910976,0.786827114208349,
7.56670252222139));
#386309=CARTESIAN_POINT('Ctrl Pts',(2.57360907150672,0.782732040497738,
7.56004874999029));
#386310=CARTESIAN_POINT('Ctrl Pts',(2.57807976992147,0.775455419514101,
7.55786368756705));
#386311=CARTESIAN_POINT('Ctrl Pts',(2.59996831818662,0.809172551432348,
7.5388891333356));
#386312=CARTESIAN_POINT('Ctrl Pts',(2.59586156815985,0.805053140498195,
7.53222002137279));
#386313=CARTESIAN_POINT('Ctrl Pts',(2.60037064305195,0.797754463334677,
7.53005029815326));
#386314=CARTESIAN_POINT('Ctrl Pts',(2.62220239177471,0.83147517157032,7.51101258149734));
#386315=CARTESIAN_POINT('Ctrl Pts',(2.61804586047545,0.827305825890515,
7.5043616886572));
#386316=CARTESIAN_POINT('Ctrl Pts',(2.6226187357238,0.820012246967404,7.50217374673251));
#386317=CARTESIAN_POINT('',(2.62143154819291,0.818824543767695,7.50366116523517));
#386318=CARTESIAN_POINT('Ctrl Pts',(2.61614521332082,0.82539931913465,7.51860402984325));
#386319=CARTESIAN_POINT('Ctrl Pts',(2.61645699862685,0.825712065659369,
7.51734760759494));
#386320=CARTESIAN_POINT('Ctrl Pts',(2.61678087653057,0.825952671069652,
7.51608817408572));
#386321=CARTESIAN_POINT('Ctrl Pts',(2.61712406542064,0.826109862572553,
7.51481005913119));
#386322=CARTESIAN_POINT('Ctrl Pts',(2.61743493411804,0.826252250392093,
7.51365231206383));
#386323=CARTESIAN_POINT('Ctrl Pts',(2.61776198182467,0.826326623841287,
7.51247773061043));
#386324=CARTESIAN_POINT('Ctrl Pts',(2.61810773746039,0.826295690232712,
7.51129758471022));
#386325=CARTESIAN_POINT('Ctrl Pts',(2.61853747222881,0.826257243290004,
7.50983079813402));
#386326=CARTESIAN_POINT('Ctrl Pts',(2.61898123088401,0.8260443758982,7.50839324291155));
#386327=CARTESIAN_POINT('Ctrl Pts',(2.6194065965824,0.825581204338881,7.50715379678855));
#386328=CARTESIAN_POINT('Ctrl Pts',(2.61960310327844,0.825367232424444,
7.50658120839351));
#386329=CARTESIAN_POINT('Ctrl Pts',(2.61981662153139,0.825062996159295,
7.50598221009429));
#386330=CARTESIAN_POINT('Ctrl Pts',(2.62002345116589,0.824662668982309,
7.50545747549611));
#386331=CARTESIAN_POINT('Ctrl Pts',(2.62013382186084,0.824449042009384,
7.50517746087247));
#386332=CARTESIAN_POINT('Ctrl Pts',(2.62024366461122,0.824205828466814,
7.50491486231392));
#386333=CARTESIAN_POINT('Ctrl Pts',(2.6203485504252,0.823938782502934,7.50468370960992));
#386334=CARTESIAN_POINT('Ctrl Pts',(2.62050538780146,0.823539464552062,
7.50433806340447));
#386335=CARTESIAN_POINT('Ctrl Pts',(2.6206553264377,0.823074680524733,7.50405484070984));
#386336=CARTESIAN_POINT('Ctrl Pts',(2.62078758644981,0.822575512814678,
7.50385766036131));
#386337=CARTESIAN_POINT('Ctrl Pts',(2.62080172960231,0.822522134586908,
7.50383657498791));
#386338=CARTESIAN_POINT('Ctrl Pts',(2.62081567828758,0.822468390482977,
7.50381643264937));
#386339=CARTESIAN_POINT('Ctrl Pts',(2.62082942521803,0.822414338256762,
7.50379723213559));
#386340=CARTESIAN_POINT('Ctrl Pts',(2.62092119047576,0.822053521965076,
7.50366906242519));
#386341=CARTESIAN_POINT('Ctrl Pts',(2.62100526478185,0.821670949923771,
7.50358235568538));
#386342=CARTESIAN_POINT('Ctrl Pts',(2.62107743801798,0.821300249590857,
7.5035341175365));
#386343=CARTESIAN_POINT('Ctrl Pts',(2.62118565361712,0.820744426396829,
7.50346178989176));
#386344=CARTESIAN_POINT('Ctrl Pts',(2.62127843601656,0.820141885920979,
7.50346967198526));
#386345=CARTESIAN_POINT('Ctrl Pts',(2.62135131886642,0.819547575210617,
7.50354272648692));
#386346=CARTESIAN_POINT('Ctrl Pts',(2.62138129709116,0.819303122913942,
7.50357277531559));
#386347=CARTESIAN_POINT('Ctrl Pts',(2.6214080095276,0.819060405024635,7.50361331098761));
#386348=CARTESIAN_POINT('Ctrl Pts',(2.62143154819427,0.818824543768117,
7.50366116523658));
#386349=CARTESIAN_POINT('',(2.56344583459815,0.76081726790679,7.57603338622103));
#386350=CARTESIAN_POINT('Origin',(2.57191833523268,0.763328885433888,7.58486873427624));
#386351=CARTESIAN_POINT('Ctrl Pts',(2.62143154822949,0.818824543811863,
7.50366116529968));
#386352=CARTESIAN_POINT('Ctrl Pts',(2.60213510841253,0.799519746242575,
7.52783573079709));
#386353=CARTESIAN_POINT('Ctrl Pts',(2.58280746249008,0.780184887893108,
7.55196141284069));
#386354=CARTESIAN_POINT('Ctrl Pts',(2.56344583519718,0.760817269006253,
7.57603338728831));
#386355=CARTESIAN_POINT('Ctrl Pts',(2.55662067806349,0.765442247231722,
7.59639677331372));
#386356=CARTESIAN_POINT('Ctrl Pts',(2.54113756247318,0.754196289838712,
7.59974925422225));
#386357=CARTESIAN_POINT('Ctrl Pts',(2.5602488397315,0.753217766653679,7.59639677331371));
#386358=CARTESIAN_POINT('Ctrl Pts',(2.55313724428124,0.76368702839399,7.58707626057424));
#386359=CARTESIAN_POINT('Ctrl Pts',(2.55101612578581,0.757128195576313,
7.58811717123966));
#386360=CARTESIAN_POINT('Ctrl Pts',(2.55637188217917,0.752788459978747,
7.58707626057422));
#386361=CARTESIAN_POINT('Ctrl Pts',(2.55888304972317,0.761709314540876,
7.58015376756929));
#386362=CARTESIAN_POINT('Ctrl Pts',(2.55764184525409,0.759094674335489,
7.5820876076604));
#386363=CARTESIAN_POINT('Ctrl Pts',(2.56010846144153,0.757580495838136,
7.5801537675693));
#386364=CARTESIAN_POINT('Ctrl Pts',(2.56344583380473,0.760817267671516,
7.57603338509286));
#386365=CARTESIAN_POINT('Ctrl Pts',(2.56344583380473,0.760817267671516,
7.57603338509286));
#386366=CARTESIAN_POINT('Ctrl Pts',(2.56344583380473,0.760817267671516,
7.57603338509286));
#386367=CARTESIAN_POINT('Origin',(2.57191671161825,0.763334355930457,7.58486873427622));
#386368=CARTESIAN_POINT('Ctrl Pts',(2.65126187924781,0.733647821794611,
7.51098857897448));
#386369=CARTESIAN_POINT('Ctrl Pts',(2.64550378996543,0.734874573516824,
7.50433767179956));
#386370=CARTESIAN_POINT('Ctrl Pts',(2.64535737577417,0.743481931646183,
7.50214974420965));
#386371=CARTESIAN_POINT('Ctrl Pts',(2.62045204982553,0.740211806729772,
7.5388732158917));
#386372=CARTESIAN_POINT('Ctrl Pts',(2.61476295267152,0.741423859789251,
7.53220407452065));
#386373=CARTESIAN_POINT('Ctrl Pts',(2.61456026023065,0.750000679461852,
7.53003438070912));
#386374=CARTESIAN_POINT('Ctrl Pts',(2.58958305416543,0.746788396937374,
7.56669465659231));
#386375=CARTESIAN_POINT('Ctrl Pts',(2.58392757851788,0.747993286988592,
7.56004085833299));
#386376=CARTESIAN_POINT('Ctrl Pts',(2.58370474861185,0.75653067516997,7.55785582193789));
#386377=CARTESIAN_POINT('Ctrl Pts',(2.55865628834872,0.753377294984544,
7.59443891967696));
#386378=CARTESIAN_POINT('Ctrl Pts',(2.55299261296562,0.754583931976354,
7.58783901202978));
#386379=CARTESIAN_POINT('Ctrl Pts',(2.5527923475989,0.763071515364528,7.58560008491213));
#386380=CARTESIAN_POINT('',(2.64368796492175,0.743835290548502,7.50366116523517));
#386381=CARTESIAN_POINT('Ctrl Pts',(2.64368796492211,0.743835290548603,
7.50366116523554));
#386382=CARTESIAN_POINT('Ctrl Pts',(2.64403606905883,0.743162266754996,
7.50350835821027));
#386383=CARTESIAN_POINT('Ctrl Pts',(2.64433416512128,0.742532269335402,
7.50345484956));
#386384=CARTESIAN_POINT('Ctrl Pts',(2.64459165855155,0.741926824793144,
7.50349758195598));
#386385=CARTESIAN_POINT('Ctrl Pts',(2.64472377177749,0.741616186842028,
7.50351950684424));
#386386=CARTESIAN_POINT('Ctrl Pts',(2.6448583372899,0.741281445250328,7.50357029184312));
#386387=CARTESIAN_POINT('Ctrl Pts',(2.6449792244816,0.74095509093709,7.50365515313923));
#386388=CARTESIAN_POINT('Ctrl Pts',(2.64516519793449,0.740453025849417,
7.50378570417639));
#386389=CARTESIAN_POINT('Ctrl Pts',(2.64532458362198,0.739956193803965,
7.50400001621911));
#386390=CARTESIAN_POINT('Ctrl Pts',(2.64544308808559,0.739501717390469,
7.50428903009634));
#386391=CARTESIAN_POINT('Ctrl Pts',(2.64545624116933,0.739451274005102,
7.50432110841318));
#386392=CARTESIAN_POINT('Ctrl Pts',(2.64546891357409,0.739401332602668,
7.50435406373354));
#386393=CARTESIAN_POINT('Ctrl Pts',(2.64548110249555,0.739351929091606,
7.50438785222352));
#386394=CARTESIAN_POINT('Ctrl Pts',(2.64555552171984,0.739050296910222,
7.50459414719561));
#386395=CARTESIAN_POINT('Ctrl Pts',(2.64561260228404,0.738763789814967,
7.50483629897752));
#386396=CARTESIAN_POINT('Ctrl Pts',(2.64565144811457,0.738503640946567,
7.5050991045531));
#386397=CARTESIAN_POINT('Ctrl Pts',(2.6457371459184,0.737929726413397,7.50567888004914));
#386398=CARTESIAN_POINT('Ctrl Pts',(2.64573798903582,0.737461555509749,
7.50637912803144));
#386399=CARTESIAN_POINT('Ctrl Pts',(2.645683829865,0.737091112458748,7.50710440483569));
#386400=CARTESIAN_POINT('Ctrl Pts',(2.6456705489611,0.737000272468318,7.50728225710685));
#386401=CARTESIAN_POINT('Ctrl Pts',(2.64565384064822,0.736913479663692,
7.50746498566954));
#386402=CARTESIAN_POINT('Ctrl Pts',(2.64563450403443,0.73683268131825,7.50764697238949));
#386403=CARTESIAN_POINT('Ctrl Pts',(2.64553055572032,0.736398331649459,
7.50862528291182));
#386404=CARTESIAN_POINT('Ctrl Pts',(2.64534524283224,0.736096819786135,
7.50965856837421));
#386405=CARTESIAN_POINT('Ctrl Pts',(2.64512364214822,0.735879530093703,
7.51067959873202));
#386406=CARTESIAN_POINT('Ctrl Pts',(2.64500169501229,0.735759955301882,
7.51124147302578));
#386407=CARTESIAN_POINT('Ctrl Pts',(2.64486842488808,0.735666166627857,
7.51180065547253));
#386408=CARTESIAN_POINT('Ctrl Pts',(2.64472951425972,0.735592069739074,
7.512351757165));
#386409=CARTESIAN_POINT('Ctrl Pts',(2.64424952270334,0.735336035471634,
7.51425603304536));
#386410=CARTESIAN_POINT('Ctrl Pts',(2.64364210055535,0.735289940333101,
7.5162690050518));
#386411=CARTESIAN_POINT('Ctrl Pts',(2.64295636119802,0.735418705226031,
7.51827788969244));
#386412=CARTESIAN_POINT('Ctrl Pts',(2.64291924768814,0.735425674225368,
7.51838661432545));
#386413=CARTESIAN_POINT('Ctrl Pts',(2.64288189864373,0.735433163274049,
7.51849533314857));
#386414=CARTESIAN_POINT('Ctrl Pts',(2.64284431997726,0.735441169348903,
7.51860402984325));
#386415=CARTESIAN_POINT('Ctrl Pts',(2.56344583570119,0.760817267312242,
7.57603338728985));
#386416=CARTESIAN_POINT('Ctrl Pts',(2.59023829728888,0.755147939734382,
7.55196141284922));
#386417=CARTESIAN_POINT('Ctrl Pts',(2.61698440749374,0.749487530346329,
7.52783573083105));
#386418=CARTESIAN_POINT('Ctrl Pts',(2.64368796497828,0.743835290530981,
7.50366116530176));
#386419=CARTESIAN_POINT('Origin',(8.85789032694959E-16,2.62897535302361E-16,
7.49482233047033));
#386420=CARTESIAN_POINT('Origin',(2.61299471585144,0.816189233531341,7.49482233047033));
#386421=CARTESIAN_POINT('Origin',(0.,0.,7.50366116523517));
#386422=CARTESIAN_POINT('Origin',(2.63517950238394,0.741441326212352,7.49482233047033));
#386423=CARTESIAN_POINT('Ctrl Pts',(2.61614446651996,0.825398570094828,
7.51860402984325));
#386424=CARTESIAN_POINT('Ctrl Pts',(2.62151698305455,0.830786737883201,
7.51860402984325));
#386425=CARTESIAN_POINT('Ctrl Pts',(2.61919823167326,0.838033784044352,
7.51860402984325));
#386426=CARTESIAN_POINT('Ctrl Pts',(2.61813931767337,0.827399234462656,
7.51041458714366));
#386427=CARTESIAN_POINT('Ctrl Pts',(2.62096763486515,0.832503643108405,
7.51004642900443));
#386428=CARTESIAN_POINT('Ctrl Pts',(2.61919759218916,0.838035782693636,
7.5072913648301));
#386429=CARTESIAN_POINT('Ctrl Pts',(2.62069593195854,0.826221329289853,
7.50215815450137));
#386430=CARTESIAN_POINT('Ctrl Pts',(2.62208629631496,0.829007895534876,
7.49877163671529));
#386431=CARTESIAN_POINT('Ctrl Pts',(2.62105762822771,0.832301186527272,
7.4948158853317));
#386432=CARTESIAN_POINT('Ctrl Pts',(2.62143102271335,0.818824379629568,
7.50366171572174));
#386433=CARTESIAN_POINT('Ctrl Pts',(2.62492619857234,0.819916125008284,
7.50000045605858));
#386434=CARTESIAN_POINT('Ctrl Pts',(2.6249261985723,0.819916125008403,7.49482233047317));
#386435=CARTESIAN_POINT('Origin',(2.60729278516565,0.834224539571422,7.51860402984325));
#386436=CARTESIAN_POINT('Origin',(2.60729278516565,0.834224539571422,9.));
#386437=CARTESIAN_POINT('Origin',(2.60729278516565,0.834224539571422,8.75721825406948));
#386438=CARTESIAN_POINT('Ctrl Pts',(2.60435458367724,0.813572382352496,
8.78942910404913));
#386439=CARTESIAN_POINT('Ctrl Pts',(2.60830313188505,0.817504480488642,
8.79672699501691));
#386440=CARTESIAN_POINT('Ctrl Pts',(2.60327327413769,0.824878354438172,
8.79893251111266));
#386441=CARTESIAN_POINT('Ctrl Pts',(2.61211678181375,0.821358504547112,
8.78111911759577));
#386442=CARTESIAN_POINT('Ctrl Pts',(2.61679257887839,0.826025327013849,
8.78644465894811));
#386443=CARTESIAN_POINT('Ctrl Pts',(2.61376706025929,0.83354608155451,8.78817647674132));
#386444=CARTESIAN_POINT('Ctrl Pts',(2.61695436881582,0.826211001637836,
8.76780923932034));
#386445=CARTESIAN_POINT('Ctrl Pts',(2.62247035001552,0.831723595235669,
8.76988516158376));
#386446=CARTESIAN_POINT('Ctrl Pts',(2.62031418371861,0.838968409056361,
8.77093053738832));
#386447=CARTESIAN_POINT('Ctrl Pts',(2.61601110555621,0.82526483111746,8.75371302330491));
#386448=CARTESIAN_POINT('Ctrl Pts',(2.62139224614752,0.830641589183852,
8.75300828287559));
#386449=CARTESIAN_POINT('Ctrl Pts',(2.61903693688884,0.837911187359152,
8.75267964240738));
#386450=CARTESIAN_POINT('Origin',(2.59739259559947,0.824293828210157,8.78727029226991));
#386451=CARTESIAN_POINT('Ctrl Pts',(2.5557700913641,0.764838063661159,8.85049129520029));
#386452=CARTESIAN_POINT('Ctrl Pts',(2.55989296307186,0.768973645978611,
8.85711686593484));
#386453=CARTESIAN_POINT('Ctrl Pts',(2.55537491841651,0.776232298374626,
8.85933012996512));
#386454=CARTESIAN_POINT('Ctrl Pts',(2.57261954817433,0.781739466513905,
8.82945683644723));
#386455=CARTESIAN_POINT('Ctrl Pts',(2.57677664221,0.785909376665029,8.8360746990239));
#386456=CARTESIAN_POINT('Ctrl Pts',(2.57221349406443,0.793169522772296,
8.83829567148519));
#386457=CARTESIAN_POINT('Ctrl Pts',(2.58944388951045,0.798615676462769,
8.80838214965002));
#386458=CARTESIAN_POINT('Ctrl Pts',(2.59361738938009,0.802802043026221,
8.81501364461988));
#386459=CARTESIAN_POINT('Ctrl Pts',(2.58902700057119,0.810080582933261,
8.81722098428722));
#386460=CARTESIAN_POINT('Ctrl Pts',(2.60624502375464,0.815468607773385,
8.78727029226991));
#386461=CARTESIAN_POINT('Ctrl Pts',(2.61041921685633,0.819655669706082,
8.79393457792714));
#386462=CARTESIAN_POINT('Ctrl Pts',(2.60581736094343,0.82696746410521,8.79610912703474));
#386463=CARTESIAN_POINT('Origin',(2.54691766320893,0.773663284097931,8.85049129520029));
#386464=CARTESIAN_POINT('Ctrl Pts',(2.55920636991202,0.753260100986319,
8.85049129520029));
#386465=CARTESIAN_POINT('Ctrl Pts',(2.56491780413929,0.752043289049059,
8.85711686593484));
#386466=CARTESIAN_POINT('Ctrl Pts',(2.56509113287406,0.743495147773693,
8.85933012996512));
#386467=CARTESIAN_POINT('Ctrl Pts',(2.55415354649658,0.754336596942347,
8.86332496987232));
#386468=CARTESIAN_POINT('Ctrl Pts',(2.55573644967854,0.749995363028666,
8.86648636486736));
#386469=CARTESIAN_POINT('Ctrl Pts',(2.55095922330301,0.746523445683803,
8.87206031107457));
#386470=CARTESIAN_POINT('Ctrl Pts',(2.55209786073928,0.761154511730837,
8.86341338519876));
#386471=CARTESIAN_POINT('Ctrl Pts',(2.55102439395549,0.765662409211744,
8.86654584966058));
#386472=CARTESIAN_POINT('Ctrl Pts',(2.54510291120593,0.765907755566788,
8.87215952290714));
#386473=CARTESIAN_POINT('Ctrl Pts',(2.5557700913641,0.764838063661158,8.85049129520029));
#386474=CARTESIAN_POINT('Ctrl Pts',(2.55989296307186,0.768973645978611,
8.85711686593484));
#386475=CARTESIAN_POINT('Ctrl Pts',(2.55537491841651,0.776232298374626,
8.85933012996512));
#386476=CARTESIAN_POINT('Origin',(2.55660172093491,0.741034480196109,8.85049129520029));
#386477=CARTESIAN_POINT('Ctrl Pts',(2.62912953922426,0.738363081476945,
8.78727029226991));
#386478=CARTESIAN_POINT('Ctrl Pts',(2.63491206922812,0.737131122698069,
8.79393457792714));
#386479=CARTESIAN_POINT('Ctrl Pts',(2.63504414756229,0.728492721775916,
8.79610912703474));
#386480=CARTESIAN_POINT('Ctrl Pts',(2.60585484624786,0.743321717630804,
8.80838214965002));
#386481=CARTESIAN_POINT('Ctrl Pts',(2.61163641591401,0.74208996345033,8.8150136446199));
#386482=CARTESIAN_POINT('Ctrl Pts',(2.61175996320558,0.733485688427888,
8.81722098428721));
#386483=CARTESIAN_POINT('Ctrl Pts',(2.58254800437416,0.748287203055872,
8.82945683644723));
#386484=CARTESIAN_POINT('Ctrl Pts',(2.58830684695872,0.747060290843834,
8.83607469902389));
#386485=CARTESIAN_POINT('Ctrl Pts',(2.58844318986646,0.738486292178741,
8.83829567148519));
#386486=CARTESIAN_POINT('Ctrl Pts',(2.55920636991202,0.753260100986318,
8.85049129520029));
#386487=CARTESIAN_POINT('Ctrl Pts',(2.56491780413929,0.752043289049059,
8.85711686593484));
#386488=CARTESIAN_POINT('Ctrl Pts',(2.56509113287406,0.743495147773693,
8.85933012996512));
#386489=CARTESIAN_POINT('Origin',(2.62652489024714,0.726137460686736,8.78727029226991));
#386490=CARTESIAN_POINT('Ctrl Pts',(2.64266321935266,0.735479733686564,
8.75374538247849));
#386491=CARTESIAN_POINT('Ctrl Pts',(2.65009811484497,0.733909158185006,
8.75304829418602));
#386492=CARTESIAN_POINT('Ctrl Pts',(2.65209331987869,0.726540996943395,
8.75272238421917));
#386493=CARTESIAN_POINT('Ctrl Pts',(2.64395422903473,0.73520468657252,8.76769408445017));
#386494=CARTESIAN_POINT('Ctrl Pts',(2.65157607685313,0.733593913216396,
8.76974318093968));
#386495=CARTESIAN_POINT('Ctrl Pts',(2.65372225373277,0.726354280485274,
8.7707786988043));
#386496=CARTESIAN_POINT('Ctrl Pts',(2.63733724884731,0.736614421409556,
8.78108014887994));
#386497=CARTESIAN_POINT('Ctrl Pts',(2.64379727590478,0.735253066306277,
8.78639403366326));
#386498=CARTESIAN_POINT('Ctrl Pts',(2.64538156698146,0.727315050337962,
8.78812224174741));
#386499=CARTESIAN_POINT('Ctrl Pts',(2.62649347902617,0.738924665570915,
8.78944554828685));
#386500=CARTESIAN_POINT('Ctrl Pts',(2.63193890460373,0.737782843388512,
8.79673892988685));
#386501=CARTESIAN_POINT('Ctrl Pts',(2.63174894852014,0.728868390460666,
8.79894799272499));
#386502=CARTESIAN_POINT('Origin',(2.64023967100014,0.723215548558698,8.75721825406948));
#386503=CARTESIAN_POINT('Origin',(2.64023967100014,0.723215548558698,9.));
#386504=CARTESIAN_POINT('Origin',(2.64023967100014,0.723215548558698,7.51860402984325));
#386505=CARTESIAN_POINT('Ctrl Pts',(2.64368720766141,0.7438350774836,7.50366195182966));
#386506=CARTESIAN_POINT('Ctrl Pts',(2.64721228549989,0.744826903044238,
7.50000065167735));
#386507=CARTESIAN_POINT('Ctrl Pts',(2.64721228549992,0.744826903044126,
7.49482233047108));
#386508=CARTESIAN_POINT('Ctrl Pts',(2.64710868794002,0.737228469253212,
7.50215800491336));
#386509=CARTESIAN_POINT('Ctrl Pts',(2.64979433702035,0.735649866645935,
7.49877273257264));
#386510=CARTESIAN_POINT('Ctrl Pts',(2.65072935414104,0.732326780830922,
7.49481816995649));
#386511=CARTESIAN_POINT('Ctrl Pts',(2.64560110706609,0.7348541869931,7.51043025814043));
#386512=CARTESIAN_POINT('Ctrl Pts',(2.65076076619579,0.732120933500987,
7.51006209594517));
#386513=CARTESIAN_POINT('Ctrl Pts',(2.65229622879822,0.726515460750279,
7.507312818217));
#386514=CARTESIAN_POINT('Ctrl Pts',(2.64284284172668,0.735441484194402,
7.51860402984326));
#386515=CARTESIAN_POINT('Ctrl Pts',(2.65028527911173,0.733856825505522,
7.51860402984326));
#386516=CARTESIAN_POINT('Ctrl Pts',(2.65229555990882,0.7265179026617,7.51860402984327));
#386517=CARTESIAN_POINT('Origin',(0.,0.,7.5));
#386518=CARTESIAN_POINT('Origin',(2.6022097463239,0.587743532225645,7.5));
#386519=CARTESIAN_POINT('',(2.6022097463239,0.587743532225645,7.59394543036555));
#386520=CARTESIAN_POINT('',(2.6022097463239,0.587743532225645,8.85049129520029));
#386521=CARTESIAN_POINT('',(2.6022097463239,0.587743532225645,7.5));
#386522=CARTESIAN_POINT('',(2.67103479566853,0.568397127400971,8.78727029226991));
#386523=CARTESIAN_POINT('Ctrl Pts',(2.6022097463239,0.587743532225645,8.85049129520029));
#386524=CARTESIAN_POINT('Ctrl Pts',(2.62518477739697,0.58128535665975,8.82945686509571));
#386525=CARTESIAN_POINT('Ctrl Pts',(2.64812565330824,0.574836781952744,
8.80838212259896));
#386526=CARTESIAN_POINT('Ctrl Pts',(2.67103479566853,0.568397127400971,
8.78727029226991));
#386527=CARTESIAN_POINT('',(2.68453419038076,0.564602509634941,8.75721825406948));
#386528=CARTESIAN_POINT('Origin',(2.64390988332938,0.576022025127795,8.75937679713151));
#386529=CARTESIAN_POINT('',(2.68453419038076,0.564602509634941,7.51860402984325));
#386530=CARTESIAN_POINT('',(2.68453419038076,0.564602509634941,7.5));
#386531=CARTESIAN_POINT('Ctrl Pts',(2.68453419038076,0.564602509634941,
7.51860402984325));
#386532=CARTESIAN_POINT('Ctrl Pts',(2.67393251538731,0.567582591715464,
7.52834476460825));
#386533=CARTESIAN_POINT('Ctrl Pts',(2.66332395793944,0.570564608422277,
7.53807742314407));
#386534=CARTESIAN_POINT('Ctrl Pts',(2.65270828694957,0.573548624713022,
7.54780169004674));
#386535=CARTESIAN_POINT('Ctrl Pts',(2.63589363782969,0.578275145245242,
7.5632044032688));
#386536=CARTESIAN_POINT('Ctrl Pts',(2.61906112037001,0.583006688485576,
7.57858609112103));
#386537=CARTESIAN_POINT('Ctrl Pts',(2.6022097463239,0.587743532225645,7.59394543036555));
#386538=CARTESIAN_POINT('Origin',(2.80575616266556,0.781431603558372,7.5));
#386539=CARTESIAN_POINT('',(2.66365357834824,0.656086448390735,8.75721825406948));
#386540=CARTESIAN_POINT('',(2.65313746692184,0.646810448064383,8.78727029226991));
#386541=CARTESIAN_POINT('Origin',(2.62644365380812,0.623264499460921,8.75658640621069));
#386542=CARTESIAN_POINT('',(2.5995223305943,0.599517869856918,8.85049129520029));
#386543=CARTESIAN_POINT('Ctrl Pts',(2.65313746692184,0.646810448064383,
8.78727029226991));
#386544=CARTESIAN_POINT('Ctrl Pts',(2.63529110426043,0.631068615445932,
8.80838212259896));
#386545=CARTESIAN_POINT('Ctrl Pts',(2.61742002096781,0.61530497737356,8.82945686509571));
#386546=CARTESIAN_POINT('Ctrl Pts',(2.5995223305943,0.599517869856918,8.85049129520029));
#386547=CARTESIAN_POINT('',(2.5995223305943,0.599517869856918,7.59394543036555));
#386548=CARTESIAN_POINT('',(2.5995223305943,0.599517869856918,7.5));
#386549=CARTESIAN_POINT('',(2.66365357834824,0.656086448390735,7.51860402984325));
#386550=CARTESIAN_POINT('Ctrl Pts',(2.5995223305943,0.599517869856917,7.59394543036555));
#386551=CARTESIAN_POINT('Ctrl Pts',(2.61264965451766,0.61109715577923,7.57858609112103));
#386552=CARTESIAN_POINT('Ctrl Pts',(2.62576228904419,0.622663484549934,
7.56320440326857));
#386553=CARTESIAN_POINT('Ctrl Pts',(2.63886100402437,0.63421753523505,7.54780169004651));
#386554=CARTESIAN_POINT('Ctrl Pts',(2.64713067695232,0.641512008036651,
7.53807742314383));
#386555=CARTESIAN_POINT('Ctrl Pts',(2.65539480838749,0.648801592825318,
7.52834476460825));
#386556=CARTESIAN_POINT('Ctrl Pts',(2.66365357834824,0.656086448390733,
7.51860402984325));
#386557=CARTESIAN_POINT('',(2.66365357834824,0.656086448390735,7.5));
#386558=CARTESIAN_POINT('Origin',(2.60407017393683,0.594362024055136,7.5));
#386559=CARTESIAN_POINT('Ctrl Pts',(2.5995223305943,0.599517869856918,8.85049129520029));
#386560=CARTESIAN_POINT('Ctrl Pts',(2.5993770958507,0.599389761901953,8.85097269580138));
#386561=CARTESIAN_POINT('Ctrl Pts',(2.59923925769927,0.5992569622011,8.85143669361005));
#386562=CARTESIAN_POINT('Ctrl Pts',(2.59910307573752,0.599112726143938,
8.8519052845931));
#386563=CARTESIAN_POINT('Ctrl Pts',(2.59883671245668,0.598830609563248,
8.85282181883899));
#386564=CARTESIAN_POINT('Ctrl Pts',(2.59858368043392,0.598511863228102,
8.85372622499636));
#386565=CARTESIAN_POINT('Ctrl Pts',(2.59835208540563,0.598141898916068,
8.85462257735071));
#386566=CARTESIAN_POINT('Ctrl Pts',(2.59815982343862,0.597834767684107,
8.85536669723986));
#386567=CARTESIAN_POINT('Ctrl Pts',(2.5979822646424,0.597492285139559,8.85610498449051));
#386568=CARTESIAN_POINT('Ctrl Pts',(2.59783113602521,0.597102392478176,
8.85681338218371));
#386569=CARTESIAN_POINT('Ctrl Pts',(2.59769398656776,0.596748564275631,
8.85745625420285));
#386570=CARTESIAN_POINT('Ctrl Pts',(2.5975763254901,0.59635146893287,8.85808743050666));
#386571=CARTESIAN_POINT('Ctrl Pts',(2.59749937853404,0.595891941011388,
8.85866804508411));
#386572=CARTESIAN_POINT('Ctrl Pts',(2.59746387687652,0.595679924789762,
8.85893592806396));
#386573=CARTESIAN_POINT('Ctrl Pts',(2.59743724001533,0.595454478746938,
8.85919241173848));
#386574=CARTESIAN_POINT('Ctrl Pts',(2.5974229722392,0.595212990999105,8.85943017985534));
#386575=CARTESIAN_POINT('Ctrl Pts',(2.59740370651771,0.594886911051505,
8.8597512372));
#386576=CARTESIAN_POINT('Ctrl Pts',(2.5974071424151,0.594523244909351,8.86004599534706));
#386577=CARTESIAN_POINT('Ctrl Pts',(2.59744365327854,0.594126460281423,
8.86026130871721));
#386578=CARTESIAN_POINT('Ctrl Pts',(2.597457020935,0.593981186242596,8.86034014101236));
#386579=CARTESIAN_POINT('Ctrl Pts',(2.59747501080946,0.593829289371773,
8.86040910639692));
#386580=CARTESIAN_POINT('Ctrl Pts',(2.59749746682199,0.593674947576375,
8.86046313645506));
#386581=CARTESIAN_POINT('Ctrl Pts',(2.59753250924147,0.593434098497258,
8.86054744990829));
#386582=CARTESIAN_POINT('Ctrl Pts',(2.59757952936704,0.593180742414891,
8.86059655985668));
#386583=CARTESIAN_POINT('Ctrl Pts',(2.59763522361598,0.592931074369274,
8.86059725258816));
#386584=CARTESIAN_POINT('Ctrl Pts',(2.59769104654089,0.592680829490728,
8.86059794692011));
#386585=CARTESIAN_POINT('Ctrl Pts',(2.5977587958359,0.592432092904116,8.86056369958366));
#386586=CARTESIAN_POINT('Ctrl Pts',(2.59783114559448,0.592197441881941,
8.86048590497774));
#386587=CARTESIAN_POINT('Ctrl Pts',(2.59785002672736,0.592136204951556,
8.86046560290182));
#386588=CARTESIAN_POINT('Ctrl Pts',(2.59786955336763,0.592075157355808,
8.86044257503091));
#386589=CARTESIAN_POINT('Ctrl Pts',(2.59788909086021,0.592016175515313,
8.86041778462584));
#386590=CARTESIAN_POINT('Ctrl Pts',(2.59802055394132,0.591619300919147,
8.86025097596201));
#386591=CARTESIAN_POINT('Ctrl Pts',(2.5981704640267,0.591262804918446,8.8599848982295));
#386592=CARTESIAN_POINT('Ctrl Pts',(2.59832663557419,0.590953808487266,
8.85968173251461));
#386593=CARTESIAN_POINT('Ctrl Pts',(2.59840924137526,0.590790367078556,
8.85952137522076));
#386594=CARTESIAN_POINT('Ctrl Pts',(2.59849502086838,0.590636978528661,
8.85934740853961));
#386595=CARTESIAN_POINT('Ctrl Pts',(2.59858140757177,0.590495047191074,
8.8591675900182));
#386596=CARTESIAN_POINT('Ctrl Pts',(2.59892829508878,0.589925119096225,
8.85844552518696));
#386597=CARTESIAN_POINT('Ctrl Pts',(2.59930199401607,0.589506147419881,
8.85759444184125));
#386598=CARTESIAN_POINT('Ctrl Pts',(2.59963737144715,0.589191908284455,
8.8568349891514));
#386599=CARTESIAN_POINT('Ctrl Pts',(2.59967246780213,0.589159023995817,
8.85675551444999));
#386600=CARTESIAN_POINT('Ctrl Pts',(2.59970715503213,0.589127303602798,
8.85667699793652));
#386601=CARTESIAN_POINT('Ctrl Pts',(2.59974136484002,0.58909670563257,8.85659965593547));
#386602=CARTESIAN_POINT('Ctrl Pts',(2.60020313057239,0.588683692669124,
8.85555568965886));
#386603=CARTESIAN_POINT('Ctrl Pts',(2.60070656329426,0.588353449731756,
8.85434650606346));
#386604=CARTESIAN_POINT('Ctrl Pts',(2.60125074290954,0.588099147829294,
8.85297329937117));
#386605=CARTESIAN_POINT('Ctrl Pts',(2.60155681078578,0.587956118504001,
8.85220095427747));
#386606=CARTESIAN_POINT('Ctrl Pts',(2.60187602688497,0.587837339225057,
8.85137579139183));
#386607=CARTESIAN_POINT('Ctrl Pts',(2.6022097463239,0.587743532225645,8.85049129520029));
#386608=CARTESIAN_POINT('Origin',(2.60407017393683,0.594362024055136,7.59394543036555));
#386609=CARTESIAN_POINT('Ctrl Pts',(2.59910066513915,0.599145929246844,
7.59443877723642));
#386610=CARTESIAN_POINT('Ctrl Pts',(2.59475791666676,0.595315298834728,
7.58783886950016));
#386611=CARTESIAN_POINT('Ctrl Pts',(2.59874842803423,0.587821634806851,
7.58559994247159));
#386612=CARTESIAN_POINT('Ctrl Pts',(2.62280760163913,0.620057228280669,
7.56670252222137));
#386613=CARTESIAN_POINT('Ctrl Pts',(2.61847112967123,0.616232134217035,
7.5600487499903));
#386614=CARTESIAN_POINT('Ctrl Pts',(2.6224664278495,0.608684025200656,7.55786368756704));
#386615=CARTESIAN_POINT('Ctrl Pts',(2.64647026780379,0.640929477552829,
7.53888913333558));
#386616=CARTESIAN_POINT('Ctrl Pts',(2.64210802397063,0.637081650767913,
7.53222002137278));
#386617=CARTESIAN_POINT('Ctrl Pts',(2.64614020663337,0.629509072099142,
7.53005029815326));
#386618=CARTESIAN_POINT('Ctrl Pts',(2.6700875928815,0.66176173257994,7.51101258149734));
#386619=CARTESIAN_POINT('Ctrl Pts',(2.6656724707267,0.657867263142695,7.5043616886572));
#386620=CARTESIAN_POINT('Ctrl Pts',(2.66976864930636,0.650295684536609,
7.50217374673251));
#386621=CARTESIAN_POINT('',(2.6685078045743,0.649186484966767,7.50366116523517));
#386622=CARTESIAN_POINT('Ctrl Pts',(2.66365357834824,0.656086448390735,
7.51860402984325));
#386623=CARTESIAN_POINT('Ctrl Pts',(2.66398476079656,0.656378576191033,
7.51734760759493));
#386624=CARTESIAN_POINT('Ctrl Pts',(2.66432338889996,0.656597936323158,
7.51608817408572));
#386625=CARTESIAN_POINT('Ctrl Pts',(2.66467594396582,0.656732816671575,
7.51481005913119));
#386626=CARTESIAN_POINT('Ctrl Pts',(2.66499529676906,0.656854994514241,
7.51365231206383));
#386627=CARTESIAN_POINT('Ctrl Pts',(2.66532643764435,0.656908261136698,
7.51247773061042));
#386628=CARTESIAN_POINT('Ctrl Pts',(2.66566950096493,0.656855238444899,
7.51129758471022));
#386629=CARTESIAN_POINT('Ctrl Pts',(2.6660958894931,0.656789337294412,7.50983079813402));
#386630=CARTESIAN_POINT('Ctrl Pts',(2.66652509793794,0.656548475546837,
7.50839324291155));
#386631=CARTESIAN_POINT('Ctrl Pts',(2.66691991417319,0.656059002349293,
7.50715379678855));
#386632=CARTESIAN_POINT('Ctrl Pts',(2.66710230789751,0.65583287983586,7.50658120839351));
#386633=CARTESIAN_POINT('Ctrl Pts',(2.66729589496988,0.655515588495312,
7.50598221009429));
#386634=CARTESIAN_POINT('Ctrl Pts',(2.66747665060042,0.655102832213265,
7.50545747549611));
#386635=CARTESIAN_POINT('Ctrl Pts',(2.66757310739979,0.654882572685162,
7.50517746087247));
#386636=CARTESIAN_POINT('Ctrl Pts',(2.66766714172128,0.654632821201721,
7.50491486231392));
#386637=CARTESIAN_POINT('Ctrl Pts',(2.66775470234246,0.65435960385524,7.50468370960993));
#386638=CARTESIAN_POINT('Ctrl Pts',(2.66788563309054,0.653951057740731,
7.50433806340447));
#386639=CARTESIAN_POINT('Ctrl Pts',(2.66800548484691,0.653477622060633,
7.50405484070985));
#386640=CARTESIAN_POINT('Ctrl Pts',(2.66810549133164,0.65297100601611,7.50385766036132));
#386641=CARTESIAN_POINT('Ctrl Pts',(2.66811618547073,0.652916831304736,
7.50383657498792));
#386642=CARTESIAN_POINT('Ctrl Pts',(2.66812666210036,0.652862303928491,
7.50381643264937));
#386643=CARTESIAN_POINT('Ctrl Pts',(2.66813691764825,0.652807481989508,
7.50379723213559));
#386644=CARTESIAN_POINT('Ctrl Pts',(2.66820537678523,0.652441527613342,
7.50366906242519));
#386645=CARTESIAN_POINT('Ctrl Pts',(2.6682647668768,0.652054354948041,7.50358235568538));
#386646=CARTESIAN_POINT('Ctrl Pts',(2.6683130409734,0.651679792103603,7.5035341175365));
#386647=CARTESIAN_POINT('Ctrl Pts',(2.66838542251767,0.651118177510698,
7.50346178989176));
#386648=CARTESIAN_POINT('Ctrl Pts',(2.66843940938489,0.650510930430136,
7.50346967198527));
#386649=CARTESIAN_POINT('Ctrl Pts',(2.66847406487117,0.649913171174646,
7.50354272648692));
#386650=CARTESIAN_POINT('Ctrl Pts',(2.66848831939,0.649667300419978,7.50357277531559));
#386651=CARTESIAN_POINT('Ctrl Pts',(2.66849942595432,0.649423369748924,
7.50361331098761));
#386652=CARTESIAN_POINT('Ctrl Pts',(2.66850780457568,0.649186484967102,
7.50366116523659));
#386653=CARTESIAN_POINT('',(2.60692468992218,0.595013548701134,7.57603338622103));
#386654=CARTESIAN_POINT('Origin',(2.61554070278251,0.596977170861226,7.58486873427627));
#386655=CARTESIAN_POINT('Ctrl Pts',(2.66850780461363,0.649186485008502,
7.50366116529969));
#386656=CARTESIAN_POINT('Ctrl Pts',(2.64801414877486,0.631157678360177,
7.52783573079709));
#386657=CARTESIAN_POINT('Ctrl Pts',(2.62748742494611,0.613100872076781,
7.55196141284068));
#386658=CARTESIAN_POINT('Ctrl Pts',(2.60692469059042,0.595013549759952,
7.57603338728831));
#386659=CARTESIAN_POINT('Ctrl Pts',(2.60040987984641,0.60006631479062,7.59639677331371));
#386660=CARTESIAN_POINT('Ctrl Pts',(2.58423804501348,0.589835470045181,
7.59974925422225));
#386661=CARTESIAN_POINT('Ctrl Pts',(2.60324736190728,0.58763449360278,7.59639677331372));
#386662=CARTESIAN_POINT('Ctrl Pts',(2.59682114589539,0.598537886606984,
7.58707626057423));
#386663=CARTESIAN_POINT('Ctrl Pts',(2.59428415960392,0.592128430143389,
7.58811717123965));
#386664=CARTESIAN_POINT('Ctrl Pts',(2.59935086420695,0.587454466507722,
7.58707626057423));
#386665=CARTESIAN_POINT('Ctrl Pts',(2.60242843340217,0.596196101160384,
7.5801537675693));
#386666=CARTESIAN_POINT('Ctrl Pts',(2.60102225854765,0.593666357257041,
7.58208760766041));
#386667=CARTESIAN_POINT('Ctrl Pts',(2.60338679305817,0.591997253160117,
7.5801537675693));
#386668=CARTESIAN_POINT('Ctrl Pts',(2.60692468911531,0.595013548517179,
7.57603338509286));
#386669=CARTESIAN_POINT('Ctrl Pts',(2.60692468911531,0.595013548517179,
7.57603338509286));
#386670=CARTESIAN_POINT('Ctrl Pts',(2.60692468911531,0.595013548517179,
7.57603338509286));
#386671=CARTESIAN_POINT('Origin',(2.61553943299981,0.59698273414312,7.58486873427623));
#386672=CARTESIAN_POINT('Ctrl Pts',(2.69281955470071,0.562273531831367,
7.51098857897448));
#386673=CARTESIAN_POINT('Ctrl Pts',(2.68715189428301,0.563866685107589,
7.50433767179956));
#386674=CARTESIAN_POINT('Ctrl Pts',(2.68755725624421,0.572465739285978,
7.50214974420965));
#386675=CARTESIAN_POINT('Ctrl Pts',(2.66249358333604,0.570798022904151,
7.53887321589168));
#386676=CARTESIAN_POINT('Ctrl Pts',(2.65689383154843,0.572372087376793,
7.53220407452062));
#386677=CARTESIAN_POINT('Ctrl Pts',(2.6572410742841,0.580944271602793,7.53003438070911));
#386678=CARTESIAN_POINT('Ctrl Pts',(2.63210937491955,0.579338884144357,
7.56669465659231));
#386679=CARTESIAN_POINT('Ctrl Pts',(2.62654271662392,0.580903646188594,
7.560040858333));
#386680=CARTESIAN_POINT('Ctrl Pts',(2.62686733688466,0.589437770151413,
7.55785582193789));
#386681=CARTESIAN_POINT('Ctrl Pts',(2.60166830360741,0.587895729283,7.59443891967696));
#386682=CARTESIAN_POINT('Ctrl Pts',(2.59609357435032,0.589462760037394,
7.58783901202978));
#386683=CARTESIAN_POINT('Ctrl Pts',(2.59643752178506,0.597945735821307,
7.58560008491213));
#386684=CARTESIAN_POINT('',(2.68591391515803,0.572925331695086,7.50366116523517));
#386685=CARTESIAN_POINT('Ctrl Pts',(2.6859139151584,0.572925331695164,7.50366116523554));
#386686=CARTESIAN_POINT('Ctrl Pts',(2.68621818329533,0.572231387592507,
7.50350835821027));
#386687=CARTESIAN_POINT('Ctrl Pts',(2.68647530281419,0.571583585489882,
7.50345484956));
#386688=CARTESIAN_POINT('Ctrl Pts',(2.68669347623158,0.570962887237649,
7.50349758195598));
#386689=CARTESIAN_POINT('Ctrl Pts',(2.68680541537486,0.570644423002071,
7.50351950684424));
#386690=CARTESIAN_POINT('Ctrl Pts',(2.68691825744058,0.57030174753089,7.50357029184312));
#386691=CARTESIAN_POINT('Ctrl Pts',(2.68701798666393,0.569968318478625,
7.50365515313924));
#386692=CARTESIAN_POINT('Ctrl Pts',(2.68717141059381,0.569455369577485,
7.50378570417639));
#386693=CARTESIAN_POINT('Ctrl Pts',(2.68729863666787,0.568949346450696,
7.50400001621911));
#386694=CARTESIAN_POINT('Ctrl Pts',(2.68738777924756,0.568488211200682,
7.50428903009634));
#386695=CARTESIAN_POINT('Ctrl Pts',(2.68739767338808,0.568437028735691,
7.50432110841318));
#386696=CARTESIAN_POINT('Ctrl Pts',(2.68740711999938,0.568386378019464,
7.50435406373354));
#386697=CARTESIAN_POINT('Ctrl Pts',(2.68741611858358,0.568336295066333,
7.50438785222352));
#386698=CARTESIAN_POINT('Ctrl Pts',(2.68747105926538,0.568030514564544,
7.50459414719561));
#386699=CARTESIAN_POINT('Ctrl Pts',(2.68750966597882,0.567740938964541,
7.50483629897752));
#386700=CARTESIAN_POINT('Ctrl Pts',(2.68753176420119,0.567478835738985,
7.5050991045531));
#386701=CARTESIAN_POINT('Ctrl Pts',(2.68758051509931,0.566900609697632,
7.50567888004914));
#386702=CARTESIAN_POINT('Ctrl Pts',(2.68755136067166,0.566433346682598,
7.50637912803144));
#386703=CARTESIAN_POINT('Ctrl Pts',(2.6874735784089,0.566067134736563,7.50710440483569));
#386704=CARTESIAN_POINT('Ctrl Pts',(2.68745450465387,0.56597733229707,7.50728225710685));
#386705=CARTESIAN_POINT('Ctrl Pts',(2.68743226983592,0.565891788322851,
7.50746498566954));
#386706=CARTESIAN_POINT('Ctrl Pts',(2.68740779618352,0.565812394887375,
7.50764697238949));
#386707=CARTESIAN_POINT('Ctrl Pts',(2.68727623256354,0.565385597627915,
7.50862528291181));
#386708=CARTESIAN_POINT('Ctrl Pts',(2.68707198248925,0.565096578290556,
7.50965856837421));
#386709=CARTESIAN_POINT('Ctrl Pts',(2.68683691530922,0.564893933047675,
7.51067959873201));
#386710=CARTESIAN_POINT('Ctrl Pts',(2.68670755754354,0.564782417114912,
7.51124147302578));
#386711=CARTESIAN_POINT('Ctrl Pts',(2.68656855217611,0.564697359785952,
7.51180065547253));
#386712=CARTESIAN_POINT('Ctrl Pts',(2.68642517955058,0.56463231517169,7.51235175716501));
#386713=CARTESIAN_POINT('Ctrl Pts',(2.68592977001648,0.564407560118717,
7.51425603304536));
#386714=CARTESIAN_POINT('Ctrl Pts',(2.68532064255678,0.564400477358233,
7.51626900505182));
#386715=CARTESIAN_POINT('Ctrl Pts',(2.68464456211952,0.564572913161355,
7.51827788969245));
#386716=CARTESIAN_POINT('Ctrl Pts',(2.68460797136864,0.564582245712878,
7.51838661432546));
#386717=CARTESIAN_POINT('Ctrl Pts',(2.68457117888685,0.564592112335995,
7.51849533314857));
#386718=CARTESIAN_POINT('Ctrl Pts',(2.68453419038076,0.564602509634937,
7.51860402984325));
#386719=CARTESIAN_POINT('Ctrl Pts',(2.60692469098486,0.59501354803714,7.57603338728985));
#386720=CARTESIAN_POINT('Ctrl Pts',(2.63329886952168,0.587639269793085,
7.55196141284922));
#386721=CARTESIAN_POINT('Ctrl Pts',(2.65962736329994,0.580276861158748,
7.52783573083105));
#386722=CARTESIAN_POINT('Ctrl Pts',(2.68591391521332,0.57292533167398,7.50366116530176));
#386723=CARTESIAN_POINT('Origin',(9.00812987045921E-16,2.05604685939141E-16,
7.49482233047033));
#386724=CARTESIAN_POINT('Origin',(2.65991946170316,0.647097138961989,7.49482233047033));
#386725=CARTESIAN_POINT('Origin',(0.,0.,7.50366116523517));
#386726=CARTESIAN_POINT('Origin',(2.6772695523474,0.571081425081912,7.49482233047033));
#386727=CARTESIAN_POINT('Ctrl Pts',(2.66365278509062,0.656085748737588,
7.51860402984325));
#386728=CARTESIAN_POINT('Ctrl Pts',(2.66935948430929,0.661118627641139,
7.51860402984325));
#386729=CARTESIAN_POINT('Ctrl Pts',(2.66750981689315,0.668499346879792,
7.51860402984325));
#386730=CARTESIAN_POINT('Ctrl Pts',(2.66577172061454,0.657954491973673,
7.51041458714367));
#386731=CARTESIAN_POINT('Ctrl Pts',(2.66892126731012,0.66286720215976,7.51004642900444));
#386732=CARTESIAN_POINT('Ctrl Pts',(2.66750930677684,0.668501382394517,
7.50729136483012));
#386733=CARTESIAN_POINT('Ctrl Pts',(2.66824761341795,0.656615204093723,
7.50215815450136));
#386734=CARTESIAN_POINT('Ctrl Pts',(2.66981365703399,0.659306964089372,
7.49877163671527));
#386735=CARTESIAN_POINT('Ctrl Pts',(2.66899810433397,0.66265939565286,7.49481588533168));
#386736=CARTESIAN_POINT('Ctrl Pts',(2.66850726965803,0.64918635483347,7.50366171572174));
#386737=CARTESIAN_POINT('Ctrl Pts',(2.67206521266993,0.650051920418061,
7.50000045605858));
#386738=CARTESIAN_POINT('Ctrl Pts',(2.6720652126699,0.650051920418182,7.49482233047317));
#386739=CARTESIAN_POINT('Origin',(2.6553847722709,0.665460713484883,7.51860402984325));
#386740=CARTESIAN_POINT('Origin',(2.6553847722709,0.665460713484883,9.));
#386741=CARTESIAN_POINT('Origin',(2.6553847722709,0.665460713484883,8.75721825406948));
#386742=CARTESIAN_POINT('Ctrl Pts',(2.65112941937648,0.645039239553609,
8.78942910404912));
#386743=CARTESIAN_POINT('Ctrl Pts',(2.65532178526108,0.648710274420148,
8.79672699501691));
#386744=CARTESIAN_POINT('Ctrl Pts',(2.65077470762197,0.656391262047141,
8.79893251111267));
#386745=CARTESIAN_POINT('Ctrl Pts',(2.65937452780626,0.652312038583003,
8.78111911759583));
#386746=CARTESIAN_POINT('Ctrl Pts',(2.6643397222864,0.656669693215929,8.78644465894813));
#386747=CARTESIAN_POINT('Ctrl Pts',(2.66180227631761,0.664368841203266,
8.78817647674132));
#386748=CARTESIAN_POINT('Ctrl Pts',(2.66451307602303,0.656844620434605,
8.76780923932029));
#386749=CARTESIAN_POINT('Ctrl Pts',(2.67037091713223,0.661992477688804,
8.76988516158374));
#386750=CARTESIAN_POINT('Ctrl Pts',(2.66868335772545,0.669360552311447,
8.77093053738833));
#386751=CARTESIAN_POINT('Ctrl Pts',(2.66351112944559,0.655960829007586,
8.75371302330492));
#386752=CARTESIAN_POINT('Ctrl Pts',(2.66922570397851,0.660981769086442,
8.75300828287559));
#386753=CARTESIAN_POINT('Ctrl Pts',(2.66734099870957,0.668387336274949,
8.75267964240738));
#386754=CARTESIAN_POINT('Origin',(2.6448686608445,0.656184713158531,8.78727029226991));
#386755=CARTESIAN_POINT('Ctrl Pts',(2.5995223305943,0.599517869856918,8.85049129520029));
#386756=CARTESIAN_POINT('Ctrl Pts',(2.60390169908879,0.60338080187969,8.85711686593484));
#386757=CARTESIAN_POINT('Ctrl Pts',(2.59985800069652,0.610914012710821,
8.85933012996512));
#386758=CARTESIAN_POINT('Ctrl Pts',(2.61742004498717,0.615304998560444,
8.82945683644722));
#386759=CARTESIAN_POINT('Ctrl Pts',(2.62183576488798,0.619199995254582,
8.83607469902389));
#386760=CARTESIAN_POINT('Ctrl Pts',(2.61774715137786,0.626737586518525,
8.8382956714852));
#386761=CARTESIAN_POINT('Ctrl Pts',(2.63529108139348,0.631068595275567,
8.80838214965002));
#386762=CARTESIAN_POINT('Ctrl Pts',(2.63972422778672,0.634978963445221,
8.81501364461994));
#386763=CARTESIAN_POINT('Ctrl Pts',(2.63560960807689,0.642536656032147,
8.81722098428721));
#386764=CARTESIAN_POINT('Ctrl Pts',(2.65313746692184,0.646810448064383,
8.78727029226991));
#386765=CARTESIAN_POINT('Ctrl Pts',(2.65757134967522,0.650721465759011,
8.79393457792714));
#386766=CARTESIAN_POINT('Ctrl Pts',(2.65344741704445,0.658313079213018,
8.79610912703474));
#386767=CARTESIAN_POINT('Origin',(2.59125352451696,0.608892134951066,8.85049129520029));
#386768=CARTESIAN_POINT('Ctrl Pts',(2.6022097463239,0.587743532225645,8.85049129520029));
#386769=CARTESIAN_POINT('Ctrl Pts',(2.60783148438851,0.586163287511667,
8.85711686593484));
#386770=CARTESIAN_POINT('Ctrl Pts',(2.60745677570886,0.577621604099172,
8.85933012996512));
#386771=CARTESIAN_POINT('Ctrl Pts',(2.5972362758088,0.589141551913027,8.86332496987232));
#386772=CARTESIAN_POINT('Ctrl Pts',(2.59853778293458,0.584707820574949,
8.86648636486737));
#386773=CARTESIAN_POINT('Ctrl Pts',(2.59354792537494,0.581549114601405,
8.87206031107456));
#386774=CARTESIAN_POINT('Ctrl Pts',(2.59562163897866,0.596077166803049,
8.86341338519876));
#386775=CARTESIAN_POINT('Ctrl Pts',(2.59483919973077,0.600644579578093,
8.86654584966058));
#386776=CARTESIAN_POINT('Ctrl Pts',(2.58894560269752,0.601268812545118,
8.87215952290715));
#386777=CARTESIAN_POINT('Ctrl Pts',(2.5995223305943,0.599517869856918,8.85049129520029));
#386778=CARTESIAN_POINT('Ctrl Pts',(2.60390169908879,0.60338080187969,8.85711686593484));
#386779=CARTESIAN_POINT('Ctrl Pts',(2.59985800069652,0.610914012710821,
8.85933012996512));
#386780=CARTESIAN_POINT('Origin',(2.59882715066403,0.575709910717479,8.85049129520029));
#386781=CARTESIAN_POINT('Ctrl Pts',(2.67103479566853,0.568397127400971,
8.78727029226991));
#386782=CARTESIAN_POINT('Ctrl Pts',(2.67672651297435,0.56679721184414,8.79393457792714));
#386783=CARTESIAN_POINT('Ctrl Pts',(2.67630485569206,0.558168097155223,
8.79610912703474));
#386784=CARTESIAN_POINT('Ctrl Pts',(2.64812562395424,0.574836790204019,
8.80838214965003));
#386785=CARTESIAN_POINT('Ctrl Pts',(2.65381639600417,0.573237140354268,
8.81501364461993));
#386786=CARTESIAN_POINT('Ctrl Pts',(2.65338841166109,0.564642628035515,
8.81722098428721));
#386787=CARTESIAN_POINT('Ctrl Pts',(2.6251848082303,0.581285347992641,8.82945683644722));
#386788=CARTESIAN_POINT('Ctrl Pts',(2.63085321011981,0.579691986292097,
8.83607469902389));
#386789=CARTESIAN_POINT('Ctrl Pts',(2.63043993491584,0.57112686830673,8.8382956714852));
#386790=CARTESIAN_POINT('Ctrl Pts',(2.6022097463239,0.587743532225645,8.85049129520029));
#386791=CARTESIAN_POINT('Ctrl Pts',(2.60783148438851,0.586163287511667,
8.85711686593484));
#386792=CARTESIAN_POINT('Ctrl Pts',(2.60745677570886,0.577621604099171,
8.85933012996512));
#386793=CARTESIAN_POINT('Origin',(2.66765220000865,0.556363505892805,8.78727029226991));
#386794=CARTESIAN_POINT('Ctrl Pts',(2.68435593267242,0.564652597894885,
8.75374538247847));
#386795=CARTESIAN_POINT('Ctrl Pts',(2.69167492525666,0.562608893919413,
8.75304829418602));
#386796=CARTESIAN_POINT('Ctrl Pts',(2.69319395121605,0.555128038129891,
8.75272238421917));
#386797=CARTESIAN_POINT('Ctrl Pts',(2.68562666750752,0.564295400620314,
8.7676940844502));
#386798=CARTESIAN_POINT('Ctrl Pts',(2.6931296528189,0.56219960330441,8.76974318093968));
#386799=CARTESIAN_POINT('Ctrl Pts',(2.69480757528628,0.554837339150392,
8.7707786988043));
#386800=CARTESIAN_POINT('Ctrl Pts',(2.67911360463672,0.566126190382139,
8.78108014887992));
#386801=CARTESIAN_POINT('Ctrl Pts',(2.6854731365548,0.564353736974275,8.78639403366327));
#386802=CARTESIAN_POINT('Ctrl Pts',(2.68654558210626,0.55633052463332,8.78812224174741));
#386803=CARTESIAN_POINT('Ctrl Pts',(2.66844013235527,0.569126450616964,
8.78944554828686));
#386804=CARTESIAN_POINT('Ctrl Pts',(2.67380121292356,0.567638084816047,
8.79673892988686));
#386805=CARTESIAN_POINT('Ctrl Pts',(2.67304049616502,0.558754118115881,
8.79894799272499));
#386806=CARTESIAN_POINT('Origin',(2.68115159472089,0.552568888126775,8.75721825406948));
#386807=CARTESIAN_POINT('Origin',(2.68115159472089,0.552568888126775,9.));
#386808=CARTESIAN_POINT('Origin',(2.68115159472089,0.552568888126776,7.51860402984325));
#386809=CARTESIAN_POINT('Ctrl Pts',(2.68591314580245,0.572925167585785,
7.50366195182966));
#386810=CARTESIAN_POINT('Ctrl Pts',(2.6894945274723,0.573689102821876,7.50000065167735));
#386811=CARTESIAN_POINT('Ctrl Pts',(2.68949452747232,0.573689102821761,
7.49482233047108));
#386812=CARTESIAN_POINT('Ctrl Pts',(2.68890430944023,0.566112918346452,
7.50215800491336));
#386813=CARTESIAN_POINT('Ctrl Pts',(2.69148329915018,0.56436548902017,7.49877273257265));
#386814=CARTESIAN_POINT('Ctrl Pts',(2.69220348433873,0.560989324088758,
7.49481816995649));
#386815=CARTESIAN_POINT('Ctrl Pts',(2.68724770526619,0.563840105342118,
7.51043025814043));
#386816=CARTESIAN_POINT('Ctrl Pts',(2.69222164317034,0.560781887116979,
7.51006209594516));
#386817=CARTESIAN_POINT('Ctrl Pts',(2.69339480712793,0.555089553984509,
7.507312818217));
#386818=CARTESIAN_POINT('Ctrl Pts',(2.68453273533962,0.564602918545393,
7.51860402984326));
#386819=CARTESIAN_POINT('Ctrl Pts',(2.69185835200808,0.562544677107289,
7.51860402984327));
#386820=CARTESIAN_POINT('Ctrl Pts',(2.69339429606665,0.555092033734655,
7.51860402984327));
#386821=CARTESIAN_POINT('Origin',(0.,0.,7.5));
#386822=CARTESIAN_POINT('Origin',(2.6345200847159,0.419811799220462,7.5));
#386823=CARTESIAN_POINT('',(2.6345200847159,0.419811799220462,7.59394543036555));
#386824=CARTESIAN_POINT('',(2.6345200847159,0.419811799220462,8.85049129520029));
#386825=CARTESIAN_POINT('',(2.6345200847159,0.419811799220462,7.5));
#386826=CARTESIAN_POINT('',(2.70196419720223,0.396095507607702,8.78727029226991));
#386827=CARTESIAN_POINT('Ctrl Pts',(2.6345200847159,0.419811799220462,8.85049129520029));
#386828=CARTESIAN_POINT('Ctrl Pts',(2.65703413439438,0.41189487737399,8.82945686509571));
#386829=CARTESIAN_POINT('Ctrl Pts',(2.67951471421565,0.403989724989143,
8.80838212259895));
#386830=CARTESIAN_POINT('Ctrl Pts',(2.70196419720223,0.396095507607702,
8.78727029226991));
#386831=CARTESIAN_POINT('',(2.71519273396521,0.391443777102025,8.75721825406948));
#386832=CARTESIAN_POINT('Origin',(2.67538354477845,0.405442638265208,8.75937679713132));
#386833=CARTESIAN_POINT('',(2.71519273396521,0.391443777102025,7.51860402984325));
#386834=CARTESIAN_POINT('',(2.71519273396521,0.391443777102025,7.5));
#386835=CARTESIAN_POINT('Ctrl Pts',(2.71519273396521,0.391443777102025,
7.51860402984325));
#386836=CARTESIAN_POINT('Ctrl Pts',(2.70480377576452,0.395096987933295,
7.52834476460825));
#386837=CARTESIAN_POINT('Ctrl Pts',(2.69440807320208,0.398752570376327,
7.53807742314407));
#386838=CARTESIAN_POINT('Ctrl Pts',(2.68400539982696,0.402410604061131,
7.54780169004674));
#386839=CARTESIAN_POINT('Ctrl Pts',(2.6675281274173,0.40820473171801,7.5632044032688));
#386840=CARTESIAN_POINT('Ctrl Pts',(2.65103334518628,0.414005016591771,
7.57858609112103));
#386841=CARTESIAN_POINT('Ctrl Pts',(2.6345200847159,0.419811799220462,7.59394543036555));
#386842=CARTESIAN_POINT('Origin',(2.85005793045282,0.60006065396636,7.5));
#386843=CARTESIAN_POINT('',(2.70021641947034,0.484077577700278,8.75721825406948));
#386844=CARTESIAN_POINT('',(2.68912759914126,0.475494405483876,8.78727029226991));
#386845=CARTESIAN_POINT('Origin',(2.66098003722313,0.453707113035681,8.75658640621088));
#386846=CARTESIAN_POINT('',(2.6325925749723,0.431734128529253,8.85049129520029));
#386847=CARTESIAN_POINT('Ctrl Pts',(2.68912759914126,0.475494405483876,
8.78727029226991));
#386848=CARTESIAN_POINT('Ctrl Pts',(2.67030932106718,0.460928336530414,
8.80838212259895));
#386849=CARTESIAN_POINT('Ctrl Pts',(2.65146497607287,0.446342090780963,
8.82945686509571));
#386850=CARTESIAN_POINT('Ctrl Pts',(2.6325925749723,0.431734128529253,8.85049129520029));
#386851=CARTESIAN_POINT('',(2.6325925749723,0.431734128529253,7.59394543036555));
#386852=CARTESIAN_POINT('',(2.6325925749723,0.431734128529253,7.5));
#386853=CARTESIAN_POINT('',(2.70021641947034,0.484077577700278,7.51860402984325));
#386854=CARTESIAN_POINT('Ctrl Pts',(2.6325925749723,0.431734128529252,7.59394543036555));
#386855=CARTESIAN_POINT('Ctrl Pts',(2.64643481479702,0.442448553035235,
7.57858609112103));
#386856=CARTESIAN_POINT('Ctrl Pts',(2.6602615652383,0.453150988164354,7.56320440326857));
#386857=CARTESIAN_POINT('Ctrl Pts',(2.67407363807278,0.463842062262924,
7.54780169004651));
#386858=CARTESIAN_POINT('Ctrl Pts',(2.68279367854782,0.470591708024162,
7.53807742314383));
#386859=CARTESIAN_POINT('Ctrl Pts',(2.69150787573962,0.477336830860077,
7.52834476460825));
#386860=CARTESIAN_POINT('Ctrl Pts',(2.70021641947034,0.484077577700278,
7.51860402984325));
#386861=CARTESIAN_POINT('',(2.70021641947034,0.484077577700278,7.5));
#386862=CARTESIAN_POINT('Origin',(2.63680073810823,0.42629749464224,7.5));
#386863=CARTESIAN_POINT('Ctrl Pts',(2.6325925749723,0.431734128529253,8.85049129520029));
#386864=CARTESIAN_POINT('Ctrl Pts',(2.6324394307242,0.431615589007792,8.85097269580138));
#386865=CARTESIAN_POINT('Ctrl Pts',(2.63229336726998,0.431491893478853,
8.85143669361005));
#386866=CARTESIAN_POINT('Ctrl Pts',(2.63214822387277,0.431356678978386,
8.8519052845931));
#386867=CARTESIAN_POINT('Ctrl Pts',(2.63186433259248,0.431092207990465,
8.85282181883899));
#386868=CARTESIAN_POINT('Ctrl Pts',(2.63159139830333,0.430790328371211,
8.85372622499636));
#386869=CARTESIAN_POINT('Ctrl Pts',(2.63133657541701,0.430435962534942,
8.85462257735071));
#386870=CARTESIAN_POINT('Ctrl Pts',(2.63112503050723,0.430141780603558,
8.85536669723987));
#386871=CARTESIAN_POINT('Ctrl Pts',(2.63092589359264,0.429811377957262,
8.85610498449051));
#386872=CARTESIAN_POINT('Ctrl Pts',(2.63075009497682,0.429431969215917,
8.85681338218371));
#386873=CARTESIAN_POINT('Ctrl Pts',(2.63059055745687,0.429087655187274,
8.85745625420284));
#386874=CARTESIAN_POINT('Ctrl Pts',(2.63044769614054,0.428698914290614,
8.85808743050665));
#386875=CARTESIAN_POINT('Ctrl Pts',(2.63034146522524,0.428245260526937,
8.85866804508409));
#386876=CARTESIAN_POINT('Ctrl Pts',(2.63029245258373,0.428035954514381,
8.85893592806395));
#386877=CARTESIAN_POINT('Ctrl Pts',(2.63025142607327,0.427812678304184,
8.85919241173848));
#386878=CARTESIAN_POINT('Ctrl Pts',(2.63022171543869,0.42757260085838,8.85943017985534));
#386879=CARTESIAN_POINT('Ctrl Pts',(2.63018159728671,0.427248425236019,
8.8597512372));
#386880=CARTESIAN_POINT('Ctrl Pts',(2.63016172595496,0.426885286146255,
8.86004599534705));
#386881=CARTESIAN_POINT('Ctrl Pts',(2.63017273972451,0.426486977495848,
8.86026130871721));
#386882=CARTESIAN_POINT('Ctrl Pts',(2.63017677217606,0.426341145469424,
8.86034014101235));
#386883=CARTESIAN_POINT('Ctrl Pts',(2.63018499302247,0.426188408071798,
8.86040910639693));
#386884=CARTESIAN_POINT('Ctrl Pts',(2.63019751418393,0.42603294462651,8.86046313645507));
#386885=CARTESIAN_POINT('Ctrl Pts',(2.63021705335152,0.425790345222132,
8.8605474499083));
#386886=CARTESIAN_POINT('Ctrl Pts',(2.63024774428927,0.425534497097221,
8.86059655985668));
#386887=CARTESIAN_POINT('Ctrl Pts',(2.6302873278218,0.425281773678598,8.86059725258816));
#386888=CARTESIAN_POINT('Ctrl Pts',(2.6303270028081,0.425028466367915,8.86059794692011));
#386889=CARTESIAN_POINT('Ctrl Pts',(2.6303786762971,0.424775900125062,8.86056369958366));
#386890=CARTESIAN_POINT('Ctrl Pts',(2.63043584326273,0.42453709575363,8.86048590497774));
#386891=CARTESIAN_POINT('Ctrl Pts',(2.6304507621387,0.424474774922749,8.86046560290182));
#386892=CARTESIAN_POINT('Ctrl Pts',(2.6304663373265,0.424412601679696,8.86044257503091));
#386893=CARTESIAN_POINT('Ctrl Pts',(2.63048205569772,0.424352489252271,
8.86041778462584));
#386894=CARTESIAN_POINT('Ctrl Pts',(2.63058782083114,0.423948007209002,
8.86025097596201));
#386895=CARTESIAN_POINT('Ctrl Pts',(2.63071458213298,0.42358263889542,8.8599848982295));
#386896=CARTESIAN_POINT('Ctrl Pts',(2.63085063533997,0.423264271385145,
8.85968173251462));
#386897=CARTESIAN_POINT('Ctrl Pts',(2.63092259969155,0.423095873212493,
8.85952137522077));
#386898=CARTESIAN_POINT('Ctrl Pts',(2.63099837530336,0.42293730390483,8.85934740853961));
#386899=CARTESIAN_POINT('Ctrl Pts',(2.63107549094398,0.422790129365309,
8.8591675900182));
#386900=CARTESIAN_POINT('Ctrl Pts',(2.63138515032498,0.422199147089328,
8.85844552518695));
#386901=CARTESIAN_POINT('Ctrl Pts',(2.63173123784028,0.421757093262747,
8.85759444184125));
#386902=CARTESIAN_POINT('Ctrl Pts',(2.63204579283192,0.42142201205954,8.85683498915139));
#386903=CARTESIAN_POINT('Ctrl Pts',(2.63207871017407,0.421386946704019,
8.85675551444998));
#386904=CARTESIAN_POINT('Ctrl Pts',(2.63211129380288,0.421353069065494,
8.85667699793651));
#386905=CARTESIAN_POINT('Ctrl Pts',(2.63214347290436,0.421320342132163,
8.85659965593547));
#386906=CARTESIAN_POINT('Ctrl Pts',(2.63257782805809,0.420878592316094,
8.85555568965886));
#386907=CARTESIAN_POINT('Ctrl Pts',(2.63305906768579,0.420516772853024,
8.85434650606346));
#386908=CARTESIAN_POINT('Ctrl Pts',(2.63358583604685,0.420228127733434,
8.85297329937117));
#386909=CARTESIAN_POINT('Ctrl Pts',(2.63388211115348,0.42006578244107,8.85220095427747));
#386910=CARTESIAN_POINT('Ctrl Pts',(2.63419306117444,0.419926794961197,
8.85137579139183));
#386911=CARTESIAN_POINT('Ctrl Pts',(2.6345200847159,0.419811799220462,8.85049129520029));
#386912=CARTESIAN_POINT('Origin',(2.63680073810823,0.42629749464224,7.59394543036555));
#386913=CARTESIAN_POINT('Ctrl Pts',(2.63214794555735,0.431389968309522,
7.59443877723642));
#386914=CARTESIAN_POINT('Ctrl Pts',(2.62756869039428,0.427845449188369,
7.58783886950016));
#386915=CARTESIAN_POINT('Ctrl Pts',(2.63107088212544,0.42011150875578,7.58559994247159));
#386916=CARTESIAN_POINT('Ctrl Pts',(2.65714596514289,0.45073939420012,7.56670252222134));
#386917=CARTESIAN_POINT('Ctrl Pts',(2.65257332830363,0.447199997915403,
7.56004874999029));
#386918=CARTESIAN_POINT('Ctrl Pts',(2.65607680870819,0.439411417665382,
7.55786368756704));
#386919=CARTESIAN_POINT('Ctrl Pts',(2.68209730342447,0.47005268697112,7.53888913333559));
#386920=CARTESIAN_POINT('Ctrl Pts',(2.67749749118058,0.466492255880997,
7.53222002137278));
#386921=CARTESIAN_POINT('Ctrl Pts',(2.68103621251043,0.458676893057078,
7.53005029815327));
#386922=CARTESIAN_POINT('Ctrl Pts',(2.70700083133714,0.48932897268294,7.51101258149734));
#386923=CARTESIAN_POINT('Ctrl Pts',(2.70234526101077,0.485725382698534,
7.5043616886572));
#386924=CARTESIAN_POINT('Ctrl Pts',(2.70594791084534,0.477906917650063,
7.50217374673251));
#386925=CARTESIAN_POINT('',(2.70461858999357,0.476880779649044,7.50366116523517));
#386926=CARTESIAN_POINT('Ctrl Pts',(2.70021641947034,0.484077577700279,
7.51860402984325));
#386927=CARTESIAN_POINT('Ctrl Pts',(2.70056563816122,0.484347886360363,
7.51734760759493));
#386928=CARTESIAN_POINT('Ctrl Pts',(2.70091762496878,0.484545099816493,
7.51608817408572));
#386929=CARTESIAN_POINT('Ctrl Pts',(2.70127809748605,0.484657114758144,
7.51481005913119));
#386930=CARTESIAN_POINT('Ctrl Pts',(2.70160462210596,0.484758580568974,
7.51365231206383));
#386931=CARTESIAN_POINT('Ctrl Pts',(2.70193849542102,0.484790521480719,
7.51247773061042));
#386932=CARTESIAN_POINT('Ctrl Pts',(2.70227745670569,0.48471562758731,7.51129758471022));
#386933=CARTESIAN_POINT('Ctrl Pts',(2.70269874687169,0.484622543031008,
7.50983079813402));
#386934=CARTESIAN_POINT('Ctrl Pts',(2.70311164139659,0.484354676680247,
7.50839324291155));
#386935=CARTESIAN_POINT('Ctrl Pts',(2.7034742857841,0.48384091319484,7.50715379678855));
#386936=CARTESIAN_POINT('Ctrl Pts',(2.70364181704178,0.483603569268321,
7.50658120839351));
#386937=CARTESIAN_POINT('Ctrl Pts',(2.70381467744276,0.483274526670549,
7.50598221009429));
#386938=CARTESIAN_POINT('Ctrl Pts',(2.70396861630568,0.482851037387539,
7.50545747549611));
#386939=CARTESIAN_POINT('Ctrl Pts',(2.70405076284779,0.482625050397906,
7.50517746087247));
#386940=CARTESIAN_POINT('Ctrl Pts',(2.7041286023332,0.482369787256009,7.50491486231392));
#386941=CARTESIAN_POINT('Ctrl Pts',(2.7041984779562,0.482091521235608,7.50468370960993));
#386942=CARTESIAN_POINT('Ctrl Pts',(2.70430296405359,0.481675425761071,
7.50433806340447));
#386943=CARTESIAN_POINT('Ctrl Pts',(2.7043922364335,0.481195283876951,7.50405484070984));
#386944=CARTESIAN_POINT('Ctrl Pts',(2.70445957844276,0.480683301291942,
7.50385766036131));
#386945=CARTESIAN_POINT('Ctrl Pts',(2.70446677962392,0.480628552712486,
7.50383657498791));
#386946=CARTESIAN_POINT('Ctrl Pts',(2.70447374114721,0.480573466128624,
7.50381643264937));
#386947=CARTESIAN_POINT('Ctrl Pts',(2.70448046317028,0.480518099751992,
7.50379723213559));
#386948=CARTESIAN_POINT('Ctrl Pts',(2.70452533487324,0.480148511076374,
7.50366906242519));
#386949=CARTESIAN_POINT('Ctrl Pts',(2.70455979670366,0.479758328762606,
7.50358235568538));
#386950=CARTESIAN_POINT('Ctrl Pts',(2.70458397329211,0.479381442565715,
7.5035341175365));
#386951=CARTESIAN_POINT('Ctrl Pts',(2.70462022335022,0.47881634436876,7.50346178989176));
#386952=CARTESIAN_POINT('Ctrl Pts',(2.7046351928416,0.478206885991993,7.50346967198527));
#386953=CARTESIAN_POINT('Ctrl Pts',(2.70463147855747,0.477608134512373,
7.50354272648692));
#386954=CARTESIAN_POINT('Ctrl Pts',(2.70462995079553,0.477361855635383,
7.50357277531559));
#386955=CARTESIAN_POINT('Ctrl Pts',(2.70462540584846,0.477117714546036,
7.50361331098761));
#386956=CARTESIAN_POINT('Ctrl Pts',(2.70461858999496,0.47688077964929,7.50366116523658));
#386957=CARTESIAN_POINT('',(2.63969113251172,0.426764791193857,7.57603338622103));
#386958=CARTESIAN_POINT('Origin',(2.64841525255361,0.428172349042287,7.5848687342763));
#386959=CARTESIAN_POINT('Ctrl Pts',(2.70461859003549,0.476880779688174,
7.50366116529968));
#386960=CARTESIAN_POINT('Ctrl Pts',(2.68301193100262,0.460202048194502,
7.52783573079709));
#386961=CARTESIAN_POINT('Ctrl Pts',(2.66137047797874,0.44349749326739,7.55196141284069));
#386962=CARTESIAN_POINT('Ctrl Pts',(2.63969113324643,0.426764792207688,
7.57603338728831));
#386963=CARTESIAN_POINT('Ctrl Pts',(2.63351343964686,0.432224581148209,
7.59639677331371));
#386964=CARTESIAN_POINT('Ctrl Pts',(2.6174729176982,0.423462528228453,7.59959882295468));
#386965=CARTESIAN_POINT('Ctrl Pts',(2.63537086205299,0.419671433336357,
7.59642833564546));
#386966=CARTESIAN_POINT('Ctrl Pts',(2.62983415240467,0.430929224257913,
7.58707626057421));
#386967=CARTESIAN_POINT('Ctrl Pts',(2.62694184795774,0.424801674501049,
7.58809943920599));
#386968=CARTESIAN_POINT('Ctrl Pts',(2.63152868410626,0.419834247104491,
7.58710240504252));
#386969=CARTESIAN_POINT('Ctrl Pts',(2.63527988042916,0.428232990116564,
7.58015376756929));
#386970=CARTESIAN_POINT('Ctrl Pts',(2.63373782678302,0.425834794555615,
7.58205880659761));
#386971=CARTESIAN_POINT('Ctrl Pts',(2.6359024780102,0.424034416788969,7.58020924244127));
#386972=CARTESIAN_POINT('Ctrl Pts',(2.63969113169473,0.426764791061976,
7.57603338509286));
#386973=CARTESIAN_POINT('Ctrl Pts',(2.63969113169473,0.426764791061976,
7.57603338509286));
#386974=CARTESIAN_POINT('Ctrl Pts',(2.63969113169473,0.426764791061976,
7.57603338509286));
#386975=CARTESIAN_POINT('Origin',(2.64841434182079,0.428177982249355,7.58486873427618));
#386976=CARTESIAN_POINT('Ctrl Pts',(2.72331185699535,0.388588739318531,
7.51098857897448));
#386977=CARTESIAN_POINT('Ctrl Pts',(2.71775791507471,0.39054174754022,7.50433767179956));
#386978=CARTESIAN_POINT('Ctrl Pts',(2.71871338746911,0.399097162409528,
7.50214974420965));
#386979=CARTESIAN_POINT('Ctrl Pts',(2.69359435960956,0.399038707566622,
7.53887321589169));
#386980=CARTESIAN_POINT('Ctrl Pts',(2.6881069637696,0.400968315283842,7.53220407452063));
#386981=CARTESIAN_POINT('Ctrl Pts',(2.68900271478691,0.409500639119538,
7.53003438070911));
#386982=CARTESIAN_POINT('Ctrl Pts',(2.66381979366645,0.409508743608587,
7.56669465659231));
#386983=CARTESIAN_POINT('Ctrl Pts',(2.65836482731568,0.411426947702931,
7.56004085833299));
#386984=CARTESIAN_POINT('Ctrl Pts',(2.65923556380893,0.419922738901277,
7.55785582193789));
#386985=CARTESIAN_POINT('Ctrl Pts',(2.63398950575049,0.419998373926593,
7.59443891967696));
#386986=CARTESIAN_POINT('Ctrl Pts',(2.62852663037769,0.421919359178073,
7.58783901202978));
#386987=CARTESIAN_POINT('Ctrl Pts',(2.6294133772601,0.430362868990635,7.58560008491213));
#386988=CARTESIAN_POINT('',(2.7171028689902,0.399661099761635,7.50366116523517));
#386989=CARTESIAN_POINT('Ctrl Pts',(2.71710286899057,0.399661099761689,
7.50366116523554));
#386990=CARTESIAN_POINT('Ctrl Pts',(2.71736205082467,0.39894908691515,7.50350835821027));
#386991=CARTESIAN_POINT('Ctrl Pts',(2.71757713724068,0.398286142087287,
7.50345484956));
#386992=CARTESIAN_POINT('Ctrl Pts',(2.71775509412383,0.397652740707336,
7.50349758195598));
#386993=CARTESIAN_POINT('Ctrl Pts',(2.71784639920251,0.397327758825151,
7.50351950684424));
#386994=CARTESIAN_POINT('Ctrl Pts',(2.71793705412928,0.396978557601504,
7.50357029184312));
#386995=CARTESIAN_POINT('Ctrl Pts',(2.71801521557552,0.396639423941707,
7.50365515313923));
#386996=CARTESIAN_POINT('Ctrl Pts',(2.71813545953054,0.39611769904416,7.50378570417639));
#386997=CARTESIAN_POINT('Ctrl Pts',(2.71823000319194,0.395604564193603,
7.50400001621911));
#386998=CARTESIAN_POINT('Ctrl Pts',(2.71828941758173,0.395138665010726,
7.50428903009634));
#386999=CARTESIAN_POINT('Ctrl Pts',(2.71829601212189,0.395086953785839,
7.50432110841318));
#387000=CARTESIAN_POINT('Ctrl Pts',(2.71830219412158,0.395035801890477,
7.50435406373354));
#387001=CARTESIAN_POINT('Ctrl Pts',(2.7183079653914,0.394985245296876,7.50438785222351));
#387002=CARTESIAN_POINT('Ctrl Pts',(2.71834320176766,0.394676572992355,
7.50459414719561));
#387003=CARTESIAN_POINT('Ctrl Pts',(2.71836317598707,0.394385118815853,
7.50483629897752));
#387004=CARTESIAN_POINT('Ctrl Pts',(2.71836843579496,0.394122138271516,
7.50509910455309));
#387005=CARTESIAN_POINT('Ctrl Pts',(2.71838003945946,0.393541976776812,
7.50567888004914));
#387006=CARTESIAN_POINT('Ctrl Pts',(2.71832100728855,0.393077541734351,
7.50637912803144));
#387007=CARTESIAN_POINT('Ctrl Pts',(2.71821992155784,0.392717065736721,
7.50710440483569));
#387008=CARTESIAN_POINT('Ctrl Pts',(2.71819513332984,0.392628669865651,
7.50728225710685));
#387009=CARTESIAN_POINT('Ctrl Pts',(2.71816746337446,0.392544726240379,
7.50746498566954));
#387010=CARTESIAN_POINT('Ctrl Pts',(2.71813795325093,0.392467063959524,
7.50764697238949));
#387011=CARTESIAN_POINT('Ctrl Pts',(2.71797931494821,0.39204957291088,7.50862528291182));
#387012=CARTESIAN_POINT('Ctrl Pts',(2.71775696699509,0.391774233741938,
7.50965856837421));
#387013=CARTESIAN_POINT('Ctrl Pts',(2.71750939926049,0.391587065661377,
7.51067959873202));
#387014=CARTESIAN_POINT('Ctrl Pts',(2.71737316242388,0.391484066830562,
7.51124147302578));
#387015=CARTESIAN_POINT('Ctrl Pts',(2.7172289930161,0.391408090365477,7.51180065547253));
#387016=CARTESIAN_POINT('Ctrl Pts',(2.71708174754226,0.391352365308008,
7.51235175716501));
#387017=CARTESIAN_POINT('Ctrl Pts',(2.71657295577451,0.391159813036229,
7.51425603304535));
#387018=CARTESIAN_POINT('Ctrl Pts',(2.71596462603848,0.391191771758375,
7.51626900505179));
#387019=CARTESIAN_POINT('Ctrl Pts',(2.71530098268083,0.391407169895982,
7.51827788969241));
#387020=CARTESIAN_POINT('Ctrl Pts',(2.7152650650482,0.391418827650236,7.51838661432544));
#387021=CARTESIAN_POINT('Ctrl Pts',(2.71522898031722,0.391431031303721,
7.51849533314856));
#387022=CARTESIAN_POINT('Ctrl Pts',(2.71519273396521,0.391443777102021,
7.51860402984325));
#387023=CARTESIAN_POINT('Ctrl Pts',(2.63969113352968,0.42676479046314,7.57603338728985));
#387024=CARTESIAN_POINT('Ctrl Pts',(2.66553865185877,0.417715864043958,
7.55196141284922));
#387025=CARTESIAN_POINT('Ctrl Pts',(2.69134133978206,0.408681709879649,
7.52783573083105));
#387026=CARTESIAN_POINT('Ctrl Pts',(2.71710286904403,0.39966109973703,7.50366116530176));
#387027=CARTESIAN_POINT('Origin',(9.12135307609332E-16,1.4746696281933E-16,
7.49482233047033));
#387028=CARTESIAN_POINT('Origin',(2.69591402793581,0.475345983446739,7.49482233047033));
#387029=CARTESIAN_POINT('Origin',(0.,0.,7.50366116523517));
#387030=CARTESIAN_POINT('Origin',(2.70835812744774,0.398374827879226,7.49482233047033));
#387031=CARTESIAN_POINT('Ctrl Pts',(2.70021558301562,0.484076930308837,
7.51860402984325));
#387032=CARTESIAN_POINT('Ctrl Pts',(2.70623301486718,0.488733839148602,
7.51860402984325));
#387033=CARTESIAN_POINT('Ctrl Pts',(2.70486003209636,0.49621790250624,7.51860402984325));
#387034=CARTESIAN_POINT('Ctrl Pts',(2.70244989574947,0.485806073346375,
7.51041458714366));
#387035=CARTESIAN_POINT('Ctrl Pts',(2.70590772978589,0.490506897692874,
7.51004642900444));
#387036=CARTESIAN_POINT('Ctrl Pts',(2.70485965344402,0.496219966522045,
7.50729136483011));
#387037=CARTESIAN_POINT('Ctrl Pts',(2.70483489309648,0.484310906180456,
7.50215815450137));
#387038=CARTESIAN_POINT('Ctrl Pts',(2.70657018076301,0.48689679890752,7.49877163671527));
#387039=CARTESIAN_POINT('Ctrl Pts',(2.70597109473123,0.49029459518171,7.49481588533168));
#387040=CARTESIAN_POINT('Ctrl Pts',(2.70461804783867,0.476880684055324,
7.50366171572174));
#387041=CARTESIAN_POINT('Ctrl Pts',(2.70822413765248,0.477516513051137,
7.50000045605858));
#387042=CARTESIAN_POINT('Ctrl Pts',(2.70822413765245,0.47751651305126,7.49482233047317));
#387043=CARTESIAN_POINT('Origin',(2.69256521376865,0.493962366585757,7.51860402984325));
#387044=CARTESIAN_POINT('Origin',(2.69256521376865,0.493962366585757,9.));
#387045=CARTESIAN_POINT('Origin',(2.69256521376865,0.493962366585757,8.75721825406948));
#387046=CARTESIAN_POINT('Ctrl Pts',(2.68701019562603,0.473855492158912,
8.78942910404912));
#387047=CARTESIAN_POINT('Ctrl Pts',(2.69142915185674,0.477250378686132,
8.7967269950169));
#387048=CARTESIAN_POINT('Ctrl Pts',(2.68738353924325,0.485206917164866,
8.79893251111267));
#387049=CARTESIAN_POINT('Ctrl Pts',(2.69570433342994,0.480585082531835,
8.78111911759583));
#387050=CARTESIAN_POINT('Ctrl Pts',(2.70093852227643,0.484615662793375,
8.78644465894813));
#387051=CARTESIAN_POINT('Ctrl Pts',(2.69889957586775,0.492461566776851,
8.78817647674131));
#387052=CARTESIAN_POINT('Ctrl Pts',(2.7011227274646,0.484779123793268,8.76780923932029));
#387053=CARTESIAN_POINT('Ctrl Pts',(2.7072983573577,0.489541091054149,8.76988516158374));
#387054=CARTESIAN_POINT('Ctrl Pts',(2.70608633938462,0.497002149479685,
8.77093053738834));
#387055=CARTESIAN_POINT('Ctrl Pts',(2.70006621478272,0.483961343148155,
8.75371302330491));
#387056=CARTESIAN_POINT('Ctrl Pts',(2.70609074084473,0.488605833119703,
8.75300828287559));
#387057=CARTESIAN_POINT('Ctrl Pts',(2.70468438422376,0.496116938257354,
8.75267964240738));
#387058=CARTESIAN_POINT('Origin',(2.68147639343957,0.485379194369355,8.78727029226991));
#387059=CARTESIAN_POINT('Ctrl Pts',(2.6325925749723,0.431734128529253,8.85049129520029));
#387060=CARTESIAN_POINT('Ctrl Pts',(2.637210444489,0.435308536641068,8.85711686593484));
#387061=CARTESIAN_POINT('Ctrl Pts',(2.63365770878388,0.44308535032814,8.85933012996512));
#387062=CARTESIAN_POINT('Ctrl Pts',(2.65146500140033,0.446342110385393,
8.82945683644723));
#387063=CARTESIAN_POINT('Ctrl Pts',(2.65612120202604,0.449946188245652,
8.8360746990239));
#387064=CARTESIAN_POINT('Ctrl Pts',(2.65252392414127,0.457730251086974,
8.8382956714852));
#387065=CARTESIAN_POINT('Ctrl Pts',(2.6703092969549,0.460928317866582,8.80838214965001));
#387066=CARTESIAN_POINT('Ctrl Pts',(2.67498387312226,0.464546619100827,
8.81501364461995));
#387067=CARTESIAN_POINT('Ctrl Pts',(2.6713619303665,0.472352408187726,8.81722098428721));
#387068=CARTESIAN_POINT('Ctrl Pts',(2.68912759914126,0.475494405483876,
8.78727029226991));
#387069=CARTESIAN_POINT('Ctrl Pts',(2.69380295177103,0.479113307729818,
8.79393457792714));
#387070=CARTESIAN_POINT('Ctrl Pts',(2.69017388854614,0.486953544670625,
8.79610912703474));
#387071=CARTESIAN_POINT('Origin',(2.62494136927061,0.441618917414731,8.85049129520029));
#387072=CARTESIAN_POINT('Ctrl Pts',(2.6345200847159,0.419811799220462,8.85049129520029));
#387073=CARTESIAN_POINT('Ctrl Pts',(2.64002902569027,0.417874615294257,
8.85711686593484));
#387074=CARTESIAN_POINT('Ctrl Pts',(2.63910781935455,0.409374489353958,
8.85933012996512));
#387075=CARTESIAN_POINT('Ctrl Pts',(2.62964640415828,0.421525597876429,
8.86332496987232));
#387076=CARTESIAN_POINT('Ctrl Pts',(2.63066116705591,0.417017588267043,
8.86648636486738));
#387077=CARTESIAN_POINT('Ctrl Pts',(2.62547918270721,0.41418507346522,8.87206031107457));
#387078=CARTESIAN_POINT('Ctrl Pts',(2.62847945114438,0.428550412938709,
8.86341338519876));
#387079=CARTESIAN_POINT('Ctrl Pts',(2.62799125464308,0.43315857252909,8.86654584966058));
#387080=CARTESIAN_POINT('Ctrl Pts',(2.62214976138055,0.434159127000924,
8.87215952290714));
#387081=CARTESIAN_POINT('Ctrl Pts',(2.6325925749723,0.431734128529253,8.85049129520029));
#387082=CARTESIAN_POINT('Ctrl Pts',(2.637210444489,0.435308536641068,8.85711686593484));
#387083=CARTESIAN_POINT('Ctrl Pts',(2.63365770878387,0.44308535032814,8.85933012996512));
#387084=CARTESIAN_POINT('Origin',(2.6303734421844,0.408019625726321,8.85049129520029));
#387085=CARTESIAN_POINT('Ctrl Pts',(2.70196419720223,0.396095507607702,
8.78727029226991));
#387086=CARTESIAN_POINT('Ctrl Pts',(2.70754171332274,0.394134209669121,
8.79393457792714));
#387087=CARTESIAN_POINT('Ctrl Pts',(2.70656805310419,0.385549840096635,
8.79610912703474));
#387088=CARTESIAN_POINT('Ctrl Pts',(2.67951468545062,0.403989735104181,
8.80838214965002));
#387089=CARTESIAN_POINT('Ctrl Pts',(2.68509127528127,0.402028762889524,
8.81501364461993));
#387090=CARTESIAN_POINT('Ctrl Pts',(2.68411351798303,0.393479329969083,
8.81722098428721));
#387091=CARTESIAN_POINT('Ctrl Pts',(2.65703416460906,0.411894866749188,
8.82945683644722));
#387092=CARTESIAN_POINT('Ctrl Pts',(2.66258883312431,0.409941603025147,
8.8360746990239));
#387093=CARTESIAN_POINT('Ctrl Pts',(2.66162763804507,0.401420561626523,
8.8382956714852));
#387094=CARTESIAN_POINT('Ctrl Pts',(2.6345200847159,0.419811799220462,8.85049129520029));
#387095=CARTESIAN_POINT('Ctrl Pts',(2.64002902569027,0.417874615294257,
8.85711686593484));
#387096=CARTESIAN_POINT('Ctrl Pts',(2.63910781935455,0.409374489353958,
8.85933012996512));
#387097=CARTESIAN_POINT('Origin',(2.69781755467072,0.384303334113561,8.78727029226991));
#387098=CARTESIAN_POINT('Ctrl Pts',(2.71501805167228,0.391505183460855,
8.75374538247848));
#387099=CARTESIAN_POINT('Ctrl Pts',(2.72219106603803,0.38899674902948,8.75304829418602));
#387100=CARTESIAN_POINT('Ctrl Pts',(2.72322767091958,0.381433939133116,
8.75272238421917));
#387101=CARTESIAN_POINT('Ctrl Pts',(2.71626328993838,0.391067303825981,
8.76769408445022));
#387102=CARTESIAN_POINT('Ctrl Pts',(2.72361658136666,0.388495094631037,
8.76974318093969));
#387103=CARTESIAN_POINT('Ctrl Pts',(2.72481935447853,0.381040452176713,
8.7707786988043));
#387104=CARTESIAN_POINT('Ctrl Pts',(2.70988090795657,0.393311625404765,
8.78108014887987));
#387105=CARTESIAN_POINT('Ctrl Pts',(2.71611381205456,0.391135357083546,
8.78639403366325));
#387106=CARTESIAN_POINT('Ctrl Pts',(2.71667000517195,0.383059917470437,
8.78812224174741));
#387107=CARTESIAN_POINT('Ctrl Pts',(2.69942159280191,0.396989573000186,
8.78944554828686));
#387108=CARTESIAN_POINT('Ctrl Pts',(2.70467629853092,0.395160779595101,
8.79673892988685));
#387109=CARTESIAN_POINT('Ctrl Pts',(2.70334794704577,0.386343805247372,
8.79894799272499));
#387110=CARTESIAN_POINT('Origin',(2.71104609143371,0.379651603607884,8.75721825406948));
#387111=CARTESIAN_POINT('Origin',(2.71104609143371,0.379651603607884,9.));
#387112=CARTESIAN_POINT('Origin',(2.71104609143371,0.379651603607884,7.51860402984325));
#387113=CARTESIAN_POINT('Ctrl Pts',(2.71710209070083,0.399660985282296,
7.50366195182966));
#387114=CARTESIAN_POINT('Ctrl Pts',(2.72072505953656,0.40019389102009,7.50000065167735));
#387115=CARTESIAN_POINT('Ctrl Pts',(2.72072505953658,0.400193891019974,
7.49482233047108));
#387116=CARTESIAN_POINT('Ctrl Pts',(2.71965064636477,0.392671088027359,
7.50215800491338));
#387117=CARTESIAN_POINT('Ctrl Pts',(2.72211237908243,0.390762012544002,
7.49877273257265));
#387118=CARTESIAN_POINT('Ctrl Pts',(2.72261477294344,0.387346641882077,
7.49481816995647));
#387119=CARTESIAN_POINT('Ctrl Pts',(2.71785182623253,0.390509083754953,
7.51043025814042));
#387120=CARTESIAN_POINT('Ctrl Pts',(2.72261960393337,0.387138467671458,
7.51006209594515));
#387121=CARTESIAN_POINT('Ctrl Pts',(2.72342564846378,0.381382665175079,
7.50731281821701));
#387122=CARTESIAN_POINT('Ctrl Pts',(2.7151913081126,0.39144427839713,7.51860402984326));
#387123=CARTESIAN_POINT('Ctrl Pts',(2.72237000153422,0.388920911965361,
7.51860402984326));
#387124=CARTESIAN_POINT('Ctrl Pts',(2.72342529733067,0.381385172574125,
7.51860402984327));
#387125=CARTESIAN_POINT('Origin',(0.,0.,7.5));
#387126=CARTESIAN_POINT('Origin',(2.65600461497701,0.250154969482936,7.5));
#387127=CARTESIAN_POINT('',(2.65600461497701,0.250154969482936,7.59394543036555));
#387128=CARTESIAN_POINT('',(2.65600461497701,0.250154969482936,8.85049129520029));
#387129=CARTESIAN_POINT('',(2.65600461497701,0.250154969482936,7.5));
#387130=CARTESIAN_POINT('',(2.72179064828012,0.222166246411456,8.78727029226991));
#387131=CARTESIAN_POINT('Ctrl Pts',(2.65600461497701,0.250154969482936,
8.85049129520029));
#387132=CARTESIAN_POINT('Ctrl Pts',(2.67796516820153,0.240811833685928,
8.82945686509571));
#387133=CARTESIAN_POINT('Ctrl Pts',(2.69989307440824,0.231482587590037,
8.80838212259896));
#387134=CARTESIAN_POINT('Ctrl Pts',(2.72179064828012,0.222166246411456,
8.78727029226991));
#387135=CARTESIAN_POINT('',(2.73469396819878,0.216676518124572,8.75721825406948));
#387136=CARTESIAN_POINT('Origin',(2.69586348137518,0.233197200634467,8.75937679713141));
#387137=CARTESIAN_POINT('',(2.73469396819878,0.216676518124572,7.51860402984325));
#387138=CARTESIAN_POINT('',(2.73469396819878,0.216676518124572,7.5));
#387139=CARTESIAN_POINT('Ctrl Pts',(2.73469396819878,0.216676518124572,
7.51860402984325));
#387140=CARTESIAN_POINT('Ctrl Pts',(2.72456041724852,0.220987845879672,
7.52834476460825));
#387141=CARTESIAN_POINT('Ctrl Pts',(2.71442028774321,0.225301972486544,
7.53807742314407));
#387142=CARTESIAN_POINT('Ctrl Pts',(2.70427335879911,0.229618991920351,
7.54780169004674));
#387143=CARTESIAN_POINT('Ctrl Pts',(2.68820117174637,0.236456917388509,
7.5632044032688));
#387144=CARTESIAN_POINT('Ctrl Pts',(2.67211190534232,0.243302109280994,
7.57858609112103));
#387145=CARTESIAN_POINT('Ctrl Pts',(2.65600461497701,0.250154969482936,
7.59394543036555));
#387146=CARTESIAN_POINT('Origin',(2.88264819886835,0.416223926434595,7.5));
#387147=CARTESIAN_POINT('',(2.72568349213022,0.310079528408739,8.75721825406948));
#387148=CARTESIAN_POINT('',(2.71406752923974,0.302224454398009,8.78727029226991));
#387149=CARTESIAN_POINT('Origin',(2.68458188288363,0.282285346760939,8.75658640620963));
#387150=CARTESIAN_POINT('',(2.6548449317704,0.262176299060784,8.85049129520029));
#387151=CARTESIAN_POINT('Ctrl Pts',(2.71406752923974,0.302224454398009,
8.78727029226991));
#387152=CARTESIAN_POINT('Ctrl Pts',(2.69435466409412,0.288894004211287,
8.80838212259896));
#387153=CARTESIAN_POINT('Ctrl Pts',(2.67461449285379,0.275545088797271,
8.82945686509571));
#387154=CARTESIAN_POINT('Ctrl Pts',(2.6548449317704,0.262176299060784,8.85049129520029));
#387155=CARTESIAN_POINT('',(2.6548449317704,0.262176299060784,7.59394543036555));
#387156=CARTESIAN_POINT('',(2.6548449317704,0.262176299060784,7.5));
#387157=CARTESIAN_POINT('',(2.72568349213022,0.310079528408739,7.51860402984325));
#387158=CARTESIAN_POINT('Ctrl Pts',(2.6548449317704,0.262176299060783,7.59394543036555));
#387159=CARTESIAN_POINT('Ctrl Pts',(2.66934520676389,0.271981834281903,
7.57858609112103));
#387160=CARTESIAN_POINT('Ctrl Pts',(2.68382925603652,0.281776397167827,
7.56320440326857));
#387161=CARTESIAN_POINT('Ctrl Pts',(2.69829792995535,0.291560562763152,
7.54780169004651));
#387162=CARTESIAN_POINT('Ctrl Pts',(2.70743250546073,0.2977376457418,7.53807742314383));
#387163=CARTESIAN_POINT('Ctrl Pts',(2.7165609599037,0.3039105894684,7.52834476460825));
#387164=CARTESIAN_POINT('Ctrl Pts',(2.72568349213022,0.310079528408737,
7.51860402984324));
#387165=CARTESIAN_POINT('',(2.72568349213022,0.310079528408739,7.5));
#387166=CARTESIAN_POINT('Origin',(2.65869612245474,0.256481217383335,7.5));
#387167=CARTESIAN_POINT('Ctrl Pts',(2.6548449317704,0.262176299060783,8.85049129520029));
#387168=CARTESIAN_POINT('Ctrl Pts',(2.65468450732037,0.262067815077147,
8.85097269580138));
#387169=CARTESIAN_POINT('Ctrl Pts',(2.65453081876943,0.261953732011581,
8.85143669361005));
#387170=CARTESIAN_POINT('Ctrl Pts',(2.65437731036211,0.261828094693195,
8.8519052845931));
#387171=CARTESIAN_POINT('Ctrl Pts',(2.65407705765252,0.261582356066062,
8.85282181883899));
#387172=CARTESIAN_POINT('Ctrl Pts',(2.65378534264253,0.26129858365081,8.85372622499636));
#387173=CARTESIAN_POINT('Ctrl Pts',(2.65350833902008,0.260961272455542,
8.85462257735071));
#387174=CARTESIAN_POINT('Ctrl Pts',(2.65327838045095,0.260681248681391,
8.85536669723986));
#387175=CARTESIAN_POINT('Ctrl Pts',(2.65305848371428,0.260364283628691,
8.85610498449051));
#387176=CARTESIAN_POINT('Ctrl Pts',(2.65285873749404,0.259996917879283,
8.85681338218371));
#387177=CARTESIAN_POINT('Ctrl Pts',(2.65267746748548,0.259663532884738,
8.85745625420284));
#387178=CARTESIAN_POINT('Ctrl Pts',(2.65250999297828,0.259284743853906,
8.85808743050665));
#387179=CARTESIAN_POINT('Ctrl Pts',(2.65237491462936,0.258838828408651,
8.85866804508409));
#387180=CARTESIAN_POINT('Ctrl Pts',(2.6523125924073,0.25863309268847,8.85893592806395));
#387181=CARTESIAN_POINT('Ctrl Pts',(2.6522573448343,0.258412903800744,8.85919241173848));
#387182=CARTESIAN_POINT('Ctrl Pts',(2.65221231342864,0.258175223186696,
8.85943017985534));
#387183=CARTESIAN_POINT('Ctrl Pts',(2.65215150770028,0.25785428399674,8.8597512372));
#387184=CARTESIAN_POINT('Ctrl Pts',(2.65210841079494,0.257493164175779,
8.86004599534705));
#387185=CARTESIAN_POINT('Ctrl Pts',(2.65209388221267,0.257094968238574,
8.86026130871721));
#387186=CARTESIAN_POINT('Ctrl Pts',(2.6520885628891,0.256949177479631,8.86034014101235));
#387187=CARTESIAN_POINT('Ctrl Pts',(2.65208698092624,0.256796227185932,
8.86040910639692));
#387188=CARTESIAN_POINT('Ctrl Pts',(2.65208951578449,0.256640280923396,
8.86046313645506));
#387189=CARTESIAN_POINT('Ctrl Pts',(2.65209347140956,0.256396928086748,
8.86054744990829));
#387190=CARTESIAN_POINT('Ctrl Pts',(2.65210770704384,0.256139639254116,
8.86059655985669));
#387191=CARTESIAN_POINT('Ctrl Pts',(2.65213101720273,0.255884898957225,
8.86059725258816));
#387192=CARTESIAN_POINT('Ctrl Pts',(2.6521543812174,0.255629570108478,8.86059794692011));
#387193=CARTESIAN_POINT('Ctrl Pts',(2.65218976656293,0.255374212058251,
8.86056369958365));
#387194=CARTESIAN_POINT('Ctrl Pts',(2.65223151582429,0.255132235635948,
8.86048590497774));
#387195=CARTESIAN_POINT('Ctrl Pts',(2.65224241113849,0.255069086994233,
8.86046560290182));
#387196=CARTESIAN_POINT('Ctrl Pts',(2.65225397087203,0.255006043587067,
8.86044257503091));
#387197=CARTESIAN_POINT('Ctrl Pts',(2.65226580553172,0.254945047587569,
8.86041778462583));
#387198=CARTESIAN_POINT('Ctrl Pts',(2.65234543810585,0.254534620200674,
8.86025097596201));
#387199=CARTESIAN_POINT('Ctrl Pts',(2.65244852973477,0.254161880950984,
8.85998489822951));
#387200=CARTESIAN_POINT('Ctrl Pts',(2.65256390552944,0.253835450602003,
8.85968173251462));
#387201=CARTESIAN_POINT('Ctrl Pts',(2.65262493271457,0.253662787649621,
8.85952137522077));
#387202=CARTESIAN_POINT('Ctrl Pts',(2.65269039306684,0.253499689179489,
8.85934740853961));
#387203=CARTESIAN_POINT('Ctrl Pts',(2.65275792075998,0.253347876209786,
8.8591675900182));
#387204=CARTESIAN_POINT('Ctrl Pts',(2.65302907954814,0.252738268225621,
8.85844552518696));
#387205=CARTESIAN_POINT('Ctrl Pts',(2.6533461335036,0.252274948742803,8.85759444184126));
#387206=CARTESIAN_POINT('Ctrl Pts',(2.65363857348188,0.251920402392356,
8.85683498915141));
#387207=CARTESIAN_POINT('Ctrl Pts',(2.65366917654678,0.251883300061011,
8.85675551445));
#387208=CARTESIAN_POINT('Ctrl Pts',(2.65369952268128,0.251847404387458,
8.85667699793652));
#387209=CARTESIAN_POINT('Ctrl Pts',(2.65372953884553,0.251812682973008,
8.85659965593547));
#387210=CARTESIAN_POINT('Ctrl Pts',(2.65413469856212,0.251344011549065,
8.85555568965886));
#387211=CARTESIAN_POINT('Ctrl Pts',(2.6545917675788,0.250952102354077,8.85434650606346));
#387212=CARTESIAN_POINT('Ctrl Pts',(2.65509896008146,0.25063030012207,8.85297329937118));
#387213=CARTESIAN_POINT('Ctrl Pts',(2.65538422496052,0.250449305974264,
8.85220095427748));
#387214=CARTESIAN_POINT('Ctrl Pts',(2.65568563114289,0.250290681422829,
8.85137579139184));
#387215=CARTESIAN_POINT('Ctrl Pts',(2.65600461497701,0.250154969482936,
8.85049129520029));
#387216=CARTESIAN_POINT('Origin',(2.65869612245474,0.256481217383335,7.59394543036555));
#387217=CARTESIAN_POINT('Ctrl Pts',(2.65437916547328,0.261861333459561,
7.59443877723642));
#387218=CARTESIAN_POINT('Ctrl Pts',(2.64958222076125,0.258617490818736,
7.58783886950016));
#387219=CARTESIAN_POINT('Ctrl Pts',(2.65258170159906,0.250675054401599,
7.58559994247159));
#387220=CARTESIAN_POINT('Ctrl Pts',(2.68056554591985,0.279569375265512,
7.56670252222133));
#387221=CARTESIAN_POINT('Ctrl Pts',(2.67577553415482,0.276330220898256,
7.56004874999026));
#387222=CARTESIAN_POINT('Ctrl Pts',(2.67877280023321,0.268333174361465,
7.55786368756705));
#387223=CARTESIAN_POINT('Ctrl Pts',(2.70670302591731,0.297244349072657,
7.53888913333558));
#387224=CARTESIAN_POINT('Ctrl Pts',(2.70188454687784,0.293985944252378,
7.53222002137278));
#387225=CARTESIAN_POINT('Ctrl Pts',(2.70491526550984,0.285959912275532,
7.53005029815327));
#387226=CARTESIAN_POINT('Ctrl Pts',(2.73279042272696,0.314885455076452,
7.51101258149734));
#387227=CARTESIAN_POINT('Ctrl Pts',(2.72791353496612,0.311587552469099,
7.5043616886572));
#387228=CARTESIAN_POINT('Ctrl Pts',(2.73100785199465,0.303554328728184,
7.50217374673251));
#387229=CARTESIAN_POINT('',(2.72961551748768,0.302615468917139,7.50366116523517));
#387230=CARTESIAN_POINT('Ctrl Pts',(2.72568349213022,0.310079528408739,
7.51860402984325));
#387231=CARTESIAN_POINT('Ctrl Pts',(2.72604931204916,0.310326907172344,
7.51734760759493));
#387232=CARTESIAN_POINT('Ctrl Pts',(2.7264132111716,0.310501163560087,7.51608817408572));
#387233=CARTESIAN_POINT('Ctrl Pts',(2.72678011988137,0.310589852801548,
7.51481005913119));
#387234=CARTESIAN_POINT('Ctrl Pts',(2.72711247455824,0.310670189635761,
7.51365231206383));
#387235=CARTESIAN_POINT('Ctrl Pts',(2.72744770835602,0.310680673584736,
7.51247773061042));
#387236=CARTESIAN_POINT('Ctrl Pts',(2.72778117474014,0.310584216244789,
7.51129758471022));
#387237=CARTESIAN_POINT('Ctrl Pts',(2.72819563537232,0.31046433078708,7.50983079813402));
#387238=CARTESIAN_POINT('Ctrl Pts',(2.72859051930512,0.310170560553426,
7.50839324291155));
#387239=CARTESIAN_POINT('Ctrl Pts',(2.72891950166131,0.309634617944518,
7.50715379678855));
#387240=CARTESIAN_POINT('Ctrl Pts',(2.72907148203047,0.309387027902018,
7.50658120839351));
#387241=CARTESIAN_POINT('Ctrl Pts',(2.72922290543959,0.309047586153636,
7.50598221009429));
#387242=CARTESIAN_POINT('Ctrl Pts',(2.72934939496709,0.308615104077967,
7.50545747549611));
#387243=CARTESIAN_POINT('Ctrl Pts',(2.72941689369418,0.308384318255817,
7.50517746087247));
#387244=CARTESIAN_POINT('Ctrl Pts',(2.72947821848437,0.308124592386469,
7.50491486231392));
#387245=CARTESIAN_POINT('Ctrl Pts',(2.72953012197526,0.307842421146914,
7.50468370960993));
#387246=CARTESIAN_POINT('Ctrl Pts',(2.72960773406618,0.307420486137913,
7.50433806340447));
#387247=CARTESIAN_POINT('Ctrl Pts',(2.72966606023027,0.306935611055772,
7.50405484070984));
#387248=CARTESIAN_POINT('Ctrl Pts',(2.7297004610413,0.306420365776551,7.50385766036131));
#387249=CARTESIAN_POINT('Ctrl Pts',(2.72970413967333,0.306365268302659,
7.50383657498791));
#387250=CARTESIAN_POINT('Ctrl Pts',(2.72970755748387,0.306309848873761,
7.50381643264937));
#387251=CARTESIAN_POINT('Ctrl Pts',(2.7297107183599,0.306254165571787,7.50379723213559));
#387252=CARTESIAN_POINT('Ctrl Pts',(2.72973181824138,0.305882461315862,
7.50366906242519));
#387253=CARTESIAN_POINT('Ctrl Pts',(2.7297412101996,0.305490872696448,7.50358235568538));
#387254=CARTESIAN_POINT('Ctrl Pts',(2.72974118993311,0.30511321185333,7.5035341175365));
#387255=CARTESIAN_POINT('Ctrl Pts',(2.72974115954581,0.304546952162028,
7.50346178989176));
#387256=CARTESIAN_POINT('Ctrl Pts',(2.72971705014849,0.303937786884254,
7.50346967198527));
#387257=CARTESIAN_POINT('Ctrl Pts',(2.72967498135674,0.303340503578766,
7.50354272648692));
#387258=CARTESIAN_POINT('Ctrl Pts',(2.72965767759192,0.303094828592186,
7.50357277531559));
#387259=CARTESIAN_POINT('Ctrl Pts',(2.72963749980964,0.302851480312651,
7.50361331098761));
#387260=CARTESIAN_POINT('Ctrl Pts',(2.72961551748909,0.302615468917296,
7.50366116523659));
#387261=CARTESIAN_POINT('',(2.6616105180258,0.256762365618806,7.57603338622103));
#387262=CARTESIAN_POINT('Origin',(2.67040689596839,0.257608075198453,7.58486873427629));
#387263=CARTESIAN_POINT('Ctrl Pts',(2.72961551753202,0.302615468953502,
7.50366116529969));
#387264=CARTESIAN_POINT('Ctrl Pts',(2.70698464170165,0.287355349099742,
7.52783573079709));
#387265=CARTESIAN_POINT('Ctrl Pts',(2.68431738885518,0.272071688128246,
7.55196141284069));
#387266=CARTESIAN_POINT('Ctrl Pts',(2.66161051882396,0.256762366583483,
7.57603338728831));
#387267=CARTESIAN_POINT('Ctrl Pts',(2.65579532783698,0.262606743989991,
7.5963967733137));
#387268=CARTESIAN_POINT('Ctrl Pts',(2.63922637620257,0.254890413417597,
7.59959882295473));
#387269=CARTESIAN_POINT('Ctrl Pts',(2.65684465102774,0.249960382504451,
7.59642833564546));
#387270=CARTESIAN_POINT('Ctrl Pts',(2.65204060628408,0.261549781292375,
7.5870762605742));
#387271=CARTESIAN_POINT('Ctrl Pts',(2.64876165092591,0.255620131825807,
7.588099439206));
#387272=CARTESIAN_POINT('Ctrl Pts',(2.65302079876161,0.2503690309405,7.58710240504254));
#387273=CARTESIAN_POINT('Ctrl Pts',(2.65730239716172,0.258510177860652,
7.58015376756929));
#387274=CARTESIAN_POINT('Ctrl Pts',(2.65560985891301,0.256215709366007,
7.58205880659762));
#387275=CARTESIAN_POINT('Ctrl Pts',(2.65765471203255,0.254280340988258,
7.58020924244125));
#387276=CARTESIAN_POINT('Ctrl Pts',(2.66161051720204,0.256762365539542,
7.57603338509286));
#387277=CARTESIAN_POINT('Ctrl Pts',(2.66161051720204,0.256762365539542,
7.57603338509286));
#387278=CARTESIAN_POINT('Ctrl Pts',(2.66161051720204,0.256762365539542,
7.57603338509286));
#387279=CARTESIAN_POINT('Origin',(2.67040634802725,0.257613755182223,7.5848687342762));
#387280=CARTESIAN_POINT('Ctrl Pts',(2.74261348672104,0.213307152323814,
7.51098857897448));
#387281=CARTESIAN_POINT('Ctrl Pts',(2.73719608563612,0.215611990161267,
7.50433767179956));
#387282=CARTESIAN_POINT('Ctrl Pts',(2.73869774222272,0.224088609686666,
7.50214974420965));
#387283=CARTESIAN_POINT('Ctrl Pts',(2.71362657888527,0.225639656586166,
7.53887321589169));
#387284=CARTESIAN_POINT('Ctrl Pts',(2.70827408787951,0.227916878375974,
7.53220407452065));
#387285=CARTESIAN_POINT('Ctrl Pts',(2.70971466634537,0.236374280672535,
7.53003438070911));
#387286=CARTESIAN_POINT('Ctrl Pts',(2.68458400549363,0.237995843805974,
7.56669465659234));
#387287=CARTESIAN_POINT('Ctrl Pts',(2.67926314671456,0.240259607638394,
7.56004085833298));
#387288=CARTESIAN_POINT('Ctrl Pts',(2.68067642139728,0.24868215504385,7.55785582193789));
#387289=CARTESIAN_POINT('Ctrl Pts',(2.65548708002545,0.250375155162354,
7.59443891967696));
#387290=CARTESIAN_POINT('Ctrl Pts',(2.65015850666364,0.252642201170471,
7.58783901202978));
#387291=CARTESIAN_POINT('Ctrl Pts',(2.65158440916058,0.261011548818738,
7.58560008491213));
#387292=CARTESIAN_POINT('',(2.73712666431695,0.224754574642228,7.50366116523517));
#387293=CARTESIAN_POINT('Ctrl Pts',(2.73712666431733,0.224754574642259,
7.50366116523554));
#387294=CARTESIAN_POINT('Ctrl Pts',(2.73733969481484,0.22402741886535,7.50350835821027));
#387295=CARTESIAN_POINT('Ctrl Pts',(2.73751186429179,0.223352055494748,
7.50345484956));
#387296=CARTESIAN_POINT('Ctrl Pts',(2.73764887337768,0.222708553769215,
7.50349758195598));
#387297=CARTESIAN_POINT('Ctrl Pts',(2.7377191691996,0.222378389660684,7.50351950684424));
#387298=CARTESIAN_POINT('Ctrl Pts',(2.73778726446689,0.222024097627302,
7.50357029184312));
#387299=CARTESIAN_POINT('Ctrl Pts',(2.73784353695387,0.221680652932927,
7.50365515313923));
#387300=CARTESIAN_POINT('Ctrl Pts',(2.73793010682584,0.221152295918489,
7.50378570417639));
#387301=CARTESIAN_POINT('Ctrl Pts',(2.73799157957439,0.220634157925334,
7.50400001621911));
#387302=CARTESIAN_POINT('Ctrl Pts',(2.7380210216278,0.220165409289273,7.50428903009634));
#387303=CARTESIAN_POINT('Ctrl Pts',(2.73802428946922,0.220113381797004,
7.50432110841318));
#387304=CARTESIAN_POINT('Ctrl Pts',(2.73802718145414,0.220061938916616,
7.50435406373354));
#387305=CARTESIAN_POINT('Ctrl Pts',(2.73802970169419,0.22001111643043,7.50438785222352));
#387306=CARTESIAN_POINT('Ctrl Pts',(2.73804508897109,0.219700820723885,
7.50459414719561));
#387307=CARTESIAN_POINT('Ctrl Pts',(2.73804634861812,0.219408685618617,
7.50483629897752));
#387308=CARTESIAN_POINT('Ctrl Pts',(2.73803474839784,0.219145908398964,
7.5050991045531));
#387309=CARTESIAN_POINT('Ctrl Pts',(2.73800915714678,0.218566195458937,
7.50567888004914));
#387310=CARTESIAN_POINT('Ctrl Pts',(2.73792048980846,0.218106496852257,
7.50637912803144));
#387311=CARTESIAN_POINT('Ctrl Pts',(2.73779651599276,0.217753238076229,
7.50710440483569));
#387312=CARTESIAN_POINT('Ctrl Pts',(2.73776611515193,0.217666612011177,
7.50728225710685));
#387313=CARTESIAN_POINT('Ctrl Pts',(2.73773312376091,0.217584613677214,
7.50746498566954));
#387314=CARTESIAN_POINT('Ctrl Pts',(2.73769869842967,0.217509001681951,
7.50764697238949));
#387315=CARTESIAN_POINT('Ctrl Pts',(2.73751363732303,0.217102532404395,
7.50862528291182));
#387316=CARTESIAN_POINT('Ctrl Pts',(2.7372741051665,0.216842004831574,7.50965856837422));
#387317=CARTESIAN_POINT('Ctrl Pts',(2.73701505418627,0.216671083027123,
7.51067959873202));
#387318=CARTESIAN_POINT('Ctrl Pts',(2.7368724981051,0.216577024542544,7.51124147302579));
#387319=CARTESIAN_POINT('Ctrl Pts',(2.73672375708,0.216510441144925,7.51180065547253));
#387320=CARTESIAN_POINT('Ctrl Pts',(2.73657324382109,0.216464264630464,
7.51235175716501));
#387321=CARTESIAN_POINT('Ctrl Pts',(2.73605316055418,0.21630470637846,7.51425603304536));
#387322=CARTESIAN_POINT('Ctrl Pts',(2.73544812829919,0.216375575257993,
7.51626900505181));
#387323=CARTESIAN_POINT('Ctrl Pts',(2.73479964907405,0.21663305061294,7.51827788969244));
#387324=CARTESIAN_POINT('Ctrl Pts',(2.73476455215293,0.216646985665711,
7.51838661432546));
#387325=CARTESIAN_POINT('Ctrl Pts',(2.73472932345267,0.216661476202132,
7.51849533314857));
#387326=CARTESIAN_POINT('Ctrl Pts',(2.73469396819878,0.216676518124568,
7.51860402984325));
#387327=CARTESIAN_POINT('Ctrl Pts',(2.66161051899485,0.256762364824367,
7.57603338728985));
#387328=CARTESIAN_POINT('Ctrl Pts',(2.68682516411914,0.246075974209705,
7.55196141284922));
#387329=CARTESIAN_POINT('Ctrl Pts',(2.7119960174081,0.235407197792705,7.52783573083104));
#387330=CARTESIAN_POINT('Ctrl Pts',(2.73712666436909,0.224754574614226,
7.50366116530176));
#387331=CARTESIAN_POINT('Origin',(9.19709468541365E-16,8.87232663177303E-17,
7.49482233047033));
#387332=CARTESIAN_POINT('Origin',(2.72083050515592,0.301641529324114,7.49482233047033));
#387333=CARTESIAN_POINT('Origin',(0.,0.,7.50366116523517));
#387334=CARTESIAN_POINT('Origin',(2.7283174780614,0.224031223057655,7.49482233047033));
#387335=CARTESIAN_POINT('Ctrl Pts',(2.72568261591557,0.310078935939271,
7.51860402984325));
#387336=CARTESIAN_POINT('Ctrl Pts',(2.73198605348183,0.314340738477925,
7.51860402984325));
#387337=CARTESIAN_POINT('Ctrl Pts',(2.73109539723703,0.321897392332887,
7.51860402984325));
#387338=CARTESIAN_POINT('Ctrl Pts',(2.72802312458908,0.311661373358629,
7.51041458714367));
#387339=CARTESIAN_POINT('Ctrl Pts',(2.7317750369846,0.316130995169986,7.51004642900442));
#387340=CARTESIAN_POINT('Ctrl Pts',(2.73109515160461,0.321899476368297,
7.5072913648301));
#387341=CARTESIAN_POINT('Ctrl Pts',(2.73030742601402,0.310016470869326,
7.50215815450137));
#387342=CARTESIAN_POINT('Ctrl Pts',(2.7322048270618,0.312485870339915,7.49877163671531));
#387343=CARTESIAN_POINT('Ctrl Pts',(2.73182466947127,0.315915069051093,
7.4948158853317));
#387344=CARTESIAN_POINT('Ctrl Pts',(2.72961497032199,0.30261540825581,7.50366171572174));
#387345=CARTESIAN_POINT('Ctrl Pts',(2.73325438874115,0.303018887905119,
7.50000045605858));
#387346=CARTESIAN_POINT('Ctrl Pts',(2.73325438874114,0.303018887905242,
7.49482233047317));
#387347=CARTESIAN_POINT('Origin',(2.71868132724959,0.320434222367736,7.51860402984325));
#387348=CARTESIAN_POINT('Origin',(2.71868132724959,0.320434222367736,9.));
#387349=CARTESIAN_POINT('Origin',(2.71868132724959,0.320434222367736,8.75721825406948));
#387350=CARTESIAN_POINT('Ctrl Pts',(2.71184947061986,0.300724570905254,
8.78942910404913));
#387351=CARTESIAN_POINT('Ctrl Pts',(2.71647685875768,0.30382935877622,8.79672699501691));
#387352=CARTESIAN_POINT('Ctrl Pts',(2.71294933545981,0.312028752983415,
8.79893251111267));
#387353=CARTESIAN_POINT('Ctrl Pts',(2.72095691172079,0.306883299291368,
8.78111911759584));
#387354=CARTESIAN_POINT('Ctrl Pts',(2.72643858652893,0.310570242662666,
8.78644465894814));
#387355=CARTESIAN_POINT('Ctrl Pts',(2.72490651814849,0.31853066213987,8.78817647674132));
#387356=CARTESIAN_POINT('Ctrl Pts',(2.72663288623002,0.310721565747487,
8.7678092393203));
#387357=CARTESIAN_POINT('Ctrl Pts',(2.73310092791912,0.315078075070137,
8.76988516158373));
#387358=CARTESIAN_POINT('Ctrl Pts',(2.73236943182155,0.322601458209093,
8.77093053738833));
#387359=CARTESIAN_POINT('Ctrl Pts',(2.72552614888092,0.309973156320347,
8.75371302330492));
#387360=CARTESIAN_POINT('Ctrl Pts',(2.73183587040218,0.314222110979058,
8.75300828287559));
#387361=CARTESIAN_POINT('Ctrl Pts',(2.73091364145018,0.321807889323718,
8.75267964240738));
#387362=CARTESIAN_POINT('Origin',(2.70706536435911,0.312579148357006,8.78727029226991));
#387363=CARTESIAN_POINT('Ctrl Pts',(2.6548449317704,0.262176299060784,8.85049129520029));
#387364=CARTESIAN_POINT('Ctrl Pts',(2.65968232649294,0.265447495252001,
8.85711686593484));
#387365=CARTESIAN_POINT('Ctrl Pts',(2.65663515242803,0.273435955199454,
8.85933012996512));
#387366=CARTESIAN_POINT('Ctrl Pts',(2.67461451938527,0.27554510673868,8.82945683644721));
#387367=CARTESIAN_POINT('Ctrl Pts',(2.67949206740875,0.27884345583608,8.83607469902389));
#387368=CARTESIAN_POINT('Ctrl Pts',(2.67640090713581,0.28684200387085,8.83829567148518));
#387369=CARTESIAN_POINT('Ctrl Pts',(2.69435463883558,0.288893987130678,
8.80838214965003));
#387370=CARTESIAN_POINT('Ctrl Pts',(2.69925143594087,0.292205353053615,
8.81501364461992));
#387371=CARTESIAN_POINT('Ctrl Pts',(2.69613705347889,0.300227162978777,
8.81722098428722));
#387372=CARTESIAN_POINT('Ctrl Pts',(2.71406752923974,0.302224454398009,
8.78727029226991));
#387373=CARTESIAN_POINT('Ctrl Pts',(2.71896513971909,0.305536370349683,
8.79393457792714));
#387374=CARTESIAN_POINT('Ctrl Pts',(2.71584585849932,0.313593013561975,
8.79610912703474));
#387375=CARTESIAN_POINT('Origin',(2.64784276688977,0.272530993019781,8.85049129520029));
#387376=CARTESIAN_POINT('Ctrl Pts',(2.65600461497701,0.250154969482936,
8.85049129520029));
#387377=CARTESIAN_POINT('Ctrl Pts',(2.66137812144103,0.24786880664878,8.85711686593484));
#387378=CARTESIAN_POINT('Ctrl Pts',(2.65991420288366,0.239445167021439,
8.85933012996512));
#387379=CARTESIAN_POINT('Ctrl Pts',(2.65125075137568,0.252177504741206,
8.86332496987232));
#387380=CARTESIAN_POINT('Ctrl Pts',(2.65197460016676,0.247613741238966,
8.86648636486736));
#387381=CARTESIAN_POINT('Ctrl Pts',(2.64662178291422,0.245119057019738,
8.87206031107457));
#387382=CARTESIAN_POINT('Ctrl Pts',(2.65053627743827,0.259262653503836,
8.86341338519876));
#387383=CARTESIAN_POINT('Ctrl Pts',(2.6503443297877,0.263892623993351,8.86654584966058));
#387384=CARTESIAN_POINT('Ctrl Pts',(2.64457894424469,0.265265388477058,
8.87215952290714));
#387385=CARTESIAN_POINT('Ctrl Pts',(2.6548449317704,0.262176299060783,8.85049129520029));
#387386=CARTESIAN_POINT('Ctrl Pts',(2.65968232649294,0.265447495252001,
8.85711686593484));
#387387=CARTESIAN_POINT('Ctrl Pts',(2.65663515242803,0.273435955199453,
8.85933012996512));
#387388=CARTESIAN_POINT('Origin',(2.65111096501749,0.23865270057312,8.85049129520029));
#387389=CARTESIAN_POINT('Ctrl Pts',(2.72179064828012,0.222166246411456,
8.78727029226991));
#387390=CARTESIAN_POINT('Ctrl Pts',(2.7272310440052,0.219851625485051,8.79393457792714));
#387391=CARTESIAN_POINT('Ctrl Pts',(2.7257093818291,0.21134727604491,8.79610912703474));
#387392=CARTESIAN_POINT('Ctrl Pts',(2.69989304635039,0.231482599527275,
8.80838214965002));
#387393=CARTESIAN_POINT('Ctrl Pts',(2.70533253855793,0.229168363003168,
8.81501364461988));
#387394=CARTESIAN_POINT('Ctrl Pts',(2.70380902611905,0.220699140934762,
8.81722098428721));
#387395=CARTESIAN_POINT('Ctrl Pts',(2.67796519767341,0.240811821147091,
8.82945683644723));
#387396=CARTESIAN_POINT('Ctrl Pts',(2.68338330748996,0.238506681779163,
8.83607469902389));
#387397=CARTESIAN_POINT('Ctrl Pts',(2.68187814229223,0.230064731754138,
8.8382956714852));
#387398=CARTESIAN_POINT('Ctrl Pts',(2.65600461497701,0.250154969482936,
8.85049129520029));
#387399=CARTESIAN_POINT('Ctrl Pts',(2.66137812144103,0.24786880664878,8.85711686593484));
#387400=CARTESIAN_POINT('Ctrl Pts',(2.65991420288366,0.239445167021439,
8.85933012996512));
#387401=CARTESIAN_POINT('Origin',(2.71689699832061,0.21066397750164,8.78727029226991));
#387402=CARTESIAN_POINT('Ctrl Pts',(2.73452357912826,0.216748990250391,
8.75374538247847));
#387403=CARTESIAN_POINT('Ctrl Pts',(2.74152113982086,0.213786133058247,
8.75304829418601));
#387404=CARTESIAN_POINT('Ctrl Pts',(2.74207106399279,0.206172446263127,
8.75272238421917));
#387405=CARTESIAN_POINT('Ctrl Pts',(2.7357382038743,0.216232227596534,8.76769408445021));
#387406=CARTESIAN_POINT('Ctrl Pts',(2.74291158516778,0.213194176281851,
8.76974318093971));
#387407=CARTESIAN_POINT('Ctrl Pts',(2.7436342664713,0.205677788252101,8.7707786988043));
#387408=CARTESIAN_POINT('Ctrl Pts',(2.72951272935799,0.218880858593531,
8.78108014887987));
#387409=CARTESIAN_POINT('Ctrl Pts',(2.73559339329593,0.216309718112314,
8.78639403366322));
#387410=CARTESIAN_POINT('Ctrl Pts',(2.73563104846251,0.208215234940591,
8.78812224174741));
#387411=CARTESIAN_POINT('Ctrl Pts',(2.71931055089962,0.223221380073952,
8.78944554828685));
#387412=CARTESIAN_POINT('Ctrl Pts',(2.72443728907638,0.221059673969063,
8.79673892988686));
#387413=CARTESIAN_POINT('Ctrl Pts',(2.72254676134579,0.212345922812613,
8.79894799272499));
#387414=CARTESIAN_POINT('Origin',(2.72980031823926,0.205174249214755,8.75721825406948));
#387415=CARTESIAN_POINT('Origin',(2.72980031823926,0.205174249214755,9.));
#387416=CARTESIAN_POINT('Origin',(2.72980031823926,0.205174249214756,7.51860402984325));
#387417=CARTESIAN_POINT('Ctrl Pts',(2.73712588029194,0.22475451026327,7.50366195182966));
#387418=CARTESIAN_POINT('Ctrl Pts',(2.74077554873749,0.225054196678783,
7.50000065167735));
#387419=CARTESIAN_POINT('Ctrl Pts',(2.7407755487375,0.225054196678667,7.49482233047108));
#387420=CARTESIAN_POINT('Ctrl Pts',(2.73922135542018,0.217615687979893,
7.50215800491337));
#387421=CARTESIAN_POINT('Ctrl Pts',(2.74155571535778,0.215552811140105,
7.49877273257265));
#387422=CARTESIAN_POINT('Ctrl Pts',(2.74183825344708,0.212112269238307,
7.49481816995647));
#387423=CARTESIAN_POINT('Ctrl Pts',(2.73728771106749,0.215573376578712,
7.51043025814043));
#387424=CARTESIAN_POINT('Ctrl Pts',(2.74182973674376,0.211904213221347,
7.51006209594516));
#387425=CARTESIAN_POINT('Ctrl Pts',(2.74226534963713,0.206108593188127,
7.50731281821701));
#387426=CARTESIAN_POINT('Ctrl Pts',(2.73469257739382,0.216677109744404,
7.51860402984326));
#387427=CARTESIAN_POINT('Ctrl Pts',(2.74169484877752,0.213698987372904,
7.51860402984326));
#387428=CARTESIAN_POINT('Ctrl Pts',(2.74226515987506,0.206111117932626,
7.51860402984327));
#387429=CARTESIAN_POINT('Origin',(0.,0.,7.5));
#387430=CARTESIAN_POINT('Origin',(2.66657505256398,0.0794701993177319,7.5));
#387431=CARTESIAN_POINT('',(2.66657505256398,0.0794701993177319,7.59394543036555));
#387432=CARTESIAN_POINT('',(2.66657505256398,0.0794701993177319,8.85049129520029));
#387433=CARTESIAN_POINT('',(2.66657505256398,0.0794701993177319,7.5));
#387434=CARTESIAN_POINT('',(2.73043267776197,0.0473240564541946,8.78727029226991));
#387435=CARTESIAN_POINT('Ctrl Pts',(2.66657505256398,0.0794701993177318,
8.85049129520029));
#387436=CARTESIAN_POINT('Ctrl Pts',(2.68789186871081,0.0687392425192737,
8.82945686509571));
#387437=CARTESIAN_POINT('Ctrl Pts',(2.70917699483285,0.0580242385856641,
8.80838212259896));
#387438=CARTESIAN_POINT('Ctrl Pts',(2.73043267776197,0.0473240564541948,
8.78727029226991));
#387439=CARTESIAN_POINT('',(2.742957758327,0.0410188888571772,8.75721825406948));
#387440=CARTESIAN_POINT('Origin',(2.70526553666578,0.0599935056857609,8.75937679713137));
#387441=CARTESIAN_POINT('',(2.742957758327,0.0410188888571772,7.51860402984325));
#387442=CARTESIAN_POINT('',(2.742957758327,0.0410188888571772,7.5));
#387443=CARTESIAN_POINT('Ctrl Pts',(2.742957758327,0.041018888857177,7.51860402984325));
#387444=CARTESIAN_POINT('Ctrl Pts',(2.73312125556167,0.0459706173655847,
7.52834476460825));
#387445=CARTESIAN_POINT('Ctrl Pts',(2.72327836708068,0.0509255604646928,
7.53807742314407));
#387446=CARTESIAN_POINT('Ctrl Pts',(2.71342887847514,0.0558838260886514,
7.54780169004674));
#387447=CARTESIAN_POINT('Ctrl Pts',(2.69782782084339,0.0637374508656102,
7.5632044032688));
#387448=CARTESIAN_POINT('Ctrl Pts',(2.68221018451309,0.0715994214150438,
7.57858609112103));
#387449=CARTESIAN_POINT('Ctrl Pts',(2.66657505256398,0.0794701993177321,
7.59394543036555));
#387450=CARTESIAN_POINT('Origin',(2.90339304750862,0.230676845509359,7.5));
#387451=CARTESIAN_POINT('',(2.73995014666366,0.134807295823118,8.75721825406948));
#387452=CARTESIAN_POINT('',(2.72785477369492,0.127712598202077,8.78727029226991));
#387453=CARTESIAN_POINT('Origin',(2.6971522057523,0.109703609450326,8.75658640621094));
#387454=CARTESIAN_POINT('',(2.66618796128141,0.0915411309428337,8.85049129520029));
#387455=CARTESIAN_POINT('Ctrl Pts',(2.72785477369492,0.127712598202077,
8.78727029226991));
#387456=CARTESIAN_POINT('Ctrl Pts',(2.70732832586903,0.115672544461277,
8.80838212259895));
#387457=CARTESIAN_POINT('Ctrl Pts',(2.68677344498056,0.103615812939474,
8.82945686509571));
#387458=CARTESIAN_POINT('Ctrl Pts',(2.66618796128141,0.0915411309428339,
8.85049129520029));
#387459=CARTESIAN_POINT('',(2.66618796128141,0.0915411309428337,7.59394543036555));
#387460=CARTESIAN_POINT('',(2.66618796128141,0.0915411309428337,7.5));
#387461=CARTESIAN_POINT('',(2.73995014666366,0.134807295823118,7.51860402984325));
#387462=CARTESIAN_POINT('Ctrl Pts',(2.6661879612814,0.0915411309428325,
7.59394543036555));
#387463=CARTESIAN_POINT('Ctrl Pts',(2.68128668670342,0.100397483831588,
7.57858609112103));
#387464=CARTESIAN_POINT('Ctrl Pts',(2.69636851674212,0.10924392651449,7.56320440326857));
#387465=CARTESIAN_POINT('Ctrl Pts',(2.71143433686065,0.118080978371442,
7.54780169004651));
#387466=CARTESIAN_POINT('Ctrl Pts',(2.72094591146625,0.12366011560856,7.53807742314383));
#387467=CARTESIAN_POINT('Ctrl Pts',(2.73045111238304,0.129235514275984,
7.52834476460825));
#387468=CARTESIAN_POINT('Ctrl Pts',(2.73995014666366,0.134807295823118,
7.51860402984325));
#387469=CARTESIAN_POINT('',(2.73995014666366,0.134807295823118,7.5));
#387470=CARTESIAN_POINT('Origin',(2.66966635414557,0.0856110037871532,7.5));
#387471=CARTESIAN_POINT('Ctrl Pts',(2.66618796128141,0.0915411309428336,
8.85049129520029));
#387472=CARTESIAN_POINT('Ctrl Pts',(2.66602091584792,0.0914431482809804,
8.85097269580138));
#387473=CARTESIAN_POINT('Ctrl Pts',(2.66586023373948,0.0913391464705742,
8.85143669361005));
#387474=CARTESIAN_POINT('Ctrl Pts',(2.66569899112102,0.0912236026049601,
8.8519052845931));
#387475=CARTESIAN_POINT('Ctrl Pts',(2.66538361078493,0.0909976061313448,
8.85282181883899));
#387476=CARTESIAN_POINT('Ctrl Pts',(2.66507431377364,0.0907331070018158,
8.85372622499635));
#387477=CARTESIAN_POINT('Ctrl Pts',(2.66477626768235,0.0904142365316012,
8.85462257735071));
#387478=CARTESIAN_POINT('Ctrl Pts',(2.66452884040296,0.0901495215924372,
8.85536669723986));
#387479=CARTESIAN_POINT('Ctrl Pts',(2.66428908744706,0.0898472966107245,
8.85610498449051));
#387480=CARTESIAN_POINT('Ctrl Pts',(2.66406621442249,0.0894934834379194,
8.85681338218371));
#387481=CARTESIAN_POINT('Ctrl Pts',(2.66386395680265,0.0891723974279239,
8.85745625420285));
#387482=CARTESIAN_POINT('Ctrl Pts',(2.66367255729327,0.0888051167882957,
8.85808743050666));
#387483=CARTESIAN_POINT('Ctrl Pts',(2.66350918657662,0.0883687720236747,
8.85866804508411));
#387484=CARTESIAN_POINT('Ctrl Pts',(2.66343381086941,0.0881674520080747,
8.85893592806396));
#387485=CARTESIAN_POINT('Ctrl Pts',(2.663364569258,0.0879512552461915,8.85919241173848));
#387486=CARTESIAN_POINT('Ctrl Pts',(2.66330440212497,0.087716948144525,
8.85943017985534));
#387487=CARTESIAN_POINT('Ctrl Pts',(2.66322315868399,0.0874005641949481,
8.8597512372));
#387488=CARTESIAN_POINT('Ctrl Pts',(2.6631570132995,0.0870429475615944,
8.86004599534706));
#387489=CARTESIAN_POINT('Ctrl Pts',(2.66311700206647,0.086646500610111,
8.86026130871721));
#387490=CARTESIAN_POINT('Ctrl Pts',(2.66310235282602,0.0865013502041498,
8.86034014101235));
#387491=CARTESIAN_POINT('Ctrl Pts',(2.66309097455451,0.0863488155199414,
8.86040910639693));
#387492=CARTESIAN_POINT('Ctrl Pts',(2.66308351269328,0.0861930272568014,
8.86046313645507));
#387493=CARTESIAN_POINT('Ctrl Pts',(2.66307186852131,0.0859499209768873,
8.8605474499083));
#387494=CARTESIAN_POINT('Ctrl Pts',(2.66306959035485,0.0856922486915364,
8.86059655985668));
#387495=CARTESIAN_POINT('Ctrl Pts',(2.66307653135366,0.0854365382988978,
8.86059725258816));
#387496=CARTESIAN_POINT('Ctrl Pts',(2.66308348838895,0.0851802371130951,
8.86059794692011));
#387497=CARTESIAN_POINT('Ctrl Pts',(2.66310244018504,0.0849231365764974,
8.86056369958366));
#387498=CARTESIAN_POINT('Ctrl Pts',(2.66312860018546,0.0846789824363461,
8.86048590497774));
#387499=CARTESIAN_POINT('Ctrl Pts',(2.6631354271667,0.0846152654751113,
8.86046560290182));
#387500=CARTESIAN_POINT('Ctrl Pts',(2.66314292394457,0.0845516109627158,
8.86044257503091));
#387501=CARTESIAN_POINT('Ctrl Pts',(2.66315082626157,0.0844899820367909,
8.86041778462583));
#387502=CARTESIAN_POINT('Ctrl Pts',(2.66320399904907,0.0840752958404387,
8.86025097596201));
#387503=CARTESIAN_POINT('Ctrl Pts',(2.66328299737946,0.0836967173201699,
8.8599848982295));
#387504=CARTESIAN_POINT('Ctrl Pts',(2.66337722165791,0.0833635655048054,
8.85968173251461));
#387505=CARTESIAN_POINT('Ctrl Pts',(2.66342706090281,0.0831873472818008,
8.85952137522076));
#387506=CARTESIAN_POINT('Ctrl Pts',(2.6634819370049,0.0830203898557986,
8.85934740853961));
#387507=CARTESIAN_POINT('Ctrl Pts',(2.66353959926479,0.0828645622879688,
8.8591675900182));
#387508=CARTESIAN_POINT('Ctrl Pts',(2.66377114321049,0.0822388336055786,
8.85844552518696));
#387509=CARTESIAN_POINT('Ctrl Pts',(2.66405786076342,0.081756152345655,
8.85759444184125));
#387510=CARTESIAN_POINT('Ctrl Pts',(2.66432698402973,0.0813835977549701,
8.8568349891514));
#387511=CARTESIAN_POINT('Ctrl Pts',(2.66435514706282,0.0813446109092454,
8.85675551444999));
#387512=CARTESIAN_POINT('Ctrl Pts',(2.66438313100423,0.0813068447036919,
8.85667699793652));
#387513=CARTESIAN_POINT('Ctrl Pts',(2.66441086088838,0.0812702714858658,
8.85659965593547));
#387514=CARTESIAN_POINT('Ctrl Pts',(2.66478516027966,0.0807766043254579,
8.85555568965886));
#387515=CARTESIAN_POINT('Ctrl Pts',(2.66521618049069,0.0803562158374976,
8.85434650606346));
#387516=CARTESIAN_POINT('Ctrl Pts',(2.66570171297216,0.0800025788474723,
8.85297329937117));
#387517=CARTESIAN_POINT('Ctrl Pts',(2.66597479540906,0.0798036795880011,
8.85220095427747));
#387518=CARTESIAN_POINT('Ctrl Pts',(2.6662654192102,0.079626069787311,8.85137579139184));
#387519=CARTESIAN_POINT('Ctrl Pts',(2.66657505256398,0.0794701993177319,
8.85049129520029));
#387520=CARTESIAN_POINT('Origin',(2.66966635414557,0.0856110037871532,7.59394543036555));
#387521=CARTESIAN_POINT('Ctrl Pts',(2.66570297203574,0.0912566542213349,
7.59443877723642));
#387522=CARTESIAN_POINT('Ctrl Pts',(2.66070804944951,0.088326817706052,
7.58783886950016));
#387523=CARTESIAN_POINT('Ctrl Pts',(2.66319249388382,0.0802085224792507,
7.58559994247159));
#387524=CARTESIAN_POINT('Ctrl Pts',(2.69297010788919,0.107250545800535,
7.5667025222214));
#387525=CARTESIAN_POINT('Ctrl Pts',(2.68798240438419,0.104324943730763,
7.5600487499903));
#387526=CARTESIAN_POINT('Ctrl Pts',(2.69046113972711,0.0961522924868117,
7.55786368756705));
#387527=CARTESIAN_POINT('Ctrl Pts',(2.72018632509071,0.123214570385162,
7.5388891333356));
#387528=CARTESIAN_POINT('Ctrl Pts',(2.71516897941957,0.120271581319099,
7.5322200213728));
#387529=CARTESIAN_POINT('Ctrl Pts',(2.71767924148075,0.112067860876272,
7.53005029815327));
#387530=CARTESIAN_POINT('Ctrl Pts',(2.74735039208809,0.139148005592338,
7.51101258149734));
#387531=CARTESIAN_POINT('Ctrl Pts',(2.74227222707067,0.136169342151249,
7.5043616886572));
#387532=CARTESIAN_POINT('Ctrl Pts',(2.74484549608077,0.127954369957362,
7.50217374673251));
#387533=CARTESIAN_POINT('',(2.74339586931974,0.127106646312639,7.50366116523517));
#387534=CARTESIAN_POINT('Ctrl Pts',(2.73995014666366,0.134807295823118,
7.51860402984325));
#387535=CARTESIAN_POINT('Ctrl Pts',(2.74033106457816,0.135030728157842,
7.51734760759494));
#387536=CARTESIAN_POINT('Ctrl Pts',(2.74070538067591,0.135181311420322,
7.51608817408573));
#387537=CARTESIAN_POINT('Ctrl Pts',(2.74107721787159,0.135246310518477,
7.5148100591312));
#387538=CARTESIAN_POINT('Ctrl Pts',(2.74141403688878,0.13530518825479,7.51365231206384));
#387539=CARTESIAN_POINT('Ctrl Pts',(2.74174925362168,0.135294172160199,
7.51247773061043));
#387540=CARTESIAN_POINT('Ctrl Pts',(2.74207585482037,0.135176547737615,
7.51129758471022));
#387541=CARTESIAN_POINT('Ctrl Pts',(2.74248178281107,0.135030354013559,
7.50983079813402));
#387542=CARTESIAN_POINT('Ctrl Pts',(2.74285703348899,0.134711887061916,
7.50839324291155));
#387543=CARTESIAN_POINT('Ctrl Pts',(2.7431510019548,0.134155967632647,7.50715379678855));
#387544=CARTESIAN_POINT('Ctrl Pts',(2.7432868069155,0.133899148874757,7.50658120839351));
#387545=CARTESIAN_POINT('Ctrl Pts',(2.7434161711015,0.13355070281472,7.50598221009429));
#387546=CARTESIAN_POINT('Ctrl Pts',(2.74351469152097,0.133111005108007,
7.50545747549611));
#387547=CARTESIAN_POINT('Ctrl Pts',(2.74356726506629,0.132876368801788,
7.50517746087247));
#387548=CARTESIAN_POINT('Ctrl Pts',(2.74361182316454,0.132613247474295,
7.50491486231392));
#387549=CARTESIAN_POINT('Ctrl Pts',(2.74364554124075,0.132328330517735,
7.50468370960993));
#387550=CARTESIAN_POINT('Ctrl Pts',(2.74369596040046,0.131902289795719,
7.50433806340447));
#387551=CARTESIAN_POINT('Ctrl Pts',(2.74372310067401,0.131414673971269,
7.50405484070984));
#387552=CARTESIAN_POINT('Ctrl Pts',(2.74372441892651,0.130898283251197,
7.50385766036131));
#387553=CARTESIAN_POINT('Ctrl Pts',(2.74372455989312,0.130843063290216,
7.50383657498791));
#387554=CARTESIAN_POINT('Ctrl Pts',(2.74372441994641,0.13078753874661,7.50381643264937));
#387555=CARTESIAN_POINT('Ctrl Pts',(2.74372400668667,0.130731767333936,
7.50379723213559));
#387556=CARTESIAN_POINT('Ctrl Pts',(2.74372124804273,0.130359474910222,
7.50366906242519));
#387557=CARTESIAN_POINT('Ctrl Pts',(2.74370553153518,0.129968089106795,
7.50358235568538));
#387558=CARTESIAN_POINT('Ctrl Pts',(2.74368131449704,0.129591205506861,
7.5035341175365));
#387559=CARTESIAN_POINT('Ctrl Pts',(2.74364500378917,0.129026111203748,
7.50346178989176));
#387560=CARTESIAN_POINT('Ctrl Pts',(2.74358191457385,0.128419742215759,
7.50346967198527));
#387561=CARTESIAN_POINT('Ctrl Pts',(2.74350166414417,0.127826381449622,
7.50354272648692));
#387562=CARTESIAN_POINT('Ctrl Pts',(2.74346865548136,0.127582319884669,
7.50357277531559));
#387563=CARTESIAN_POINT('Ctrl Pts',(2.74343292777869,0.127340764385223,
7.50361331098761));
#387564=CARTESIAN_POINT('Ctrl Pts',(2.74339586932116,0.127106646312705,
7.50366116523659));
#387565=CARTESIAN_POINT('',(2.67259277500765,0.0857048484080739,7.57603338622103));
#387566=CARTESIAN_POINT('Origin',(2.68142526464665,0.0859852345169799,7.58486873427628));
#387567=CARTESIAN_POINT('Ctrl Pts',(2.74339586936632,0.127106646346087,
7.50366116529969));
#387568=CARTESIAN_POINT('Ctrl Pts',(2.71983377186153,0.113327845238031,
7.52783573079709));
#387569=CARTESIAN_POINT('Ctrl Pts',(2.69623386379653,0.099527882063393,
7.55196141284069));
#387570=CARTESIAN_POINT('Ctrl Pts',(2.67259277586597,0.0857048493196314,
7.57603338728831));
#387571=CARTESIAN_POINT('Ctrl Pts',(2.66716398335868,0.0919097993917303,
7.59639677331369));
#387572=CARTESIAN_POINT('Ctrl Pts',(2.65013468741495,0.0852708992241862,
7.59959882295478));
#387573=CARTESIAN_POINT('Ctrl Pts',(2.66740089544003,0.0792221908444998,
7.59642833564546));
#387574=CARTESIAN_POINT('Ctrl Pts',(2.66334925645134,0.0910955741732249,
7.58707626057418));
#387575=CARTESIAN_POINT('Ctrl Pts',(2.65969712411285,0.0853881911985396,
7.588099439206));
#387576=CARTESIAN_POINT('Ctrl Pts',(2.66361108188368,0.0798749947243845,
7.58710240504253));
#387577=CARTESIAN_POINT('Ctrl Pts',(2.66840548835475,0.0877250918336626,
7.58015376756928));
#387578=CARTESIAN_POINT('Ctrl Pts',(2.66656942050619,0.0855437788684957,
7.58205880659763));
#387579=CARTESIAN_POINT('Ctrl Pts',(2.66848607277801,0.0834813727234763,
7.58020924244124));
#387580=CARTESIAN_POINT('Ctrl Pts',(2.6725927741805,0.0857048483817501,
7.57603338509286));
#387581=CARTESIAN_POINT('Ctrl Pts',(2.6725927741805,0.0857048483817501,
7.57603338509286));
#387582=CARTESIAN_POINT('Ctrl Pts',(2.6725927741805,0.0857048483817501,
7.57603338509286));
#387583=CARTESIAN_POINT('Origin',(2.68142508174979,0.0859909379372544,7.58486873427624));
#387584=CARTESIAN_POINT('Ctrl Pts',(2.75064512934104,0.0371490404859579,
7.51098857897448));
#387585=CARTESIAN_POINT('Ctrl Pts',(2.74538653035493,0.0397962368661161,
7.50433767179956));
#387586=CARTESIAN_POINT('Ctrl Pts',(2.74742820050471,0.048159228799746,
7.50214974420965));
#387587=CARTESIAN_POINT('Ctrl Pts',(2.72250792447727,0.0513134038572373,
7.5388732158917));
#387588=CARTESIAN_POINT('Ctrl Pts',(2.71731233283935,0.0539288821268522,
7.53220407452064));
#387589=CARTESIAN_POINT('Ctrl Pts',(2.71929181910785,0.0622766096041079,
7.53003438070911));
#387590=CARTESIAN_POINT('Ctrl Pts',(2.69431668580073,0.065504968031232,
7.56669465659231));
#387591=CARTESIAN_POINT('Ctrl Pts',(2.68915179914344,0.0681049893104947,
7.560040858333));
#387592=CARTESIAN_POINT('Ctrl Pts',(2.69110180456681,0.0764196828692079,
7.55785582193789));
#387593=CARTESIAN_POINT('Ctrl Pts',(2.6660726882884,0.0797230911802505,
7.59443891967696));
#387594=CARTESIAN_POINT('Ctrl Pts',(2.6609003131885,0.0823268821666794,
7.58783901202978));
#387595=CARTESIAN_POINT('Ctrl Pts',(2.66285951196075,0.0905876762059419,
7.58560008491213));
#387596=CARTESIAN_POINT('',(2.7459030190682,0.0489244847659116,7.50366116523517));
#387597=CARTESIAN_POINT('Ctrl Pts',(2.74590301906857,0.0489244847659182,
7.50366116523554));
#387598=CARTESIAN_POINT('Ctrl Pts',(2.7460690228415,0.0481851740977019,
7.50350835821027));
#387599=CARTESIAN_POINT('Ctrl Pts',(2.74619756789807,0.047500167397315,
7.50345484956));
#387600=CARTESIAN_POINT('Ctrl Pts',(2.74629306618699,0.04684920961282,7.50349758195598));
#387601=CARTESIAN_POINT('Ctrl Pts',(2.74634206389154,0.0465152199930862,
7.50351950684424));
#387602=CARTESIAN_POINT('Ctrl Pts',(2.74638731968128,0.0461572930119301,
7.50357029184312));
#387603=CARTESIAN_POINT('Ctrl Pts',(2.74642147197328,0.0458109485708934,
7.50365515313923));
#387604=CARTESIAN_POINT('Ctrl Pts',(2.74647401202802,0.045278130571864,
7.50378570417639));
#387605=CARTESIAN_POINT('Ctrl Pts',(2.74650216125901,0.044757118576261,
7.50400001621911));
#387606=CARTESIAN_POINT('Ctrl Pts',(2.74650150999234,0.0442874466757047,
7.50428903009635));
#387607=CARTESIAN_POINT('Ctrl Pts',(2.74650143770675,0.0442353167081828,
7.50432110841318));
#387608=CARTESIAN_POINT('Ctrl Pts',(2.74650102779312,0.0441837942326017,
7.50435406373354));
#387609=CARTESIAN_POINT('Ctrl Pts',(2.7465002866472,0.0441329146943328,
7.50438785222352));
#387610=CARTESIAN_POINT('Ctrl Pts',(2.7464957615951,0.0438222706573802,
7.50459414719561));
#387611=CARTESIAN_POINT('Ctrl Pts',(2.7464783014936,0.043530655069155,7.50483629897752));
#387612=CARTESIAN_POINT('Ctrl Pts',(2.74644988891295,0.0432691609821475,
7.5050991045531));
#387613=CARTESIAN_POINT('Ctrl Pts',(2.74638720790626,0.0426922787616146,
7.50567888004914));
#387614=CARTESIAN_POINT('Ctrl Pts',(2.74626926975364,0.0422392055908945,
7.50637912803144));
#387615=CARTESIAN_POINT('Ctrl Pts',(2.74612291728795,0.041894615652552,
7.50710440483569));
#387616=CARTESIAN_POINT('Ctrl Pts',(2.74608702875786,0.0418101153586019,
7.50728225710685));
#387617=CARTESIAN_POINT('Ctrl Pts',(2.7460488514999,0.0417303992646909,
7.50746498566954));
#387618=CARTESIAN_POINT('Ctrl Pts',(2.74600965242202,0.0416571482609263,
7.50764697238949));
#387619=CARTESIAN_POINT('Ctrl Pts',(2.74579892896725,0.0412633710239055,
7.50862528291182));
#387620=CARTESIAN_POINT('Ctrl Pts',(2.74554319689632,0.041018725610885,
7.50965856837422));
#387621=CARTESIAN_POINT('Ctrl Pts',(2.7452737271665,0.0408647524369028,
7.51067959873204));
#387622=CARTESIAN_POINT('Ctrl Pts',(2.74512543763429,0.0407800208050494,
7.51124147302579));
#387623=CARTESIAN_POINT('Ctrl Pts',(2.74497273620065,0.0407231040803606,
7.51180065547253));
#387624=CARTESIAN_POINT('Ctrl Pts',(2.74481957364794,0.0406866658581097,
7.51235175716501));
#387625=CARTESIAN_POINT('Ctrl Pts',(2.74429033601557,0.0405607572849682,
7.51425603304535));
#387626=CARTESIAN_POINT('Ctrl Pts',(2.74369108744894,0.0406702451064588,
7.51626900505179));
#387627=CARTESIAN_POINT('Ctrl Pts',(2.74306043709656,0.0409687396572797,
7.51827788969242));
#387628=CARTESIAN_POINT('Ctrl Pts',(2.74302630510772,0.0409848947464477,
7.51838661432544));
#387629=CARTESIAN_POINT('Ctrl Pts',(2.74299207720045,0.0410016126210851,
7.51849533314856));
#387630=CARTESIAN_POINT('Ctrl Pts',(2.742957758327,0.0410188888571731,7.51860402984325));
#387631=CARTESIAN_POINT('Ctrl Pts',(2.67259277592381,0.0857048475531805,
7.57603338728985));
#387632=CARTESIAN_POINT('Ctrl Pts',(2.69707093545794,0.0734249054142994,
7.55196141284922));
#387633=CARTESIAN_POINT('Ctrl Pts',(2.7215065216773,0.0611653470353345,
7.52783573083105));
#387634=CARTESIAN_POINT('Ctrl Pts',(2.74590301911844,0.048924484734626,
7.50366116530176));
#387635=CARTESIAN_POINT('Origin',(9.235043459901E-16,2.96149868837505E-17,
7.49482233047033));
#387636=CARTESIAN_POINT('Origin',(2.73456650621404,0.126697565455592,7.49482233047033));
#387637=CARTESIAN_POINT('Origin',(0.,0.,7.50366116523517));
#387638=CARTESIAN_POINT('Origin',(2.73706558693544,0.0487670258859925,7.49482233047033));
#387639=CARTESIAN_POINT('Ctrl Pts',(2.73994923428965,0.134806760710208,
7.51860402984325));
#387640=CARTESIAN_POINT('Ctrl Pts',(2.74651277539354,0.138655944286965,
7.51860402984325));
#387641=CARTESIAN_POINT('Ctrl Pts',(2.74610810557233,0.146254136727663,
7.51860402984325));
#387642=CARTESIAN_POINT('Ctrl Pts',(2.74238632125063,0.136235989936594,
7.51041458714366));
#387643=CARTESIAN_POINT('Ctrl Pts',(2.74641689459242,0.140456042578031,
7.51004642900443));
#387644=CARTESIAN_POINT('Ctrl Pts',(2.7461079939692,0.146256232218917,7.5072913648301));
#387645=CARTESIAN_POINT('Ctrl Pts',(2.74456054006896,0.134448111381071,
7.50215815450137));
#387646=CARTESIAN_POINT('Ctrl Pts',(2.74661225767011,0.136790870303093,
7.4987716367153));
#387647=CARTESIAN_POINT('Ctrl Pts',(2.74645259066989,0.140237380138185,
7.49481588533171));
#387648=CARTESIAN_POINT('Ctrl Pts',(2.74339531939167,0.127106620832972,
7.50366171572174));
#387649=CARTESIAN_POINT('Ctrl Pts',(2.74705311126526,0.12727609315135,7.50000045605858));
#387650=CARTESIAN_POINT('Ctrl Pts',(2.74705311126525,0.127276093151474,
7.49482233047317));
#387651=CARTESIAN_POINT('Origin',(2.73362579600155,0.145589345197082,7.51860402984325));
#387652=CARTESIAN_POINT('Origin',(2.73362579600155,0.145589345197082,9.));
#387653=CARTESIAN_POINT('Origin',(2.73362579600155,0.145589345197082,8.75721825406948));
#387654=CARTESIAN_POINT('Ctrl Pts',(2.72554517444904,0.126357907884526,
8.78942910404912));
#387655=CARTESIAN_POINT('Ctrl Pts',(2.73036197956352,0.129159838859895,
8.79672699501691));
#387656=CARTESIAN_POINT('Ctrl Pts',(2.72736704093116,0.137568395725993,
8.79893251111267));
#387657=CARTESIAN_POINT('Ctrl Pts',(2.73502849441794,0.131920466747849,
8.78111911759583));
#387658=CARTESIAN_POINT('Ctrl Pts',(2.74073512981015,0.135248622787749,
8.78644465894813));
#387659=CARTESIAN_POINT('Ctrl Pts',(2.73971623505555,0.143290846687543,
8.78817647674132));
#387660=CARTESIAN_POINT('Ctrl Pts',(2.74093872560499,0.13538718613847,8.76780923932031));
#387661=CARTESIAN_POINT('Ctrl Pts',(2.7476726005194,0.139320335691617,8.76988516158374));
#387662=CARTESIAN_POINT('Ctrl Pts',(2.74742463217173,0.146875128348925,
8.77093053738832));
#387663=CARTESIAN_POINT('Ctrl Pts',(2.73978631140984,0.134711223304185,
8.75371302330492));
#387664=CARTESIAN_POINT('Ctrl Pts',(2.7463553003912,0.138547182783965,8.75300828287559));
#387665=CARTESIAN_POINT('Ctrl Pts',(2.74592098874475,0.146176462745271,
8.75267964240738));
#387666=CARTESIAN_POINT('Origin',(2.7215304230328,0.138494647576042,8.78727029226991));
#387667=CARTESIAN_POINT('Ctrl Pts',(2.66618796128141,0.0915411309428337,
8.85049129520029));
#387668=CARTESIAN_POINT('Ctrl Pts',(2.67122500331725,0.0944956731666353,
8.85711686593484));
#387669=CARTESIAN_POINT('Ctrl Pts',(2.66869591238441,0.102662953079024,
8.85933012996512));
#387670=CARTESIAN_POINT('Ctrl Pts',(2.68677347260705,0.103615829144148,
8.82945683644723));
#387671=CARTESIAN_POINT('Ctrl Pts',(2.69185232513725,0.106594895854754,
8.83607469902389));
#387672=CARTESIAN_POINT('Ctrl Pts',(2.68927998471671,0.114775061333436,
8.83829567148519));
#387673=CARTESIAN_POINT('Ctrl Pts',(2.70732829956803,0.115672529034086,
8.80838214965002));
#387674=CARTESIAN_POINT('Ctrl Pts',(2.71242719562162,0.118663352532845,
8.81501364461993));
#387675=CARTESIAN_POINT('Ctrl Pts',(2.70983317111897,0.126868219958632,
8.81722098428721));
#387676=CARTESIAN_POINT('Ctrl Pts',(2.72785477369492,0.127712598202077,
8.78727029226991));
#387677=CARTESIAN_POINT('Ctrl Pts',(2.73295451669185,0.130703918486436,
8.79393457792714));
#387678=CARTESIAN_POINT('Ctrl Pts',(2.7303578352728,0.138943861495108,8.79610912703474));
#387679=CARTESIAN_POINT('Origin',(2.65986361061929,0.102323180316798,8.85049129520029));
#387680=CARTESIAN_POINT('Ctrl Pts',(2.66657505256398,0.0794701993177319,
8.85049129520029));
#387681=CARTESIAN_POINT('Ctrl Pts',(2.67179104362696,0.0768444519090915,
8.85711686593484));
#387682=CARTESIAN_POINT('Ctrl Pts',(2.66979042840331,0.0685319131368021,
8.85933012996512));
#387683=CARTESIAN_POINT('Ctrl Pts',(2.66196054056419,0.0817931601470906,
8.86332496987232));
#387684=CARTESIAN_POINT('Ctrl Pts',(2.66239050079878,0.07719239623515,8.86648636486738));
#387685=CARTESIAN_POINT('Ctrl Pts',(2.65688884651666,0.0750457937910984,
8.87206031107456));
#387686=CARTESIAN_POINT('Ctrl Pts',(2.66170148162992,0.0889095282140474,
8.86341338519875));
#387687=CARTESIAN_POINT('Ctrl Pts',(2.66180657158416,0.0935422840608315,
8.86654584966058));
#387688=CARTESIAN_POINT('Ctrl Pts',(2.65614098496653,0.0952816175726944,
8.87215952290715));
#387689=CARTESIAN_POINT('Ctrl Pts',(2.66618796128141,0.0915411309428336,
8.85049129520029));
#387690=CARTESIAN_POINT('Ctrl Pts',(2.67122500331725,0.0944956731666351,
8.85711686593484));
#387691=CARTESIAN_POINT('Ctrl Pts',(2.66869591238441,0.102662953079024,
8.85933012996512));
#387692=CARTESIAN_POINT('Origin',(2.66095450423382,0.0683051002824203,8.85049129520029));
#387693=CARTESIAN_POINT('Ctrl Pts',(2.73043267776197,0.0473240564541944,
8.78727029226991));
#387694=CARTESIAN_POINT('Ctrl Pts',(2.73571359733862,0.0446656238138374,
8.79393457792714));
#387695=CARTESIAN_POINT('Ctrl Pts',(2.73365018604124,0.0362762407020694,
8.79610912703474));
#387696=CARTESIAN_POINT('Ctrl Pts',(2.70917696759746,0.05802425229605,8.80838214965003));
#387697=CARTESIAN_POINT('Ctrl Pts',(2.7144570101417,0.0553662611567555,
8.81501364461989));
#387698=CARTESIAN_POINT('Ctrl Pts',(2.71239400300152,0.0470120517905135,
8.81722098428721));
#387699=CARTESIAN_POINT('Ctrl Pts',(2.68789189731877,0.0687392281179318,
8.82945683644722));
#387700=CARTESIAN_POINT('Ctrl Pts',(2.69315118426123,0.0660916854182478,
8.83607469902389));
#387701=CARTESIAN_POINT('Ctrl Pts',(2.69110823399166,0.0577635165502676,
8.83829567148519));
#387702=CARTESIAN_POINT('Ctrl Pts',(2.66657505256398,0.0794701993177318,
8.85049129520029));
#387703=CARTESIAN_POINT('Ctrl Pts',(2.67179104362696,0.0768444519090914,
8.85711686593484));
#387704=CARTESIAN_POINT('Ctrl Pts',(2.66979042840331,0.0685319131368021,
8.85933012996512));
#387705=CARTESIAN_POINT('Origin',(2.72481212943181,0.0361589574188829,8.78727029226991));
#387706=CARTESIAN_POINT('Ctrl Pts',(2.74279236264415,0.0411021289464723,
8.75374538247848));
#387707=CARTESIAN_POINT('Ctrl Pts',(2.74958571518574,0.0376970240092931,
8.75304829418602));
#387708=CARTESIAN_POINT('Ctrl Pts',(2.74964669889166,0.0300637465875896,
8.75272238421917));
#387709=CARTESIAN_POINT('Ctrl Pts',(2.74397138271649,0.0405086067622311,
8.7676940844502));
#387710=CARTESIAN_POINT('Ctrl Pts',(2.75093537691271,0.0370171973323222,
8.76974318093968));
#387711=CARTESIAN_POINT('Ctrl Pts',(2.75117499675544,0.0294699501778223,
8.7707786988043));
#387712=CARTESIAN_POINT('Ctrl Pts',(2.73792839747585,0.043550663384532,
8.78108014887989));
#387713=CARTESIAN_POINT('Ctrl Pts',(2.74383183450135,0.0405952161110573,
8.78639403366326));
#387714=CARTESIAN_POINT('Ctrl Pts',(2.74335079698391,0.0325149513483312,
8.78812224174741));
#387715=CARTESIAN_POINT('Ctrl Pts',(2.72802527865339,0.0485359226161603,
8.78944554828685));
#387716=CARTESIAN_POINT('Ctrl Pts',(2.73300298241106,0.0460501867255351,
8.79673892988686));
#387717=CARTESIAN_POINT('Ctrl Pts',(2.73055804701899,0.0374754654329649,
8.79894799272499));
#387718=CARTESIAN_POINT('Origin',(2.73733720999684,0.0298537898218656,8.75721825406948));
#387719=CARTESIAN_POINT('Origin',(2.73733720999684,0.0298537898218656,9.));
#387720=CARTESIAN_POINT('Origin',(2.73733720999684,0.0298537898218657,7.51860402984325));
#387721=CARTESIAN_POINT('Ctrl Pts',(2.74590223252928,0.0489244707518819,
7.50366195182966));
#387722=CARTESIAN_POINT('Ctrl Pts',(2.74956360331414,0.0489897063693508,
7.50000065167735));
#387723=CARTESIAN_POINT('Ctrl Pts',(2.74956360331415,0.0489897063692339,
7.49482233047108));
#387724=CARTESIAN_POINT('Ctrl Pts',(2.74753601636502,0.0416660583920878,
7.50215800491338));
#387725=CARTESIAN_POINT('Ctrl Pts',(2.74973341113686,0.0394578569992938,
7.49877273257265));
#387726=CARTESIAN_POINT('Ctrl Pts',(2.74979493244485,0.0360062817823014,
7.49481816995647));
#387727=CARTESIAN_POINT('Ctrl Pts',(2.7454754935513,0.0397518321577599,
7.51043025814042));
#387728=CARTESIAN_POINT('Ctrl Pts',(2.74977310304522,0.0357991989057975,
7.51006209594515));
#387729=CARTESIAN_POINT('Ctrl Pts',(2.74983649427474,0.0299875767816046,
7.507312818217));
#387730=CARTESIAN_POINT('Ctrl Pts',(2.74295640828482,0.0410195683706412,
7.51860402984326));
#387731=CARTESIAN_POINT('Ctrl Pts',(2.7497534837955,0.0375989278030361,
7.51860402984326));
#387732=CARTESIAN_POINT('Ctrl Pts',(2.74983646666349,0.0299901084968461,
7.51860402984327));
#387733=CARTESIAN_POINT('Origin',(0.,0.,7.5));
#387734=CARTESIAN_POINT('Origin',(2.66618796128141,-0.0915411309427755,
7.5));
#387735=CARTESIAN_POINT('',(2.66618796128141,-0.0915411309427755,7.59394543036555));
#387736=CARTESIAN_POINT('',(2.66618796128141,-0.0915411309427755,8.85049129520029));
#387737=CARTESIAN_POINT('',(2.66618796128141,-0.0915411309427755,7.5));
#387738=CARTESIAN_POINT('',(2.72785477369492,-0.127712598202018,8.78727029226991));
#387739=CARTESIAN_POINT('Ctrl Pts',(2.66618796128141,-0.0915411309427756,
8.85049129520029));
#387740=CARTESIAN_POINT('Ctrl Pts',(2.68677344498056,-0.103615812939416,
8.82945686509571));
#387741=CARTESIAN_POINT('Ctrl Pts',(2.70732832586904,-0.115672544461219,
8.80838212259896));
#387742=CARTESIAN_POINT('Ctrl Pts',(2.72785477369492,-0.127712598202018,
8.78727029226991));
#387743=CARTESIAN_POINT('',(2.73995014666367,-0.134807295823058,8.75721825406948));
#387744=CARTESIAN_POINT('Origin',(2.70355107558665,-0.113456715445245,8.75937679713058));
#387745=CARTESIAN_POINT('',(2.73995014666367,-0.134807295823058,7.51860402984325));
#387746=CARTESIAN_POINT('',(2.73995014666367,-0.134807295823058,7.5));
#387747=CARTESIAN_POINT('Ctrl Pts',(2.73995014666367,-0.134807295823058,
7.51860402984325));
#387748=CARTESIAN_POINT('Ctrl Pts',(2.73045111238304,-0.129235514275926,
7.52834476460825));
#387749=CARTESIAN_POINT('Ctrl Pts',(2.72094591146644,-0.123660115608609,
7.53807742314407));
#387750=CARTESIAN_POINT('Ctrl Pts',(2.71143433686084,-0.118080978371492,
7.54780169004674));
#387751=CARTESIAN_POINT('Ctrl Pts',(2.69636851674231,-0.109243926514539,
7.5632044032688));
#387752=CARTESIAN_POINT('Ctrl Pts',(2.68128668670343,-0.100397483831532,
7.57858609112103));
#387753=CARTESIAN_POINT('Ctrl Pts',(2.66618796128141,-0.0915411309427754,
7.59394543036555));
#387754=CARTESIAN_POINT('Origin',(2.91220723134083,0.0441818639458939,7.5));
#387755=CARTESIAN_POINT('',(2.742957758327,-0.0410188888571173,8.75721825406948));
#387756=CARTESIAN_POINT('',(2.73043267776197,-0.047324056454135,8.78727029226991));
#387757=CARTESIAN_POINT('Origin',(2.69863935166543,-0.0633289235258057,
8.75658640621032));
#387758=CARTESIAN_POINT('',(2.66657505256398,-0.0794701993176737,8.85049129520029));
#387759=CARTESIAN_POINT('Ctrl Pts',(2.73043267776197,-0.0473240564541348,
8.78727029226991));
#387760=CARTESIAN_POINT('Ctrl Pts',(2.70917699483285,-0.0580242385856055,
8.80838212259896));
#387761=CARTESIAN_POINT('Ctrl Pts',(2.68789186871081,-0.0687392425192154,
8.82945686509571));
#387762=CARTESIAN_POINT('Ctrl Pts',(2.66657505256398,-0.0794701993176736,
8.85049129520029));
#387763=CARTESIAN_POINT('',(2.66657505256398,-0.0794701993176737,7.59394543036555));
#387764=CARTESIAN_POINT('',(2.66657505256398,-0.0794701993176737,7.5));
#387765=CARTESIAN_POINT('',(2.742957758327,-0.0410188888571173,7.51860402984325));
#387766=CARTESIAN_POINT('Ctrl Pts',(2.66657505256398,-0.0794701993176739,
7.59394543036555));
#387767=CARTESIAN_POINT('Ctrl Pts',(2.68221018451309,-0.0715994214149867,
7.57858609112103));
#387768=CARTESIAN_POINT('Ctrl Pts',(2.6978278208432,-0.0637374508656468,
7.56320440326857));
#387769=CARTESIAN_POINT('Ctrl Pts',(2.71342887847495,-0.0558838260886891,
7.54780169004651));
#387770=CARTESIAN_POINT('Ctrl Pts',(2.72327836708049,-0.0509255604647293,
7.53807742314383));
#387771=CARTESIAN_POINT('Ctrl Pts',(2.73312125556166,-0.0459706173655272,
7.52834476460825));
#387772=CARTESIAN_POINT('Ctrl Pts',(2.742957758327,-0.0410188888571183,
7.51860402984325));
#387773=CARTESIAN_POINT('',(2.742957758327,-0.0410188888571173,7.5));
#387774=CARTESIAN_POINT('Origin',(2.66966635414557,-0.0856110037870949,
7.5));
#387775=CARTESIAN_POINT('Ctrl Pts',(2.66657505256398,-0.0794701993176738,
8.85049129520029));
#387776=CARTESIAN_POINT('Ctrl Pts',(2.66640207257255,-0.079557278025969,
8.85097269580138));
#387777=CARTESIAN_POINT('Ctrl Pts',(2.66623505718387,-0.0796507712154674,
8.85143669361005));
#387778=CARTESIAN_POINT('Ctrl Pts',(2.66606674293477,-0.079755746833782,
8.8519052845931));
#387779=CARTESIAN_POINT('Ctrl Pts',(2.66573753093763,-0.0799610724858936,
8.85282181883899));
#387780=CARTESIAN_POINT('Ctrl Pts',(2.66541192289281,-0.0802052114460414,
8.85372622499636));
#387781=CARTESIAN_POINT('Ctrl Pts',(2.66509405906801,-0.0805043308840431,
8.85462257735071));
#387782=CARTESIAN_POINT('Ctrl Pts',(2.66483017981012,-0.0807526492177544,
8.85536669723986));
#387783=CARTESIAN_POINT('Ctrl Pts',(2.66457155583132,-0.0810388922212037,
8.85610498449051));
#387784=CARTESIAN_POINT('Ctrl Pts',(2.66432647183546,-0.0813776989231866,
8.85681338218371));
#387785=CARTESIAN_POINT('Ctrl Pts',(2.66410405772431,-0.0816851665373423,
8.85745625420284));
#387786=CARTESIAN_POINT('Ctrl Pts',(2.66388951971436,-0.0820394295508348,
8.85808743050666));
#387787=CARTESIAN_POINT('Ctrl Pts',(2.66369852795532,-0.0824644106005847,
8.85866804508411));
#387788=CARTESIAN_POINT('Ctrl Pts',(2.6636104084979,-0.0826604876444791,
8.85893592806396));
#387789=CARTESIAN_POINT('Ctrl Pts',(2.66352745737671,-0.0828718038816539,
8.85919241173848));
#387790=CARTESIAN_POINT('Ctrl Pts',(2.66345240175596,-0.083101774652802,
8.85943017985534));
#387791=CARTESIAN_POINT('Ctrl Pts',(2.6633510544491,-0.0834123032724869,
8.8597512372));
#387792=CARTESIAN_POINT('Ctrl Pts',(2.66326213239103,-0.0837649471947781,
8.86004599534705));
#387793=CARTESIAN_POINT('Ctrl Pts',(2.66319680292198,-0.0841580160749788,
8.86026130871721));
#387794=CARTESIAN_POINT('Ctrl Pts',(2.66317288396152,-0.0843019296738054,
8.86034014101235));
#387795=CARTESIAN_POINT('Ctrl Pts',(2.66315175613712,-0.0844534219507867,
8.86040910639693));
#387796=CARTESIAN_POINT('Ctrl Pts',(2.66313432821879,-0.084608412047141,
8.86046313645507));
#387797=CARTESIAN_POINT('Ctrl Pts',(2.66310713209819,-0.0848502727944706,
8.8605474499083));
#387798=CARTESIAN_POINT('Ctrl Pts',(2.66308834949246,-0.0851072697018491,
8.86059655985668));
#387799=CARTESIAN_POINT('Ctrl Pts',(2.66307889280913,-0.0853628994213819,
8.86059725258815));
#387800=CARTESIAN_POINT('Ctrl Pts',(2.66306941427709,-0.0856191197476916,
8.86059794692011));
#387801=CARTESIAN_POINT('Ctrl Pts',(2.66307185464675,-0.0858769062894076,
8.86056369958366));
#387802=CARTESIAN_POINT('Ctrl Pts',(2.66308231788918,-0.0861222348656741,
8.86048590497774));
#387803=CARTESIAN_POINT('Ctrl Pts',(2.66308504848392,-0.0861862583197678,
8.86046560290182));
#387804=CARTESIAN_POINT('Ctrl Pts',(2.66308845150025,-0.0862502623673478,
8.86044257503091));
#387805=CARTESIAN_POINT('Ctrl Pts',(2.66309238900225,-0.0863122709732237,
8.86041778462583));
#387806=CARTESIAN_POINT('Ctrl Pts',(2.66311888350473,-0.0867295119445019,
8.860250975962));
#387807=CARTESIAN_POINT('Ctrl Pts',(2.66317346391551,-0.0871123740750049,
8.8599848982295));
#387808=CARTESIAN_POINT('Ctrl Pts',(2.66324614948998,-0.0874508783644821,
8.85968173251461));
#387809=CARTESIAN_POINT('Ctrl Pts',(2.66328459599449,-0.087629927739632,
8.85952137522076));
#387810=CARTESIAN_POINT('Ctrl Pts',(2.66332866234873,-0.0878000580576296,
8.85934740853961));
#387811=CARTESIAN_POINT('Ctrl Pts',(2.66337622222878,-0.0879592598946845,
8.8591675900182));
#387812=CARTESIAN_POINT('Ctrl Pts',(2.66356719986828,-0.0885985380219406,
8.85844552518694));
#387813=CARTESIAN_POINT('Ctrl Pts',(2.66382240283475,-0.0890985976181462,
8.85759444184121));
#387814=CARTESIAN_POINT('Ctrl Pts',(2.66406710350387,-0.0894876295423471,
8.85683498915134));
#387815=CARTESIAN_POINT('Ctrl Pts',(2.6640927107772,-0.0895283406971303,
8.85675551444995));
#387816=CARTESIAN_POINT('Ctrl Pts',(2.6641182175335,-0.0895678222452359,
8.8566769979365));
#387817=CARTESIAN_POINT('Ctrl Pts',(2.66414354718951,-0.0896060969792316,
8.85659965593547));
#387818=CARTESIAN_POINT('Ctrl Pts',(2.66448544817898,-0.0901227312918511,
8.85555568965886));
#387819=CARTESIAN_POINT('Ctrl Pts',(2.66488864842986,-0.0905698716063139,
8.85434650606346));
#387820=CARTESIAN_POINT('Ctrl Pts',(2.66535052573303,-0.0909538901841117,
8.85297329937117));
#387821=CARTESIAN_POINT('Ctrl Pts',(2.66561030357347,-0.0911698772355271,
8.85220095427747));
#387822=CARTESIAN_POINT('Ctrl Pts',(2.66588895075784,-0.0913657424487038,
8.85137579139183));
#387823=CARTESIAN_POINT('Ctrl Pts',(2.66618796128141,-0.0915411309427756,
8.85049129520029));
#387824=CARTESIAN_POINT('Origin',(2.66966635414557,-0.085611003787095,7.59394543036555));
#387825=CARTESIAN_POINT('Ctrl Pts',(2.66607283329461,-0.0797230181835804,
7.59443877723642));
#387826=CARTESIAN_POINT('Ctrl Pts',(2.6609004580425,-0.0823268092466323,
7.58783886950016));
#387827=CARTESIAN_POINT('Ctrl Pts',(2.6628596569582,-0.0905876034666415,
7.58559994247159));
#387828=CARTESIAN_POINT('Ctrl Pts',(2.69430867804487,-0.0655089991623543,
7.56670252222138));
#387829=CARTESIAN_POINT('Ctrl Pts',(2.68914377834347,-0.0681090270081297,
7.56004874999028));
#387830=CARTESIAN_POINT('Ctrl Pts',(2.69109379729576,-0.0764236997822774,
7.55786368756705));
#387831=CARTESIAN_POINT('Ctrl Pts',(2.72249179517612,-0.0513215234015166,
7.53888913333557));
#387832=CARTESIAN_POINT('Ctrl Pts',(2.71729620022289,-0.0539370033400398,
7.53222002137276));
#387833=CARTESIAN_POINT('Ctrl Pts',(2.71927569050806,-0.0622847014018507,
7.53005029815326));
#387834=CARTESIAN_POINT('Ctrl Pts',(2.75062090938332,-0.0371612328939121,
7.51101258149734));
#387835=CARTESIAN_POINT('Ctrl Pts',(2.74536233437864,-0.0398084172017366,
7.5043616886572));
#387836=CARTESIAN_POINT('Ctrl Pts',(2.74740398125597,-0.0481713807657444,
7.50217374673251));
#387837=CARTESIAN_POINT('',(2.7459030190682,-0.0489244847658516,7.50366116523517));
#387838=CARTESIAN_POINT('Ctrl Pts',(2.742957758327,-0.0410188888571166,
7.51860402984325));
#387839=CARTESIAN_POINT('Ctrl Pts',(2.74335220896362,-0.0408203210826641,
7.51734760759494));
#387840=CARTESIAN_POINT('Ctrl Pts',(2.74373540389156,-0.0406940297243718,
7.51608817408573));
#387841=CARTESIAN_POINT('Ctrl Pts',(2.74411064161436,-0.0406529878647593,
7.51481005913119));
#387842=CARTESIAN_POINT('Ctrl Pts',(2.74445054091028,-0.0406158111675953,
7.51365231206383));
#387843=CARTESIAN_POINT('Ctrl Pts',(2.74478436310084,-0.0406482820382562,
7.51247773061042));
#387844=CARTESIAN_POINT('Ctrl Pts',(2.74510275703971,-0.0407865901994944,
7.51129758471022));
#387845=CARTESIAN_POINT('Ctrl Pts',(2.74549848434376,-0.0409584914485253,
7.50983079813402));
#387846=CARTESIAN_POINT('Ctrl Pts',(2.74585255978126,-0.0413003464691425,
7.50839324291155));
#387847=CARTESIAN_POINT('Ctrl Pts',(2.7461103063772,-0.041873958326594,
7.50715379678855));
#387848=CARTESIAN_POINT('Ctrl Pts',(2.74622937787774,-0.042138950476508,
7.50658120839351));
#387849=CARTESIAN_POINT('Ctrl Pts',(2.74633615125543,-0.0424949690085999,
7.50598221009429));
#387850=CARTESIAN_POINT('Ctrl Pts',(2.74640629772533,-0.0429400755341653,
7.50545747549611));
#387851=CARTESIAN_POINT('Ctrl Pts',(2.74644373005291,-0.0431775981535425,
7.50517746087247));
#387852=CARTESIAN_POINT('Ctrl Pts',(2.74647133836043,-0.0434430337172053,
7.50491486231392));
#387853=CARTESIAN_POINT('Ctrl Pts',(2.74648673246716,-0.0437295256058809,
7.50468370960992));
#387854=CARTESIAN_POINT('Ctrl Pts',(2.74650975151252,-0.0441579213481969,
7.50433806340446));
#387855=CARTESIAN_POINT('Ctrl Pts',(2.74650559437033,-0.0446462741969396,
7.50405484070983));
#387856=CARTESIAN_POINT('Ctrl Pts',(2.7464738246473,-0.0451616883976252,
7.5038576603613));
#387857=CARTESIAN_POINT('Ctrl Pts',(2.74647042736924,-0.0452168039350331,
7.50383657498791));
#387858=CARTESIAN_POINT('Ctrl Pts',(2.74646673024033,-0.0452722054310887,
7.50381643264937));
#387859=CARTESIAN_POINT('Ctrl Pts',(2.746462744543,-0.0453278357777696,
7.50379723213559));
#387860=CARTESIAN_POINT('Ctrl Pts',(2.74643613870952,-0.0456991865398469,
7.50366906242519));
#387861=CARTESIAN_POINT('Ctrl Pts',(2.74639537831869,-0.0460887612390686,
7.50358235568538));
#387862=CARTESIAN_POINT('Ctrl Pts',(2.74634706402189,-0.0464633189002641,
7.5035341175365));
#387863=CARTESIAN_POINT('Ctrl Pts',(2.74627462220197,-0.0470249257214849,
7.50346178989177));
#387864=CARTESIAN_POINT('Ctrl Pts',(2.74617281241575,-0.0476260067194501,
7.50346967198527));
#387865=CARTESIAN_POINT('Ctrl Pts',(2.74605471011437,-0.0482130066995723,
7.50354272648693));
#387866=CARTESIAN_POINT('Ctrl Pts',(2.74600613219324,-0.0484544519415771,
7.50357277531559));
#387867=CARTESIAN_POINT('Ctrl Pts',(2.74595500138299,-0.048693222057574,
7.50361331098762));
#387868=CARTESIAN_POINT('Ctrl Pts',(2.74590301906962,-0.0489244847658769,
7.50366116523659));
#387869=CARTESIAN_POINT('',(2.67259277500764,-0.0857048484084028,7.57603338622103));
#387870=CARTESIAN_POINT('Origin',(2.68142508174926,-0.0859909379370269,
7.5848687342763));
#387871=CARTESIAN_POINT('Ctrl Pts',(2.74590301911683,-0.048924484735458,
7.50366116529969));
#387872=CARTESIAN_POINT('Ctrl Pts',(2.72150652165033,-0.0611653470485443,
7.52783573079709));
#387873=CARTESIAN_POINT('Ctrl Pts',(2.69707093545121,-0.0734249054175328,
7.55196141284069));
#387874=CARTESIAN_POINT('Ctrl Pts',(2.6725927759226,-0.0857048475537104,
7.57603338728831));
#387875=CARTESIAN_POINT('Ctrl Pts',(2.66757268996768,-0.0791648222868913,
7.59639677331372));
#387876=CARTESIAN_POINT('Ctrl Pts',(2.64933465654094,-0.0849590058181688,
7.59974925422226));
#387877=CARTESIAN_POINT('Ctrl Pts',(2.66716398335852,-0.0919097993916128,
7.59639677331371));
#387878=CARTESIAN_POINT('Ctrl Pts',(2.66371363323709,-0.0797329642003548,
7.58707626057423));
#387879=CARTESIAN_POINT('Ctrl Pts',(2.65963383141741,-0.0852892803103274,
7.58811717123965));
#387880=CARTESIAN_POINT('Ctrl Pts',(2.66334925645125,-0.0910955741730033,
7.58707626057423));
#387881=CARTESIAN_POINT('Ctrl Pts',(2.66854352902493,-0.083420475412555,
7.5801537675693));
#387882=CARTESIAN_POINT('Ctrl Pts',(2.66654166217443,-0.0855108009974158,
7.58208760766041));
#387883=CARTESIAN_POINT('Ctrl Pts',(2.66840548835473,-0.0877250918336702,
7.58015376756929));
#387884=CARTESIAN_POINT('Ctrl Pts',(2.6725927741805,-0.0857048483816766,
7.57603338509286));
#387885=CARTESIAN_POINT('Ctrl Pts',(2.6725927741805,-0.0857048483816766,
7.57603338509286));
#387886=CARTESIAN_POINT('Ctrl Pts',(2.6725927741805,-0.0857048483816766,
7.57603338509286));
#387887=CARTESIAN_POINT('Origin',(2.68142526464748,-0.0859852345167185,
7.5848687342762));
#387888=CARTESIAN_POINT('Ctrl Pts',(2.74737378111305,-0.139161724727701,
7.51098857897448));
#387889=CARTESIAN_POINT('Ctrl Pts',(2.74229559293695,-0.136183047702587,
7.50433767179956));
#387890=CARTESIAN_POINT('Ctrl Pts',(2.74486888698932,-0.127968048688437,
7.50214974420965));
#387891=CARTESIAN_POINT('Ctrl Pts',(2.72020190103146,-0.123223706654822,
7.53887321589169));
#387892=CARTESIAN_POINT('Ctrl Pts',(2.71518455856187,-0.120280719466635,
7.53220407452062));
#387893=CARTESIAN_POINT('Ctrl Pts',(2.71769481849935,-0.112076969411449,
7.53003438070911));
#387894=CARTESIAN_POINT('Ctrl Pts',(2.69297784091681,-0.107255081707945,
7.56669465659233));
#387895=CARTESIAN_POINT('Ctrl Pts',(2.68799015000838,-0.104329487026956,
7.560040858333));
#387896=CARTESIAN_POINT('Ctrl Pts',(2.69046887318185,-0.0961568141743312,
7.55785582193789));
#387897=CARTESIAN_POINT('Ctrl Pts',(2.66570283200437,-0.091256572084064,
7.59443891967696));
#387898=CARTESIAN_POINT('Ctrl Pts',(2.66070790956513,-0.088326735654999,
7.58783901202978));
#387899=CARTESIAN_POINT('Ctrl Pts',(2.6631923538447,-0.0802084405993816,
7.58560008491213));
#387900=CARTESIAN_POINT('',(2.74339586931974,-0.12710664631258,7.50366116523517));
#387901=CARTESIAN_POINT('Ctrl Pts',(2.74339586932012,-0.127106646312597,
7.50366116523554));
#387902=CARTESIAN_POINT('Ctrl Pts',(2.74351416422334,-0.127855073886004,
7.50350835821027));
#387903=CARTESIAN_POINT('Ctrl Pts',(2.74359855664032,-0.12854690907671,
7.50345484955999));
#387904=CARTESIAN_POINT('Ctrl Pts',(2.74365215170931,-0.129202647995,7.50349758195598));
#387905=CARTESIAN_POINT('Ctrl Pts',(2.74367964995442,-0.129539090690949,
7.50351950684424));
#387906=CARTESIAN_POINT('Ctrl Pts',(2.74370188030086,-0.129899181821139,
7.50357029184312));
#387907=CARTESIAN_POINT('Ctrl Pts',(2.7437137720588,-0.130247002805238,
7.50365515313923));
#387908=CARTESIAN_POINT('Ctrl Pts',(2.74373206639795,-0.130782092325406,
7.50378570417639));
#387909=CARTESIAN_POINT('Ctrl Pts',(2.74372677644015,-0.131303837373406,
7.50400001621911));
#387910=CARTESIAN_POINT('Ctrl Pts',(2.7436960345296,-0.13177250255587,7.50428903009634));
#387911=CARTESIAN_POINT('Ctrl Pts',(2.74369262241404,-0.131824520785431,
7.50432110841318));
#387912=CARTESIAN_POINT('Ctrl Pts',(2.74368891228627,-0.131875911139305,
7.50435406373354));
#387913=CARTESIAN_POINT('Ctrl Pts',(2.7436849127999,-0.131926638654725,
7.50438785222352));
#387914=CARTESIAN_POINT('Ctrl Pts',(2.74366049401323,-0.132236354519104,
7.50459414719561));
#387915=CARTESIAN_POINT('Ctrl Pts',(2.74362438591049,-0.132526252279283,
7.50483629897752));
#387916=CARTESIAN_POINT('Ctrl Pts',(2.74357927772286,-0.132785388698351,
7.5050991045531));
#387917=CARTESIAN_POINT('Ctrl Pts',(2.74347976453025,-0.133357069666604,
7.50567888004914));
#387918=CARTESIAN_POINT('Ctrl Pts',(2.7433330401965,-0.13380165562652,7.50637912803144));
#387919=CARTESIAN_POINT('Ctrl Pts',(2.74316491047449,-0.134136160733206,
7.50710440483569));
#387920=CARTESIAN_POINT('Ctrl Pts',(2.74312368172882,-0.134218188026222,
7.50728225710685));
#387921=CARTESIAN_POINT('Ctrl Pts',(2.74308047548245,-0.134295294309552,
7.50746498566954));
#387922=CARTESIAN_POINT('Ctrl Pts',(2.74303666373536,-0.134365883317731,
7.50764697238949));
#387923=CARTESIAN_POINT('Ctrl Pts',(2.74280114384032,-0.134745350399082,
7.50862528291182));
#387924=CARTESIAN_POINT('Ctrl Pts',(2.74253026271293,-0.134973108351822,
7.50965856837422));
#387925=CARTESIAN_POINT('Ctrl Pts',(2.74225148154245,-0.135109500186538,
7.51067959873203));
#387926=CARTESIAN_POINT('Ctrl Pts',(2.74209806791269,-0.135184556785218,
7.51124147302579));
#387927=CARTESIAN_POINT('Ctrl Pts',(2.74194203355346,-0.135231572953947,
7.51180065547253));
#387928=CARTESIAN_POINT('Ctrl Pts',(2.74178685108471,-0.135258123151517,
7.51235175716501));
#387929=CARTESIAN_POINT('Ctrl Pts',(2.74125063383784,-0.135349864660465,
7.51425603304536));
#387930=CARTESIAN_POINT('Ctrl Pts',(2.74065963140047,-0.135202207805959,
7.5162690050518));
#387931=CARTESIAN_POINT('Ctrl Pts',(2.74004940139841,-0.134863920637395,
7.51827788969243));
#387932=CARTESIAN_POINT('Ctrl Pts',(2.74001637459752,-0.134845611896558,
7.51838661432545));
#387933=CARTESIAN_POINT('Ctrl Pts',(2.73998328813306,-0.13482673538104,
7.51849533314857));
#387934=CARTESIAN_POINT('Ctrl Pts',(2.73995014666366,-0.134807295823061,
7.51860402984325));
#387935=CARTESIAN_POINT('Ctrl Pts',(2.67259277586714,-0.0857048493202394,
7.57603338728985));
#387936=CARTESIAN_POINT('Ctrl Pts',(2.69623386380305,-0.0995278820670532,
7.55196141284922));
#387937=CARTESIAN_POINT('Ctrl Pts',(2.71983377188761,-0.113327845252912,
7.52783573083104));
#387938=CARTESIAN_POINT('Ctrl Pts',(2.74339586936787,-0.127106646347019,
7.50366116530176));
#387939=CARTESIAN_POINT('Origin',(9.23504345990101E-16,-2.96149868837303E-17,
7.49482233047033));
#387940=CARTESIAN_POINT('Origin',(2.73706558693544,-0.0487670258859327,
7.49482233047033));
#387941=CARTESIAN_POINT('Origin',(0.,0.,7.50366116523517));
#387942=CARTESIAN_POINT('Origin',(2.73456650621404,-0.126697565455532,7.49482233047033));
#387943=CARTESIAN_POINT('Ctrl Pts',(2.74295681354276,-0.0410193644145763,
7.51860402984325));
#387944=CARTESIAN_POINT('Ctrl Pts',(2.74975348718602,-0.0375986169206801,
7.51860402984325));
#387945=CARTESIAN_POINT('Ctrl Pts',(2.74983646666349,-0.0299901084967906,
7.51860402984325));
#387946=CARTESIAN_POINT('Ctrl Pts',(2.74548046427813,-0.0397492163906277,
7.51041458714366));
#387947=CARTESIAN_POINT('Ctrl Pts',(2.74977313607578,-0.0357960740205906,
7.51004642900442));
#387948=CARTESIAN_POINT('Ctrl Pts',(2.74983648954825,-0.0299880101605093,
7.5072913648301));
#387949=CARTESIAN_POINT('Ctrl Pts',(2.74753566615837,-0.0416727242358742,
7.50215815450137));
#387950=CARTESIAN_POINT('Ctrl Pts',(2.74973326936515,-0.0394662327613699,
7.49877163671529));
#387951=CARTESIAN_POINT('Ctrl Pts',(2.74979474906121,-0.0360165742505425,
7.49481588533171));
#387952=CARTESIAN_POINT('Ctrl Pts',(2.74590246863753,-0.0489244749591564,
7.50366171572174));
#387953=CARTESIAN_POINT('Ctrl Pts',(2.74956360331413,-0.0489897063698166,
7.50000045605858));
#387954=CARTESIAN_POINT('Ctrl Pts',(2.74956360331414,-0.048989706369692,
7.49482233047317));
#387955=CARTESIAN_POINT('Origin',(2.73733720999684,-0.0298537898218058,
7.51860402984325));
#387956=CARTESIAN_POINT('Origin',(2.73733720999684,-0.0298537898218058,
9.));
#387957=CARTESIAN_POINT('Origin',(2.73733720999684,-0.0298537898218059,
8.75721825406948));
#387958=CARTESIAN_POINT('Ctrl Pts',(2.72804102852879,-0.0485279868833891,
8.78942910404912));
#387959=CARTESIAN_POINT('Ctrl Pts',(2.73302745733453,-0.0460404265390077,
8.79672699501691));
#387960=CARTESIAN_POINT('Ctrl Pts',(2.73057741021293,-0.0374572595777989,
8.79893251111267));
#387961=CARTESIAN_POINT('Ctrl Pts',(2.73786125836976,-0.0435844552903896,
8.78111911759582));
#387962=CARTESIAN_POINT('Ctrl Pts',(2.74376940455713,-0.0406287626889416,
8.78644465894813));
#387963=CARTESIAN_POINT('Ctrl Pts',(2.74326787028548,-0.0325377815896124,
8.78817647674133));
#387964=CARTESIAN_POINT('Ctrl Pts',(2.74398145982693,-0.0405035284588546,
8.7678092393203));
#387965=CARTESIAN_POINT('Ctrl Pts',(2.7509534970302,-0.037009900830377,
8.76988516158373));
#387966=CARTESIAN_POINT('Ctrl Pts',(2.75119007538758,-0.0294547429182473,
8.77093053738833));
#387967=CARTESIAN_POINT('Ctrl Pts',(2.74278810430285,-0.0411042670240045,
8.75371302330492));
#387968=CARTESIAN_POINT('Ctrl Pts',(2.74958936735954,-0.0376970655034697,
8.75300828287559));
#387969=CARTESIAN_POINT('Ctrl Pts',(2.74964475769837,-0.0300556342733529,
8.75267964240738));
#387970=CARTESIAN_POINT('Origin',(2.72481212943181,-0.0361589574188236,
8.78727029226991));
#387971=CARTESIAN_POINT('Ctrl Pts',(2.66657505256398,-0.0794701993176737,
8.85049129520029));
#387972=CARTESIAN_POINT('Ctrl Pts',(2.67179104362696,-0.0768444519090332,
8.85711686593484));
#387973=CARTESIAN_POINT('Ctrl Pts',(2.66979042840332,-0.0685319131367439,
8.85933012996512));
#387974=CARTESIAN_POINT('Ctrl Pts',(2.68789189731878,-0.0687392281178691,
8.82945683644722));
#387975=CARTESIAN_POINT('Ctrl Pts',(2.69315118426121,-0.06609168541817,
8.83607469902389));
#387976=CARTESIAN_POINT('Ctrl Pts',(2.69110823399166,-0.0577635165501877,
8.83829567148519));
#387977=CARTESIAN_POINT('Ctrl Pts',(2.70917696759746,-0.0580242522959924,
8.80838214965003));
#387978=CARTESIAN_POINT('Ctrl Pts',(2.71445701014171,-0.0553662611567007,
8.81501364461988));
#387979=CARTESIAN_POINT('Ctrl Pts',(2.71239400300152,-0.0470120517904646,
8.81722098428721));
#387980=CARTESIAN_POINT('Ctrl Pts',(2.73043267776197,-0.0473240564541349,
8.78727029226991));
#387981=CARTESIAN_POINT('Ctrl Pts',(2.73571359733862,-0.0446656238137779,
8.79393457792714));
#387982=CARTESIAN_POINT('Ctrl Pts',(2.73365018604124,-0.0362762407020098,
8.79610912703474));
#387983=CARTESIAN_POINT('Origin',(2.66095450423382,-0.0683051002823623,
8.85049129520029));
#387984=CARTESIAN_POINT('Ctrl Pts',(2.66618796128141,-0.0915411309427756,
8.85049129520029));
#387985=CARTESIAN_POINT('Ctrl Pts',(2.67122500331725,-0.0944956731665771,
8.85711686593484));
#387986=CARTESIAN_POINT('Ctrl Pts',(2.66869591238441,-0.102662953078966,
8.85933012996512));
#387987=CARTESIAN_POINT('Ctrl Pts',(2.66173176290277,-0.0889272900866481,
8.8633249698723));
#387988=CARTESIAN_POINT('Ctrl Pts',(2.66186606778201,-0.0935461488825097,
8.86648636486736));
#387989=CARTESIAN_POINT('Ctrl Pts',(2.65623818394787,-0.0953358487015099,
8.87206031107457));
#387990=CARTESIAN_POINT('Ctrl Pts',(2.66192918350039,-0.0818089453981995,
8.86341338519877));
#387991=CARTESIAN_POINT('Ctrl Pts',(2.66233087922226,-0.0771924411816615,
8.86654584966058));
#387992=CARTESIAN_POINT('Ctrl Pts',(2.6567883726407,-0.0750936859361302,
8.87215952290714));
#387993=CARTESIAN_POINT('Ctrl Pts',(2.66657505256398,-0.0794701993176738,
8.85049129520029));
#387994=CARTESIAN_POINT('Ctrl Pts',(2.67179104362696,-0.0768444519090336,
8.85711686593485));
#387995=CARTESIAN_POINT('Ctrl Pts',(2.66979042840332,-0.068531913136744,
8.85933012996512));
#387996=CARTESIAN_POINT('Origin',(2.65986361061929,-0.10232318031674,8.85049129520029));
#387997=CARTESIAN_POINT('Ctrl Pts',(2.72785477369492,-0.127712598202018,
8.78727029226991));
#387998=CARTESIAN_POINT('Ctrl Pts',(2.73295451669186,-0.130703918486376,
8.79393457792714));
#387999=CARTESIAN_POINT('Ctrl Pts',(2.73035783527281,-0.138943861495048,
8.79610912703474));
#388000=CARTESIAN_POINT('Ctrl Pts',(2.70732829956804,-0.115672529034026,
8.80838214965002));
#388001=CARTESIAN_POINT('Ctrl Pts',(2.71242719562159,-0.118663352532773,
8.81501364461988));
#388002=CARTESIAN_POINT('Ctrl Pts',(2.70983317111897,-0.126868219958582,
8.81722098428721));
#388003=CARTESIAN_POINT('Ctrl Pts',(2.68677347260705,-0.103615829144088,
8.82945683644722));
#388004=CARTESIAN_POINT('Ctrl Pts',(2.69185232513724,-0.106594895854689,
8.83607469902389));
#388005=CARTESIAN_POINT('Ctrl Pts',(2.6892799847167,-0.114775061333372,
8.8382956714852));
#388006=CARTESIAN_POINT('Ctrl Pts',(2.66618796128141,-0.0915411309427756,
8.85049129520029));
#388007=CARTESIAN_POINT('Ctrl Pts',(2.67122500331725,-0.0944956731665771,
8.85711686593484));
#388008=CARTESIAN_POINT('Ctrl Pts',(2.66869591238441,-0.102662953078966,
8.85933012996512));
#388009=CARTESIAN_POINT('Origin',(2.72153042303281,-0.138494647575983,8.78727029226991));
#388010=CARTESIAN_POINT('Ctrl Pts',(2.73979042401482,-0.134713629821672,
8.75374538247847));
#388011=CARTESIAN_POINT('Ctrl Pts',(2.74635165306265,-0.13854699019731,
8.75304829418601));
#388012=CARTESIAN_POINT('Ctrl Pts',(2.74592344570742,-0.146168491471333,
8.75272238421917));
#388013=CARTESIAN_POINT('Ctrl Pts',(2.74092899456703,-0.13538147262631,
8.76769408445022));
#388014=CARTESIAN_POINT('Ctrl Pts',(2.74765498512006,-0.139311893221183,
8.76974318093972));
#388015=CARTESIAN_POINT('Ctrl Pts',(2.74741055885273,-0.146858986243019,
8.7707786988043));
#388016=CARTESIAN_POINT('Ctrl Pts',(2.73509333052471,-0.131958490841916,
8.78108014887986));
#388017=CARTESIAN_POINT('Ctrl Pts',(2.74079528214875,-0.135286100340862,
8.78639403366322));
#388018=CARTESIAN_POINT('Ctrl Pts',(2.7397975286336,-0.143318943153455,
8.78812224174741));
#388019=CARTESIAN_POINT('Ctrl Pts',(2.72552996537758,-0.126348979358583,
8.78944554828686));
#388020=CARTESIAN_POINT('Ctrl Pts',(2.73033818026369,-0.129148530612979,
8.79673892988686));
#388021=CARTESIAN_POINT('Ctrl Pts',(2.72734888397413,-0.137548986672613,
8.79894799272499));
#388022=CARTESIAN_POINT('Origin',(2.73362579600155,-0.145589345197023,8.75721825406948));
#388023=CARTESIAN_POINT('Origin',(2.73362579600155,-0.145589345197023,9.));
#388024=CARTESIAN_POINT('Origin',(2.73362579600155,-0.145589345197022,7.51860402984325));
#388025=CARTESIAN_POINT('Ctrl Pts',(2.74339508349897,-0.127106609904094,
7.50366195182966));
#388026=CARTESIAN_POINT('Ctrl Pts',(2.74705311126524,-0.127276093151815,
7.50000065167735));
#388027=CARTESIAN_POINT('Ctrl Pts',(2.74705311126523,-0.127276093151932,
7.49482233047108));
#388028=CARTESIAN_POINT('Ctrl Pts',(2.744560462474,-0.134454785966985,7.50215800491337));
#388029=CARTESIAN_POINT('Ctrl Pts',(2.74661186251358,-0.136799237939605,
7.49877273257267));
#388030=CARTESIAN_POINT('Ctrl Pts',(2.74645211423604,-0.140247663208879,
7.49481816995647));
#388031=CARTESIAN_POINT('Ctrl Pts',(2.74238152832946,-0.136233061068268,
7.51043025814042));
#388032=CARTESIAN_POINT('Ctrl Pts',(2.74641706184182,-0.140452921996967,
7.51006209594514));
#388033=CARTESIAN_POINT('Ctrl Pts',(2.7461079709193,-0.146256665010223,
7.50731281821701));
#388034=CARTESIAN_POINT('Ctrl Pts',(2.73994884293186,-0.134806531208225,
7.51860402984326));
#388035=CARTESIAN_POINT('Ctrl Pts',(2.74651279192828,-0.138655633826115,
7.51860402984327));
#388036=CARTESIAN_POINT('Ctrl Pts',(2.74610810557234,-0.146254136727608,
7.51860402984327));
#388037=CARTESIAN_POINT('Origin',(0.,0.,7.5));
#388038=CARTESIAN_POINT('Origin',(2.65484493177041,-0.262176299060726,7.5));
#388039=CARTESIAN_POINT('',(2.65484493177041,-0.262176299060726,7.59394543036555));
#388040=CARTESIAN_POINT('',(2.65484493177041,-0.262176299060726,8.85049129520029));
#388041=CARTESIAN_POINT('',(2.65484493177041,-0.262176299060726,7.5));
#388042=CARTESIAN_POINT('',(2.71406752923975,-0.302224454397949,8.78727029226991));
#388043=CARTESIAN_POINT('Ctrl Pts',(2.65484493177041,-0.262176299060726,
8.85049129520029));
#388044=CARTESIAN_POINT('Ctrl Pts',(2.67461449285379,-0.275545088797212,
8.82945686509571));
#388045=CARTESIAN_POINT('Ctrl Pts',(2.69435466409413,-0.288894004211227,
8.80838212259896));
#388046=CARTESIAN_POINT('Ctrl Pts',(2.71406752923975,-0.302224454397949,
8.78727029226991));
#388047=CARTESIAN_POINT('',(2.72568349213023,-0.310079528408679,8.75721825406948));
#388048=CARTESIAN_POINT('Origin',(2.69072714323144,-0.286440718598037,8.75937679713118));
#388049=CARTESIAN_POINT('',(2.72568349213023,-0.310079528408679,7.51860402984325));
#388050=CARTESIAN_POINT('',(2.72568349213023,-0.310079528408679,7.5));
#388051=CARTESIAN_POINT('Ctrl Pts',(2.72568349213022,-0.310079528408679,
7.51860402984325));
#388052=CARTESIAN_POINT('Ctrl Pts',(2.71656095990371,-0.303910589468343,
7.52834476460825));
#388053=CARTESIAN_POINT('Ctrl Pts',(2.70743250546091,-0.29773764574186,
7.53807742314406));
#388054=CARTESIAN_POINT('Ctrl Pts',(2.69829792995554,-0.291560562763214,
7.54780169004674));
#388055=CARTESIAN_POINT('Ctrl Pts',(2.6838292560367,-0.281776397167888,
7.5632044032688));
#388056=CARTESIAN_POINT('Ctrl Pts',(2.6693452067639,-0.271981834281848,
7.57858609112103));
#388057=CARTESIAN_POINT('Ctrl Pts',(2.65484493177041,-0.262176299060725,
7.59394543036555));
#388058=CARTESIAN_POINT('Origin',(2.90905453099297,-0.142494670373502,7.5));
#388059=CARTESIAN_POINT('',(2.73469396819878,-0.216676518124512,8.75721825406948));
#388060=CARTESIAN_POINT('',(2.72179064828013,-0.222166246411397,8.78727029226991));
#388061=CARTESIAN_POINT('Origin',(2.6890372096248,-0.236101224371513,8.75658640620901));
#388062=CARTESIAN_POINT('',(2.65600461497702,-0.250154969482878,8.85049129520029));
#388063=CARTESIAN_POINT('Ctrl Pts',(2.72179064828013,-0.222166246411397,
8.78727029226991));
#388064=CARTESIAN_POINT('Ctrl Pts',(2.69989307440824,-0.231482587589983,
8.80838212259894));
#388065=CARTESIAN_POINT('Ctrl Pts',(2.67796516820153,-0.240811833685869,
8.82945686509571));
#388066=CARTESIAN_POINT('Ctrl Pts',(2.65600461497702,-0.250154969482878,
8.85049129520029));
#388067=CARTESIAN_POINT('',(2.65600461497702,-0.250154969482878,7.59394543036555));
#388068=CARTESIAN_POINT('',(2.65600461497702,-0.250154969482878,7.5));
#388069=CARTESIAN_POINT('',(2.73469396819878,-0.216676518124512,7.51860402984325));
#388070=CARTESIAN_POINT('Ctrl Pts',(2.65600461497702,-0.250154969482878,
7.59394543036555));
#388071=CARTESIAN_POINT('Ctrl Pts',(2.67211190534232,-0.243302109280937,
7.57858609112103));
#388072=CARTESIAN_POINT('Ctrl Pts',(2.68820117174618,-0.236456917388534,
7.56320440326857));
#388073=CARTESIAN_POINT('Ctrl Pts',(2.70427335879892,-0.229618991920377,
7.54780169004651));
#388074=CARTESIAN_POINT('Ctrl Pts',(2.71442028774302,-0.225301972486568,
7.53807742314383));
#388075=CARTESIAN_POINT('Ctrl Pts',(2.72456041724852,-0.220987845879614,
7.52834476460825));
#388076=CARTESIAN_POINT('Ctrl Pts',(2.73469396819878,-0.216676518124513,
7.51860402984325));
#388077=CARTESIAN_POINT('',(2.73469396819878,-0.216676518124512,7.5));
#388078=CARTESIAN_POINT('Origin',(2.65869612245475,-0.256481217383277,7.5));
#388079=CARTESIAN_POINT('Ctrl Pts',(2.65600461497702,-0.250154969482878,
8.85049129520029));
#388080=CARTESIAN_POINT('Ctrl Pts',(2.65582641123954,-0.250230786412525,
8.85097269580139));
#388081=CARTESIAN_POINT('Ctrl Pts',(2.65565374887267,-0.250313386797546,
8.85143669361005));
#388082=CARTESIAN_POINT('Ctrl Pts',(2.65547905463229,-0.250407362801228,
8.8519052845931));
#388083=CARTESIAN_POINT('Ctrl Pts',(2.6551373637768,-0.250591173904689,
8.85282181883899));
#388084=CARTESIAN_POINT('Ctrl Pts',(2.65479678269175,-0.2508139494761,8.85372622499635));
#388085=CARTESIAN_POINT('Ctrl Pts',(2.65446040730407,-0.251092088735957,
8.8546225773507));
#388086=CARTESIAN_POINT('Ctrl Pts',(2.65418116040415,-0.251322990070918,
8.85536669723986));
#388087=CARTESIAN_POINT('Ctrl Pts',(2.65390472814385,-0.251592074862203,
8.85610498449051));
#388088=CARTESIAN_POINT('Ctrl Pts',(2.65363844027942,-0.251914482863951,
8.85681338218371));
#388089=CARTESIAN_POINT('Ctrl Pts',(2.65339678362424,-0.252207068631889,
8.85745625420284));
#388090=CARTESIAN_POINT('Ctrl Pts',(2.65315998869644,-0.252546858276533,
8.85808743050665));
#388091=CARTESIAN_POINT('Ctrl Pts',(2.65294216072111,-0.252958729273119,
8.8586680450841));
#388092=CARTESIAN_POINT('Ctrl Pts',(2.65284165961522,-0.253148757622676,
8.85893592806395));
#388093=CARTESIAN_POINT('Ctrl Pts',(2.65274533984821,-0.253354324991397,
8.85919241173848));
#388094=CARTESIAN_POINT('Ctrl Pts',(2.65265570415938,-0.253579014432801,
8.85943017985534));
#388095=CARTESIAN_POINT('Ctrl Pts',(2.65253466944446,-0.253882411693887,
8.8597512372));
#388096=CARTESIAN_POINT('Ctrl Pts',(2.65242333611262,-0.254228633815598,
8.86004599534706));
#388097=CARTESIAN_POINT('Ctrl Pts',(2.65233295686034,-0.254616709420175,
8.86026130871721));
#388098=CARTESIAN_POINT('Ctrl Pts',(2.65229986646803,-0.25475879484002,
8.86034014101236));
#388099=CARTESIAN_POINT('Ctrl Pts',(2.65226907590949,-0.254908622195513,
8.86040910639693));
#388100=CARTESIAN_POINT('Ctrl Pts',(2.65224175354912,-0.255062177237531,
8.86046313645507));
#388101=CARTESIAN_POINT('Ctrl Pts',(2.65219911723458,-0.255301798594587,
8.8605474499083));
#388102=CARTESIAN_POINT('Ctrl Pts',(2.65216390737134,-0.255557064068575,
8.86059655985668));
#388103=CARTESIAN_POINT('Ctrl Pts',(2.65213809186542,-0.255811562677652,
8.86059725258816));
#388104=CARTESIAN_POINT('Ctrl Pts',(2.65211221671537,-0.256066649280189,
8.86059794692011));
#388105=CARTESIAN_POINT('Ctrl Pts',(2.65209813563059,-0.256324062526829,
8.86056369958366));
#388106=CARTESIAN_POINT('Ctrl Pts',(2.65209285911932,-0.256569557431468,
8.86048590497774));
#388107=CARTESIAN_POINT('Ctrl Pts',(2.65209148210697,-0.256633624292315,
8.86046560290182));
#388108=CARTESIAN_POINT('Ctrl Pts',(2.65209077737803,-0.256697714868719,
8.86044257503091));
#388109=CARTESIAN_POINT('Ctrl Pts',(2.65209073388499,-0.256759848347883,
8.86041778462583));
#388110=CARTESIAN_POINT('Ctrl Pts',(2.65209044123086,-0.257177929561439,
8.860250975962));
#388111=CARTESIAN_POINT('Ctrl Pts',(2.65212037943941,-0.257563502039559,
8.8599848982295));
#388112=CARTESIAN_POINT('Ctrl Pts',(2.65217122762928,-0.257905967816415,
8.85968173251462));
#388113=CARTESIAN_POINT('Ctrl Pts',(2.65219812340846,-0.258087112591422,
8.85952137522077));
#388114=CARTESIAN_POINT('Ctrl Pts',(2.65223119893676,-0.258259716699445,
8.85934740853961));
#388115=CARTESIAN_POINT('Ctrl Pts',(2.65226846100321,-0.258421638611228,
8.8591675900182));
#388116=CARTESIAN_POINT('Ctrl Pts',(2.65241808756843,-0.259071839252373,
8.85844552518695));
#388117=CARTESIAN_POINT('Ctrl Pts',(2.65264072726469,-0.259587222332702,
8.85759444184124));
#388118=CARTESIAN_POINT('Ctrl Pts',(2.65285999980908,-0.259991132974789,
8.85683498915138));
#388119=CARTESIAN_POINT('Ctrl Pts',(2.65288294609688,-0.26003340114778,
8.85675551444998));
#388120=CARTESIAN_POINT('Ctrl Pts',(2.65290587085534,-0.260074435800304,
8.85667699793651));
#388121=CARTESIAN_POINT('Ctrl Pts',(2.65292869619824,-0.260114254771393,
8.85659965593547));
#388122=CARTESIAN_POINT('Ctrl Pts',(2.65323679384139,-0.260651733275015,
8.85555568965886));
#388123=CARTESIAN_POINT('Ctrl Pts',(2.65361051729581,-0.261123788020516,
8.85434650606346));
#388124=CARTESIAN_POINT('Ctrl Pts',(2.65404684146777,-0.261536610171378,
8.85297329937117));
#388125=CARTESIAN_POINT('Ctrl Pts',(2.65429224722887,-0.261768797477614,
8.85220095427747));
#388126=CARTESIAN_POINT('Ctrl Pts',(2.65455777277543,-0.261982113251104,
8.85137579139183));
#388127=CARTESIAN_POINT('Ctrl Pts',(2.65484493177041,-0.262176299060726,
8.85049129520029));
#388128=CARTESIAN_POINT('Origin',(2.65869612245475,-0.256481217383277,7.59394543036555));
#388129=CARTESIAN_POINT('Ctrl Pts',(2.65548722941064,-0.250375091606243,
7.59443877723642));
#388130=CARTESIAN_POINT('Ctrl Pts',(2.65015865589203,-0.252642137681074,
7.58783886950016));
#388131=CARTESIAN_POINT('Ctrl Pts',(2.65158455852055,-0.261011485518907,
7.58559994247159));
#388132=CARTESIAN_POINT('Ctrl Pts',(2.68457575591506,-0.237999353596044,
7.56670252222135));
#388133=CARTESIAN_POINT('Ctrl Pts',(2.67925488369801,-0.240263123145666,
7.56004874999029));
#388134=CARTESIAN_POINT('Ctrl Pts',(2.68066817321353,-0.248685650676148,
7.55786368756704));
#388135=CARTESIAN_POINT('Ctrl Pts',(2.71360996250254,-0.225646726040084,
7.5388891333356));
#388136=CARTESIAN_POINT('Ctrl Pts',(2.70825746808137,-0.227923949282997,
7.5322200213728));
#388137=CARTESIAN_POINT('Ctrl Pts',(2.70969805244026,-0.236381322481853,
7.53005029815327));
#388138=CARTESIAN_POINT('Ctrl Pts',(2.74258853535555,-0.213317767903139,
7.51101258149734));
#388139=CARTESIAN_POINT('Ctrl Pts',(2.73717115897627,-0.215622595229558,
7.5043616886572));
#388140=CARTESIAN_POINT('Ctrl Pts',(2.7386727941559,-0.224099184952553,
7.50217374673251));
#388141=CARTESIAN_POINT('',(2.73712666431696,-0.224754574642168,7.50366116523517));
#388142=CARTESIAN_POINT('Ctrl Pts',(2.73469396819878,-0.216676518124511,
7.51860402984325));
#388143=CARTESIAN_POINT('Ctrl Pts',(2.73510033067526,-0.216503630867908,
7.51734760759493));
#388144=CARTESIAN_POINT('Ctrl Pts',(2.73549082980322,-0.216402150372084,
7.51608817408572));
#388145=CARTESIAN_POINT('Ctrl Pts',(2.73586792612086,-0.216385234400819,
7.51481005913119));
#388146=CARTESIAN_POINT('Ctrl Pts',(2.73620950897638,-0.216369911509826,
7.51365231206383));
#388147=CARTESIAN_POINT('Ctrl Pts',(2.73654056487762,-0.216423703726785,
7.51247773061042));
#388148=CARTESIAN_POINT('Ctrl Pts',(2.73684944320768,-0.216582127288776,
7.51129758471022));
#388149=CARTESIAN_POINT('Ctrl Pts',(2.7372333436967,-0.216779029683677,
7.50983079813402));
#388150=CARTESIAN_POINT('Ctrl Pts',(2.73756478892187,-0.217142868017661,
7.50839324291155));
#388151=CARTESIAN_POINT('Ctrl Pts',(2.7377852545119,-0.217731815209133,
7.50715379678855));
#388152=CARTESIAN_POINT('Ctrl Pts',(2.73788710326193,-0.218003891841488,
7.50658120839351));
#388153=CARTESIAN_POINT('Ctrl Pts',(2.73797084707659,-0.218366019889119,
7.50598221009429));
#388154=CARTESIAN_POINT('Ctrl Pts',(2.73801233135004,-0.218814706195348,
7.50545747549611));
#388155=CARTESIAN_POINT('Ctrl Pts',(2.73803446864242,-0.219054139096492,
7.50517746087247));
#388156=CARTESIAN_POINT('Ctrl Pts',(2.73804501371075,-0.219320798164657,
7.50491486231392));
#388157=CARTESIAN_POINT('Ctrl Pts',(2.73804202059031,-0.219607687728826,
7.50468370960992));
#388158=CARTESIAN_POINT('Ctrl Pts',(2.73803754493112,-0.220036678121437,
7.50433806340447));
#388159=CARTESIAN_POINT('Ctrl Pts',(2.73800210745578,-0.220523761247855,
7.50405484070984));
#388160=CARTESIAN_POINT('Ctrl Pts',(2.73793738030584,-0.221036080981636,
7.50385766036131));
#388161=CARTESIAN_POINT('Ctrl Pts',(2.73793045874324,-0.221090865613916,
7.50383657498791));
#388162=CARTESIAN_POINT('Ctrl Pts',(2.73792321962444,-0.221145916405801,
7.50381643264937));
#388163=CARTESIAN_POINT('Ctrl Pts',(2.7379156778676,-0.221201177089471,
7.50379723213559));
#388164=CARTESIAN_POINT('Ctrl Pts',(2.73786533417364,-0.221570060229976,
7.50366906242519));
#388165=CARTESIAN_POINT('Ctrl Pts',(2.73779969739273,-0.22195622297899,
7.50358235568538));
#388166=CARTESIAN_POINT('Ctrl Pts',(2.73772748437109,-0.222326915563675,
7.5035341175365));
#388167=CARTESIAN_POINT('Ctrl Pts',(2.73761920911807,-0.22288272714011,
7.50346178989176));
#388168=CARTESIAN_POINT('Ctrl Pts',(2.73747909711921,-0.2234760501773,7.50346967198527));
#388169=CARTESIAN_POINT('Ctrl Pts',(2.73732362825383,-0.224054277262578,
7.50354272648692));
#388170=CARTESIAN_POINT('Ctrl Pts',(2.73725968069148,-0.224292114031345,
7.50357277531559));
#388171=CARTESIAN_POINT('Ctrl Pts',(2.73719335688109,-0.224527117606271,
7.50361331098761));
#388172=CARTESIAN_POINT('Ctrl Pts',(2.73712666431837,-0.224754574642284,
7.50366116523659));
#388173=CARTESIAN_POINT('',(2.66161051802577,-0.256762365619137,7.57603338622103));
#388174=CARTESIAN_POINT('Origin',(2.67040634802705,-0.25761375518207,7.58486873427628));
#388175=CARTESIAN_POINT('Ctrl Pts',(2.73712666436744,-0.224754574614952,
7.50366116529968));
#388176=CARTESIAN_POINT('Ctrl Pts',(2.71199601738035,-0.235407197804142,
7.52783573079709));
#388177=CARTESIAN_POINT('Ctrl Pts',(2.68682516411221,-0.246075974212514,
7.55196141284068));
#388178=CARTESIAN_POINT('Ctrl Pts',(2.66161051899361,-0.256762364824825,
7.57603338728831));
#388179=CARTESIAN_POINT('Ctrl Pts',(2.65701976820131,-0.24991413872985,
7.5963967733137));
#388180=CARTESIAN_POINT('Ctrl Pts',(2.63928131883209,-0.254320875588142,
7.59959882295472));
#388181=CARTESIAN_POINT('Ctrl Pts',(2.65563227986823,-0.262527877830806,
7.59642833564546));
#388182=CARTESIAN_POINT('Ctrl Pts',(2.65313223933926,-0.250233862721098,
7.5870762605742));
#388183=CARTESIAN_POINT('Ctrl Pts',(2.64878024702139,-0.255427363842895,
7.588099439206));
#388184=CARTESIAN_POINT('Ctrl Pts',(2.65195705933609,-0.261395802860866,
7.58710240504253));
#388185=CARTESIAN_POINT('Ctrl Pts',(2.65771595193358,-0.254223250031781,
7.58015376756929));
#388186=CARTESIAN_POINT('Ctrl Pts',(2.65561601806597,-0.256151863302553,
7.58205880659761));
#388187=CARTESIAN_POINT('Ctrl Pts',(2.65725320000503,-0.258442433174035,
7.58020924244126));
#388188=CARTESIAN_POINT('Ctrl Pts',(2.66161051720204,-0.256762365539468,
7.57603338509286));
#388189=CARTESIAN_POINT('Ctrl Pts',(2.66161051720205,-0.256762365539468,
7.57603338509286));
#388190=CARTESIAN_POINT('Ctrl Pts',(2.66161051720205,-0.256762365539468,
7.57603338509286));
#388191=CARTESIAN_POINT('Origin',(2.67040689596867,-0.257608075198336,7.58486873427622));
#388192=CARTESIAN_POINT('Ctrl Pts',(2.73281288470864,-0.314900644564356,
7.51098857897448));
#388193=CARTESIAN_POINT('Ctrl Pts',(2.72793597470703,-0.311602726917105,
7.50433767179956));
#388194=CARTESIAN_POINT('Ctrl Pts',(2.73103031844477,-0.303569478015496,
7.50214974420965));
#388195=CARTESIAN_POINT('Ctrl Pts',(2.70671798449283,-0.297254464524829,
7.53887321589167));
#388196=CARTESIAN_POINT('Ctrl Pts',(2.70189950852799,-0.293996061783733,
7.53220407452061));
#388197=CARTESIAN_POINT('Ctrl Pts',(2.70493022693792,-0.28597000011928,
7.53003438070911));
#388198=CARTESIAN_POINT('Ctrl Pts',(2.68057297244262,-0.279574397310241,
7.56669465659236));
#388199=CARTESIAN_POINT('Ctrl Pts',(2.67578297277488,-0.276335251123579,
7.56004085833303));
#388200=CARTESIAN_POINT('Ctrl Pts',(2.67878022809322,-0.268338182242846,
7.55785582193789));
#388201=CARTESIAN_POINT('Ctrl Pts',(2.65437903099218,-0.26186124251921,
7.59443891967696));
#388202=CARTESIAN_POINT('Ctrl Pts',(2.64958208642131,-0.258617399973843,
7.58783901202978));
#388203=CARTESIAN_POINT('Ctrl Pts',(2.65258156709373,-0.250674963717624,
7.58560008491213));
#388204=CARTESIAN_POINT('',(2.72961551748769,-0.30261546891708,7.50366116523517));
#388205=CARTESIAN_POINT('Ctrl Pts',(2.72961551748806,-0.302615468917121,
7.50366116523554));
#388206=CARTESIAN_POINT('Ctrl Pts',(2.72968561742245,-0.303369937946282,
7.50350835821027));
#388207=CARTESIAN_POINT('Ctrl Pts',(2.7297255104133,-0.30406575872811,7.50345484956));
#388208=CARTESIAN_POINT('Ctrl Pts',(2.72973698202872,-0.304723584208325,
7.50349758195598));
#388209=CARTESIAN_POINT('Ctrl Pts',(2.7297428678182,-0.305061097465285,
7.50351950684424));
#388210=CARTESIAN_POINT('Ctrl Pts',(2.72974198137209,-0.305421873052815,
7.50357029184312));
#388211=CARTESIAN_POINT('Ctrl Pts',(2.72973156373016,-0.305769741308945,
7.50365515313923));
#388212=CARTESIAN_POINT('Ctrl Pts',(2.72971553717836,-0.306304903552644,
7.50378570417639));
#388213=CARTESIAN_POINT('Ctrl Pts',(2.72967682976936,-0.306825237690729,
7.50400001621911));
#388214=CARTESIAN_POINT('Ctrl Pts',(2.72961612354001,-0.307290970309341,
7.50428903009635));
#388215=CARTESIAN_POINT('Ctrl Pts',(2.7296093856156,-0.307342663046873,
7.50432110841318));
#388216=CARTESIAN_POINT('Ctrl Pts',(2.72960239051942,-0.307393710105049,
7.50435406373354));
#388217=CARTESIAN_POINT('Ctrl Pts',(2.72959514912735,-0.307444077147374,
7.50438785222352));
#388218=CARTESIAN_POINT('Ctrl Pts',(2.72955093694813,-0.307751592150259,
7.50459414719561));
#388219=CARTESIAN_POINT('Ctrl Pts',(2.72949632922009,-0.308038580830313,
7.50483629897752));
#388220=CARTESIAN_POINT('Ctrl Pts',(2.72943471078469,-0.308294294734311,
7.5050991045531));
#388221=CARTESIAN_POINT('Ctrl Pts',(2.72929877432722,-0.308858425290561,
7.50567888004914));
#388222=CARTESIAN_POINT('Ctrl Pts',(2.72912386673409,-0.309292697140601,
7.50637912803144));
#388223=CARTESIAN_POINT('Ctrl Pts',(2.72893465063687,-0.309615742862395,
7.50710440483569));
#388224=CARTESIAN_POINT('Ctrl Pts',(2.72888825109336,-0.309694960086735,
7.50728225710685));
#388225=CARTESIAN_POINT('Ctrl Pts',(2.72884019340232,-0.309769139713227,
7.50746498566954));
#388226=CARTESIAN_POINT('Ctrl Pts',(2.72879194901789,-0.309836776660444,
7.50764697238949));
#388227=CARTESIAN_POINT('Ctrl Pts',(2.72853260048436,-0.310200374274494,
7.50862528291182));
#388228=CARTESIAN_POINT('Ctrl Pts',(2.72824768340916,-0.310410308860673,
7.50965856837422));
#388229=CARTESIAN_POINT('Ctrl Pts',(2.72796073636963,-0.310528558892816,
7.51067959873202));
#388230=CARTESIAN_POINT('Ctrl Pts',(2.72780282905185,-0.310593632034658,
7.51124147302579));
#388231=CARTESIAN_POINT('Ctrl Pts',(2.72764410294566,-0.310630554447905,
7.51180065547253));
#388232=CARTESIAN_POINT('Ctrl Pts',(2.72748753823894,-0.310647107520337,
7.51235175716501));
#388233=CARTESIAN_POINT('Ctrl Pts',(2.72694654480926,-0.310704304979551,
7.51425603304536));
#388234=CARTESIAN_POINT('Ctrl Pts',(2.72636621705692,-0.310519085845715,
7.51626900505181));
#388235=CARTESIAN_POINT('Ctrl Pts',(2.72577891497115,-0.310142396153948,
7.51827788969245));
#388236=CARTESIAN_POINT('Ctrl Pts',(2.72574712907242,-0.310122008995986,
7.51838661432546));
#388237=CARTESIAN_POINT('Ctrl Pts',(2.72571532001016,-0.310101051407239,
7.51849533314857));
#388238=CARTESIAN_POINT('Ctrl Pts',(2.72568349213022,-0.310079528408683,
7.51860402984325));
#388239=CARTESIAN_POINT('Ctrl Pts',(2.66161051882509,-0.256762366584167,
7.57603338728985));
#388240=CARTESIAN_POINT('Ctrl Pts',(2.68431738886144,-0.272071688132325,
7.55196141284922));
#388241=CARTESIAN_POINT('Ctrl Pts',(2.70698464172671,-0.287355349116283,
7.52783573083105));
#388242=CARTESIAN_POINT('Ctrl Pts',(2.72961551753351,-0.302615468954532,
7.50366116530176));
#388243=CARTESIAN_POINT('Origin',(9.19709468541367E-16,-8.87232663177103E-17,
7.49482233047033));
#388244=CARTESIAN_POINT('Origin',(2.7283174780614,-0.224031223057595,7.49482233047033));
#388245=CARTESIAN_POINT('Origin',(0.,0.,7.50366116523517));
#388246=CARTESIAN_POINT('Origin',(2.72083050515593,-0.301641529324055,7.49482233047033));
#388247=CARTESIAN_POINT('Ctrl Pts',(2.73469299488662,-0.216676932172354,
7.51860402984325));
#388248=CARTESIAN_POINT('Ctrl Pts',(2.74169487207939,-0.21369867734652,
7.51860402984325));
#388249=CARTESIAN_POINT('Ctrl Pts',(2.74226515987506,-0.206111117932571,
7.51860402984325));
#388250=CARTESIAN_POINT('Ctrl Pts',(2.73729283917419,-0.215571084661517,
7.51041458714366));
#388251=CARTESIAN_POINT('Ctrl Pts',(2.74182996991852,-0.211901096872824,
7.51004642900443));
#388252=CARTESIAN_POINT('Ctrl Pts',(2.74226531715367,-0.206109025373781,
7.5072913648301));
#388253=CARTESIAN_POINT('Ctrl Pts',(2.73922057885099,-0.217622317690166,
7.50215815450137));
#388254=CARTESIAN_POINT('Ctrl Pts',(2.74155503724043,-0.215561160609934,
7.49877163671529));
#388255=CARTESIAN_POINT('Ctrl Pts',(2.74183741099952,-0.212122528810137,
7.4948158853317));
#388256=CARTESIAN_POINT('Ctrl Pts',(2.73712611564553,-0.224754529589408,
7.50366171572174));
#388257=CARTESIAN_POINT('Ctrl Pts',(2.74077554873745,-0.225054196679248,
7.50000045605858));
#388258=CARTESIAN_POINT('Ctrl Pts',(2.74077554873746,-0.225054196679124,
7.49482233047317));
#388259=CARTESIAN_POINT('Origin',(2.72980031823927,-0.205174249214696,7.51860402984325));
#388260=CARTESIAN_POINT('Origin',(2.72980031823927,-0.205174249214696,9.));
#388261=CARTESIAN_POINT('Origin',(2.72980031823927,-0.205174249214696,8.75721825406948));
#388262=CARTESIAN_POINT('Ctrl Pts',(2.71932677685935,-0.223214469743979,
8.78942910404913));
#388263=CARTESIAN_POINT('Ctrl Pts',(2.7244623390508,-0.221051501949621,
8.7967269950169));
#388264=CARTESIAN_POINT('Ctrl Pts',(2.72256725120911,-0.212328994967426,
8.79893251111267));
#388265=CARTESIAN_POINT('Ctrl Pts',(2.72944356314156,-0.218910279452994,
8.78111911759579));
#388266=CARTESIAN_POINT('Ctrl Pts',(2.73552894228411,-0.216339195864893,
8.78644465894814));
#388267=CARTESIAN_POINT('Ctrl Pts',(2.73554682940729,-0.208232705142873,
8.78817647674132));
#388268=CARTESIAN_POINT('Ctrl Pts',(2.73574858564825,-0.216227805369768,
8.76780923932032));
#388269=CARTESIAN_POINT('Ctrl Pts',(2.74293013554404,-0.21318805573127,
8.76988516158373));
#388270=CARTESIAN_POINT('Ctrl Pts',(2.74365028845524,-0.205663578328759,
8.77093053738833));
#388271=CARTESIAN_POINT('Ctrl Pts',(2.73451919254909,-0.216750851102149,
8.75371302330491));
#388272=CARTESIAN_POINT('Ctrl Pts',(2.74152478183233,-0.21378640846275,
8.75300828287559));
#388273=CARTESIAN_POINT('Ctrl Pts',(2.74206964654565,-0.206164226243825,
8.75267964240737));
#388274=CARTESIAN_POINT('Origin',(2.71689699832061,-0.210663977501581,8.78727029226991));
#388275=CARTESIAN_POINT('Ctrl Pts',(2.65600461497702,-0.250154969482878,
8.85049129520029));
#388276=CARTESIAN_POINT('Ctrl Pts',(2.66137812144103,-0.247868806648722,
8.85711686593484));
#388277=CARTESIAN_POINT('Ctrl Pts',(2.65991420288367,-0.239445167021381,
8.85933012996512));
#388278=CARTESIAN_POINT('Ctrl Pts',(2.67796519767341,-0.240811821147034,
8.82945683644722));
#388279=CARTESIAN_POINT('Ctrl Pts',(2.68338330748995,-0.238506681779115,
8.83607469902389));
#388280=CARTESIAN_POINT('Ctrl Pts',(2.68187814229224,-0.230064731754072,
8.8382956714852));
#388281=CARTESIAN_POINT('Ctrl Pts',(2.69989304635038,-0.231482599527222,
8.80838214965001));
#388282=CARTESIAN_POINT('Ctrl Pts',(2.70533253855797,-0.229168363003102,
8.8150136446199));
#388283=CARTESIAN_POINT('Ctrl Pts',(2.70380902611905,-0.220699140934707,
8.81722098428721));
#388284=CARTESIAN_POINT('Ctrl Pts',(2.72179064828013,-0.222166246411397,
8.78727029226991));
#388285=CARTESIAN_POINT('Ctrl Pts',(2.72723104400521,-0.219851625484992,
8.79393457792714));
#388286=CARTESIAN_POINT('Ctrl Pts',(2.7257093818291,-0.211347276044851,
8.79610912703474));
#388287=CARTESIAN_POINT('Origin',(2.6511109650175,-0.238652700573062,8.85049129520029));
#388288=CARTESIAN_POINT('Ctrl Pts',(2.65484493177041,-0.262176299060726,
8.85049129520029));
#388289=CARTESIAN_POINT('Ctrl Pts',(2.65968232649295,-0.265447495251943,
8.85711686593484));
#388290=CARTESIAN_POINT('Ctrl Pts',(2.65663515242804,-0.273435955199396,
8.85933012996512));
#388291=CARTESIAN_POINT('Ctrl Pts',(2.6505653584879,-0.259282319010569,
8.86332496987231));
#388292=CARTESIAN_POINT('Ctrl Pts',(2.65040345612427,-0.263900292808822,
8.86648636486736));
#388293=CARTESIAN_POINT('Ctrl Pts',(2.64467246891995,-0.265325735742317,
8.87206031107457));
#388294=CARTESIAN_POINT('Ctrl Pts',(2.65121844737383,-0.252191248505847,
8.86341338519876));
#388295=CARTESIAN_POINT('Ctrl Pts',(2.65191509820944,-0.247609966125603,
8.86654584966059));
#388296=CARTESIAN_POINT('Ctrl Pts',(2.64651844701235,-0.245160413381895,
8.87215952290715));
#388297=CARTESIAN_POINT('Ctrl Pts',(2.65600461497702,-0.250154969482878,
8.85049129520029));
#388298=CARTESIAN_POINT('Ctrl Pts',(2.66137812144103,-0.247868806648722,
8.85711686593484));
#388299=CARTESIAN_POINT('Ctrl Pts',(2.65991420288367,-0.239445167021382,
8.85933012996512));
#388300=CARTESIAN_POINT('Origin',(2.64784276688978,-0.272530993019724,8.85049129520029));
#388301=CARTESIAN_POINT('Ctrl Pts',(2.71406752923975,-0.30222445439795,
8.78727029226991));
#388302=CARTESIAN_POINT('Ctrl Pts',(2.7189651397191,-0.305536370349624,
8.79393457792714));
#388303=CARTESIAN_POINT('Ctrl Pts',(2.71584585849932,-0.313593013561916,
8.79610912703474));
#388304=CARTESIAN_POINT('Ctrl Pts',(2.6943546388356,-0.288893987130622,
8.80838214965002));
#388305=CARTESIAN_POINT('Ctrl Pts',(2.69925143594085,-0.292205353053535,
8.81501364461988));
#388306=CARTESIAN_POINT('Ctrl Pts',(2.6961370534789,-0.300227162978743,
8.81722098428721));
#388307=CARTESIAN_POINT('Ctrl Pts',(2.67461451938527,-0.27554510673862,
8.82945683644722));
#388308=CARTESIAN_POINT('Ctrl Pts',(2.67949206740876,-0.278843455836032,
8.83607469902389));
#388309=CARTESIAN_POINT('Ctrl Pts',(2.6764009071358,-0.286842003870797,
8.8382956714852));
#388310=CARTESIAN_POINT('Ctrl Pts',(2.65484493177041,-0.262176299060726,
8.85049129520029));
#388311=CARTESIAN_POINT('Ctrl Pts',(2.65968232649295,-0.265447495251944,
8.85711686593484));
#388312=CARTESIAN_POINT('Ctrl Pts',(2.65663515242804,-0.273435955199396,
8.85933012996512));
#388313=CARTESIAN_POINT('Origin',(2.70706536435912,-0.312579148356947,8.78727029226991));
#388314=CARTESIAN_POINT('Ctrl Pts',(2.72553009885,-0.309975821388891,8.75374538247847));
#388315=CARTESIAN_POINT('Ctrl Pts',(2.73183224290654,-0.314221685102948,
8.75304829418602));
#388316=CARTESIAN_POINT('Ctrl Pts',(2.73091660408603,-0.321800091845756,
8.75272238421917));
#388317=CARTESIAN_POINT('Ctrl Pts',(2.72662354125151,-0.310715240504611,
8.76769408445022));
#388318=CARTESIAN_POINT('Ctrl Pts',(2.73308388962346,-0.315068521323158,
8.76974318093968));
#388319=CARTESIAN_POINT('Ctrl Pts',(2.73235642164598,-0.322584447588229,
8.77077869880429));
#388320=CARTESIAN_POINT('Ctrl Pts',(2.72101917840274,-0.306925399324471,
8.78108014887987));
#388321=CARTESIAN_POINT('Ctrl Pts',(2.72649621408303,-0.310611497187703,
8.78639403366327));
#388322=CARTESIAN_POINT('Ctrl Pts',(2.72498584455341,-0.318563909376018,
8.78812224174742));
#388323=CARTESIAN_POINT('Ctrl Pts',(2.7118348648497,-0.300714686275373,
8.78944554828686));
#388324=CARTESIAN_POINT('Ctrl Pts',(2.71645383287793,-0.303816548936929,
8.79673892988685));
#388325=CARTESIAN_POINT('Ctrl Pts',(2.71293245935052,-0.312008220487782,
8.79894799272499));
#388326=CARTESIAN_POINT('Origin',(2.7186813272496,-0.320434222367677,8.75721825406948));
#388327=CARTESIAN_POINT('Origin',(2.7186813272496,-0.320434222367677,9.));
#388328=CARTESIAN_POINT('Origin',(2.7186813272496,-0.320434222367677,7.51860402984325));
#388329=CARTESIAN_POINT('Ctrl Pts',(2.72961473561416,-0.30261538223569,
7.50366195182966));
#388330=CARTESIAN_POINT('Ctrl Pts',(2.7332543887411,-0.303018887905582,
7.50000065167735));
#388331=CARTESIAN_POINT('Ctrl Pts',(2.73325438874109,-0.303018887905698,
7.49482233047108));
#388332=CARTESIAN_POINT('Ctrl Pts',(2.73030692093631,-0.310023126770065,
7.50215800491337));
#388333=CARTESIAN_POINT('Ctrl Pts',(2.73220389660085,-0.312494195466464,
7.49877273257265));
#388334=CARTESIAN_POINT('Ctrl Pts',(2.73182353517771,-0.315925300468896,
7.49481816995647));
#388335=CARTESIAN_POINT('Ctrl Pts',(2.72801852916871,-0.311658143424456,
7.51043025814043));
#388336=CARTESIAN_POINT('Ctrl Pts',(2.73177540382666,-0.316127891716176,
7.51006209594516));
#388337=CARTESIAN_POINT('Ctrl Pts',(2.73109510087304,-0.321899906793571,
7.50731281821701));
#388338=CARTESIAN_POINT('Ctrl Pts',(2.72568224006611,-0.310078681834444,
7.51860402984326));
#388339=CARTESIAN_POINT('Ctrl Pts',(2.73198608987389,-0.314340429714334,
7.51860402984326));
#388340=CARTESIAN_POINT('Ctrl Pts',(2.73109539723704,-0.321897392332832,
7.51860402984327));
#388341=CARTESIAN_POINT('Origin',(0.,0.,7.5));
#388342=CARTESIAN_POINT('Origin',(2.63259257497231,-0.431734128529198,7.5));
#388343=CARTESIAN_POINT('',(2.63259257497231,-0.431734128529198,7.59394543036555));
#388344=CARTESIAN_POINT('',(2.63259257497231,-0.431734128529198,8.85049129520029));
#388345=CARTESIAN_POINT('',(2.63259257497231,-0.431734128529198,7.5));
#388346=CARTESIAN_POINT('',(2.68912759914127,-0.47549440548382,8.78727029226991));
#388347=CARTESIAN_POINT('Ctrl Pts',(2.63259257497231,-0.431734128529198,
8.85049129520029));
#388348=CARTESIAN_POINT('Ctrl Pts',(2.65146497607288,-0.446342090780907,
8.82945686509571));
#388349=CARTESIAN_POINT('Ctrl Pts',(2.6703093210672,-0.460928336530369,
8.80838212259897));
#388350=CARTESIAN_POINT('Ctrl Pts',(2.68912759914127,-0.47549440548382,
8.78727029226991));
#388351=CARTESIAN_POINT('',(2.70021641947035,-0.484077577700222,8.75721825406948));
#388352=CARTESIAN_POINT('Origin',(2.66684643588504,-0.45824767539666,8.75937679713162));
#388353=CARTESIAN_POINT('',(2.70021641947035,-0.484077577700222,7.51860402984325));
#388354=CARTESIAN_POINT('',(2.70021641947035,-0.484077577700222,7.5));
#388355=CARTESIAN_POINT('Ctrl Pts',(2.70021641947035,-0.484077577700221,
7.51860402984325));
#388356=CARTESIAN_POINT('Ctrl Pts',(2.69150787573963,-0.477336830860021,
7.52834476460825));
#388357=CARTESIAN_POINT('Ctrl Pts',(2.682793678548,-0.470591708024237,7.53807742314407));
#388358=CARTESIAN_POINT('Ctrl Pts',(2.67407363807296,-0.463842062263,7.54780169004674));
#388359=CARTESIAN_POINT('Ctrl Pts',(2.66026156523847,-0.453150988164429,
7.5632044032688));
#388360=CARTESIAN_POINT('Ctrl Pts',(2.64643481479703,-0.442448553035182,
7.57858609112103));
#388361=CARTESIAN_POINT('Ctrl Pts',(2.63259257497231,-0.431734128529198,
7.59394543036555));
#388362=CARTESIAN_POINT('Origin',(2.89394790158701,-0.328585663527325,7.5));
#388363=CARTESIAN_POINT('',(2.71519273396522,-0.391443777101968,8.75721825406948));
#388364=CARTESIAN_POINT('',(2.70196419720224,-0.396095507607646,8.78727029226991));
#388365=CARTESIAN_POINT('Origin',(2.66838523689802,-0.407903334640574,8.75658640620977));
#388366=CARTESIAN_POINT('',(2.63452008471591,-0.419811799220407,8.85049129520029));
#388367=CARTESIAN_POINT('Ctrl Pts',(2.70196419720224,-0.396095507607646,
8.78727029226991));
#388368=CARTESIAN_POINT('Ctrl Pts',(2.67951471421566,-0.403989724989084,
8.80838212259896));
#388369=CARTESIAN_POINT('Ctrl Pts',(2.65703413439439,-0.411894877373934,
8.82945686509571));
#388370=CARTESIAN_POINT('Ctrl Pts',(2.63452008471591,-0.419811799220407,
8.85049129520029));
#388371=CARTESIAN_POINT('',(2.63452008471591,-0.419811799220407,7.59394543036555));
#388372=CARTESIAN_POINT('',(2.63452008471591,-0.419811799220407,7.5));
#388373=CARTESIAN_POINT('',(2.71519273396522,-0.391443777101968,7.51860402984325));
#388374=CARTESIAN_POINT('Ctrl Pts',(2.63452008471591,-0.419811799220408,
7.59394543036555));
#388375=CARTESIAN_POINT('Ctrl Pts',(2.65103334518629,-0.414005016591717,
7.57858609112103));
#388376=CARTESIAN_POINT('Ctrl Pts',(2.66752812741711,-0.408204731718024,
7.56320440326857));
#388377=CARTESIAN_POINT('Ctrl Pts',(2.68400539982677,-0.402410604061146,
7.54780169004651));
#388378=CARTESIAN_POINT('Ctrl Pts',(2.69440807320189,-0.398752570376341,
7.53807742314383));
#388379=CARTESIAN_POINT('Ctrl Pts',(2.70480377576452,-0.395096987933239,
7.52834476460825));
#388380=CARTESIAN_POINT('Ctrl Pts',(2.71519273396522,-0.391443777101968,
7.51860402984325));
#388381=CARTESIAN_POINT('',(2.71519273396522,-0.391443777101968,7.5));
#388382=CARTESIAN_POINT('Origin',(2.63680073810824,-0.426297494642185,7.5));
#388383=CARTESIAN_POINT('Ctrl Pts',(2.63452008471591,-0.419811799220407,
8.85049129520029));
#388384=CARTESIAN_POINT('Ctrl Pts',(2.63433738950976,-0.419876042823379,
8.85097269580138));
#388385=CARTESIAN_POINT('Ctrl Pts',(2.6341597896714,-0.419947410981222,
8.85143669361005));
#388386=CARTESIAN_POINT('Ctrl Pts',(2.63397943329584,-0.420030001202715,
8.8519052845931));
#388387=CARTESIAN_POINT('Ctrl Pts',(2.63362666766303,-0.420191542438274,
8.85282181883899));
#388388=CARTESIAN_POINT('Ctrl Pts',(2.63327251305848,-0.420392039188342,
8.85372622499636));
#388389=CARTESIAN_POINT('Ctrl Pts',(2.63291900834655,-0.420648055336175,
8.85462257735071));
#388390=CARTESIAN_POINT('Ctrl Pts',(2.63262554129001,-0.420860590849272,
8.85536669723986));
#388391=CARTESIAN_POINT('Ctrl Pts',(2.63233243666767,-0.421111411701267,
8.85610498449051));
#388392=CARTESIAN_POINT('Ctrl Pts',(2.63204603916862,-0.421416096159145,
8.85681338218371));
#388393=CARTESIAN_POINT('Ctrl Pts',(2.63178613298843,-0.421692597783186,
8.85745625420285));
#388394=CARTESIAN_POINT('Ctrl Pts',(2.63152805418393,-0.42201651779045,
8.85808743050666));
#388395=CARTESIAN_POINT('Ctrl Pts',(2.63128428509418,-0.422413586267606,
8.8586680450841));
#388396=CARTESIAN_POINT('Ctrl Pts',(2.63117181532044,-0.422596785055575,
8.85893592806395));
#388397=CARTESIAN_POINT('Ctrl Pts',(2.63106252270619,-0.422795758835428,
8.85919241173848));
#388398=CARTESIAN_POINT('Ctrl Pts',(2.63095867528155,-0.423014243649973,
8.85943017985534));
#388399=CARTESIAN_POINT('Ctrl Pts',(2.63081845051617,-0.423309262828037,
8.8597512372));
#388400=CARTESIAN_POINT('Ctrl Pts',(2.6306851634031,-0.423647640448203,
8.86004599534705));
#388401=CARTESIAN_POINT('Ctrl Pts',(2.63057010575534,-0.424029128091254,
8.86026130871721));
#388402=CARTESIAN_POINT('Ctrl Pts',(2.63052797990668,-0.42416880147265,
8.86034014101235));
#388403=CARTESIAN_POINT('Ctrl Pts',(2.63048765313902,-0.424316348233914,
8.86040910639693));
#388404=CARTESIAN_POINT('Ctrl Pts',(2.63045054861005,-0.42446783723099,
8.86046313645507));
#388405=CARTESIAN_POINT('Ctrl Pts',(2.63039264730334,-0.424704234542217,
8.8605474499083));
#388406=CARTESIAN_POINT('Ctrl Pts',(2.63034115486746,-0.424956719642228,
8.86059655985668));
#388407=CARTESIAN_POINT('Ctrl Pts',(2.6302990866204,-0.425209041351474,
8.86059725258815));
#388408=CARTESIAN_POINT('Ctrl Pts',(2.63025692117888,-0.425461946024673,
8.86059794692011));
#388409=CARTESIAN_POINT('Ctrl Pts',(2.63022637650186,-0.42571792820999,
8.86056369958366));
#388410=CARTESIAN_POINT('Ctrl Pts',(2.6302053819192,-0.42596258065178,8.86048590497774));
#388411=CARTESIAN_POINT('Ctrl Pts',(2.63019990295821,-0.426026427654907,
8.86046560290182));
#388412=CARTESIAN_POINT('Ctrl Pts',(2.63019509337987,-0.426090341398209,
8.86044257503091));
#388413=CARTESIAN_POINT('Ctrl Pts',(2.63019106907053,-0.426152344430869,
8.86041778462583));
#388414=CARTESIAN_POINT('Ctrl Pts',(2.63016399046236,-0.426569547901318,
8.860250975962));
#388415=CARTESIAN_POINT('Ctrl Pts',(2.63016916344615,-0.426956246327036,
8.8599848982295));
#388416=CARTESIAN_POINT('Ctrl Pts',(2.6301979653053,-0.427301266325934,
8.85968173251461));
#388417=CARTESIAN_POINT('Ctrl Pts',(2.63021319983864,-0.427483762138062,
8.85952137522076));
#388418=CARTESIAN_POINT('Ctrl Pts',(2.63023514862655,-0.427658130768808,
8.85934740853961));
#388419=CARTESIAN_POINT('Ctrl Pts',(2.63026195976158,-0.427822107383451,
8.8591675900182));
#388420=CARTESIAN_POINT('Ctrl Pts',(2.63036962040486,-0.428480558724585,
8.85844552518696));
#388421=CARTESIAN_POINT('Ctrl Pts',(2.63055878195666,-0.429009147469412,
8.85759444184126));
#388422=CARTESIAN_POINT('Ctrl Pts',(2.63075172533839,-0.429426277073917,
8.85683498915141));
#388423=CARTESIAN_POINT('Ctrl Pts',(2.63077191634944,-0.429469928576126,
8.85675551445));
#388424=CARTESIAN_POINT('Ctrl Pts',(2.63079216490732,-0.429512347712879,
8.85667699793652));
#388425=CARTESIAN_POINT('Ctrl Pts',(2.63081239214287,-0.429553547296367,
8.85659965593547));
#388426=CARTESIAN_POINT('Ctrl Pts',(2.63108542040041,-0.430109661376531,
8.85555568965886));
#388427=CARTESIAN_POINT('Ctrl Pts',(2.63142813134851,-0.430604690778865,
8.85434650606346));
#388428=CARTESIAN_POINT('Ctrl Pts',(2.63183710943965,-0.431044620128023,
8.85297329937117));
#388429=CARTESIAN_POINT('Ctrl Pts',(2.63206713469651,-0.431292053581636,
8.85220095427747));
#388430=CARTESIAN_POINT('Ctrl Pts',(2.63231844750382,-0.43152194335517,
8.85137579139183));
#388431=CARTESIAN_POINT('Ctrl Pts',(2.63259257497231,-0.431734128529198,
8.85049129520029));
#388432=CARTESIAN_POINT('Origin',(2.63680073810824,-0.426297494642185,7.59394543036555));
#388433=CARTESIAN_POINT('Ctrl Pts',(2.6339896589008,-0.419998320072209,
7.59443877723642));
#388434=CARTESIAN_POINT('Ctrl Pts',(2.62852678336725,-0.421919305380218,
7.58783886950016));
#388435=CARTESIAN_POINT('Ctrl Pts',(2.62941353036883,-0.430362815390389,
7.58559994247159));
#388436=CARTESIAN_POINT('Ctrl Pts',(2.66381133616453,-0.409511717635095,
7.56670252222135));
#388437=CARTESIAN_POINT('Ctrl Pts',(2.65835635603704,-0.411429926574036,
7.56004874999023));
#388438=CARTESIAN_POINT('Ctrl Pts',(2.65922710860603,-0.419925698888471,
7.55786368756704));
#388439=CARTESIAN_POINT('Ctrl Pts',(2.69357732442548,-0.399044697880303,
7.53888913333558));
#388440=CARTESIAN_POINT('Ctrl Pts',(2.688089925084,-0.400974306828814,7.53222002137274));
#388441=CARTESIAN_POINT('Ctrl Pts',(2.68898568384657,-0.409506602004158,
7.53005029815327));
#388442=CARTESIAN_POINT('Ctrl Pts',(2.72328627675262,-0.388597734447536,
7.51101258149734));
#388443=CARTESIAN_POINT('Ctrl Pts',(2.7177323601603,-0.390550733762682,
7.5043616886572));
#388444=CARTESIAN_POINT('Ctrl Pts',(2.71868781310116,-0.399106117519269,
7.50217374673251));
#388445=CARTESIAN_POINT('',(2.71710286899021,-0.399661099761578,7.50366116523517));
#388446=CARTESIAN_POINT('Ctrl Pts',(2.71519273396522,-0.391443777101968,
7.51860402984325));
#388447=CARTESIAN_POINT('Ctrl Pts',(2.71560933845096,-0.391297280794034,
7.51734760759493));
#388448=CARTESIAN_POINT('Ctrl Pts',(2.71600553713428,-0.391221028165804,
7.51608817408572));
#388449=CARTESIAN_POINT('Ctrl Pts',(2.71638294247709,-0.391228307594241,
7.51481005913119));
#388450=CARTESIAN_POINT('Ctrl Pts',(2.71672480525499,-0.391234901474467,
7.51365231206383));
#388451=CARTESIAN_POINT('Ctrl Pts',(2.71705173448721,-0.391309793993965,
7.51247773061042));
#388452=CARTESIAN_POINT('Ctrl Pts',(2.71734982796114,-0.391487681960311,
7.51129758471022));
#388453=CARTESIAN_POINT('Ctrl Pts',(2.71772032410568,-0.391708776386907,
7.50983079813401));
#388454=CARTESIAN_POINT('Ctrl Pts',(2.71802777713899,-0.392093102944501,
7.50839324291155));
#388455=CARTESIAN_POINT('Ctrl Pts',(2.71821005578271,-0.392694965359655,
7.50715379678855));
#388456=CARTESIAN_POINT('Ctrl Pts',(2.71829426326387,-0.392973008453208,
7.50658120839351));
#388457=CARTESIAN_POINT('Ctrl Pts',(2.71835463339421,-0.393339757954554,
7.50598221009429));
#388458=CARTESIAN_POINT('Ctrl Pts',(2.71836728500343,-0.393790180293171,
7.50545747549611));
#388459=CARTESIAN_POINT('Ctrl Pts',(2.71837403629372,-0.394030539594932,
7.50517746087247));
#388460=CARTESIAN_POINT('Ctrl Pts',(2.71836747479092,-0.394297326408292,
7.50491486231392));
#388461=CARTESIAN_POINT('Ctrl Pts',(2.71834610674268,-0.394583434757196,
7.50468370960992));
#388462=CARTESIAN_POINT('Ctrl Pts',(2.71831415477039,-0.395011256986576,
7.50433806340446));
#388463=CARTESIAN_POINT('Ctrl Pts',(2.71824758258208,-0.39549506886164,
7.50405484070983));
#388464=CARTESIAN_POINT('Ctrl Pts',(2.71815016398296,-0.396002188896856,
7.5038576603613));
#388465=CARTESIAN_POINT('Ctrl Pts',(2.71813974657802,-0.396056417502185,
7.50383657498791));
#388466=CARTESIAN_POINT('Ctrl Pts',(2.71812899521642,-0.396110891374371,
7.50381643264937));
#388467=CARTESIAN_POINT('Ctrl Pts',(2.71811792839077,-0.396165555317011,
7.50379723213559));
#388468=CARTESIAN_POINT('Ctrl Pts',(2.71804405370937,-0.396530455015994,
7.50366906242519));
#388469=CARTESIAN_POINT('Ctrl Pts',(2.71795381025399,-0.396911618989233,
7.50358235568538));
#388470=CARTESIAN_POINT('Ctrl Pts',(2.7178579952463,-0.397276923242064,
7.5035341175365));
#388471=CARTESIAN_POINT('Ctrl Pts',(2.71771433148643,-0.397824655624726,
7.50346178989176));
#388472=CARTESIAN_POINT('Ctrl Pts',(2.71753649302519,-0.398407782609515,
7.50346967198527));
#388473=CARTESIAN_POINT('Ctrl Pts',(2.71734429645071,-0.398974860740826,
7.50354272648693));
#388474=CARTESIAN_POINT('Ctrl Pts',(2.71726524202139,-0.399208111714057,
7.50357277531559));
#388475=CARTESIAN_POINT('Ctrl Pts',(2.71718399774965,-0.399438383067811,
7.50361331098762));
#388476=CARTESIAN_POINT('Ctrl Pts',(2.71710286899161,-0.399661099761784,
7.50366116523659));
#388477=CARTESIAN_POINT('',(2.63969113251167,-0.426764791194187,7.57603338622103));
#388478=CARTESIAN_POINT('Origin',(2.64841434182012,-0.428177982248983,7.58486873427629));
#388479=CARTESIAN_POINT('Ctrl Pts',(2.71710286904233,-0.399661099737652,
7.50366116529968));
#388480=CARTESIAN_POINT('Ctrl Pts',(2.69134133975362,-0.408681709889291,
7.52783573079709));
#388481=CARTESIAN_POINT('Ctrl Pts',(2.66553865185168,-0.417715864046317,
7.55196141284068));
#388482=CARTESIAN_POINT('Ctrl Pts',(2.63969113352841,-0.426764790463517,
7.57603338728831));
#388483=CARTESIAN_POINT('Ctrl Pts',(2.63452008471591,-0.419811799220407,
7.59394543036555));
#388484=CARTESIAN_POINT('Ctrl Pts',(2.62260349002129,-0.42400219367279,
7.59394543036555));
#388485=CARTESIAN_POINT('Ctrl Pts',(2.63259257497231,-0.431734128529198,
7.59394543036555));
#388486=CARTESIAN_POINT('Ctrl Pts',(2.63231908349194,-0.42058576725028,
7.58587155981959));
#388487=CARTESIAN_POINT('Ctrl Pts',(2.62837738985167,-0.424935673020103,
7.58685956158229));
#388488=CARTESIAN_POINT('Ctrl Pts',(2.63074758579823,-0.430306036148894,
7.5858715598196));
#388489=CARTESIAN_POINT('Ctrl Pts',(2.63624690107239,-0.424282632632025,
7.57982961904599));
#388490=CARTESIAN_POINT('Ctrl Pts',(2.63431416214112,-0.425895484323621,
7.58148017275035));
#388491=CARTESIAN_POINT('Ctrl Pts',(2.63564021630889,-0.428035192411078,
7.57982961904594));
#388492=CARTESIAN_POINT('Ctrl Pts',(2.63969113169474,-0.426764791061906,
7.57603338509286));
#388493=CARTESIAN_POINT('Ctrl Pts',(2.63969113169474,-0.426764791061906,
7.57603338509286));
#388494=CARTESIAN_POINT('Ctrl Pts',(2.63969113169474,-0.426764791061906,
7.57603338509286));
#388495=CARTESIAN_POINT('Origin',(2.6484152525544,-0.428172349042147,7.58486873427623));
#388496=CARTESIAN_POINT('Ctrl Pts',(2.70702227397444,-0.489345570106521,
7.51098857897448));
#388497=CARTESIAN_POINT('Ctrl Pts',(2.70236668241661,-0.485741963688148,
7.50433767179956));
#388498=CARTESIAN_POINT('Ctrl Pts',(2.70596936051755,-0.477923475241943,
7.50214974420965));
#388499=CARTESIAN_POINT('Ctrl Pts',(2.68211158316674,-0.470063740039231,
7.53887321589167));
#388500=CARTESIAN_POINT('Ctrl Pts',(2.67751177385794,-0.466503311221007,
7.53220407452061));
#388501=CARTESIAN_POINT('Ctrl Pts',(2.68105049686829,-0.458687918756247,
7.53003438070911));
#388502=CARTESIAN_POINT('Ctrl Pts',(2.65715305464352,-0.450744881745442,
7.56669465659232));
#388503=CARTESIAN_POINT('Ctrl Pts',(2.65258042935253,-0.447205494399605,
7.56004085833298));
#388504=CARTESIAN_POINT('Ctrl Pts',(2.6560839004508,-0.439416891162163,
7.55785582193789));
#388505=CARTESIAN_POINT('Ctrl Pts',(2.63214781717912,-0.431389868939786,
7.59443891967696));
#388506=CARTESIAN_POINT('Ctrl Pts',(2.6275685621508,-0.427845349922939,
7.58783901202978));
#388507=CARTESIAN_POINT('Ctrl Pts',(2.6310707537066,-0.420111409640341,
7.58560008491213));
#388508=CARTESIAN_POINT('',(2.70461858999358,-0.476880779648988,7.50366116523517));
#388509=CARTESIAN_POINT('Ctrl Pts',(2.70461858999394,-0.476880779649052,
7.50366116523554));
#388510=CARTESIAN_POINT('Ctrl Pts',(2.70464020690383,-0.477638189858893,
7.50350835821027));
#388511=CARTESIAN_POINT('Ctrl Pts',(2.7046354365397,-0.478335136954998,
7.50345484955999));
#388512=CARTESIAN_POINT('Ctrl Pts',(2.70460473756223,-0.478992345851136,
7.50349758195598));
#388513=CARTESIAN_POINT('Ctrl Pts',(2.7045889867101,-0.479329542754738,
7.50351950684424));
#388514=CARTESIAN_POINT('Ctrl Pts',(2.70456498711403,-0.479689520295334,
7.50357029184312));
#388515=CARTESIAN_POINT('Ctrl Pts',(2.70453230288058,-0.480036006358213,
7.50365515313923));
#388516=CARTESIAN_POINT('Ctrl Pts',(2.70448202129437,-0.480569042228984,
7.50378570417639));
#388517=CARTESIAN_POINT('Ctrl Pts',(2.7044100554912,-0.481085827292566,
7.50400001621911));
#388518=CARTESIAN_POINT('Ctrl Pts',(2.70431963439798,-0.481546713552094,
7.50428903009634));
#388519=CARTESIAN_POINT('Ctrl Pts',(2.70430959835229,-0.481597868381055,
7.50432110841318));
#388520=CARTESIAN_POINT('Ctrl Pts',(2.70429934703204,-0.481648362380225,
7.50435406373354));
#388521=CARTESIAN_POINT('Ctrl Pts',(2.7042888934907,-0.481698161980479,
7.50438785222351));
#388522=CARTESIAN_POINT('Ctrl Pts',(2.70422506959627,-0.482002212476761,
7.50459414719561));
#388523=CARTESIAN_POINT('Ctrl Pts',(2.7041521866378,-0.482285112778645,
7.50483629897752));
#388524=CARTESIAN_POINT('Ctrl Pts',(2.704074311158,-0.482536353384292,7.5050991045531));
#388525=CARTESIAN_POINT('Ctrl Pts',(2.70390251002772,-0.483090615395077,
7.50567888004914));
#388526=CARTESIAN_POINT('Ctrl Pts',(2.70370013790804,-0.483512788619057,
7.50637912803144));
#388527=CARTESIAN_POINT('Ctrl Pts',(2.70349061296512,-0.483823047491796,
7.50710440483569));
#388528=CARTESIAN_POINT('Ctrl Pts',(2.70343923328946,-0.483899129126894,
7.50728225710685));
#388529=CARTESIAN_POINT('Ctrl Pts',(2.70338652163312,-0.483970077276551,
7.50746498566954));
#388530=CARTESIAN_POINT('Ctrl Pts',(2.70333404285786,-0.484034484228082,
7.50764697238949));
#388531=CARTESIAN_POINT('Ctrl Pts',(2.70305193140459,-0.484380718274245,
7.50862528291182));
#388532=CARTESIAN_POINT('Ctrl Pts',(2.70275414916696,-0.484571966827617,
7.50965856837422));
#388533=CARTESIAN_POINT('Ctrl Pts',(2.70246021538533,-0.484671589142442,
7.51067959873203));
#388534=CARTESIAN_POINT('Ctrl Pts',(2.70229846325455,-0.484726411427947,
7.51124147302579));
#388535=CARTESIAN_POINT('Ctrl Pts',(2.70213769764104,-0.484753088363596,
7.51180065547253));
#388536=CARTESIAN_POINT('Ctrl Pts',(2.70198039405431,-0.484759576290765,
7.51235175716501));
#388537=CARTESIAN_POINT('Ctrl Pts',(2.70143684749986,-0.484781994663616,
7.51425603304535));
#388538=CARTESIAN_POINT('Ctrl Pts',(2.70086957912379,-0.484559974355606,
7.51626900505178));
#388539=CARTESIAN_POINT('Ctrl Pts',(2.70030761830456,-0.484146430039385,
7.5182778896924));
#388540=CARTESIAN_POINT('Ctrl Pts',(2.70027720392306,-0.484124048239498,
7.51838661432543));
#388541=CARTESIAN_POINT('Ctrl Pts',(2.70024680297324,-0.484101095696744,
7.51849533314855));
#388542=CARTESIAN_POINT('Ctrl Pts',(2.70021641947034,-0.484077577700225,
7.51860402984325));
#388543=CARTESIAN_POINT('Ctrl Pts',(2.63969113324751,-0.426764792208446,
7.57603338728985));
#388544=CARTESIAN_POINT('Ctrl Pts',(2.66137047798472,-0.443497493271866,
7.55196141284922));
#388545=CARTESIAN_POINT('Ctrl Pts',(2.68301193102657,-0.460202048212605,
7.52783573083105));
#388546=CARTESIAN_POINT('Ctrl Pts',(2.7046185900369,-0.476880779689299,
7.50366116530176));
#388547=CARTESIAN_POINT('Origin',(9.12135307609335E-16,-1.47466962819311E-16,
7.49482233047033));
#388548=CARTESIAN_POINT('Origin',(2.70835812744774,-0.39837482787917,7.49482233047033));
#388549=CARTESIAN_POINT('Origin',(0.,0.,7.50366116523517));
#388550=CARTESIAN_POINT('Origin',(2.69591402793582,-0.475345983446682,7.49482233047033));
#388551=CARTESIAN_POINT('Ctrl Pts',(2.7151917361247,-0.391444127938779,
7.51860402984325));
#388552=CARTESIAN_POINT('Ctrl Pts',(2.72237004465167,-0.388920604068918,
7.51860402984325));
#388553=CARTESIAN_POINT('Ctrl Pts',(2.72342529733067,-0.381385172574072,
7.51860402984325));
#388554=CARTESIAN_POINT('Ctrl Pts',(2.71785709064665,-0.390507125105668,
7.51041458714366));
#388555=CARTESIAN_POINT('Ctrl Pts',(2.72262003629419,-0.387135372665372,
7.51004642900442));
#388556=CARTESIAN_POINT('Ctrl Pts',(2.72342558835683,-0.38138309439154,
7.5072913648301));
#388557=CARTESIAN_POINT('Ctrl Pts',(2.71964944662412,-0.392677654361235,
7.50215815450138));
#388558=CARTESIAN_POINT('Ctrl Pts',(2.72211116740598,-0.390770301411823,
7.4987716367153));
#388559=CARTESIAN_POINT('Ctrl Pts',(2.72261327489375,-0.387356826398718,
7.49481588533171));
#388560=CARTESIAN_POINT('Ctrl Pts',(2.71710232433262,-0.399661019647884,
7.50366171572174));
#388561=CARTESIAN_POINT('Ctrl Pts',(2.72072505953649,-0.400193891020553,
7.50000045605858));
#388562=CARTESIAN_POINT('Ctrl Pts',(2.72072505953651,-0.400193891020429,
7.49482233047317));
#388563=CARTESIAN_POINT('Origin',(2.71104609143371,-0.379651603607827,7.51860402984325));
#388564=CARTESIAN_POINT('Origin',(2.71104609143371,-0.379651603607827,9.));
#388565=CARTESIAN_POINT('Origin',(2.71104609143371,-0.379651603607827,8.75721825406948));
#388566=CARTESIAN_POINT('Ctrl Pts',(2.69943822817004,-0.396983716469034,
8.78942910404912));
#388567=CARTESIAN_POINT('Ctrl Pts',(2.70470182062058,-0.395154229323313,
8.79672699501691));
#388568=CARTESIAN_POINT('Ctrl Pts',(2.70336947938123,-0.386328224972305,
8.79893251111267));
#388569=CARTESIAN_POINT('Ctrl Pts',(2.70980999884858,-0.393336554321229,
8.78111911759582));
#388570=CARTESIAN_POINT('Ctrl Pts',(2.71604760481809,-0.391160644880441,
8.78644465894812));
#388571=CARTESIAN_POINT('Ctrl Pts',(2.71658483983411,-0.383071955844943,
8.78817647674132));
#388572=CARTESIAN_POINT('Ctrl Pts',(2.71627393371496,-0.391063555847674,
8.7678092393203));
#388573=CARTESIAN_POINT('Ctrl Pts',(2.7236354857743,-0.388490175182447,
8.76988516158376));
#388574=CARTESIAN_POINT('Ctrl Pts',(2.72483625397649,-0.381027297981203,
8.77093053738833));
#388575=CARTESIAN_POINT('Ctrl Pts',(2.71501355488061,-0.391506759440208,
8.75371302330492));
#388576=CARTESIAN_POINT('Ctrl Pts',(2.72219468292135,-0.388997257212617,
8.75300828287558));
#388577=CARTESIAN_POINT('Ctrl Pts',(2.72322678304318,-0.381425645186582,
8.75267964240737));
#388578=CARTESIAN_POINT('Origin',(2.69781755467073,-0.384303334113505,8.78727029226991));
#388579=CARTESIAN_POINT('Ctrl Pts',(2.63452008471591,-0.419811799220407,
8.85049129520029));
#388580=CARTESIAN_POINT('Ctrl Pts',(2.64002902569028,-0.417874615294201,
8.85711686593484));
#388581=CARTESIAN_POINT('Ctrl Pts',(2.63910781935456,-0.409374489353903,
8.85933012996512));
#388582=CARTESIAN_POINT('Ctrl Pts',(2.65703416460907,-0.411894866749133,
8.82945683644723));
#388583=CARTESIAN_POINT('Ctrl Pts',(2.66258883312431,-0.40994160302509,
8.8360746990239));
#388584=CARTESIAN_POINT('Ctrl Pts',(2.66162763804509,-0.401420561626453,
8.83829567148519));
#388585=CARTESIAN_POINT('Ctrl Pts',(2.67951468545064,-0.403989735104122,
8.80838214965002));
#388586=CARTESIAN_POINT('Ctrl Pts',(2.68509127528129,-0.402028762889457,
8.81501364461993));
#388587=CARTESIAN_POINT('Ctrl Pts',(2.68411351798303,-0.393479329969036,
8.81722098428722));
#388588=CARTESIAN_POINT('Ctrl Pts',(2.70196419720224,-0.396095507607646,
8.78727029226991));
#388589=CARTESIAN_POINT('Ctrl Pts',(2.70754171332274,-0.394134209669065,
8.79393457792714));
#388590=CARTESIAN_POINT('Ctrl Pts',(2.7065680531042,-0.385549840096578,
8.79610912703474));
#388591=CARTESIAN_POINT('Origin',(2.6303734421844,-0.408019625726266,8.85049129520029));
#388592=CARTESIAN_POINT('Ctrl Pts',(2.63259257497231,-0.431734128529198,
8.85049129520029));
#388593=CARTESIAN_POINT('Ctrl Pts',(2.63721044448901,-0.435308536641013,
8.85711686593484));
#388594=CARTESIAN_POINT('Ctrl Pts',(2.63365770878388,-0.443085350328085,
8.85933012996512));
#388595=CARTESIAN_POINT('Ctrl Pts',(2.62850721247053,-0.428571901269797,
8.86332496987233));
#388596=CARTESIAN_POINT('Ctrl Pts',(2.62804976815553,-0.433170013825567,
8.86648636486737));
#388597=CARTESIAN_POINT('Ctrl Pts',(2.62223922743675,-0.434225342422791,
8.87206031107457));
#388598=CARTESIAN_POINT('Ctrl Pts',(2.62961328596244,-0.421537243678529,
8.86341338519875));
#388599=CARTESIAN_POINT('Ctrl Pts',(2.63060202922409,-0.417010008606569,
8.86654584966057));
#388600=CARTESIAN_POINT('Ctrl Pts',(2.62537340940882,-0.414219724102321,
8.87215952290714));
#388601=CARTESIAN_POINT('Ctrl Pts',(2.63452008471591,-0.419811799220407,
8.85049129520029));
#388602=CARTESIAN_POINT('Ctrl Pts',(2.64002902569028,-0.417874615294201,
8.85711686593484));
#388603=CARTESIAN_POINT('Ctrl Pts',(2.63910781935456,-0.409374489353903,
8.85933012996512));
#388604=CARTESIAN_POINT('Origin',(2.62494136927062,-0.441618917414677,8.85049129520029));
#388605=CARTESIAN_POINT('Ctrl Pts',(2.68912759914127,-0.47549440548382,
8.78727029226991));
#388606=CARTESIAN_POINT('Ctrl Pts',(2.69380295177104,-0.479113307729762,
8.79393457792714));
#388607=CARTESIAN_POINT('Ctrl Pts',(2.69017388854615,-0.486953544670569,
8.79610912703474));
#388608=CARTESIAN_POINT('Ctrl Pts',(2.67030929695492,-0.460928317866537,
8.80838214965004));
#388609=CARTESIAN_POINT('Ctrl Pts',(2.67498387312222,-0.464546619100754,
8.81501364461989));
#388610=CARTESIAN_POINT('Ctrl Pts',(2.6713619303665,-0.472352408187678,
8.81722098428721));
#388611=CARTESIAN_POINT('Ctrl Pts',(2.65146500140035,-0.446342110385339,
8.82945683644723));
#388612=CARTESIAN_POINT('Ctrl Pts',(2.65612120202605,-0.449946188245605,
8.8360746990239));
#388613=CARTESIAN_POINT('Ctrl Pts',(2.65252392414128,-0.457730251086919,
8.8382956714852));
#388614=CARTESIAN_POINT('Ctrl Pts',(2.63259257497231,-0.431734128529198,
8.85049129520029));
#388615=CARTESIAN_POINT('Ctrl Pts',(2.63721044448901,-0.435308536641013,
8.85711686593484));
#388616=CARTESIAN_POINT('Ctrl Pts',(2.63365770878388,-0.443085350328085,
8.85933012996512));
#388617=CARTESIAN_POINT('Origin',(2.68147639343958,-0.485379194369299,8.78727029226991));
#388618=CARTESIAN_POINT('Ctrl Pts',(2.70006998588465,-0.483964255816424,
8.75374538247849));
#388619=CARTESIAN_POINT('Ctrl Pts',(2.70608714808813,-0.488605175704168,
8.75304829418602));
#388620=CARTESIAN_POINT('Ctrl Pts',(2.70468784035867,-0.496109346616881,
8.75272238421917));
#388621=CARTESIAN_POINT('Ctrl Pts',(2.70111380694607,-0.484772212811475,
8.76769408445016));
#388622=CARTESIAN_POINT('Ctrl Pts',(2.70728196617974,-0.489530465289032,
8.76974318093965));
#388623=CARTESIAN_POINT('Ctrl Pts',(2.70607444581406,-0.496984340244159,
8.77077869880429));
#388624=CARTESIAN_POINT('Ctrl Pts',(2.69576377481994,-0.480631085505929,
8.78108014887994));
#388625=CARTESIAN_POINT('Ctrl Pts',(2.70099338824204,-0.484660524766635,
8.7863940336633));
#388626=CARTESIAN_POINT('Ctrl Pts',(2.69897660913033,-0.492499828163205,
8.78812224174742));
#388627=CARTESIAN_POINT('Ctrl Pts',(2.6869962531754,-0.473844692043162,
8.78944554828685));
#388628=CARTESIAN_POINT('Ctrl Pts',(2.69140699401535,-0.477236119892865,
8.79673892988685));
#388629=CARTESIAN_POINT('Ctrl Pts',(2.68736801332924,-0.485185345599418,
8.79894799272499));
#388630=CARTESIAN_POINT('Origin',(2.69256521376866,-0.4939623665857,8.75721825406948));
#388631=CARTESIAN_POINT('Origin',(2.69256521376866,-0.4939623665857,9.));
#388632=CARTESIAN_POINT('Origin',(2.69256521376866,-0.4939623665857,7.51860402984325));
#388633=CARTESIAN_POINT('Ctrl Pts',(2.7046178152802,-0.476880643050886,
7.50366195182966));
#388634=CARTESIAN_POINT('Ctrl Pts',(2.70822413765239,-0.477516513051599,
7.50000065167734));
#388635=CARTESIAN_POINT('Ctrl Pts',(2.70822413765237,-0.477516513051714,
7.49482233047108));
#388636=CARTESIAN_POINT('Ctrl Pts',(2.70483396261146,-0.484317516045493,
7.50215800491338));
#388637=CARTESIAN_POINT('Ctrl Pts',(2.70656871882112,-0.486905047314359,
7.49877273257269));
#388638=CARTESIAN_POINT('Ctrl Pts',(2.70596930723901,-0.490304732903523,
7.49481816995649));
#388639=CARTESIAN_POINT('Ctrl Pts',(2.7024455167135,-0.485802555618879,
7.51043025814041));
#388640=CARTESIAN_POINT('Ctrl Pts',(2.70590829471323,-0.490503824119134,
7.51006209594513));
#388641=CARTESIAN_POINT('Ctrl Pts',(2.70485957523923,-0.496220392812597,
7.50731281821699));
#388642=CARTESIAN_POINT('Ctrl Pts',(2.70021522421894,-0.484076652645348,
7.51860402984326));
#388643=CARTESIAN_POINT('Ctrl Pts',(2.70623307096702,-0.488733533351057,
7.51860402984326));
#388644=CARTESIAN_POINT('Ctrl Pts',(2.70486003209637,-0.496217902506188,
7.51860402984327));
#388645=CARTESIAN_POINT('Origin',(0.,0.,7.5));
#388646=CARTESIAN_POINT('Origin',(2.59952233059431,-0.599517869856861,7.5));
#388647=CARTESIAN_POINT('',(2.59952233059431,-0.599517869856861,7.59394543036555));
#388648=CARTESIAN_POINT('',(2.59952233059431,-0.599517869856861,8.85049129520029));
#388649=CARTESIAN_POINT('',(2.59952233059431,-0.599517869856861,7.5));
#388650=CARTESIAN_POINT('',(2.65313746692185,-0.646810448064325,8.78727029226991));
#388651=CARTESIAN_POINT('Ctrl Pts',(2.59952233059431,-0.599517869856862,
8.85049129520029));
#388652=CARTESIAN_POINT('Ctrl Pts',(2.61742002096782,-0.615304977373503,
8.82945686509571));
#388653=CARTESIAN_POINT('Ctrl Pts',(2.63529110426045,-0.631068615445882,
8.80838212259897));
#388654=CARTESIAN_POINT('Ctrl Pts',(2.65313746692185,-0.646810448064325,
8.78727029226991));
#388655=CARTESIAN_POINT('',(2.66365357834826,-0.656086448390676,8.75721825406948));
#388656=CARTESIAN_POINT('Origin',(2.63200708449507,-0.628171594201918,8.75937679713125));
#388657=CARTESIAN_POINT('',(2.66365357834826,-0.656086448390676,7.51860402984325));
#388658=CARTESIAN_POINT('',(2.66365357834826,-0.656086448390676,7.5));
#388659=CARTESIAN_POINT('Ctrl Pts',(2.66365357834826,-0.656086448390676,
7.51860402984325));
#388660=CARTESIAN_POINT('Ctrl Pts',(2.65539480838751,-0.648801592825264,
7.52834476460825));
#388661=CARTESIAN_POINT('Ctrl Pts',(2.64713067695249,-0.641512008036736,
7.53807742314407));
#388662=CARTESIAN_POINT('Ctrl Pts',(2.63886100402454,-0.634217535235136,
7.54780169004674));
#388663=CARTESIAN_POINT('Ctrl Pts',(2.62576228904436,-0.62266348455002,
7.5632044032688));
#388664=CARTESIAN_POINT('Ctrl Pts',(2.61264965451768,-0.611097155779176,
7.57858609112103));
#388665=CARTESIAN_POINT('Ctrl Pts',(2.59952233059431,-0.599517869856862,
7.59394543036555));
#388666=CARTESIAN_POINT('Origin',(2.86694941950356,-0.513326427708308,7.5));
#388667=CARTESIAN_POINT('',(2.68453419038077,-0.564602509634883,8.75721825406948));
#388668=CARTESIAN_POINT('',(2.67103479566854,-0.568397127400913,8.78727029226991));
#388669=CARTESIAN_POINT('Origin',(2.63676829686558,-0.57802928261299,8.75658640621034));
#388670=CARTESIAN_POINT('',(2.60220974632392,-0.587743532225588,8.85049129520029));
#388671=CARTESIAN_POINT('Ctrl Pts',(2.67103479566854,-0.568397127400913,
8.78727029226991));
#388672=CARTESIAN_POINT('Ctrl Pts',(2.64812565330825,-0.574836781952687,
8.80838212259896));
#388673=CARTESIAN_POINT('Ctrl Pts',(2.62518477739698,-0.581285356659693,
8.82945686509571));
#388674=CARTESIAN_POINT('Ctrl Pts',(2.60220974632392,-0.587743532225588,
8.85049129520029));
#388675=CARTESIAN_POINT('',(2.60220974632392,-0.587743532225588,7.59394543036555));
#388676=CARTESIAN_POINT('',(2.60220974632392,-0.587743532225588,7.5));
#388677=CARTESIAN_POINT('',(2.68453419038077,-0.564602509634883,7.51860402984325));
#388678=CARTESIAN_POINT('Ctrl Pts',(2.60220974632392,-0.587743532225589,
7.59394543036555));
#388679=CARTESIAN_POINT('Ctrl Pts',(2.61906112037002,-0.58300668848552,
7.57858609112103));
#388680=CARTESIAN_POINT('Ctrl Pts',(2.6358936378295,-0.578275145245242,
7.56320440326857));
#388681=CARTESIAN_POINT('Ctrl Pts',(2.65270828694938,-0.573548624713022,
7.54780169004651));
#388682=CARTESIAN_POINT('Ctrl Pts',(2.66332395793925,-0.570564608422276,
7.53807742314383));
#388683=CARTESIAN_POINT('Ctrl Pts',(2.67393251538732,-0.567582591715406,
7.52834476460825));
#388684=CARTESIAN_POINT('Ctrl Pts',(2.68453419038077,-0.564602509634883,
7.51860402984325));
#388685=CARTESIAN_POINT('',(2.68453419038077,-0.564602509634883,7.5));
#388686=CARTESIAN_POINT('Origin',(2.60407017393685,-0.594362024055079,7.5));
#388687=CARTESIAN_POINT('Ctrl Pts',(2.60220974632392,-0.587743532225589,
8.85049129520029));
#388688=CARTESIAN_POINT('Ctrl Pts',(2.60202331038289,-0.58779593851114,
8.85097269580138));
#388689=CARTESIAN_POINT('Ctrl Pts',(2.60184150286887,-0.587855781174737,
8.85143669361005));
#388690=CARTESIAN_POINT('Ctrl Pts',(2.60165622548117,-0.587926646233105,
8.8519052845931));
#388691=CARTESIAN_POINT('Ctrl Pts',(2.60129383466069,-0.588065253793175,
8.85282181883899));
#388692=CARTESIAN_POINT('Ctrl Pts',(2.60092756183387,-0.588242647837744,
8.85372622499635));
#388693=CARTESIAN_POINT('Ctrl Pts',(2.60055838042438,-0.588475488848286,
8.85462257735071));
#388694=CARTESIAN_POINT('Ctrl Pts',(2.6002518991303,-0.588668785185507,
8.85536669723986));
#388695=CARTESIAN_POINT('Ctrl Pts',(2.59994332657568,-0.588900311421531,
8.85610498449051));
#388696=CARTESIAN_POINT('Ctrl Pts',(2.59963799631076,-0.589186020321747,
8.85681338218371));
#388697=CARTESIAN_POINT('Ctrl Pts',(2.59936090861582,-0.589445301597408,
8.85745625420284));
#388698=CARTESIAN_POINT('Ctrl Pts',(2.59908260643578,-0.5897520209105,8.85808743050666));
#388699=CARTESIAN_POINT('Ctrl Pts',(2.59881389793109,-0.590132655228678,
8.8586680450841));
#388700=CARTESIAN_POINT('Ctrl Pts',(2.59868992165192,-0.590308271651945,
8.85893592806396));
#388701=CARTESIAN_POINT('Ctrl Pts',(2.59856810529722,-0.59049983421699,
8.85919241173848));
#388702=CARTESIAN_POINT('Ctrl Pts',(2.59845047286813,-0.590711216603711,
8.85943017985534));
#388703=CARTESIAN_POINT('Ctrl Pts',(2.59829163426593,-0.590996645401669,
8.8597512372));
#388704=CARTESIAN_POINT('Ctrl Pts',(2.59813694107697,-0.591325788054068,
8.86004599534705));
#388705=CARTESIAN_POINT('Ctrl Pts',(2.59799767783027,-0.59169912012104,
8.86026130871721));
#388706=CARTESIAN_POINT('Ctrl Pts',(2.59794668962941,-0.591835807516104,
8.86034014101235));
#388707=CARTESIAN_POINT('Ctrl Pts',(2.59789699236397,-0.591980467381848,
8.86040910639692));
#388708=CARTESIAN_POINT('Ctrl Pts',(2.59785025813687,-0.592129267833198,
8.86046313645506));
#388709=CARTESIAN_POINT('Ctrl Pts',(2.59777732976686,-0.592361469691337,
8.86054744990829));
#388710=CARTESIAN_POINT('Ctrl Pts',(2.59770976635182,-0.592610136901937,
8.86059655985669));
#388711=CARTESIAN_POINT('Ctrl Pts',(2.59765161823107,-0.592859244867328,
8.86059725258816));
#388712=CARTESIAN_POINT('Ctrl Pts',(2.59759333576493,-0.593108928371637,
8.86059794692011));
#388713=CARTESIAN_POINT('Ctrl Pts',(2.5975464530103,-0.593362427609925,
8.86056369958366));
#388714=CARTESIAN_POINT('Ctrl Pts',(2.59750982662749,-0.593605232259505,
8.86048590497774));
#388715=CARTESIAN_POINT('Ctrl Pts',(2.59750026823208,-0.59366859704388,
8.86046560290182));
#388716=CARTESIAN_POINT('Ctrl Pts',(2.59749137356795,-0.593732071318801,
8.86044257503091));
#388717=CARTESIAN_POINT('Ctrl Pts',(2.59748338497903,-0.593793689121195,
8.86041778462583));
#388718=CARTESIAN_POINT('Ctrl Pts',(2.59742963168864,-0.594208300469986,
8.86025097596201));
#388719=CARTESIAN_POINT('Ctrl Pts',(2.59741001819078,-0.594594535816525,
8.8599848982295));
#388720=CARTESIAN_POINT('Ctrl Pts',(2.5974166553662,-0.594940692276284,
8.85968173251462));
#388721=CARTESIAN_POINT('Ctrl Pts',(2.59742016605173,-0.595123789211096,
8.85952137522077));
#388722=CARTESIAN_POINT('Ctrl Pts',(2.59743089790697,-0.595299205846458,
8.85934740853961));
#388723=CARTESIAN_POINT('Ctrl Pts',(2.59744714793787,-0.595464563348879,
8.8591675900182));
#388724=CARTESIAN_POINT('Ctrl Pts',(2.59751240025854,-0.596128559672226,
8.85844552518695));
#388725=CARTESIAN_POINT('Ctrl Pts',(2.59766730636048,-0.59666818199703,
8.85759444184123));
#388726=CARTESIAN_POINT('Ctrl Pts',(2.59783312773383,-0.597096816488941,
8.85683498915137));
#388727=CARTESIAN_POINT('Ctrl Pts',(2.59785048049893,-0.597141671946968,
8.85675551444997));
#388728=CARTESIAN_POINT('Ctrl Pts',(2.59786796965055,-0.597185301258604,
8.85667699793651));
#388729=CARTESIAN_POINT('Ctrl Pts',(2.59788551566069,-0.597227712156552,
8.85659965593547));
#388730=CARTESIAN_POINT('Ctrl Pts',(2.59812235260095,-0.597800176621216,
8.85555568965886));
#388731=CARTESIAN_POINT('Ctrl Pts',(2.59843264276995,-0.598316146498386,
8.85434650606346));
#388732=CARTESIAN_POINT('Ctrl Pts',(2.59881259420155,-0.59878137528178,
8.85297329937118));
#388733=CARTESIAN_POINT('Ctrl Pts',(2.59902629373105,-0.599043038125634,
8.85220095427748));
#388734=CARTESIAN_POINT('Ctrl Pts',(2.59926236110088,-0.599288557232821,
8.85137579139184));
#388735=CARTESIAN_POINT('Ctrl Pts',(2.59952233059431,-0.599517869856861,
8.85049129520029));
#388736=CARTESIAN_POINT('Origin',(2.60407017393685,-0.594362024055079,7.59394543036555));
#388737=CARTESIAN_POINT('Ctrl Pts',(2.60166845989353,-0.587895685351639,
7.59443877723642));
#388738=CARTESIAN_POINT('Ctrl Pts',(2.59609373047239,-0.589462716152146,
7.58783886950016));
#388739=CARTESIAN_POINT('Ctrl Pts',(2.59643767801339,-0.597945692140895,
7.58559994247159));
#388740=CARTESIAN_POINT('Ctrl Pts',(2.63210074424794,-0.579341310186399,
7.56670252222136));
#388741=CARTESIAN_POINT('Ctrl Pts',(2.62653407189352,-0.580906076182544,
7.56004874999027));
#388742=CARTESIAN_POINT('Ctrl Pts',(2.62685870940684,-0.589440182330275,
7.55786368756705));
#388743=CARTESIAN_POINT('Ctrl Pts',(2.66247619935189,-0.570802909462089,
7.5388891333356));
#388744=CARTESIAN_POINT('Ctrl Pts',(2.6568764439911,-0.572376974939164,
7.53222002137279));
#388745=CARTESIAN_POINT('Ctrl Pts',(2.65722369629234,-0.580949131059928,
7.53005029815326));
#388746=CARTESIAN_POINT('Ctrl Pts',(2.69279345069543,-0.562280869547134,
7.51101258149734));
#388747=CARTESIAN_POINT('Ctrl Pts',(2.68712581612466,-0.563874015557904,
7.5043616886572));
#388748=CARTESIAN_POINT('Ctrl Pts',(2.68753116066568,-0.572473037441103,
7.50217374673251));
#388749=CARTESIAN_POINT('',(2.68591391515804,-0.572925331695027,7.50366116523517));
#388750=CARTESIAN_POINT('Ctrl Pts',(2.68453419038077,-0.564602509634882,
7.51860402984325));
#388751=CARTESIAN_POINT('Ctrl Pts',(2.6849593249586,-0.564483006260371,
7.51734760759493));
#388752=CARTESIAN_POINT('Ctrl Pts',(2.68535959513189,-0.564432294838141,
7.51608817408573));
#388753=CARTESIAN_POINT('Ctrl Pts',(2.68573575866036,-0.564463739753546,
7.5148100591312));
#388754=CARTESIAN_POINT('Ctrl Pts',(2.68607649657317,-0.564492223309321,
7.51365231206384));
#388755=CARTESIAN_POINT('Ctrl Pts',(2.68639795571402,-0.564587908381932,
7.51247773061043));
#388756=CARTESIAN_POINT('Ctrl Pts',(2.68668403940181,-0.564784529772823,
7.51129758471022));
#388757=CARTESIAN_POINT('Ctrl Pts',(2.68703960875373,-0.565028907706691,
7.50983079813402));
#388758=CARTESIAN_POINT('Ctrl Pts',(2.68732180620472,-0.56543214320763,
7.50839324291155));
#388759=CARTESIAN_POINT('Ctrl Pts',(2.68746514888008,-0.566044447664703,
7.50715379678855));
#388760=CARTESIAN_POINT('Ctrl Pts',(2.68753136906577,-0.566327314680742,
7.50658120839351));
#388761=CARTESIAN_POINT('Ctrl Pts',(2.68756811743797,-0.566697178583436,
7.50598221009429));
#388762=CARTESIAN_POINT('Ctrl Pts',(2.68755188439479,-0.567147486072437,
7.50545747549611));
#388763=CARTESIAN_POINT('Ctrl Pts',(2.68754322194049,-0.567387784086888,
7.50517746087247));
#388764=CARTESIAN_POINT('Ctrl Pts',(2.68751958082918,-0.567653602361198,
7.50491486231392));
#388765=CARTESIAN_POINT('Ctrl Pts',(2.68747992565903,-0.567937753814264,
7.50468370960993));
#388766=CARTESIAN_POINT('Ctrl Pts',(2.68742062867114,-0.568362649867092,
7.50433806340447));
#388767=CARTESIAN_POINT('Ctrl Pts',(2.68732319532928,-0.568841202404014,
7.50405484070984));
#388768=CARTESIAN_POINT('Ctrl Pts',(2.68719348559491,-0.569341038875649,
7.50385766036131));
#388769=CARTESIAN_POINT('Ctrl Pts',(2.68717961515497,-0.569394488617071,
7.50383657498791));
#388770=CARTESIAN_POINT('Ctrl Pts',(2.68716539573022,-0.569448161724747,
7.50381643264937));
#388771=CARTESIAN_POINT('Ctrl Pts',(2.68715084931172,-0.569502004300505,
7.50379723213559));
#388772=CARTESIAN_POINT('Ctrl Pts',(2.68705374720979,-0.569861421106833,
7.50366906242519));
#388773=CARTESIAN_POINT('Ctrl Pts',(2.68693926790965,-0.570236020019771,
7.50358235568538));
#388774=CARTESIAN_POINT('Ctrl Pts',(2.68682024464033,-0.570594434827216,
7.5035341175365));
#388775=CARTESIAN_POINT('Ctrl Pts',(2.68664178271882,-0.571131837266257,
7.50346178989176));
#388776=CARTESIAN_POINT('Ctrl Pts',(2.68642694857157,-0.571702372004782,
7.50346967198527));
#388777=CARTESIAN_POINT('Ctrl Pts',(2.68619881406495,-0.572255970936448,
7.50354272648692));
#388778=CARTESIAN_POINT('Ctrl Pts',(2.68610497762027,-0.57248367763586,
7.50357277531559));
#388779=CARTESIAN_POINT('Ctrl Pts',(2.68600914673731,-0.572708270534058,
7.50361331098761));
#388780=CARTESIAN_POINT('Ctrl Pts',(2.68591391515943,-0.572925331695323,
7.50366116523658));
#388781=CARTESIAN_POINT('',(2.6069246899221,-0.595013548701457,7.57603338622103));
#388782=CARTESIAN_POINT('Origin',(2.61553943300004,-0.596982734143167,7.58486873427627));
#388783=CARTESIAN_POINT('Ctrl Pts',(2.68591391521158,-0.572925331674489,
7.50366116529968));
#388784=CARTESIAN_POINT('Ctrl Pts',(2.65962736327094,-0.580276861166546,
7.52783573079709));
#388785=CARTESIAN_POINT('Ctrl Pts',(2.63329886951445,-0.587639269794973,
7.55196141284068));
#388786=CARTESIAN_POINT('Ctrl Pts',(2.60692469098357,-0.595013548037431,
7.57603338728831));
#388787=CARTESIAN_POINT('Ctrl Pts',(2.6032473619073,-0.587634493602723,
7.59639677331372));
#388788=CARTESIAN_POINT('Ctrl Pts',(2.58509102396104,-0.589736708654588,
7.59959882295462));
#388789=CARTESIAN_POINT('Ctrl Pts',(2.60025825567991,-0.599967246010105,
7.59642833564546));
#388790=CARTESIAN_POINT('Ctrl Pts',(2.59935086420696,-0.587454466507662,
7.58707626057423));
#388791=CARTESIAN_POINT('Ctrl Pts',(2.59437047150332,-0.592048808631775,
7.58809943920598));
#388792=CARTESIAN_POINT('Ctrl Pts',(2.5967579751915,-0.598374488589822,
7.58710240504251));
#388793=CARTESIAN_POINT('Ctrl Pts',(2.6033867930582,-0.591997253160062,
7.58015376756929));
#388794=CARTESIAN_POINT('Ctrl Pts',(2.6010574740276,-0.593641498959718,
7.5820588065976));
#388795=CARTESIAN_POINT('Ctrl Pts',(2.60238830315171,-0.596122621463801,
7.58020924244129));
#388796=CARTESIAN_POINT('Ctrl Pts',(2.60692468911533,-0.595013548517107,
7.57603338509286));
#388797=CARTESIAN_POINT('Ctrl Pts',(2.60692468911533,-0.595013548517107,
7.57603338509286));
#388798=CARTESIAN_POINT('Ctrl Pts',(2.60692468911533,-0.595013548517107,
7.57603338509286));
#388799=CARTESIAN_POINT('Origin',(2.61554070278287,-0.596977170861152,7.58486873427624));
#388800=CARTESIAN_POINT('Ctrl Pts',(2.67010792806202,-0.661779669736821,
7.51098857897448));
#388801=CARTESIAN_POINT('Ctrl Pts',(2.66569278577231,-0.65788518253907,
7.50433767179956));
#388802=CARTESIAN_POINT('Ctrl Pts',(2.66978899405937,-0.650313582394355,
7.50214974420965));
#388803=CARTESIAN_POINT('Ctrl Pts',(2.64648381003428,-0.640941422817449,
7.53887321589167));
#388804=CARTESIAN_POINT('Ctrl Pts',(2.64212156898467,-0.637093598487795,
7.5322040745206));
#388805=CARTESIAN_POINT('Ctrl Pts',(2.64615375522351,-0.629520990346774,
7.53003438070911));
#388806=CARTESIAN_POINT('Ctrl Pts',(2.62281432498536,-0.620063158777086,
7.56669465659232));
#388807=CARTESIAN_POINT('Ctrl Pts',(2.61847786396932,-0.616238074373868,
7.560040858333));
#388808=CARTESIAN_POINT('Ctrl Pts',(2.62247315433322,-0.608689941821077,
7.55785582193789));
#388809=CARTESIAN_POINT('Ctrl Pts',(2.59910054339133,-0.599145821856049,
7.59443891967696));
#388810=CARTESIAN_POINT('Ctrl Pts',(2.59475779504673,-0.59531519155666,
7.58783901202978));
#388811=CARTESIAN_POINT('Ctrl Pts',(2.5987483062296,-0.587821527667229,
7.58560008491213));
#388812=CARTESIAN_POINT('',(2.66850780457432,-0.649186484966709,7.50366116523517));
#388813=CARTESIAN_POINT('Ctrl Pts',(2.66850780457468,-0.649186484966797,
7.50366116523554));
#388814=CARTESIAN_POINT('Ctrl Pts',(2.66848084963155,-0.649943723996302,
7.50350835821027));
#388815=CARTESIAN_POINT('Ctrl Pts',(2.66843143551488,-0.650638933501571,
7.50345484956));
#388816=CARTESIAN_POINT('Ctrl Pts',(2.66835869209321,-0.651292825201307,
7.50349758195598));
#388817=CARTESIAN_POINT('Ctrl Pts',(2.6683213693231,-0.651628320137145,
7.50351950684424));
#388818=CARTESIAN_POINT('Ctrl Pts',(2.66827435519656,-0.651986020405876,
7.50357029184312));
#388819=CARTESIAN_POINT('Ctrl Pts',(2.6682195386781,-0.652329700489952,
7.50365515313924));
#388820=CARTESIAN_POINT('Ctrl Pts',(2.6681352086753,-0.652858419629069,
7.50378570417639));
#388821=CARTESIAN_POINT('Ctrl Pts',(2.66803028020088,-0.653369532037473,
7.50400001621911));
#388822=CARTESIAN_POINT('Ctrl Pts',(2.66791051580347,-0.653823678057418,
7.50428903009635));
#388823=CARTESIAN_POINT('Ctrl Pts',(2.66789722287677,-0.653874084771641,
7.50432110841318));
#388824=CARTESIAN_POINT('Ctrl Pts',(2.66788375745731,-0.65392381822113,
7.50435406373355));
#388825=CARTESIAN_POINT('Ctrl Pts',(2.66787013472256,-0.653972845742071,
7.50438785222352));
#388826=CARTESIAN_POINT('Ctrl Pts',(2.66778696137898,-0.654272182323043,
7.50459414719561));
#388827=CARTESIAN_POINT('Ctrl Pts',(2.66769610268179,-0.654549831748733,
7.50483629897752));
#388828=CARTESIAN_POINT('Ctrl Pts',(2.66760229016465,-0.654795566654488,
7.5050991045531));
#388829=CARTESIAN_POINT('Ctrl Pts',(2.66739533032926,-0.655337682538318,
7.50567888004914));
#388830=CARTESIAN_POINT('Ctrl Pts',(2.66716632527347,-0.655746022335905,
7.50637912803144));
#388831=CARTESIAN_POINT('Ctrl Pts',(2.66693735246779,-0.656042219439331,
7.50710440483569));
#388832=CARTESIAN_POINT('Ctrl Pts',(2.66688120379009,-0.656114852849427,
7.50728225710685));
#388833=CARTESIAN_POINT('Ctrl Pts',(2.66682405477194,-0.656182277981084,
7.50746498566954));
#388834=CARTESIAN_POINT('Ctrl Pts',(2.6667675572524,-0.656243190274951,
7.50764697238949));
#388835=CARTESIAN_POINT('Ctrl Pts',(2.66646384213587,-0.65657063800326,
7.50862528291182));
#388836=CARTESIAN_POINT('Ctrl Pts',(2.6661544183869,-0.656742414642496,
7.50965856837422));
#388837=CARTESIAN_POINT('Ctrl Pts',(2.66585470570012,-0.656822999870543,
7.51067959873202));
#388838=CARTESIAN_POINT('Ctrl Pts',(2.66568977343055,-0.656867346023182,
7.51124147302578));
#388839=CARTESIAN_POINT('Ctrl Pts',(2.66552762893009,-0.656883667859983,
7.51180065547253));
#388840=CARTESIAN_POINT('Ctrl Pts',(2.66537023285753,-0.656880063981605,
7.512351757165));
#388841=CARTESIAN_POINT('Ctrl Pts',(2.66482636672769,-0.656867611146191,
7.51425603304535));
#388842=CARTESIAN_POINT('Ctrl Pts',(2.66427448875531,-0.656609701993072,
7.51626900505179));
#388843=CARTESIAN_POINT('Ctrl Pts',(2.66374017842016,-0.656161002394689,
7.51827788969243));
#388844=CARTESIAN_POINT('Ctrl Pts',(2.66371126053511,-0.656136717924499,
7.51838661432545));
#388845=CARTESIAN_POINT('Ctrl Pts',(2.66368239262177,-0.656111864744666,
7.51849533314856));
#388846=CARTESIAN_POINT('Ctrl Pts',(2.66365357834825,-0.65608644839068,
7.51860402984325));
#388847=CARTESIAN_POINT('Ctrl Pts',(2.60692469059145,-0.595013549760779,
7.57603338728985));
#388848=CARTESIAN_POINT('Ctrl Pts',(2.62748742495179,-0.613100872081639,
7.55196141284922));
#388849=CARTESIAN_POINT('Ctrl Pts',(2.6480141487976,-0.631157678379778,
7.52783573083104));
#388850=CARTESIAN_POINT('Ctrl Pts',(2.66850780461497,-0.649186485009713,
7.50366116530176));
#388851=CARTESIAN_POINT('Origin',(9.00812987045925E-16,-2.05604685939121E-16,
7.49482233047033));
#388852=CARTESIAN_POINT('Origin',(2.67726955234741,-0.571081425081853,7.49482233047033));
#388853=CARTESIAN_POINT('Origin',(0.,0.,7.50366116523517));
#388854=CARTESIAN_POINT('Origin',(2.65991946170317,-0.647097138961931,7.49482233047033));
#388855=CARTESIAN_POINT('Ctrl Pts',(2.68453317211224,-0.564602795819,7.51860402984325));
#388856=CARTESIAN_POINT('Ctrl Pts',(2.69185841476393,-0.562544372605989,
7.51860402984325));
#388857=CARTESIAN_POINT('Ctrl Pts',(2.69339429606666,-0.555092033734601,
7.51860402984325));
#388858=CARTESIAN_POINT('Ctrl Pts',(2.68725308435511,-0.563838488009249,
7.51041458714365));
#388859=CARTESIAN_POINT('Ctrl Pts',(2.69222227294058,-0.560778826171352,
7.51004642900443));
#388860=CARTESIAN_POINT('Ctrl Pts',(2.69339471964448,-0.555089978468018,
7.5072913648301));
#388861=CARTESIAN_POINT('Ctrl Pts',(2.68890269145811,-0.566119394321436,
7.50215815450138));
#388862=CARTESIAN_POINT('Ctrl Pts',(2.69148155889366,-0.564373683225253,
7.49877163671529));
#388863=CARTESIAN_POINT('Ctrl Pts',(2.69220133684272,-0.560999391699851,
7.49481588533171));
#388864=CARTESIAN_POINT('Ctrl Pts',(2.68591337675242,-0.572925216849604,
7.50366171572174));
#388865=CARTESIAN_POINT('Ctrl Pts',(2.6894945274722,-0.573689102822331,
7.50000045605858));
#388866=CARTESIAN_POINT('Ctrl Pts',(2.68949452747223,-0.57368910282221,
7.49482233047317));
#388867=CARTESIAN_POINT('Origin',(2.6811515947209,-0.552568888126717,7.51860402984325));
#388868=CARTESIAN_POINT('Origin',(2.6811515947209,-0.552568888126717,9.));
#388869=CARTESIAN_POINT('Origin',(2.6811515947209,-0.552568888126717,8.75721825406948));
#388870=CARTESIAN_POINT('Ctrl Pts',(2.66845710877349,-0.569121671950379,
8.78942910404912));
#388871=CARTESIAN_POINT('Ctrl Pts',(2.67382710225269,-0.567633183208407,
8.7967269950169));
#388872=CARTESIAN_POINT('Ctrl Pts',(2.67306298249164,-0.558739949433627,
8.79893251111267));
#388873=CARTESIAN_POINT('Ctrl Pts',(2.67904124401792,-0.566146524917328,
8.78111911759582));
#388874=CARTESIAN_POINT('Ctrl Pts',(2.68540544515353,-0.564374730902475,
8.78644465894816));
#388875=CARTESIAN_POINT('Ctrl Pts',(2.68645982044843,-0.556337081711761,
8.78817647674132));
#388876=CARTESIAN_POINT('Ctrl Pts',(2.68563752954907,-0.564292342291746,
8.76780923932029));
#388877=CARTESIAN_POINT('Ctrl Pts',(2.69314883357549,-0.562195905172935,
8.76988516158372));
#388878=CARTESIAN_POINT('Ctrl Pts',(2.69482528285461,-0.554825294736144,
8.77093053738833));
#388879=CARTESIAN_POINT('Ctrl Pts',(2.68435134414655,-0.564653882525788,
8.75371302330492));
#388880=CARTESIAN_POINT('Ctrl Pts',(2.69167850214931,-0.562609632792947,
8.75300828287559));
#388881=CARTESIAN_POINT('Ctrl Pts',(2.69319359655887,-0.555119704337719,
8.75267964240738));
#388882=CARTESIAN_POINT('Origin',(2.66765220000866,-0.556363505892747,8.78727029226991));
#388883=CARTESIAN_POINT('Ctrl Pts',(2.60220974632392,-0.587743532225588,
8.85049129520029));
#388884=CARTESIAN_POINT('Ctrl Pts',(2.60783148438852,-0.58616328751161,
8.85711686593484));
#388885=CARTESIAN_POINT('Ctrl Pts',(2.60745677570887,-0.577621604099115,
8.85933012996512));
#388886=CARTESIAN_POINT('Ctrl Pts',(2.62518480823033,-0.58128534799258,
8.82945683644723));
#388887=CARTESIAN_POINT('Ctrl Pts',(2.63085321011983,-0.57969198629205,
8.8360746990239));
#388888=CARTESIAN_POINT('Ctrl Pts',(2.63043993491586,-0.571126868306674,
8.8382956714852));
#388889=CARTESIAN_POINT('Ctrl Pts',(2.64812562395425,-0.574836790203962,
8.80838214965002));
#388890=CARTESIAN_POINT('Ctrl Pts',(2.65381639600414,-0.573237140354229,
8.81501364461987));
#388891=CARTESIAN_POINT('Ctrl Pts',(2.65338841166109,-0.564642628035467,
8.81722098428721));
#388892=CARTESIAN_POINT('Ctrl Pts',(2.67103479566854,-0.568397127400913,
8.78727029226991));
#388893=CARTESIAN_POINT('Ctrl Pts',(2.67672651297436,-0.566797211844082,
8.79393457792714));
#388894=CARTESIAN_POINT('Ctrl Pts',(2.67630485569207,-0.558168097155164,
8.79610912703474));
#388895=CARTESIAN_POINT('Origin',(2.59882715066404,-0.575709910717423,8.85049129520029));
#388896=CARTESIAN_POINT('Ctrl Pts',(2.59952233059431,-0.599517869856861,
8.85049129520029));
#388897=CARTESIAN_POINT('Ctrl Pts',(2.6039016990888,-0.603380801879633,
8.85711686593484));
#388898=CARTESIAN_POINT('Ctrl Pts',(2.59985800069653,-0.610914012710764,
8.85933012996512));
#388899=CARTESIAN_POINT('Ctrl Pts',(2.59564796650409,-0.596100389658331,
8.86332496987232));
#388900=CARTESIAN_POINT('Ctrl Pts',(2.59489685997457,-0.600659746340801,
8.86648636486738));
#388901=CARTESIAN_POINT('Ctrl Pts',(2.58903064249949,-0.601340624030181,
8.87206031107456));
#388902=CARTESIAN_POINT('Ctrl Pts',(2.59720247950873,-0.589151051897485,
8.86341338519876));
#388903=CARTESIAN_POINT('Ctrl Pts',(2.59847925223829,-0.584696467513797,
8.86654584966059));
#388904=CARTESIAN_POINT('Ctrl Pts',(2.59344014932518,-0.58157691712656,
8.87215952290715));
#388905=CARTESIAN_POINT('Ctrl Pts',(2.60220974632392,-0.587743532225589,
8.85049129520029));
#388906=CARTESIAN_POINT('Ctrl Pts',(2.60783148438852,-0.58616328751161,
8.85711686593484));
#388907=CARTESIAN_POINT('Ctrl Pts',(2.60745677570887,-0.577621604099115,
8.85933012996512));
#388908=CARTESIAN_POINT('Origin',(2.59125352451697,-0.608892134951009,8.85049129520029));
#388909=CARTESIAN_POINT('Ctrl Pts',(2.65313746692185,-0.646810448064325,
8.78727029226991));
#388910=CARTESIAN_POINT('Ctrl Pts',(2.65757134967523,-0.650721465758954,
8.79393457792714));
#388911=CARTESIAN_POINT('Ctrl Pts',(2.65344741704446,-0.658313079212961,
8.79610912703474));
#388912=CARTESIAN_POINT('Ctrl Pts',(2.63529108139351,-0.63106859527552,
8.80838214965003));
#388913=CARTESIAN_POINT('Ctrl Pts',(2.63972422778674,-0.634978963445167,
8.81501364461996));
#388914=CARTESIAN_POINT('Ctrl Pts',(2.63560960807689,-0.642536656032114,
8.81722098428721));
#388915=CARTESIAN_POINT('Ctrl Pts',(2.61742004498719,-0.615304998560392,
8.82945683644724));
#388916=CARTESIAN_POINT('Ctrl Pts',(2.62183576488801,-0.619199995254531,
8.83607469902391));
#388917=CARTESIAN_POINT('Ctrl Pts',(2.61774715137787,-0.626737586518466,
8.8382956714852));
#388918=CARTESIAN_POINT('Ctrl Pts',(2.59952233059431,-0.599517869856861,
8.85049129520029));
#388919=CARTESIAN_POINT('Ctrl Pts',(2.6039016990888,-0.603380801879633,
8.85711686593484));
#388920=CARTESIAN_POINT('Ctrl Pts',(2.59985800069653,-0.610914012710764,
8.85933012996512));
#388921=CARTESIAN_POINT('Origin',(2.64486866084451,-0.656184713158474,8.78727029226991));
#388922=CARTESIAN_POINT('Ctrl Pts',(2.66351470618409,-0.655963977306794,
8.75374538247849));
#388923=CARTESIAN_POINT('Ctrl Pts',(2.66922216072437,-0.660980882832925,
8.75304829418602));
#388924=CARTESIAN_POINT('Ctrl Pts',(2.66734493414156,-0.668379981667633,
8.75272238421917));
#388925=CARTESIAN_POINT('Ctrl Pts',(2.66450461662079,-0.656837152112578,
8.76769408445016));
#388926=CARTESIAN_POINT('Ctrl Pts',(2.6703552404268,-0.661980823569088,
8.76974318093967));
#388927=CARTESIAN_POINT('Ctrl Pts',(2.66867262963315,-0.669342017643224,
8.7707786988043));
#388928=CARTESIAN_POINT('Ctrl Pts',(2.65943089964688,-0.652361755461981,
8.78108014887994));
#388929=CARTESIAN_POINT('Ctrl Pts',(2.6643916012075,-0.656717978289939,
8.78639403366328));
#388930=CARTESIAN_POINT('Ctrl Pts',(2.66187669989166,-0.664411959515576,
8.78812224174741));
#388931=CARTESIAN_POINT('Ctrl Pts',(2.65111619753791,-0.645027568331975,
8.78944554828685));
#388932=CARTESIAN_POINT('Ctrl Pts',(2.65530058650937,-0.648694625265325,
8.79673892988685));
#388933=CARTESIAN_POINT('Ctrl Pts',(2.65076059570257,-0.656368740054055,
8.79894799272499));
#388934=CARTESIAN_POINT('Origin',(2.65538477227092,-0.665460713484825,8.75721825406948));
#388935=CARTESIAN_POINT('Origin',(2.65538477227092,-0.665460713484825,9.));
#388936=CARTESIAN_POINT('Origin',(2.65538477227092,-0.665460713484825,7.51860402984325));
#388937=CARTESIAN_POINT('Ctrl Pts',(2.66850704020454,-0.649186299013206,
7.50366195182966));
#388938=CARTESIAN_POINT('Ctrl Pts',(2.67206521266982,-0.650051920418514,
7.50000065167735));
#388939=CARTESIAN_POINT('Ctrl Pts',(2.67206521266979,-0.650051920418627,
7.49482233047108));
#388940=CARTESIAN_POINT('Ctrl Pts',(2.6682462613492,-0.656621740761695,
7.50215800491337));
#388941=CARTESIAN_POINT('Ctrl Pts',(2.66981166961859,-0.659315101882027,
7.49877273257266));
#388942=CARTESIAN_POINT('Ctrl Pts',(2.66899567098828,-0.662669398020607,
7.49481816995647));
#388943=CARTESIAN_POINT('Ctrl Pts',(2.66576757595735,-0.657950700907921,
7.51043025814041));
#388944=CARTESIAN_POINT('Ctrl Pts',(2.66892202800129,-0.662864171096018,
7.51006209594513));
#388945=CARTESIAN_POINT('Ctrl Pts',(2.6675092014202,-0.668501802798599,
7.50731281821699));
#388946=CARTESIAN_POINT('Ctrl Pts',(2.66365244482109,-0.656085448656407,
7.51860402984325));
#388947=CARTESIAN_POINT('Ctrl Pts',(2.66935955988638,-0.661118326066217,
7.51860402984324));
#388948=CARTESIAN_POINT('Ctrl Pts',(2.66750981689316,-0.668499346879738,
7.51860402984325));
#388949=CARTESIAN_POINT('Origin',(0.,0.,7.5));
#388950=CARTESIAN_POINT('Origin',(2.55577009136411,-0.764838063661105,7.5));
#388951=CARTESIAN_POINT('',(2.55577009136411,-0.764838063661105,7.59394543036555));
#388952=CARTESIAN_POINT('',(2.55577009136411,-0.764838063661105,8.85049129520029));
#388953=CARTESIAN_POINT('',(2.55577009136411,-0.764838063661105,7.5));
#388954=CARTESIAN_POINT('',(2.60624502375466,-0.81546860777333,8.78727029226991));
#388955=CARTESIAN_POINT('Ctrl Pts',(2.55577009136411,-0.764838063661105,
8.85049129520029));
#388956=CARTESIAN_POINT('Ctrl Pts',(2.57261952556178,-0.78173944383157,
8.82945686509571));
#388957=CARTESIAN_POINT('Ctrl Pts',(2.58944391103811,-0.798615698056724,
8.80838212259895));
#388958=CARTESIAN_POINT('Ctrl Pts',(2.60624502375466,-0.81546860777333,
8.78727029226991));
#388959=CARTESIAN_POINT('',(2.61614521332083,-0.825399319134594,8.75721825406948));
#388960=CARTESIAN_POINT('Origin',(2.58635225143055,-0.795514221183445,8.75937679713058));
#388961=CARTESIAN_POINT('',(2.61614521332083,-0.825399319134594,7.51860402984325));
#388962=CARTESIAN_POINT('',(2.61614521332083,-0.825399319134594,7.5));
#388963=CARTESIAN_POINT('Ctrl Pts',(2.61614521332084,-0.825399319134594,
7.51860402984325));
#388964=CARTESIAN_POINT('Ctrl Pts',(2.60837015418733,-0.817600289878085,
7.52834476460825));
#388965=CARTESIAN_POINT('Ctrl Pts',(2.60059004759763,-0.809796197604318,
7.53807742314407));
#388966=CARTESIAN_POINT('Ctrl Pts',(2.59280472407668,-0.801986872315757,
7.54780169004674));
#388967=CARTESIAN_POINT('Ctrl Pts',(2.58047319238032,-0.789617323116697,
7.5632044032688));
#388968=CARTESIAN_POINT('Ctrl Pts',(2.56812855639631,-0.777234629230145,
7.57858609112103));
#388969=CARTESIAN_POINT('Ctrl Pts',(2.55577009136411,-0.764838063661105,
7.59394543036555));
#388970=CARTESIAN_POINT('Origin',(2.82817002729664,-0.695957823489667,7.5));
#388971=CARTESIAN_POINT('',(2.64284431997728,-0.735441169348851,8.75721825406948));
#388972=CARTESIAN_POINT('',(2.62912953922427,-0.73836308147689,8.78727029226991));
#388973=CARTESIAN_POINT('Origin',(2.59431631031598,-0.745779984276522,8.75658640621069));
#388974=CARTESIAN_POINT('',(2.55920636991204,-0.753260100986265,8.85049129520029));
#388975=CARTESIAN_POINT('Ctrl Pts',(2.62912953922427,-0.73836308147689,
8.78727029226991));
#388976=CARTESIAN_POINT('Ctrl Pts',(2.60585487607023,-0.743321711277145,
8.80838212259895));
#388977=CARTESIAN_POINT('Ctrl Pts',(2.58254797304888,-0.748287209729622,
8.82945686509571));
#388978=CARTESIAN_POINT('Ctrl Pts',(2.55920636991204,-0.753260100986265,
8.85049129520029));
#388979=CARTESIAN_POINT('',(2.55920636991204,-0.753260100986265,7.59394543036555));
#388980=CARTESIAN_POINT('',(2.55920636991204,-0.753260100986265,7.5));
#388981=CARTESIAN_POINT('',(2.64284431997728,-0.735441169348851,7.51860402984325));
#388982=CARTESIAN_POINT('Ctrl Pts',(2.55920636991204,-0.753260100986265,
7.59394543036555));
#388983=CARTESIAN_POINT('Ctrl Pts',(2.5763266116233,-0.749612660841797,
7.57858609112103));
#388984=CARTESIAN_POINT('Ctrl Pts',(2.59342769588663,-0.74596930216102,
7.56320440326857));
#388985=CARTESIAN_POINT('Ctrl Pts',(2.61051062671677,-0.742329811040161,
7.54780169004651));
#388986=CARTESIAN_POINT('Ctrl Pts',(2.62129567325224,-0.740032074106483,
7.53807742314383));
#388987=CARTESIAN_POINT('Ctrl Pts',(2.63207349274766,-0.737735876882134,
7.52834476460825));
#388988=CARTESIAN_POINT('Ctrl Pts',(2.64284431997728,-0.735441169348852,
7.51860402984325));
#388989=CARTESIAN_POINT('',(2.64284431997728,-0.735441169348851,7.5));
#388990=CARTESIAN_POINT('Origin',(2.56063892684945,-0.75998419242088,7.5));
#388991=CARTESIAN_POINT('Ctrl Pts',(2.55920636991204,-0.753260100986265,
8.85049129520029));
#388992=CARTESIAN_POINT('Ctrl Pts',(2.5590169593414,-0.753300454605728,
8.85097269580138));
#388993=CARTESIAN_POINT('Ctrl Pts',(2.5588316912378,-0.753348525868738,
8.85143669361005));
#388994=CARTESIAN_POINT('Ctrl Pts',(2.55864225418249,-0.753407374564256,
8.8519052845931));
#388995=CARTESIAN_POINT('Ctrl Pts',(2.55827172731595,-0.753522478880641,
8.85282181883899));
#388996=CARTESIAN_POINT('Ctrl Pts',(2.55789484136048,-0.753676041269533,
8.85372622499636));
#388997=CARTESIAN_POINT('Ctrl Pts',(2.55751150029902,-0.753884750349128,
8.85462257735071));
#388998=CARTESIAN_POINT('Ctrl Pts',(2.55719326416478,-0.754058013214361,
8.85536669723986));
#388999=CARTESIAN_POINT('Ctrl Pts',(2.55687049166869,-0.754269293443448,
8.85610498449051));
#389000=CARTESIAN_POINT('Ctrl Pts',(2.55654748330547,-0.754534852746846,
8.85681338218371));
#389001=CARTESIAN_POINT('Ctrl Pts',(2.55625435270854,-0.754775848231751,
8.85745625420285));
#389002=CARTESIAN_POINT('Ctrl Pts',(2.55595697075632,-0.755064106475223,
8.85808743050666));
#389003=CARTESIAN_POINT('Ctrl Pts',(2.55566442701757,-0.755426742526368,
8.85866804508411));
#389004=CARTESIAN_POINT('Ctrl Pts',(2.55552945367809,-0.755594054939378,
8.85893592806396));
#389005=CARTESIAN_POINT('Ctrl Pts',(2.55539561415247,-0.755777419117943,
8.85919241173848));
#389006=CARTESIAN_POINT('Ctrl Pts',(2.5552646800958,-0.755980830461269,
8.85943017985534));
#389007=CARTESIAN_POINT('Ctrl Pts',(2.55508788035868,-0.756255495990965,
8.8597512372));
#389008=CARTESIAN_POINT('Ctrl Pts',(2.55491241676132,-0.756574051157839,
8.86004599534705));
#389009=CARTESIAN_POINT('Ctrl Pts',(2.55474952017824,-0.756937693547188,
8.86026130871721));
#389010=CARTESIAN_POINT('Ctrl Pts',(2.55468987914664,-0.757070833278094,
8.86034014101235));
#389011=CARTESIAN_POINT('Ctrl Pts',(2.55463101560014,-0.7572120118099,8.86040910639693));
#389012=CARTESIAN_POINT('Ctrl Pts',(2.55457484371587,-0.757357512262553,
8.86046313645507));
#389013=CARTESIAN_POINT('Ctrl Pts',(2.55448718796089,-0.757584564500361,
8.8605474499083));
#389014=CARTESIAN_POINT('Ctrl Pts',(2.55440383119924,-0.757828391994643,
8.86059655985668));
#389015=CARTESIAN_POINT('Ctrl Pts',(2.5543298421479,-0.758073262578114,
8.86059725258816));
#389016=CARTESIAN_POINT('Ctrl Pts',(2.55425568215229,-0.758318698910459,
8.86059794692011));
#389017=CARTESIAN_POINT('Ctrl Pts',(2.55419265397135,-0.758568673518972,
8.86056369958366));
#389018=CARTESIAN_POINT('Ctrl Pts',(2.55414054629406,-0.758808632639955,
8.86048590497774));
#389019=CARTESIAN_POINT('Ctrl Pts',(2.55412694774172,-0.758871254826088,
8.86046560290182));
#389020=CARTESIAN_POINT('Ctrl Pts',(2.55411400454188,-0.758934028803215,
8.86044257503091));
#389021=CARTESIAN_POINT('Ctrl Pts',(2.55410208450022,-0.758995008174577,
8.86041778462583));
#389022=CARTESIAN_POINT('Ctrl Pts',(2.5540218774114,-0.759405323674745,
8.86025097596201));
#389023=CARTESIAN_POINT('Ctrl Pts',(2.55397755802796,-0.759789508818218,
8.8599848982295));
#389024=CARTESIAN_POINT('Ctrl Pts',(2.55396200324607,-0.760135379307695,
8.85968173251461));
#389025=CARTESIAN_POINT('Ctrl Pts',(2.55395377565762,-0.760318324980611,
8.85952137522076));
#389026=CARTESIAN_POINT('Ctrl Pts',(2.5539532464807,-0.760494068796009,
8.85934740853961));
#389027=CARTESIAN_POINT('Ctrl Pts',(2.55395886863261,-0.760660127696761,
8.8591675900182));
#389028=CARTESIAN_POINT('Ctrl Pts',(2.55398144449489,-0.761326940498993,
8.85844552518694));
#389029=CARTESIAN_POINT('Ctrl Pts',(2.55410145860458,-0.761875378979886,
8.85759444184121));
#389030=CARTESIAN_POINT('Ctrl Pts',(2.55423947657395,-0.762313757008132,
8.85683498915135));
#389031=CARTESIAN_POINT('Ctrl Pts',(2.55425391978687,-0.762359632101284,
8.85675551444996));
#389032=CARTESIAN_POINT('Ctrl Pts',(2.55426857766555,-0.762404292305608,
8.8566769979365));
#389033=CARTESIAN_POINT('Ctrl Pts',(2.55428337034997,-0.762447740242545,
8.85659965593547));
#389034=CARTESIAN_POINT('Ctrl Pts',(2.55448304275915,-0.763034202712432,
8.85555568965886));
#389035=CARTESIAN_POINT('Ctrl Pts',(2.55475963710019,-0.763568992833538,
8.85434650606346));
#389036=CARTESIAN_POINT('Ctrl Pts',(2.55510900057033,-0.764057609326306,
8.85297329937117));
#389037=CARTESIAN_POINT('Ctrl Pts',(2.55530549623526,-0.764332426331648,
8.85220095427747));
#389038=CARTESIAN_POINT('Ctrl Pts',(2.55552534811616,-0.764592565881812,
8.85137579139183));
#389039=CARTESIAN_POINT('Ctrl Pts',(2.55577009136411,-0.764838063661105,
8.85049129520029));
#389040=CARTESIAN_POINT('Origin',(2.56063892684945,-0.75998419242088,7.59394543036555));
#389041=CARTESIAN_POINT('Ctrl Pts',(2.55865644712842,-0.753377261156732,
7.59443877723642));
#389042=CARTESIAN_POINT('Ctrl Pts',(2.55299277157866,-0.75458389818405,
7.58783886950016));
#389043=CARTESIAN_POINT('Ctrl Pts',(2.55279250630485,-0.763071481783448,
7.58559994247159));
#389044=CARTESIAN_POINT('Ctrl Pts',(2.5895742857894,-0.746790265025826,
7.56670252222135));
#389045=CARTESIAN_POINT('Ctrl Pts',(2.58391879585876,-0.747995158120077,
7.56004874999028));
#389046=CARTESIAN_POINT('Ctrl Pts',(2.58369598431129,-0.756532529628371,
7.55786368756704));
#389047=CARTESIAN_POINT('Ctrl Pts',(2.62043438847577,-0.740215569452069,
7.5388891333356));
#389048=CARTESIAN_POINT('Ctrl Pts',(2.61474528769158,-0.741427623284978,
7.5322200213728));
#389049=CARTESIAN_POINT('Ctrl Pts',(2.61454260659734,-0.750004415522975,
7.53005029815327));
#389050=CARTESIAN_POINT('Ctrl Pts',(2.65123535874696,-0.733653471944896,
7.51101258149734));
#389051=CARTESIAN_POINT('Ctrl Pts',(2.64547729572389,-0.734880218072603,
7.5043616886572));
#389052=CARTESIAN_POINT('Ctrl Pts',(2.6453308662174,-0.743487542857012,
7.50217374673251));
#389053=CARTESIAN_POINT('',(2.64368796492176,-0.743835290548446,7.50366116523517));
#389054=CARTESIAN_POINT('Ctrl Pts',(2.64284431997728,-0.735441169348851,
7.51860402984325));
#389055=CARTESIAN_POINT('Ctrl Pts',(2.64327623767801,-0.735349149972762,
7.51734760759494));
#389056=CARTESIAN_POINT('Ctrl Pts',(2.64367893454528,-0.735324188140642,
7.51608817408573));
#389057=CARTESIAN_POINT('Ctrl Pts',(2.64405231052279,-0.735379669329115,
7.5148100591312));
#389058=CARTESIAN_POINT('Ctrl Pts',(2.64439052340533,-0.735429925515399,
7.51365231206384));
#389059=CARTESIAN_POINT('Ctrl Pts',(2.64470519151025,-0.735546009950635,
7.51247773061043));
#389060=CARTESIAN_POINT('Ctrl Pts',(2.64497808983265,-0.7357605568066,7.51129758471022));
#389061=CARTESIAN_POINT('Ctrl Pts',(2.64531727128122,-0.736027214046389,
7.50983079813402));
#389062=CARTESIAN_POINT('Ctrl Pts',(2.64557305354003,-0.736447701509509,
7.50839324291155));
#389063=CARTESIAN_POINT('Ctrl Pts',(2.64567687122123,-0.737067931918148,
7.50715379678855));
#389064=CARTESIAN_POINT('Ctrl Pts',(2.6457248319985,-0.73735446049543,7.50658120839351));
#389065=CARTESIAN_POINT('Ctrl Pts',(2.64573780760563,-0.737725918949358,
7.50598221009429));
#389066=CARTESIAN_POINT('Ctrl Pts',(2.64569275661509,-0.73817426117868,
7.50545747549611));
#389067=CARTESIAN_POINT('Ctrl Pts',(2.64566871601209,-0.738413510469735,
7.50517746087247));
#389068=CARTESIAN_POINT('Ctrl Pts',(2.64562809243867,-0.73867726790069,
7.50491486231392));
#389069=CARTESIAN_POINT('Ctrl Pts',(2.64557031309822,-0.738958294818646,
7.50468370960992));
#389070=CARTESIAN_POINT('Ctrl Pts',(2.64548391475877,-0.739378518705906,
7.50433806340446));
#389071=CARTESIAN_POINT('Ctrl Pts',(2.64535602063784,-0.739849845429672,
7.50405484070983));
#389072=CARTESIAN_POINT('Ctrl Pts',(2.64519455277334,-0.740340344402456,
7.50385766036131));
#389073=CARTESIAN_POINT('Ctrl Pts',(2.64517728629502,-0.740392795643512,
7.50383657498791));
#389074=CARTESIAN_POINT('Ctrl Pts',(2.64515965723779,-0.740445447432358,
7.50381643264937));
#389075=CARTESIAN_POINT('Ctrl Pts',(2.64514169100079,-0.740498247390535,
7.50379723213559));
#389076=CARTESIAN_POINT('Ctrl Pts',(2.64502176049169,-0.740850704383455,
7.50366906242519));
#389077=CARTESIAN_POINT('Ctrl Pts',(2.6448835157668,-0.741217198928807,
7.50358235568538));
#389078=CARTESIAN_POINT('Ctrl Pts',(2.644741773328,-0.741567251487542,7.5035341175365));
#389079=CARTESIAN_POINT('Ctrl Pts',(2.64452924658315,-0.742092115681066,
7.50346178989176));
#389080=CARTESIAN_POINT('Ctrl Pts',(2.6442782995495,-0.742647713723708,
7.50346967198527));
#389081=CARTESIAN_POINT('Ctrl Pts',(2.64401516456436,-0.74318555859897,
7.50354272648692));
#389082=CARTESIAN_POINT('Ctrl Pts',(2.64390693169839,-0.743406785328894,
7.50357277531559));
#389083=CARTESIAN_POINT('Ctrl Pts',(2.64379690799386,-0.743624776871144,
7.50361331098761));
#389084=CARTESIAN_POINT('Ctrl Pts',(2.64368796492313,-0.74383529054883,
7.50366116523659));
#389085=CARTESIAN_POINT('',(2.56344583459805,-0.76081726790711,7.57603338622103));
#389086=CARTESIAN_POINT('Origin',(2.57191671161794,-0.763334355930191,7.58486873427627));
#389087=CARTESIAN_POINT('Ctrl Pts',(2.64368796497651,-0.743835290531381,
7.50366116529969));
#389088=CARTESIAN_POINT('Ctrl Pts',(2.6169844074643,-0.749487530352269,
7.52783573079709));
#389089=CARTESIAN_POINT('Ctrl Pts',(2.59023829728154,-0.755147939735823,
7.55196141284068));
#389090=CARTESIAN_POINT('Ctrl Pts',(2.56344583569989,-0.760817267312457,
7.57603338728831));
#389091=CARTESIAN_POINT('Ctrl Pts',(2.5602488397315,-0.753217766653626,
7.59639677331372));
#389092=CARTESIAN_POINT('Ctrl Pts',(2.54199511654789,-0.754152381912878,
7.59959882295465));
#389093=CARTESIAN_POINT('Ctrl Pts',(2.5564757127837,-0.76533366740497,7.59642833564546));
#389094=CARTESIAN_POINT('Ctrl Pts',(2.55637188217916,-0.752788459978709,
7.58707626057422));
#389095=CARTESIAN_POINT('Ctrl Pts',(2.55110736171589,-0.757054267678081,
7.58809943920599));
#389096=CARTESIAN_POINT('Ctrl Pts',(2.55308467231526,-0.763519918734743,
7.58710240504252));
#389097=CARTESIAN_POINT('Ctrl Pts',(2.56010846144155,-0.757580495838072,
7.58015376756929));
#389098=CARTESIAN_POINT('Ctrl Pts',(2.55767858105665,-0.75907212337566,
7.5820588065976));
#389099=CARTESIAN_POINT('Ctrl Pts',(2.55884770978496,-0.761633414662241,
7.58020924244128));
#389100=CARTESIAN_POINT('Ctrl Pts',(2.56344583380475,-0.760817267671448,
7.57603338509286));
#389101=CARTESIAN_POINT('Ctrl Pts',(2.56344583380475,-0.760817267671448,
7.57603338509286));
#389102=CARTESIAN_POINT('Ctrl Pts',(2.56344583380475,-0.760817267671448,
7.57603338509286));
#389103=CARTESIAN_POINT('Origin',(2.57191833523284,-0.763328885433835,7.58486873427623));
#389104=CARTESIAN_POINT('Ctrl Pts',(2.62222153593684,-0.831494374752881,
7.51098857897448));
#389105=CARTESIAN_POINT('Ctrl Pts',(2.61806498568195,-0.827325010059011,
7.50433767179956));
#389106=CARTESIAN_POINT('Ctrl Pts',(2.62263789195665,-0.820031411544884,
7.50214974420965));
#389107=CARTESIAN_POINT('Ctrl Pts',(2.59998106725742,-0.809185339807828,
7.53887321589168));
#389108=CARTESIAN_POINT('Ctrl Pts',(2.59587431985113,-0.805065931502269,
7.53220407452063));
#389109=CARTESIAN_POINT('Ctrl Pts',(2.6003834002003,-0.797767225156165,
7.53003438070911));
#389110=CARTESIAN_POINT('Ctrl Pts',(2.57769788867394,-0.786833463286194,
7.56669465659233));
#389111=CARTESIAN_POINT('Ctrl Pts',(2.57361541138128,-0.782738399917892,
7.56004085833298));
#389112=CARTESIAN_POINT('Ctrl Pts',(2.57808610350575,-0.775461754945457,
7.5578558219379));
#389113=CARTESIAN_POINT('Ctrl Pts',(2.55537300796543,-0.764439756073933,
7.59443891967696));
#389114=CARTESIAN_POINT('Ctrl Pts',(2.55128461158901,-0.760338755373568,
7.58783901202978));
#389115=CARTESIAN_POINT('Ctrl Pts',(2.55574704453253,-0.753116160949613,
7.58560008491213));
#389116=CARTESIAN_POINT('',(2.62143154819293,-0.81882454376764,7.50366116523517));
#389117=CARTESIAN_POINT('Ctrl Pts',(2.62143154819329,-0.818824543767751,
7.50366116523554));
#389118=CARTESIAN_POINT('Ctrl Pts',(2.62135613216078,-0.81957849995932,
7.50350835821026));
#389119=CARTESIAN_POINT('Ctrl Pts',(2.62126227734477,-0.820269115108774,
7.50345484955999));
#389120=CARTESIAN_POINT('Ctrl Pts',(2.62114778839722,-0.820917002630855,
7.50349758195598));
#389121=CARTESIAN_POINT('Ctrl Pts',(2.6210890470764,-0.821249416978274,
7.50351950684424));
#389122=CARTESIAN_POINT('Ctrl Pts',(2.62101921161052,-0.821603370108011,
7.50357029184312));
#389123=CARTESIAN_POINT('Ctrl Pts',(2.62094248805989,-0.821942831958098,
7.50365515313924));
#389124=CARTESIAN_POINT('Ctrl Pts',(2.62082445617058,-0.822465061745213,
7.50378570417639));
#389125=CARTESIAN_POINT('Ctrl Pts',(2.62068699619852,-0.822968401227922,
7.50400001621911));
#389126=CARTESIAN_POINT('Ctrl Pts',(2.62053838063451,-0.823413940824877,
7.50428903009635));
#389127=CARTESIAN_POINT('Ctrl Pts',(2.62052188545028,-0.823463392292358,
7.50432110841318));
#389128=CARTESIAN_POINT('Ctrl Pts',(2.62050526126392,-0.823512160826751,
7.50435406373354));
#389129=CARTESIAN_POINT('Ctrl Pts',(2.62048852531449,-0.823560214803777,
7.50438785222352));
#389130=CARTESIAN_POINT('Ctrl Pts',(2.62038634429887,-0.82385360743122,
7.50459414719561));
#389131=CARTESIAN_POINT('Ctrl Pts',(2.62027788322084,-0.824124865059671,
7.50483629897752));
#389132=CARTESIAN_POINT('Ctrl Pts',(2.6201685191621,-0.824364084488096,
7.5050991045531));
#389133=CARTESIAN_POINT('Ctrl Pts',(2.61992725106396,-0.82489182657452,
7.50567888004914));
#389134=CARTESIAN_POINT('Ctrl Pts',(2.61967255410297,-0.825284654989899,
7.50637912803144));
#389135=CARTESIAN_POINT('Ctrl Pts',(2.6194250743329,-0.825565573186579,
7.50710440483569));
#389136=CARTESIAN_POINT('Ctrl Pts',(2.61936438738011,-0.825634459905412,
7.50728225710685));
#389137=CARTESIAN_POINT('Ctrl Pts',(2.61930303583774,-0.825698084954741,
7.50746498566954));
#389138=CARTESIAN_POINT('Ctrl Pts',(2.61924275173434,-0.825755252289261,
7.50764697238949));
#389139=CARTESIAN_POINT('Ctrl Pts',(2.6189186809851,-0.826062568146767,
7.50862528291182));
#389140=CARTESIAN_POINT('Ctrl Pts',(2.61859888721334,-0.826214167004811,
7.50965856837422));
#389141=CARTESIAN_POINT('Ctrl Pts',(2.61829462720514,-0.826275384004091,
7.51067959873202));
#389142=CARTESIAN_POINT('Ctrl Pts',(2.61812719253885,-0.82630907179601,
7.51124147302579));
#389143=CARTESIAN_POINT('Ctrl Pts',(2.61796433543799,-0.826314971464034,
7.51180065547253));
#389144=CARTESIAN_POINT('Ctrl Pts',(2.61780749365382,-0.826301290589217,
7.51235175716501));
#389145=CARTESIAN_POINT('Ctrl Pts',(2.61726554281117,-0.82625401771691,
7.51425603304535));
#389146=CARTESIAN_POINT('Ctrl Pts',(2.61673132302745,-0.825961279522712,
7.51626900505179));
#389147=CARTESIAN_POINT('Ctrl Pts',(2.61622685877216,-0.825479268445067,
7.51827788969242));
#389148=CARTESIAN_POINT('Ctrl Pts',(2.61619955621336,-0.825453181094669,
7.51838661432544));
#389149=CARTESIAN_POINT('Ctrl Pts',(2.61617233996095,-0.825426529404801,
7.51849533314856));
#389150=CARTESIAN_POINT('Ctrl Pts',(2.61614521332083,-0.825399319134597,
7.51860402984325));
#389151=CARTESIAN_POINT('Ctrl Pts',(2.56344583519815,-0.760817269007141,
7.57603338728985));
#389152=CARTESIAN_POINT('Ctrl Pts',(2.58280746249545,-0.780184887898307,
7.55196141284922));
#389153=CARTESIAN_POINT('Ctrl Pts',(2.60213510843395,-0.799519746263608,
7.52783573083105));
#389154=CARTESIAN_POINT('Ctrl Pts',(2.62143154823075,-0.818824543813161,
7.50366116530176));
#389155=CARTESIAN_POINT('Origin',(8.85789032694965E-16,-2.62897535302342E-16,
7.49482233047033));
#389156=CARTESIAN_POINT('Origin',(2.63517950238396,-0.741441326212297,7.49482233047033));
#389157=CARTESIAN_POINT('Origin',(0.,0.,7.50366116523517));
#389158=CARTESIAN_POINT('Origin',(2.61299471585146,-0.816189233531286,7.49482233047033));
#389159=CARTESIAN_POINT('Ctrl Pts',(2.642843285465,-0.735441389704284,7.51860402984325));
#389160=CARTESIAN_POINT('Ctrl Pts',(2.65028536124811,-0.733856525650637,
7.51860402984325));
#389161=CARTESIAN_POINT('Ctrl Pts',(2.65229555990884,-0.726517902661649,
7.51860402984325));
#389162=CARTESIAN_POINT('Ctrl Pts',(2.64560657872595,-0.734852917622631,
7.51041458714366));
#389163=CARTESIAN_POINT('Ctrl Pts',(2.65076159078755,-0.732117919193931,
7.51004642900443));
#389164=CARTESIAN_POINT('Ctrl Pts',(2.65229611429776,-0.726515878756562,
7.5072913648301));
#389165=CARTESIAN_POINT('Ctrl Pts',(2.64710665836508,-0.737234828258142,
7.50215815450137));
#389166=CARTESIAN_POINT('Ctrl Pts',(2.64979207533486,-0.735657932516524,
7.49877163671529));
#389167=CARTESIAN_POINT('Ctrl Pts',(2.65072656602324,-0.732336690166488,
7.4948158853317));
#389168=CARTESIAN_POINT('Ctrl Pts',(2.64368743498052,-0.743835141443218,
7.50366171572174));
#389169=CARTESIAN_POINT('Ctrl Pts',(2.64721228549976,-0.744826903044689,
7.50000045605858));
#389170=CARTESIAN_POINT('Ctrl Pts',(2.6472122854998,-0.744826903044569,
7.49482233047317));
#389171=CARTESIAN_POINT('Origin',(2.64023967100016,-0.723215548558642,7.51860402984325));
#389172=CARTESIAN_POINT('Origin',(2.64023967100016,-0.723215548558642,9.));
#389173=CARTESIAN_POINT('Origin',(2.64023967100016,-0.723215548558642,8.75721825406948));
#389174=CARTESIAN_POINT('Ctrl Pts',(2.62651072673474,-0.738920984405465,
8.78942910404912));
#389175=CARTESIAN_POINT('Ctrl Pts',(2.63196505478754,-0.737779610586762,
8.79672699501691));
#389176=CARTESIAN_POINT('Ctrl Pts',(2.63177229643678,-0.728855691593386,
8.79893251111267));
#389177=CARTESIAN_POINT('Ctrl Pts',(2.63726373406304,-0.736630078004493,
8.78111911759583));
#389178=CARTESIAN_POINT('Ctrl Pts',(2.64372837849715,-0.735269680097221,
8.78644465894813));
#389179=CARTESIAN_POINT('Ctrl Pts',(2.64529556141671,-0.727316099175898,
8.78817647674132));
#389180=CARTESIAN_POINT('Ctrl Pts',(2.64396526470683,-0.735202330461012,
8.76780923932029));
#389181=CARTESIAN_POINT('Ctrl Pts',(2.6515954551409,-0.73359145159842,8.76988516158375));
#389182=CARTESIAN_POINT('Ctrl Pts',(2.65374069660727,-0.726343395345369,
8.77093053738833));
#389183=CARTESIAN_POINT('Ctrl Pts',(2.64265855794783,-0.735480721690193,
8.75371302330492));
#389184=CARTESIAN_POINT('Ctrl Pts',(2.65010163704873,-0.733910124712743,
8.75300828287559));
#389185=CARTESIAN_POINT('Ctrl Pts',(2.65209349989809,-0.72653265755093,
8.75267964240738));
#389186=CARTESIAN_POINT('Origin',(2.62652489024715,-0.726137460686681,8.78727029226991));
#389187=CARTESIAN_POINT('Ctrl Pts',(2.55920636991204,-0.753260100986265,
8.85049129520029));
#389188=CARTESIAN_POINT('Ctrl Pts',(2.56491780413931,-0.752043289049005,
8.85711686593484));
#389189=CARTESIAN_POINT('Ctrl Pts',(2.56509113287407,-0.74349514777364,
8.85933012996512));
#389190=CARTESIAN_POINT('Ctrl Pts',(2.58254800437418,-0.748287203055817,
8.82945683644722));
#389191=CARTESIAN_POINT('Ctrl Pts',(2.58830684695874,-0.747060290843777,
8.83607469902391));
#389192=CARTESIAN_POINT('Ctrl Pts',(2.58844318986648,-0.738486292178674,
8.83829567148519));
#389193=CARTESIAN_POINT('Ctrl Pts',(2.60585484624788,-0.743321717630749,
8.80838214965002));
#389194=CARTESIAN_POINT('Ctrl Pts',(2.61163641591406,-0.742089963450265,
8.81501364461993));
#389195=CARTESIAN_POINT('Ctrl Pts',(2.61175996320559,-0.73348568842784,
8.81722098428721));
#389196=CARTESIAN_POINT('Ctrl Pts',(2.62912953922427,-0.73836308147689,
8.78727029226991));
#389197=CARTESIAN_POINT('Ctrl Pts',(2.63491206922813,-0.737131122698014,
8.79393457792714));
#389198=CARTESIAN_POINT('Ctrl Pts',(2.63504414756231,-0.728492721775861,
8.79610912703474));
#389199=CARTESIAN_POINT('Origin',(2.55660172093492,-0.741034480196056,8.85049129520029));
#389200=CARTESIAN_POINT('Ctrl Pts',(2.55577009136411,-0.764838063661105,
8.85049129520029));
#389201=CARTESIAN_POINT('Ctrl Pts',(2.55989296307188,-0.768973645978557,
8.85711686593484));
#389202=CARTESIAN_POINT('Ctrl Pts',(2.55537491841653,-0.776232298374573,
8.85933012996512));
#389203=CARTESIAN_POINT('Ctrl Pts',(2.55212264627854,-0.761179373682616,
8.86332496987233));
#389204=CARTESIAN_POINT('Ctrl Pts',(2.55108096399232,-0.765681239117223,
8.86648636486738));
#389205=CARTESIAN_POINT('Ctrl Pts',(2.54518317530685,-0.76598486802628,
8.87206031107457));
#389206=CARTESIAN_POINT('Ctrl Pts',(2.55411921096855,-0.754343912071688,
8.86341338519876));
#389207=CARTESIAN_POINT('Ctrl Pts',(2.55567876663298,-0.749980283219023,
8.86654584966059));
#389208=CARTESIAN_POINT('Ctrl Pts',(2.55084988737681,-0.746544285850476,
8.87215952290714));
#389209=CARTESIAN_POINT('Ctrl Pts',(2.55920636991204,-0.753260100986265,
8.85049129520029));
#389210=CARTESIAN_POINT('Ctrl Pts',(2.56491780413931,-0.752043289049005,
8.85711686593484));
#389211=CARTESIAN_POINT('Ctrl Pts',(2.56509113287407,-0.74349514777364,
8.85933012996512));
#389212=CARTESIAN_POINT('Origin',(2.54691766320895,-0.773663284097878,8.85049129520029));
#389213=CARTESIAN_POINT('Ctrl Pts',(2.60624502375466,-0.81546860777333,
8.78727029226991));
#389214=CARTESIAN_POINT('Ctrl Pts',(2.61041921685634,-0.819655669706028,
8.79393457792714));
#389215=CARTESIAN_POINT('Ctrl Pts',(2.60581736094344,-0.826967464105156,
8.79610912703474));
#389216=CARTESIAN_POINT('Ctrl Pts',(2.58944388951046,-0.798615676462708,
8.80838214965002));
#389217=CARTESIAN_POINT('Ctrl Pts',(2.59361738938015,-0.802802043026193,
8.81501364461994));
#389218=CARTESIAN_POINT('Ctrl Pts',(2.58902700057123,-0.81008058293319,
8.8172209842872));
#389219=CARTESIAN_POINT('Ctrl Pts',(2.57261954817435,-0.781739466513853,
8.82945683644723));
#389220=CARTESIAN_POINT('Ctrl Pts',(2.57677664221001,-0.785909376664964,
8.83607469902389));
#389221=CARTESIAN_POINT('Ctrl Pts',(2.57221349406444,-0.793169522772234,
8.8382956714852));
#389222=CARTESIAN_POINT('Ctrl Pts',(2.55577009136411,-0.764838063661105,
8.85049129520029));
#389223=CARTESIAN_POINT('Ctrl Pts',(2.55989296307187,-0.768973645978557,
8.85711686593484));
#389224=CARTESIAN_POINT('Ctrl Pts',(2.55537491841653,-0.776232298374573,
8.85933012996512));
#389225=CARTESIAN_POINT('Origin',(2.59739259559949,-0.824293828210103,8.78727029226991));
#389226=CARTESIAN_POINT('Ctrl Pts',(2.61601447323371,-0.825268202110584,
8.75374538247849));
#389227=CARTESIAN_POINT('Ctrl Pts',(2.62138876695584,-0.830640477734179,
8.75304829418602));
#389228=CARTESIAN_POINT('Ctrl Pts',(2.61904133544637,-0.837904100006663,
8.75272238421917));
#389229=CARTESIAN_POINT('Ctrl Pts',(2.61694640529134,-0.826203006664499,
8.76769408445017));
#389230=CARTESIAN_POINT('Ctrl Pts',(2.62245545220154,-0.831710960650612,
8.76974318093966));
#389231=CARTESIAN_POINT('Ctrl Pts',(2.62030466518859,-0.838949225118367,
8.7707786988043));
#389232=CARTESIAN_POINT('Ctrl Pts',(2.61216985246104,-0.821411731033702,
8.78108014887994));
#389233=CARTESIAN_POINT('Ctrl Pts',(2.61684125757341,-0.826076836774897,
8.78639403366329));
#389234=CARTESIAN_POINT('Ctrl Pts',(2.61383856832237,-0.833593879610382,
8.78812224174741));
#389235=CARTESIAN_POINT('Ctrl Pts',(2.60434213678209,-0.813559887984529,
8.78944554828685));
#389236=CARTESIAN_POINT('Ctrl Pts',(2.60828297933323,-0.817487505278007,
8.79673892988685));
#389237=CARTESIAN_POINT('Ctrl Pts',(2.60326063420179,-0.82485497456516,
8.79894799272499));
#389238=CARTESIAN_POINT('Origin',(2.60729278516567,-0.834224539571367,8.75721825406948));
#389239=CARTESIAN_POINT('Origin',(2.60729278516567,-0.834224539571367,9.));
#389240=CARTESIAN_POINT('Origin',(2.60729278516567,-0.834224539571367,7.51860402984325));
#389241=CARTESIAN_POINT('Ctrl Pts',(2.62143079730771,-0.818824309222858,
7.50366195182966));
#389242=CARTESIAN_POINT('Ctrl Pts',(2.6249261985722,-0.819916125008732,
7.50000065167735));
#389243=CARTESIAN_POINT('Ctrl Pts',(2.62492619857216,-0.819916125008843,
7.49482233047108));
#389244=CARTESIAN_POINT('Ctrl Pts',(2.62069416386203,-0.826227765900201,
7.50215800491337));
#389245=CARTESIAN_POINT('Ctrl Pts',(2.62208379159276,-0.829015889273437,
7.49877273257264));
#389246=CARTESIAN_POINT('Ctrl Pts',(2.62105455902768,-0.832311012439098,
7.49481816995647));
#389247=CARTESIAN_POINT('Ctrl Pts',(2.61813542442623,-0.827395185636949,
7.51043025814041));
#389248=CARTESIAN_POINT('Ctrl Pts',(2.62096858819432,-0.832500667009942,
7.51006209594515));
#389249=CARTESIAN_POINT('Ctrl Pts',(2.61919746011361,-0.838036195483721,
7.50731281821699));
#389250=CARTESIAN_POINT('Ctrl Pts',(2.61614414617582,-0.825398248829051,
7.51860402984325));
#389251=CARTESIAN_POINT('Ctrl Pts',(2.62151707779834,-0.830786441770137,
7.51860402984325));
#389252=CARTESIAN_POINT('Ctrl Pts',(2.61919823167327,-0.838033784044301,
7.51860402984325));
#389253=CARTESIAN_POINT('Origin',(0.,0.,7.5));
#389254=CARTESIAN_POINT('Origin',(2.50151564461753,-0.927015373804513,7.5));
#389255=CARTESIAN_POINT('',(2.50151564461753,-0.927015373804513,7.59394543036555));
#389256=CARTESIAN_POINT('',(2.50151564461753,-0.927015373804513,8.85049129520029));
#389257=CARTESIAN_POINT('',(2.50151564461753,-0.927015373804513,7.5));
#389258=CARTESIAN_POINT('',(2.54864296074705,-0.980775832055524,8.78727029226991));
#389259=CARTESIAN_POINT('Ctrl Pts',(2.50151564461753,-0.927015373804513,
8.85049129520029));
#389260=CARTESIAN_POINT('Ctrl Pts',(2.51724758470005,-0.944961575232345,
8.82945686509571));
#389261=CARTESIAN_POINT('Ctrl Pts',(2.53295613735135,-0.962881097461731,
8.80838212259895));
#389262=CARTESIAN_POINT('Ctrl Pts',(2.54864296074705,-0.980775832055525,
8.78727029226991));
#389263=CARTESIAN_POINT('',(2.55788654645049,-0.991320447028587,8.75721825406948));
#389264=CARTESIAN_POINT('Origin',(2.53006954219644,-0.959587909595145,8.759376797131));
#389265=CARTESIAN_POINT('',(2.55788654645049,-0.991320447028587,7.51860402984325));
#389266=CARTESIAN_POINT('',(2.55788654645049,-0.991320447028587,7.5));
#389267=CARTESIAN_POINT('Ctrl Pts',(2.55788654645049,-0.991320447028587,
7.51860402984325));
#389268=CARTESIAN_POINT('Ctrl Pts',(2.55062714752995,-0.983039291965081,
7.52834476460825));
#389269=CARTESIAN_POINT('Ctrl Pts',(2.54336303591238,-0.974752760895201,
7.53807742314407));
#389270=CARTESIAN_POINT('Ctrl Pts',(2.53609405336271,-0.966460673312385,
7.54780169004674));
#389271=CARTESIAN_POINT('Ctrl Pts',(2.52458037785902,-0.953326454730298,
7.5632044032688));
#389272=CARTESIAN_POINT('Ctrl Pts',(2.51305446717487,-0.940178278873301,
7.57858609112103));
#389273=CARTESIAN_POINT('Ctrl Pts',(2.50151564461753,-0.927015373804512,
7.59394543036555));
#389274=CARTESIAN_POINT('Origin',(2.777769077807,-0.875729379291819,7.5));
#389275=CARTESIAN_POINT('',(2.59029443537467,-0.903257743546327,8.75721825406948));
#389276=CARTESIAN_POINT('',(2.57642062555681,-0.905294943272693,8.78727029226991));
#389277=CARTESIAN_POINT('Origin',(2.54120372156407,-0.910466116016109,8.75658640620982));
#389278=CARTESIAN_POINT('',(2.50568666557815,-0.915681362418202,8.85049129520029));
#389279=CARTESIAN_POINT('Ctrl Pts',(2.57642062555681,-0.905294943272693,
8.78727029226991));
#389280=CARTESIAN_POINT('Ctrl Pts',(2.55287608219231,-0.908752172247956,
8.80838212259895));
#389281=CARTESIAN_POINT('Ctrl Pts',(2.52929892512472,-0.912214190147666,
8.82945686509571));
#389282=CARTESIAN_POINT('Ctrl Pts',(2.50568666557815,-0.915681362418202,
8.85049129520029));
#389283=CARTESIAN_POINT('',(2.50568666557815,-0.915681362418202,7.59394543036555));
#389284=CARTESIAN_POINT('',(2.50568666557815,-0.915681362418202,7.5));
#389285=CARTESIAN_POINT('',(2.59029443537467,-0.903257743546327,7.51860402984325));
#389286=CARTESIAN_POINT('Ctrl Pts',(2.50568666557815,-0.915681362418202,
7.59394543036555));
#389287=CARTESIAN_POINT('Ctrl Pts',(2.5230054242091,-0.913138313983261,
7.57858609112103));
#389288=CARTESIAN_POINT('Ctrl Pts',(2.54030480325287,-0.910598111204303,
7.56320440326857));
#389289=CARTESIAN_POINT('Ctrl Pts',(2.55758581836621,-0.908060604944488,
7.54780169004651));
#389290=CARTESIAN_POINT('Ctrl Pts',(2.56849592237768,-0.906458589261801,
7.53807742314383));
#389291=CARTESIAN_POINT('Ctrl Pts',(2.57939871554832,-0.9048576470869,7.52834476460825));
#389292=CARTESIAN_POINT('Ctrl Pts',(2.59029443537467,-0.903257743546327,
7.51860402984325));
#389293=CARTESIAN_POINT('',(2.59029443537467,-0.903257743546327,7.5));
#389294=CARTESIAN_POINT('Origin',(2.50668546515631,-0.922483422723923,7.5));
#389295=CARTESIAN_POINT('Ctrl Pts',(2.50568666557815,-0.915681362418202,
8.85049129520029));
#389296=CARTESIAN_POINT('Ctrl Pts',(2.50549505870656,-0.915709497549898,
8.85097269580138));
#389297=CARTESIAN_POINT('Ctrl Pts',(2.50530709131976,-0.915745599877189,
8.85143669361005));
#389298=CARTESIAN_POINT('Ctrl Pts',(2.50511427303432,-0.915792190387944,
8.8519052845931));
#389299=CARTESIAN_POINT('Ctrl Pts',(2.5047371326961,-0.915883318472319,
8.85282181883899));
#389300=CARTESIAN_POINT('Ctrl Pts',(2.50435118231721,-0.916012418184739,
8.85372622499636));
#389301=CARTESIAN_POINT('Ctrl Pts',(2.50395525683443,-0.916196137703011,
8.85462257735071));
#389302=CARTESIAN_POINT('Ctrl Pts',(2.50362657356057,-0.916348655121979,
8.85536669723987));
#389303=CARTESIAN_POINT('Ctrl Pts',(2.50329092746444,-0.916538821148347,
8.85610498449051));
#389304=CARTESIAN_POINT('Ctrl Pts',(2.50295156831355,-0.916783139614788,
8.85681338218371));
#389305=CARTESIAN_POINT('Ctrl Pts',(2.50264359935115,-0.917004859006794,
8.85745625420285));
#389306=CARTESIAN_POINT('Ctrl Pts',(2.50232835963297,-0.917273471665691,
8.85808743050666));
#389307=CARTESIAN_POINT('Ctrl Pts',(2.50201318278514,-0.917616619300479,
8.85866804508411));
#389308=CARTESIAN_POINT('Ctrl Pts',(2.50186776701975,-0.917774940180641,
8.85893592806396));
#389309=CARTESIAN_POINT('Ctrl Pts',(2.50172245429853,-0.917949352489988,
8.85919241173848));
#389310=CARTESIAN_POINT('Ctrl Pts',(2.50157875665042,-0.918143956929082,
8.85943017985534));
#389311=CARTESIAN_POINT('Ctrl Pts',(2.5013847222864,-0.918406730530938,
8.8597512372));
#389312=CARTESIAN_POINT('Ctrl Pts',(2.5011892092982,-0.918713389200776,
8.86004599534705));
#389313=CARTESIAN_POINT('Ctrl Pts',(2.50100334875575,-0.919065847627924,
8.86026130871721));
#389314=CARTESIAN_POINT('Ctrl Pts',(2.50093529997119,-0.919194892594958,
8.86034014101235));
#389315=CARTESIAN_POINT('Ctrl Pts',(2.50086751202658,-0.919332009659955,
8.86040910639692));
#389316=CARTESIAN_POINT('Ctrl Pts',(2.50080213330745,-0.919473612221341,
8.86046313645506));
#389317=CARTESIAN_POINT('Ctrl Pts',(2.5007001103638,-0.919694581832473,
8.86054744990829));
#389318=CARTESIAN_POINT('Ctrl Pts',(2.50060130278637,-0.919932567670962,
8.86059655985668));
#389319=CARTESIAN_POINT('Ctrl Pts',(2.50051177684131,-0.92017219464676,
8.86059725258815));
#389320=CARTESIAN_POINT('Ctrl Pts',(2.50042204405556,-0.920412375256605,
8.86059794692011));
#389321=CARTESIAN_POINT('Ctrl Pts',(2.50034312944462,-0.920657798036057,
8.86056369958366));
#389322=CARTESIAN_POINT('Ctrl Pts',(2.50027575459448,-0.920893925584945,
8.86048590497774));
#389323=CARTESIAN_POINT('Ctrl Pts',(2.50025817176459,-0.92095554784484,
8.86046560290182));
#389324=CARTESIAN_POINT('Ctrl Pts',(2.50024123321541,-0.921017363572437,
8.86044257503091));
#389325=CARTESIAN_POINT('Ctrl Pts',(2.50022543070302,-0.921077453935449,
8.86041778462583));
#389326=CARTESIAN_POINT('Ctrl Pts',(2.50011909940391,-0.921481787512591,
8.86025097596201));
#389327=CARTESIAN_POINT('Ctrl Pts',(2.50005025625274,-0.921862343753837,
8.8599848982295));
#389328=CARTESIAN_POINT('Ctrl Pts',(2.50001257343147,-0.922206507017,8.85968173251461));
#389329=CARTESIAN_POINT('Ctrl Pts',(2.49999264137798,-0.92238854966501,
8.85952137522076));
#389330=CARTESIAN_POINT('Ctrl Pts',(2.49998085334339,-0.922563898491408,
8.85934740853961));
#389331=CARTESIAN_POINT('Ctrl Pts',(2.49997582451369,-0.922729976418849,
8.8591675900182));
#389332=CARTESIAN_POINT('Ctrl Pts',(2.49995563114852,-0.923396865623115,
8.85844552518695));
#389333=CARTESIAN_POINT('Ctrl Pts',(2.50004026010222,-0.923951866608731,
8.85759444184124));
#389334=CARTESIAN_POINT('Ctrl Pts',(2.50014990752216,-0.924398186783957,
8.85683498915138));
#389335=CARTESIAN_POINT('Ctrl Pts',(2.50016138183264,-0.924444893001646,
8.85675551444998));
#389336=CARTESIAN_POINT('Ctrl Pts',(2.50017314820603,-0.924490400580309,
8.85667699793651));
#389337=CARTESIAN_POINT('Ctrl Pts',(2.50018512677842,-0.924534707019351,
8.85659965593547));
#389338=CARTESIAN_POINT('Ctrl Pts',(2.50034681415976,-0.925132757594376,
8.85555568965886));
#389339=CARTESIAN_POINT('Ctrl Pts',(2.50058857608736,-0.925684170392098,
8.85434650606346));
#389340=CARTESIAN_POINT('Ctrl Pts',(2.5009059159866,-0.926194166764263,
8.85297329937118));
#389341=CARTESIAN_POINT('Ctrl Pts',(2.50108440034413,-0.926481008649071,
8.85220095427747));
#389342=CARTESIAN_POINT('Ctrl Pts',(2.50128713331755,-0.926754699673002,
8.85137579139184));
#389343=CARTESIAN_POINT('Ctrl Pts',(2.50151564461753,-0.927015373804513,
8.85049129520029));
#389344=CARTESIAN_POINT('Origin',(2.50668546515631,-0.922483422723923,7.59394543036555));
#389345=CARTESIAN_POINT('Ctrl Pts',(2.50513036619197,-0.915763048196814,
7.59443877723642));
#389346=CARTESIAN_POINT('Ctrl Pts',(2.49940101777127,-0.916604333120576,
7.58783886950016));
#389347=CARTESIAN_POINT('Ctrl Pts',(2.49865736261564,-0.925061647029031,
7.58559994247159));
#389348=CARTESIAN_POINT('Ctrl Pts',(2.5364067111286,-0.911170498480252,
7.56670252222135));
#389349=CARTESIAN_POINT('Ctrl Pts',(2.53068564324298,-0.912010567508453,
7.56004874999026));
#389350=CARTESIAN_POINT('Ctrl Pts',(2.52991629821514,-0.920516122486497,
7.55786368756704));
#389351=CARTESIAN_POINT('Ctrl Pts',(2.56762465061598,-0.906586524891429,
7.53888913333557));
#389352=CARTESIAN_POINT('Ctrl Pts',(2.56186958214379,-0.907431586490991,
7.53222002137278));
#389353=CARTESIAN_POINT('Ctrl Pts',(2.56111780051421,-0.915977770967209,
7.53005029815327));
#389354=CARTESIAN_POINT('Ctrl Pts',(2.59878277202119,-0.902011334858258,
7.51101258149734));
#389355=CARTESIAN_POINT('Ctrl Pts',(2.59295794166189,-0.902866640139928,
7.5043616886572));
#389356=CARTESIAN_POINT('Ctrl Pts',(2.59226033981814,-0.911446898481741,
7.50217374673251));
#389357=CARTESIAN_POINT('',(2.59059853376833,-0.91168867064083,7.50366116523517));
#389358=CARTESIAN_POINT('Ctrl Pts',(2.59029443537467,-0.903257743546327,
7.51860402984325));
#389359=CARTESIAN_POINT('Ctrl Pts',(2.59073136135583,-0.903193586296015,
7.51734760759494));
#389360=CARTESIAN_POINT('Ctrl Pts',(2.59113483014927,-0.903194476627528,
7.51608817408573));
#389361=CARTESIAN_POINT('Ctrl Pts',(2.59150388429384,-0.903273766104963,
7.5148100591312));
#389362=CARTESIAN_POINT('Ctrl Pts',(2.59183818235683,-0.903345588408308,
7.51365231206384));
#389363=CARTESIAN_POINT('Ctrl Pts',(2.59214476638707,-0.903481595190324,
7.51247773061043));
#389364=CARTESIAN_POINT('Ctrl Pts',(2.59240335794634,-0.903713185892312,
7.51129758471022));
#389365=CARTESIAN_POINT('Ctrl Pts',(2.59272475772225,-0.904001026686227,
7.50983079813402));
#389366=CARTESIAN_POINT('Ctrl Pts',(2.59295307372471,-0.904437038238346,
7.50839324291155));
#389367=CARTESIAN_POINT('Ctrl Pts',(2.59301693980263,-0.905062645938763,
7.50715379678855));
#389368=CARTESIAN_POINT('Ctrl Pts',(2.59304644409036,-0.905351658669903,
7.50658120839351));
#389369=CARTESIAN_POINT('Ctrl Pts',(2.59303559361286,-0.905723185272602,
7.50598221009429));
#389370=CARTESIAN_POINT('Ctrl Pts',(2.59296190979915,-0.906167719907855,
7.50545747549611));
#389371=CARTESIAN_POINT('Ctrl Pts',(2.59292258983543,-0.90640493734886,
7.50517746087247));
#389372=CARTESIAN_POINT('Ctrl Pts',(2.59286515073088,-0.906665550100599,
7.50491486231392));
#389373=CARTESIAN_POINT('Ctrl Pts',(2.59278948464783,-0.906942297683558,
7.50468370960992));
#389374=CARTESIAN_POINT('Ctrl Pts',(2.59267633998614,-0.907356122615158,
7.50433806340447));
#389375=CARTESIAN_POINT('Ctrl Pts',(2.59251851063053,-0.907818286743156,
7.50405484070984));
#389376=CARTESIAN_POINT('Ctrl Pts',(2.59232594814199,-0.908297432651594,
7.50385766036131));
#389377=CARTESIAN_POINT('Ctrl Pts',(2.59230535657694,-0.908348669858887,
7.50383657498791));
#389378=CARTESIAN_POINT('Ctrl Pts',(2.5922843903288,-0.908400083971413,
7.50381643264937));
#389379=CARTESIAN_POINT('Ctrl Pts',(2.59226307810043,-0.908451624345659,
7.50379723213559));
#389380=CARTESIAN_POINT('Ctrl Pts',(2.59212081200436,-0.908795673203785,
7.50366906242519));
#389381=CARTESIAN_POINT('Ctrl Pts',(2.59195936993194,-0.909152557376852,
7.50358235568538));
#389382=CARTESIAN_POINT('Ctrl Pts',(2.59179549077373,-0.909492809245827,
7.5035341175365));
#389383=CARTESIAN_POINT('Ctrl Pts',(2.59154977252354,-0.91000297841428,
7.50346178989176));
#389384=CARTESIAN_POINT('Ctrl Pts',(2.59126374379867,-0.910541356689506,
7.50346967198527));
#389385=CARTESIAN_POINT('Ctrl Pts',(2.5909666896131,-0.911061237388405,
7.50354272648692));
#389386=CARTESIAN_POINT('Ctrl Pts',(2.59084450507791,-0.911275075080755,
7.50357277531559));
#389387=CARTESIAN_POINT('Ctrl Pts',(2.59072074066282,-0.91148556949305,
7.50361331098761));
#389388=CARTESIAN_POINT('Ctrl Pts',(2.59059853376967,-0.9116886706413,7.50366116523659));
#389389=CARTESIAN_POINT('',(2.50943323048224,-0.923494625764139,7.57603338622103));
#389390=CARTESIAN_POINT('Origin',(2.51772543279387,-0.92654927311432,7.58486873427625));
#389391=CARTESIAN_POINT('Ctrl Pts',(2.59059853382406,-0.911688670627307,
7.50366116529968));
#389392=CARTESIAN_POINT('Ctrl Pts',(2.563587701386,-0.915618394511217,7.52783573079709));
#389393=CARTESIAN_POINT('Ctrl Pts',(2.53653388028073,-0.919553544813569,
7.55196141284068));
#389394=CARTESIAN_POINT('Ctrl Pts',(2.5094332316199,-0.923494625241301,
7.57603338728831));
#389395=CARTESIAN_POINT('Ctrl Pts',(2.50672970590158,-0.915705906336646,
7.59639677331371));
#389396=CARTESIAN_POINT('Ctrl Pts',(2.48845360594461,-0.915469081268716,
7.59959882295466));
#389397=CARTESIAN_POINT('Ctrl Pts',(2.50218806282135,-0.927555168596909,
7.59642833564546));
#389398=CARTESIAN_POINT('Ctrl Pts',(2.50288821974744,-0.915029084195087,
7.58707626057421));
#389399=CARTESIAN_POINT('Ctrl Pts',(2.49736120456837,-0.918948828350837,
7.58809943920599));
#389400=CARTESIAN_POINT('Ctrl Pts',(2.49892019688552,-0.925527881759068,
7.58710240504253));
#389401=CARTESIAN_POINT('Ctrl Pts',(2.5063100950153,-0.920050677758169,
7.5801537675693));
#389402=CARTESIAN_POINT('Ctrl Pts',(2.50378963817576,-0.921383557616306,
7.58205880659761));
#389403=CARTESIAN_POINT('Ctrl Pts',(2.50479226230758,-0.92401449278997,
7.58020924244128));
#389404=CARTESIAN_POINT('Ctrl Pts',(2.50943322970566,-0.923494625478133,
7.57603338509286));
#389405=CARTESIAN_POINT('Ctrl Pts',(2.50943322970566,-0.923494625478133,
7.57603338509286));
#389406=CARTESIAN_POINT('Ctrl Pts',(2.50943322970566,-0.923494625478133,
7.57603338509286));
#389407=CARTESIAN_POINT('Origin',(2.51772740356796,-0.926543917882699,7.58486873427622));
#389408=CARTESIAN_POINT('Ctrl Pts',(2.56355987305573,-0.997792291028094,
7.51098857897448));
#389409=CARTESIAN_POINT('Ctrl Pts',(2.55967899499225,-0.99336518165196,
7.50433767179956));
#389410=CARTESIAN_POINT('Ctrl Pts',(2.56470980820182,-0.986379555729187,
7.50214974420965));
#389411=CARTESIAN_POINT('Ctrl Pts',(2.54279444458098,-0.974104140667198,
7.53887321589167));
#389412=CARTESIAN_POINT('Ctrl Pts',(2.53896006632404,-0.969730075918102,
7.53220407452064));
#389413=CARTESIAN_POINT('Ctrl Pts',(2.54392751200519,-0.962735263316842,
7.53003438070911));
#389414=CARTESIAN_POINT('Ctrl Pts',(2.52198913882352,-0.950370500319426,
7.56669465659235));
#389415=CARTESIAN_POINT('Ctrl Pts',(2.51817742102915,-0.946022285479792,
7.56004085833302));
#389416=CARTESIAN_POINT('Ctrl Pts',(2.52310514388123,-0.939047029382757,
7.5578558219379));
#389417=CARTESIAN_POINT('Ctrl Pts',(2.50114489672401,-0.926592443362293,
7.59443891967696));
#389418=CARTESIAN_POINT('Ctrl Pts',(2.49732765241344,-0.922237924152493,
7.58783901202978));
#389419=CARTESIAN_POINT('Ctrl Pts',(2.50224367002345,-0.915316078383742,
7.58560008491213));
#389420=CARTESIAN_POINT('',(2.56358326728472,-0.985097876880914,7.50366116523517));
#389421=CARTESIAN_POINT('Ctrl Pts',(2.56358326728507,-0.985097876881048,
7.50366116523554));
#389422=CARTESIAN_POINT('Ctrl Pts',(2.56345970006384,-0.985845452066967,
7.50350835821027));
#389423=CARTESIAN_POINT('Ctrl Pts',(2.56332179021807,-0.98652863497482,
7.50345484956));
#389424=CARTESIAN_POINT('Ctrl Pts',(2.56316602620427,-0.987167856010446,
7.50349758195598));
#389425=CARTESIAN_POINT('Ctrl Pts',(2.56308610771344,-0.98749582380759,
7.50351950684424));
#389426=CARTESIAN_POINT('Ctrl Pts',(2.56299373787713,-0.987844575329,7.50357029184312));
#389427=CARTESIAN_POINT('Ctrl Pts',(2.56289542256784,-0.988178424023541,
7.50365515313924));
#389428=CARTESIAN_POINT('Ctrl Pts',(2.56274417381037,-0.988692018504435,
7.50378570417639));
#389429=CARTESIAN_POINT('Ctrl Pts',(2.56257474719319,-0.989185516731543,
7.50400001621911));
#389430=CARTESIAN_POINT('Ctrl Pts',(2.5623978911558,-0.989620619087731,
7.50428903009635));
#389431=CARTESIAN_POINT('Ctrl Pts',(2.5623782614963,-0.989668912101789,
7.50432110841318));
#389432=CARTESIAN_POINT('Ctrl Pts',(2.56235854685539,-0.989716515320723,
7.50435406373354));
#389433=CARTESIAN_POINT('Ctrl Pts',(2.56233876646288,-0.98976339828974,
7.50438785222352));
#389434=CARTESIAN_POINT('Ctrl Pts',(2.56221799765893,-0.990049641350414,
7.50459414719561));
#389435=CARTESIAN_POINT('Ctrl Pts',(2.56209237988989,-0.990313392525846,
7.50483629897752));
#389436=CARTESIAN_POINT('Ctrl Pts',(2.56196791368994,-0.990545113472999,
7.5050991045531));
#389437=CARTESIAN_POINT('Ctrl Pts',(2.56169332875141,-0.991056313156583,
7.50567888004914));
#389438=CARTESIAN_POINT('Ctrl Pts',(2.56141398648965,-0.991432015973533,
7.50637912803144));
#389439=CARTESIAN_POINT('Ctrl Pts',(2.56114901670265,-0.99169650091034,
7.50710440483569));
#389440=CARTESIAN_POINT('Ctrl Pts',(2.5610840408505,-0.991761357867607,
7.50728225710685));
#389441=CARTESIAN_POINT('Ctrl Pts',(2.56101873889053,-0.991820921385632,
7.50746498566954));
#389442=CARTESIAN_POINT('Ctrl Pts',(2.56095491592359,-0.991874108847966,
7.50764697238949));
#389443=CARTESIAN_POINT('Ctrl Pts',(2.56061182121787,-0.992160030007889,
7.50862528291181));
#389444=CARTESIAN_POINT('Ctrl Pts',(2.56028297152454,-0.992290828132516,
7.50965856837421));
#389445=CARTESIAN_POINT('Ctrl Pts',(2.55997541446454,-0.992332425349248,
7.51067959873201));
#389446=CARTESIAN_POINT('Ctrl Pts',(2.55980616542649,-0.992355316350085,
7.51124147302578));
#389447=CARTESIAN_POINT('Ctrl Pts',(2.55964326493998,-0.992350769606331,
7.51180065547252));
#389448=CARTESIAN_POINT('Ctrl Pts',(2.55948762194074,-0.992327067952724,
7.51235175716501));
#389449=CARTESIAN_POINT('Ctrl Pts',(2.55894981337755,-0.992245169297896,
7.51425603304536));
#389450=CARTESIAN_POINT('Ctrl Pts',(2.55843544700616,-0.991918804986652,
7.5162690050518));
#389451=CARTESIAN_POINT('Ctrl Pts',(2.55796290178257,-0.991405463116651,
7.51827788969244));
#389452=CARTESIAN_POINT('Ctrl Pts',(2.55793732674208,-0.991377680084565,
7.51838661432545));
#389453=CARTESIAN_POINT('Ctrl Pts',(2.55791187398801,-0.991349339402174,
7.51849533314857));
#389454=CARTESIAN_POINT('Ctrl Pts',(2.55788654645049,-0.99132044702859,
7.51860402984325));
#389455=CARTESIAN_POINT('Ctrl Pts',(2.50943323101062,-0.923494626900362,
7.57603338728985));
#389456=CARTESIAN_POINT('Ctrl Pts',(2.52751419016524,-0.944062956661477,
7.55196141284923));
#389457=CARTESIAN_POINT('Ctrl Pts',(2.54556333675353,-0.964596416013586,
7.52783573083105));
#389458=CARTESIAN_POINT('Ctrl Pts',(2.56358326731954,-0.985097876928764,
7.50366116530176));
#389459=CARTESIAN_POINT('Origin',(8.67125181207509E-16,-3.1911008230166E-16,
7.49482233047033));
#389460=CARTESIAN_POINT('Origin',(2.58226093460098,-0.908754485894666,7.49482233047033));
#389461=CARTESIAN_POINT('Origin',(0.,0.,7.50366116523517));
#389462=CARTESIAN_POINT('Origin',(2.55533261422669,-0.981927431468018,7.49482233047033));
#389463=CARTESIAN_POINT('Ctrl Pts',(2.59029338886968,-0.903257897167587,
7.51860402984325));
#389464=CARTESIAN_POINT('Ctrl Pts',(2.59782171669849,-0.902153104819651,
7.51860402984325));
#389465=CARTESIAN_POINT('Ctrl Pts',(2.60029797237974,-0.894958353689057,
7.51860402984325));
#389466=CARTESIAN_POINT('Ctrl Pts',(2.593088708184,-0.902847678972038,7.51041458714366));
#389467=CARTESIAN_POINT('Ctrl Pts',(2.59840836067142,-0.900448582647727,
7.51004642900443));
#389468=CARTESIAN_POINT('Ctrl Pts',(2.60029865530166,-0.894956369462121,
7.5072913648301));
#389469=CARTESIAN_POINT('Ctrl Pts',(2.59443309621023,-0.90532080614916,
7.50215815450137));
#389470=CARTESIAN_POINT('Ctrl Pts',(2.59721402775987,-0.903919205564955,
7.49877163671529));
#389471=CARTESIAN_POINT('Ctrl Pts',(2.5983593911649,-0.900664660087504,
7.4948158853317));
#389472=CARTESIAN_POINT('Ctrl Pts',(2.59059801446911,-0.911688487888502,
7.50366171572174));
#389473=CARTESIAN_POINT('Ctrl Pts',(2.59405208042095,-0.912904049757564,
7.50000045605858));
#389474=CARTESIAN_POINT('Ctrl Pts',(2.59405208042099,-0.912904049757446,
7.49482233047317));
#389475=CARTESIAN_POINT('Origin',(2.58847843614165,-0.890890361172289,7.51860402984325));
#389476=CARTESIAN_POINT('Origin',(2.58847843614165,-0.890890361172289,9.));
#389477=CARTESIAN_POINT('Origin',(2.58847843614165,-0.890890361172289,8.75721825406948));
#389478=CARTESIAN_POINT('Ctrl Pts',(2.57377144873504,-0.905683912037573,
8.78942910404913));
#389479=CARTESIAN_POINT('Ctrl Pts',(2.57928769835755,-0.904894343291985,
8.79672699501692));
#389480=CARTESIAN_POINT('Ctrl Pts',(2.57966709350248,-0.895976409377319,
8.79893251111267));
#389481=CARTESIAN_POINT('Ctrl Pts',(2.58464914173358,-0.904086660094482,
8.78111911759576));
#389482=CARTESIAN_POINT('Ctrl Pts',(2.59118766485554,-0.903143248461614,
8.78644465894809));
#389483=CARTESIAN_POINT('Ctrl Pts',(2.593261215509,-0.895306418779725,8.78817647674132));
#389484=CARTESIAN_POINT('Ctrl Pts',(2.59142837946313,-0.903091214554007,
8.76780923932035));
#389485=CARTESIAN_POINT('Ctrl Pts',(2.59914610221575,-0.901972513394413,
8.76988516158378));
#389486=CARTESIAN_POINT('Ctrl Pts',(2.60175132061198,-0.894876795142932,
8.77093053738833));
#389487=CARTESIAN_POINT('Ctrl Pts',(2.59010652088601,-0.903285312809052,
8.75371302330491));
#389488=CARTESIAN_POINT('Ctrl Pts',(2.59763493587648,-0.902194822506869,
8.75300828287558));
#389489=CARTESIAN_POINT('Ctrl Pts',(2.60009538217395,-0.894960132233495,
8.75267964240738));
#389490=CARTESIAN_POINT('Origin',(2.5746046263238,-0.892927560898654,8.78727029226991));
#389491=CARTESIAN_POINT('Ctrl Pts',(2.50568666557815,-0.915681362418202,
8.85049129520029));
#389492=CARTESIAN_POINT('Ctrl Pts',(2.51146432645974,-0.914832983398916,
8.85711686593484));
#389493=CARTESIAN_POINT('Ctrl Pts',(2.51218498036397,-0.906313510406752,
8.85933012996512));
#389494=CARTESIAN_POINT('Ctrl Pts',(2.52929895681325,-0.912214185494592,
8.82945683644724));
#389495=CARTESIAN_POINT('Ctrl Pts',(2.53512457577341,-0.911358764416513,
8.8360746990239));
#389496=CARTESIAN_POINT('Ctrl Pts',(2.5358099765306,-0.902811117471319,
8.8382956714852));
#389497=CARTESIAN_POINT('Ctrl Pts',(2.55287605202416,-0.908752176677781,
8.80838214965001));
#389498=CARTESIAN_POINT('Ctrl Pts',(2.55872466159663,-0.907893379708745,
8.81501364461986));
#389499=CARTESIAN_POINT('Ctrl Pts',(2.55939923284054,-0.899314698794276,
8.8172209842872));
#389500=CARTESIAN_POINT('Ctrl Pts',(2.57642062555681,-0.905294943272693,
8.78727029226991));
#389501=CARTESIAN_POINT('Ctrl Pts',(2.58227020660258,-0.904436003654647,
8.79393457792714));
#389502=CARTESIAN_POINT('Ctrl Pts',(2.58295547781501,-0.89582381354158,
8.79610912703474));
#389503=CARTESIAN_POINT('Origin',(2.50387066634513,-0.903313980044163,8.85049129520029));
#389504=CARTESIAN_POINT('Ctrl Pts',(2.50151564461753,-0.927015373804513,
8.85049129520029));
#389505=CARTESIAN_POINT('Ctrl Pts',(2.50536507777437,-0.931406612421822,
8.85711686593484));
#389506=CARTESIAN_POINT('Ctrl Pts',(2.50039125247055,-0.938360879023052,
8.85933012996512));
#389507=CARTESIAN_POINT('Ctrl Pts',(2.49811010667084,-0.923130508387983,
8.86332496987232));
#389508=CARTESIAN_POINT('Ctrl Pts',(2.49678212912386,-0.927556383443994,
8.86648636486737));
#389509=CARTESIAN_POINT('Ctrl Pts',(2.4908770045068,-0.927481515896429,
8.87206031107457));
#389510=CARTESIAN_POINT('Ctrl Pts',(2.50054051873364,-0.916437011304924,
8.86341338519876));
#389511=CARTESIAN_POINT('Ctrl Pts',(2.50237644878422,-0.912182269070235,
8.86654584966059));
#389512=CARTESIAN_POINT('Ctrl Pts',(2.49777763608562,-0.908443943970582,
8.87215952290714));
#389513=CARTESIAN_POINT('Ctrl Pts',(2.50568666557815,-0.915681362418202,
8.85049129520029));
#389514=CARTESIAN_POINT('Ctrl Pts',(2.51146432645974,-0.914832983398916,
8.85711686593484));
#389515=CARTESIAN_POINT('Ctrl Pts',(2.51218498036397,-0.906313510406752,
8.85933012996512));
#389516=CARTESIAN_POINT('Origin',(2.49211597091067,-0.935255284860132,8.85049129520029));
#389517=CARTESIAN_POINT('Ctrl Pts',(2.54864296074705,-0.980775832055525,
8.78727029226991));
#389518=CARTESIAN_POINT('Ctrl Pts',(2.55254031154223,-0.985221732690688,
8.79393457792714));
#389519=CARTESIAN_POINT('Ctrl Pts',(2.54747944236024,-0.992223662303376,
8.79610912703474));
#389520=CARTESIAN_POINT('Ctrl Pts',(2.53295611725147,-0.962881074532807,
8.80838214965001));
#389521=CARTESIAN_POINT('Ctrl Pts',(2.53685282079144,-0.967326236811936,
8.81501364461995));
#389522=CARTESIAN_POINT('Ctrl Pts',(2.53180552577563,-0.974295714957295,
8.81722098428721));
#389523=CARTESIAN_POINT('Ctrl Pts',(2.5172476058129,-0.944961599316815,
8.82945683644724));
#389524=CARTESIAN_POINT('Ctrl Pts',(2.52112899159235,-0.949389287869639,
8.8360746990239));
#389525=CARTESIAN_POINT('Ctrl Pts',(2.51611005976585,-0.956342155322605,
8.83829567148519));
#389526=CARTESIAN_POINT('Ctrl Pts',(2.50151564461753,-0.927015373804513,
8.85049129520029));
#389527=CARTESIAN_POINT('Ctrl Pts',(2.50536507777437,-0.931406612421822,
8.85711686593484));
#389528=CARTESIAN_POINT('Ctrl Pts',(2.50039125247055,-0.938360879023052,
8.85933012996512));
#389529=CARTESIAN_POINT('Origin',(2.53924328704018,-0.989015743111143,8.78727029226991));
#389530=CARTESIAN_POINT('Ctrl Pts',(2.55776447567946,-0.991181222852413,
8.75374538247848));
#389531=CARTESIAN_POINT('Ctrl Pts',(2.56278352445775,-0.996886792740585,
8.75304829418601));
#389532=CARTESIAN_POINT('Ctrl Pts',(2.55997553412123,-1.00398509066889,
8.75272238421917));
#389533=CARTESIAN_POINT('Ctrl Pts',(2.55863459984933,-0.992173815842068,
8.76769408445022));
#389534=CARTESIAN_POINT('Ctrl Pts',(2.56377943200829,-0.998023418993408,
8.76974318093971));
#389535=CARTESIAN_POINT('Ctrl Pts',(2.56116930682118,-1.00510901027346,
8.7707786988043));
#389536=CARTESIAN_POINT('Ctrl Pts',(2.55417483904274,-0.987086349610299,
8.78108014887987));
#389537=CARTESIAN_POINT('Ctrl Pts',(2.55853775190122,-0.992041168344586,
8.78639403366322));
#389538=CARTESIAN_POINT('Ctrl Pts',(2.55505961340924,-0.999350383648536,
8.78812224174741));
#389539=CARTESIAN_POINT('Ctrl Pts',(2.5468662755566,-0.978749115549309,
8.78944554828685));
#389540=CARTESIAN_POINT('Ctrl Pts',(2.55054737792009,-0.982921153780983,
8.79673892988686));
#389541=CARTESIAN_POINT('Ctrl Pts',(2.54506331635742,-0.989951703054938,
8.79894799272499));
#389542=CARTESIAN_POINT('Origin',(2.54848687274363,-0.999560358084206,8.75721825406948));
#389543=CARTESIAN_POINT('Origin',(2.54848687274363,-0.999560358084206,9.));
#389544=CARTESIAN_POINT('Origin',(2.54848687274363,-0.999560358084206,7.51860402984325));
#389545=CARTESIAN_POINT('Ctrl Pts',(2.56358253296961,-0.985097594708649,
7.50366195182966));
#389546=CARTESIAN_POINT('Ctrl Pts',(2.56700079967973,-0.986411118369829,
7.50000065167735));
#389547=CARTESIAN_POINT('Ctrl Pts',(2.56700079967969,-0.986411118369938,
7.49482233047108));
#389548=CARTESIAN_POINT('Ctrl Pts',(2.56237307191841,-0.992438643923323,
7.50215800491337));
#389549=CARTESIAN_POINT('Ctrl Pts',(2.56358120883207,-0.99531007255245,
7.49877273257265));
#389550=CARTESIAN_POINT('Ctrl Pts',(2.5623429716696,-0.998532482377318,
7.49481816995647));
#389551=CARTESIAN_POINT('Ctrl Pts',(2.55974479284785,-0.993439726072484,
7.51043025814041));
#389552=CARTESIAN_POINT('Ctrl Pts',(2.56224502626245,-0.998716239112309,
7.51006209594514));
#389553=CARTESIAN_POINT('Ctrl Pts',(2.56012287462732,-1.0041269176834,7.50731281821699));
#389554=CARTESIAN_POINT('Ctrl Pts',(2.55788555007275,-0.991319310549886,
7.51860402984325));
#389555=CARTESIAN_POINT('Ctrl Pts',(2.56290221972397,-0.997040677781688,
7.51860402984325));
#389556=CARTESIAN_POINT('Ctrl Pts',(2.56012379910318,-1.00412456063254,
7.51860402984325));
#389557=CARTESIAN_POINT('Origin',(0.,0.,7.5));
#389558=CARTESIAN_POINT('Origin',(2.4369819335138,-1.08538337893279,7.5));
#389559=CARTESIAN_POINT('',(2.4369819335138,-1.08538337893279,7.59394543036555));
#389560=CARTESIAN_POINT('',(2.4369819335138,-1.08538337893279,8.85049129520029));
#389561=CARTESIAN_POINT('',(2.4369819335138,-1.08538337893279,7.5));
#389562=CARTESIAN_POINT('',(2.48056797713153,-1.14205283806805,8.78727029226991));
#389563=CARTESIAN_POINT('Ctrl Pts',(2.4369819335138,-1.08538337893279,8.85049129520029));
#389564=CARTESIAN_POINT('Ctrl Pts',(2.45153173356487,-1.10430065682687,
8.82945686509571));
#389565=CARTESIAN_POINT('Ctrl Pts',(2.46605990357883,-1.12318981189993,
8.80838212259896));
#389566=CARTESIAN_POINT('Ctrl Pts',(2.48056797713153,-1.14205283806805,
8.78727029226991));
#389567=CARTESIAN_POINT('',(2.48911697509583,-1.15316802656817,8.75721825406948));
#389568=CARTESIAN_POINT('Origin',(2.46339023451441,-1.11971844545458,8.75937679713111));
#389569=CARTESIAN_POINT('',(2.48911697509583,-1.15316802656817,7.51860402984325));
#389570=CARTESIAN_POINT('',(2.48911697509583,-1.15316802656817,7.5));
#389571=CARTESIAN_POINT('Ctrl Pts',(2.48911697509583,-1.15316802656817,
7.51860402984325));
#389572=CARTESIAN_POINT('Ctrl Pts',(2.48240306681555,-1.14443877474013,
7.52834476460825));
#389573=CARTESIAN_POINT('Ctrl Pts',(2.47568479996291,-1.13570385600776,
7.53807742314407));
#389574=CARTESIAN_POINT('Ctrl Pts',(2.46896202819301,-1.12696308009721,
7.54780169004674));
#389575=CARTESIAN_POINT('Ctrl Pts',(2.45831352104431,-1.11311816345353,
7.5632044032688));
#389576=CARTESIAN_POINT('Ctrl Pts',(2.44765369809931,-1.09925853430096,
7.57858609112103));
#389577=CARTESIAN_POINT('Ctrl Pts',(2.4369819335138,-1.08538337893279,7.59394543036555));
#389578=CARTESIAN_POINT('Origin',(2.71595367934704,-1.0519023752311,7.5));
#389579=CARTESIAN_POINT('',(2.52710047532069,-1.0673626379274,8.75721825406948));
#389580=CARTESIAN_POINT('',(2.51312464689845,-1.06850675396143,8.78727029226991));
#389581=CARTESIAN_POINT('Origin',(2.47764878164183,-1.07141094718957,8.75658640621155));
#389582=CARTESIAN_POINT('',(2.44187055726729,-1.07433989271893,8.85049129520029));
#389583=CARTESIAN_POINT('Ctrl Pts',(2.51312464689845,-1.06850675396143,
8.78727029226991));
#389584=CARTESIAN_POINT('Ctrl Pts',(2.48940697290248,-1.07044837561627,
8.80838212259896));
#389585=CARTESIAN_POINT('Ctrl Pts',(2.4656564453843,-1.07239268678907,8.82945686509571));
#389586=CARTESIAN_POINT('Ctrl Pts',(2.44187055726729,-1.07433989271893,
8.85049129520029));
#389587=CARTESIAN_POINT('',(2.44187055726729,-1.07433989271893,7.59394543036555));
#389588=CARTESIAN_POINT('',(2.44187055726729,-1.07433989271893,7.5));
#389589=CARTESIAN_POINT('',(2.52710047532069,-1.0673626379274,7.51860402984325));
#389590=CARTESIAN_POINT('Ctrl Pts',(2.44187055726729,-1.07433989271893,
7.59394543036555));
#389591=CARTESIAN_POINT('Ctrl Pts',(2.45931666632385,-1.07291168592502,
7.57858609112103));
#389592=CARTESIAN_POINT('Ctrl Pts',(2.47674325328887,-1.07148507728597,
7.56320440326857));
#389593=CARTESIAN_POINT('Ctrl Pts',(2.49415134128755,-1.07005998304471,
7.54780169004651));
#389594=CARTESIAN_POINT('Ctrl Pts',(2.50514167081742,-1.06916027163909,
7.53807742314383));
#389595=CARTESIAN_POINT('Ctrl Pts',(2.51612463574749,-1.06826116312843,
7.52834476460825));
#389596=CARTESIAN_POINT('Ctrl Pts',(2.52710047532068,-1.0673626379274,7.51860402984325));
#389597=CARTESIAN_POINT('',(2.52710047532069,-1.0673626379274,7.5));
#389598=CARTESIAN_POINT('Origin',(2.44243149520449,-1.08119197077092,7.5));
#389599=CARTESIAN_POINT('Ctrl Pts',(2.44187055726729,-1.07433989271893,
8.85049129520029));
#389600=CARTESIAN_POINT('Ctrl Pts',(2.4416775414485,-1.07435569374957,8.85097269580138));
#389601=CARTESIAN_POINT('Ctrl Pts',(2.4414876471768,-1.07437967878893,8.85143669361005));
#389602=CARTESIAN_POINT('Ctrl Pts',(2.44129223999294,-1.07441381966452,
8.8519052845931));
#389603=CARTESIAN_POINT('Ctrl Pts',(2.44091003593358,-1.07448059705204,
8.85282181883899));
#389604=CARTESIAN_POINT('Ctrl Pts',(2.44051660708416,-1.07458470358958,
8.85372622499635));
#389605=CARTESIAN_POINT('Ctrl Pts',(2.4401097241228,-1.07474267860362,8.8546225773507));
#389606=CARTESIAN_POINT('Ctrl Pts',(2.43977194433939,-1.07487382384953,
8.85536669723986));
#389607=CARTESIAN_POINT('Ctrl Pts',(2.43942480388502,-1.07504209424019,
8.85610498449051));
#389608=CARTESIAN_POINT('Ctrl Pts',(2.43907048844601,-1.07526416791268,
8.85681338218371));
#389609=CARTESIAN_POINT('Ctrl Pts',(2.43874894662865,-1.07546570011925,
8.85745625420285));
#389610=CARTESIAN_POINT('Ctrl Pts',(2.43841714453213,-1.07571356340654,
8.85808743050666));
#389611=CARTESIAN_POINT('Ctrl Pts',(2.43808062970449,-1.07603581255774,
8.85866804508411));
#389612=CARTESIAN_POINT('Ctrl Pts',(2.43792536905777,-1.0761844913306,8.85893592806396));
#389613=CARTESIAN_POINT('Ctrl Pts',(2.4377691802621,-1.07634923507313,8.85919241173849));
#389614=CARTESIAN_POINT('Ctrl Pts',(2.43761330950699,-1.07653423293661,
8.85943017985535));
#389615=CARTESIAN_POINT('Ctrl Pts',(2.43740283784491,-1.07678403481753,
8.85975123720001));
#389616=CARTESIAN_POINT('Ctrl Pts',(2.43718807887067,-1.07707753686408,
8.86004599534706));
#389617=CARTESIAN_POINT('Ctrl Pts',(2.43698001810968,-1.07741736300175,
8.86026130871721));
#389618=CARTESIAN_POINT('Ctrl Pts',(2.43690384119922,-1.07754178293146,
8.86034014101236));
#389619=CARTESIAN_POINT('Ctrl Pts',(2.43682740741169,-1.07767427508622,
8.86040910639693));
#389620=CARTESIAN_POINT('Ctrl Pts',(2.4367530905129,-1.07781139788104,8.86046313645507));
#389621=CARTESIAN_POINT('Ctrl Pts',(2.43663711961474,-1.07802537685396,
8.8605474499083));
#389622=CARTESIAN_POINT('Ctrl Pts',(2.43652326724304,-1.0782565431018,8.86059655985669));
#389623=CARTESIAN_POINT('Ctrl Pts',(2.43641857228559,-1.07848994179129,
8.86059725258816));
#389624=CARTESIAN_POINT('Ctrl Pts',(2.43631363544096,-1.07872387972499,
8.86059794692012));
#389625=CARTESIAN_POINT('Ctrl Pts',(2.43621915867709,-1.07896374218053,
8.86056369958366));
#389626=CARTESIAN_POINT('Ctrl Pts',(2.4361367935118,-1.07919506785858,8.86048590497774));
#389627=CARTESIAN_POINT('Ctrl Pts',(2.43611529865597,-1.07925543697315,
8.86046560290182));
#389628=CARTESIAN_POINT('Ctrl Pts',(2.43609443436159,-1.07931604043714,
8.86044257503091));
#389629=CARTESIAN_POINT('Ctrl Pts',(2.43607481431438,-1.07937499486761,
8.86041778462583));
#389630=CARTESIAN_POINT('Ctrl Pts',(2.4359427957431,-1.07977168502833,8.86025097596201));
#389631=CARTESIAN_POINT('Ctrl Pts',(2.43584971171548,-1.08014704858012,
8.8599848982295));
#389632=CARTESIAN_POINT('Ctrl Pts',(2.43579005570162,-1.0804880903763,8.85968173251462));
#389633=CARTESIAN_POINT('Ctrl Pts',(2.43575850108817,-1.08066848194711,
8.85952137522077));
#389634=CARTESIAN_POINT('Ctrl Pts',(2.43573550263548,-1.08084271523857,
8.85934740853961));
#389635=CARTESIAN_POINT('Ctrl Pts',(2.43571984348871,-1.08100812974288,
8.8591675900182));
#389636=CARTESIAN_POINT('Ctrl Pts',(2.43565696387494,-1.0816723549584,8.85844552518695));
#389637=CARTESIAN_POINT('Ctrl Pts',(2.43570585991415,-1.08223163783065,
8.85759444184123));
#389638=CARTESIAN_POINT('Ctrl Pts',(2.4357866862199,-1.08268406612753,8.85683498915138));
#389639=CARTESIAN_POINT('Ctrl Pts',(2.43579514447754,-1.08273141154388,
8.85675551444997));
#389640=CARTESIAN_POINT('Ctrl Pts',(2.43580397099507,-1.08277757949647,
8.85667699793651));
#389641=CARTESIAN_POINT('Ctrl Pts',(2.4358130862329,-1.08282256237295,8.85659965593547));
#389642=CARTESIAN_POINT('Ctrl Pts',(2.43593612417828,-1.08342974353502,
8.85555568965886));
#389643=CARTESIAN_POINT('Ctrl Pts',(2.43614206024082,-1.08399551313589,
8.85434650606346));
#389644=CARTESIAN_POINT('Ctrl Pts',(2.43642607255145,-1.08452479370297,
8.85297329937117));
#389645=CARTESIAN_POINT('Ctrl Pts',(2.43658581217106,-1.08482248177241,
8.85220095427747));
#389646=CARTESIAN_POINT('Ctrl Pts',(2.43677059316374,-1.08510859961498,
8.85137579139183));
#389647=CARTESIAN_POINT('Ctrl Pts',(2.4369819335138,-1.08538337893279,8.85049129520029));
#389648=CARTESIAN_POINT('Origin',(2.44243149520449,-1.08119197077092,7.59394543036555));
#389649=CARTESIAN_POINT('Ctrl Pts',(2.44131016723206,-1.0743857684413,7.59443877723642));
#389650=CARTESIAN_POINT('Ctrl Pts',(2.43553868906203,-1.0748582442413,7.58783886950016));
#389651=CARTESIAN_POINT('Ctrl Pts',(2.43425469986311,-1.08325053554187,
7.58559994247159));
#389652=CARTESIAN_POINT('Ctrl Pts',(2.47281649723425,-1.07180653691096,
7.56670252222134));
#389653=CARTESIAN_POINT('Ctrl Pts',(2.46705336048877,-1.07227832984929,
7.56004874999028));
#389654=CARTESIAN_POINT('Ctrl Pts',(2.46574064338428,-1.08071711714724,
7.55786368756704));
#389655=CARTESIAN_POINT('Ctrl Pts',(2.50426399231308,-1.06923212183781,
7.53888913333559));
#389656=CARTESIAN_POINT('Ctrl Pts',(2.49846660496369,-1.06970671866468,
7.53222002137277));
#389657=CARTESIAN_POINT('Ctrl Pts',(2.49716881203072,-1.0781871772739,7.53005029815326));
#389658=CARTESIAN_POINT('Ctrl Pts',(2.53565122944802,-1.06666263971587,
7.51101258149734));
#389659=CARTESIAN_POINT('Ctrl Pts',(2.52978356722987,-1.06714298951863,
7.5043616886572));
#389660=CARTESIAN_POINT('Ctrl Pts',(2.52853765964447,-1.07566092329587,
7.50217374673251));
#389661=CARTESIAN_POINT('',(2.526863777558,-1.07579572642895,7.50366116523517));
#389662=CARTESIAN_POINT('Ctrl Pts',(2.52710047532069,-1.06736263792739,
7.51860402984325));
#389663=CARTESIAN_POINT('Ctrl Pts',(2.5275406141597,-1.06732660643876,7.51734760759493));
#389664=CARTESIAN_POINT('Ctrl Pts',(2.52794319693951,-1.06735334527535,
7.51608817408573));
#389665=CARTESIAN_POINT('Ctrl Pts',(2.52830641272849,-1.06745611722427,
7.51481005913119));
#389666=CARTESIAN_POINT('Ctrl Pts',(2.52863542226948,-1.06754921051143,
7.51365231206383));
#389667=CARTESIAN_POINT('Ctrl Pts',(2.52893266240551,-1.06770458075918,
7.51247773061042));
#389668=CARTESIAN_POINT('Ctrl Pts',(2.52917588459346,-1.06795226365132,
7.51129758471022));
#389669=CARTESIAN_POINT('Ctrl Pts',(2.52947818199607,-1.0682601051998,7.50983079813402));
#389670=CARTESIAN_POINT('Ctrl Pts',(2.52967809354277,-1.06870984917593,
7.50839324291155));
#389671=CARTESIAN_POINT('Ctrl Pts',(2.52970174557798,-1.06933826341189,
7.50715379678855));
#389672=CARTESIAN_POINT('Ctrl Pts',(2.52971267213674,-1.06962857268158,
7.50658120839351));
#389673=CARTESIAN_POINT('Ctrl Pts',(2.52967804016154,-1.06999864075055,
7.50598221009429));
#389674=CARTESIAN_POINT('Ctrl Pts',(2.52957602630726,-1.07043754110356,
7.50545747549611));
#389675=CARTESIAN_POINT('Ctrl Pts',(2.52952158855699,-1.07067175191717,
7.50517746087247));
#389676=CARTESIAN_POINT('Ctrl Pts',(2.52944756995091,-1.070928149076,7.50491486231392));
#389677=CARTESIAN_POINT('Ctrl Pts',(2.52935432805342,-1.07119948010878,
7.50468370960992));
#389678=CARTESIAN_POINT('Ctrl Pts',(2.52921490200518,-1.07160520558931,
7.50433806340447));
#389679=CARTESIAN_POINT('Ctrl Pts',(2.52902778596955,-1.07205630799,7.50405484070984));
#389680=CARTESIAN_POINT('Ctrl Pts',(2.52880492013754,-1.07252213192078,
7.50385766036131));
#389681=CARTESIAN_POINT('Ctrl Pts',(2.52878108810092,-1.07257194454964,
7.50383657498791));
#389682=CARTESIAN_POINT('Ctrl Pts',(2.5287568708167,-1.07262190971423,7.50381643264937));
#389683=CARTESIAN_POINT('Ctrl Pts',(2.52873230017347,-1.07267197871409,
7.50379723213559));
#389684=CARTESIAN_POINT('Ctrl Pts',(2.52856828309232,-1.07300620566686,
7.50366906242519));
#389685=CARTESIAN_POINT('Ctrl Pts',(2.52838430707248,-1.07335201295403,
7.50358235568538));
#389686=CARTESIAN_POINT('Ctrl Pts',(2.52819896460948,-1.07368106596533,
7.5035341175365));
#389687=CARTESIAN_POINT('Ctrl Pts',(2.52792106456294,-1.07417444371417,
7.50346178989176));
#389688=CARTESIAN_POINT('Ctrl Pts',(2.52760112950024,-1.07469338991016,
7.50346967198527));
#389689=CARTESIAN_POINT('Ctrl Pts',(2.5272713767736,-1.07519317013139,7.50354272648692));
#389690=CARTESIAN_POINT('Ctrl Pts',(2.52713574265166,-1.07539874008122,
7.50357277531559));
#389691=CARTESIAN_POINT('Ctrl Pts',(2.52699874610053,-1.07560087239687,
7.50361331098761));
#389692=CARTESIAN_POINT('Ctrl Pts',(2.5268637775593,-1.0757957264295,7.50366116523659));
#389693=CARTESIAN_POINT('',(2.44510882695063,-1.08237714611493,7.57603338622103));
#389694=CARTESIAN_POINT('Origin',(2.45318828011514,-1.08595680059038,7.58486873427632));
#389695=CARTESIAN_POINT('Ctrl Pts',(2.52686377761448,-1.07579572641902,
7.50366116529969));
#389696=CARTESIAN_POINT('Ctrl Pts',(2.49965666355486,-1.07798678628757,
7.52783573079709));
#389697=CARTESIAN_POINT('Ctrl Pts',(2.47240630148104,-1.08018050713206,
7.55196141284068));
#389698=CARTESIAN_POINT('Ctrl Pts',(2.44510882811946,-1.08237714566606,
7.57603338728831));
#389699=CARTESIAN_POINT('Ctrl Pts',(2.44272911426497,-1.07441992109173,
7.59642833564546));
#389700=CARTESIAN_POINT('Ctrl Pts',(2.42445489603489,-1.07354713207804,
7.59959882295456));
#389701=CARTESIAN_POINT('Ctrl Pts',(2.43774827562796,-1.08609137277743,
7.59639677331373));
#389702=CARTESIAN_POINT('Ctrl Pts',(2.43897129681562,-1.07360282396487,
7.58710240504251));
#389703=CARTESIAN_POINT('Ctrl Pts',(2.43327446304227,-1.07724431895329,
7.58809943920598));
#389704=CARTESIAN_POINT('Ctrl Pts',(2.43451789319205,-1.08390511263708,
7.58707626057424));
#389705=CARTESIAN_POINT('Ctrl Pts',(2.44213665289714,-1.07877505939748,
7.5802092424413));
#389706=CARTESIAN_POINT('Ctrl Pts',(2.43958612281158,-1.07996748185641,
7.58205880659758));
#389707=CARTESIAN_POINT('Ctrl Pts',(2.44046943008487,-1.08267839307895,
7.58015376756931));
#389708=CARTESIAN_POINT('Ctrl Pts',(2.44510882619397,-1.08237714577975,
7.57603338509286));
#389709=CARTESIAN_POINT('Ctrl Pts',(2.44510882619397,-1.08237714577975,
7.57603338509286));
#389710=CARTESIAN_POINT('Ctrl Pts',(2.44510882619397,-1.08237714577975,
7.57603338509286));
#389711=CARTESIAN_POINT('Origin',(2.45319058995175,-1.08595158263002,7.58486873427622));
#389712=CARTESIAN_POINT('Ctrl Pts',(2.49436399277438,-1.1599900647537,7.51098857897448));
#389713=CARTESIAN_POINT('Ctrl Pts',(2.49077473426271,-1.15532340263734,
7.50433767179956));
#389714=CARTESIAN_POINT('Ctrl Pts',(2.49624278171656,-1.14867445474125,
7.50214974420965));
#389715=CARTESIAN_POINT('Ctrl Pts',(2.47515893410405,-1.13502013866787,
7.53887321589163));
#389716=CARTESIAN_POINT('Ctrl Pts',(2.47161268127914,-1.13040939144548,
7.53220407452058));
#389717=CARTESIAN_POINT('Ctrl Pts',(2.47701807999251,-1.12374721577447,
7.53003438070911));
#389718=CARTESIAN_POINT('Ctrl Pts',(2.45591699463666,-1.11000226111298,
7.56669465659233));
#389719=CARTESIAN_POINT('Ctrl Pts',(2.4523916995066,-1.10541876254948,7.56004085833298));
#389720=CARTESIAN_POINT('Ctrl Pts',(2.45775620401618,-1.09877355815133,
7.55785582193789));
#389721=CARTESIAN_POINT('Ctrl Pts',(2.43663904460805,-1.08493756354742,
7.59443891967696));
#389722=CARTESIAN_POINT('Ctrl Pts',(2.433108638239,-1.08034741948166,7.58783901202978));
#389723=CARTESIAN_POINT('Ctrl Pts',(2.43845803954467,-1.07375476571711,
7.58560008491213));
#389724=CARTESIAN_POINT('',(2.49520067284434,-1.14732323151525,7.50366116523517));
#389725=CARTESIAN_POINT('Ctrl Pts',(2.49520067284468,-1.14732323151541,
7.50366116523554));
#389726=CARTESIAN_POINT('Ctrl Pts',(2.49502946219895,-1.14806135374889,
7.50350835821027));
#389727=CARTESIAN_POINT('Ctrl Pts',(2.49484806402456,-1.14873429707003,
7.50345484956));
#389728=CARTESIAN_POINT('Ctrl Pts',(2.49465166501226,-1.14936222492285,
7.50349758195598));
#389729=CARTESIAN_POINT('Ctrl Pts',(2.49455089775363,-1.14968439847969,
7.50351950684424));
#389730=CARTESIAN_POINT('Ctrl Pts',(2.49443637311436,-1.15002651529797,
7.50357029184312));
#389731=CARTESIAN_POINT('Ctrl Pts',(2.49431687004512,-1.15035337898107,
7.50365515313923));
#389732=CARTESIAN_POINT('Ctrl Pts',(2.49413302593307,-1.15085622768585,
7.50378570417639));
#389733=CARTESIAN_POINT('Ctrl Pts',(2.49393232888108,-1.15133785676729,
7.50400001621911));
#389734=CARTESIAN_POINT('Ctrl Pts',(2.49372795910971,-1.1517607339538,7.50428903009634));
#389735=CARTESIAN_POINT('Ctrl Pts',(2.49370527563742,-1.15180767006808,
7.50432110841318));
#389736=CARTESIAN_POINT('Ctrl Pts',(2.49368255155364,-1.15185391235972,
7.50435406373354));
#389737=CARTESIAN_POINT('Ctrl Pts',(2.49365980799993,-1.15189943166855,
7.50438785222352));
#389738=CARTESIAN_POINT('Ctrl Pts',(2.49352094767258,-1.15217734892832,
7.50459414719561));
#389739=CARTESIAN_POINT('Ctrl Pts',(2.49337868940289,-1.15243250984058,
7.50483629897752));
#389740=CARTESIAN_POINT('Ctrl Pts',(2.49323963252004,-1.15265578011538,
7.5050991045531));
#389741=CARTESIAN_POINT('Ctrl Pts',(2.49293285906953,-1.15314833676698,
7.50567888004914));
#389742=CARTESIAN_POINT('Ctrl Pts',(2.49263001938427,-1.15350537014203,
7.50637912803144));
#389743=CARTESIAN_POINT('Ctrl Pts',(2.49234864839804,-1.15375233499363,
7.50710440483569));
#389744=CARTESIAN_POINT('Ctrl Pts',(2.49227965064622,-1.15381289567818,
7.50728225710685));
#389745=CARTESIAN_POINT('Ctrl Pts',(2.49221066660843,-1.15386815290563,
7.50746498566954));
#389746=CARTESIAN_POINT('Ctrl Pts',(2.49214356704021,-1.15391714193709,
7.50764697238949));
#389747=CARTESIAN_POINT('Ctrl Pts',(2.49178285822775,-1.15418049348805,
7.50862528291181));
#389748=CARTESIAN_POINT('Ctrl Pts',(2.49144630392676,-1.15428995340171,
7.50965856837421));
#389749=CARTESIAN_POINT('Ctrl Pts',(2.4911367136329,-1.15431175990401,7.51067959873201));
#389750=CARTESIAN_POINT('Ctrl Pts',(2.49096634570369,-1.15432376004973,
7.51124147302578));
#389751=CARTESIAN_POINT('Ctrl Pts',(2.49080407122457,-1.15430878557774,
7.51180065547253));
#389752=CARTESIAN_POINT('Ctrl Pts',(2.49065026658073,-1.15427516054053,
7.51235175716501));
#389753=CARTESIAN_POINT('Ctrl Pts',(2.49011881026774,-1.15415897264232,
7.51425603304536));
#389754=CARTESIAN_POINT('Ctrl Pts',(2.48962641095044,-1.15380032331499,
7.51626900505181));
#389755=CARTESIAN_POINT('Ctrl Pts',(2.48918772654823,-1.15325776008449,
7.51827788969245));
#389756=CARTESIAN_POINT('Ctrl Pts',(2.48916398411938,-1.15322839553715,
7.51838661432546));
#389757=CARTESIAN_POINT('Ctrl Pts',(2.48914039945448,-1.15319848232018,
7.51849533314857));
#389758=CARTESIAN_POINT('Ctrl Pts',(2.48911697509583,-1.15316802656818,
7.51860402984325));
#389759=CARTESIAN_POINT('Ctrl Pts',(2.44510882740513,-1.08237714728266,
7.57603338728985));
#389760=CARTESIAN_POINT('Ctrl Pts',(2.46183481987757,-1.10406166823482,
7.55196141284922));
#389761=CARTESIAN_POINT('Ctrl Pts',(2.47853129930077,-1.12570935218487,
7.52783573083104));
#389762=CARTESIAN_POINT('Ctrl Pts',(2.49520067287603,-1.14732323156524,
7.50366116530176));
#389763=CARTESIAN_POINT('Origin',(8.44898126352703E-16,-3.74011337523904E-16,
7.49482233047033));
#389764=CARTESIAN_POINT('Origin',(2.5187313027445,-1.07233337846727,7.49482233047033));
#389765=CARTESIAN_POINT('Origin',(0.,0.,7.50366116523517));
#389766=CARTESIAN_POINT('Origin',(2.48717010277295,-1.14363067896608,7.49482233047033));
#389767=CARTESIAN_POINT('Ctrl Pts',(2.52709942112331,-1.06736272418322,
7.51860402984325));
#389768=CARTESIAN_POINT('Ctrl Pts',(2.53468306548395,-1.06674254336973,
7.51860402984325));
#389769=CARTESIAN_POINT('Ctrl Pts',(2.53761520271997,-1.05972122887319,
7.51860402984325));
#389770=CARTESIAN_POINT('Ctrl Pts',(2.52991527992432,-1.06713244554834,
7.51041458714367));
#389771=CARTESIAN_POINT('Ctrl Pts',(2.53537771324442,-1.06507910972981,
7.51004642900443));
#389772=CARTESIAN_POINT('Ctrl Pts',(2.5376160113686,-1.05971929247802,7.5072913648301));
#389773=CARTESIAN_POINT('Ctrl Pts',(2.5310984519589,-1.06968662665701,7.50215815450137));
#389774=CARTESIAN_POINT('Ctrl Pts',(2.53396347064419,-1.06846608070767,
7.49877163671529));
#389775=CARTESIAN_POINT('Ctrl Pts',(2.53531500022192,-1.06529160572826,
7.4948158853317));
#389776=CARTESIAN_POINT('Ctrl Pts',(2.52686327103472,-1.07579551078049,
7.50366171572174));
#389777=CARTESIAN_POINT('Ctrl Pts',(2.53023235892126,-1.07722987791268,
7.50000045605858));
#389778=CARTESIAN_POINT('Ctrl Pts',(2.53023235892131,-1.07722987791257,
7.49482233047317));
#389779=CARTESIAN_POINT('Origin',(2.52608058816215,-1.0549043141965,7.51860402984325));
#389780=CARTESIAN_POINT('Origin',(2.52608058816215,-1.0549043141965,9.));
#389781=CARTESIAN_POINT('Origin',(2.52608058816215,-1.0549043141965,8.75721825406948));
#389782=CARTESIAN_POINT('Ctrl Pts',(2.51045599178025,-1.06872519020653,
8.78942910404913));
#389783=CARTESIAN_POINT('Ctrl Pts',(2.51601149551951,-1.06829067104139,
8.79672699501691));
#389784=CARTESIAN_POINT('Ctrl Pts',(2.51696148514411,-1.0594153679088,8.79893251111267));
#389785=CARTESIAN_POINT('Ctrl Pts',(2.52141367167525,-1.06782815617216,
8.78111911759577));
#389786=CARTESIAN_POINT('Ctrl Pts',(2.52799920529107,-1.06730560749445,
8.78644465894813));
#389787=CARTESIAN_POINT('Ctrl Pts',(2.53057060301399,-1.05961773226614,
8.78817647674131));
#389788=CARTESIAN_POINT('Ctrl Pts',(2.52824275914858,-1.06726910313394,
8.76780923932033));
#389789=CARTESIAN_POINT('Ctrl Pts',(2.53601630044145,-1.06664717666037,
8.76988516158374));
#389790=CARTESIAN_POINT('Ctrl Pts',(2.53907079036638,-1.0597329542388,8.77093053738834));
#389791=CARTESIAN_POINT('Ctrl Pts',(2.52691118055377,-1.06737811082349,
8.75371302330491));
#389792=CARTESIAN_POINT('Ctrl Pts',(2.53449399556177,-1.06677220825513,
8.75300828287559));
#389793=CARTESIAN_POINT('Ctrl Pts',(2.53741291480575,-1.05971002376437,
8.75267964240737));
#389794=CARTESIAN_POINT('Origin',(2.51210475973992,-1.05604843023054,8.78727029226991));
#389795=CARTESIAN_POINT('Ctrl Pts',(2.44187055726729,-1.07433989271893,
8.85049129520029));
#389796=CARTESIAN_POINT('Ctrl Pts',(2.44769070315535,-1.07386343278898,
8.85711686593484));
#389797=CARTESIAN_POINT('Ctrl Pts',(2.44895572090757,-1.06540763642197,
8.85933012996512));
#389798=CARTESIAN_POINT('Ctrl Pts',(2.46565647730585,-1.07239268417584,
8.82945683644723));
#389799=CARTESIAN_POINT('Ctrl Pts',(2.4715249339237,-1.07191226934043,8.8360746990239));
#389800=CARTESIAN_POINT('Ctrl Pts',(2.47275657607163,-1.06342609822989,
8.8382956714852));
#389801=CARTESIAN_POINT('Ctrl Pts',(2.48940694251249,-1.07044837810411,
8.80838214965003));
#389802=CARTESIAN_POINT('Ctrl Pts',(2.49529855880008,-1.06996606732744,
8.81501364461988));
#389803=CARTESIAN_POINT('Ctrl Pts',(2.49652138203833,-1.06144823216095,
8.81722098428721));
#389804=CARTESIAN_POINT('Ctrl Pts',(2.51312464689845,-1.06850675396143,
8.78727029226991));
#389805=CARTESIAN_POINT('Ctrl Pts',(2.51901724180287,-1.06802436307135,
8.79393457792714));
#389806=CARTESIAN_POINT('Ctrl Pts',(2.52025288996717,-1.05947377310385,
8.79610912703474));
#389807=CARTESIAN_POINT('Origin',(2.44085067010875,-1.06188156898803,8.85049129520029));
#389808=CARTESIAN_POINT('Ctrl Pts',(2.4369819335138,-1.08538337893279,8.85049129520029));
#389809=CARTESIAN_POINT('Ctrl Pts',(2.44054210997316,-1.09001222930856,
8.85711686593484));
#389810=CARTESIAN_POINT('Ctrl Pts',(2.43513294253592,-1.09663353354185,
8.85933012996512));
#389811=CARTESIAN_POINT('Ctrl Pts',(2.43383229679189,-1.08128830182351,
8.8633249698723));
#389812=CARTESIAN_POINT('Ctrl Pts',(2.43222348092875,-1.08561999963098,
8.86648636486735));
#389813=CARTESIAN_POINT('Ctrl Pts',(2.42633528580379,-1.08516694327358,
8.87206031107458));
#389814=CARTESIAN_POINT('Ctrl Pts',(2.43668656914299,-1.07476427428359,
8.86341338519877));
#389815=CARTESIAN_POINT('Ctrl Pts',(2.4387913293493,-1.07063590231533,8.86654584966058));
#389816=CARTESIAN_POINT('Ctrl Pts',(2.43444148071613,-1.06661061106431,
8.87215952290713));
#389817=CARTESIAN_POINT('Ctrl Pts',(2.44187055726729,-1.07433989271893,
8.85049129520029));
#389818=CARTESIAN_POINT('Ctrl Pts',(2.44769070315535,-1.07386343278898,
8.85711686593484));
#389819=CARTESIAN_POINT('Ctrl Pts',(2.44895572090757,-1.06540763642197,
8.85933012996512));
#389820=CARTESIAN_POINT('Origin',(2.42707363953072,-1.09300412104527,8.85049129520029));
#389821=CARTESIAN_POINT('Ctrl Pts',(2.48056797713153,-1.14205283806805,
8.78727029226991));
#389822=CARTESIAN_POINT('Ctrl Pts',(2.4841724705698,-1.14673930824632,8.79393457792714));
#389823=CARTESIAN_POINT('Ctrl Pts',(2.47867338431575,-1.15340260064189,
8.79610912703474));
#389824=CARTESIAN_POINT('Ctrl Pts',(2.4660598849893,-1.12318978773031,8.80838214965003));
#389825=CARTESIAN_POINT('Ctrl Pts',(2.46966377980884,-1.12787547959981,
8.81501364461995));
#389826=CARTESIAN_POINT('Ctrl Pts',(2.46418031900404,-1.13450725690287,
8.81722098428722));
#389827=CARTESIAN_POINT('Ctrl Pts',(2.45153175309124,-1.10430068221456,
8.82945683644722));
#389828=CARTESIAN_POINT('Ctrl Pts',(2.45512148116773,-1.10896795484711,
8.83607469902388));
#389829=CARTESIAN_POINT('Ctrl Pts',(2.44966738952776,-1.11558497282199,
8.83829567148519));
#389830=CARTESIAN_POINT('Ctrl Pts',(2.4369819335138,-1.08538337893279,8.85049129520029));
#389831=CARTESIAN_POINT('Ctrl Pts',(2.44054210997316,-1.09001222930856,
8.85711686593484));
#389832=CARTESIAN_POINT('Ctrl Pts',(2.43513294253592,-1.09663353354185,
8.85933012996512));
#389833=CARTESIAN_POINT('Origin',(2.47065968314845,-1.14967358018053,8.78727029226991));
#389834=CARTESIAN_POINT('Ctrl Pts',(2.48900407525589,-1.15302126734185,
8.75374538247847));
#389835=CARTESIAN_POINT('Ctrl Pts',(2.49364725474232,-1.15903668608408,
8.75304829418602));
#389836=CARTESIAN_POINT('Ctrl Pts',(2.49039024421335,-1.16594049123944,
8.75272238421917));
#389837=CARTESIAN_POINT('Ctrl Pts',(2.48980881601113,-1.15406756998971,
8.76769408445022));
#389838=CARTESIAN_POINT('Ctrl Pts',(2.49456829219993,-1.16023478503221,
8.7697431809397));
#389839=CARTESIAN_POINT('Ctrl Pts',(2.49150955440295,-1.16713858691014,
8.7707786988043));
#389840=CARTESIAN_POINT('Ctrl Pts',(2.48568417334205,-1.14870481864703,
8.78108014887987));
#389841=CARTESIAN_POINT('Ctrl Pts',(2.48972066580186,-1.15392898996142,
8.78639403366324));
#389842=CARTESIAN_POINT('Ctrl Pts',(2.48578137048604,-1.1610003426003,8.7881222417474));
#389843=CARTESIAN_POINT('Ctrl Pts',(2.47892479450374,-1.13991645305727,
8.78944554828686));
#389844=CARTESIAN_POINT('Ctrl Pts',(2.48233103024035,-1.14431576842715,
8.79673892988686));
#389845=CARTESIAN_POINT('Ctrl Pts',(2.47640778743176,-1.15098050765289,
8.79894799272499));
#389846=CARTESIAN_POINT('Origin',(2.47920868111276,-1.16078876868065,8.75721825406948));
#389847=CARTESIAN_POINT('Origin',(2.47920868111276,-1.16078876868065,9.));
#389848=CARTESIAN_POINT('Origin',(2.47920868111276,-1.16078876868065,7.51860402984325));
#389849=CARTESIAN_POINT('Ctrl Pts',(2.4951999581168,-1.14732290287501,7.50366195182966));
#389850=CARTESIAN_POINT('Ctrl Pts',(2.49852704388144,-1.14885273686103,
7.50000065167735));
#389851=CARTESIAN_POINT('Ctrl Pts',(2.4985270438814,-1.14885273686113,7.49482233047108));
#389852=CARTESIAN_POINT('Ctrl Pts',(2.49352263939498,-1.15457137868114,
7.50215800491337));
#389853=CARTESIAN_POINT('Ctrl Pts',(2.49454432099785,-1.15751431325002,
7.49877273257263));
#389854=CARTESIAN_POINT('Ctrl Pts',(2.49310216742008,-1.1606507681609,7.49481816995647));
#389855=CARTESIAN_POINT('Ctrl Pts',(2.49083562085213,-1.15540200958143,
7.51043025814042));
#389856=CARTESIAN_POINT('Ctrl Pts',(2.49299264991785,-1.16082787196419,
7.51006209594515));
#389857=CARTESIAN_POINT('Ctrl Pts',(2.49052819510455,-1.16609146699378,
7.50731281821699));
#389858=CARTESIAN_POINT('Ctrl Pts',(2.4891160535797,-1.15316682858634,7.51860402984325));
#389859=CARTESIAN_POINT('Ctrl Pts',(2.49375584668795,-1.15919785978368,
7.51860402984325));
#389860=CARTESIAN_POINT('Ctrl Pts',(2.49052926869775,-1.1660891740171,7.51860402984325));
#389861=CARTESIAN_POINT('Origin',(0.,0.,7.5));
#389862=CARTESIAN_POINT('Origin',(2.36243414091427,-1.23929131094302,7.5));
#389863=CARTESIAN_POINT('',(2.36243414091427,-1.23929131094302,7.59394543036555));
#389864=CARTESIAN_POINT('',(2.36243414091427,-1.23929131094302,8.85049129520029));
#389865=CARTESIAN_POINT('',(2.36243414091427,-1.23929131094302,7.5));
#389866=CARTESIAN_POINT('',(2.40229980761781,-1.29863690399938,8.78727029226991));
#389867=CARTESIAN_POINT('Ctrl Pts',(2.36243414091427,-1.23929131094302,
8.85049129520029));
#389868=CARTESIAN_POINT('Ctrl Pts',(2.37574201268456,-1.25910193015075,
8.82945686509571));
#389869=CARTESIAN_POINT('Ctrl Pts',(2.3890301006943,-1.27888309847755,8.80838212259895));
#389870=CARTESIAN_POINT('Ctrl Pts',(2.40229980761781,-1.29863690399938,
8.78727029226991));
#389871=CARTESIAN_POINT('',(2.41011908817659,-1.31027699133282,8.75721825406948));
#389872=CARTESIAN_POINT('Origin',(2.38658832796362,-1.27524781804343,8.75937679713138));
#389873=CARTESIAN_POINT('',(2.41011908817659,-1.31027699133282,7.51860402984325));
#389874=CARTESIAN_POINT('',(2.41011908817659,-1.31027699133282,7.5));
#389875=CARTESIAN_POINT('Ctrl Pts',(2.41011908817659,-1.31027699133282,
7.51860402984325));
#389876=CARTESIAN_POINT('Ctrl Pts',(2.40397825942583,-1.30113551310842,
7.52834476460825));
#389877=CARTESIAN_POINT('Ctrl Pts',(2.39783344413766,-1.29198810036826,
7.53807742314407));
#389878=CARTESIAN_POINT('Ctrl Pts',(2.39168450845877,-1.28283455385309,
7.54780169004674));
#389879=CARTESIAN_POINT('Ctrl Pts',(2.38194492666503,-1.26833583088004,
7.5632044032688));
#389880=CARTESIAN_POINT('Ctrl Pts',(2.37219499495819,-1.25382170062096,
7.57858609112103));
#389881=CARTESIAN_POINT('Ctrl Pts',(2.36243414091427,-1.23929131094302,
7.59394543036555));
#389882=CARTESIAN_POINT('Origin',(2.64297784464841,-1.2237528786782,7.5));
#389883=CARTESIAN_POINT('',(2.45352211735226,-1.22708151028065,8.75721825406948));
#389884=CARTESIAN_POINT('',(2.43950170000244,-1.22732784120416,8.78727029226991));
#389885=CARTESIAN_POINT('Origin',(2.40391265141233,-1.22795312096492,8.75658640621001));
#389886=CARTESIAN_POINT('',(2.36802027905703,-1.22858372995529,8.85049129520029));
#389887=CARTESIAN_POINT('Ctrl Pts',(2.43950170000244,-1.22732784120416,
8.78727029226991));
#389888=CARTESIAN_POINT('Ctrl Pts',(2.41570835638485,-1.22774587699872,
8.80838212259895));
#389889=CARTESIAN_POINT('Ctrl Pts',(2.39188205442815,-1.22816449185294,
8.82945686509571));
#389890=CARTESIAN_POINT('Ctrl Pts',(2.36802027905703,-1.22858372995529,
8.85049129520029));
#389891=CARTESIAN_POINT('',(2.36802027905703,-1.22858372995529,7.59394543036555));
#389892=CARTESIAN_POINT('',(2.36802027905703,-1.22858372995529,7.5));
#389893=CARTESIAN_POINT('',(2.45352211735226,-1.22708151028065,7.51860402984325));
#389894=CARTESIAN_POINT('Ctrl Pts',(2.36802027905703,-1.22858372995529,
7.59394543036555));
#389895=CARTESIAN_POINT('Ctrl Pts',(2.38552204873491,-1.22827623361047,
7.57858609112103));
#389896=CARTESIAN_POINT('Ctrl Pts',(2.40300423403734,-1.22796908135223,
7.56320440326857));
#389897=CARTESIAN_POINT('Ctrl Pts',(2.42046786135375,-1.22766225514746,
7.54780169004651));
#389898=CARTESIAN_POINT('Ctrl Pts',(2.43149325478056,-1.22746854512605,
7.53807742314383));
#389899=CARTESIAN_POINT('Ctrl Pts',(2.44251126011133,-1.22727496490937,
7.52834476460825));
#389900=CARTESIAN_POINT('Ctrl Pts',(2.45352211735226,-1.22708151028065,
7.51860402984325));
#389901=CARTESIAN_POINT('',(2.45352211735226,-1.22708151028065,7.5));
#389902=CARTESIAN_POINT('Origin',(2.36814105033896,-1.23545766909507,7.5));
#389903=CARTESIAN_POINT('Ctrl Pts',(2.36802027905703,-1.22858372995529,
8.85049129520029));
#389904=CARTESIAN_POINT('Ctrl Pts',(2.36782664743443,-1.22858713195504,
8.85097269580138));
#389905=CARTESIAN_POINT('Ctrl Pts',(2.36763560659413,-1.22859890114681,
8.85143669361005));
#389906=CARTESIAN_POINT('Ctrl Pts',(2.36743841348188,-1.22862045209506,
8.8519052845931));
#389907=CARTESIAN_POINT('Ctrl Pts',(2.36705271625984,-1.22866260438311,
8.85282181883899));
#389908=CARTESIAN_POINT('Ctrl Pts',(2.36665342562342,-1.22874128994967,
8.85372622499636));
#389909=CARTESIAN_POINT('Ctrl Pts',(2.36623725715284,-1.22887287130626,
8.85462257735071));
#389910=CARTESIAN_POINT('Ctrl Pts',(2.36589176886947,-1.22898210547517,
8.85536669723986));
#389911=CARTESIAN_POINT('Ctrl Pts',(2.36553456053145,-1.22912778877099,
8.85610498449051));
#389912=CARTESIAN_POINT('Ctrl Pts',(2.36516674476246,-1.22932670510119,
8.8568133821837));
#389913=CARTESIAN_POINT('Ctrl Pts',(2.36483295137445,-1.22950722198325,
8.85745625420284));
#389914=CARTESIAN_POINT('Ctrl Pts',(2.36448595034558,-1.22973331737552,
8.85808743050665));
#389915=CARTESIAN_POINT('Ctrl Pts',(2.36412948034975,-1.23003334385224,
8.85866804508409));
#389916=CARTESIAN_POINT('Ctrl Pts',(2.36396501282099,-1.23017176956482,
8.85893592806395));
#389917=CARTESIAN_POINT('Ctrl Pts',(2.36379858976412,-1.23032616777317,
8.85919241173848));
#389918=CARTESIAN_POINT('Ctrl Pts',(2.36363118640838,-1.23050079886513,
8.85943017985534));
#389919=CARTESIAN_POINT('Ctrl Pts',(2.36340514232144,-1.23073660253561,
8.8597512372));
#389920=CARTESIAN_POINT('Ctrl Pts',(2.36317201985187,-1.23101574189601,
8.86004599534706));
#389921=CARTESIAN_POINT('Ctrl Pts',(2.36294261383862,-1.2313415393257,8.86026130871721));
#389922=CARTESIAN_POINT('Ctrl Pts',(2.36285862182954,-1.23146082294991,
8.86034014101235));
#389923=CARTESIAN_POINT('Ctrl Pts',(2.36277385628191,-1.23158814575575,
8.86040910639693));
#389924=CARTESIAN_POINT('Ctrl Pts',(2.36269090658754,-1.23172022531703,
8.86046313645507));
#389925=CARTESIAN_POINT('Ctrl Pts',(2.36256146428415,-1.23192633436625,
8.8605474499083));
#389926=CARTESIAN_POINT('Ctrl Pts',(2.36243303496201,-1.23214973111174,
8.86059655985668));
#389927=CARTESIAN_POINT('Ctrl Pts',(2.3623136012062,-1.23237594242963,8.86059725258816));
#389928=CARTESIAN_POINT('Ctrl Pts',(2.36219389151071,-1.23260267638603,
8.86059794692011));
#389929=CARTESIAN_POINT('Ctrl Pts',(2.36208424081918,-1.23283599287139,
8.86056369958366));
#389930=CARTESIAN_POINT('Ctrl Pts',(2.36198722379488,-1.23306156611176,
8.86048590497774));
#389931=CARTESIAN_POINT('Ctrl Pts',(2.36196190524008,-1.23312043401138,
8.86046560290182));
#389932=CARTESIAN_POINT('Ctrl Pts',(2.36193720093637,-1.23317957617911,
8.86044257503091));
#389933=CARTESIAN_POINT('Ctrl Pts',(2.36191384397732,-1.23323715242064,
8.86041778462583));
#389934=CARTESIAN_POINT('Ctrl Pts',(2.36175668062649,-1.23362456907998,
8.860250975962));
#389935=CARTESIAN_POINT('Ctrl Pts',(2.36163973822465,-1.23399319749297,
8.8599848982295));
#389936=CARTESIAN_POINT('Ctrl Pts',(2.36155835415756,-1.23432971640827,
8.85968173251461));
#389937=CARTESIAN_POINT('Ctrl Pts',(2.36151530664883,-1.23450771563423,
8.85952137522076));
#389938=CARTESIAN_POINT('Ctrl Pts',(2.36148119228362,-1.23468011742878,
8.85934740853961));
#389939=CARTESIAN_POINT('Ctrl Pts',(2.36145496716656,-1.23484418878627,
8.8591675900182));
#389940=CARTESIAN_POINT('Ctrl Pts',(2.36134965969003,-1.23550302056916,
8.85844552518695));
#389941=CARTESIAN_POINT('Ctrl Pts',(2.36136262189043,-1.23606428711475,
8.85759444184125));
#389942=CARTESIAN_POINT('Ctrl Pts',(2.36141429494935,-1.23652096440835,
8.8568349891514));
#389943=CARTESIAN_POINT('Ctrl Pts',(2.36141970239735,-1.2365687544709,8.85675551444999));
#389944=CARTESIAN_POINT('Ctrl Pts',(2.36142555278898,-1.2366153930834,8.85667699793652));
#389945=CARTESIAN_POINT('Ctrl Pts',(2.36143176723579,-1.23666086755304,
8.85659965593547));
#389946=CARTESIAN_POINT('Ctrl Pts',(2.36151565015589,-1.23727468426451,
8.85555568965886));
#389947=CARTESIAN_POINT('Ctrl Pts',(2.36168491411791,-1.23785248579989,
8.85434650606346));
#389948=CARTESIAN_POINT('Ctrl Pts',(2.36193443177243,-1.2383988756345,8.85297329937117));
#389949=CARTESIAN_POINT('Ctrl Pts',(2.36207477024977,-1.23870618662444,
8.85220095427747));
#389950=CARTESIAN_POINT('Ctrl Pts',(2.36224083995696,-1.23900355556607,
8.85137579139183));
#389951=CARTESIAN_POINT('Ctrl Pts',(2.36243414091427,-1.23929131094302,
8.85049129520029));
#389952=CARTESIAN_POINT('Origin',(2.36814105033896,-1.23545766909507,7.59394543036555));
#389953=CARTESIAN_POINT('Ctrl Pts',(2.36745810113561,-1.22859360710823,
7.59443877723642));
#389954=CARTESIAN_POINT('Ctrl Pts',(2.36166820945803,-1.22869533228006,
7.58783886950016));
#389955=CARTESIAN_POINT('Ctrl Pts',(2.35984916240285,-1.23698811524766,
7.58559994247159));
#389956=CARTESIAN_POINT('Ctrl Pts',(2.39906494993534,-1.22803829237972,
7.56670252222139));
#389957=CARTESIAN_POINT('Ctrl Pts',(2.39328342629499,-1.22813987052987,
7.56004874999027));
#389958=CARTESIAN_POINT('Ctrl Pts',(2.39143273135005,-1.23647721336053,
7.55786368756704));
#389959=CARTESIAN_POINT('Ctrl Pts',(2.43061277610281,-1.22748401464598,
7.5388891333356));
#389960=CARTESIAN_POINT('Ctrl Pts',(2.4247968925844,-1.22758619647998,7.53222002137277));
#389961=CARTESIAN_POINT('Ctrl Pts',(2.42295842125756,-1.23596608119878,
7.53005029815326));
#389962=CARTESIAN_POINT('Ctrl Pts',(2.46210015207758,-1.22693079898846,
7.51101258149734));
#389963=CARTESIAN_POINT('Ctrl Pts',(2.45621376948322,-1.22703421945195,
7.5043616886572));
#389964=CARTESIAN_POINT('Ctrl Pts',(2.4544246758577,-1.23545482664762,7.50217374673251));
#389965=CARTESIAN_POINT('',(2.4527455960751,-1.2354821068197,7.50366116523517));
#389966=CARTESIAN_POINT('Ctrl Pts',(2.45352211735226,-1.22708151028065,
7.51860402984325));
#389967=CARTESIAN_POINT('Ctrl Pts',(2.45396366042423,-1.22707375261481,
7.51734760759493));
#389968=CARTESIAN_POINT('Ctrl Pts',(2.45436370289139,-1.22712623008085,
7.51608817408572));
#389969=CARTESIAN_POINT('Ctrl Pts',(2.45471958779321,-1.22725206218929,
7.51481005913119));
#389970=CARTESIAN_POINT('Ctrl Pts',(2.45504195684142,-1.22736604391997,
7.51365231206383));
#389971=CARTESIAN_POINT('Ctrl Pts',(2.45532863165976,-1.22754013918379,
7.51247773061042));
#389972=CARTESIAN_POINT('Ctrl Pts',(2.45555548502426,-1.22780289648395,
7.51129758471022));
#389973=CARTESIAN_POINT('Ctrl Pts',(2.4558374378487,-1.22812947380003,7.50983079813402));
#389974=CARTESIAN_POINT('Ctrl Pts',(2.4560081234602,-1.2285911021057,7.50839324291155));
#389975=CARTESIAN_POINT('Ctrl Pts',(2.45599146426144,-1.22921974058831,
7.50715379678855));
#389976=CARTESIAN_POINT('Ctrl Pts',(2.45598376819163,-1.2295101534535,7.50658120839351));
#389977=CARTESIAN_POINT('Ctrl Pts',(2.45592549702895,-1.22987724229966,
7.50598221009429));
#389978=CARTESIAN_POINT('Ctrl Pts',(2.45579557233092,-1.23030870483474,
7.50545747549611));
#389979=CARTESIAN_POINT('Ctrl Pts',(2.4557262404905,-1.23053894659848,7.50517746087247));
#389980=CARTESIAN_POINT('Ctrl Pts',(2.45563594654121,-1.23079007457347,
7.50491486231392));
#389981=CARTESIAN_POINT('Ctrl Pts',(2.45552551198024,-1.23105487409866,
7.50468370960992));
#389982=CARTESIAN_POINT('Ctrl Pts',(2.45536037747697,-1.2314508329151,7.50433806340446));
#389983=CARTESIAN_POINT('Ctrl Pts',(2.45514474366126,-1.23188901991197,
7.50405484070983));
#389984=CARTESIAN_POINT('Ctrl Pts',(2.45489249028928,-1.23233960769465,
7.5038576603613));
#389985=CARTESIAN_POINT('Ctrl Pts',(2.45486551571206,-1.23238779105428,
7.50383657498791));
#389986=CARTESIAN_POINT('Ctrl Pts',(2.45483814690575,-1.23243610195335,
7.50381643264937));
#389987=CARTESIAN_POINT('Ctrl Pts',(2.45481041881372,-1.23248449383456,
7.50379723213559));
#389988=CARTESIAN_POINT('Ctrl Pts',(2.45462532472886,-1.23280752547174,
7.50366906242519));
#389989=CARTESIAN_POINT('Ctrl Pts',(2.45441957075853,-1.23314083487669,
7.50358235568538));
#389990=CARTESIAN_POINT('Ctrl Pts',(2.45421352660268,-1.23345733688091,
7.5035341175365));
#389991=CARTESIAN_POINT('Ctrl Pts',(2.45390458671068,-1.23393189581513,
7.50346178989176));
#389992=CARTESIAN_POINT('Ctrl Pts',(2.45355205999195,-1.23442927747066,
7.50346967198527));
#389993=CARTESIAN_POINT('Ctrl Pts',(2.45319096374894,-1.23490690351009,
7.50354272648692));
#389994=CARTESIAN_POINT('Ctrl Pts',(2.45304243738994,-1.23510336098639,
7.50357277531559));
#389995=CARTESIAN_POINT('Ctrl Pts',(2.45289277165099,-1.23529630060034,
7.50361331098761));
#389996=CARTESIAN_POINT('Ctrl Pts',(2.45274559607637,-1.23548210682034,
7.50366116523658));
#389997=CARTESIAN_POINT('',(2.37073694677488,-1.23681194660316,7.57603338622103));
#389998=CARTESIAN_POINT('Origin',(2.37857045058689,-1.24090189863638,7.58486873427626));
#389999=CARTESIAN_POINT('Ctrl Pts',(2.4527455961321,-1.23548210681342,7.50366116529969));
#390000=CARTESIAN_POINT('Ctrl Pts',(2.4254540003185,-1.23592549913165,7.52783573079709));
#390001=CARTESIAN_POINT('Ctrl Pts',(2.39811907485908,-1.23636877604875,
7.55196141284068));
#390002=CARTESIAN_POINT('Ctrl Pts',(2.37073694797006,-1.2368119462301,7.57603338728831));
#390003=CARTESIAN_POINT('Ctrl Pts',(2.36905161742718,-1.22874145340458,
7.59639677331371));
#390004=CARTESIAN_POINT('Ctrl Pts',(2.35095584851581,-1.22616947687808,
7.59959882295464));
#390005=CARTESIAN_POINT('Ctrl Pts',(2.36303201114798,-1.239912660959,7.59642833564546));
#390006=CARTESIAN_POINT('Ctrl Pts',(2.3653282199157,-1.22757894961742,7.58707626057423));
#390007=CARTESIAN_POINT('Ctrl Pts',(2.35934533569769,-1.23075973371418,
7.58809943920598));
#390008=CARTESIAN_POINT('Ctrl Pts',(2.36005021803306,-1.23748413269744,
7.58710240504251));
#390009=CARTESIAN_POINT('Ctrl Pts',(2.36807985450295,-1.23299689566364,
7.58015376756929));
#390010=CARTESIAN_POINT('Ctrl Pts',(2.36540964568615,-1.23399652372966,
7.58205880659761));
#390011=CARTESIAN_POINT('Ctrl Pts',(2.36606760176506,-1.23673407169023,
7.58020924244128));
#390012=CARTESIAN_POINT('Ctrl Pts',(2.37073694604125,-1.23681194622019,
7.57603338509286));
#390013=CARTESIAN_POINT('Ctrl Pts',(2.37073694604125,-1.23681194622019,
7.57603338509286));
#390014=CARTESIAN_POINT('Ctrl Pts',(2.37073694604125,-1.23681194622019,
7.57603338509286));
#390015=CARTESIAN_POINT('Origin',(2.37857308999301,-1.24089683938831,7.58486873427622));
#390016=CARTESIAN_POINT('Ctrl Pts',(2.41491823580731,-1.31742119048614,
7.51098857897448));
#390017=CARTESIAN_POINT('Ctrl Pts',(2.41163534588057,-1.31253415194519,
7.50433767179957));
#390018=CARTESIAN_POINT('Ctrl Pts',(2.41751815819882,-1.30624920402888,
7.50214974420965));
#390019=CARTESIAN_POINT('Ctrl Pts',(2.39735246464699,-1.29127209545774,
7.53887321589167));
#390020=CARTESIAN_POINT('Ctrl Pts',(2.39410890956768,-1.28644361231143,
7.53220407452063));
#390021=CARTESIAN_POINT('Ctrl Pts',(2.39993004937041,-1.2801414498795,7.53003438070911));
#390022=CARTESIAN_POINT('Ctrl Pts',(2.37975296072629,-1.26507278452087,
7.56669465659228));
#390023=CARTESIAN_POINT('Ctrl Pts',(2.37652857445443,-1.26027283681224,
7.56004085833293));
#390024=CARTESIAN_POINT('Ctrl Pts',(2.38230781672176,-1.25398499068329,
7.55785582193789));
#390025=CARTESIAN_POINT('Ctrl Pts',(2.36212052000037,-1.23882444256556,
7.59443891967696));
#390026=CARTESIAN_POINT('Ctrl Pts',(2.35889145876987,-1.23401753553038,
7.58783901202978));
#390027=CARTESIAN_POINT('Ctrl Pts',(2.36465226193379,-1.22778116439847,
7.58560008491213));
#390028=CARTESIAN_POINT('',(2.41656476362039,-1.30483398889123,7.50366116523517));
#390029=CARTESIAN_POINT('Ctrl Pts',(2.41656476362071,-1.30483398889141,
7.50366116523554));
#390030=CARTESIAN_POINT('Ctrl Pts',(2.41634661309174,-1.30555962506986,
7.50350835821027));
#390031=CARTESIAN_POINT('Ctrl Pts',(2.41612247199273,-1.30621956353584,
7.50345484956));
#390032=CARTESIAN_POINT('Ctrl Pts',(2.41588624502761,-1.30683361791562,
7.50349758195598));
#390033=CARTESIAN_POINT('Ctrl Pts',(2.41576504307546,-1.30714867335191,
7.50351950684424));
#390034=CARTESIAN_POINT('Ctrl Pts',(2.41562883423954,-1.30748274963566,
7.50357029184312));
#390035=CARTESIAN_POINT('Ctrl Pts',(2.4154886344741,-1.30780128515433,7.50365515313923));
#390036=CARTESIAN_POINT('Ctrl Pts',(2.41527295046236,-1.30829132176982,
7.50378570417639));
#390037=CARTESIAN_POINT('Ctrl Pts',(2.41504180768278,-1.30875910258838,
7.50400001621911));
#390038=CARTESIAN_POINT('Ctrl Pts',(2.41481076397667,-1.30916801691215,
7.50428903009634));
#390039=CARTESIAN_POINT('Ctrl Pts',(2.41478511990283,-1.30921340325609,
7.50432110841318));
#390040=CARTESIAN_POINT('Ctrl Pts',(2.41475947975433,-1.30925809460094,
7.50435406373354));
#390041=CARTESIAN_POINT('Ctrl Pts',(2.41473386649755,-1.30930206320098,
7.50438785222352));
#390042=CARTESIAN_POINT('Ctrl Pts',(2.41457748525367,-1.30957051263821,
7.50459414719561));
#390043=CARTESIAN_POINT('Ctrl Pts',(2.41441917105307,-1.30981603477638,
7.50483629897752));
#390044=CARTESIAN_POINT('Ctrl Pts',(2.41426609490188,-1.31002993691338,
7.5050991045531));
#390045=CARTESIAN_POINT('Ctrl Pts',(2.4139283935373,-1.31050182651205,7.50567888004914));
#390046=CARTESIAN_POINT('Ctrl Pts',(2.41360330086178,-1.31083872331849,
7.50637912803144));
#390047=CARTESIAN_POINT('Ctrl Pts',(2.41330668489005,-1.31106715325333,
7.50710440483569));
#390048=CARTESIAN_POINT('Ctrl Pts',(2.41323394876513,-1.31112316880832,
7.50728225710685));
#390049=CARTESIAN_POINT('Ctrl Pts',(2.41316156611973,-1.3111738926814,7.50746498566954));
#390050=CARTESIAN_POINT('Ctrl Pts',(2.41309146567674,-1.31121848197554,
7.50764697238949));
#390051=CARTESIAN_POINT('Ctrl Pts',(2.41271462498742,-1.31145818174953,
7.50862528291182));
#390052=CARTESIAN_POINT('Ctrl Pts',(2.41237174905259,-1.31154585365796,
7.50965856837422));
#390053=CARTESIAN_POINT('Ctrl Pts',(2.41206139769779,-1.31154777983823,
7.51067959873202));
#390054=CARTESIAN_POINT('Ctrl Pts',(2.41189061095579,-1.31154883981766,
7.51124147302578));
#390055=CARTESIAN_POINT('Ctrl Pts',(2.41172962930471,-1.31152349915076,
7.51180065547253));
#390056=CARTESIAN_POINT('Ctrl Pts',(2.41157829503253,-1.31148008890242,
7.51235175716501));
#390057=CARTESIAN_POINT('Ctrl Pts',(2.41105537483773,-1.31133008920183,
7.51425603304535));
#390058=CARTESIAN_POINT('Ctrl Pts',(2.41058696594895,-1.31094062862543,
7.51626900505179));
#390059=CARTESIAN_POINT('Ctrl Pts',(2.41018394501642,-1.31037107354313,
7.51827788969242));
#390060=CARTESIAN_POINT('Ctrl Pts',(2.41016213276194,-1.31034024814576,
7.51838661432544));
#390061=CARTESIAN_POINT('Ctrl Pts',(2.41014051310065,-1.31030888531403,
7.51849533314856));
#390062=CARTESIAN_POINT('Ctrl Pts',(2.41011908817659,-1.31027699133282,
7.51860402984325));
#390063=CARTESIAN_POINT('Ctrl Pts',(2.37073694715363,-1.23681194779762,
7.57603338728985));
#390064=CARTESIAN_POINT('Ctrl Pts',(2.3860392422531,-1.25952355359293,7.55196141284922));
#390065=CARTESIAN_POINT('Ctrl Pts',(2.40131444509586,-1.28219650716416,
7.52783573083105));
#390066=CARTESIAN_POINT('Ctrl Pts',(2.4165647636488,-1.30483398894315,7.50366116530176));
#390067=CARTESIAN_POINT('Origin',(8.19199203866634E-16,-4.2737569993508E-16,
7.49482233047033));
#390068=CARTESIAN_POINT('Origin',(2.44485166369886,-1.23150582317296,7.49482233047033));
#390069=CARTESIAN_POINT('Origin',(0.,0.,7.50366116523517));
#390070=CARTESIAN_POINT('Origin',(2.4087872758706,-1.30063450269625,7.49482233047033));
#390071=CARTESIAN_POINT('Ctrl Pts',(2.45352105979442,-1.22708152881659,
7.51860402984325));
#390072=CARTESIAN_POINT('Ctrl Pts',(2.46112885786553,-1.22694850799354,
7.51860402984325));
#390073=CARTESIAN_POINT('Ctrl Pts',(2.46450482787547,-1.2201294822184,7.51860402984325));
#390074=CARTESIAN_POINT('Ctrl Pts',(2.45634588711433,-1.22703213600668,
7.51041458714366));
#390075=CARTESIAN_POINT('Ctrl Pts',(2.46192865495691,-1.22533299829126,
7.51004642900444));
#390076=CARTESIAN_POINT('Ctrl Pts',(2.46450575892791,-1.22012760161205,
7.50729136483012));
#390077=CARTESIAN_POINT('Ctrl Pts',(2.45736298124955,-1.22965687536886,
7.50215815450137));
#390078=CARTESIAN_POINT('Ctrl Pts',(2.46030031409413,-1.22862239953949,
7.49877163671528));
#390079=CARTESIAN_POINT('Ctrl Pts',(2.46185245611966,-1.22554103965674,
7.49481588533168));
#390080=CARTESIAN_POINT('Ctrl Pts',(2.45274510440917,-1.23548185916126,
7.50366171572174));
#390081=CARTESIAN_POINT('Ctrl Pts',(2.45601536992562,-1.23712913743437,
7.50000045605858));
#390082=CARTESIAN_POINT('Ctrl Pts',(2.45601536992568,-1.23712913743426,
7.49482233047317));
#390083=CARTESIAN_POINT('Origin',(2.4533025332033,-1.2145834391174,7.51860402984325));
#390084=CARTESIAN_POINT('Origin',(2.4533025332033,-1.2145834391174,9.));
#390085=CARTESIAN_POINT('Origin',(2.4533025332033,-1.2145834391174,8.75721825406948));
#390086=CARTESIAN_POINT('Ctrl Pts',(2.43682453266412,-1.22737484732809,
8.78942910404913));
#390087=CARTESIAN_POINT('Ctrl Pts',(2.44239646176361,-1.22729716327585,
8.7967269950169));
#390088=CARTESIAN_POINT('Ctrl Pts',(2.44391314215674,-1.21850096144966,
8.79893251111267));
#390089=CARTESIAN_POINT('Ctrl Pts',(2.4478171719985,-1.2271817173077,8.78111911759583));
#390090=CARTESIAN_POINT('Ctrl Pts',(2.45442265473793,-1.22708217884974,
8.78644465894815));
#390091=CARTESIAN_POINT('Ctrl Pts',(2.4574813331055,-1.21957484920337,8.78817647674131));
#390092=CARTESIAN_POINT('Ctrl Pts',(2.45466804703033,-1.22706135404059,
8.7678092393203));
#390093=CARTESIAN_POINT('Ctrl Pts',(2.46246546371487,-1.22693875788232,
8.76988516158373));
#390094=CARTESIAN_POINT('Ctrl Pts',(2.46595667361419,-1.2202344433137,8.77093053738834));
#390095=CARTESIAN_POINT('Ctrl Pts',(2.4533322201599,-1.22708482322866,8.75371302330492));
#390096=CARTESIAN_POINT('Ctrl Pts',(2.46093827577204,-1.22696599817774,
8.75300828287559));
#390097=CARTESIAN_POINT('Ctrl Pts',(2.46430367349725,-1.22010533950051,
8.75267964240738));
#390098=CARTESIAN_POINT('Origin',(2.43928211585348,-1.21482977004092,8.78727029226991));
#390099=CARTESIAN_POINT('Ctrl Pts',(2.36802027905703,-1.22858372995529,
8.85049129520029));
#390100=CARTESIAN_POINT('Ctrl Pts',(2.37385899372368,-1.22848114699074,
8.85711686593484));
#390101=CARTESIAN_POINT('Ctrl Pts',(2.3756631770946,-1.2201237739299,8.85933012996512));
#390102=CARTESIAN_POINT('Ctrl Pts',(2.39188208645158,-1.2281644912903,8.82945683644727));
#390103=CARTESIAN_POINT('Ctrl Pts',(2.39776926598011,-1.22806105682512,
8.83607469902394));
#390104=CARTESIAN_POINT('Ctrl Pts',(2.39954208843698,-1.21967123304662,
8.8382956714852));
#390105=CARTESIAN_POINT('Ctrl Pts',(2.41570832589791,-1.22774587753436,
8.80838214965001));
#390106=CARTESIAN_POINT('Ctrl Pts',(2.42161873898552,-1.22764203486849,
8.81501364461988));
#390107=CARTESIAN_POINT('Ctrl Pts',(2.42338478937515,-1.21922004706177,
8.81722098428721));
#390108=CARTESIAN_POINT('Ctrl Pts',(2.43950170000244,-1.22732784120416,
8.78727029226991));
#390109=CARTESIAN_POINT('Ctrl Pts',(2.44541309482909,-1.22722398128969,
8.79393457792714));
#390110=CARTESIAN_POINT('Ctrl Pts',(2.44719404240189,-1.21877012767603,
8.79610912703474));
#390111=CARTESIAN_POINT('Origin',(2.36780069490807,-1.21608565879204,8.85049129520029));
#390112=CARTESIAN_POINT('Ctrl Pts',(2.36243414091427,-1.23929131094302,
8.85049129520029));
#390113=CARTESIAN_POINT('Ctrl Pts',(2.36569043114743,-1.24413875213817,
8.85711686593484));
#390114=CARTESIAN_POINT('Ctrl Pts',(2.35986814900604,-1.25039988564417,
8.85933012996512));
#390115=CARTESIAN_POINT('Ctrl Pts',(2.35955334795003,-1.23500284969122,
8.86332496987232));
#390116=CARTESIAN_POINT('Ctrl Pts',(2.35767030474025,-1.23922257037471,
8.86648636486737));
#390117=CARTESIAN_POINT('Ctrl Pts',(2.35182323496413,-1.23839318691325,
8.87206031107457));
#390118=CARTESIAN_POINT('Ctrl Pts',(2.36281975177211,-1.22867510032301,
8.86341338519876));
#390119=CARTESIAN_POINT('Ctrl Pts',(2.365184693223,-1.22469006298715,8.86654584966058));
#390120=CARTESIAN_POINT('Ctrl Pts',(2.36110168311631,-1.2203943463699,8.87215952290714));
#390121=CARTESIAN_POINT('Ctrl Pts',(2.36802027905703,-1.22858372995529,
8.85049129520029));
#390122=CARTESIAN_POINT('Ctrl Pts',(2.37385899372368,-1.22848114699074,
8.85711686593484));
#390123=CARTESIAN_POINT('Ctrl Pts',(2.3756631770946,-1.2201237739299,8.85933012996512));
#390124=CARTESIAN_POINT('Origin',(2.35205794196028,-1.24626156884838,8.85049129520029));
#390125=CARTESIAN_POINT('Ctrl Pts',(2.40229980761781,-1.29863690399938,
8.78727029226991));
#390126=CARTESIAN_POINT('Ctrl Pts',(2.40559663206248,-1.30354468600957,
8.79393457792714));
#390127=CARTESIAN_POINT('Ctrl Pts',(2.39968192566134,-1.30984196029027,
8.79610912703474));
#390128=CARTESIAN_POINT('Ctrl Pts',(2.38903008369152,-1.27888307316656,
8.80838214965002));
#390129=CARTESIAN_POINT('Ctrl Pts',(2.39232636061378,-1.28379004011344,
8.81501364461994));
#390130=CARTESIAN_POINT('Ctrl Pts',(2.38642926673667,-1.29005686517877,
8.81722098428721));
#390131=CARTESIAN_POINT('Ctrl Pts',(2.37574203054421,-1.25910195673733,
8.82945683644721));
#390132=CARTESIAN_POINT('Ctrl Pts',(2.37902534995513,-1.26398963462521,
8.83607469902388));
#390133=CARTESIAN_POINT('Ctrl Pts',(2.37315851053407,-1.27024361237585,
8.8382956714852));
#390134=CARTESIAN_POINT('Ctrl Pts',(2.36243414091427,-1.23929131094302,
8.85049129520029));
#390135=CARTESIAN_POINT('Ctrl Pts',(2.36569043114743,-1.24413875213817,
8.85711686593484));
#390136=CARTESIAN_POINT('Ctrl Pts',(2.35986814900604,-1.25039988564417,
8.85933012996512));
#390137=CARTESIAN_POINT('Origin',(2.39192360866382,-1.30560716190474,8.78727029226991));
#390138=CARTESIAN_POINT('Ctrl Pts',(2.41001582319739,-1.31012330012149,
8.75374538247848));
#390139=CARTESIAN_POINT('Ctrl Pts',(2.4142640535715,-1.31642384907187,8.75304829418602));
#390140=CARTESIAN_POINT('Ctrl Pts',(2.41057140660496,-1.32310479223804,
8.75272238421917));
#390141=CARTESIAN_POINT('Ctrl Pts',(2.41075187368563,-1.31121901294557,
8.76769408445017));
#390142=CARTESIAN_POINT('Ctrl Pts',(2.41510643619571,-1.31767849746976,
8.76974318093966));
#390143=CARTESIAN_POINT('Ctrl Pts',(2.41161165479856,-1.32437214074275,
8.77077869880429));
#390144=CARTESIAN_POINT('Ctrl Pts',(2.40697929819551,-1.30560301318752,
8.78108014887992));
#390145=CARTESIAN_POINT('Ctrl Pts',(2.41067278344331,-1.3110750698415,8.78639403366328));
#390146=CARTESIAN_POINT('Ctrl Pts',(2.40628851871305,-1.31787950211055,
8.78812224174742));
#390147=CARTESIAN_POINT('Ctrl Pts',(2.40079687974257,-1.29639962934831,
8.78944554828685));
#390148=CARTESIAN_POINT('Ctrl Pts',(2.40391425189903,-1.30100814412588,
8.79673892988685));
#390149=CARTESIAN_POINT('Ctrl Pts',(2.39757616771976,-1.30727968646034,
8.79894799272499));
#390150=CARTESIAN_POINT('Origin',(2.3997428892226,-1.31724724923818,8.75721825406948));
#390151=CARTESIAN_POINT('Origin',(2.3997428892226,-1.31724724923818,9.));
#390152=CARTESIAN_POINT('Origin',(2.3997428892226,-1.31724724923818,7.51860402984325));
#390153=CARTESIAN_POINT('Ctrl Pts',(2.41656407141738,-1.30483361513347,
7.50366195182966));
#390154=CARTESIAN_POINT('Ctrl Pts',(2.41978630452747,-1.30657347302832,
7.50000065167735));
#390155=CARTESIAN_POINT('Ctrl Pts',(2.41978630452742,-1.30657347302842,
7.49482233047108));
#390156=CARTESIAN_POINT('Ctrl Pts',(2.41442578748733,-1.31195973198917,
7.50215800491338));
#390157=CARTESIAN_POINT('Ctrl Pts',(2.41525681547057,-1.3149620793484,7.49877273257266));
#390158=CARTESIAN_POINT('Ctrl Pts',(2.41361667159589,-1.31799969097932,
7.49481816995647));
#390159=CARTESIAN_POINT('Ctrl Pts',(2.41169107100778,-1.31261649840008,
7.51043025814041));
#390160=CARTESIAN_POINT('Ctrl Pts',(2.41349603202948,-1.31816941409338,
7.51006209594513));
#390161=CARTESIAN_POINT('Ctrl Pts',(2.41069940101147,-1.32326429634043,
7.50731281821699));
#390162=CARTESIAN_POINT('Ctrl Pts',(2.41011824530877,-1.31027573677064,
7.51860402984325));
#390163=CARTESIAN_POINT('Ctrl Pts',(2.41436209596894,-1.31659164913266,
7.51860402984324));
#390164=CARTESIAN_POINT('Ctrl Pts',(2.41070061931038,-1.32326207686028,
7.51860402984325));
#390165=CARTESIAN_POINT('Origin',(0.,0.,7.5));
#390166=CARTESIAN_POINT('Origin',(-0.33515558185988,2.64662214142562,7.5));
#390167=CARTESIAN_POINT('',(-0.33515558185988,2.64662214142562,7.59394543036555));
#390168=CARTESIAN_POINT('',(-0.33515558185988,2.64662214142562,8.85049129520029));
#390169=CARTESIAN_POINT('',(-0.33515558185988,2.64662214142562,7.5));
#390170=CARTESIAN_POINT('',(-0.309289785090423,2.71327145765926,8.78727029226991));
#390171=CARTESIAN_POINT('Ctrl Pts',(-0.33515558185988,2.64662214142562,
8.85049129520029));
#390172=CARTESIAN_POINT('Ctrl Pts',(-0.32652111678987,2.66887087391543,
8.82945686509571));
#390173=CARTESIAN_POINT('Ctrl Pts',(-0.317899487896255,2.6910865309741,
8.80838212259895));
#390174=CARTESIAN_POINT('Ctrl Pts',(-0.309289785090423,2.71327145765926,
8.78727029226991));
#390175=CARTESIAN_POINT('',(-0.304216449096299,2.72634410251322,8.75721825406948));
#390176=CARTESIAN_POINT('Origin',(-0.319484065187221,2.68700405222604,8.7593767971307));
#390177=CARTESIAN_POINT('',(-0.304216449096299,2.72634410251322,7.51860402984325));
#390178=CARTESIAN_POINT('',(-0.304216449096299,2.72634410251322,7.5));
#390179=CARTESIAN_POINT('Ctrl Pts',(-0.304216449096299,2.72634410251322,
7.51860402984325));
#390180=CARTESIAN_POINT('Ctrl Pts',(-0.308200765466687,2.71607757316129,
7.52834476460825));
#390181=CARTESIAN_POINT('Ctrl Pts',(-0.312187668397775,2.70580437892665,
7.53807742314407));
#390182=CARTESIAN_POINT('Ctrl Pts',(-0.316177244736769,2.69552429602699,
7.54780169004674));
#390183=CARTESIAN_POINT('Ctrl Pts',(-0.322496518039534,2.67924120030501,
7.5632044032688));
#390184=CARTESIAN_POINT('Ctrl Pts',(-0.328822506613102,2.66294080110644,
7.57858609112103));
#390185=CARTESIAN_POINT('Ctrl Pts',(-0.33515558185988,2.64662214142562,
7.59394543036555));
#390186=CARTESIAN_POINT('Origin',(-0.508403499682097,2.86782650745936,7.5));
#390187=CARTESIAN_POINT('',(-0.397282670454307,2.71434454205174,8.75721825406948));
#390188=CARTESIAN_POINT('',(-0.389059322317692,2.70298631476879,8.78727029226991));
#390189=CARTESIAN_POINT('Origin',(-0.368185397591817,2.67415489751821,8.756586406211));
#390190=CARTESIAN_POINT('',(-0.347133565397089,2.64507775146798,8.85049129520029));
#390191=CARTESIAN_POINT('Ctrl Pts',(-0.389059322317692,2.70298631476879,
8.78727029226991));
#390192=CARTESIAN_POINT('Ctrl Pts',(-0.375103892673939,2.68371083973215,
8.80838212259896));
#390193=CARTESIAN_POINT('Ctrl Pts',(-0.361129132086614,2.66440866446988,
8.82945686509571));
#390194=CARTESIAN_POINT('Ctrl Pts',(-0.347133565397089,2.64507775146798,
8.85049129520029));
#390195=CARTESIAN_POINT('',(-0.347133565397089,2.64507775146798,7.59394543036555));
#390196=CARTESIAN_POINT('',(-0.347133565397089,2.64507775146798,7.5));
#390197=CARTESIAN_POINT('',(-0.397282670454307,2.71434454205174,7.51860402984325));
#390198=CARTESIAN_POINT('Ctrl Pts',(-0.347133565397089,2.64507775146798,
7.59394543036555));
#390199=CARTESIAN_POINT('Ctrl Pts',(-0.357398819381834,2.65925629358232,
7.57858609112103));
#390200=CARTESIAN_POINT('Ctrl Pts',(-0.367652586608838,2.67341896999297,
7.56320440326857));
#390201=CARTESIAN_POINT('Ctrl Pts',(-0.377895469082858,2.68756661219899,
7.54780169004651));
#390202=CARTESIAN_POINT('Ctrl Pts',(-0.384362155931739,2.6964985092532,
7.53807742314383));
#390203=CARTESIAN_POINT('Ctrl Pts',(-0.390824509465548,2.70542442105947,
7.52834476460825));
#390204=CARTESIAN_POINT('Ctrl Pts',(-0.397282670454307,2.71434454205174,
7.51860402984325));
#390205=CARTESIAN_POINT('',(-0.397282670454307,2.71434454205174,7.5));
#390206=CARTESIAN_POINT('Origin',(-0.341564846497304,2.6491094998251,7.5));
#390207=CARTESIAN_POINT('Ctrl Pts',(-0.347133565397089,2.64507775146798,
8.85049129520029));
#390208=CARTESIAN_POINT('Ctrl Pts',(-0.347019995294062,2.64492088652425,
8.85097269580139));
#390209=CARTESIAN_POINT('Ctrl Pts',(-0.346901044882014,2.64477093347823,
8.85143669361005));
#390210=CARTESIAN_POINT('Ctrl Pts',(-0.346770551927422,2.64462153081529,
8.8519052845931));
#390211=CARTESIAN_POINT('Ctrl Pts',(-0.346515315983802,2.64432930868135,
8.85282181883899));
#390212=CARTESIAN_POINT('Ctrl Pts',(-0.346222339439948,2.64404683890339,
8.85372622499636));
#390213=CARTESIAN_POINT('Ctrl Pts',(-0.345876323146614,2.64378078895684,
8.85462257735071));
#390214=CARTESIAN_POINT('Ctrl Pts',(-0.345589072709225,2.64355992374042,
8.85536669723986));
#390215=CARTESIAN_POINT('Ctrl Pts',(-0.345265222470721,2.64335029921311,
8.85610498449051));
#390216=CARTESIAN_POINT('Ctrl Pts',(-0.34489164328641,2.64316243027106,
8.85681338218371));
#390217=CARTESIAN_POINT('Ctrl Pts',(-0.344552619589932,2.6429919389111,
8.85745625420284));
#390218=CARTESIAN_POINT('Ctrl Pts',(-0.344168657352609,2.6428366912356,
8.85808743050666));
#390219=CARTESIAN_POINT('Ctrl Pts',(-0.343718641537305,2.64271597458123,
8.8586680450841));
#390220=CARTESIAN_POINT('Ctrl Pts',(-0.343511013995271,2.64266027853372,
8.85893592806395));
#390221=CARTESIAN_POINT('Ctrl Pts',(-0.343289167465158,2.64261211674724,
8.85919241173848));
#390222=CARTESIAN_POINT('Ctrl Pts',(-0.343050165639967,2.64257472651662,
8.85943017985534));
#390223=CARTESIAN_POINT('Ctrl Pts',(-0.342727442423848,2.6425242386366,
8.8597512372));
#390224=CARTESIAN_POINT('Ctrl Pts',(-0.342365126816596,2.64249273833371,
8.86004599534705));
#390225=CARTESIAN_POINT('Ctrl Pts',(-0.341966669802032,2.64249098002396,
8.86026130871721));
#390226=CARTESIAN_POINT('Ctrl Pts',(-0.341820783455307,2.64249033625719,
8.86034014101235));
#390227=CARTESIAN_POINT('Ctrl Pts',(-0.341667861040585,2.64249365740532,
8.86040910639693));
#390228=CARTESIAN_POINT('Ctrl Pts',(-0.341512076146919,2.64250118928493,
8.86046313645507));
#390229=CARTESIAN_POINT('Ctrl Pts',(-0.341268975125039,2.64251294271999,
8.8605474499083));
#390230=CARTESIAN_POINT('Ctrl Pts',(-0.341012274757778,2.6425354175532,
8.86059655985669));
#390231=CARTESIAN_POINT('Ctrl Pts',(-0.34075841246969,2.6425668805641,8.86059725258816));
#390232=CARTESIAN_POINT('Ctrl Pts',(-0.340503963658298,2.64259841626712,
8.86059794692011));
#390233=CARTESIAN_POINT('Ctrl Pts',(-0.340249870963048,2.64264196806059,
8.86056369958366));
#390234=CARTESIAN_POINT('Ctrl Pts',(-0.340009356993999,2.64269145159793,
8.86048590497774));
#390235=CARTESIAN_POINT('Ctrl Pts',(-0.339946590009041,2.64270436532787,
8.86046560290182));
#390236=CARTESIAN_POINT('Ctrl Pts',(-0.339883949500254,2.64271793976287,
8.86044257503091));
#390237=CARTESIAN_POINT('Ctrl Pts',(-0.339823364159025,2.64273172336011,
8.86041778462583));
#390238=CARTESIAN_POINT('Ctrl Pts',(-0.339415699992699,2.64282446986554,
8.860250975962));
#390239=CARTESIAN_POINT('Ctrl Pts',(-0.339046456499739,2.64293945540863,
8.8599848982295));
#390240=CARTESIAN_POINT('Ctrl Pts',(-0.338723891841615,2.64306523453273,
8.85968173251461));
#390241=CARTESIAN_POINT('Ctrl Pts',(-0.338553273618219,2.6431317644831,
8.85952137522076));
#390242=CARTESIAN_POINT('Ctrl Pts',(-0.338392357052997,2.64320241876617,
8.85934740853961));
#390243=CARTESIAN_POINT('Ctrl Pts',(-0.338242786451433,2.64327477760985,
8.8591675900182));
#390244=CARTESIAN_POINT('Ctrl Pts',(-0.33764218274091,2.64356533597861,
8.85844552518696));
#390245=CARTESIAN_POINT('Ctrl Pts',(-0.337189263383585,2.64389707715723,
8.85759444184127));
#390246=CARTESIAN_POINT('Ctrl Pts',(-0.336844272355958,2.64420073065444,
8.85683498915143));
#390247=CARTESIAN_POINT('Ctrl Pts',(-0.336808169963697,2.64423250718423,
8.85675551445001));
#390248=CARTESIAN_POINT('Ctrl Pts',(-0.336773265374242,2.64426398824035,
8.85667699793653));
#390249=CARTESIAN_POINT('Ctrl Pts',(-0.336739523864507,2.64429510185888,
8.85659965593548));
#390250=CARTESIAN_POINT('Ctrl Pts',(-0.336284079244434,2.64471507506948,
8.85555568965887));
#390251=CARTESIAN_POINT('Ctrl Pts',(-0.335907021189084,2.64518447055947,
8.85434650606346));
#390252=CARTESIAN_POINT('Ctrl Pts',(-0.335601640613694,2.64570171674404,
8.85297329937118));
#390253=CARTESIAN_POINT('Ctrl Pts',(-0.335429882647148,2.64599263620658,
8.85220095427747));
#390254=CARTESIAN_POINT('Ctrl Pts',(-0.335281000138073,2.64629897169846,
8.85137579139184));
#390255=CARTESIAN_POINT('Ctrl Pts',(-0.33515558185988,2.64662214142562,
8.85049129520029));
#390256=CARTESIAN_POINT('Origin',(-0.341564846497304,2.6491094998251,7.59394543036555));
#390257=CARTESIAN_POINT('Ctrl Pts',(-0.346803833075487,2.64462231961844,
7.59443877723642));
#390258=CARTESIAN_POINT('Ctrl Pts',(-0.343407907422914,2.63993180977292,
7.58783886950016));
#390259=CARTESIAN_POINT('Ctrl Pts',(-0.335565689793683,2.643184317143,7.58559994247159));
#390260=CARTESIAN_POINT('Ctrl Pts',(-0.365342091580668,2.67022767525142,
7.56670252222137));
#390261=CARTESIAN_POINT('Ctrl Pts',(-0.36195107400472,2.66554394452432,
7.56004874999028));
#390262=CARTESIAN_POINT('Ctrl Pts',(-0.35405420332713,2.66879598861332,
7.55786368756704));
#390263=CARTESIAN_POINT('Ctrl Pts',(-0.383845731740252,2.695785215441,7.53888913333557));
#390264=CARTESIAN_POINT('Ctrl Pts',(-0.380434561180877,2.69107364907285,
7.53222002137277));
#390265=CARTESIAN_POINT('Ctrl Pts',(-0.372509792162566,2.69436005755723,
7.53005029815326));
#390266=CARTESIAN_POINT('Ctrl Pts',(-0.402313916252076,2.72129378369128,
7.51101258149734));
#390267=CARTESIAN_POINT('Ctrl Pts',(-0.398861396107279,2.71652510457761,
7.5043616886572));
#390268=CARTESIAN_POINT('Ctrl Pts',(-0.39093147744885,2.71987530929006,
7.50217374673251));
#390269=CARTESIAN_POINT('',(-0.389948473491309,2.71851378208007,7.50366116523517));
#390270=CARTESIAN_POINT('Ctrl Pts',(-0.397282670454307,2.71434454205174,
7.51860402984325));
#390271=CARTESIAN_POINT('Ctrl Pts',(-0.397541647224221,2.71470224513871,
7.51734760759493));
#390272=CARTESIAN_POINT('Ctrl Pts',(-0.397727477622806,2.71506037210354,
7.51608817408572));
#390273=CARTESIAN_POINT('Ctrl Pts',(-0.397827881300144,2.71542424967146,
7.51481005913118));
#390274=CARTESIAN_POINT('Ctrl Pts',(-0.3979188293503,2.71575385866761,7.51365231206383));
#390275=CARTESIAN_POINT('Ctrl Pts',(-0.397940052684864,2.71608858420058,
7.51247773061042));
#390276=CARTESIAN_POINT('Ctrl Pts',(-0.397854333026815,2.716424970865,7.51129758471022));
#390277=CARTESIAN_POINT('Ctrl Pts',(-0.397747793281414,2.71684306107206,
7.50983079813402));
#390278=CARTESIAN_POINT('Ctrl Pts',(-0.397466830635151,2.71724715791932,
7.50839324291155));
#390279=CARTESIAN_POINT('Ctrl Pts',(-0.396941707788383,2.71759314905582,
7.50715379678855));
#390280=CARTESIAN_POINT('Ctrl Pts',(-0.396699116164227,2.71775298699138,
7.50658120839351));
#390281=CARTESIAN_POINT('Ctrl Pts',(-0.396364702174659,2.71791521224514,
7.50598221009429));
#390282=CARTESIAN_POINT('Ctrl Pts',(-0.395936496490176,2.71805549851716,
7.50545747549611));
#390283=CARTESIAN_POINT('Ctrl Pts',(-0.395707992682731,2.71813035961418,
7.50517746087247));
#390284=CARTESIAN_POINT('Ctrl Pts',(-0.395450365812596,2.71819997752053,
7.50491486231392));
#390285=CARTESIAN_POINT('Ctrl Pts',(-0.395170003136817,2.71826089837762,
7.50468370960993));
#390286=CARTESIAN_POINT('Ctrl Pts',(-0.394750772501136,2.71835199427538,
7.50433806340447));
#390287=CARTESIAN_POINT('Ctrl Pts',(-0.394268015985526,2.71842583148374,
7.50405484070984));
#390288=CARTESIAN_POINT('Ctrl Pts',(-0.39375413803124,2.71847672904423,
7.50385766036131));
#390289=CARTESIAN_POINT('Ctrl Pts',(-0.393699186771502,2.71848217174719,
7.50383657498791));
#390290=CARTESIAN_POINT('Ctrl Pts',(-0.393643905362433,2.71848736408184,
7.50381643264937));
#390291=CARTESIAN_POINT('Ctrl Pts',(-0.393588351980706,2.71849230807154,
7.50379723213559));
#390292=CARTESIAN_POINT('Ctrl Pts',(-0.393217514984894,2.71852531082003,
7.50366906242519));
#390293=CARTESIAN_POINT('Ctrl Pts',(-0.392826428584446,2.71854724898583,
7.50358235568538));
#390294=CARTESIAN_POINT('Ctrl Pts',(-0.392448961127778,2.71855933335556,
7.5035341175365));
#390295=CARTESIAN_POINT('Ctrl Pts',(-0.391882991397572,2.71857745250029,
7.50346178989176));
#390296=CARTESIAN_POINT('Ctrl Pts',(-0.391273366354832,2.71857288019814,
7.50346967198527));
#390297=CARTESIAN_POINT('Ctrl Pts',(-0.390675041552688,2.71854997689286,
7.50354272648692));
#390298=CARTESIAN_POINT('Ctrl Pts',(-0.390428938176975,2.71854055628932,
7.50357277531559));
#390299=CARTESIAN_POINT('Ctrl Pts',(-0.390185068196088,2.71852818857031,
7.50361331098761));
#390300=CARTESIAN_POINT('Ctrl Pts',(-0.389948473491511,2.71851378208147,
7.50366116523658));
#390301=CARTESIAN_POINT('',(-0.341939261259086,2.65201338678246,7.57603338622103));
#390302=CARTESIAN_POINT('Origin',(-0.343066474116784,2.6607781389627,7.58486873427628));
#390303=CARTESIAN_POINT('Ctrl Pts',(-0.389948473529075,2.71851378212322,
7.50366116529969));
#390304=CARTESIAN_POINT('Ctrl Pts',(-0.373970838805478,2.69638364458546,
7.52783573079709));
#390305=CARTESIAN_POINT('Ctrl Pts',(-0.357968509118427,2.67421790325149,
7.55196141284068));
#390306=CARTESIAN_POINT('Ctrl Pts',(-0.341939262248846,2.65201338754928,
7.57603338728831));
#390307=CARTESIAN_POINT('Ctrl Pts',(-0.347594250863845,2.64601386279727,
7.59639677331372));
#390308=CARTESIAN_POINT('Ctrl Pts',(-0.339350823778407,2.62970074459056,
7.5995988229546));
#390309=CARTESIAN_POINT('Ctrl Pts',(-0.334988019337677,2.64746798269907,
7.59642833564546));
#390310=CARTESIAN_POINT('Ctrl Pts',(-0.346417486467329,2.64229494768144,
7.58707626057423));
#390311=CARTESIAN_POINT('Ctrl Pts',(-0.34038578786662,2.63920773161741,
7.58809943920598));
#390312=CARTESIAN_POINT('Ctrl Pts',(-0.335273897319224,2.64363299723925,
7.58710240504252));
#390313=CARTESIAN_POINT('Ctrl Pts',(-0.343548093433324,2.6476514592214,
7.5801537675693));
#390314=CARTESIAN_POINT('Ctrl Pts',(-0.341200555278549,2.64603333190639,
7.5820588065976));
#390315=CARTESIAN_POINT('Ctrl Pts',(-0.339331722030058,2.64813916602316,
7.58020924244129));
#390316=CARTESIAN_POINT('Ctrl Pts',(-0.34193926115346,2.65201338596165,
7.57603338509286));
#390317=CARTESIAN_POINT('Ctrl Pts',(-0.34193926115346,2.65201338596165,
7.57603338509286));
#390318=CARTESIAN_POINT('Ctrl Pts',(-0.34193926115346,2.65201338596165,
7.57603338509286));
#390319=CARTESIAN_POINT('Origin',(-0.343072133619813,2.66077740925,7.58486873427622));
#390320=CARTESIAN_POINT('Ctrl Pts',(-0.30110264748335,2.73436754560449,
7.51098857897448));
#390321=CARTESIAN_POINT('Ctrl Pts',(-0.303232664881353,2.72887905420375,
7.50433767179956));
#390322=CARTESIAN_POINT('Ctrl Pts',(-0.311753059719538,2.73010825023526,
7.50214974420965));
#390323=CARTESIAN_POINT('Ctrl Pts',(-0.312499739379753,2.70500025455533,
7.53887321589167));
#390324=CARTESIAN_POINT('Ctrl Pts',(-0.314604235389233,2.69957752502185,
7.53220407452058));
#390325=CARTESIAN_POINT('Ctrl Pts',(-0.323103465221934,2.70074629025613,
7.53003438070911));
#390326=CARTESIAN_POINT('Ctrl Pts',(-0.3239187178968,2.67557656747423,7.56669465659233));
#390327=CARTESIAN_POINT('Ctrl Pts',(-0.326010776726107,2.67018588526414,
7.56004085833299));
#390328=CARTESIAN_POINT('Ctrl Pts',(-0.334474294446307,2.67132847789769,
7.55785582193789));
#390329=CARTESIAN_POINT('Ctrl Pts',(-0.335359066599817,2.64609781507675,
7.59443891967696));
#390330=CARTESIAN_POINT('Ctrl Pts',(-0.337454158653971,2.64069931704862,
7.58783901202978));
#390331=CARTESIAN_POINT('Ctrl Pts',(-0.345864908691495,2.64185623614459,
7.58560008491213));
#390332=CARTESIAN_POINT('',(-0.312368326987727,2.72851663429644,7.50366116523517));
#390333=CARTESIAN_POINT('Ctrl Pts',(-0.31236832698777,2.72851663429681,
7.50366116523554));
#390334=CARTESIAN_POINT('Ctrl Pts',(-0.311648372775235,2.7287528618325,
7.50350835821027));
#390335=CARTESIAN_POINT('Ctrl Pts',(-0.310978874698737,2.72894658931302,
7.50345484956));
#390336=CARTESIAN_POINT('Ctrl Pts',(-0.31034009495131,2.72910415325133,
7.50349758195598));
#390337=CARTESIAN_POINT('Ctrl Pts',(-0.310012353567739,2.72918499523694,
7.50351950684424));
#390338=CARTESIAN_POINT('Ctrl Pts',(-0.309660426124605,2.72926441113657,
7.50357029184312));
#390339=CARTESIAN_POINT('Ctrl Pts',(-0.309318961508532,2.72933166265592,
7.50365515313923));
#390340=CARTESIAN_POINT('Ctrl Pts',(-0.308793650656337,2.72943512272552,
7.50378570417639));
#390341=CARTESIAN_POINT('Ctrl Pts',(-0.308277749172659,2.72951317103045,
7.5040000162191));
#390342=CARTESIAN_POINT('Ctrl Pts',(-0.307810185036314,2.72955762209029,
7.50428903009634));
#390343=CARTESIAN_POINT('Ctrl Pts',(-0.307758289014399,2.72956255581594,
7.50432110841317));
#390344=CARTESIAN_POINT('Ctrl Pts',(-0.307706965257206,2.72956709514048,
7.50435406373354));
#390345=CARTESIAN_POINT('Ctrl Pts',(-0.307656249660458,2.72957124302654,
7.50438785222352));
#390346=CARTESIAN_POINT('Ctrl Pts',(-0.307346606565319,2.7295965678646,
7.50459414719561));
#390347=CARTESIAN_POINT('Ctrl Pts',(-0.30705466192801,2.72960719025544,
7.50483629897752));
#390348=CARTESIAN_POINT('Ctrl Pts',(-0.306791647913675,2.72960401841961,
7.5050991045531));
#390349=CARTESIAN_POINT('Ctrl Pts',(-0.306211412580796,2.72959702103118,
7.50567888004914));
#390350=CARTESIAN_POINT('Ctrl Pts',(-0.305749108231741,2.72952313331425,
7.50637912803144));
#390351=CARTESIAN_POINT('Ctrl Pts',(-0.305392057397979,2.72941054569536,
7.50710440483569));
#390352=CARTESIAN_POINT('Ctrl Pts',(-0.305304501445088,2.72938293697603,
7.50728225710685));
#390353=CARTESIAN_POINT('Ctrl Pts',(-0.305221487814413,2.72935259071141,
7.50746498566955));
#390354=CARTESIAN_POINT('Ctrl Pts',(-0.305144811281192,2.72932060655108,
7.50764697238949));
#390355=CARTESIAN_POINT('Ctrl Pts',(-0.304732619340553,2.72914866850742,
7.50862528291182));
#390356=CARTESIAN_POINT('Ctrl Pts',(-0.304464548239082,2.72891760973834,
7.50965856837421));
#390357=CARTESIAN_POINT('Ctrl Pts',(-0.304285411258898,2.72866417016778,
7.51067959873201));
#390358=CARTESIAN_POINT('Ctrl Pts',(-0.304186831952749,2.72852470205243,
7.51124147302578));
#390359=CARTESIAN_POINT('Ctrl Pts',(-0.304115515380097,2.728378171551,7.51180065547253));
#390360=CARTESIAN_POINT('Ctrl Pts',(-0.304064538402986,2.72822921565349,
7.51235175716501));
#390361=CARTESIAN_POINT('Ctrl Pts',(-0.303888392640254,2.72771451369063,
7.51425603304536));
#390362=CARTESIAN_POINT('Ctrl Pts',(-0.303939832870249,2.72710752083202,
7.51626900505181));
#390363=CARTESIAN_POINT('Ctrl Pts',(-0.304176391156343,2.72645112229369,
7.51827788969244));
#390364=CARTESIAN_POINT('Ctrl Pts',(-0.304189194137819,2.72641559676438,
7.51838661432546));
#390365=CARTESIAN_POINT('Ctrl Pts',(-0.304202548093819,2.7263799217195,
7.51849533314857));
#390366=CARTESIAN_POINT('Ctrl Pts',(-0.304216449096295,2.72634410251322,
7.51860402984325));
#390367=CARTESIAN_POINT('Ctrl Pts',(-0.341939260496117,2.65201338777647,
7.57603338728985));
#390368=CARTESIAN_POINT('Ctrl Pts',(-0.332066529529967,2.67755759370233,
7.55196141284922));
#390369=CARTESIAN_POINT('Ctrl Pts',(-0.322210000114179,2.70305746572958,
7.52783573083105));
#390370=CARTESIAN_POINT('Ctrl Pts',(-0.31236832696141,2.72851663434944,
7.50366116530176));
#390371=CARTESIAN_POINT('Origin',(-1.18155821115204E-16,9.16393216063563E-16,
7.49482233047033));
#390372=CARTESIAN_POINT('Origin',(-0.388693460788449,2.70976449964574,7.49482233047033));
#390373=CARTESIAN_POINT('Origin',(0.,0.,7.50366116523517));
#390374=CARTESIAN_POINT('Origin',(-0.311362998732866,2.71973515861749,7.49482233047033));
#390375=CARTESIAN_POINT('Ctrl Pts',(-0.397282050205177,2.71434368527686,
7.51860402984325));
#390376=CARTESIAN_POINT('Ctrl Pts',(-0.401743698216853,2.72050728674435,
7.51860402984325));
#390377=CARTESIAN_POINT('Ctrl Pts',(-0.409267922647769,2.71937488542709,
7.51860402984325));
#390378=CARTESIAN_POINT('Ctrl Pts',(-0.398938691589132,2.71663227181923,
7.51041458714367));
#390379=CARTESIAN_POINT('Ctrl Pts',(-0.403526271692389,2.72023899811274,
7.51004642900444));
#390380=CARTESIAN_POINT('Ctrl Pts',(-0.409269997739523,2.71937457312425,
7.50729136483011));
#390381=CARTESIAN_POINT('Ctrl Pts',(-0.397367849688397,2.71896812132684,
7.50215815450137));
#390382=CARTESIAN_POINT('Ctrl Pts',(-0.399896795118419,2.72078539937201,
7.49877163671528));
#390383=CARTESIAN_POINT('Ctrl Pts',(-0.403312047312352,2.72029552587179,
7.49481588533169));
#390384=CARTESIAN_POINT('Ctrl Pts',(-0.389948395323623,2.71851323713979,
7.50366171572174));
#390385=CARTESIAN_POINT('Ctrl Pts',(-0.390468316773402,2.72213785352545,
7.50000045605858));
#390386=CARTESIAN_POINT('Ctrl Pts',(-0.390468316773525,2.72213785352544,
7.49482233047317));
#390387=CARTESIAN_POINT('Origin',(-0.407407613908461,2.70701409049333,7.51860402984325));
#390388=CARTESIAN_POINT('Origin',(-0.407407613908461,2.70701409049333,9.));
#390389=CARTESIAN_POINT('Origin',(-0.40740761390846,2.70701409049333,8.75721825406948));
#390390=CARTESIAN_POINT('Ctrl Pts',(-0.387489117162865,2.70081746938362,
8.78942910404913));
#390391=CARTESIAN_POINT('Ctrl Pts',(-0.390740624933972,2.70534296669508,
8.7967269950169));
#390392=CARTESIAN_POINT('Ctrl Pts',(-0.39882274373864,2.70155445226207,
8.79893251111267));
#390393=CARTESIAN_POINT('Ctrl Pts',(-0.393936589149031,2.70972283426824,
8.78111911759585));
#390394=CARTESIAN_POINT('Ctrl Pts',(-0.397797334553896,2.7150835203292,
8.78644465894814));
#390395=CARTESIAN_POINT('Ctrl Pts',(-0.405704558887993,2.7132970950983,
8.78817647674132));
#390396=CARTESIAN_POINT('Ctrl Pts',(-0.39795480750331,2.71527287005867,
8.76780923932029));
#390397=CARTESIAN_POINT('Ctrl Pts',(-0.402516389461986,2.72159795557625,
8.76988516158373));
#390398=CARTESIAN_POINT('Ctrl Pts',(-0.410012461604652,2.72062569901123,
8.77093053738832));
#390399=CARTESIAN_POINT('Ctrl Pts',(-0.39717130991881,2.71419068903609,
8.75371302330492));
#390400=CARTESIAN_POINT('Ctrl Pts',(-0.401620318062246,2.72036098302482,
8.75300828287559));
#390401=CARTESIAN_POINT('Ctrl Pts',(-0.409172640064091,2.71919609173606,
8.75267964240738));
#390402=CARTESIAN_POINT('Origin',(-0.399184265771846,2.69565586321038,8.78727029226991));
#390403=CARTESIAN_POINT('Ctrl Pts',(-0.347133565397089,2.64507775146798,
8.85049129520029));
#390404=CARTESIAN_POINT('Ctrl Pts',(-0.350558127032893,2.649807813817,8.85711686593485));
#390405=CARTESIAN_POINT('Ctrl Pts',(-0.358444815903127,2.64650616259708,
8.85933012996512));
#390406=CARTESIAN_POINT('Ctrl Pts',(-0.361129150869188,2.66440869041269,
8.82945683644724));
#390407=CARTESIAN_POINT('Ctrl Pts',(-0.364582138437099,2.66917801513907,
8.83607469902392));
#390408=CARTESIAN_POINT('Ctrl Pts',(-0.372477500384183,2.66583207697137,
8.8382956714852));
#390409=CARTESIAN_POINT('Ctrl Pts',(-0.375103874792535,2.68371081503405,
8.80838214965002));
#390410=CARTESIAN_POINT('Ctrl Pts',(-0.378570489461573,2.68849896174259,
8.81501364461993));
#390411=CARTESIAN_POINT('Ctrl Pts',(-0.386488357039706,2.68512906773677,
8.81722098428721));
#390412=CARTESIAN_POINT('Ctrl Pts',(-0.389059322317692,2.70298631476879,
8.78727029226991));
#390413=CARTESIAN_POINT('Ctrl Pts',(-0.392526512802801,2.70777525680419,
8.79393457792714));
#390414=CARTESIAN_POINT('Ctrl Pts',(-0.400479038758349,2.70439935009568,
8.79610912703474));
#390415=CARTESIAN_POINT('Origin',(-0.357258508851243,2.63774729990957,8.85049129520029));
#390416=CARTESIAN_POINT('Ctrl Pts',(-0.33515558185988,2.64662214142562,
8.85049129520029));
#390417=CARTESIAN_POINT('Ctrl Pts',(-0.333042822978414,2.65206616219449,
8.85711686593484));
#390418=CARTESIAN_POINT('Ctrl Pts',(-0.324576590381445,2.65087298671372,
8.85933012996512));
#390419=CARTESIAN_POINT('Ctrl Pts',(-0.337024709144314,2.64180589483668,
8.86332496987231));
#390420=CARTESIAN_POINT('Ctrl Pts',(-0.332486490925511,2.64267564754589,
8.86648636486737));
#390421=CARTESIAN_POINT('Ctrl Pts',(-0.32982152219722,2.6374055390489,8.87206031107457));
#390422=CARTESIAN_POINT('Ctrl Pts',(-0.344083317655468,2.64086469778923,
8.86341338519876));
#390423=CARTESIAN_POINT('Ctrl Pts',(-0.348704757116131,2.64052445089996,
8.86654584966059));
#390424=CARTESIAN_POINT('Ctrl Pts',(-0.349892026593743,2.63471802825129,
8.87215952290714));
#390425=CARTESIAN_POINT('Ctrl Pts',(-0.347133565397089,2.64507775146798,
8.85049129520029));
#390426=CARTESIAN_POINT('Ctrl Pts',(-0.350558127032894,2.649807813817,8.85711686593484));
#390427=CARTESIAN_POINT('Ctrl Pts',(-0.358444815903127,2.64650616259708,
8.85933012996512));
#390428=CARTESIAN_POINT('Origin',(-0.323502373428199,2.64209967160839,8.85049129520029));
#390429=CARTESIAN_POINT('Ctrl Pts',(-0.309289785090423,2.71327145765926,
8.78727029226991));
#390430=CARTESIAN_POINT('Ctrl Pts',(-0.307150726644354,2.71878324544933,
8.79393457792714));
#390431=CARTESIAN_POINT('Ctrl Pts',(-0.298601974927904,2.71753494289437,
8.79610912703474));
#390432=CARTESIAN_POINT('Ctrl Pts',(-0.317899498928061,2.69108650254806,
8.80838214965001));
#390433=CARTESIAN_POINT('Ctrl Pts',(-0.315760795727614,2.69659737496409,
8.81501364461985));
#390434=CARTESIAN_POINT('Ctrl Pts',(-0.307247094031194,2.69534609720933,
8.81722098428721));
#390435=CARTESIAN_POINT('Ctrl Pts',(-0.326521105202102,2.66887090377404,
8.82945683644721));
#390436=CARTESIAN_POINT('Ctrl Pts',(-0.324390809144525,2.67436011320682,
8.83607469902389));
#390437=CARTESIAN_POINT('Ctrl Pts',(-0.315904953537554,2.67312629915468,
8.8382956714852));
#390438=CARTESIAN_POINT('Ctrl Pts',(-0.33515558185988,2.64662214142562,
8.85049129520029));
#390439=CARTESIAN_POINT('Ctrl Pts',(-0.333042822978414,2.65206616219449,
8.85711686593484));
#390440=CARTESIAN_POINT('Ctrl Pts',(-0.324576590381445,2.65087298671372,
8.85933012996512));
#390441=CARTESIAN_POINT('Origin',(-0.297636576658742,2.70874898784202,8.78727029226991));
#390442=CARTESIAN_POINT('Ctrl Pts',(-0.304283422748602,2.72617147813989,
8.75374538247847));
#390443=CARTESIAN_POINT('Ctrl Pts',(-0.301546370683836,2.73326040784629,
8.75304829418601));
#390444=CARTESIAN_POINT('Ctrl Pts',(-0.293954221614899,2.73405408014902,
8.75272238421917));
#390445=CARTESIAN_POINT('Ctrl Pts',(-0.303805856238297,2.72740204188969,
8.76769408445023));
#390446=CARTESIAN_POINT('Ctrl Pts',(-0.300999284012138,2.73466911195344,
8.76974318093973));
#390447=CARTESIAN_POINT('Ctrl Pts',(-0.293509920856647,2.73563233404903,
8.7707786988043));
#390448=CARTESIAN_POINT('Ctrl Pts',(-0.306253590132211,2.72109487311948,
8.78108014887986));
#390449=CARTESIAN_POINT('Ctrl Pts',(-0.30387866553322,2.72725482201938,
8.78639403366321));
#390450=CARTESIAN_POINT('Ctrl Pts',(-0.295789548083303,2.72755189879462,
8.78812224174741));
#390451=CARTESIAN_POINT('Ctrl Pts',(-0.310264885608762,2.71075881581417,
8.78944554828686));
#390452=CARTESIAN_POINT('Ctrl Pts',(-0.308268610199807,2.71595220604683,
8.79673892988687));
#390453=CARTESIAN_POINT('Ctrl Pts',(-0.299498741631327,2.71434193910989,
8.79894799272499));
#390454=CARTESIAN_POINT('Origin',(-0.292563240664618,2.72182163269598,8.75721825406948));
#390455=CARTESIAN_POINT('Origin',(-0.292563240664618,2.72182163269598,9.));
#390456=CARTESIAN_POINT('Origin',(-0.292563240664619,2.72182163269598,7.51860402984325));
#390457=CARTESIAN_POINT('Ctrl Pts',(-0.312368237512607,2.72851585273769,
7.50366195182966));
#390458=CARTESIAN_POINT('Ctrl Pts',(-0.312784747585389,2.73215404062032,
7.50000065167735));
#390459=CARTESIAN_POINT('Ctrl Pts',(-0.312784747585273,2.73215404062034,
7.49482233047108));
#390460=CARTESIAN_POINT('Ctrl Pts',(-0.305300246324094,2.73083906176095,
7.50215800491336));
#390461=CARTESIAN_POINT('Ctrl Pts',(-0.303313249275625,2.73323834079927,
7.49877273257266));
#390462=CARTESIAN_POINT('Ctrl Pts',(-0.299883530860003,2.73363100852074,
7.49481816995649));
#390463=CARTESIAN_POINT('Ctrl Pts',(-0.303197007877448,2.72897187018571,
7.51043025814043));
#390464=CARTESIAN_POINT('Ctrl Pts',(-0.299675308765067,2.73362916471674,
7.51006209594515));
#390465=CARTESIAN_POINT('Ctrl Pts',(-0.293896628507968,2.73425031256432,
7.507312818217));
#390466=CARTESIAN_POINT('Ctrl Pts',(-0.304216995834675,2.72634269346048,
7.51860402984326));
#390467=CARTESIAN_POINT('Ctrl Pts',(-0.301464837418634,2.7334368207108,
7.51860402984327));
#390468=CARTESIAN_POINT('Ctrl Pts',(-0.293899145873127,2.7342500419777,
7.51860402984327));
#390469=CARTESIAN_POINT('Origin',(0.,0.,7.5));
#390470=CARTESIAN_POINT('Origin',(-0.504036631578591,2.6197108805292,7.5));
#390471=CARTESIAN_POINT('',(-0.504036631578591,2.6197108805292,7.59394543036555));
#390472=CARTESIAN_POINT('',(-0.504036631578591,2.6197108805292,8.85049129520029));
#390473=CARTESIAN_POINT('',(-0.504036631578591,2.6197108805292,7.5));
#390474=CARTESIAN_POINT('',(-0.482494215215348,2.68788048588352,8.78727029226991));
#390475=CARTESIAN_POINT('Ctrl Pts',(-0.504036631578591,2.6197108805292,
8.85049129520029));
#390476=CARTESIAN_POINT('Ctrl Pts',(-0.496845388128025,2.64246711268839,
8.82945686509571));
#390477=CARTESIAN_POINT('Ctrl Pts',(-0.489664835330401,2.66518951495683,
8.80838212259896));
#390478=CARTESIAN_POINT('Ctrl Pts',(-0.482494215215348,2.68788048588352,
8.78727029226991));
#390479=CARTESIAN_POINT('',(-0.478268870165661,2.70125132133977,8.75721825406948));
#390480=CARTESIAN_POINT('Origin',(-0.490984591625891,2.6610138998837,8.75937679713081));
#390481=CARTESIAN_POINT('',(-0.478268870165661,2.70125132133977,7.51860402984325));
#390482=CARTESIAN_POINT('',(-0.478268870165661,2.70125132133977,7.5));
#390483=CARTESIAN_POINT('Ctrl Pts',(-0.478268870165661,2.70125132133977,
7.51860402984325));
#390484=CARTESIAN_POINT('Ctrl Pts',(-0.481587221536733,2.69075060964715,
7.52834476460825));
#390485=CARTESIAN_POINT('Ctrl Pts',(-0.484907727133636,2.68024308104402,
7.53807742314407));
#390486=CARTESIAN_POINT('Ctrl Pts',(-0.488230459287361,2.66972850664355,
7.54780169004674));
#390487=CARTESIAN_POINT('Ctrl Pts',(-0.493493487440511,2.65307398905746,
7.5632044032688));
#390488=CARTESIAN_POINT('Ctrl Pts',(-0.498762108429668,2.63640177329775,
7.57858609112103));
#390489=CARTESIAN_POINT('Ctrl Pts',(-0.504036631578591,2.6197108805292,
7.59394543036555));
#390490=CARTESIAN_POINT('Origin',(-0.691101205365338,2.82936072626276,7.5));
#390491=CARTESIAN_POINT('',(-0.570375062512128,2.68331364198702,8.75721825406948));
#390492=CARTESIAN_POINT('',(-0.561440886005602,2.67250562312429,8.78727029226991));
#390493=CARTESIAN_POINT('Origin',(-0.538762613750377,2.64507084006066,8.75658640621043));
#390494=CARTESIAN_POINT('',(-0.515891055659666,2.61740223164621,8.85049129520029));
#390495=CARTESIAN_POINT('Ctrl Pts',(-0.561440886005602,2.67250562312429,
8.78727029226991));
#390496=CARTESIAN_POINT('Ctrl Pts',(-0.546279145362939,2.6541638790656,
8.80838212259896));
#390497=CARTESIAN_POINT('Ctrl Pts',(-0.531096402804868,2.63579672817756,
8.82945686509571));
#390498=CARTESIAN_POINT('Ctrl Pts',(-0.515891055659666,2.61740223164621,
8.85049129520029));
#390499=CARTESIAN_POINT('',(-0.515891055659666,2.61740223164621,7.59394543036555));
#390500=CARTESIAN_POINT('',(-0.515891055659666,2.61740223164621,7.5));
#390501=CARTESIAN_POINT('',(-0.570375062512128,2.68331364198702,7.51860402984325));
#390502=CARTESIAN_POINT('Ctrl Pts',(-0.515891055659666,2.61740223164621,
7.59394543036555));
#390503=CARTESIAN_POINT('Ctrl Pts',(-0.527043640891426,2.63089394534417,
7.57858609112103));
#390504=CARTESIAN_POINT('Ctrl Pts',(-0.538183746447094,2.64437056189533,
7.56320440326857));
#390505=CARTESIAN_POINT('Ctrl Pts',(-0.549312026368875,2.65783287251976,
7.54780169004651));
#390506=CARTESIAN_POINT('Ctrl Pts',(-0.556337695325183,2.66633209598458,
7.53807742314383));
#390507=CARTESIAN_POINT('Ctrl Pts',(-0.563358656393526,2.67482562413523,
7.52834476460825));
#390508=CARTESIAN_POINT('Ctrl Pts',(-0.570375062512127,2.68331364198702,
7.51860402984325));
#390509=CARTESIAN_POINT('',(-0.570375062512128,2.68331364198702,7.5));
#390510=CARTESIAN_POINT('Origin',(-0.510592093294252,2.62178248538885,7.5));
#390511=CARTESIAN_POINT('Ctrl Pts',(-0.515891055659666,2.61740223164621,
8.85049129520029));
#390512=CARTESIAN_POINT('Ctrl Pts',(-0.515767668527143,2.61725296545981,
8.85097269580138));
#390513=CARTESIAN_POINT('Ctrl Pts',(-0.515639354986829,2.61711094168747,
8.85143669361005));
#390514=CARTESIAN_POINT('Ctrl Pts',(-0.515499557882527,2.61697020670063,
8.8519052845931));
#390515=CARTESIAN_POINT('Ctrl Pts',(-0.515226123612123,2.61669493799147,
8.85282181883899));
#390516=CARTESIAN_POINT('Ctrl Pts',(-0.514915651119187,2.61643181964957,
8.85372622499635));
#390517=CARTESIAN_POINT('Ctrl Pts',(-0.514553299874838,2.61618848567121,
8.8546225773507));
#390518=CARTESIAN_POINT('Ctrl Pts',(-0.514252488741278,2.61598647844478,
8.85536669723986));
#390519=CARTESIAN_POINT('Ctrl Pts',(-0.513915873198243,2.61579803376955,
8.85610498449051));
#390520=CARTESIAN_POINT('Ctrl Pts',(-0.513531024767989,2.61563448612492,
8.85681338218371));
#390521=CARTESIAN_POINT('Ctrl Pts',(-0.513181774213118,2.61548606638055,
8.85745625420284));
#390522=CARTESIAN_POINT('Ctrl Pts',(-0.512788654114669,2.61535573822306,
8.85808743050666));
#390523=CARTESIAN_POINT('Ctrl Pts',(-0.512331828562521,2.61526410220628,
8.8586680450841));
#390524=CARTESIAN_POINT('Ctrl Pts',(-0.512121059155524,2.61522182333457,
8.85893592806395));
#390525=CARTESIAN_POINT('Ctrl Pts',(-0.511896582696646,2.61518797425763,
8.85919241173848));
#390526=CARTESIAN_POINT('Ctrl Pts',(-0.511655676326038,2.61516597374877,
8.85943017985534));
#390527=CARTESIAN_POINT('Ctrl Pts',(-0.511330381409799,2.61513626654896,
8.8597512372));
#390528=CARTESIAN_POINT('Ctrl Pts',(-0.510966791987485,2.61512804460748,
8.86004599534705));
#390529=CARTESIAN_POINT('Ctrl Pts',(-0.510569040990299,2.61515181913895,
8.86026130871721));
#390530=CARTESIAN_POINT('Ctrl Pts',(-0.510423413136441,2.61516052366519,
8.86034014101235));
#390531=CARTESIAN_POINT('Ctrl Pts',(-0.510271017703912,2.61517363576241,
8.86040910639692));
#390532=CARTESIAN_POINT('Ctrl Pts',(-0.510116035456201,2.61519113333938,
8.86046313645506));
#390533=CARTESIAN_POINT('Ctrl Pts',(-0.509874186956613,2.61521843816169,
8.86054744990829));
#390534=CARTESIAN_POINT('Ctrl Pts',(-0.509619453975295,2.61525731366695,
8.86059655985668));
#390535=CARTESIAN_POINT('Ctrl Pts',(-0.509368129116534,2.61530497704636,
8.86059725258816));
#390536=CARTESIAN_POINT('Ctrl Pts',(-0.509116223596944,2.61535275054721,
8.86059794692011));
#390537=CARTESIAN_POINT('Ctrl Pts',(-0.508865443335376,2.61541249263374,
8.86056369958366));
#390538=CARTESIAN_POINT('Ctrl Pts',(-0.508628593949195,2.61547728428475,
8.86048590497774));
#390539=CARTESIAN_POINT('Ctrl Pts',(-0.508566783311257,2.61549419297658,
8.86046560290182));
#390540=CARTESIAN_POINT('Ctrl Pts',(-0.508505141221149,2.61551175291262,
8.86044257503091));
#390541=CARTESIAN_POINT('Ctrl Pts',(-0.50844556347711,2.61552938990613,
8.86041778462584));
#390542=CARTESIAN_POINT('Ctrl Pts',(-0.50804467918954,2.61564806498672,
8.86025097596201));
#390543=CARTESIAN_POINT('Ctrl Pts',(-0.507683561495978,2.61578647179151,
8.8599848982295));
#390544=CARTESIAN_POINT('Ctrl Pts',(-0.507369718277689,2.61593265927751,
8.85968173251461));
#390545=CARTESIAN_POINT('Ctrl Pts',(-0.507203713196287,2.61600998408207,
8.85952137522076));
#390546=CARTESIAN_POINT('Ctrl Pts',(-0.507047654086865,2.61609080315807,
8.85934740853961));
#390547=CARTESIAN_POINT('Ctrl Pts',(-0.506903026841176,2.61617259635409,
8.8591675900182));
#390548=CARTESIAN_POINT('Ctrl Pts',(-0.506322273273992,2.61650103855137,
8.85844552518696));
#390549=CARTESIAN_POINT('Ctrl Pts',(-0.505891539218353,2.61686111677502,
8.85759444184127));
#390550=CARTESIAN_POINT('Ctrl Pts',(-0.505566712158157,2.61718625003458,
8.85683498915142));
#390551=CARTESIAN_POINT('Ctrl Pts',(-0.505532719871388,2.6172202743643,
8.85675551445));
#390552=CARTESIAN_POINT('Ctrl Pts',(-0.505499903995347,2.61725392708393,
8.85667699793652));
#390553=CARTESIAN_POINT('Ctrl Pts',(-0.505468225267547,2.61728713860215,
8.85659965593547));
#390554=CARTESIAN_POINT('Ctrl Pts',(-0.50504062418328,2.61773542936974,
8.85555568965886));
#390555=CARTESIAN_POINT('Ctrl Pts',(-0.504694415106446,2.61822801862891,
8.85434650606346));
#390556=CARTESIAN_POINT('Ctrl Pts',(-0.50442280204503,2.61876376787636,
8.85297329937117));
#390557=CARTESIAN_POINT('Ctrl Pts',(-0.50427003624761,2.61906509418437,
8.85220095427747));
#390558=CARTESIAN_POINT('Ctrl Pts',(-0.50414108661597,2.61938033921224,
8.85137579139183));
#390559=CARTESIAN_POINT('Ctrl Pts',(-0.504036631578591,2.6197108805292,
8.85049129520029));
#390560=CARTESIAN_POINT('Origin',(-0.510592093294252,2.62178248538885,7.59394543036555));
#390561=CARTESIAN_POINT('Ctrl Pts',(-0.515532821189696,2.61696886155263,
7.59443877723642));
#390562=CARTESIAN_POINT('Ctrl Pts',(-0.511843350832965,2.61250556656624,
7.58783886950016));
#390563=CARTESIAN_POINT('Ctrl Pts',(-0.504225634743617,2.61625384391974,
7.58559994247159));
#390564=CARTESIAN_POINT('Ctrl Pts',(-0.535673531622635,2.6413338579358,
7.56670252222136));
#390565=CARTESIAN_POINT('Ctrl Pts',(-0.531989393598023,2.63687701367783,
7.56004874999029));
#390566=CARTESIAN_POINT('Ctrl Pts',(-0.524317107068314,2.64062833033498,
7.55786368756704));
#390567=CARTESIAN_POINT('Ctrl Pts',(-0.555776631291146,2.66565335512259,
7.53888913333559));
#390568=CARTESIAN_POINT('Ctrl Pts',(-0.552070598253881,2.66117002362097,
7.53222002137278));
#390569=CARTESIAN_POINT('Ctrl Pts',(-0.544372672437959,2.66495742152094,
7.53005029815327));
#390570=CARTESIAN_POINT('Ctrl Pts',(-0.575841210516351,2.68992625263927,
7.51101258149734));
#390571=CARTESIAN_POINT('Ctrl Pts',(-0.572090253624643,2.68538857501344,
7.5043616886572));
#390572=CARTESIAN_POINT('Ctrl Pts',(-0.564391276187486,2.68923996800388,
7.50217374673251));
#390573=CARTESIAN_POINT('',(-0.563323058569149,2.68794421947736,7.50366116523517));
#390574=CARTESIAN_POINT('Ctrl Pts',(-0.570375062512129,2.68331364198702,
7.51860402984325));
#390575=CARTESIAN_POINT('Ctrl Pts',(-0.570656425301962,2.68365401743601,
7.51734760759493));
#390576=CARTESIAN_POINT('Ctrl Pts',(-0.570864819165481,2.68399950239607,
7.51608817408573));
#390577=CARTESIAN_POINT('Ctrl Pts',(-0.570988330268519,2.6843561994528,
7.5148100591312));
#390578=CARTESIAN_POINT('Ctrl Pts',(-0.571100209577045,2.68467930417034,
7.51365231206383));
#390579=CARTESIAN_POINT('Ctrl Pts',(-0.571142835244524,2.6850119821901,
7.51247773061042));
#390580=CARTESIAN_POINT('Ctrl Pts',(-0.571078844074294,2.68535316978938,
7.51129758471022));
#390581=CARTESIAN_POINT('Ctrl Pts',(-0.570999310357765,2.6857772270102,
7.50983079813401));
#390582=CARTESIAN_POINT('Ctrl Pts',(-0.570744815553289,2.6861984949357,
7.50839324291155));
#390583=CARTESIAN_POINT('Ctrl Pts',(-0.570242939355954,2.6865774199326,
7.50715379678855));
#390584=CARTESIAN_POINT('Ctrl Pts',(-0.570011087014001,2.68675247236271,
7.50658120839351));
#390585=CARTESIAN_POINT('Ctrl Pts',(-0.569687753921535,2.68693579028516,
7.50598221009429));
#390586=CARTESIAN_POINT('Ctrl Pts',(-0.569269416203865,2.6871032235564,
7.50545747549611));
#390587=CARTESIAN_POINT('Ctrl Pts',(-0.569046178248952,2.68719257113247,
7.50517746087247));
#390588=CARTESIAN_POINT('Ctrl Pts',(-0.568793541135426,2.68727855221161,
7.50491486231392));
#390589=CARTESIAN_POINT('Ctrl Pts',(-0.568517657707549,2.68735731079858,
7.50468370960992));
#390590=CARTESIAN_POINT('Ctrl Pts',(-0.568105124960383,2.68747507972909,
7.50433806340447));
#390591=CARTESIAN_POINT('Ctrl Pts',(-0.567628091085996,2.68757969554714,
7.50405484070984));
#390592=CARTESIAN_POINT('Ctrl Pts',(-0.567118529966982,2.68766341280671,
7.50385766036131));
#390593=CARTESIAN_POINT('Ctrl Pts',(-0.567064040325673,2.68767236506636,
7.50383657498791));
#390594=CARTESIAN_POINT('Ctrl Pts',(-0.567009205172207,2.68768108862484,
7.50381643264937));
#390595=CARTESIAN_POINT('Ctrl Pts',(-0.566954082693363,2.68768958177397,
7.50379723213559));
#390596=CARTESIAN_POINT('Ctrl Pts',(-0.566586122115288,2.68774627632267,
7.50366906242519));
#390597=CARTESIAN_POINT('Ctrl Pts',(-0.566197244826902,2.68779322640586,
7.50358235568538));
#390598=CARTESIAN_POINT('Ctrl Pts',(-0.565821327165834,2.68782947036995,
7.5035341175365));
#390599=CARTESIAN_POINT('Ctrl Pts',(-0.565257681178725,2.68788381409206,
7.50346178989176));
#390600=CARTESIAN_POINT('Ctrl Pts',(-0.564649015727611,2.6879183099948,
7.50346967198527));
#390601=CARTESIAN_POINT('Ctrl Pts',(-0.564050452828134,2.6879337885485,
7.50354272648692));
#390602=CARTESIAN_POINT('Ctrl Pts',(-0.563804251518062,2.68794015519803,
7.50357277531559));
#390603=CARTESIAN_POINT('Ctrl Pts',(-0.56356009019173,2.68794343769315,
7.50361331098761));
#390604=CARTESIAN_POINT('Ctrl Pts',(-0.56332305856944,2.68794421947875,
7.50366116523658));
#390605=CARTESIAN_POINT('',(-0.511151791456907,2.62465641716285,7.57603338622103));
#390606=CARTESIAN_POINT('Origin',(-0.512838247935151,2.63333094044407,7.58486873427626));
#390607=CARTESIAN_POINT('Ctrl Pts',(-0.563323058609602,2.68794421951801,
7.50366116529968));
#390608=CARTESIAN_POINT('Ctrl Pts',(-0.545960368869896,2.66688324129278,
7.52783573079709));
#390609=CARTESIAN_POINT('Ctrl Pts',(-0.528570753762134,2.6457883146349,
7.55196141284068));
#390610=CARTESIAN_POINT('Ctrl Pts',(-0.511151792493766,2.62465641786469,
7.57603338728831));
#390611=CARTESIAN_POINT('Ctrl Pts',(-0.516410771457565,2.61830690341526,
7.59639677331371));
#390612=CARTESIAN_POINT('Ctrl Pts',(-0.507139096305122,2.60255546044572,
7.59959882295469));
#390613=CARTESIAN_POINT('Ctrl Pts',(-0.503923606568019,2.6205657196987,
7.59642833564546));
#390614=CARTESIAN_POINT('Ctrl Pts',(-0.514998153140207,2.6146710247631,
7.58707626057421));
#390615=CARTESIAN_POINT('Ctrl Pts',(-0.508781048698786,2.61197660397168,
7.58809943920599));
#390616=CARTESIAN_POINT('Ctrl Pts',(-0.503963188820572,2.61672029736263,
7.58710240504253));
#390617=CARTESIAN_POINT('Ctrl Pts',(-0.51247784845448,2.62020037341849,
7.5801537675693));
#390618=CARTESIAN_POINT('Ctrl Pts',(-0.510031459795522,2.61873597800557,
7.58205880659761));
#390619=CARTESIAN_POINT('Ctrl Pts',(-0.508301387520508,2.62095722201767,
7.58020924244127));
#390620=CARTESIAN_POINT('Ctrl Pts',(-0.511151791298909,2.62465641635051,
7.57603338509286));
#390621=CARTESIAN_POINT('Ctrl Pts',(-0.511151791298909,2.62465641635051,
7.57603338509286));
#390622=CARTESIAN_POINT('Ctrl Pts',(-0.511151791298909,2.62465641635051,
7.57603338509286));
#390623=CARTESIAN_POINT('Origin',(-0.512843849057692,2.63332984962579,7.58486873427619));
#390624=CARTESIAN_POINT('Ctrl Pts',(-0.475675529955941,2.70945778136102,
7.51098857897448));
#390625=CARTESIAN_POINT('Ctrl Pts',(-0.477449522153347,2.70384409597124,
7.50433767179956));
#390626=CARTESIAN_POINT('Ctrl Pts',(-0.486031165786666,2.70452486291607,
7.50214974420965));
#390627=CARTESIAN_POINT('Ctrl Pts',(-0.485167636506951,2.679420614376,7.53887321589167));
#390628=CARTESIAN_POINT('Ctrl Pts',(-0.486920373129571,2.67387419089971,
7.53220407452062));
#390629=CARTESIAN_POINT('Ctrl Pts',(-0.495477023428703,2.67449600725536,
7.53003438070911));
#390630=CARTESIAN_POINT('Ctrl Pts',(-0.494677971404018,2.64932576495017,
7.56669465659235));
#390631=CARTESIAN_POINT('Ctrl Pts',(-0.496420349679053,2.64381211980541,
7.560040858333));
#390632=CARTESIAN_POINT('Ctrl Pts',(-0.504939684355754,2.6444101054177,
7.55785582193789));
#390633=CARTESIAN_POINT('Ctrl Pts',(-0.504206104532792,2.619174594153,7.59443891967696));
#390634=CARTESIAN_POINT('Ctrl Pts',(-0.505951009039396,2.61365295490927,
7.58783901202978));
#390635=CARTESIAN_POINT('Ctrl Pts',(-0.514418602349896,2.61426861838577,
7.58560008491213));
#390636=CARTESIAN_POINT('',(-0.486543193738941,2.70289709681367,7.50366116523517));
#390637=CARTESIAN_POINT('Ctrl Pts',(-0.486543193739007,2.70289709681404,
7.50366116523554));
#390638=CARTESIAN_POINT('Ctrl Pts',(-0.485839853899794,2.7031789666197,
7.50350835821027));
#390639=CARTESIAN_POINT('Ctrl Pts',(-0.48518414354119,2.70341519095537,
7.50345484955999));
#390640=CARTESIAN_POINT('Ctrl Pts',(-0.484556771391452,2.70361335792061,
7.50349758195598));
#390641=CARTESIAN_POINT('Ctrl Pts',(-0.484234882951505,2.70371503227022,
7.50351950684424));
#390642=CARTESIAN_POINT('Ctrl Pts',(-0.483888766775207,2.70381683307007,
7.50357029184312));
#390643=CARTESIAN_POINT('Ctrl Pts',(-0.483552312554448,2.70390582412704,
7.50365515313923));
#390644=CARTESIAN_POINT('Ctrl Pts',(-0.48303470971915,2.70404272840869,
7.50378570417639));
#390645=CARTESIAN_POINT('Ctrl Pts',(-0.482524868782461,2.70415367027655,
7.50400001621911));
#390646=CARTESIAN_POINT('Ctrl Pts',(-0.482061113295957,2.70422798694399,
7.50428903009635));
#390647=CARTESIAN_POINT('Ctrl Pts',(-0.482009640004878,2.70423623552231,
7.50432110841318));
#390648=CARTESIAN_POINT('Ctrl Pts',(-0.481958712533376,2.70424405384474,
7.50435406373354));
#390649=CARTESIAN_POINT('Ctrl Pts',(-0.481908366893239,2.70425144256795,
7.50438785222351));
#390650=CARTESIAN_POINT('Ctrl Pts',(-0.481600982560994,2.70429655427464,
7.50459414719561));
#390651=CARTESIAN_POINT('Ctrl Pts',(-0.48131031833417,2.70432585979777,
7.50483629897752));
#390652=CARTESIAN_POINT('Ctrl Pts',(-0.481047641490116,2.70433954584457,
7.5050991045531));
#390653=CARTESIAN_POINT('Ctrl Pts',(-0.480468149988743,2.70436973863845,
7.50567888004914));
#390654=CARTESIAN_POINT('Ctrl Pts',(-0.480002061491276,2.7043256226731,
7.50637912803144));
#390655=CARTESIAN_POINT('Ctrl Pts',(-0.479638530743235,2.70423614270301,
7.50710440483569));
#390656=CARTESIAN_POINT('Ctrl Pts',(-0.479549385786719,2.70421420043792,
7.50728225710685));
#390657=CARTESIAN_POINT('Ctrl Pts',(-0.479464598424601,2.70418923522453,
7.50746498566954));
#390658=CARTESIAN_POINT('Ctrl Pts',(-0.479386030199354,2.70416222946144,
7.50764697238949));
#390659=CARTESIAN_POINT('Ctrl Pts',(-0.47896366904298,2.70401705391124,
7.50862528291182));
#390660=CARTESIAN_POINT('Ctrl Pts',(-0.478681344736173,2.70380364525162,
7.50965856837423));
#390661=CARTESIAN_POINT('Ctrl Pts',(-0.478486337883089,2.70356220374557,
7.51067959873204));
#390662=CARTESIAN_POINT('Ctrl Pts',(-0.47837902536587,2.70342933818025,
7.5112414730258));
#390663=CARTESIAN_POINT('Ctrl Pts',(-0.478298467079306,2.70328767800995,
7.51180065547253));
#390664=CARTESIAN_POINT('Ctrl Pts',(-0.478238051202743,2.70314229426445,
7.51235175716501));
#390665=CARTESIAN_POINT('Ctrl Pts',(-0.478029290282389,2.70263993550974,
7.51425603304535));
#390666=CARTESIAN_POINT('Ctrl Pts',(-0.478041734656937,2.70203089399621,
7.51626900505179));
#390667=CARTESIAN_POINT('Ctrl Pts',(-0.478235751309913,2.70136068775766,
7.51827788969242));
#390668=CARTESIAN_POINT('Ctrl Pts',(-0.478246251857814,2.70132441492951,
7.51838661432544));
#390669=CARTESIAN_POINT('Ctrl Pts',(-0.478257292668706,2.70128795759193,
7.51849533314856));
#390670=CARTESIAN_POINT('Ctrl Pts',(-0.478268870165657,2.70125132133976,
7.51860402984325));
#390671=CARTESIAN_POINT('Ctrl Pts',(-0.51115179075919,2.62465641820371,
7.57603338728985));
#390672=CARTESIAN_POINT('Ctrl Pts',(-0.502935967270557,2.6507806888637,
7.55196141284922));
#390673=CARTESIAN_POINT('Ctrl Pts',(-0.494733471561833,2.67685967867694,
7.52783573083105));
#390674=CARTESIAN_POINT('Ctrl Pts',(-0.486543193716074,2.70289709686826,
7.50366116530176));
#390675=CARTESIAN_POINT('Origin',(-1.76626572250576E-16,9.06940118467443E-16,
7.49482233047033));
#390676=CARTESIAN_POINT('Origin',(-0.561510055974246,2.6792933223221,7.49482233047033));
#390677=CARTESIAN_POINT('Origin',(0.,0.,7.50366116523517));
#390678=CARTESIAN_POINT('Origin',(-0.484977299960294,2.69419807522076,7.49482233047033));
#390679=CARTESIAN_POINT('Ctrl Pts',(-0.570374388643616,2.68331282671198,
7.51860402984325));
#390680=CARTESIAN_POINT('Ctrl Pts',(-0.575221773022837,2.68917790562962,
7.51860402984325));
#390681=CARTESIAN_POINT('Ctrl Pts',(-0.582657984926183,2.68756575223785,
7.51860402984325));
#390682=CARTESIAN_POINT('Ctrl Pts',(-0.572174256523385,2.68549056972994,
7.51041458714365));
#390683=CARTESIAN_POINT('Ctrl Pts',(-0.576983494698349,2.68879595835108,
7.5100464290044));
#390684=CARTESIAN_POINT('Ctrl Pts',(-0.582660035745125,2.68756530762508,
7.50729136483009));
#390685=CARTESIAN_POINT('Ctrl Pts',(-0.570756300477604,2.68792226417035,
7.50215815450138));
#390686=CARTESIAN_POINT('Ctrl Pts',(-0.573396483322125,2.68957377833286,
7.49877163671533));
#390687=CARTESIAN_POINT('Ctrl Pts',(-0.576773332211222,2.68886609537093,
7.49481588533172));
#390688=CARTESIAN_POINT('Ctrl Pts',(-0.563322945647624,2.68794368066495,
7.50366171572174));
#390689=CARTESIAN_POINT('Ctrl Pts',(-0.564074028832197,2.69152753840584,
7.50000045605858));
#390690=CARTESIAN_POINT('Ctrl Pts',(-0.564074028832319,2.69152753840582,
7.49482233047317));
#390691=CARTESIAN_POINT('Origin',(-0.580009539540154,2.67534954427313,7.51860402984325));
#390692=CARTESIAN_POINT('Origin',(-0.580009539540154,2.67534954427313,9.));
#390693=CARTESIAN_POINT('Origin',(-0.580009539540154,2.67534954427313,8.75721825406948));
#390694=CARTESIAN_POINT('Ctrl Pts',(-0.559734948604734,2.67044183725424,
8.78942910404913));
#390695=CARTESIAN_POINT('Ctrl Pts',(-0.563269725412667,2.67474971162797,
8.7967269950169));
#390696=CARTESIAN_POINT('Ctrl Pts',(-0.571092507684332,2.67045115797444,
8.79893251111267));
#390697=CARTESIAN_POINT('Ctrl Pts',(-0.566739742255377,2.67891581416313,
8.78111911759577));
#390698=CARTESIAN_POINT('Ctrl Pts',(-0.570936015679921,2.68401812731229,
8.78644465894813));
#390699=CARTESIAN_POINT('Ctrl Pts',(-0.578712537116064,2.68172875488109,
8.78817647674132));
#390700=CARTESIAN_POINT('Ctrl Pts',(-0.57110529676308,2.68419699867589,
8.76780923932035));
#390701=CARTESIAN_POINT('Ctrl Pts',(-0.576062756082901,2.69021682706735,
8.76988516158374));
#390702=CARTESIAN_POINT('Ctrl Pts',(-0.583481134049413,2.68876629311658,
8.77093053738834));
#390703=CARTESIAN_POINT('Ctrl Pts',(-0.570254073382235,2.6831672399729,
8.75371302330491));
#390704=CARTESIAN_POINT('Ctrl Pts',(-0.57508927265449,2.68903980750043,
8.75300828287559));
#390705=CARTESIAN_POINT('Ctrl Pts',(-0.582551442759682,2.68739343067373,
8.75267964240737));
#390706=CARTESIAN_POINT('Origin',(-0.571075363033628,2.66454152541039,8.78727029226991));
#390707=CARTESIAN_POINT('Ctrl Pts',(-0.515891055659666,2.61740223164621,
8.85049129520029));
#390708=CARTESIAN_POINT('Ctrl Pts',(-0.519611637301531,2.6219031631575,
8.85711686593484));
#390709=CARTESIAN_POINT('Ctrl Pts',(-0.527270584603676,2.61810299364327,
8.85933012996512));
#390710=CARTESIAN_POINT('Ctrl Pts',(-0.53109642321101,2.63579675286366,
8.82945683644724));
#390711=CARTESIAN_POINT('Ctrl Pts',(-0.53484788793001,2.64033504482781,
8.8360746990239));
#390712=CARTESIAN_POINT('Ctrl Pts',(-0.542512653014755,2.63649012367216,
8.8382956714852));
#390713=CARTESIAN_POINT('Ctrl Pts',(-0.54627912593586,2.65416385556391,
8.80838214965003));
#390714=CARTESIAN_POINT('Ctrl Pts',(-0.55004539568616,2.65872005774703,
8.81501364461989));
#390715=CARTESIAN_POINT('Ctrl Pts',(-0.557731085305916,2.6548497880324,
8.81722098428721));
#390716=CARTESIAN_POINT('Ctrl Pts',(-0.561440886005602,2.67250562312429,
8.78727029226991));
#390717=CARTESIAN_POINT('Ctrl Pts',(-0.565207781345687,2.67706258210756,
8.79393457792714));
#390718=CARTESIAN_POINT('Ctrl Pts',(-0.572927672898306,2.67318409147408,
8.79610912703474));
#390719=CARTESIAN_POINT('Origin',(-0.525525532687691,2.60943813393231,8.85049129520029));
#390720=CARTESIAN_POINT('Ctrl Pts',(-0.504036631578591,2.6197108805292,
8.85049129520029));
#390721=CARTESIAN_POINT('Ctrl Pts',(-0.502277013195081,2.62527908089984,
8.85711686593484));
#390722=CARTESIAN_POINT('Ctrl Pts',(-0.493751728365454,2.62463079031095,
8.85933012996512));
#390723=CARTESIAN_POINT('Ctrl Pts',(-0.505593340562126,2.61478477403912,
8.86332496987232));
#390724=CARTESIAN_POINT('Ctrl Pts',(-0.501120171846769,2.61594350438772,
8.86648636486738));
#390725=CARTESIAN_POINT('Ctrl Pts',(-0.498123021571836,2.61085496902652,
8.87206031107457));
#390726=CARTESIAN_POINT('Ctrl Pts',(-0.512577143703185,2.61339326418189,
8.86341338519875));
#390727=CARTESIAN_POINT('Ctrl Pts',(-0.517167288227793,2.61275761972348,
8.86654584966058));
#390728=CARTESIAN_POINT('Ctrl Pts',(-0.517980099556504,2.60688705837628,
8.87215952290714));
#390729=CARTESIAN_POINT('Ctrl Pts',(-0.515891055659666,2.61740223164621,
8.85049129520029));
#390730=CARTESIAN_POINT('Ctrl Pts',(-0.519611637301531,2.6219031631575,
8.85711686593484));
#390731=CARTESIAN_POINT('Ctrl Pts',(-0.527270584603676,2.61810299364327,
8.85933012996512));
#390732=CARTESIAN_POINT('Origin',(-0.492117610277389,2.61594432623894,8.85049129520029));
#390733=CARTESIAN_POINT('Ctrl Pts',(-0.482494215215348,2.68788048588352,
8.78727029226991));
#390734=CARTESIAN_POINT('Ctrl Pts',(-0.480712693150467,2.69351799905962,
8.79393457792714));
#390735=CARTESIAN_POINT('Ctrl Pts',(-0.472101526741971,2.69281998167918,
8.79610912703474));
#390736=CARTESIAN_POINT('Ctrl Pts',(-0.489664844518278,2.66518948588238,
8.80838214965002));
#390737=CARTESIAN_POINT('Ctrl Pts',(-0.487883618320903,2.67082606280458,
8.81501364461995));
#390738=CARTESIAN_POINT('Ctrl Pts',(-0.479307239296716,2.67012283067463,
8.81722098428721));
#390739=CARTESIAN_POINT('Ctrl Pts',(-0.496845378477109,2.6424671432281,
8.82945683644723));
#390740=CARTESIAN_POINT('Ctrl Pts',(-0.495071154197115,2.64808156302841,
8.8360746990239));
#390741=CARTESIAN_POINT('Ctrl Pts',(-0.486523682952882,2.64739397461503,
8.83829567148519));
#390742=CARTESIAN_POINT('Ctrl Pts',(-0.504036631578591,2.6197108805292,
8.85049129520029));
#390743=CARTESIAN_POINT('Ctrl Pts',(-0.50227701319508,2.62527908089984,
8.85711686593484));
#390744=CARTESIAN_POINT('Ctrl Pts',(-0.493751728365454,2.62463079031095,
8.85933012996512));
#390745=CARTESIAN_POINT('Origin',(-0.470575193914146,2.68411393159325,8.78727029226991));
#390746=CARTESIAN_POINT('Ctrl Pts',(-0.478324646131838,2.70107476062509,
8.75374538247847));
#390747=CARTESIAN_POINT('Ctrl Pts',(-0.476047406919802,2.70832448889302,
8.75304829418601));
#390748=CARTESIAN_POINT('Ctrl Pts',(-0.468521707494412,2.70960296117184,
8.75272238421917));
#390749=CARTESIAN_POINT('Ctrl Pts',(-0.477926903323299,2.70233339384106,
8.76769408445023));
#390750=CARTESIAN_POINT('Ctrl Pts',(-0.475591700278383,2.70976535062987,
8.76974318093971));
#390751=CARTESIAN_POINT('Ctrl Pts',(-0.468179438674284,2.71120643882727,
8.7707786988043));
#390752=CARTESIAN_POINT('Ctrl Pts',(-0.479965506394844,2.6958823569765,
8.78108014887987));
#390753=CARTESIAN_POINT('Ctrl Pts',(-0.47799013061423,2.70218181154224,
8.78639403366322));
#390754=CARTESIAN_POINT('Ctrl Pts',(-0.469936666898015,2.70299654947583,
8.78812224174741));
#390755=CARTESIAN_POINT('Ctrl Pts',(-0.483306326769345,2.68531053162587,
8.78944554828686));
#390756=CARTESIAN_POINT('Ctrl Pts',(-0.481646894576971,2.69062115328589,
8.79673892988687));
#390757=CARTESIAN_POINT('Ctrl Pts',(-0.472791874487153,2.68957608222346,
8.79894799272499));
#390758=CARTESIAN_POINT('Origin',(-0.466349848864459,2.6974847670495,8.75721825406948));
#390759=CARTESIAN_POINT('Origin',(-0.466349848864459,2.6974847670495,9.));
#390760=CARTESIAN_POINT('Origin',(-0.466349848864459,2.6974847670495,7.51860402984325));
#390761=CARTESIAN_POINT('Ctrl Pts',(-0.486543054373017,2.70289632259342,
7.50366195182966));
#390762=CARTESIAN_POINT('Ctrl Pts',(-0.487191808179154,2.70650034953686,
7.50000065167735));
#390763=CARTESIAN_POINT('Ctrl Pts',(-0.487191808179039,2.70650034953688,
7.49482233047108));
#390764=CARTESIAN_POINT('Ctrl Pts',(-0.479638433643609,2.70566760608483,
7.50215800491338));
#390765=CARTESIAN_POINT('Ctrl Pts',(-0.477809241429461,2.70818926288503,
7.49877273257264));
#390766=CARTESIAN_POINT('Ctrl Pts',(-0.47441172804546,2.70880086664194,
7.49481816995649));
#390767=CARTESIAN_POINT('Ctrl Pts',(-0.477419885150963,2.70393900580489,
7.51043025814042));
#390768=CARTESIAN_POINT('Ctrl Pts',(-0.474203815632229,2.70881236746164,
7.51006209594516));
#390769=CARTESIAN_POINT('Ctrl Pts',(-0.468476805372723,2.70980248040963,
7.507312818217));
#390770=CARTESIAN_POINT('Ctrl Pts',(-0.478269325502383,2.70124988015244,
7.51860402984326));
#390771=CARTESIAN_POINT('Ctrl Pts',(-0.475977343984474,2.70850576315261,
7.51860402984326));
#390772=CARTESIAN_POINT('Ctrl Pts',(-0.468479300229132,2.70980204909083,
7.51860402984327));
#390773=CARTESIAN_POINT('Origin',(0.,0.,7.5));
#390774=CARTESIAN_POINT('Origin',(-0.670846486662627,2.58203466569847,7.5));
#390775=CARTESIAN_POINT('',(-0.670846486662627,2.58203466569847,7.59394543036555));
#390776=CARTESIAN_POINT('',(-0.670846486662627,2.58203466569847,8.85049129520029));
#390777=CARTESIAN_POINT('',(-0.670846486662627,2.58203466569847,7.5));
#390778=CARTESIAN_POINT('',(-0.653715973115269,2.65144443664272,8.78727029226991));
#390779=CARTESIAN_POINT('Ctrl Pts',(-0.670846486662627,2.58203466569847,
8.85049129520029));
#390780=CARTESIAN_POINT('Ctrl Pts',(-0.66512801519336,2.6052048872879,8.82945686509571));
#390781=CARTESIAN_POINT('Ctrl Pts',(-0.659418044923399,2.62834066354124,
8.80838212259897));
#390782=CARTESIAN_POINT('Ctrl Pts',(-0.653715973115269,2.65144443664272,
8.78727029226991));
#390783=CARTESIAN_POINT('',(-0.650355981859161,2.66505851907034,8.75721825406948));
#390784=CARTESIAN_POINT('Origin',(-0.660467557061359,2.62408907064251,8.7593767971312));
#390785=CARTESIAN_POINT('',(-0.650355981859161,2.66505851907034,7.51860402984325));
#390786=CARTESIAN_POINT('',(-0.650355981859161,2.66505851907034,7.5));
#390787=CARTESIAN_POINT('Ctrl Pts',(-0.650355981859161,2.66505851907034,
7.51860402984325));
#390788=CARTESIAN_POINT('Ctrl Pts',(-0.652994732413348,2.65436677471377,
7.52834476460825));
#390789=CARTESIAN_POINT('Ctrl Pts',(-0.655635196006324,2.64366808943105,
7.53807742314407));
#390790=CARTESIAN_POINT('Ctrl Pts',(-0.658277430155635,2.63296223017134,
7.54780169004674));
#390791=CARTESIAN_POINT('Ctrl Pts',(-0.662462586247572,2.61600472770629,
7.5632044032688));
#390792=CARTESIAN_POINT('Ctrl Pts',(-0.66665218975856,2.59902920509617,
7.57858609112103));
#390793=CARTESIAN_POINT('Ctrl Pts',(-0.670846486662627,2.58203466569847,
7.59394543036555));
#390794=CARTESIAN_POINT('Origin',(-0.870959027954988,2.77926849494598,7.5));
#390795=CARTESIAN_POINT('',(-0.74112366109302,2.64125643059841,8.75721825406948));
#390796=CARTESIAN_POINT('',(-0.731515368664223,2.6310430326237,8.78727029226991));
#390797=CARTESIAN_POINT('Origin',(-0.707125938766606,2.60511761915751,8.75658640621092));
#390798=CARTESIAN_POINT('',(-0.682528638916253,2.57897124462358,8.85049129520029));
#390799=CARTESIAN_POINT('Ctrl Pts',(-0.731515368664224,2.6310430326237,
8.78727029226991));
#390800=CARTESIAN_POINT('Ctrl Pts',(-0.715209619867131,2.6137103897036,
8.80838212259896));
#390801=CARTESIAN_POINT('Ctrl Pts',(-0.698881284484175,2.59635373775254,
8.82945686509571));
#390802=CARTESIAN_POINT('Ctrl Pts',(-0.682528638916253,2.57897124462358,
8.85049129520029));
#390803=CARTESIAN_POINT('',(-0.682528638916253,2.57897124462358,7.59394543036555));
#390804=CARTESIAN_POINT('',(-0.682528638916253,2.57897124462358,7.5));
#390805=CARTESIAN_POINT('',(-0.74112366109302,2.64125643059841,7.51860402984325));
#390806=CARTESIAN_POINT('Ctrl Pts',(-0.682528638916253,2.57897124462358,
7.59394543036555));
#390807=CARTESIAN_POINT('Ctrl Pts',(-0.694522727030089,2.59172068955962,
7.57858609112103));
#390808=CARTESIAN_POINT('Ctrl Pts',(-0.706503393831148,2.60445586794315,
7.56320440326857));
#390809=CARTESIAN_POINT('Ctrl Pts',(-0.718471342711481,2.61717752746398,
7.54780169004651));
#390810=CARTESIAN_POINT('Ctrl Pts',(-0.726027123794475,2.62520915220711,
7.53807742314383));
#390811=CARTESIAN_POINT('Ctrl Pts',(-0.733577841762333,2.63323539497312,
7.52834476460825));
#390812=CARTESIAN_POINT('Ctrl Pts',(-0.741123661093021,2.64125643059841,
7.51860402984325));
#390813=CARTESIAN_POINT('',(-0.74112366109302,2.64125643059841,7.5));
#390814=CARTESIAN_POINT('Origin',(-0.677521207658193,2.58368200434955,7.5));
#390815=CARTESIAN_POINT('Ctrl Pts',(-0.682528638916253,2.57897124462358,
8.85049129520029));
#390816=CARTESIAN_POINT('Ctrl Pts',(-0.682395941778429,2.5788301905613,
8.85097269580138));
#390817=CARTESIAN_POINT('Ctrl Pts',(-0.682258792377709,2.57869667966879,
8.85143669361005));
#390818=CARTESIAN_POINT('Ctrl Pts',(-0.682110265579986,2.5785651906683,
8.8519052845931));
#390819=CARTESIAN_POINT('Ctrl Pts',(-0.681819756582866,2.57830800652208,
8.85282181883899));
#390820=CARTESIAN_POINT('Ctrl Pts',(-0.681493063938917,2.57806532082595,
8.85372622499636));
#390821=CARTESIAN_POINT('Ctrl Pts',(-0.681115866722538,2.57784570272728,
8.85462257735071));
#390822=CARTESIAN_POINT('Ctrl Pts',(-0.680802730990279,2.57766338358186,
8.85536669723986));
#390823=CARTESIAN_POINT('Ctrl Pts',(-0.680454733368184,2.57749689311832,
8.85610498449051));
#390824=CARTESIAN_POINT('Ctrl Pts',(-0.680060197116736,2.57735833882345,
8.85681338218371));
#390825=CARTESIAN_POINT('Ctrl Pts',(-0.679702154848916,2.57723260058325,
8.85745625420284));
#390826=CARTESIAN_POINT('Ctrl Pts',(-0.679301492304152,2.57712772749012,
8.85808743050666));
#390827=CARTESIAN_POINT('Ctrl Pts',(-0.678839734209342,2.57706554866298,
8.8586680450841));
#390828=CARTESIAN_POINT('Ctrl Pts',(-0.678626689034085,2.57703686070002,
8.85893592806395));
#390829=CARTESIAN_POINT('Ctrl Pts',(-0.678400505068362,2.57701746342574,
8.85919241173848));
#390830=CARTESIAN_POINT('Ctrl Pts',(-0.678158684088287,2.57701094304344,
8.85943017985534));
#390831=CARTESIAN_POINT('Ctrl Pts',(-0.677832154178514,2.5770021385971,
8.8597512372));
#390832=CARTESIAN_POINT('Ctrl Pts',(-0.677468785008064,2.57701722880275,
8.86004599534705));
#390833=CARTESIAN_POINT('Ctrl Pts',(-0.677073374472421,2.57706643848078,
8.86026130871721));
#390834=CARTESIAN_POINT('Ctrl Pts',(-0.676928603527518,2.57708445553128,
8.86034014101235));
#390835=CARTESIAN_POINT('Ctrl Pts',(-0.676777361302704,2.57710730469718,
8.86040910639692));
#390836=CARTESIAN_POINT('Ctrl Pts',(-0.676623818556248,2.5771346960702,
8.86046313645506));
#390837=CARTESIAN_POINT('Ctrl Pts',(-0.676384216386312,2.57717744007839,
8.86054744990829));
#390838=CARTESIAN_POINT('Ctrl Pts',(-0.676132497543398,2.57723255650791,
8.86059655985669));
#390839=CARTESIAN_POINT('Ctrl Pts',(-0.675884742861718,2.57729622439678,
8.86059725258816));
#390840=CARTESIAN_POINT('Ctrl Pts',(-0.675636415767744,2.57736003938391,
8.86059794692011));
#390841=CARTESIAN_POINT('Ctrl Pts',(-0.675389978449745,2.57743572627043,
8.86056369958366));
#390842=CARTESIAN_POINT('Ctrl Pts',(-0.675157766911362,2.57751555979232,
8.86048590497774));
#390843=CARTESIAN_POINT('Ctrl Pts',(-0.675097166613615,2.5775363939646,
8.86046560290182));
#390844=CARTESIAN_POINT('Ctrl Pts',(-0.675036776242757,2.57755786724415,
8.86044257503091));
#390845=CARTESIAN_POINT('Ctrl Pts',(-0.674978450913636,2.57757928515972,
8.86041778462583));
#390846=CARTESIAN_POINT('Ctrl Pts',(-0.67458599382435,2.57772340115413,
8.86025097596201));
#390847=CARTESIAN_POINT('Ctrl Pts',(-0.674234485840249,2.57788466047735,
8.8599848982295));
#390848=CARTESIAN_POINT('Ctrl Pts',(-0.673930653710898,2.57805065560953,
8.85968173251462));
#390849=CARTESIAN_POINT('Ctrl Pts',(-0.673769943921977,2.57813845752406,
8.85952137522077));
#390850=CARTESIAN_POINT('Ctrl Pts',(-0.673619383548711,2.57822910929007,
8.85934740853961));
#390851=CARTESIAN_POINT('Ctrl Pts',(-0.673480293963271,2.57832000073264,
8.8591675900182));
#390852=CARTESIAN_POINT('Ctrl Pts',(-0.672921776980401,2.57868497711901,
8.85844552518695));
#390853=CARTESIAN_POINT('Ctrl Pts',(-0.672514998205071,2.57907191274904,
8.85759444184124));
#390854=CARTESIAN_POINT('Ctrl Pts',(-0.672211669896369,2.57941718972865,
8.85683498915139));
#390855=CARTESIAN_POINT('Ctrl Pts',(-0.672179927396693,2.57945332204502,
8.85675551444998));
#390856=CARTESIAN_POINT('Ctrl Pts',(-0.672149335081543,2.57948900814193,
8.85667699793651));
#390857=CARTESIAN_POINT('Ctrl Pts',(-0.672119849310369,2.57952418108658,
8.85659965593547));
#390858=CARTESIAN_POINT('Ctrl Pts',(-0.671721848866485,2.57999894728824,
8.85555568965886));
#390859=CARTESIAN_POINT('Ctrl Pts',(-0.671407911415525,2.58051270616165,
8.85434650606346));
#390860=CARTESIAN_POINT('Ctrl Pts',(-0.671171181984412,2.58106475696341,
8.85297329937117));
#390861=CARTESIAN_POINT('Ctrl Pts',(-0.671038036103547,2.58137525190245,
8.85220095427747));
#390862=CARTESIAN_POINT('Ctrl Pts',(-0.670929549231038,2.58169811105686,
8.85137579139183));
#390863=CARTESIAN_POINT('Ctrl Pts',(-0.670846486662627,2.58203466569847,
8.85049129520029));
#390864=CARTESIAN_POINT('Origin',(-0.677521207658193,2.58368200434955,7.59394543036555));
#390865=CARTESIAN_POINT('Ctrl Pts',(-0.682143374360193,2.57856171709663,
7.59443877723642));
#390866=CARTESIAN_POINT('Ctrl Pts',(-0.678175520124387,2.57434397760585,
7.58783886950016));
#390867=CARTESIAN_POINT('Ctrl Pts',(-0.67081360840433,2.57857262246712,
7.58559994247159));
#390868=CARTESIAN_POINT('Ctrl Pts',(-0.703803774221552,2.60158623323358,
7.56670252222134));
#390869=CARTESIAN_POINT('Ctrl Pts',(-0.699841654661634,2.5973745895738,
7.56004874999027));
#390870=CARTESIAN_POINT('Ctrl Pts',(-0.692425479350873,2.60160976383429,
7.55786368756704));
#390871=CARTESIAN_POINT('Ctrl Pts',(-0.725423725450335,2.6245677533871,
7.53888913333559));
#390872=CARTESIAN_POINT('Ctrl Pts',(-0.721438058819866,2.62033107972285,
7.5322200213728));
#390873=CARTESIAN_POINT('Ctrl Pts',(-0.713998608634745,2.62460390380804,
7.53005029815327));
#390874=CARTESIAN_POINT('Ctrl Pts',(-0.747002249729062,2.6475052376278,
7.51101258149734));
#390875=CARTESIAN_POINT('Ctrl Pts',(-0.742968269576889,2.6432172077805,
7.5043616886572));
#390876=CARTESIAN_POINT('Ctrl Pts',(-0.735531870110719,2.64755396284901,
7.50217374673251));
#390877=CARTESIAN_POINT('',(-0.734382828366911,2.6463293175146,7.50366116523517));
#390878=CARTESIAN_POINT('Ctrl Pts',(-0.741123661093021,2.64125643059841,
7.51860402984325));
#390879=CARTESIAN_POINT('Ctrl Pts',(-0.74142625372272,2.6415780797337,7.51734760759494));
#390880=CARTESIAN_POINT('Ctrl Pts',(-0.741656354716085,2.64190950301717,
7.51608817408573));
#390881=CARTESIAN_POINT('Ctrl Pts',(-0.741802465711207,2.642257553818,7.5148100591312));
#390882=CARTESIAN_POINT('Ctrl Pts',(-0.741934816542025,2.64257282655034,
7.51365231206384));
#390883=CARTESIAN_POINT('Ctrl Pts',(-0.741998669384408,2.64290209001153,
7.51247773061043));
#390884=CARTESIAN_POINT('Ctrl Pts',(-0.74195666965544,2.64324667653265,
7.51129758471022));
#390885=CARTESIAN_POINT('Ctrl Pts',(-0.741904468788883,2.64367495822514,
7.50983079813402));
#390886=CARTESIAN_POINT('Ctrl Pts',(-0.741677487599936,2.64411166614862,
7.50839324291155));
#390887=CARTESIAN_POINT('Ctrl Pts',(-0.741200920368982,2.64452196792184,
7.50715379678855));
#390888=CARTESIAN_POINT('Ctrl Pts',(-0.740980760040236,2.64471151551851,
7.50658120839351));
#390889=CARTESIAN_POINT('Ctrl Pts',(-0.740669836489905,2.64491517281699,
7.50598221009429));
#390890=CARTESIAN_POINT('Ctrl Pts',(-0.740263085778462,2.64510906506821,
7.50545747549611));
#390891=CARTESIAN_POINT('Ctrl Pts',(-0.740046031008724,2.64521253197498,
7.50517746087247));
#390892=CARTESIAN_POINT('Ctrl Pts',(-0.739799421791897,2.64531452291222,
7.50491486231392));
#390893=CARTESIAN_POINT('Ctrl Pts',(-0.739529151276104,2.64541079559314,
7.50468370960992));
#390894=CARTESIAN_POINT('Ctrl Pts',(-0.739125011602992,2.64555475361861,
7.50433806340446));
#390895=CARTESIAN_POINT('Ctrl Pts',(-0.738655660604332,2.64568971815751,
7.50405484070983));
#390896=CARTESIAN_POINT('Ctrl Pts',(-0.738152510216519,2.64580591110398,
7.5038576603613));
#390897=CARTESIAN_POINT('Ctrl Pts',(-0.738098706103272,2.64581833613356,
7.50383657498791));
#390898=CARTESIAN_POINT('Ctrl Pts',(-0.738044542534825,2.6458305550689,
7.50381643264937));
#390899=CARTESIAN_POINT('Ctrl Pts',(-0.737990077468964,2.64584256247728,
7.50379723213559));
#390900=CARTESIAN_POINT('Ctrl Pts',(-0.737626505337567,2.64592271585614,
7.50366906242519));
#390901=CARTESIAN_POINT('Ctrl Pts',(-0.737241435141435,2.64599448492876,
7.50358235568538));
#390902=CARTESIAN_POINT('Ctrl Pts',(-0.73686861200227,2.64605473955297,
7.5035341175365));
#390903=CARTESIAN_POINT('Ctrl Pts',(-0.736309605900523,2.64614508454247,
7.50346178989176));
#390904=CARTESIAN_POINT('Ctrl Pts',(-0.735704401177935,2.64621850689902,
7.50346967198527));
#390905=CARTESIAN_POINT('Ctrl Pts',(-0.735108059804471,2.64627230370702,
7.50354272648692));
#390906=CARTESIAN_POINT('Ctrl Pts',(-0.734862772254031,2.64629443144767,
7.50357277531559));
#390907=CARTESIAN_POINT('Ctrl Pts',(-0.734619322893515,2.64631335066844,
7.50361331098761));
#390908=CARTESIAN_POINT('Ctrl Pts',(-0.73438282836729,2.64632931751596,
7.50366116523659));
#390909=CARTESIAN_POINT('',(-0.678263889301916,2.5865141713381,7.57603338622103));
#390910=CARTESIAN_POINT('Origin',(-0.680502659389315,2.59506282024345,7.58486873427627));
#390911=CARTESIAN_POINT('Ctrl Pts',(-0.734382828409885,2.64632931755257,
7.50366116529968));
#390912=CARTESIAN_POINT('Ctrl Pts',(-0.715706430670505,2.62642404271696,
7.52783573079709));
#390913=CARTESIAN_POINT('Ctrl Pts',(-0.697000987800555,2.60648661431366,
7.55196141284069));
#390914=CARTESIAN_POINT('Ctrl Pts',(-0.678263890381611,2.58651417197206,
7.57603338728831));
#390915=CARTESIAN_POINT('Ctrl Pts',(-0.683105249421492,2.57984075934186,
7.59639677331372));
#390916=CARTESIAN_POINT('Ctrl Pts',(-0.672361328299493,2.56400514804978,
7.59974925422227));
#390917=CARTESIAN_POINT('Ctrl Pts',(-0.670770761278395,2.58307524303173,
7.5963967733137));
#390918=CARTESIAN_POINT('Ctrl Pts',(-0.681462581934839,2.57630285775874,
7.58707626057425));
#390919=CARTESIAN_POINT('Ctrl Pts',(-0.674975104133204,2.57397260812082,
7.58811717123965));
#390920=CARTESIAN_POINT('Ctrl Pts',(-0.670465937779981,2.57918651744118,
7.58707626057421));
#390921=CARTESIAN_POINT('Ctrl Pts',(-0.679301722070269,2.58198232224995,
7.5801537675693));
#390922=CARTESIAN_POINT('Ctrl Pts',(-0.676728207785925,2.58065795214825,
7.58208760766041));
#390923=CARTESIAN_POINT('Ctrl Pts',(-0.675135748308942,2.58307476921869,
7.5801537675693));
#390924=CARTESIAN_POINT('Ctrl Pts',(-0.678263889092194,2.58651417053754,
7.57603338509286));
#390925=CARTESIAN_POINT('Ctrl Pts',(-0.678263889092194,2.58651417053754,
7.57603338509286));
#390926=CARTESIAN_POINT('Ctrl Pts',(-0.678263889092194,2.58651417053754,
7.57603338509286));
#390927=CARTESIAN_POINT('Origin',(-0.680508179114778,2.59506137280114,7.58486873427621));
#390928=CARTESIAN_POINT('Ctrl Pts',(-0.648293759643861,2.67341427391706,
7.51098857897448));
#390929=CARTESIAN_POINT('Ctrl Pts',(-0.649704436926212,2.66769846237564,
7.50433767179956));
#390930=CARTESIAN_POINT('Ctrl Pts',(-0.658312065540219,2.66782800281639,
7.50214974420965));
#390931=CARTESIAN_POINT('Ctrl Pts',(-0.655841875747604,2.64283066015831,
7.5388732158917));
#390932=CARTESIAN_POINT('Ctrl Pts',(-0.657235650612588,2.6371833341829,
7.53220407452063));
#390933=CARTESIAN_POINT('Ctrl Pts',(-0.665814560266708,2.6372556464832,
7.53003438070911));
#390934=CARTESIAN_POINT('Ctrl Pts',(-0.663404487018657,2.61218831457929,
7.56669465659232));
#390935=CARTESIAN_POINT('Ctrl Pts',(-0.664790024933311,2.60657436325045,
7.560040858333));
#390936=CARTESIAN_POINT('Ctrl Pts',(-0.673330168792972,2.60662528459036,
7.55785582193789));
#390937=CARTESIAN_POINT('Ctrl Pts',(-0.670981251430372,2.58148862301069,
7.59443891967696));
#390938=CARTESIAN_POINT('Ctrl Pts',(-0.672368798202527,2.57586653215139,
7.58783901202978));
#390939=CARTESIAN_POINT('Ctrl Pts',(-0.680858439628796,2.57593841011513,
7.58560008491213));
#390940=CARTESIAN_POINT('',(-0.658718750143892,2.66617077539049,7.50366116523517));
#390941=CARTESIAN_POINT('Ctrl Pts',(-0.658718750143982,2.66617077539085,
7.50366116523554));
#390942=CARTESIAN_POINT('Ctrl Pts',(-0.658034914852356,2.66649712920298,
7.50350835821027));
#390943=CARTESIAN_POINT('Ctrl Pts',(-0.657395686666161,2.66677487969734,
7.50345484956));
#390944=CARTESIAN_POINT('Ctrl Pts',(-0.656782300120846,2.66701283537894,
7.50349758195598));
#390945=CARTESIAN_POINT('Ctrl Pts',(-0.656467587333167,2.66713492429086,
7.50351950684424));
#390946=CARTESIAN_POINT('Ctrl Pts',(-0.656128704689314,2.6672586916696,
7.50357029184312));
#390947=CARTESIAN_POINT('Ctrl Pts',(-0.655798643426432,2.66736905658083,
7.50365515313924));
#390948=CARTESIAN_POINT('Ctrl Pts',(-0.655290875549116,2.66753884250547,
7.50378570417639));
#390949=CARTESIAN_POINT('Ctrl Pts',(-0.654789190205193,2.66768222205234,
7.50400001621911));
#390950=CARTESIAN_POINT('Ctrl Pts',(-0.654331149039306,2.66778609894425,
7.50428903009635));
#390951=CARTESIAN_POINT('Ctrl Pts',(-0.654280309993851,2.66779762848007,
7.50432110841318));
#390952=CARTESIAN_POINT('Ctrl Pts',(-0.654229988079937,2.66780869367321,
7.50435406373354));
#390953=CARTESIAN_POINT('Ctrl Pts',(-0.654180219277436,2.66781929287174,
7.50438785222352));
#390954=CARTESIAN_POINT('Ctrl Pts',(-0.65387635681624,2.66788400607338,
7.50459414719561));
#390955=CARTESIAN_POINT('Ctrl Pts',(-0.653588167401559,2.66793187430612,
7.50483629897752));
#390956=CARTESIAN_POINT('Ctrl Pts',(-0.653326907123282,2.66796236199666,
7.5050991045531));
#390957=CARTESIAN_POINT('Ctrl Pts',(-0.652750540708295,2.66802962090417,
7.50567888004914));
#390958=CARTESIAN_POINT('Ctrl Pts',(-0.652282583320029,2.66801545797237,
7.50637912803144));
#390959=CARTESIAN_POINT('Ctrl Pts',(-0.651914066483531,2.66794945334347,
7.50710440483569));
#390960=CARTESIAN_POINT('Ctrl Pts',(-0.651823698839137,2.66793326769808,
7.50728225710685));
#390961=CARTESIAN_POINT('Ctrl Pts',(-0.651737486155035,2.66791378612335,
7.50746498566954));
#390962=CARTESIAN_POINT('Ctrl Pts',(-0.651657349091451,2.66789186972997,
7.50764697238949));
#390963=CARTESIAN_POINT('Ctrl Pts',(-0.651226554291936,2.66777405323071,
7.50862528291182));
#390964=CARTESIAN_POINT('Ctrl Pts',(-0.65093113691093,2.66757917162252,
7.50965856837422));
#390965=CARTESIAN_POINT('Ctrl Pts',(-0.650721061509935,2.66735072031591,
7.51067959873202));
#390966=CARTESIAN_POINT('Ctrl Pts',(-0.650605456751792,2.66722500327373,
7.51124147302579));
#390967=CARTESIAN_POINT('Ctrl Pts',(-0.650515987782593,2.66708879554658,
7.51180065547253));
#390968=CARTESIAN_POINT('Ctrl Pts',(-0.650446381268371,2.66694758136608,
7.512351757165));
#390969=CARTESIAN_POINT('Ctrl Pts',(-0.650205863033793,2.6664596301194,
7.51425603304535));
#390970=CARTESIAN_POINT('Ctrl Pts',(-0.650179260416289,2.66585104263316,
7.5162690050518));
#390971=CARTESIAN_POINT('Ctrl Pts',(-0.650329938180108,2.66516978271556,
7.51827788969243));
#390972=CARTESIAN_POINT('Ctrl Pts',(-0.650338093145428,2.66513291164142,
7.51838661432545));
#390973=CARTESIAN_POINT('Ctrl Pts',(-0.650346775442151,2.66509582182217,
7.51849533314856));
#390974=CARTESIAN_POINT('Ctrl Pts',(-0.650355981859157,2.66505851907034,
7.51860402984325));
#390975=CARTESIAN_POINT('Ctrl Pts',(-0.678263888672321,2.58651417242152,
7.57603338728985));
#390976=CARTESIAN_POINT('Ctrl Pts',(-0.671738733242212,2.61311115758385,
7.55196141284922));
#390977=CARTESIAN_POINT('Ctrl Pts',(-0.665223977054838,2.63966210102001,
7.52783573083105));
#390978=CARTESIAN_POINT('Ctrl Pts',(-0.65871875012457,2.66617077544643,
7.50366116530176));
#390979=CARTESIAN_POINT('Origin',(-2.3437152691429E-16,8.93760209386495E-16,
7.49482233047033));
#390980=CARTESIAN_POINT('Origin',(-0.732019285896515,2.63781235403043,7.49482233047033));
#390981=CARTESIAN_POINT('Origin',(0.,0.,7.50366116523517));
#390982=CARTESIAN_POINT('Origin',(-0.656598725434881,2.65758995402927,7.49482233047033));
#390983=CARTESIAN_POINT('Ctrl Pts',(-0.741122936374192,2.64125566017334,
7.51860402984325));
#390984=CARTESIAN_POINT('Ctrl Pts',(-0.746336138178783,2.64679811567381,
7.51860402984325));
#390985=CARTESIAN_POINT('Ctrl Pts',(-0.753653780564788,2.64471283489161,
7.51860402984325));
#390986=CARTESIAN_POINT('Ctrl Pts',(-0.743058634706594,2.64331361085372,
7.51041458714365));
#390987=CARTESIAN_POINT('Ctrl Pts',(-0.748069768762018,2.64630407925161,
7.5100464290044));
#390988=CARTESIAN_POINT('Ctrl Pts',(-0.753655798683677,2.64471225979593,
7.50729136483009));
#390989=CARTESIAN_POINT('Ctrl Pts',(-0.7417993912013,2.64583115787287,7.50215815450138));
#390990=CARTESIAN_POINT('Ctrl Pts',(-0.744539962382695,2.64731012172676,
7.49877163671532));
#390991=CARTESIAN_POINT('Ctrl Pts',(-0.747864531770537,2.64638753732423,
7.49481588533172));
#390992=CARTESIAN_POINT('Ctrl Pts',(-0.734382681155565,2.64632878704414,
7.50366171572174));
#390993=CARTESIAN_POINT('Ctrl Pts',(-0.735361839713022,2.64985715930008,
7.50000045605858));
#390994=CARTESIAN_POINT('Ctrl Pts',(-0.735361839713142,2.64985715930005,
7.49482233047317));
#390995=CARTESIAN_POINT('Origin',(-0.75022808156222,2.63269141291483,7.51860402984325));
#390996=CARTESIAN_POINT('Origin',(-0.75022808156222,2.63269141291483,9.));
#390997=CARTESIAN_POINT('Origin',(-0.75022808156222,2.63269141291483,8.75721825406948));
#390998=CARTESIAN_POINT('Ctrl Pts',(-0.729680709080017,2.62909278680762,
8.78942910404913));
#390999=CARTESIAN_POINT('Ctrl Pts',(-0.733484229768665,2.63316533626376,
8.79672699501691));
#391000=CARTESIAN_POINT('Ctrl Pts',(-0.741015530016991,2.62837440706872,
8.79893251111267));
#391001=CARTESIAN_POINT('Ctrl Pts',(-0.737214040195502,2.63710055435199,
8.78111911759576));
#391002=CARTESIAN_POINT('Ctrl Pts',(-0.741728598252128,2.64192352809016,
8.78644465894812));
#391003=CARTESIAN_POINT('Ctrl Pts',(-0.749342461395661,2.63914061598106,
8.78817647674132));
#391004=CARTESIAN_POINT('Ctrl Pts',(-0.741908991856752,2.64209118606712,
8.76780923932033));
#391005=CARTESIAN_POINT('Ctrl Pts',(-0.747241957274005,2.64778102056638,
8.76988516158375));
#391006=CARTESIAN_POINT('Ctrl Pts',(-0.75455215735806,2.64585816978495,
8.77093053738833));
#391007=CARTESIAN_POINT('Ctrl Pts',(-0.740993540539016,2.64111808118309,
8.75371302330491));
#391008=CARTESIAN_POINT('Ctrl Pts',(-0.746195062069134,2.64666879060978,
8.75300828287558));
#391009=CARTESIAN_POINT('Ctrl Pts',(-0.753536416620075,2.64454769356067,
8.75267964240737));
#391010=CARTESIAN_POINT('Origin',(-0.740619789133423,2.62247801494012,8.78727029226991));
#391011=CARTESIAN_POINT('Ctrl Pts',(-0.682528638916253,2.57897124462358,
8.85049129520029));
#391012=CARTESIAN_POINT('Ctrl Pts',(-0.68652995189615,2.58322455000411,
8.85711686593484));
#391013=CARTESIAN_POINT('Ctrl Pts',(-0.693929685372903,2.57894147790724,
8.85933012996512));
#391014=CARTESIAN_POINT('Ctrl Pts',(-0.698881306430035,2.59635376108049,
8.82945683644723));
#391015=CARTESIAN_POINT('Ctrl Pts',(-0.7029158327269,2.60064237146728,8.8360746990239));
#391016=CARTESIAN_POINT('Ctrl Pts',(-0.710318504785493,2.59631426692943,
8.83829567148519));
#391017=CARTESIAN_POINT('Ctrl Pts',(-0.715209598974206,2.61371036749489,
8.80838214965003));
#391018=CARTESIAN_POINT('Ctrl Pts',(-0.719260047395539,2.61801590274055,
8.81501364461988));
#391019=CARTESIAN_POINT('Ctrl Pts',(-0.726681976909672,2.6136611610855,
8.81722098428721));
#391020=CARTESIAN_POINT('Ctrl Pts',(-0.731515368664224,2.6310430326237,
8.78727029226991));
#391021=CARTESIAN_POINT('Ctrl Pts',(-0.735566489878335,2.63534928303293,
8.79393457792714));
#391022=CARTESIAN_POINT('Ctrl Pts',(-0.743022024337723,2.63098414602442,
8.79610912703474));
#391023=CARTESIAN_POINT('Origin',(-0.691633059385452,2.57040622694001,8.85049129520029));
#391024=CARTESIAN_POINT('Ctrl Pts',(-0.670846486662627,2.58203466569847,
8.85049129520029));
#391025=CARTESIAN_POINT('Ctrl Pts',(-0.669447239426447,2.58770416474116,
8.85711686593485));
#391026=CARTESIAN_POINT('Ctrl Pts',(-0.660897934588195,2.58760342300925,
8.85933012996512));
#391027=CARTESIAN_POINT('Ctrl Pts',(-0.67208438049413,2.57701894173547,
8.86332496987231));
#391028=CARTESIAN_POINT('Ctrl Pts',(-0.667694642491979,2.5784618882519,
8.86648636486737));
#391029=CARTESIAN_POINT('Ctrl Pts',(-0.664377626603758,2.57357583590977,
8.87206031107457));
#391030=CARTESIAN_POINT('Ctrl Pts',(-0.678964680319968,2.57518283708094,
8.86341338519876));
#391031=CARTESIAN_POINT('Ctrl Pts',(-0.683504668020055,2.57425440705277,
8.86654584966056));
#391032=CARTESIAN_POINT('Ctrl Pts',(-0.683939681183819,2.56834383040287,
8.87215952290714));
#391033=CARTESIAN_POINT('Ctrl Pts',(-0.682528638916253,2.57897124462358,
8.85049129520029));
#391034=CARTESIAN_POINT('Ctrl Pts',(-0.68652995189615,2.58322455000411,
8.85711686593484));
#391035=CARTESIAN_POINT('Ctrl Pts',(-0.693929685372902,2.57894147790724,
8.85933012996512));
#391036=CARTESIAN_POINT('Origin',(-0.658710630307053,2.57903950451468,8.85049129520029));
#391037=CARTESIAN_POINT('Ctrl Pts',(-0.653715973115268,2.65144443664272,
8.78727029226991));
#391038=CARTESIAN_POINT('Ctrl Pts',(-0.652299308087875,2.65718450945398,
8.79393457792714));
#391039=CARTESIAN_POINT('Ctrl Pts',(-0.643661112117194,2.6570396455512,
8.79610912703474));
#391040=CARTESIAN_POINT('Ctrl Pts',(-0.659418052229592,2.62834063393786,
8.80838214965003));
#391041=CARTESIAN_POINT('Ctrl Pts',(-0.658001622475827,2.63407975346251,
8.8150136446199));
#391042=CARTESIAN_POINT('Ctrl Pts',(-0.649397808304885,2.63392745668914,
8.81722098428722));
#391043=CARTESIAN_POINT('Ctrl Pts',(-0.665128007518958,2.6052049183832,
8.82945683644723));
#391044=CARTESIAN_POINT('Ctrl Pts',(-0.663717145684714,2.6109214776958,
8.8360746990239));
#391045=CARTESIAN_POINT('Ctrl Pts',(-0.655143182195944,2.61078294036945,
8.83829567148519));
#391046=CARTESIAN_POINT('Ctrl Pts',(-0.670846486662627,2.58203466569847,
8.85049129520029));
#391047=CARTESIAN_POINT('Ctrl Pts',(-0.669447239426447,2.58770416474116,
8.85711686593485));
#391048=CARTESIAN_POINT('Ctrl Pts',(-0.660897934588195,2.58760342300925,
8.85933012996512));
#391049=CARTESIAN_POINT('Origin',(-0.641580116759695,2.64844927545893,8.78727029226991));
#391050=CARTESIAN_POINT('Ctrl Pts',(-0.650400330943802,2.66487874754017,
8.75374538247849));
#391051=CARTESIAN_POINT('Ctrl Pts',(-0.648592262248888,2.6722594836811,
8.75304829418602));
#391052=CARTESIAN_POINT('Ctrl Pts',(-0.64116393718024,2.6740175024192,8.75272238421917));
#391053=CARTESIAN_POINT('Ctrl Pts',(-0.650084046247546,2.66616027822844,
8.76769408445017));
#391054=CARTESIAN_POINT('Ctrl Pts',(-0.648229808234074,2.67372658223775,
8.76974318093967));
#391055=CARTESIAN_POINT('Ctrl Pts',(-0.640925106754231,2.67563961479641,
8.77077869880429));
#391056=CARTESIAN_POINT('Ctrl Pts',(-0.651705141439419,2.65959188196377,
8.78108014887993));
#391057=CARTESIAN_POINT('Ctrl Pts',(-0.650137431719988,2.66600495638529,
8.78639403366328));
#391058=CARTESIAN_POINT('Ctrl Pts',(-0.642152715147332,2.66733400754429,
8.78812224174742));
#391059=CARTESIAN_POINT('Ctrl Pts',(-0.654361758564352,2.64882773046581,
8.78944554828685));
#391060=CARTESIAN_POINT('Ctrl Pts',(-0.65304598855138,2.65423376106967,
8.79673892988685));
#391061=CARTESIAN_POINT('Ctrl Pts',(-0.644142204117176,2.65375818030292,
8.79894799272499));
#391062=CARTESIAN_POINT('Origin',(-0.638220125503587,2.66206335788655,8.75721825406948));
#391063=CARTESIAN_POINT('Origin',(-0.638220125503587,2.66206335788655,9.));
#391064=CARTESIAN_POINT('Origin',(-0.638220125503587,2.66206335788655,7.51860402984325));
#391065=CARTESIAN_POINT('Ctrl Pts',(-0.658718561459849,2.66617001169016,
7.50366195182966));
#391066=CARTESIAN_POINT('Ctrl Pts',(-0.659596893130796,2.66972506797464,
7.50000065167735));
#391067=CARTESIAN_POINT('Ctrl Pts',(-0.659596893130682,2.66972506797467,
7.49482233047108));
#391068=CARTESIAN_POINT('Ctrl Pts',(-0.652005683757179,2.66937798185144,
7.50215800491337));
#391069=CARTESIAN_POINT('Ctrl Pts',(-0.650341812920523,2.67201165438486,
7.49877273257265));
#391070=CARTESIAN_POINT('Ctrl Pts',(-0.646990465679397,2.67283968096613,
7.49481816995649));
#391071=CARTESIAN_POINT('Ctrl Pts',(-0.649680941710149,2.66779507605612,
7.51043025814042));
#391072=CARTESIAN_POINT('Ctrl Pts',(-0.646783717304557,2.67286447915024,
7.51006209594515));
#391073=CARTESIAN_POINT('Ctrl Pts',(-0.641131910556218,2.67421948861214,
7.507312818217));
#391074=CARTESIAN_POINT('Ctrl Pts',(-0.650356343923157,2.66505705167055,
7.51860402984326));
#391075=CARTESIAN_POINT('Ctrl Pts',(-0.648533957547067,2.67244487444096,
7.51860402984326));
#391076=CARTESIAN_POINT('Ctrl Pts',(-0.641134372652,2.67421889833352,7.51860402984327));
#391077=CARTESIAN_POINT('Origin',(0.,0.,7.5));
#391078=CARTESIAN_POINT('Origin',(-0.834899689636847,2.53374831658168,7.5));
#391079=CARTESIAN_POINT('',(-0.834899689636847,2.53374831658168,7.59394543036555));
#391080=CARTESIAN_POINT('',(-0.834899689636847,2.53374831658168,8.85049129520029));
#391081=CARTESIAN_POINT('',(-0.834899689636847,2.53374831658168,7.5));
#391082=CARTESIAN_POINT('',(-0.822251471860022,2.60411303347871,8.78727029226991));
#391083=CARTESIAN_POINT('Ctrl Pts',(-0.834899689636846,2.53374831658168,
8.85049129520029));
#391084=CARTESIAN_POINT('Ctrl Pts',(-0.830677488574754,2.55723731619084,
8.82945686509571));
#391085=CARTESIAN_POINT('Ctrl Pts',(-0.826461564325083,2.58069139656184,
8.80838212259895));
#391086=CARTESIAN_POINT('Ctrl Pts',(-0.822251471860022,2.60411303347871,
8.78727029226991));
#391087=CARTESIAN_POINT('',(-0.819770641322281,2.61791441969279,8.75721825406948));
#391088=CARTESIAN_POINT('Origin',(-0.827236519635746,2.57638129654181,8.75937679713087));
#391089=CARTESIAN_POINT('',(-0.819770641322281,2.61791441969279,7.51860402984325));
#391090=CARTESIAN_POINT('',(-0.819770641322281,2.61791441969279,7.5));
#391091=CARTESIAN_POINT('Ctrl Pts',(-0.819770641322281,2.61791441969279,
7.51860402984325));
#391092=CARTESIAN_POINT('Ctrl Pts',(-0.821718947867546,2.6070755773432,
7.52834476460825));
#391093=CARTESIAN_POINT('Ctrl Pts',(-0.823668519225313,2.59622969857358,
7.53807742314407));
#391094=CARTESIAN_POINT('Ctrl Pts',(-0.825619397863334,2.58537654712673,
7.54780169004674));
#391095=CARTESIAN_POINT('Ctrl Pts',(-0.828709484189964,2.56818574179771,
7.5632044032688));
#391096=CARTESIAN_POINT('Ctrl Pts',(-0.831802854243287,2.55097666840084,
7.57858609112103));
#391097=CARTESIAN_POINT('Ctrl Pts',(-0.834899689636846,2.53374831658168,
7.59394543036555));
#391098=CARTESIAN_POINT('Origin',(-1.04723789307865,2.71775565323223,7.5));
#391099=CARTESIAN_POINT('',(-0.908826823579954,2.58834572998874,8.75721825406948));
#391100=CARTESIAN_POINT('',(-0.898583897763448,2.57876892194511,8.78727029226991));
#391101=CARTESIAN_POINT('Origin',(-0.872583531620933,2.55445941115965,8.75658640621075));
#391102=CARTESIAN_POINT('',(-0.846361565593599,2.52994271156921,8.85049129520029));
#391103=CARTESIAN_POINT('Ctrl Pts',(-0.898583897763448,2.57876892194511,
8.78727029226991));
#391104=CARTESIAN_POINT('Ctrl Pts',(-0.881201144631306,2.56251660371118,
8.80838212259896));
#391105=CARTESIAN_POINT('Ctrl Pts',(-0.863794313055971,2.54624177290295,
8.82945686509571));
#391106=CARTESIAN_POINT('Ctrl Pts',(-0.846361565593599,2.52994271156921,
8.85049129520029));
#391107=CARTESIAN_POINT('',(-0.846361565593599,2.52994271156921,7.59394543036555));
#391108=CARTESIAN_POINT('',(-0.846361565593599,2.52994271156921,7.5));
#391109=CARTESIAN_POINT('',(-0.908826823579954,2.58834572998874,7.51860402984325));
#391110=CARTESIAN_POINT('Ctrl Pts',(-0.846361565593599,2.52994271156921,
7.59394543036555));
#391111=CARTESIAN_POINT('Ctrl Pts',(-0.859147870308727,2.54189749753933,
7.57858609112103));
#391112=CARTESIAN_POINT('Ctrl Pts',(-0.871919867225447,2.55383890617556,
7.56320440326857));
#391113=CARTESIAN_POINT('Ctrl Pts',(-0.884678306195266,2.56576763856503,
7.54780169004651));
#391114=CARTESIAN_POINT('Ctrl Pts',(-0.892733151079764,2.57329866091762,
7.53807742314383));
#391115=CARTESIAN_POINT('Ctrl Pts',(-0.900782598427383,2.58082463674585,
7.52834476460825));
#391116=CARTESIAN_POINT('Ctrl Pts',(-0.908826823579954,2.58834572998874,
7.51860402984325));
#391117=CARTESIAN_POINT('',(-0.908826823579954,2.58834572998874,7.5));
#391118=CARTESIAN_POINT('Origin',(-0.841666242052023,2.53496461975633,7.5));
#391119=CARTESIAN_POINT('Ctrl Pts',(-0.846361565593599,2.52994271156921,
8.85049129520029));
#391120=CARTESIAN_POINT('Ctrl Pts',(-0.846220103731476,2.52981044925243,
8.85097269580138));
#391121=CARTESIAN_POINT('Ctrl Pts',(-0.846074682046656,2.52968599986464,
8.85143669361005));
#391122=CARTESIAN_POINT('Ctrl Pts',(-0.845918035883981,2.52956429716701,
8.8519052845931));
#391123=CARTESIAN_POINT('Ctrl Pts',(-0.845611645923929,2.52932625440855,
8.85282181883899));
#391124=CARTESIAN_POINT('Ctrl Pts',(-0.845270075579119,2.52910499860578,
8.85372622499636));
#391125=CARTESIAN_POINT('Ctrl Pts',(-0.844879582374981,2.52890999884467,
8.85462257735071));
#391126=CARTESIAN_POINT('Ctrl Pts',(-0.844555408785914,2.52874811696874,
8.85536669723987));
#391127=CARTESIAN_POINT('Ctrl Pts',(-0.844197459081632,2.52860426486192,
8.85610498449051));
#391128=CARTESIAN_POINT('Ctrl Pts',(-0.843794856243075,2.52849127326612,
8.85681338218371));
#391129=CARTESIAN_POINT('Ctrl Pts',(-0.843429493534787,2.52838873321548,
8.85745625420284));
#391130=CARTESIAN_POINT('Ctrl Pts',(-0.843022934952048,2.52830974613276,
8.85808743050665));
#391131=CARTESIAN_POINT('Ctrl Pts',(-0.842558141777638,2.5282772800014,
8.85866804508409));
#391132=CARTESIAN_POINT('Ctrl Pts',(-0.842343696282442,2.52826230083217,
8.85893592806394));
#391133=CARTESIAN_POINT('Ctrl Pts',(-0.842116734248302,2.52825743506812,
8.85919241173848));
#391134=CARTESIAN_POINT('Ctrl Pts',(-0.841874992353034,2.52826642160604,
8.85943017985534));
#391135=CARTESIAN_POINT('Ctrl Pts',(-0.841548569231167,2.52827855609253,
8.8597512372));
#391136=CARTESIAN_POINT('Ctrl Pts',(-0.841186913474445,2.52831689643642,
8.86004599534705));
#391137=CARTESIAN_POINT('Ctrl Pts',(-0.840795468227052,2.52839133904788,
8.86026130871721));
#391138=CARTESIAN_POINT('Ctrl Pts',(-0.840652149085971,2.5284185945867,
8.86034014101235));
#391139=CARTESIAN_POINT('Ctrl Pts',(-0.840502681555613,2.52845108692915,
8.86040910639693));
#391140=CARTESIAN_POINT('Ctrl Pts',(-0.840351209250492,2.5284882595412,
8.86046313645507));
#391141=CARTESIAN_POINT('Ctrl Pts',(-0.84011483798692,2.52854626709098,
8.8605474499083));
#391142=CARTESIAN_POINT('Ctrl Pts',(-0.839867167649129,2.52861739795952,
8.86059655985668));
#391143=CARTESIAN_POINT('Ctrl Pts',(-0.83962400122166,2.52869680873284,
8.86059725258816));
#391144=CARTESIAN_POINT('Ctrl Pts',(-0.839380272982597,2.52877640297678,
8.86059794692011));
#391145=CARTESIAN_POINT('Ctrl Pts',(-0.839139191271967,2.52886772364965,
8.86056369958366));
#391146=CARTESIAN_POINT('Ctrl Pts',(-0.838912571788404,2.52896227098935,
8.86048590497774));
#391147=CARTESIAN_POINT('Ctrl Pts',(-0.83885343085047,2.52898694503,8.86046560290182));
#391148=CARTESIAN_POINT('Ctrl Pts',(-0.83879454035585,2.52901224341473,
8.86044257503091));
#391149=CARTESIAN_POINT('Ctrl Pts',(-0.838737707112935,2.52903735424157,
8.86041778462583));
#391150=CARTESIAN_POINT('Ctrl Pts',(-0.838355289912295,2.52920631894626,
8.86025097596201));
#391151=CARTESIAN_POINT('Ctrl Pts',(-0.838014836059358,2.52938976813877,
8.8599848982295));
#391152=CARTESIAN_POINT('Ctrl Pts',(-0.837722263530337,2.52957488880751,
8.85968173251461));
#391153=CARTESIAN_POINT('Ctrl Pts',(-0.837567509424893,2.52967280703512,
8.85952137522076));
#391154=CARTESIAN_POINT('Ctrl Pts',(-0.837423066472652,2.52977291898359,
8.85934740853961));
#391155=CARTESIAN_POINT('Ctrl Pts',(-0.837290086096403,2.52987253518028,
8.8591675900182));
#391156=CARTESIAN_POINT('Ctrl Pts',(-0.83675610076393,2.53027254598949,
8.85844552518694));
#391157=CARTESIAN_POINT('Ctrl Pts',(-0.836374948810151,2.53068474902438,
8.85759444184122));
#391158=CARTESIAN_POINT('Ctrl Pts',(-0.836094365694028,2.53104875090688,
8.85683498915136));
#391159=CARTESIAN_POINT('Ctrl Pts',(-0.836065003418184,2.53108684273446,
8.85675551444996));
#391160=CARTESIAN_POINT('Ctrl Pts',(-0.836036760374309,2.53112441556681,
8.8566769979365));
#391161=CARTESIAN_POINT('Ctrl Pts',(-0.836009588723119,2.53116140540471,
8.85659965593547));
#391162=CARTESIAN_POINT('Ctrl Pts',(-0.835642824388812,2.53166069612429,
8.85555568965886));
#391163=CARTESIAN_POINT('Ctrl Pts',(-0.835362448600052,2.53219351346654,
8.85434650606346));
#391164=CARTESIAN_POINT('Ctrl Pts',(-0.835161575571254,2.53275959732745,
8.85297329937117));
#391165=CARTESIAN_POINT('Ctrl Pts',(-0.835048596731928,2.53307798500721,
8.85220095427747));
#391166=CARTESIAN_POINT('Ctrl Pts',(-0.834961018414379,2.53340713159065,
8.85137579139183));
#391167=CARTESIAN_POINT('Ctrl Pts',(-0.834899689636846,2.53374831658168,
8.85049129520029));
#391168=CARTESIAN_POINT('Origin',(-0.841666242052023,2.53496461975633,7.59394543036555));
#391169=CARTESIAN_POINT('Ctrl Pts',(-0.845950854086149,2.52955870944534,
7.59443877723642));
#391170=CARTESIAN_POINT('Ctrl Pts',(-0.841720920735426,2.52560385704643,
7.58783886950016));
#391171=CARTESIAN_POINT('Ctrl Pts',(-0.834645065059042,2.53029549300669,
7.58559994247159));
#391172=CARTESIAN_POINT('Ctrl Pts',(-0.869041936146755,2.55114813266051,
7.56670252222133));
#391173=CARTESIAN_POINT('Ctrl Pts',(-0.864818116250629,2.54719899614617,
7.56004874999029));
#391174=CARTESIAN_POINT('Ctrl Pts',(-0.857688526813971,2.55190062477046,
7.55786368756704));
#391175=CARTESIAN_POINT('Ctrl Pts',(-0.892089897918728,2.57269723978491,
7.53888913333557));
#391176=CARTESIAN_POINT('Ctrl Pts',(-0.887840975654134,2.56872463335888,
7.53222002137276));
#391177=CARTESIAN_POINT('Ctrl Pts',(-0.880690571396409,2.57346532567864,
7.53005029815327));
#391178=CARTESIAN_POINT('Ctrl Pts',(-0.915093696466157,2.59420505570682,
7.51101258149734));
#391179=CARTESIAN_POINT('Ctrl Pts',(-0.910793269543249,2.59018429407248,
7.5043616886572));
#391180=CARTESIAN_POINT('Ctrl Pts',(-0.903650005808575,2.59498859056224,
7.50217374673251));
#391181=CARTESIAN_POINT('',(-0.90242486159829,2.59384008075031,7.50366116523517));
#391182=CARTESIAN_POINT('Ctrl Pts',(-0.908826823579954,2.58834572998874,
7.51860402984325));
#391183=CARTESIAN_POINT('Ctrl Pts',(-0.909149402631498,2.58864733108503,
7.51734760759494));
#391184=CARTESIAN_POINT('Ctrl Pts',(-0.909400265220373,2.58896333080256,
7.51608817408573));
#391185=CARTESIAN_POINT('Ctrl Pts',(-0.909568375706159,2.5893013051321,
7.5148100591312));
#391186=CARTESIAN_POINT('Ctrl Pts',(-0.909720654201314,2.58960745035595,
7.51365231206384));
#391187=CARTESIAN_POINT('Ctrl Pts',(-0.909805471833573,2.58993194624439,
7.51247773061042));
#391188=CARTESIAN_POINT('Ctrl Pts',(-0.909785636131764,2.59027851570742,
7.51129758471022));
#391189=CARTESIAN_POINT('Ctrl Pts',(-0.909760982619738,2.59070926197024,
7.50983079813401));
#391190=CARTESIAN_POINT('Ctrl Pts',(-0.909562447760712,2.59115961536516,
7.50839324291155));
#391191=CARTESIAN_POINT('Ctrl Pts',(-0.909113147813114,2.59159960789671,
7.50715379678855));
#391192=CARTESIAN_POINT('Ctrl Pts',(-0.908905584183591,2.5918028717682,
7.50658120839351));
#391193=CARTESIAN_POINT('Ctrl Pts',(-0.908608347826955,2.59202603157119,
7.50598221009429));
#391194=CARTESIAN_POINT('Ctrl Pts',(-0.908214855547661,2.59224558605754,
7.50545747549611));
#391195=CARTESIAN_POINT('Ctrl Pts',(-0.908004875887704,2.5923627471273,
7.50517746087247));
#391196=CARTESIAN_POINT('Ctrl Pts',(-0.907765307937747,2.59248032881999,
7.50491486231392));
#391197=CARTESIAN_POINT('Ctrl Pts',(-0.90750176093356,2.59259371998976,
7.50468370960992));
#391198=CARTESIAN_POINT('Ctrl Pts',(-0.907107675031109,2.59276327555579,
7.50433806340446));
#391199=CARTESIAN_POINT('Ctrl Pts',(-0.906647935572111,2.59292803421731,
7.50405484070983));
#391200=CARTESIAN_POINT('Ctrl Pts',(-0.906153263468371,2.59307622538894,
7.50385766036131));
#391201=CARTESIAN_POINT('Ctrl Pts',(-0.906100365975824,2.59309207213133,
7.50383657498791));
#391202=CARTESIAN_POINT('Ctrl Pts',(-0.906047096562114,2.5931077362333,
7.50381643264937));
#391203=CARTESIAN_POINT('Ctrl Pts',(-0.905993512717869,2.59312320855993,
7.50379723213559));
#391204=CARTESIAN_POINT('Ctrl Pts',(-0.905635823029025,2.59322649140151,
7.50366906242519));
#391205=CARTESIAN_POINT('Ctrl Pts',(-0.905256142261181,2.59332278454905,
7.50358235568538));
#391206=CARTESIAN_POINT('Ctrl Pts',(-0.904887945654168,2.59340680223421,
7.5035341175365));
#391207=CARTESIAN_POINT('Ctrl Pts',(-0.904335876513762,2.59353277724415,
7.50346178989176));
#391208=CARTESIAN_POINT('Ctrl Pts',(-0.90373661943572,2.5936448243463,7.50346967198527));
#391209=CARTESIAN_POINT('Ctrl Pts',(-0.903144950082889,2.59373671834597,
7.50354272648692));
#391210=CARTESIAN_POINT('Ctrl Pts',(-0.902901584231239,2.59377451625012,
7.50357277531559));
#391211=CARTESIAN_POINT('Ctrl Pts',(-0.90265984722218,2.59380899445341,
7.50361331098761));
#391212=CARTESIAN_POINT('Ctrl Pts',(-0.902424861598756,2.59384008075165,
7.50366116523658));
#391213=CARTESIAN_POINT('',(-0.842588855338633,2.53774338397776,7.57603338622103));
#391214=CARTESIAN_POINT('Origin',(-0.845370739448621,2.54613103027419,7.58486873427628));
#391215=CARTESIAN_POINT('Ctrl Pts',(-0.902424861643609,2.59384008078545,
7.50366116529969));
#391216=CARTESIAN_POINT('Ctrl Pts',(-0.882511501228924,2.57517230438344,
7.52783573079709));
#391217=CARTESIAN_POINT('Ctrl Pts',(-0.86256709527385,2.55647430140459,
7.55196141284068));
#391218=CARTESIAN_POINT('Ctrl Pts',(-0.842588856456727,2.53774338454124,
7.57603338728831));
#391219=CARTESIAN_POINT('Ctrl Pts',(-0.846992701390066,2.53077349621443,
7.5963967733137));
#391220=CARTESIAN_POINT('Ctrl Pts',(-0.835256263707593,2.51565878627362,
7.59974925422226));
#391221=CARTESIAN_POINT('Ctrl Pts',(-0.834890789857186,2.53479160767911,
7.59639677331372));
#391222=CARTESIAN_POINT('Ctrl Pts',(-0.845126734807296,2.5273481096967,
7.58707626057421));
#391223=CARTESIAN_POINT('Ctrl Pts',(-0.83850328661769,2.52543830193637,
7.58811717123966));
#391224=CARTESIAN_POINT('Ctrl Pts',(-0.834337441147403,2.53093040200096,
7.58707626057424));
#391225=CARTESIAN_POINT('Ctrl Pts',(-0.843334199200213,2.53315435188585,
7.58015376756929));
#391226=CARTESIAN_POINT('Ctrl Pts',(-0.840681119793224,2.53199758847089,
7.58208760766041));
#391227=CARTESIAN_POINT('Ctrl Pts',(-0.839246778196377,2.53451146916044,
7.58015376756931));
#391228=CARTESIAN_POINT('Ctrl Pts',(-0.842588855078052,2.53774338319229,
7.57603338509286));
#391229=CARTESIAN_POINT('Ctrl Pts',(-0.842588855078052,2.53774338319228,
7.57603338509286));
#391230=CARTESIAN_POINT('Ctrl Pts',(-0.842588855078052,2.53774338319228,
7.57603338509286));
#391231=CARTESIAN_POINT('Origin',(-0.845376155095137,2.54612923215639,7.58486873427622));
#391232=CARTESIAN_POINT('Ctrl Pts',(-0.818248011214828,2.62638513377601,
7.51098857897448));
#391233=CARTESIAN_POINT('Ctrl Pts',(-0.819289576806582,2.62059068357862,
7.50433767179956));
#391234=CARTESIAN_POINT('Ctrl Pts',(-0.827887819808971,2.62016846520583,
7.50214974420965));
#391235=CARTESIAN_POINT('Ctrl Pts',(-0.823821120043175,2.5953807478726,
7.53887321589169));
#391236=CARTESIAN_POINT('Ctrl Pts',(-0.824850205830686,2.58965572547187,
7.53220407452063));
#391237=CARTESIAN_POINT('Ctrl Pts',(-0.833416122259817,2.58917823657006,
7.53003438070911));
#391238=CARTESIAN_POINT('Ctrl Pts',(-0.829404931296306,2.56431682211122,
7.56669465659236));
#391239=CARTESIAN_POINT('Ctrl Pts',(-0.830427935378131,2.55862563352851,
7.56004085833303));
#391240=CARTESIAN_POINT('Ctrl Pts',(-0.838953795137743,2.55812928134927,
7.55785582193789));
#391241=CARTESIAN_POINT('Ctrl Pts',(-0.834999192440797,2.53319476138884,
7.59443891967696));
#391242=CARTESIAN_POINT('Ctrl Pts',(-0.836023679751188,2.52749532129126,
7.58783901202978));
#391243=CARTESIAN_POINT('Ctrl Pts',(-0.844500483535585,2.52702311838028,
7.58560008491213));
#391244=CARTESIAN_POINT('',(-0.828187489909775,2.61848858635939,7.50366116523517));
#391245=CARTESIAN_POINT('Ctrl Pts',(-0.828187489909887,2.61848858635975,
7.50366116523554));
#391246=CARTESIAN_POINT('Ctrl Pts',(-0.827525969191743,2.61885808312053,
7.50350835821027));
#391247=CARTESIAN_POINT('Ctrl Pts',(-0.826905849903686,2.61917621843722,
7.50345484956));
#391248=CARTESIAN_POINT('Ctrl Pts',(-0.82630896949968,2.61945298502425,
7.50349758195598));
#391249=CARTESIAN_POINT('Ctrl Pts',(-0.82600272558662,2.61959498680894,
7.50351950684424));
#391250=CARTESIAN_POINT('Ctrl Pts',(-0.825672469016687,2.61974021217986,
7.50357029184312));
#391251=CARTESIAN_POINT('Ctrl Pts',(-0.825350157004209,2.61987149743227,
7.50365515313923));
#391252=CARTESIAN_POINT('Ctrl Pts',(-0.824854310611997,2.62007346731311,
7.50378570417639));
#391253=CARTESIAN_POINT('Ctrl Pts',(-0.824362842393527,2.62024869536167,
7.50400001621911));
#391254=CARTESIAN_POINT('Ctrl Pts',(-0.823912397737656,2.62038170562562,
7.50428903009634));
#391255=CARTESIAN_POINT('Ctrl Pts',(-0.823862401846368,2.6203964687416,
7.50432110841318));
#391256=CARTESIAN_POINT('Ctrl Pts',(-0.823812892273582,2.62041073533622,
7.50435406373354));
#391257=CARTESIAN_POINT('Ctrl Pts',(-0.823763904819404,2.62042450145568,
7.50438785222352));
#391258=CARTESIAN_POINT('Ctrl Pts',(-0.823464812865288,2.62050855023184,
7.50459414719561));
#391259=CARTESIAN_POINT('Ctrl Pts',(-0.823180282494868,2.62057478447335,
7.50483629897752));
#391260=CARTESIAN_POINT('Ctrl Pts',(-0.822921512356893,2.62062194852716,
7.5050991045531));
#391261=CARTESIAN_POINT('Ctrl Pts',(-0.822350639441519,2.62072599716703,
7.50567888004914));
#391262=CARTESIAN_POINT('Ctrl Pts',(-0.821882736099741,2.6207418454673,
7.50637912803144));
#391263=CARTESIAN_POINT('Ctrl Pts',(-0.821510747489513,2.62069958740677,
7.50710440483569));
#391264=CARTESIAN_POINT('Ctrl Pts',(-0.821419528497277,2.62068922489138,
7.50728225710685));
#391265=CARTESIAN_POINT('Ctrl Pts',(-0.821332244757601,2.62067530700927,
7.50746498566954));
#391266=CARTESIAN_POINT('Ctrl Pts',(-0.821250868156063,2.62065857004476,
7.50764697238949));
#391267=CARTESIAN_POINT('Ctrl Pts',(-0.820813409941643,2.62056859672971,
7.50862528291181));
#391268=CARTESIAN_POINT('Ctrl Pts',(-0.820506113419823,2.62039304298327,
7.50965856837421));
#391269=CARTESIAN_POINT('Ctrl Pts',(-0.820281832715801,2.62017852063153,
7.51067959873201));
#391270=CARTESIAN_POINT('Ctrl Pts',(-0.820158410761484,2.62006046871078,
7.51124147302578));
#391271=CARTESIAN_POINT('Ctrl Pts',(-0.820060398756836,2.61993027313355,
7.51180065547253));
#391272=CARTESIAN_POINT('Ctrl Pts',(-0.819981887633053,2.61979380879741,
7.51235175716501));
#391273=CARTESIAN_POINT('Ctrl Pts',(-0.819710600425269,2.61932227015509,
7.51425603304536));
#391274=CARTESIAN_POINT('Ctrl Pts',(-0.819645060131577,2.61871663751267,
7.5162690050518));
#391275=CARTESIAN_POINT('Ctrl Pts',(-0.819751779838985,2.61802712335916,
7.51827788969244));
#391276=CARTESIAN_POINT('Ctrl Pts',(-0.819757555711223,2.61798980555018,
7.51838661432545));
#391277=CARTESIAN_POINT('Ctrl Pts',(-0.819763843816357,2.61795223565928,
7.51849533314857));
#391278=CARTESIAN_POINT('Ctrl Pts',(-0.819770641322276,2.61791441969279,
7.51860402984325));
#391279=CARTESIAN_POINT('Ctrl Pts',(-0.842588854779748,2.53774338509929,
7.57603338728985));
#391280=CARTESIAN_POINT('Ctrl Pts',(-0.837781180671465,2.56470379204691,
7.55196141284922));
#391281=CARTESIAN_POINT('Ctrl Pts',(-0.83298093453604,2.59161758558424,
7.52783573083105));
#391282=CARTESIAN_POINT('Ctrl Pts',(-0.828187489894076,2.61848858641645,
7.50366116530176));
#391283=CARTESIAN_POINT('Origin',(-2.91153398701378E-16,8.76907647894215E-16,
7.49482233047033));
#391284=CARTESIAN_POINT('Origin',(-0.89952049155539,2.58549204896707,7.49482233047033));
#391285=CARTESIAN_POINT('Origin',(0.,0.,7.50366116523517));
#391286=CARTESIAN_POINT('Origin',(-0.825522045906671,2.61006122566542,7.49482233047033));
#391287=CARTESIAN_POINT('Ctrl Pts',(-0.908826050988833,2.58834500757949,
7.51860402984325));
#391288=CARTESIAN_POINT('Ctrl Pts',(-0.914383648054351,2.59354206452428,
7.51860402984325));
#391289=CARTESIAN_POINT('Ctrl Pts',(-0.921552651160824,2.59099222521768,
7.51860402984325));
#391290=CARTESIAN_POINT('Ctrl Pts',(-0.910889625574214,2.59027470936151,
7.51041458714365));
#391291=CARTESIAN_POINT('Ctrl Pts',(-0.916082063685368,2.59293796906007,
7.5100464290044));
#391292=CARTESIAN_POINT('Ctrl Pts',(-0.921554628286757,2.59099152200228,
7.50729136483008));
#391293=CARTESIAN_POINT('Ctrl Pts',(-0.909794269111079,2.59286776381869,
7.50215815450138));
#391294=CARTESIAN_POINT('Ctrl Pts',(-0.912623967034531,2.59416809998427,
7.49877163671533));
#391295=CARTESIAN_POINT('Ctrl Pts',(-0.915882595552381,2.59303440523831,
7.49481588533172));
#391296=CARTESIAN_POINT('Ctrl Pts',(-0.902424680702047,2.59383956080162,
7.50366171572174));
#391297=CARTESIAN_POINT('Ctrl Pts',(-0.903627891059845,2.59729794873417,
7.50000045605858));
#391298=CARTESIAN_POINT('Ctrl Pts',(-0.903627891059962,2.59729794873413,
7.49482233047317));
#391299=CARTESIAN_POINT('Origin',(-0.917363775473728,2.57921498783033,7.51860402984325));
#391300=CARTESIAN_POINT('Origin',(-0.917363775473728,2.57921498783033,9.));
#391301=CARTESIAN_POINT('Origin',(-0.917363775473728,2.57921498783033,8.75721825406948));
#391302=CARTESIAN_POINT('Ctrl Pts',(-0.896628055005675,2.57694023016137,
8.78942910404912));
#391303=CARTESIAN_POINT('Ctrl Pts',(-0.900684690092687,2.58076071972064,
8.7967269950169));
#391304=CARTESIAN_POINT('Ctrl Pts',(-0.907893560589471,2.57549710193981,
8.79893251111266));
#391305=CARTESIAN_POINT('Ctrl Pts',(-0.904658967512578,2.58444888270675,
8.78111911759583));
#391306=CARTESIAN_POINT('Ctrl Pts',(-0.909473258913838,2.58897269840029,
8.78644465894814));
#391307=CARTESIAN_POINT('Ctrl Pts',(-0.916893176767939,2.58570768219607,
8.78817647674132));
#391308=CARTESIAN_POINT('Ctrl Pts',(-0.909664023763931,2.58912845404803,
8.76780923932029));
#391309=CARTESIAN_POINT('Ctrl Pts',(-0.915350580979807,2.59446491390463,
8.76988516158373));
#391310=CARTESIAN_POINT('Ctrl Pts',(-0.922522564001194,2.59207764769887,
8.77093053738833));
#391311=CARTESIAN_POINT('Ctrl Pts',(-0.908688106295119,2.58821600167966,
8.75371302330492));
#391312=CARTESIAN_POINT('Ctrl Pts',(-0.914234575915404,2.59342204394984,
8.7530082828756));
#391313=CARTESIAN_POINT('Ctrl Pts',(-0.921424947711518,2.59083494272108,
8.75267964240738));
#391314=CARTESIAN_POINT('Origin',(-0.907120849657222,2.5696381797867,8.78727029226991));
#391315=CARTESIAN_POINT('Ctrl Pts',(-0.846361565593599,2.52994271156921,
8.85049129520029));
#391316=CARTESIAN_POINT('Ctrl Pts',(-0.850627167658214,2.53393091307483,
8.85711686593484));
#391317=CARTESIAN_POINT('Ctrl Pts',(-0.857737280217481,2.52918253845729,
8.85933012996512));
#391318=CARTESIAN_POINT('Ctrl Pts',(-0.86379433645136,2.54624179477689,
8.82945683644721));
#391319=CARTESIAN_POINT('Ctrl Pts',(-0.868095345592135,2.55026310076633,
8.83607469902388));
#391320=CARTESIAN_POINT('Ctrl Pts',(-0.875205505457216,2.5454695979562,
8.8382956714852));
#391321=CARTESIAN_POINT('Ctrl Pts',(-0.88120112235839,2.56251658288671,
8.80838214965003));
#391322=CARTESIAN_POINT('Ctrl Pts',(-0.88551910528938,2.5665537588271,8.81501364461992));
#391323=CARTESIAN_POINT('Ctrl Pts',(-0.892646776397508,2.56173243979915,
8.81722098428721));
#391324=CARTESIAN_POINT('Ctrl Pts',(-0.898583897763448,2.57876892194511,
8.78727029226991));
#391325=CARTESIAN_POINT('Ctrl Pts',(-0.902902597925556,2.58280676847367,
8.79393457792714));
#391326=CARTESIAN_POINT('Ctrl Pts',(-0.910063138901412,2.57797292237441,
8.79610912703474));
#391327=CARTESIAN_POINT('Origin',(-0.854898517487372,2.52081196941079,8.85049129520029));
#391328=CARTESIAN_POINT('Ctrl Pts',(-0.834899689636846,2.53374831658168,
8.85049129520029));
#391329=CARTESIAN_POINT('Ctrl Pts',(-0.833866563355028,2.53949581710877,
8.85711686593484));
#391330=CARTESIAN_POINT('Ctrl Pts',(-0.825328369435551,2.53994303820322,
8.85933012996512));
#391331=CARTESIAN_POINT('Ctrl Pts',(-0.835813681545036,2.52866358583141,
8.86332496987232));
#391332=CARTESIAN_POINT('Ctrl Pts',(-0.831525412631142,2.5303848191389,
8.86648636486736));
#391333=CARTESIAN_POINT('Ctrl Pts',(-0.827902161459403,2.52572132765298,
8.87206031107457));
#391334=CARTESIAN_POINT('Ctrl Pts',(-0.842562205427849,2.52639043132742,
8.86341338519876));
#391335=CARTESIAN_POINT('Ctrl Pts',(-0.847033380520176,2.52517303084768,
8.86654584966058));
#391336=CARTESIAN_POINT('Ctrl Pts',(-0.847088807956552,2.5192467267223,
8.87215952290714));
#391337=CARTESIAN_POINT('Ctrl Pts',(-0.846361565593598,2.52994271156921,
8.85049129520029));
#391338=CARTESIAN_POINT('Ctrl Pts',(-0.850627167658214,2.53393091307483,
8.85711686593484));
#391339=CARTESIAN_POINT('Ctrl Pts',(-0.857737280217481,2.52918253845729,
8.85933012996512));
#391340=CARTESIAN_POINT('Origin',(-0.822596867063799,2.53153685626413,8.85049129520029));
#391341=CARTESIAN_POINT('Ctrl Pts',(-0.822251471860022,2.60411303347871,
8.78727029226991));
#391342=CARTESIAN_POINT('Ctrl Pts',(-0.821205485250586,2.60993207873471,
8.79393457792714));
#391343=CARTESIAN_POINT('Ctrl Pts',(-0.812575755917853,2.61034096358642,
8.79610912703474));
#391344=CARTESIAN_POINT('Ctrl Pts',(-0.826461569719569,2.58069136655117,
8.80838214965001));
#391345=CARTESIAN_POINT('Ctrl Pts',(-0.825415756823086,2.58650944540515,
8.81501364461989));
#391346=CARTESIAN_POINT('Ctrl Pts',(-0.816819862423338,2.58690870980846,
8.81722098428721));
#391347=CARTESIAN_POINT('Ctrl Pts',(-0.830677482908405,2.55723734771395,
8.82945683644722));
#391348=CARTESIAN_POINT('Ctrl Pts',(-0.829635781053811,2.5630325559704,
8.83607469902387));
#391349=CARTESIAN_POINT('Ctrl Pts',(-0.821070557575604,2.5634436390107,
8.8382956714852));
#391350=CARTESIAN_POINT('Ctrl Pts',(-0.834899689636846,2.53374831658168,
8.85049129520029));
#391351=CARTESIAN_POINT('Ctrl Pts',(-0.833866563355028,2.53949581710877,
8.85711686593484));
#391352=CARTESIAN_POINT('Ctrl Pts',(-0.825328369435551,2.53994303820322,
8.85933012996512));
#391353=CARTESIAN_POINT('Origin',(-0.809948649286974,2.60190157316116,8.78727029226991));
#391354=CARTESIAN_POINT('Ctrl Pts',(-0.819803381285488,2.6177321760669,
8.75374538247848));
#391355=CARTESIAN_POINT('Ctrl Pts',(-0.818471912849787,2.62521359105287,
8.75304829418602));
#391356=CARTESIAN_POINT('Ctrl Pts',(-0.811171486718964,2.62744393217416,
8.75272238421917));
#391357=CARTESIAN_POINT('Ctrl Pts',(-0.819569854383168,2.619031338143,8.76769408445017));
#391358=CARTESIAN_POINT('Ctrl Pts',(-0.818204200862884,2.62670089780666,
8.76974318093968));
#391359=CARTESIAN_POINT('Ctrl Pts',(-0.811037076092511,2.62907801366546,
8.7707786988043));
#391360=CARTESIAN_POINT('Ctrl Pts',(-0.820766780267511,2.61237257342735,
8.78108014887993));
#391361=CARTESIAN_POINT('Ctrl Pts',(-0.819613178664776,2.61887291500626,
8.78639403366327));
#391362=CARTESIAN_POINT('Ctrl Pts',(-0.811730020148806,2.62071081803442,
8.78812224174741));
#391363=CARTESIAN_POINT('Ctrl Pts',(-0.82272827753326,2.6014603279895,8.78944554828685));
#391364=CARTESIAN_POINT('Ctrl Pts',(-0.821761576480904,2.60693955299787,
8.79673892988685));
#391365=CARTESIAN_POINT('Ctrl Pts',(-0.812845615262405,2.60703541679017,
8.79894799272499));
#391366=CARTESIAN_POINT('Origin',(-0.807467818749233,2.61570295937524,8.75721825406948));
#391367=CARTESIAN_POINT('Origin',(-0.807467818749233,2.61570295937524,9.));
#391368=CARTESIAN_POINT('Origin',(-0.807467818749233,2.61570295937524,7.51860402984325));
#391369=CARTESIAN_POINT('Ctrl Pts',(-0.828187252682954,2.61848783631719,
7.50366195182966));
#391370=CARTESIAN_POINT('Ctrl Pts',(-0.829291552965473,2.62197931345389,
7.50000065167735));
#391371=CARTESIAN_POINT('Ctrl Pts',(-0.829291552965362,2.62197931345392,
7.49482233047108));
#391372=CARTESIAN_POINT('Ctrl Pts',(-0.821693702661397,2.62211931091084,
7.50215800491337));
#391373=CARTESIAN_POINT('Ctrl Pts',(-0.820201990404399,2.6248541768521,
7.49877273257267));
#391374=CARTESIAN_POINT('Ctrl Pts',(-0.816910580710811,2.62589522371893,
7.49481816995647));
#391375=CARTESIAN_POINT('Ctrl Pts',(-0.819272319923723,2.62068860409958,
7.51043025814042));
#391376=CARTESIAN_POINT('Ctrl Pts',(-0.816705845947807,2.62593321736633,
7.51006209594514));
#391377=CARTESIAN_POINT('Ctrl Pts',(-0.811152467196909,2.62764755531765,
7.50731281821701));
#391378=CARTESIAN_POINT('Ctrl Pts',(-0.81977090862575,2.61791293211042,
7.51860402984326));
#391379=CARTESIAN_POINT('Ctrl Pts',(-0.818425605967999,2.6254023365026,
7.51860402984327));
#391380=CARTESIAN_POINT('Ctrl Pts',(-0.811154886414749,2.62764680850481,
7.51860402984327));
#391381=CARTESIAN_POINT('Origin',(0.,0.,7.5));
#391382=CARTESIAN_POINT('Origin',(-0.995522110700926,2.47505025214474,7.5));
#391383=CARTESIAN_POINT('',(-0.995522110700926,2.47505025214474,7.59394543036555));
#391384=CARTESIAN_POINT('',(-0.995522110700926,2.47505025214474,8.85049129520029));
#391385=CARTESIAN_POINT('',(-0.995522110700926,2.47505025214474,7.5));
#391386=CARTESIAN_POINT('',(-0.987408162934515,2.54608077127965,8.78727029226991));
#391387=CARTESIAN_POINT('Ctrl Pts',(-0.995522110700926,2.47505025214474,
8.85049129520029));
#391388=CARTESIAN_POINT('Ctrl Pts',(-0.992813529975832,2.49876150843588,
8.82945686509571));
#391389=CARTESIAN_POINT('Ctrl Pts',(-0.990108975883502,2.52243751507741,
8.80838212259896));
#391390=CARTESIAN_POINT('Ctrl Pts',(-0.987408162934515,2.54608077127965,
8.78727029226991));
#391391=CARTESIAN_POINT('',(-0.985816687379956,2.56001274842384,8.75721825406948));
#391392=CARTESIAN_POINT('Origin',(-0.990606189908908,2.51808661906322,8.75937679713101));
#391393=CARTESIAN_POINT('',(-0.985816687379956,2.56001274842384,7.51860402984325));
#391394=CARTESIAN_POINT('',(-0.985816687379956,2.56001274842384,7.5));
#391395=CARTESIAN_POINT('Ctrl Pts',(-0.985816687379956,2.56001274842384,
7.51860402984325));
#391396=CARTESIAN_POINT('Ctrl Pts',(-0.987066543906795,2.54907134720938,
7.52834476460825));
#391397=CARTESIAN_POINT('Ctrl Pts',(-0.988317211822463,2.53812284299514,
7.53807742314407));
#391398=CARTESIAN_POINT('Ctrl Pts',(-0.989568718370407,2.52716699728844,
7.54780169004674));
#391399=CARTESIAN_POINT('Ctrl Pts',(-0.991551037104193,2.50981352980197,
7.5632044032688));
#391400=CARTESIAN_POINT('Ctrl Pts',(-0.993535462378776,2.49244162139227,
7.57858609112103));
#391401=CARTESIAN_POINT('Ctrl Pts',(-0.995522110700926,2.47505025214474,
7.59394543036555));
#391402=CARTESIAN_POINT('Origin',(-1.21921343306782,2.6450749705826,7.5));
#391403=CARTESIAN_POINT('',(-1.07279542170606,2.52479896157613,8.75721825406948));
#391404=CARTESIAN_POINT('',(-1.06195995288112,2.51589809662204,8.78727029226991));
#391405=CARTESIAN_POINT('Origin',(-1.03445549157308,2.49330438150983,8.7565864062095));
#391406=CARTESIAN_POINT('',(-1.00671661105393,2.47051810124198,8.85049129520029));
#391407=CARTESIAN_POINT('Ctrl Pts',(-1.06195995288112,2.51589809662204,
8.78727029226991));
#391408=CARTESIAN_POINT('Ctrl Pts',(-1.04357162487513,2.50079288733602,
8.80838212259895));
#391409=CARTESIAN_POINT('Ctrl Pts',(-1.02515782551212,2.48566675444137,
8.82945686509571));
#391410=CARTESIAN_POINT('Ctrl Pts',(-1.00671661105393,2.47051810124198,
8.85049129520029));
#391411=CARTESIAN_POINT('',(-1.00671661105393,2.47051810124198,7.59394543036555));
#391412=CARTESIAN_POINT('',(-1.00671661105393,2.47051810124198,7.5));
#391413=CARTESIAN_POINT('',(-1.07279542170606,2.52479896157613,7.51860402984325));
#391414=CARTESIAN_POINT('Ctrl Pts',(-1.00671661105393,2.47051810124198,
7.59394543036555));
#391415=CARTESIAN_POINT('Ctrl Pts',(-1.02024259070162,2.48162910346634,
7.57858609112103));
#391416=CARTESIAN_POINT('Ctrl Pts',(-1.03375343485909,2.49272767254577,
7.56320440326857));
#391417=CARTESIAN_POINT('Ctrl Pts',(-1.04724993675599,2.50381446008379,
7.54780169004651));
#391418=CARTESIAN_POINT('Ctrl Pts',(-1.05577074635661,2.5108139334596,7.53807742314383));
#391419=CARTESIAN_POINT('Ctrl Pts',(-1.06428584617823,2.51780871650104,
7.52834476460825));
#391420=CARTESIAN_POINT('Ctrl Pts',(-1.07279542170605,2.52479896157613,
7.51860402984324));
#391421=CARTESIAN_POINT('',(-1.07279542170606,2.52479896157613,7.5));
#391422=CARTESIAN_POINT('Origin',(-1.00235268932042,2.47583052179233,7.5));
#391423=CARTESIAN_POINT('Ctrl Pts',(-1.00671661105393,2.47051810124198,
8.85049129520029));
#391424=CARTESIAN_POINT('Ctrl Pts',(-1.00656696576465,2.47039517416494,
8.85097269580138));
#391425=CARTESIAN_POINT('Ctrl Pts',(-1.00641386936462,2.47028029767111,
8.85143669361005));
#391426=CARTESIAN_POINT('Ctrl Pts',(-1.00624974752968,2.47016888137882,
8.8519052845931));
#391427=CARTESIAN_POINT('Ctrl Pts',(-1.00592873562876,2.46995095817688,
8.85282181883899));
#391428=CARTESIAN_POINT('Ctrl Pts',(-1.0055736911689,2.46975204145501,8.85372622499636));
#391429=CARTESIAN_POINT('Ctrl Pts',(-1.00517150659735,2.46958246132732,
8.85462257735071));
#391430=CARTESIAN_POINT('Ctrl Pts',(-1.00483762725028,2.46944168192823,
8.85536669723986));
#391431=CARTESIAN_POINT('Ctrl Pts',(-1.00447119635593,2.46932105929728,
8.85610498449051));
#391432=CARTESIAN_POINT('Ctrl Pts',(-1.00406218131168,2.46923409470727,
8.85681338218371));
#391433=CARTESIAN_POINT('Ctrl Pts',(-1.00369099951666,2.46915517420526,
8.85745625420284));
#391434=CARTESIAN_POINT('Ctrl Pts',(-1.00328021553237,2.46910239770779,
8.85808743050665));
#391435=CARTESIAN_POINT('Ctrl Pts',(-1.0028142972132,2.46909977768252,8.85866804508409));
#391436=CARTESIAN_POINT('Ctrl Pts',(-1.00259933260061,2.46909856885965,
8.85893592806395));
#391437=CARTESIAN_POINT('Ctrl Pts',(-1.00237252513374,2.46910825460029,
8.85919241173848));
#391438=CARTESIAN_POINT('Ctrl Pts',(-1.00213185569258,2.46913271113081,
8.85943017985534));
#391439=CARTESIAN_POINT('Ctrl Pts',(-1.00180688070125,2.46916573468691,
8.8597512372));
#391440=CARTESIAN_POINT('Ctrl Pts',(-1.00144842447933,2.46922716762035,
8.86004599534706));
#391441=CARTESIAN_POINT('Ctrl Pts',(-1.00106255305268,2.4693265372646,8.86026130871721));
#391442=CARTESIAN_POINT('Ctrl Pts',(-1.00092127464451,2.46936291929288,
8.86034014101235));
#391443=CARTESIAN_POINT('Ctrl Pts',(-1.00077419600275,2.46940492129388,
8.86040910639693));
#391444=CARTESIAN_POINT('Ctrl Pts',(-1.00062541657116,2.46945172239472,
8.86046313645507));
#391445=CARTESIAN_POINT('Ctrl Pts',(-1.00039324751417,2.46952475512063,
8.8605474499083));
#391446=CARTESIAN_POINT('Ctrl Pts',(-1.00015064341205,2.46961160813619,
8.86059655985668));
#391447=CARTESIAN_POINT('Ctrl Pts',(-0.999913064461799,2.46970643547806,
8.86059725258816));
#391448=CARTESIAN_POINT('Ctrl Pts',(-0.999674936609261,2.46980148190898,
8.86059794692011));
#391449=CARTESIAN_POINT('Ctrl Pts',(-0.999440201162461,2.46990806111197,
8.86056369958366));
#391450=CARTESIAN_POINT('Ctrl Pts',(-0.999220104961786,2.47001693375418,
8.86048590497774));
#391451=CARTESIAN_POINT('Ctrl Pts',(-0.999162666406463,2.47004534627227,
8.86046560290182));
#391452=CARTESIAN_POINT('Ctrl Pts',(-0.999105517781755,2.47007436580571,
8.86044257503091));
#391453=CARTESIAN_POINT('Ctrl Pts',(-0.999050410165033,2.47010306635803,
8.86041778462583));
#391454=CARTESIAN_POINT('Ctrl Pts',(-0.998679604287343,2.47029618546078,
8.86025097596201));
#391455=CARTESIAN_POINT('Ctrl Pts',(-0.998351603563481,2.47050107069051,
8.8599848982295));
#391456=CARTESIAN_POINT('Ctrl Pts',(-0.998071492878068,2.47070455619527,
8.85968173251461));
#391457=CARTESIAN_POINT('Ctrl Pts',(-0.997923330373914,2.47081218836896,
8.85952137522076));
#391458=CARTESIAN_POINT('Ctrl Pts',(-0.99778559838977,2.47092134911842,
8.85934740853961));
#391459=CARTESIAN_POINT('Ctrl Pts',(-0.997659273667602,2.47102928072491,
8.8591675900182));
#391460=CARTESIAN_POINT('Ctrl Pts',(-0.997152014245809,2.47146268222672,
8.85844552518695));
#391461=CARTESIAN_POINT('Ctrl Pts',(-0.996798055348722,2.47189845883579,
8.85759444184124));
#391462=CARTESIAN_POINT('Ctrl Pts',(-0.99654137040139,2.47227968985935,
8.85683498915138));
#391463=CARTESIAN_POINT('Ctrl Pts',(-0.996514509005261,2.47231958467067,
8.85675551444998));
#391464=CARTESIAN_POINT('Ctrl Pts',(-0.99648873128938,2.47235888984364,
8.85667699793651));
#391465=CARTESIAN_POINT('Ctrl Pts',(-0.996463985412311,2.47239754457562,
8.85659965593547));
#391466=CARTESIAN_POINT('Ctrl Pts',(-0.996129964300902,2.47291930812045,
8.85555568965886));
#391467=CARTESIAN_POINT('Ctrl Pts',(-0.995884302298597,2.47346899447079,
8.85434650606346));
#391468=CARTESIAN_POINT('Ctrl Pts',(-0.995720111102476,2.47404678523083,
8.85297329937118));
#391469=CARTESIAN_POINT('Ctrl Pts',(-0.995627763558975,2.47437175732805,
8.85220095427747));
#391470=CARTESIAN_POINT('Ctrl Pts',(-0.995561453674479,2.4747058388066,
8.85137579139184));
#391471=CARTESIAN_POINT('Ctrl Pts',(-0.995522110700926,2.47505025214474,
8.85049129520029));
#391472=CARTESIAN_POINT('Origin',(-1.00235268932042,2.47583052179233,7.59394543036555));
#391473=CARTESIAN_POINT('Ctrl Pts',(-1.00628214029678,2.47016120246829,
7.59443877723642));
#391474=CARTESIAN_POINT('Ctrl Pts',(-1.00180750953459,2.46648548849808,
7.58783886950016));
#391475=CARTESIAN_POINT('Ctrl Pts',(-0.995046786110622,2.47162083661882,
7.58559994247159));
#391476=CARTESIAN_POINT('Ctrl Pts',(-1.03070901834743,2.49022681719079,
7.56670252222133));
#391477=CARTESIAN_POINT('Ctrl Pts',(-1.02624085469707,2.48655641567087,
7.56004874999028));
#391478=CARTESIAN_POINT('Ctrl Pts',(-1.01942714814677,2.49170517865849,
7.55786368756704));
#391479=CARTESIAN_POINT('Ctrl Pts',(-1.05509028164391,2.51025496138264,
7.53888913333558));
#391480=CARTESIAN_POINT('Ctrl Pts',(-1.05059556347818,2.50656274648674,
7.53222002137275));
#391481=CARTESIAN_POINT('Ctrl Pts',(-1.04376358769266,2.51175182651944,
7.53005029815326));
#391482=CARTESIAN_POINT('Ctrl Pts',(-1.07942482691749,2.5302447287567,7.51101258149734));
#391483=CARTESIAN_POINT('Ctrl Pts',(-1.07487562460051,2.52650775750732,
7.5043616886572));
#391484=CARTESIAN_POINT('Ctrl Pts',(-1.06805484980025,2.53175985353355,
7.50217374673251));
#391485=CARTESIAN_POINT('',(-1.06675863750384,2.53069219871726,7.50366116523517));
#391486=CARTESIAN_POINT('Ctrl Pts',(-1.07279542170606,2.52479896157613,
7.51860402984325));
#391487=CARTESIAN_POINT('Ctrl Pts',(-1.07313666163293,2.52507927528983,
7.51734760759493));
#391488=CARTESIAN_POINT('Ctrl Pts',(-1.07340725496913,2.52537855293079,
7.51608817408573));
#391489=CARTESIAN_POINT('Ctrl Pts',(-1.07359667414353,2.52570506198002,
7.5148100591312));
#391490=CARTESIAN_POINT('Ctrl Pts',(-1.07376825455802,2.52600082167899,
7.51365231206384));
#391491=CARTESIAN_POINT('Ctrl Pts',(-1.07387368844631,2.52631921657147,
7.51247773061043));
#391492=CARTESIAN_POINT('Ctrl Pts',(-1.07387609828082,2.52666634484815,
7.51129758471022));
#391493=CARTESIAN_POINT('Ctrl Pts',(-1.07387909342989,2.52709778565251,
7.50983079813402));
#391494=CARTESIAN_POINT('Ctrl Pts',(-1.07370982072311,2.52755993392017,
7.50839324291155));
#391495=CARTESIAN_POINT('Ctrl Pts',(-1.07328963432873,2.52802780918636,
7.50715379678855));
#391496=CARTESIAN_POINT('Ctrl Pts',(-1.0730955203219,2.52824395407783,7.50658120839351));
#391497=CARTESIAN_POINT('Ctrl Pts',(-1.0728131925669,2.52848569937382,7.50598221009429));
#391498=CARTESIAN_POINT('Ctrl Pts',(-1.07243457566394,2.52873001389883,
7.50545747549611));
#391499=CARTESIAN_POINT('Ctrl Pts',(-1.07223253396523,2.52886038769162,
7.50517746087247));
#391500=CARTESIAN_POINT('Ctrl Pts',(-1.07200099171823,2.52899307697136,
7.50491486231392));
#391501=CARTESIAN_POINT('Ctrl Pts',(-1.07174525119682,2.52912312068134,
7.50468370960993));
#391502=CARTESIAN_POINT('Ctrl Pts',(-1.07136283844854,2.52931757704774,
7.50433806340447));
#391503=CARTESIAN_POINT('Ctrl Pts',(-1.07091459969726,2.52951145280318,
7.50405484070984));
#391504=CARTESIAN_POINT('Ctrl Pts',(-1.07043043859138,2.52969103325066,
7.50385766036131));
#391505=CARTESIAN_POINT('Ctrl Pts',(-1.07037866508667,2.52971023658821,
7.50383657498791));
#391506=CARTESIAN_POINT('Ctrl Pts',(-1.07032650872314,2.52972928148965,
7.50381643264937));
#391507=CARTESIAN_POINT('Ctrl Pts',(-1.07027402628802,2.52974815515542,
7.50379723213559));
#391508=CARTESIAN_POINT('Ctrl Pts',(-1.06992368886538,2.52987414304837,
7.50366906242519));
#391509=CARTESIAN_POINT('Ctrl Pts',(-1.06955095771554,2.52999456458163,
7.50358235568538));
#391510=CARTESIAN_POINT('Ctrl Pts',(-1.06918890063952,2.53010200008106,
7.5035341175365));
#391511=CARTESIAN_POINT('Ctrl Pts',(-1.06864603703097,2.53026308745309,
7.50346178989176));
#391512=CARTESIAN_POINT('Ctrl Pts',(-1.06805519007335,2.53041329887528,
7.50346967198527));
#391513=CARTESIAN_POINT('Ctrl Pts',(-1.06747062403743,2.53054291245446,
7.50354272648692));
#391514=CARTESIAN_POINT('Ctrl Pts',(-1.06723017992706,2.53059622520241,
7.50357277531559));
#391515=CARTESIAN_POINT('Ctrl Pts',(-1.06699114861868,2.53064612070988,
7.50361331098761));
#391516=CARTESIAN_POINT('Ctrl Pts',(-1.06675863750439,2.53069219871857,
7.50366116523659));
#391517=CARTESIAN_POINT('',(-1.00345144303402,2.47854446470841,7.57603338622103));
#391518=CARTESIAN_POINT('Origin',(-1.00676500980815,2.48673664175956,7.58486873427627));
#391519=CARTESIAN_POINT('Ctrl Pts',(-1.06675863755131,2.53069219874943,
7.50366116529969));
#391520=CARTESIAN_POINT('Ctrl Pts',(-1.04569014273066,2.51333863067848,
7.52783573079709));
#391521=CARTESIAN_POINT('Ctrl Pts',(-1.0245887295326,2.49595688722903,7.55196141284068));
#391522=CARTESIAN_POINT('Ctrl Pts',(-1.00345144418592,2.4785444651991,7.57603338728831));
#391523=CARTESIAN_POINT('Ctrl Pts',(-1.00727768057273,2.47117287269355,
7.59642833564546));
#391524=CARTESIAN_POINT('Ctrl Pts',(-0.994757591870493,2.4578328505239,
7.59959882295464));
#391525=CARTESIAN_POINT('Ctrl Pts',(-0.995580073096938,2.47609196989962,
7.59639677331371));
#391526=CARTESIAN_POINT('Ctrl Pts',(-1.00514669506349,2.46797166347564,
7.58710240504252));
#391527=CARTESIAN_POINT('Ctrl Pts',(-0.998521053703182,2.46662434118415,
7.58809943920598));
#391528=CARTESIAN_POINT('Ctrl Pts',(-0.994780473004191,2.47227415065621,
7.58707626057423));
#391529=CARTESIAN_POINT('Ctrl Pts',(-1.00382229260949,2.47388921842956,
7.58020924244128));
#391530=CARTESIAN_POINT('Ctrl Pts',(-1.00116057348243,2.47297143505264,
7.5820588065976));
#391531=CARTESIAN_POINT('Ctrl Pts',(-0.999909163054414,2.4755333178244,
7.5801537675693));
#391532=CARTESIAN_POINT('Ctrl Pts',(-1.00345144272365,2.47854446394124,
7.57603338509286));
#391533=CARTESIAN_POINT('Ctrl Pts',(-1.00345144272365,2.47854446394124,
7.57603338509286));
#391534=CARTESIAN_POINT('Ctrl Pts',(-1.00345144272365,2.47854446394124,
7.57603338509286));
#391535=CARTESIAN_POINT('Origin',(-1.00677029912173,2.48673450035397,7.58486873427621));
#391536=CARTESIAN_POINT('Ctrl Pts',(-0.984839906194067,2.56856361376243,
7.51098857897448));
#391537=CARTESIAN_POINT('Ctrl Pts',(-0.985508080078791,2.56271433554784,
7.50433767179957));
#391538=CARTESIAN_POINT('Ctrl Pts',(-0.994061605444748,2.56174209334736,
7.50214974420965));
#391539=CARTESIAN_POINT('Ctrl Pts',(-0.988415106647414,2.53726585938646,
7.53887321589169));
#391540=CARTESIAN_POINT('Ctrl Pts',(-0.989075274623209,2.53148666590547,
7.53220407452062));
#391541=CARTESIAN_POINT('Ctrl Pts',(-0.997592998639362,2.53046133790587,
7.53003438070911));
#391542=CARTESIAN_POINT('Ctrl Pts',(-0.991997172804467,2.50590800177684,
7.56669465659237));
#391543=CARTESIAN_POINT('Ctrl Pts',(-0.992653439310206,2.50016296225487,
7.56004085833302));
#391544=CARTESIAN_POINT('Ctrl Pts',(-1.00112998038326,2.49912137617411,
7.55785582193789));
#391545=CARTESIAN_POINT('Ctrl Pts',(-0.995585942662718,2.47449145912389,
7.59443891967696));
#391546=CARTESIAN_POINT('Ctrl Pts',(-0.996243160673235,2.4687380900099,
7.58783901202978));
#391547=CARTESIAN_POINT('Ctrl Pts',(-1.00467229381074,2.46772374660725,
7.58560008491213));
#391548=CARTESIAN_POINT('',(-0.994253029633958,2.5600464660629,7.50366116523517));
#391549=CARTESIAN_POINT('Ctrl Pts',(-0.994253029634093,2.56004646606325,
7.50366116523554));
#391550=CARTESIAN_POINT('Ctrl Pts',(-0.993616541819959,2.56045758743125,
7.50350835821027));
#391551=CARTESIAN_POINT('Ctrl Pts',(-0.99301807963321,2.56081480028401,
7.50345484956));
#391552=CARTESIAN_POINT('Ctrl Pts',(-0.992440158080123,2.56112924048318,
7.50349758195598));
#391553=CARTESIAN_POINT('Ctrl Pts',(-0.99214364146361,2.56129057162485,
7.50351950684424));
#391554=CARTESIAN_POINT('Ctrl Pts',(-0.991823368062682,2.56145665822576,
7.50357029184312));
#391555=CARTESIAN_POINT('Ctrl Pts',(-0.991510129749804,2.56160832434008,
7.50365515313924));
#391556=CARTESIAN_POINT('Ctrl Pts',(-0.991028242381882,2.56184164823957,
7.50378570417639));
#391557=CARTESIAN_POINT('Ctrl Pts',(-0.990549010837197,2.56204800474018,
7.50400001621911));
#391558=CARTESIAN_POINT('Ctrl Pts',(-0.990108013665056,2.56220960180847,
7.50428903009634));
#391559=CARTESIAN_POINT('Ctrl Pts',(-0.990059066371773,2.5622275378398,
7.50432110841318));
#391560=CARTESIAN_POINT('Ctrl Pts',(-0.990010572585567,2.56224494721138,
7.50435406373354));
#391561=CARTESIAN_POINT('Ctrl Pts',(-0.989962567779668,2.56226182368384,
7.50438785222352));
#391562=CARTESIAN_POINT('Ctrl Pts',(-0.989669475365627,2.56236486266007,
7.50459414719561));
#391563=CARTESIAN_POINT('Ctrl Pts',(-0.989389773235793,2.56244919073966,
7.50483629897752));
#391564=CARTESIAN_POINT('Ctrl Pts',(-0.989134556580122,2.56251283734952,
7.5050991045531));
#391565=CARTESIAN_POINT('Ctrl Pts',(-0.988571523003624,2.56265324816357,
7.50567888004914));
#391566=CARTESIAN_POINT('Ctrl Pts',(-0.988105596423529,2.56269904257185,
7.50637912803144));
#391567=CARTESIAN_POINT('Ctrl Pts',(-0.987731664620562,2.56268070472712,
7.50710440483569));
#391568=CARTESIAN_POINT('Ctrl Pts',(-0.987639969118888,2.56267620792353,
7.50728225710685));
#391569=CARTESIAN_POINT('Ctrl Pts',(-0.987551972991248,2.5626679109256,
7.50746498566954));
#391570=CARTESIAN_POINT('Ctrl Pts',(-0.987469691245669,2.56265642216575,
7.50764697238949));
#391571=CARTESIAN_POINT('Ctrl Pts',(-0.987027367225978,2.56259466175455,
7.50862528291182));
#391572=CARTESIAN_POINT('Ctrl Pts',(-0.986709454310666,2.56243915725786,
7.50965856837422));
#391573=CARTESIAN_POINT('Ctrl Pts',(-0.986471889921137,2.56223944537934,
7.51067959873202));
#391574=CARTESIAN_POINT('Ctrl Pts',(-0.986341157937931,2.56212954368069,
7.51124147302579));
#391575=CARTESIAN_POINT('Ctrl Pts',(-0.986235005650185,2.56200589525494,
7.51180065547253));
#391576=CARTESIAN_POINT('Ctrl Pts',(-0.986147912535891,2.56187474152438,
7.51235175716501));
#391577=CARTESIAN_POINT('Ctrl Pts',(-0.985846971132227,2.56142155313986,
7.51425603304536));
#391578=CARTESIAN_POINT('Ctrl Pts',(-0.985742762481469,2.56082136401569,
7.51626900505181));
#391579=CARTESIAN_POINT('Ctrl Pts',(-0.985805085598299,2.56012642898783,
7.51827788969245));
#391580=CARTESIAN_POINT('Ctrl Pts',(-0.985808458643156,2.56008881779087,
7.51838661432546));
#391581=CARTESIAN_POINT('Ctrl Pts',(-0.98581232671753,2.56005092221107,
7.51849533314857));
#391582=CARTESIAN_POINT('Ctrl Pts',(-0.985816687379952,2.56001274842384,
7.51860402984325));
#391583=CARTESIAN_POINT('Ctrl Pts',(-1.00345144254814,2.47854446586344,
7.57603338728985));
#391584=CARTESIAN_POINT('Ctrl Pts',(-1.00038100552583,2.50575750850121,
7.55196141284922));
#391585=CARTESIAN_POINT('Ctrl Pts',(-0.997314994683384,2.53292355758908,
7.52783573083105));
#391586=CARTESIAN_POINT('Ctrl Pts',(-0.994253029621948,2.56004646612085,
7.50366116530176));
#391587=CARTESIAN_POINT('Origin',(-3.46738858720994E-16,8.56451684780636E-16,
7.49482233047033));
#391588=CARTESIAN_POINT('Origin',(-1.06332537456792,2.5225474024882,7.49482233047033));
#391589=CARTESIAN_POINT('Origin',(0.,0.,7.50366116523517));
#391590=CARTESIAN_POINT('Origin',(-0.991053119217907,2.55180719586893,7.49482233047033));
#391591=CARTESIAN_POINT('Ctrl Pts',(-1.07279460441739,2.52479829015122,
7.51860402984325));
#391592=CARTESIAN_POINT('Ctrl Pts',(-1.07867375938539,2.52962859271859,
7.51860402984325));
#391593=CARTESIAN_POINT('Ctrl Pts',(-1.08566466424082,2.52662467272424,
7.51860402984325));
#391594=CARTESIAN_POINT('Ctrl Pts',(-1.07497757558513,2.52659181347635,
7.51041458714366));
#391595=CARTESIAN_POINT('Ctrl Pts',(-1.08032998091005,2.52891692057021,
7.51004642900441));
#391596=CARTESIAN_POINT('Ctrl Pts',(-1.08566659224937,2.52662384427877,
7.5072913648301));
#391597=CARTESIAN_POINT('Ctrl Pts',(-1.07405060721883,2.5292497199546,7.50215815450137));
#391598=CARTESIAN_POINT('Ctrl Pts',(-1.07695780404858,2.53036608507162,
7.49877163671531));
#391599=CARTESIAN_POINT('Ctrl Pts',(-1.08013710129289,2.52902593857713,
7.49481588533171));
#391600=CARTESIAN_POINT('Ctrl Pts',(-1.06675842366604,2.53069169142693,
7.50366171572174));
#391601=CARTESIAN_POINT('Ctrl Pts',(-1.06818074157473,2.53406588377826,
7.50000045605858));
#391602=CARTESIAN_POINT('Ctrl Pts',(-1.06818074157484,2.53406588377821,
7.49482233047317));
#391603=CARTESIAN_POINT('Origin',(-1.0807298248579,2.51514001512095,7.51860402984325));
#391604=CARTESIAN_POINT('Origin',(-1.0807298248579,2.51514001512095,9.));
#391605=CARTESIAN_POINT('Origin',(-1.0807298248579,2.51514001512095,8.75721825406948));
#391606=CARTESIAN_POINT('Ctrl Pts',(-1.0598909639272,2.51419847335744,8.78942910404912));
#391607=CARTESIAN_POINT('Ctrl Pts',(-1.06418404382885,2.51775120380876,
8.79672699501691));
#391608=CARTESIAN_POINT('Ctrl Pts',(-1.07104086177894,2.51203652677664,
8.79893251111267));
#391609=CARTESIAN_POINT('Ctrl Pts',(-1.06838645708335,2.52117715623988,
8.78111911759581));
#391610=CARTESIAN_POINT('Ctrl Pts',(-1.07348069887324,2.52538322455977,
8.78644465894812));
#391611=CARTESIAN_POINT('Ctrl Pts',(-1.08067618140391,2.52164952091239,
8.78817647674132));
#391612=CARTESIAN_POINT('Ctrl Pts',(-1.07368105107515,2.52552643784496,
8.76780923932031));
#391613=CARTESIAN_POINT('Ctrl Pts',(-1.07969783280626,2.5304875944007,8.76988516158376));
#391614=CARTESIAN_POINT('Ctrl Pts',(-1.08670212754838,2.52764572255949,
8.77093053738833));
#391615=CARTESIAN_POINT('Ctrl Pts',(-1.07264867770945,2.52467838745472,
8.75371302330492));
#391616=CARTESIAN_POINT('Ctrl Pts',(-1.07851730378653,2.52951836982403,
8.75300828287558));
#391617=CARTESIAN_POINT('Ctrl Pts',(-1.08552714604779,2.52647589536948,
8.75267964240737));
#391618=CARTESIAN_POINT('Origin',(-1.06989435603297,2.50623915016686,8.78727029226991));
#391619=CARTESIAN_POINT('Ctrl Pts',(-1.00671661105393,2.47051810124198,
8.85049129520029));
#391620=CARTESIAN_POINT('Ctrl Pts',(-1.01122897392942,2.47422481049724,
8.85711686593484));
#391621=CARTESIAN_POINT('Ctrl Pts',(-1.01802024859358,2.46903064544886,
8.85933012996512));
#391622=CARTESIAN_POINT('Ctrl Pts',(-1.02515785026092,2.48566677477142,
8.82945683644722));
#391623=CARTESIAN_POINT('Ctrl Pts',(-1.02970766847649,2.48940425195463,
8.8360746990239));
#391624=CARTESIAN_POINT('Ctrl Pts',(-1.03649609897603,2.48416504840347,
8.8382956714852));
#391625=CARTESIAN_POINT('Ctrl Pts',(-1.04357160131376,2.50079286798138,
8.80838214965002));
#391626=CARTESIAN_POINT('Ctrl Pts',(-1.0481393752363,2.50454509499457,8.81501364461992));
#391627=CARTESIAN_POINT('Ctrl Pts',(-1.05494349880899,2.49927701042778,
8.81722098428721));
#391628=CARTESIAN_POINT('Ctrl Pts',(-1.06195995288112,2.51589809662204,
8.78727029226991));
#391629=CARTESIAN_POINT('Ctrl Pts',(-1.0665284855259,2.51965094689244,8.79393457792714));
#391630=CARTESIAN_POINT('Ctrl Pts',(-1.07336460881942,2.51436825501291,
8.79610912703474));
#391631=CARTESIAN_POINT('Origin',(-1.01465101420578,2.4608591547868,8.85049129520029));
#391632=CARTESIAN_POINT('Ctrl Pts',(-0.995522110700926,2.47505025214474,
8.85049129520029));
#391633=CARTESIAN_POINT('Ctrl Pts',(-0.994859350710966,2.48085213644373,
8.85711686593484));
#391634=CARTESIAN_POINT('Ctrl Pts',(-0.986367352980517,2.48184548263713,
8.85933012996512));
#391635=CARTESIAN_POINT('Ctrl Pts',(-0.996108444897003,2.46991740885651,
8.86332496987233));
#391636=CARTESIAN_POINT('Ctrl Pts',(-0.991939266488152,2.47190985603823,
8.86648636486737));
#391637=CARTESIAN_POINT('Ctrl Pts',(-0.988024668749171,2.46748808869535,
8.87206031107457));
#391638=CARTESIAN_POINT('Ctrl Pts',(-1.00269746170461,2.46721654538255,
8.86341338519876));
#391639=CARTESIAN_POINT('Ctrl Pts',(-1.00708145117164,2.46571517701092,
8.86654584966059));
#391640=CARTESIAN_POINT('Ctrl Pts',(-1.00675706511739,2.45979749786491,
8.87215952290714));
#391641=CARTESIAN_POINT('Ctrl Pts',(-1.00671661105393,2.47051810124198,
8.85049129520029));
#391642=CARTESIAN_POINT('Ctrl Pts',(-1.01122897392942,2.47422481049724,
8.85711686593484));
#391643=CARTESIAN_POINT('Ctrl Pts',(-1.01802024859358,2.46903064544886,
8.85933012996512));
#391644=CARTESIAN_POINT('Origin',(-0.983102876847304,2.47363158005823,8.85049129520029));
#391645=CARTESIAN_POINT('Ctrl Pts',(-0.987408162934515,2.54608077127965,
8.78727029226991));
#391646=CARTESIAN_POINT('Ctrl Pts',(-0.98673715292638,2.55195487727524,
8.79393457792714));
#391647=CARTESIAN_POINT('Ctrl Pts',(-0.978151351640492,2.55291583068589,
8.79610912703474));
#391648=CARTESIAN_POINT('Ctrl Pts',(-0.990108979344114,2.52243748478278,
8.80838214965002));
#391649=CARTESIAN_POINT('Ctrl Pts',(-0.98943808077443,2.52831061523215,
8.81501364461994));
#391650=CARTESIAN_POINT('Ctrl Pts',(-0.980885428519784,2.529259800149,8.81722098428721));
#391651=CARTESIAN_POINT('Ctrl Pts',(-0.992813526340817,2.49876154025726,
8.82945683644723));
#391652=CARTESIAN_POINT('Ctrl Pts',(-0.992145265042226,2.50461158370381,
8.83607469902389));
#391653=CARTESIAN_POINT('Ctrl Pts',(-0.9836239779151,2.50557059788233,8.8382956714852));
#391654=CARTESIAN_POINT('Ctrl Pts',(-0.995522110700926,2.47505025214474,
8.85049129520029));
#391655=CARTESIAN_POINT('Ctrl Pts',(-0.994859350710966,2.48085213644373,
8.85711686593484));
#391656=CARTESIAN_POINT('Ctrl Pts',(-0.986367352980517,2.48184548263713,
8.85933012996512));
#391657=CARTESIAN_POINT('Origin',(-0.974988929080893,2.54466209919314,8.78727029226991));
#391658=CARTESIAN_POINT('Ctrl Pts',(-0.985837683686198,2.55982878158037,
8.75374538247849));
#391659=CARTESIAN_POINT('Ctrl Pts',(-0.984988286799116,2.56738013267245,
8.75304829418602));
#391660=CARTESIAN_POINT('Ctrl Pts',(-0.977845758623018,2.57007363122687,
8.75272238421917));
#391661=CARTESIAN_POINT('Ctrl Pts',(-0.985687874189948,2.56114023650868,
8.76769408445016));
#391662=CARTESIAN_POINT('Ctrl Pts',(-0.984816416926097,2.56888153596093,
8.76974318093967));
#391663=CARTESIAN_POINT('Ctrl Pts',(-0.977816320118229,2.57171296704089,
8.77077869880429));
#391664=CARTESIAN_POINT('Ctrl Pts',(-0.986455712341564,2.55441846563454,
8.78108014887993));
#391665=CARTESIAN_POINT('Ctrl Pts',(-0.985720959251959,2.56097936307297,
8.78639403366327));
#391666=CARTESIAN_POINT('Ctrl Pts',(-0.977971752381943,2.56331856563253,
8.78812224174741));
#391667=CARTESIAN_POINT('Ctrl Pts',(-0.987714029535122,2.543402967014,8.78944554828685));
#391668=CARTESIAN_POINT('Ctrl Pts',(-0.987100369825368,2.54893287111602,
8.79673892988685));
#391669=CARTESIAN_POINT('Ctrl Pts',(-0.978208869419684,2.54959978554248,
8.79894799272499));
#391670=CARTESIAN_POINT('Origin',(-0.973397453526334,2.55859407633733,8.75721825406948));
#391671=CARTESIAN_POINT('Origin',(-0.973397453526334,2.55859407633733,9.));
#391672=CARTESIAN_POINT('Origin',(-0.973397453526334,2.55859407633733,7.51860402984325));
#391673=CARTESIAN_POINT('Ctrl Pts',(-0.994252744839177,2.56004573276092,
7.50366195182966));
#391674=CARTESIAN_POINT('Ctrl Pts',(-0.995578475926535,2.56345928352135,
7.50000065167735));
#391675=CARTESIAN_POINT('Ctrl Pts',(-0.995578475926426,2.5634592835214,
7.49482233047108));
#391676=CARTESIAN_POINT('Ctrl Pts',(-0.988005205888649,2.56408578927888,
7.50215800491337));
#391677=CARTESIAN_POINT('Ctrl Pts',(-0.986691781976944,2.5669106104772,
7.49877273257267));
#391678=CARTESIAN_POINT('Ctrl Pts',(-0.983473834939355,2.5681603997447,
7.49481816995649));
#391679=CARTESIAN_POINT('Ctrl Pts',(-0.985497132441371,2.56281316053287,
7.51043025814042));
#391680=CARTESIAN_POINT('Ctrl Pts',(-0.98327195508721,2.56821143273141,
7.51006209594513));
#391681=CARTESIAN_POINT('Ctrl Pts',(-0.977839824358198,2.57027805458973,
7.50731281821697));
#391682=CARTESIAN_POINT('Ctrl Pts',(-0.985816858824492,2.56001124677168,
7.51860402984325));
#391683=CARTESIAN_POINT('Ctrl Pts',(-0.984954168022263,2.56757145721652,
7.51860402984324));
#391684=CARTESIAN_POINT('Ctrl Pts',(-0.977842190757043,2.57027715431147,
7.51860402984325));
#391685=CARTESIAN_POINT('Origin',(0.,0.,7.5));
#391686=CARTESIAN_POINT('Origin',(-1.15205371787331,2.40618167532513,7.5));
#391687=CARTESIAN_POINT('',(-1.15205371787331,2.40618167532513,7.59394543036555));
#391688=CARTESIAN_POINT('',(-1.15205371787331,2.40618167532513,8.85049129520029));
#391689=CARTESIAN_POINT('',(-1.15205371787331,2.40618167532513,7.5));
#391690=CARTESIAN_POINT('',(-1.14850738206912,2.47758611705878,8.78727029226991));
#391691=CARTESIAN_POINT('Ctrl Pts',(-1.15205371787331,2.40618167532513,
8.85049129520029));
#391692=CARTESIAN_POINT('Ctrl Pts',(-1.1508698876244,2.43001775366008,8.82945686509571));
#391693=CARTESIAN_POINT('Ctrl Pts',(-1.14968781728231,2.45381839678238,
8.80838212259896));
#391694=CARTESIAN_POINT('Ctrl Pts',(-1.14850738206912,2.47758611705878,
8.78727029226991));
#391695=CARTESIAN_POINT('',(-1.14781180121217,2.4915914356506,8.75721825406948));
#391696=CARTESIAN_POINT('Origin',(-1.14990524686335,2.44944458354024,8.75937679713147));
#391697=CARTESIAN_POINT('',(-1.14781180121217,2.4915914356506,7.51860402984325));
#391698=CARTESIAN_POINT('',(-1.14781180121217,2.4915914356506,7.5));
#391699=CARTESIAN_POINT('Ctrl Pts',(-1.14781180121217,2.4915914356506,7.51860402984325));
#391700=CARTESIAN_POINT('Ctrl Pts',(-1.14835807179202,2.48059243613578,
7.52834476460825));
#391701=CARTESIAN_POINT('Ctrl Pts',(-1.14890469700286,2.4695862962292,7.53807742314407));
#391702=CARTESIAN_POINT('Ctrl Pts',(-1.14945168875187,2.45857277618268,
7.54780169004674));
#391703=CARTESIAN_POINT('Ctrl Pts',(-1.15031809411993,2.44112795565897,
7.5632044032688));
#391704=CARTESIAN_POINT('Ctrl Pts',(-1.15118542018666,2.42366459713434,
7.57858609112103));
#391705=CARTESIAN_POINT('Ctrl Pts',(-1.15205371787331,2.40618167532513,
7.59394543036555));
#391706=CARTESIAN_POINT('Origin',(-1.38617896354006,2.56152510751204,7.5));
#391707=CARTESIAN_POINT('',(-1.23235567333047,2.45087725266272,8.75721825406948));
#391708=CARTESIAN_POINT('',(-1.22097218676271,2.4426889063615,8.78727029226991));
#391709=CARTESIAN_POINT('Origin',(-1.19207665202441,2.42190382934773,8.75658640621025));
#391710=CARTESIAN_POINT('',(-1.16293484201941,2.40094160211228,8.85049129520029));
#391711=CARTESIAN_POINT('Ctrl Pts',(-1.22097218676271,2.4426889063615,8.78727029226991));
#391712=CARTESIAN_POINT('Ctrl Pts',(-1.20165384546695,2.42879287656842,
8.80838212259896));
#391713=CARTESIAN_POINT('Ctrl Pts',(-1.18230874456758,2.41487759811193,
8.82945686509571));
#391714=CARTESIAN_POINT('Ctrl Pts',(-1.16293484201941,2.40094160211228,
8.85049129520029));
#391715=CARTESIAN_POINT('',(-1.16293484201941,2.40094160211228,7.59394543036555));
#391716=CARTESIAN_POINT('',(-1.16293484201941,2.40094160211228,7.5));
#391717=CARTESIAN_POINT('',(-1.23235567333047,2.45087725266272,7.51860402984325));
#391718=CARTESIAN_POINT('Ctrl Pts',(-1.16293484201941,2.40094160211228,
7.59394543036555));
#391719=CARTESIAN_POINT('Ctrl Pts',(-1.17714491544798,2.41116316309944,
7.57858609112103));
#391720=CARTESIAN_POINT('Ctrl Pts',(-1.19133908788948,2.42137328622108,
7.56320440326857));
#391721=CARTESIAN_POINT('Ctrl Pts',(-1.20551819269218,2.43157257091954,
7.54780169004651));
#391722=CARTESIAN_POINT('Ctrl Pts',(-1.21446995317456,2.43801173298109,
7.53807742314383));
#391723=CARTESIAN_POINT('Ctrl Pts',(-1.22341571509854,2.44444658017185,
7.52834476460825));
#391724=CARTESIAN_POINT('Ctrl Pts',(-1.23235567333047,2.45087725266272,
7.51860402984325));
#391725=CARTESIAN_POINT('',(-1.23235567333047,2.45087725266272,7.5));
#391726=CARTESIAN_POINT('Origin',(-1.15892025438442,2.40652270515029,7.5));
#391727=CARTESIAN_POINT('Ctrl Pts',(-1.16293484201941,2.40094160211228,
8.85049129520029));
#391728=CARTESIAN_POINT('Ctrl Pts',(-1.16277762822756,2.40082851540871,
8.85097269580138));
#391729=CARTESIAN_POINT('Ctrl Pts',(-1.16261748621827,2.40072368386098,
8.85143669361005));
#391730=CARTESIAN_POINT('Ctrl Pts',(-1.16244656312289,2.40062301180748,
8.8519052845931));
#391731=CARTESIAN_POINT('Ctrl Pts',(-1.16211224838786,2.40042610365524,
8.85282181883899));
#391732=CARTESIAN_POINT('Ctrl Pts',(-1.16174518876679,2.40025034340576,
8.85372622499635));
#391733=CARTESIAN_POINT('Ctrl Pts',(-1.16133296549049,2.4001068797526,8.8546225773507));
#391734=CARTESIAN_POINT('Ctrl Pts',(-1.16099075236728,2.39998778132309,
8.85536669723986));
#391735=CARTESIAN_POINT('Ctrl Pts',(-1.160617346026,2.39989088383229,8.85610498449051));
#391736=CARTESIAN_POINT('Ctrl Pts',(-1.16020359950662,2.39983030360422,
8.8568133821837));
#391737=CARTESIAN_POINT('Ctrl Pts',(-1.15982812389048,2.3997753269521,8.85745625420284));
#391738=CARTESIAN_POINT('Ctrl Pts',(-1.15941480250413,2.39974897790985,
8.85808743050666));
#391739=CARTESIAN_POINT('Ctrl Pts',(-1.15894967359852,2.3997762147569,8.85866804508411));
#391740=CARTESIAN_POINT('Ctrl Pts',(-1.15873507320424,2.3997887812477,8.85893592806396));
#391741=CARTESIAN_POINT('Ctrl Pts',(-1.15850935230517,2.39981297869224,
8.85919241173848));
#391742=CARTESIAN_POINT('Ctrl Pts',(-1.15827074428048,2.39985280471823,
8.85943017985534));
#391743=CARTESIAN_POINT('Ctrl Pts',(-1.15794855281163,2.39990658164309,
8.8597512372));
#391744=CARTESIAN_POINT('Ctrl Pts',(-1.15759476909802,2.39999085472496,
8.86004599534705));
#391745=CARTESIAN_POINT('Ctrl Pts',(-1.15721605712056,2.40011474307081,
8.86026130871721));
#391746=CARTESIAN_POINT('Ctrl Pts',(-1.15707739998859,2.40016010208701,
8.86034014101235));
#391747=CARTESIAN_POINT('Ctrl Pts',(-1.15693331461312,2.40021144115132,
8.86040910639692));
#391748=CARTESIAN_POINT('Ctrl Pts',(-1.15678783942165,2.40026767842519,
8.86046313645506));
#391749=CARTESIAN_POINT('Ctrl Pts',(-1.15656082660371,2.40035543622008,
8.86054744990829));
#391750=CARTESIAN_POINT('Ctrl Pts',(-1.15632428564955,2.400457654485,8.86059655985668));
#391751=CARTESIAN_POINT('Ctrl Pts',(-1.15609327043939,2.40056750872953,
8.86059725258816));
#391752=CARTESIAN_POINT('Ctrl Pts',(-1.1558617214918,2.40067761678126,8.86059794692011));
#391753=CARTESIAN_POINT('Ctrl Pts',(-1.15563429688713,2.40079901655756,
8.86056369958366));
#391754=CARTESIAN_POINT('Ctrl Pts',(-1.15542162839184,2.40092176712125,
8.86048590497774));
#391755=CARTESIAN_POINT('Ctrl Pts',(-1.15536612824647,2.40095380136365,
8.86046560290182));
#391756=CARTESIAN_POINT('Ctrl Pts',(-1.15531095632764,2.40098642279829,
8.86044257503091));
#391757=CARTESIAN_POINT('Ctrl Pts',(-1.15525780078612,2.40101859513938,
8.86041778462583));
#391758=CARTESIAN_POINT('Ctrl Pts',(-1.15490012995227,2.40123507507238,
8.86025097596201));
#391759=CARTESIAN_POINT('Ctrl Pts',(-1.15458593018282,2.40146055442196,
8.8599848982295));
#391760=CARTESIAN_POINT('Ctrl Pts',(-1.1543194323759,2.40168156859716,8.85968173251462));
#391761=CARTESIAN_POINT('Ctrl Pts',(-1.15417847030455,2.40179847243324,
8.85952137522077));
#391762=CARTESIAN_POINT('Ctrl Pts',(-1.15404801525877,2.40191623341875,
8.85934740853961));
#391763=CARTESIAN_POINT('Ctrl Pts',(-1.15392886528606,2.40203203692092,
8.8591675900182));
#391764=CARTESIAN_POINT('Ctrl Pts',(-1.15345041621272,2.4024970481756,8.85844552518695));
#391765=CARTESIAN_POINT('Ctrl Pts',(-1.15312510486535,2.40295460765929,
8.85759444184124));
#391766=CARTESIAN_POINT('Ctrl Pts',(-1.15289337286031,2.40335150126387,
8.85683498915139));
#391767=CARTESIAN_POINT('Ctrl Pts',(-1.15286912272314,2.40339303512258,
8.85675551444998));
#391768=CARTESIAN_POINT('Ctrl Pts',(-1.15284591626142,2.40343391112278,
8.85667699793651));
#391769=CARTESIAN_POINT('Ctrl Pts',(-1.15282369784459,2.40347407190827,
8.85659965593547));
#391770=CARTESIAN_POINT('Ctrl Pts',(-1.15252379252047,2.40401616424001,
8.85555568965886));
#391771=CARTESIAN_POINT('Ctrl Pts',(-1.15231385378249,2.40458046081932,
8.85434650606346));
#391772=CARTESIAN_POINT('Ctrl Pts',(-1.15218701911588,2.40516758421234,
8.85297329937118));
#391773=CARTESIAN_POINT('Ctrl Pts',(-1.15211568234407,2.40549780534695,
8.85220095427748));
#391774=CARTESIAN_POINT('Ctrl Pts',(-1.15207091337417,2.40583544890816,
8.85137579139184));
#391775=CARTESIAN_POINT('Ctrl Pts',(-1.15205371787331,2.40618167532513,
8.85049129520029));
#391776=CARTESIAN_POINT('Origin',(-1.15892025438442,2.40652270515029,7.59394543036555));
#391777=CARTESIAN_POINT('Ctrl Pts',(-1.16247839734608,2.40061327326238,
7.59443877723642));
#391778=CARTESIAN_POINT('Ctrl Pts',(-1.15777745639004,2.39723180201801,
7.58783886950016));
#391779=CARTESIAN_POINT('Ctrl Pts',(-1.15135964648121,2.40278976005228,
7.58559994247159));
#391780=CARTESIAN_POINT('Ctrl Pts',(-1.18814069610537,2.4190726255773,7.56670252222139));
#391781=CARTESIAN_POINT('Ctrl Pts',(-1.1834465493436,2.41569604151893,7.5600487499903));
#391782=CARTESIAN_POINT('Ctrl Pts',(-1.17697672466144,2.4212707814983,7.55786368756704));
#391783=CARTESIAN_POINT('Ctrl Pts',(-1.21375507308567,2.43749750689605,
7.5388891333356));
#391784=CARTESIAN_POINT('Ctrl Pts',(-1.20903302877989,2.43410085563325,
7.53222002137279));
#391785=CARTESIAN_POINT('Ctrl Pts',(-1.20254755552054,2.43971700033597,
7.53005029815327));
#391786=CARTESIAN_POINT('Ctrl Pts',(-1.23932036921912,2.45588708348032,
7.51101258149734));
#391787=CARTESIAN_POINT('Ctrl Pts',(-1.23454108515619,2.45244925863236,
7.5043616886572));
#391788=CARTESIAN_POINT('Ctrl Pts',(-1.22807082731704,2.45812757220591,
7.50217374673251));
#391789=CARTESIAN_POINT('',(-1.22670887334887,2.45714515960792,7.50366116523517));
#391790=CARTESIAN_POINT('Ctrl Pts',(-1.23235567333047,2.45087725266272,
7.51860402984325));
#391791=CARTESIAN_POINT('Ctrl Pts',(-1.23271417190462,2.45113512712465,
7.51734760759493));
#391792=CARTESIAN_POINT('Ctrl Pts',(-1.23300338406208,2.45141645289303,
7.51608817408573));
#391793=CARTESIAN_POINT('Ctrl Pts',(-1.23321333356108,2.45173015496622,
7.5148100591312));
#391794=CARTESIAN_POINT('Ctrl Pts',(-1.23340351083418,2.45201431380027,
7.51365231206384));
#391795=CARTESIAN_POINT('Ctrl Pts',(-1.23352912772805,2.45232529934387,
7.51247773061043));
#391796=CARTESIAN_POINT('Ctrl Pts',(-1.23355377319633,2.45267156000965,
7.51129758471022));
#391797=CARTESIAN_POINT('Ctrl Pts',(-1.2335844046988,2.45310192247276,7.50983079813402));
#391798=CARTESIAN_POINT('Ctrl Pts',(-1.23344508972212,2.4535739665468,7.50839324291155));
#391799=CARTESIAN_POINT('Ctrl Pts',(-1.23305574351697,2.45406780194779,
7.50715379678855));
#391800=CARTESIAN_POINT('Ctrl Pts',(-1.23287587678894,2.45429593967352,
7.50658120839351));
#391801=CARTESIAN_POINT('Ctrl Pts',(-1.23260961778089,2.45455527707925,
7.50598221009429));
#391802=CARTESIAN_POINT('Ctrl Pts',(-1.23224743207232,2.45482334770212,
7.50545747549611));
#391803=CARTESIAN_POINT('Ctrl Pts',(-1.23205415856753,2.45496639848405,
7.50517746087247));
#391804=CARTESIAN_POINT('Ctrl Pts',(-1.23183159348026,2.45511365010213,
7.50491486231392));
#391805=CARTESIAN_POINT('Ctrl Pts',(-1.23158471033428,2.45525981197483,
7.50468370960992));
#391806=CARTESIAN_POINT('Ctrl Pts',(-1.23121554215618,2.45547837007868,
7.50433806340447));
#391807=CARTESIAN_POINT('Ctrl Pts',(-1.23078064602178,2.45570056625099,
7.50405484070984));
#391808=CARTESIAN_POINT('Ctrl Pts',(-1.23030898543559,2.45591079803974,
7.50385766036131));
#391809=CARTESIAN_POINT('Ctrl Pts',(-1.23025854866716,2.4559332790618,7.50383657498791));
#391810=CARTESIAN_POINT('Ctrl Pts',(-1.2302077196755,2.45595562650314,7.50381643264937));
#391811=CARTESIAN_POINT('Ctrl Pts',(-1.23015655431109,2.45597782395209,
7.50379723213559));
#391812=CARTESIAN_POINT('Ctrl Pts',(-1.22981500876628,2.45612599918515,
7.50366906242519));
#391813=CARTESIAN_POINT('Ctrl Pts',(-1.22945075886669,2.45627005426621,
7.50358235568538));
#391814=CARTESIAN_POINT('Ctrl Pts',(-1.22909632909184,2.45640046610439,
7.5035341175365));
#391815=CARTESIAN_POINT('Ctrl Pts',(-1.22856490175816,2.45659600389596,
7.50346178989176));
#391816=CARTESIAN_POINT('Ctrl Pts',(-1.22798489283784,2.45678376238722,
7.50346967198527));
#391817=CARTESIAN_POINT('Ctrl Pts',(-1.22740983222607,2.45695056293592,
7.50354272648692));
#391818=CARTESIAN_POINT('Ctrl Pts',(-1.2271732978934,2.45701917145416,7.50357277531559));
#391819=CARTESIAN_POINT('Ctrl Pts',(-1.22693795451662,2.45708427923446,
7.50361331098761));
#391820=CARTESIAN_POINT('Ctrl Pts',(-1.2267088733495,2.45714515960919,7.50366116523658));
#391821=CARTESIAN_POINT('',(-1.16019063351033,2.40916067458745,7.57603338622103));
#391822=CARTESIAN_POINT('Origin',(-1.16402226679194,2.41712371898021,7.58486873427626));
#391823=CARTESIAN_POINT('Ctrl Pts',(-1.22670887339831,2.45714515963697,
7.50366116529968));
#391824=CARTESIAN_POINT('Ctrl Pts',(-1.20457181913612,2.44117710943059,
7.5278357307971));
#391825=CARTESIAN_POINT('Ctrl Pts',(-1.18240010892814,2.42518305082276,
7.55196141284068));
#391826=CARTESIAN_POINT('Ctrl Pts',(-1.1601906346913,2.40916067500333,7.57603338728831));
#391827=CARTESIAN_POINT('Ctrl Pts',(-1.16366703458209,2.40168485817273,
7.59639677331371));
#391828=CARTESIAN_POINT('Ctrl Pts',(-1.150703165123,2.38880037120595,7.59959882295466));
#391829=CARTESIAN_POINT('Ctrl Pts',(-1.15216122323504,2.40703722617454,
7.59642833564546));
#391830=CARTESIAN_POINT('Ctrl Pts',(-1.1613783588536,2.39852620854139,7.58707626057423));
#391831=CARTESIAN_POINT('Ctrl Pts',(-1.15468113347973,2.39749690619124,
7.58809943920598));
#391832=CARTESIAN_POINT('Ctrl Pts',(-1.15122410194199,2.40330752868285,
7.58710240504253));
#391833=CARTESIAN_POINT('Ctrl Pts',(-1.16034302571033,2.40451400592808,
7.58015376756929));
#391834=CARTESIAN_POINT('Ctrl Pts',(-1.15760519591842,2.40371804146506,
7.58205880659761));
#391835=CARTESIAN_POINT('Ctrl Pts',(-1.15649513461972,2.40630548015058,
7.58020924244128));
#391836=CARTESIAN_POINT('Ctrl Pts',(-1.16019063315144,2.40916067384175,
7.57603338509286));
#391837=CARTESIAN_POINT('Ctrl Pts',(-1.16019063315144,2.40916067384175,
7.57603338509286));
#391838=CARTESIAN_POINT('Ctrl Pts',(-1.16019063315144,2.40916067384175,
7.57603338509286));
#391839=CARTESIAN_POINT('Origin',(-1.16402740803779,2.41712124308687,7.58486873427621));
#391840=CARTESIAN_POINT('Ctrl Pts',(-1.14738488275126,2.50018731490473,
7.51098857897448));
#391841=CARTESIAN_POINT('Ctrl Pts',(-1.14767691925914,2.49430724461179,
7.50433767179956));
#391842=CARTESIAN_POINT('Ctrl Pts',(-1.15615057871821,2.49278897373538,
7.50214974420965));
#391843=CARTESIAN_POINT('Ctrl Pts',(-1.14894748356406,2.46872480124226,
7.53887321589168));
#391844=CARTESIAN_POINT('Ctrl Pts',(-1.14923602095631,2.46291518462666,
7.5322040745206));
#391845=CARTESIAN_POINT('Ctrl Pts',(-1.15767055140445,2.46134623082198,
7.53003438070911));
#391846=CARTESIAN_POINT('Ctrl Pts',(-1.15051308514685,2.43720186794752,
7.5666946565923));
#391847=CARTESIAN_POINT('Ctrl Pts',(-1.15079991733676,2.431426585086,7.56004085833295));
#391848=CARTESIAN_POINT('Ctrl Pts',(-1.15919230779772,2.42984404520438,
7.55785582193789));
#391849=CARTESIAN_POINT('Ctrl Pts',(-1.15208161669372,2.40561994067663,
7.59443891967696));
#391850=CARTESIAN_POINT('Ctrl Pts',(-1.15236886475459,2.39983628437403,
7.58783901202978));
#391851=CARTESIAN_POINT('Ctrl Pts',(-1.1607156901291,2.39828396863432,7.58560008491213));
#391852=CARTESIAN_POINT('',(-1.15623297039277,2.49108456570912,7.50366116523517));
#391853=CARTESIAN_POINT('Ctrl Pts',(-1.15623297039293,2.49108456570945,
7.50366116523554));
#391854=CARTESIAN_POINT('Ctrl Pts',(-1.15562413094776,2.49153562229877,
7.50350835821027));
#391855=CARTESIAN_POINT('Ctrl Pts',(-1.15504978507181,2.49193044482337,
7.50345484956));
#391856=CARTESIAN_POINT('Ctrl Pts',(-1.15449319717327,2.49228126653247,
7.50349758195598));
#391857=CARTESIAN_POINT('Ctrl Pts',(-1.15420762630368,2.49246126408686,
7.50351950684424));
#391858=CARTESIAN_POINT('Ctrl Pts',(-1.15389865214386,2.49264752943229,
7.50357029184312));
#391859=CARTESIAN_POINT('Ctrl Pts',(-1.153595774694,2.49281895317992,7.50365515313923));
#391860=CARTESIAN_POINT('Ctrl Pts',(-1.15312982652892,2.4930826723201,7.50378570417639));
#391861=CARTESIAN_POINT('Ctrl Pts',(-1.15266480092322,2.49331930930964,
7.50400001621911));
#391862=CARTESIAN_POINT('Ctrl Pts',(-1.15223506338678,2.49350882914526,
7.50428903009635));
#391863=CARTESIAN_POINT('Ctrl Pts',(-1.15218736582644,2.49352986438893,
7.50432110841318));
#391864=CARTESIAN_POINT('Ctrl Pts',(-1.15214008709819,2.49355034499864,
7.50435406373354));
#391865=CARTESIAN_POINT('Ctrl Pts',(-1.15209326220262,2.49357026247505,
7.50438785222352));
#391866=CARTESIAN_POINT('Ctrl Pts',(-1.15180737370825,2.49369186824209,
7.50459414719561));
#391867=CARTESIAN_POINT('Ctrl Pts',(-1.15153364917505,2.49379394363759,
7.50483629897752));
#391868=CARTESIAN_POINT('Ctrl Pts',(-1.15128303474166,2.49387381126593,
7.5050991045531));
#391869=CARTESIAN_POINT('Ctrl Pts',(-1.15073015412978,2.49405000727601,
7.50567888004914));
#391870=CARTESIAN_POINT('Ctrl Pts',(-1.15026811890362,2.49412555961324,
7.50637912803144));
#391871=CARTESIAN_POINT('Ctrl Pts',(-1.1498937804739,2.49413121733846,7.50710440483569));
#391872=CARTESIAN_POINT('Ctrl Pts',(-1.14980198525928,2.494132604725,7.50728225710685));
#391873=CARTESIAN_POINT('Ctrl Pts',(-1.14971363833864,2.4941299627054,7.50746498566954));
#391874=CARTESIAN_POINT('Ctrl Pts',(-1.14963078956236,2.49412376935997,
7.50764697238949));
#391875=CARTESIAN_POINT('Ctrl Pts',(-1.14918541734167,2.49409047563941,
7.50862528291181));
#391876=CARTESIAN_POINT('Ctrl Pts',(-1.14885819440523,2.4939556593938,7.50965856837421));
#391877=CARTESIAN_POINT('Ctrl Pts',(-1.14860832253323,2.49377157864745,
7.51067959873201));
#391878=CARTESIAN_POINT('Ctrl Pts',(-1.1484708177269,2.49367027878055,7.51124147302578));
#391879=CARTESIAN_POINT('Ctrl Pts',(-1.14835696135857,2.49355368560418,
7.51180065547252));
#391880=CARTESIAN_POINT('Ctrl Pts',(-1.14826164413805,2.49342838141802,
7.512351757165));
#391881=CARTESIAN_POINT('Ctrl Pts',(-1.14793228517129,2.49299540553957,
7.51425603304535));
#391882=CARTESIAN_POINT('Ctrl Pts',(-1.14778983637917,2.4924031262395,7.5162690050518));
#391883=CARTESIAN_POINT('Ctrl Pts',(-1.14780750680636,2.49170562597439,
7.51827788969243));
#391884=CARTESIAN_POINT('Ctrl Pts',(-1.14780846316327,2.49166787594195,
7.51838661432545));
#391885=CARTESIAN_POINT('Ctrl Pts',(-1.14780989531214,2.4916298103943,7.51849533314856));
#391886=CARTESIAN_POINT('Ctrl Pts',(-1.14781180121217,2.4915914356506,7.51860402984325));
#391887=CARTESIAN_POINT('Ctrl Pts',(-1.16019063309945,2.40916067577124,
7.57603338728985));
#391888=CARTESIAN_POINT('Ctrl Pts',(-1.15887005024747,2.43651452986977,
7.55196141284922));
#391889=CARTESIAN_POINT('Ctrl Pts',(-1.15755087359416,2.46382120338538,
7.52783573083105));
#391890=CARTESIAN_POINT('Ctrl Pts',(-1.1562329703845,2.49108456576772,7.50366116530176));
#391891=CARTESIAN_POINT('Origin',(-4.00899494394873E-16,8.32476377985984E-16,
7.49482233047033));
#391892=CARTESIAN_POINT('Origin',(-1.22276082553378,2.44923706764779,7.49482233047033));
#391893=CARTESIAN_POINT('Origin',(0.,0.,7.50366116523517));
#391894=CARTESIAN_POINT('Origin',(-1.15251174268205,2.48306724294369,7.49482233047033));
#391895=CARTESIAN_POINT('Ctrl Pts',(-1.23235481470267,2.4508766349812,7.51860402984325));
#391896=CARTESIAN_POINT('Ctrl Pts',(-1.23853136886432,2.45532033442179,
7.51860402984325));
#391897=CARTESIAN_POINT('Ctrl Pts',(-1.2453154483411,2.45187467749129,7.51860402984325));
#391898=CARTESIAN_POINT('Ctrl Pts',(-1.23464821215601,2.45252660987737,
7.51041458714365));
#391899=CARTESIAN_POINT('Ctrl Pts',(-1.24013859051313,2.45450401000274,
7.51004642900441));
#391900=CARTESIAN_POINT('Ctrl Pts',(-1.24531731930967,2.45187372722002,
7.50729136483008));
#391901=CARTESIAN_POINT('Ctrl Pts',(-1.23389344099837,2.45523844646884,
7.50215815450138));
#391902=CARTESIAN_POINT('Ctrl Pts',(-1.23686619043908,2.4561662531536,7.49877163671531));
#391903=CARTESIAN_POINT('Ctrl Pts',(-1.23995309199552,2.45462516185998,
7.49481588533172));
#391904=CARTESIAN_POINT('Ctrl Pts',(-1.22670862744822,2.4571446670605,7.50366171572174));
#391905=CARTESIAN_POINT('Ctrl Pts',(-1.22834420829843,2.46042079855047,
7.50000045605858));
#391906=CARTESIAN_POINT('Ctrl Pts',(-1.22834420829854,2.46042079855041,
7.49482233047317));
#391907=CARTESIAN_POINT('Origin',(-1.23965492357592,2.4407297925936,7.51860402984325));
#391908=CARTESIAN_POINT('Origin',(-1.23965492357592,2.4407297925936,9.));
#391909=CARTESIAN_POINT('Origin',(-1.23965492357592,2.4407297925936,8.75721825406948));
#391910=CARTESIAN_POINT('Ctrl Pts',(-1.21879855353204,2.4411253357326,8.78942910404912));
#391911=CARTESIAN_POINT('Ctrl Pts',(-1.22331043706215,2.44439570814448,
8.79672699501691));
#391912=CARTESIAN_POINT('Ctrl Pts',(-1.2297870263298,2.43825345469479,8.79893251111267));
#391913=CARTESIAN_POINT('Ctrl Pts',(-1.22772371753385,2.44754537204725,
8.78111911759583));
#391914=CARTESIAN_POINT('Ctrl Pts',(-1.23307697638014,2.45141640935657,
8.78644465894813));
#391915=CARTESIAN_POINT('Ctrl Pts',(-1.24001845580617,2.44722936085515,
8.78817647674132));
#391916=CARTESIAN_POINT('Ctrl Pts',(-1.2332860926436,2.45154649178503,8.76780923932029));
#391917=CARTESIAN_POINT('Ctrl Pts',(-1.23960837464324,2.45611195858344,
8.76988516158374));
#391918=CARTESIAN_POINT('Ctrl Pts',(-1.24641619895659,2.45282715896781,
8.77093053738833));
#391919=CARTESIAN_POINT('Ctrl Pts',(-1.23220150562467,2.45076632819392,
8.75371302330492));
#391920=CARTESIAN_POINT('Ctrl Pts',(-1.23836817271516,2.45522036213663,
8.75300828287559));
#391921=CARTESIAN_POINT('Ctrl Pts',(-1.2451686804961,2.45173501663644,8.75267964240738));
#391922=CARTESIAN_POINT('Origin',(-1.22827143700815,2.43254144629238,8.78727029226991));
#391923=CARTESIAN_POINT('Ctrl Pts',(-1.16293484201941,2.40094160211228,
8.85049129520029));
#391924=CARTESIAN_POINT('Ctrl Pts',(-1.16767542343881,2.40435158745377,
8.85711686593484));
#391925=CARTESIAN_POINT('Ctrl Pts',(-1.17411995340354,2.39873297591287,
8.85933012996512));
#391926=CARTESIAN_POINT('Ctrl Pts',(-1.18230877056806,2.41487761681455,
8.82945683644722));
#391927=CARTESIAN_POINT('Ctrl Pts',(-1.18708870167946,2.41831590709606,
8.83607469902388));
#391928=CARTESIAN_POINT('Ctrl Pts',(-1.19352750769645,2.41265253181511,
8.8382956714852));
#391929=CARTESIAN_POINT('Ctrl Pts',(-1.20165382071392,2.42879285876312,
8.80838214965002));
#391930=CARTESIAN_POINT('Ctrl Pts',(-1.20645261566516,2.43224471814342,
8.81501364461987));
#391931=CARTESIAN_POINT('Ctrl Pts',(-1.21290523209919,2.42655151572733,
8.81722098428721));
#391932=CARTESIAN_POINT('Ctrl Pts',(-1.22097218676271,2.4426889063615,8.78727029226991));
#391933=CARTESIAN_POINT('Ctrl Pts',(-1.22577177880958,2.44614133910699,
8.79393457792714));
#391934=CARTESIAN_POINT('Ctrl Pts',(-1.23225539332381,2.44043150916127,
8.79610912703474));
#391935=CARTESIAN_POINT('Origin',(-1.17023409226486,2.39079414204316,8.85049129520029));
#391936=CARTESIAN_POINT('Ctrl Pts',(-1.15205371787331,2.40618167532513,
8.85049129520029));
#391937=CARTESIAN_POINT('Ctrl Pts',(-1.15176404759817,2.41201410220893,
8.85711686593484));
#391938=CARTESIAN_POINT('Ctrl Pts',(-1.14335314149695,2.41354949162871,
8.85933012996512));
#391939=CARTESIAN_POINT('Ctrl Pts',(-1.1523099849843,2.40102181145301,8.86332496987233));
#391940=CARTESIAN_POINT('Ctrl Pts',(-1.14827702912887,2.4032772851161,8.86648636486737));
#391941=CARTESIAN_POINT('Ctrl Pts',(-1.14408717074441,2.39911541190672,
8.87206031107457));
#391942=CARTESIAN_POINT('Ctrl Pts',(-1.15871241903328,2.3979043374364,8.86341338519875));
#391943=CARTESIAN_POINT('Ctrl Pts',(-1.16299120812191,2.39612517061758,
8.86654584966059));
#391944=CARTESIAN_POINT('Ctrl Pts',(-1.16228834154897,2.39024043346389,
8.87215952290714));
#391945=CARTESIAN_POINT('Ctrl Pts',(-1.16293484201941,2.40094160211228,
8.85049129520029));
#391946=CARTESIAN_POINT('Ctrl Pts',(-1.16767542343881,2.40435158745377,
8.85711686593484));
#391947=CARTESIAN_POINT('Ctrl Pts',(-1.17411995340354,2.39873297591287,
8.85933012996512));
#391948=CARTESIAN_POINT('Origin',(-1.13956910603494,2.40556162109757,8.85049129520029));
#391949=CARTESIAN_POINT('Ctrl Pts',(-1.14850738206912,2.47758611705878,
8.78727029226991));
#391950=CARTESIAN_POINT('Ctrl Pts',(-1.14821410598634,2.48349114583244,
8.79393457792714));
#391951=CARTESIAN_POINT('Ctrl Pts',(-1.13970751364643,2.48500021903835,
8.79610912703474));
#391952=CARTESIAN_POINT('Ctrl Pts',(-1.14968781879483,2.45381836632826,
8.80838214965003));
#391953=CARTESIAN_POINT('Ctrl Pts',(-1.14939459141807,2.45972241442017,
8.81501364461993));
#391954=CARTESIAN_POINT('Ctrl Pts',(-1.14092032599118,2.46121761944618,
8.81722098428721));
#391955=CARTESIAN_POINT('Ctrl Pts',(-1.15086988603566,2.43001778564899,
8.82945683644723));
#391956=CARTESIAN_POINT('Ctrl Pts',(-1.15057781132211,2.43589862520227,
8.8360746990239));
#391957=CARTESIAN_POINT('Ctrl Pts',(-1.14213547634267,2.43740162972406,
8.83829567148519));
#391958=CARTESIAN_POINT('Ctrl Pts',(-1.15205371787331,2.40618167532513,
8.85049129520029));
#391959=CARTESIAN_POINT('Ctrl Pts',(-1.15176404759817,2.41201410220893,
8.85711686593484));
#391960=CARTESIAN_POINT('Ctrl Pts',(-1.14335314149695,2.41354949162871,
8.85933012996512));
#391961=CARTESIAN_POINT('Origin',(-1.13602277023075,2.47696606283122,8.78727029226991));
#391962=CARTESIAN_POINT('Ctrl Pts',(-1.14782096758312,2.49140650154879,
8.75374538247848));
#391963=CARTESIAN_POINT('Ctrl Pts',(-1.14745713259866,2.49899675862558,
8.75304829418602));
#391964=CARTESIAN_POINT('Ctrl Pts',(-1.14050185255763,2.5021423464498,8.75272238421917));
#391965=CARTESIAN_POINT('Ctrl Pts',(-1.1477554910923,2.49272486027965,8.76769408445018));
#391966=CARTESIAN_POINT('Ctrl Pts',(-1.1473818110897,2.50050608886052,8.76974318093968));
#391967=CARTESIAN_POINT('Ctrl Pts',(-1.14057750714365,2.50378020020404,
8.7707786988043));
#391968=CARTESIAN_POINT('Ctrl Pts',(-1.14809108629952,2.48596770444543,
8.78108014887992));
#391969=CARTESIAN_POINT('Ctrl Pts',(-1.14777820098109,2.49256219760851,
8.78639403366326));
#391970=CARTESIAN_POINT('Ctrl Pts',(-1.14019478891025,2.49539308741435,
8.78812224174741));
#391971=CARTESIAN_POINT('Ctrl Pts',(-1.14864105272563,2.4748942176888,8.78944554828685));
#391972=CARTESIAN_POINT('Ctrl Pts',(-1.14838295601785,2.48045207732236,
8.79673892988686));
#391973=CARTESIAN_POINT('Ctrl Pts',(-1.13955245350738,2.48168730188856,
8.79894799272499));
#391974=CARTESIAN_POINT('Origin',(-1.1353271893738,2.49097138142304,8.75721825406948));
#391975=CARTESIAN_POINT('Origin',(-1.1353271893738,2.49097138142304,9.));
#391976=CARTESIAN_POINT('Origin',(-1.1353271893738,2.49097138142304,7.51860402984325));
#391977=CARTESIAN_POINT('Ctrl Pts',(-1.15623263920031,2.49108385216065,
7.50366195182966));
#391978=CARTESIAN_POINT('Ctrl Pts',(-1.1577743533791,2.49440544953254,7.50000065167735));
#391979=CARTESIAN_POINT('Ctrl Pts',(-1.157774353379,2.49440544953259,7.49482233047108));
#391980=CARTESIAN_POINT('Ctrl Pts',(-1.15025678379844,2.49551588914409,
7.50215800491337));
#391981=CARTESIAN_POINT('Ctrl Pts',(-1.14912704537262,2.49841905780326,
7.49877273257265));
#391982=CARTESIAN_POINT('Ctrl Pts',(-1.14599578422563,2.49987245381925,
7.49481816995647));
#391983=CARTESIAN_POINT('Ctrl Pts',(-1.14767232585334,2.49440656796784,
7.51043025814041));
#391984=CARTESIAN_POINT('Ctrl Pts',(-1.14579758885198,2.49993631643975,
7.51006209594514));
#391985=CARTESIAN_POINT('Ctrl Pts',(-1.14050902793523,2.50234673001258,
7.50731281821699));
#391986=CARTESIAN_POINT('Ctrl Pts',(-1.14781187609327,2.49158992609926,
7.51860402984325));
#391987=CARTESIAN_POINT('Ctrl Pts',(-1.14743534212812,2.49918987607039,
7.51860402984325));
#391988=CARTESIAN_POINT('Ctrl Pts',(-1.14051133179102,2.50234567996835,
7.51860402984325));
#391989=CARTESIAN_POINT('Origin',(0.,0.,7.5));
#391990=CARTESIAN_POINT('Origin',(-1.30385128920421,2.32742558187726,7.5));
#391991=CARTESIAN_POINT('',(-1.30385128920421,2.32742558187726,7.59394543036555));
#391992=CARTESIAN_POINT('',(-1.30385128920421,2.32742558187726,8.85049129520029));
#391993=CARTESIAN_POINT('',(-1.30385128920421,2.32742558187726,7.5));
#391994=CARTESIAN_POINT('',(-1.30488713801675,2.39891053004237,8.78727029226991));
#391995=CARTESIAN_POINT('Ctrl Pts',(-1.30385128920421,2.32742558187726,
8.85049129520029));
#391996=CARTESIAN_POINT('Ctrl Pts',(-1.30419707404391,2.35128853469733,
8.82945686509571));
#391997=CARTESIAN_POINT('Ctrl Pts',(-1.30454234483264,2.37511601235256,
8.80838212259895));
#391998=CARTESIAN_POINT('Ctrl Pts',(-1.30488713801675,2.39891053004237,
8.78727029226991));
#391999=CARTESIAN_POINT('',(-1.30509031014835,2.41293163922359,8.75721825406948));
#392000=CARTESIAN_POINT('Origin',(-1.30447909650469,2.37073725481655,8.75937679713112));
#392001=CARTESIAN_POINT('',(-1.30509031014835,2.41293163922359,7.51860402984325));
#392002=CARTESIAN_POINT('',(-1.30509031014835,2.41293163922359,7.5));
#392003=CARTESIAN_POINT('Ctrl Pts',(-1.30509031014835,2.4129316392236,7.51860402984325));
#392004=CARTESIAN_POINT('Ctrl Pts',(-1.30493075003822,2.4019202386567,7.52834476460825));
#392005=CARTESIAN_POINT('Ctrl Pts',(-1.30477108634398,2.39090168964745,
7.53807742314407));
#392006=CARTESIAN_POINT('Ctrl Pts',(-1.30461131558764,2.37987575217738,
7.54780169004674));
#392007=CARTESIAN_POINT('Ctrl Pts',(-1.30435824734447,2.36241126312586,
7.5632044032688));
#392008=CARTESIAN_POINT('Ctrl Pts',(-1.3041049101745,2.34492821517237,7.57858609112103));
#392009=CARTESIAN_POINT('Ctrl Pts',(-1.30385128920421,2.32742558187726,
7.59394543036555));
#392010=CARTESIAN_POINT('Origin',(-1.54744838731665,2.4674493883293,7.5));
#392011=CARTESIAN_POINT('',(-1.38685191115371,2.3668843634066,8.75721825406948));
#392012=CARTESIAN_POINT('',(-1.37496718403118,2.3594421834296,8.78727029226991));
#392013=CARTESIAN_POINT('Origin',(-1.34479931381131,2.34055115485281,8.75658640621015));
#392014=CARTESIAN_POINT('',(-1.31437432427029,2.32149911893914,8.85049129520029));
#392015=CARTESIAN_POINT('Ctrl Pts',(-1.37496718403118,2.3594421834296,8.78727029226991));
#392016=CARTESIAN_POINT('Ctrl Pts',(-1.35479821265379,2.34681243489655,
8.80838212259896));
#392017=CARTESIAN_POINT('Ctrl Pts',(-1.33460130338718,2.33416519174224,
8.82945686509571));
#392018=CARTESIAN_POINT('Ctrl Pts',(-1.31437432427029,2.32149911893914,
8.85049129520029));
#392019=CARTESIAN_POINT('',(-1.31437432427029,2.32149911893914,7.59394543036555));
#392020=CARTESIAN_POINT('',(-1.31437432427029,2.32149911893914,7.5));
#392021=CARTESIAN_POINT('',(-1.38685191115371,2.3668843634066,7.51860402984325));
#392022=CARTESIAN_POINT('Ctrl Pts',(-1.31437432427029,2.32149911893914,
7.59394543036555));
#392023=CARTESIAN_POINT('Ctrl Pts',(-1.32921009923997,2.33078923610248,
7.57858609112103));
#392024=CARTESIAN_POINT('Ctrl Pts',(-1.34402927306631,2.34006895768037,
7.56320440326857));
#392025=CARTESIAN_POINT('Ctrl Pts',(-1.35883271579176,2.34933882849071,
7.54780169004651));
#392026=CARTESIAN_POINT('Ctrl Pts',(-1.36817864245192,2.35519121933988,
7.53807742314383));
#392027=CARTESIAN_POINT('Ctrl Pts',(-1.37751830642366,2.36103968851259,
7.52834476460825));
#392028=CARTESIAN_POINT('Ctrl Pts',(-1.38685191115371,2.3668843634066,7.51860402984324));
#392029=CARTESIAN_POINT('',(-1.38685191115371,2.3668843634066,7.5));
#392030=CARTESIAN_POINT('Origin',(-1.31072556753554,2.3273259705153,7.5));
#392031=CARTESIAN_POINT('Ctrl Pts',(-1.31437432427029,2.32149911893914,
8.85049129520029));
#392032=CARTESIAN_POINT('Ctrl Pts',(-1.31421018800106,2.32139633730656,
8.85097269580138));
#392033=CARTESIAN_POINT('Ctrl Pts',(-1.31404365844039,2.32130198148025,
8.85143669361005));
#392034=CARTESIAN_POINT('Ctrl Pts',(-1.31386663644422,2.32121246734861,
8.8519052845931));
#392035=CARTESIAN_POINT('Ctrl Pts',(-1.31352039264604,2.3210373833839,8.85282181883899));
#392036=CARTESIAN_POINT('Ctrl Pts',(-1.31314282619048,2.32088550184337,
8.85372622499635));
#392037=CARTESIAN_POINT('Ctrl Pts',(-1.31272225812329,2.32076874418766,
8.8546225773507));
#392038=CARTESIAN_POINT('Ctrl Pts',(-1.31237311745107,2.32067181612874,
8.85536669723986));
#392039=CARTESIAN_POINT('Ctrl Pts',(-1.31199427006962,2.32059904195065,
8.85610498449051));
#392040=CARTESIAN_POINT('Ctrl Pts',(-1.31157749224829,2.32056509502167,
8.85681338218371));
#392041=CARTESIAN_POINT('Ctrl Pts',(-1.31119926572088,2.3205342881303,8.85745625420284));
#392042=CARTESIAN_POINT('Ctrl Pts',(-1.31078510535871,2.32053447481713,
8.85808743050666));
#392043=CARTESIAN_POINT('Ctrl Pts',(-1.31032267718111,2.32059145661445,
8.8586680450841));
#392044=CARTESIAN_POINT('Ctrl Pts',(-1.31010932284418,2.32061774678053,
8.85893592806396));
#392045=CARTESIAN_POINT('Ctrl Pts',(-1.3098856160485,2.32065635649648,8.85919241173848));
#392046=CARTESIAN_POINT('Ctrl Pts',(-1.30965004993184,2.32071138836426,
8.85943017985534));
#392047=CARTESIAN_POINT('Ctrl Pts',(-1.30933196593932,2.32078569767694,
8.8597512372));
#392048=CARTESIAN_POINT('Ctrl Pts',(-1.30898430850719,2.32089246461108,
8.86004599534705));
#392049=CARTESIAN_POINT('Ctrl Pts',(-1.30861431218768,2.32104036257474,
8.86026130871721));
#392050=CARTESIAN_POINT('Ctrl Pts',(-1.3084788461038,2.32109451218892,8.86034014101235));
#392051=CARTESIAN_POINT('Ctrl Pts',(-1.30833834607233,2.32115497735333,
8.86040910639692));
#392052=CARTESIAN_POINT('Ctrl Pts',(-1.30819677290975,2.32122041970921,
8.86046313645506));
#392053=CARTESIAN_POINT('Ctrl Pts',(-1.30797584917522,2.32132254195748,
8.86054744990829));
#392054=CARTESIAN_POINT('Ctrl Pts',(-1.30774634336653,2.32143970543498,
8.86059655985668));
#392055=CARTESIAN_POINT('Ctrl Pts',(-1.30752284118751,2.32156413516752,
8.86059725258816));
#392056=CARTESIAN_POINT('Ctrl Pts',(-1.30729882262916,2.32168885238245,
8.86059794692011));
#392057=CARTESIAN_POINT('Ctrl Pts',(-1.30707964340311,2.32182457387434,
8.86056369958366));
#392058=CARTESIAN_POINT('Ctrl Pts',(-1.30687527651367,2.32196069795111,
8.86048590497774));
#392059=CARTESIAN_POINT('Ctrl Pts',(-1.30682194284026,2.32199622228224,
8.86046560290182));
#392060=CARTESIAN_POINT('Ctrl Pts',(-1.30676897434054,2.32203231156963,
8.86044257503091));
#392061=CARTESIAN_POINT('Ctrl Pts',(-1.30671798930176,2.32206782349643,
8.86041778462583));
#392062=CARTESIAN_POINT('Ctrl Pts',(-1.30637492325793,2.32230677469719,
8.86025097596201));
#392063=CARTESIAN_POINT('Ctrl Pts',(-1.30607581555712,2.32255192162361,
8.8599848982295));
#392064=CARTESIAN_POINT('Ctrl Pts',(-1.30582402572536,2.3227895562746,8.85968173251461));
#392065=CARTESIAN_POINT('Ctrl Pts',(-1.30569084333019,2.32291525139013,
8.85952137522076));
#392066=CARTESIAN_POINT('Ctrl Pts',(-1.30556820129054,2.32304112870655,
8.85934740853961));
#392067=CARTESIAN_POINT('Ctrl Pts',(-1.30545671568009,2.32316432824297,
8.8591675900182));
#392068=CARTESIAN_POINT('Ctrl Pts',(-1.30500904300506,2.32365903841954,
8.85844552518694));
#392069=CARTESIAN_POINT('Ctrl Pts',(-1.30471371598152,2.32413650056779,
8.85759444184122));
#392070=CARTESIAN_POINT('Ctrl Pts',(-1.30450788915529,2.32454742583243,
8.85683498915136));
#392071=CARTESIAN_POINT('Ctrl Pts',(-1.30448634992609,2.32459042806699,
8.85675551444997));
#392072=CARTESIAN_POINT('Ctrl Pts',(-1.30446581007887,2.32463270692617,
8.8566769979365));
#392073=CARTESIAN_POINT('Ctrl Pts',(-1.30444621042252,2.32467420873586,
8.85659965593547));
#392074=CARTESIAN_POINT('Ctrl Pts',(-1.304181653261,2.32523440228086,8.85555568965886));
#392075=CARTESIAN_POINT('Ctrl Pts',(-1.30400830047063,2.32581099027345,
8.85434650606346));
#392076=CARTESIAN_POINT('Ctrl Pts',(-1.30391934352441,2.32640503368348,
8.85297329937117));
#392077=CARTESIAN_POINT('Ctrl Pts',(-1.30386931066238,2.32673914690602,
8.85220095427747));
#392078=CARTESIAN_POINT('Ctrl Pts',(-1.30384626657237,2.32707896510008,
8.85137579139183));
#392079=CARTESIAN_POINT('Ctrl Pts',(-1.30385128920421,2.32742558187726,
8.85049129520029));
#392080=CARTESIAN_POINT('Origin',(-1.31072556753554,2.3273259705153,7.59394543036555));
#392081=CARTESIAN_POINT('Ctrl Pts',(-1.31389778130986,2.32120070918671,
7.59443877723642));
#392082=CARTESIAN_POINT('Ctrl Pts',(-1.3089898473347,2.31812737585884,7.58783886950016));
#392083=CARTESIAN_POINT('Ctrl Pts',(-1.30294132309853,2.32408510496489,
7.58559994247159));
#392084=CARTESIAN_POINT('Ctrl Pts',(-1.34069004888757,2.3379779456558,7.56670252222137));
#392085=CARTESIAN_POINT('Ctrl Pts',(-1.33578920827042,2.33490905416713,
7.5600487499903));
#392086=CARTESIAN_POINT('Ctrl Pts',(-1.32968985135374,2.34088686333599,
7.55786368756705));
#392087=CARTESIAN_POINT('Ctrl Pts',(-1.36743228458244,2.35472385231203,
7.53888913333557));
#392088=CARTESIAN_POINT('Ctrl Pts',(-1.36250231802953,2.35163672225097,
7.53222002137277));
#392089=CARTESIAN_POINT('Ctrl Pts',(-1.35638999749711,2.35765685368049,
7.53005029815326));
#392090=CARTESIAN_POINT('Ctrl Pts',(-1.39412327829024,2.3714376713918,7.51101258149734));
#392091=CARTESIAN_POINT('Ctrl Pts',(-1.38913355158474,2.36831311970495,
7.5043616886572));
#392092=CARTESIAN_POINT('Ctrl Pts',(-1.38304039838402,2.37439431741735,
7.50217374673251));
#392093=CARTESIAN_POINT('',(-1.38161829930508,2.37350118398176,7.50366116523517));
#392094=CARTESIAN_POINT('Ctrl Pts',(-1.38685191115371,2.3668843634066,7.51860402984325));
#392095=CARTESIAN_POINT('Ctrl Pts',(-1.38722619522759,2.36711873895529,
7.51734760759493));
#392096=CARTESIAN_POINT('Ctrl Pts',(-1.38753283777152,2.36738095682315,
7.51608817408572));
#392097=CARTESIAN_POINT('Ctrl Pts',(-1.3877624548676,2.3676805628512,7.51481005913119));
#392098=CARTESIAN_POINT('Ctrl Pts',(-1.3879704475201,2.36795195315073,7.51365231206383));
#392099=CARTESIAN_POINT('Ctrl Pts',(-1.38811573123277,2.36825425143916,
7.51247773061043));
#392100=CARTESIAN_POINT('Ctrl Pts',(-1.38816251106133,2.36859822163469,
7.51129758471022));
#392101=CARTESIAN_POINT('Ctrl Pts',(-1.38822065304577,2.36902573730485,
7.50983079813402));
#392102=CARTESIAN_POINT('Ctrl Pts',(-1.38811186827432,2.36950573745492,
7.50839324291155));
#392103=CARTESIAN_POINT('Ctrl Pts',(-1.38775496216549,2.37002350371512,
7.50715379678855));
#392104=CARTESIAN_POINT('Ctrl Pts',(-1.38759008182721,2.37026269680826,
7.50658120839351));
#392105=CARTESIAN_POINT('Ctrl Pts',(-1.38734098568148,2.37053856065069,
7.50598221009429));
#392106=CARTESIAN_POINT('Ctrl Pts',(-1.38699671946607,2.37082928581175,
7.50545747549611));
#392107=CARTESIAN_POINT('Ctrl Pts',(-1.38681300835749,2.37098442575647,
7.50517746087247));
#392108=CARTESIAN_POINT('Ctrl Pts',(-1.38660033499762,2.37114563462441,
7.50491486231392));
#392109=CARTESIAN_POINT('Ctrl Pts',(-1.38636332372289,2.37130731404934,
7.50468370960992));
#392110=CARTESIAN_POINT('Ctrl Pts',(-1.38600891710619,2.3715490757885,7.50433806340446));
#392111=CARTESIAN_POINT('Ctrl Pts',(-1.38558915067018,2.37179867932595,
7.50405484070983));
#392112=CARTESIAN_POINT('Ctrl Pts',(-1.3851319287582,2.37203869856845,7.50385766036131));
#392113=CARTESIAN_POINT('Ctrl Pts',(-1.38508303598155,2.37206436489569,
7.50383657498791));
#392114=CARTESIAN_POINT('Ctrl Pts',(-1.38503374322899,2.37208992304649,
7.50381643264937));
#392115=CARTESIAN_POINT('Ctrl Pts',(-1.38498410518475,2.37211535306456,
7.50379723213559));
#392116=CARTESIAN_POINT('Ctrl Pts',(-1.38465275500166,2.3722851067539,7.50366906242519));
#392117=CARTESIAN_POINT('Ctrl Pts',(-1.38429848313329,2.37245220342954,
7.50358235568538));
#392118=CARTESIAN_POINT('Ctrl Pts',(-1.38395313708759,2.37260505571625,
7.5035341175365));
#392119=CARTESIAN_POINT('Ctrl Pts',(-1.38343532977768,2.37283424042064,
7.50346178989176));
#392120=CARTESIAN_POINT('Ctrl Pts',(-1.38286854227573,2.37305877444105,
7.50346967198527));
#392121=CARTESIAN_POINT('Ctrl Pts',(-1.38230535013551,2.37326207654003,
7.50354272648693));
#392122=CARTESIAN_POINT('Ctrl Pts',(-1.38207369755085,2.37334569890144,
7.50357277531559));
#392123=CARTESIAN_POINT('Ctrl Pts',(-1.38184300918209,2.37342575141275,
7.50361331098761));
#392124=CARTESIAN_POINT('Ctrl Pts',(-1.3816182993058,2.37350118398298,7.50366116523659));
#392125=CARTESIAN_POINT('',(-1.31216235181343,2.32987712649127,7.57603338622103));
#392126=CARTESIAN_POINT('Origin',(-1.31649630659949,2.3375783163681,7.58486873427625));
#392127=CARTESIAN_POINT('Ctrl Pts',(-1.38161829935628,2.37350118400758,
7.50366116529968));
#392128=CARTESIAN_POINT('Ctrl Pts',(-1.35850365155688,2.35898426780923,
7.52783573079709));
#392129=CARTESIAN_POINT('Ctrl Pts',(-1.33535275265205,2.34444361706052,
7.55196141284069));
#392130=CARTESIAN_POINT('Ctrl Pts',(-1.31216235301862,2.32987712683062,
7.57603338728831));
#392131=CARTESIAN_POINT('Ctrl Pts',(-1.31515263304416,2.32219393616178,
7.5963967733137));
#392132=CARTESIAN_POINT('Ctrl Pts',(-1.30074331794104,2.30960147554731,
7.59974925422225));
#392133=CARTESIAN_POINT('Ctrl Pts',(-1.30404198763951,2.328451335077,7.59639677331373));
#392134=CARTESIAN_POINT('Ctrl Pts',(-1.31266628426872,2.31918841227222,
7.58707626057421));
#392135=CARTESIAN_POINT('Ctrl Pts',(-1.30579990181482,2.31857995225015,
7.58811717123965));
#392136=CARTESIAN_POINT('Ctrl Pts',(-1.30276074036386,2.32476711066714,
7.58707626057425));
#392137=CARTESIAN_POINT('Ctrl Pts',(-1.3120167178241,2.32523024110926,7.58015376756929));
#392138=CARTESIAN_POINT('Ctrl Pts',(-1.30919143812975,2.32460196840813,
7.58208760766041));
#392139=CARTESIAN_POINT('Ctrl Pts',(-1.30826409698651,2.32734367779125,
7.58015376756931));
#392140=CARTESIAN_POINT('Ctrl Pts',(-1.3121623514075,2.32987712577009,7.57603338509286));
#392141=CARTESIAN_POINT('Ctrl Pts',(-1.3121623514075,2.32987712577009,7.57603338509286));
#392142=CARTESIAN_POINT('Ctrl Pts',(-1.3121623514075,2.32987712577009,7.57603338509286));
#392143=CARTESIAN_POINT('Origin',(-1.31650127865107,2.33757551616096,7.5848687342762));
#392144=CARTESIAN_POINT('Ctrl Pts',(-1.30521500871194,2.42153721008159,
7.51098857897448));
#392145=CARTESIAN_POINT('Ctrl Pts',(-1.30512970780232,2.4156505101804,7.50433767179956));
#392146=CARTESIAN_POINT('Ctrl Pts',(-1.31348868127019,2.41359244952876,
7.50214974420965));
#392147=CARTESIAN_POINT('Ctrl Pts',(-1.30475858882228,2.39003922334998,
7.53887321589168));
#392148=CARTESIAN_POINT('Ctrl Pts',(-1.30467430996893,2.38422305656061,
7.53220407452061));
#392149=CARTESIAN_POINT('Ctrl Pts',(-1.31299098755427,2.38211692411853,
7.53003438070911));
#392150=CARTESIAN_POINT('Ctrl Pts',(-1.30430129243808,2.35848074886471,
7.56669465659231));
#392151=CARTESIAN_POINT('Ctrl Pts',(-1.30421751165707,2.35269895453971,
7.56004085833296));
#392152=CARTESIAN_POINT('Ctrl Pts',(-1.31249126537342,2.350581963853,7.55785582193789));
#392153=CARTESIAN_POINT('Ctrl Pts',(-1.303843140241,2.32686321388928,7.59443891967696));
#392154=CARTESIAN_POINT('Ctrl Pts',(-1.30375923798832,2.3210730366824,7.58783901202978));
#392155=CARTESIAN_POINT('Ctrl Pts',(-1.31198945670398,2.31898912740397,
7.58560008491213));
#392156=CARTESIAN_POINT('',(-1.31346170186504,2.41188626453887,7.50366116523517));
#392157=CARTESIAN_POINT('Ctrl Pts',(-1.31346170186522,2.4118862645392,7.50366116523554));
#392158=CARTESIAN_POINT('Ctrl Pts',(-1.31288301264089,2.41237540286156,
7.50350835821027));
#392159=CARTESIAN_POINT('Ctrl Pts',(-1.31233514318615,2.41280621264755,
7.50345484956));
#392160=CARTESIAN_POINT('Ctrl Pts',(-1.31180217608121,2.41319197426493,
7.50349758195598));
#392161=CARTESIAN_POINT('Ctrl Pts',(-1.31152872443051,2.41338989858347,
7.50351950684424));
#392162=CARTESIAN_POINT('Ctrl Pts',(-1.3112323191529,2.41359557726915,7.50357029184312));
#392163=CARTESIAN_POINT('Ctrl Pts',(-1.31094104715446,2.41378605423315,
7.50365515313924));
#392164=CARTESIAN_POINT('Ctrl Pts',(-1.31049295287318,2.41407908493551,
7.50378570417639));
#392165=CARTESIAN_POINT('Ctrl Pts',(-1.31004404409644,2.41434503002183,
7.50400001621911));
#392166=CARTESIAN_POINT('Ctrl Pts',(-1.30962733207942,2.41456169384711,
7.50428903009635));
#392167=CARTESIAN_POINT('Ctrl Pts',(-1.30958108025152,2.4145857418648,7.50432110841318));
#392168=CARTESIAN_POINT('Ctrl Pts',(-1.30953521085965,2.41460920955342,
7.50435406373354));
#392169=CARTESIAN_POINT('Ctrl Pts',(-1.30948975828795,2.4146320861886,7.50438785222352));
#392170=CARTESIAN_POINT('Ctrl Pts',(-1.3092122484904,2.41477175904228,7.50459414719561));
#392171=CARTESIAN_POINT('Ctrl Pts',(-1.30894562634665,2.41489116230398,
7.50483629897752));
#392172=CARTESIAN_POINT('Ctrl Pts',(-1.30870064396402,2.4149869227576,7.5050991045531));
#392173=CARTESIAN_POINT('Ctrl Pts',(-1.30816018822177,2.4151981799365,7.50567888004914));
#392174=CARTESIAN_POINT('Ctrl Pts',(-1.30770394295141,2.41530317974193,
7.50637912803144));
#392175=CARTESIAN_POINT('Ctrl Pts',(-1.30733073613184,2.41533280978828,
7.50710440483569));
#392176=CARTESIAN_POINT('Ctrl Pts',(-1.30723921841049,2.41534007566389,
7.50728225710685));
#392177=CARTESIAN_POINT('Ctrl Pts',(-1.30715088373329,2.41534309947924,
7.50746498566954));
#392178=CARTESIAN_POINT('Ctrl Pts',(-1.3070678083697,2.41534222699803,7.50764697238949));
#392179=CARTESIAN_POINT('Ctrl Pts',(-1.30662121807801,2.41533753677913,
7.50862528291182));
#392180=CARTESIAN_POINT('Ctrl Pts',(-1.30628602974968,2.41522396277348,
7.50965856837421));
#392181=CARTESIAN_POINT('Ctrl Pts',(-1.30602487717232,2.41505626958658,
7.51067959873201));
#392182=CARTESIAN_POINT('Ctrl Pts',(-1.3058811645796,2.4149639878143,7.51124147302578));
#392183=CARTESIAN_POINT('Ctrl Pts',(-1.30576007199094,2.41485492899368,
7.51180065547253));
#392184=CARTESIAN_POINT('Ctrl Pts',(-1.3056569223431,2.4147359892537,7.51235175716501));
#392185=CARTESIAN_POINT('Ctrl Pts',(-1.30530049921988,2.41432500507208,
7.51425603304536));
#392186=CARTESIAN_POINT('Ctrl Pts',(-1.30512039563903,2.41374306939881,
7.5162690050518));
#392187=CARTESIAN_POINT('Ctrl Pts',(-1.30509334076502,2.41304587007464,
7.51827788969243));
#392188=CARTESIAN_POINT('Ctrl Pts',(-1.30509187650411,2.41300813632969,
7.51838661432545));
#392189=CARTESIAN_POINT('Ctrl Pts',(-1.30509086684246,2.41297005723369,
7.51849533314856));
#392190=CARTESIAN_POINT('Ctrl Pts',(-1.30509031014834,2.4129316392236,7.51860402984325));
#392191=CARTESIAN_POINT('Ctrl Pts',(-1.31216235147924,2.32987712769896,
7.57603338728985));
#392192=CARTESIAN_POINT('Ctrl Pts',(-1.31259704935576,2.35725939040438,
7.55196141284922));
#392193=CARTESIAN_POINT('Ctrl Pts',(-1.31303012767146,2.38459447936899,
7.52783573083105));
#392194=CARTESIAN_POINT('Ctrl Pts',(-1.31346170186054,2.41188626459788,
7.50366116530176));
#392195=CARTESIAN_POINT('Origin',(-4.53412748053612E-16,8.05080247188564E-16,
7.49482233047033));
#392196=CARTESIAN_POINT('Origin',(-1.37717168998615,2.36586229233671,7.49482233047033));
#392197=CARTESIAN_POINT('Origin',(0.,0.,7.50366116523517));
#392198=CARTESIAN_POINT('Origin',(-1.30923444818252,2.40412383410095,7.49482233047033));
#392199=CARTESIAN_POINT('Ctrl Pts',(-1.38685101471506,2.36688380200664,
7.51860402984325));
#392200=CARTESIAN_POINT('Ctrl Pts',(-1.39329958728443,2.37092263820629,
7.51860402984325));
#392201=CARTESIAN_POINT('Ctrl Pts',(-1.39984896414483,2.36704940328305,
7.51860402984325));
#392202=CARTESIAN_POINT('Ctrl Pts',(-1.38924541439192,2.36838344837309,
7.51041458714366));
#392203=CARTESIAN_POINT('Ctrl Pts',(-1.39485120463889,2.37000501596871,
7.51004642900442));
#392204=CARTESIAN_POINT('Ctrl Pts',(-1.39985077038519,2.36704833509086,
7.50729136483009));
#392205=CARTESIAN_POINT('Ctrl Pts',(-1.38866594195955,2.37113807155955,
7.50215815450138));
#392206=CARTESIAN_POINT('Ctrl Pts',(-1.3916920283461,2.37187350725536,7.4987716367153));
#392207=CARTESIAN_POINT('Ctrl Pts',(-1.39467384947402,2.37013780383729,
7.49481588533171));
#392208=CARTESIAN_POINT('Ctrl Pts',(-1.38161802235204,2.37350070820124,
7.50366171572174));
#392209=CARTESIAN_POINT('Ctrl Pts',(-1.38346014519123,2.37666531650283,
7.50000045605858));
#392210=CARTESIAN_POINT('Ctrl Pts',(-1.38346014519134,2.37666531650276,
7.49482233047317));
#392211=CARTESIAN_POINT('Origin',(-1.39348601430781,2.35629008781359,7.51860402984325));
#392212=CARTESIAN_POINT('Origin',(-1.39348601430781,2.35629008781359,9.));
#392213=CARTESIAN_POINT('Origin',(-1.39348601430781,2.35629008781359,8.75721825406948));
#392214=CARTESIAN_POINT('Ctrl Pts',(-1.37269783844895,2.35802109048349,
8.78942910404912));
#392215=CARTESIAN_POINT('Ctrl Pts',(-1.3774099853103,2.36099566619421,8.7967269950169));
#392216=CARTESIAN_POINT('Ctrl Pts',(-1.38347973220099,2.35445107616389,
8.79893251111267));
#392217=CARTESIAN_POINT('Ctrl Pts',(-1.38201599788306,2.36385609892403,
8.78111911759582));
#392218=CARTESIAN_POINT('Ctrl Pts',(-1.38760627609688,2.36737619830013,
8.78644465894816));
#392219=CARTESIAN_POINT('Ctrl Pts',(-1.39426522839041,2.36275301042509,
8.78817647674132));
#392220=CARTESIAN_POINT('Ctrl Pts',(-1.38782329711835,2.36749261533528,
8.7678092393203));
#392221=CARTESIAN_POINT('Ctrl Pts',(-1.39442509977365,2.37164363189404,
8.76988516158372));
#392222=CARTESIAN_POINT('Ctrl Pts',(-1.40100847884784,2.36792940245016,
8.77093053738833));
#392223=CARTESIAN_POINT('Ctrl Pts',(-1.38669095324687,2.36678354440285,
8.75371302330492));
#392224=CARTESIAN_POINT('Ctrl Pts',(-1.39313032119297,2.37083332733808,
8.7530082828756));
#392225=CARTESIAN_POINT('Ctrl Pts',(-1.39969354974842,2.36691943282452,
8.75267964240738));
#392226=CARTESIAN_POINT('Origin',(-1.38160128718528,2.34884790783659,8.78727029226991));
#392227=CARTESIAN_POINT('Ctrl Pts',(-1.31437432427029,2.32149911893914,
8.85049129520029));
#392228=CARTESIAN_POINT('Ctrl Pts',(-1.3193236441677,2.32459836800565,8.85711686593484));
#392229=CARTESIAN_POINT('Ctrl Pts',(-1.32539494747703,2.31857839805224,
8.85933012996512));
#392230=CARTESIAN_POINT('Ctrl Pts',(-1.33460133053253,2.33416520874058,
8.82945683644722));
#392231=CARTESIAN_POINT('Ctrl Pts',(-1.3395917327775,2.33729018344818,8.83607469902389));
#392232=CARTESIAN_POINT('Ctrl Pts',(-1.34565445587688,2.33122590846117,
8.8382956714852));
#392233=CARTESIAN_POINT('Ctrl Pts',(-1.35479818681084,2.34681241871377,
8.80838214965003));
#392234=CARTESIAN_POINT('Ctrl Pts',(-1.35980828351306,2.34994972603063,
8.81501364461995));
#392235=CARTESIAN_POINT('Ctrl Pts',(-1.36588287762334,2.34385480035509,
8.8172209842872));
#392236=CARTESIAN_POINT('Ctrl Pts',(-1.37496718403118,2.3594421834296,8.78727029226991));
#392237=CARTESIAN_POINT('Ctrl Pts',(-1.3799781129269,2.36258001186348,8.79393457792714));
#392238=CARTESIAN_POINT('Ctrl Pts',(-1.38608257609908,2.35646650676756,
8.79610912703474));
#392239=CARTESIAN_POINT('Origin',(-1.32100842742439,2.31090484334612,8.85049129520029));
#392240=CARTESIAN_POINT('Ctrl Pts',(-1.30385128920421,2.32742558187726,
8.85049129520029));
#392241=CARTESIAN_POINT('Ctrl Pts',(-1.30393589896118,2.33326458465275,
8.85711686593484));
#392242=CARTESIAN_POINT('Ctrl Pts',(-1.2956406467065,2.33533570805444,8.85933012996512));
#392243=CARTESIAN_POINT('Ctrl Pts',(-1.30377643617357,2.32225990040869,
8.86332496987232));
#392244=CARTESIAN_POINT('Ctrl Pts',(-1.29989627515222,2.32476913232806,
8.86648636486737));
#392245=CARTESIAN_POINT('Ctrl Pts',(-1.29544837314913,2.32088425528194,
8.87206031107457));
#392246=CARTESIAN_POINT('Ctrl Pts',(-1.30996597848912,2.31873862621885,
8.86341338519876));
#392247=CARTESIAN_POINT('Ctrl Pts',(-1.31412198473722,2.3166889719309,8.86654584966058));
#392248=CARTESIAN_POINT('Ctrl Pts',(-1.31304352587505,2.31086135841679,
8.87215952290714));
#392249=CARTESIAN_POINT('Ctrl Pts',(-1.31437432427029,2.32149911893914,
8.85049129520029));
#392250=CARTESIAN_POINT('Ctrl Pts',(-1.3193236441677,2.32459836800565,8.85711686593484));
#392251=CARTESIAN_POINT('Ctrl Pts',(-1.32539494747703,2.31857839805224,
8.85933012996512));
#392252=CARTESIAN_POINT('Origin',(-1.29135260132907,2.32760669344447,8.85049129520029));
#392253=CARTESIAN_POINT('Ctrl Pts',(-1.30488713801675,2.39891053004237,
8.78727029226991));
#392254=CARTESIAN_POINT('Ctrl Pts',(-1.30497280099365,2.40482221656423,
8.79393457792714));
#392255=CARTESIAN_POINT('Ctrl Pts',(-1.29658037301231,2.4068732084599,8.79610912703474));
#392256=CARTESIAN_POINT('Ctrl Pts',(-1.30454234439085,2.37511598186411,
8.80838214965002));
#392257=CARTESIAN_POINT('Ctrl Pts',(-1.30462799314121,2.3810266865985,8.81501364461988));
#392258=CARTESIAN_POINT('Ctrl Pts',(-1.29626693711645,2.38306176761554,
8.81722098428721));
#392259=CARTESIAN_POINT('Ctrl Pts',(-1.30419707450797,2.35128856672231,
8.82945683644724));
#392260=CARTESIAN_POINT('Ctrl Pts',(-1.30428238657708,2.35717603675116,
8.83607469902391));
#392261=CARTESIAN_POINT('Ctrl Pts',(-1.29595369511063,2.35921685544824,
8.8382956714852));
#392262=CARTESIAN_POINT('Ctrl Pts',(-1.30385128920421,2.32742558187726,
8.85049129520029));
#392263=CARTESIAN_POINT('Ctrl Pts',(-1.30393589896118,2.33326458465275,
8.85711686593484));
#392264=CARTESIAN_POINT('Ctrl Pts',(-1.2956406467065,2.33533570805444,8.85933012996512));
#392265=CARTESIAN_POINT('Origin',(-1.29238845014161,2.39909164160957,8.78727029226991));
#392266=CARTESIAN_POINT('Ctrl Pts',(-1.30508760891742,2.41274649779732,
8.75374538247848));
#392267=CARTESIAN_POINT('Ctrl Pts',(-1.30521083091158,2.42034447086438,
8.75304829418602));
#392268=CARTESIAN_POINT('Ctrl Pts',(-1.29847137974321,2.42392922206331,
8.75272238421917));
#392269=CARTESIAN_POINT('Ctrl Pts',(-1.30510673448897,2.41406634291194,
8.76769408445022));
#392270=CARTESIAN_POINT('Ctrl Pts',(-1.30523236727891,2.42185552588414,
8.76974318093968));
#392271=CARTESIAN_POINT('Ctrl Pts',(-1.29865181653908,2.4255588634654,8.7707786988043));
#392272=CARTESIAN_POINT('Ctrl Pts',(-1.3050087077191,2.40730156872033,8.78108014887988));
#392273=CARTESIAN_POINT('Ctrl Pts',(-1.30511897588473,2.41390255942112,
8.78639403366326));
#392274=CARTESIAN_POINT('Ctrl Pts',(-1.29773252047993,2.41721350373984,
8.78812224174741));
#392275=CARTESIAN_POINT('Ctrl Pts',(-1.30484806344775,2.39621559715997,
8.78944554828686));
#392276=CARTESIAN_POINT('Ctrl Pts',(-1.3049465903167,2.40177857388769,8.79673892988685));
#392277=CARTESIAN_POINT('Ctrl Pts',(-1.29621337213037,2.40357703279092,
8.79894799272499));
#392278=CARTESIAN_POINT('Origin',(-1.2925916222732,2.4131127507908,8.75721825406948));
#392279=CARTESIAN_POINT('Origin',(-1.2925916222732,2.4131127507908,9.));
#392280=CARTESIAN_POINT('Origin',(-1.2925916222732,2.4131127507908,7.51860402984325));
#392281=CARTESIAN_POINT('Ctrl Pts',(-1.31346132563585,2.41188557367603,
7.50366195182966));
#392282=CARTESIAN_POINT('Ctrl Pts',(-1.31521268767181,2.4151015685033,7.50000065167735));
#392283=CARTESIAN_POINT('Ctrl Pts',(-1.31521268767171,2.41510156850336,
7.49482233047108));
#392284=CARTESIAN_POINT('Ctrl Pts',(-1.3077817098543,2.41669137893433,7.50215800491337));
#392285=CARTESIAN_POINT('Ctrl Pts',(-1.30684029925185,2.41966096531158,
7.49877273257266));
#392286=CARTESIAN_POINT('Ctrl Pts',(-1.30380859101919,2.4213119957601,7.49481816995647));
#392287=CARTESIAN_POINT('Ctrl Pts',(-1.30513148750344,2.41574992376647,
7.51043025814042));
#392288=CARTESIAN_POINT('Ctrl Pts',(-1.30361489455134,2.42138842558916,
7.51006209594515));
#392289=CARTESIAN_POINT('Ctrl Pts',(-1.29849163527805,2.42413272597013,
7.50731281821701));
#392290=CARTESIAN_POINT('Ctrl Pts',(-1.30509028815831,2.41293012797613,
7.51860402984326));
#392291=CARTESIAN_POINT('Ctrl Pts',(-1.30520145828907,2.42053858764893,
7.51860402984327));
#392292=CARTESIAN_POINT('Ctrl Pts',(-1.29849386712376,2.42413153047478,
7.51860402984327));
#392293=CARTESIAN_POINT('Origin',(0.,0.,7.5));
#392294=CARTESIAN_POINT('Origin',(-1.45029105591254,2.23910559748223,7.5));
#392295=CARTESIAN_POINT('',(-1.45029105591254,2.23910559748223,7.59394543036555));
#392296=CARTESIAN_POINT('',(-1.45029105591254,2.23910559748223,8.85049129520029));
#392297=CARTESIAN_POINT('',(-1.45029105591254,2.23910559748223,7.5));
#392298=CARTESIAN_POINT('',(-1.45590483281685,2.31037730509331,8.78727029226991));
#392299=CARTESIAN_POINT('Ctrl Pts',(-1.45029105591254,2.23910559748223,
8.85049129520029));
#392300=CARTESIAN_POINT('Ctrl Pts',(-1.45216503493678,2.26289736679569,
8.82945686509571));
#392301=CARTESIAN_POINT('Ctrl Pts',(-1.45403622806459,2.28665376676721,
8.80838212259896));
#392302=CARTESIAN_POINT('Ctrl Pts',(-1.45590483281685,2.31037730509331,
8.78727029226991));
#392303=CARTESIAN_POINT('',(-1.45700592305913,2.3243565891188,8.75721825406948));
#392304=CARTESIAN_POINT('Origin',(-1.45369256172855,2.28228805819249,8.75937679713117));
#392305=CARTESIAN_POINT('',(-1.45700592305913,2.3243565891188,7.51860402984325));
#392306=CARTESIAN_POINT('',(-1.45700592305913,2.3243565891188,7.5));
#392307=CARTESIAN_POINT('Ctrl Pts',(-1.45700592305913,2.3243565891188,7.51860402984325));
#392308=CARTESIAN_POINT('Ctrl Pts',(-1.45614118792574,2.31337803570669,
7.52834476460825));
#392309=CARTESIAN_POINT('Ctrl Pts',(-1.4552758914188,2.30239235517613,7.53807742314407));
#392310=CARTESIAN_POINT('Ctrl Pts',(-1.45441001468941,2.29139930822463,
7.54780169004674));
#392311=CARTESIAN_POINT('Ctrl Pts',(-1.45303851274671,2.27398691597694,
7.5632044032688));
#392312=CARTESIAN_POINT('Ctrl Pts',(-1.45166555335681,2.25655602018873,
7.57858609112103));
#392313=CARTESIAN_POINT('Ctrl Pts',(-1.45029105591254,2.23910559748223,
7.59394543036555));
#392314=CARTESIAN_POINT('Origin',(-1.70235901374313,2.36323439034369,7.5));
#392315=CARTESIAN_POINT('',(-1.53564927699521,2.27316543860614,8.75721825406948));
#392316=CARTESIAN_POINT('',(-1.52331214621093,2.26650000646723,8.78727029226991));
#392317=CARTESIAN_POINT('Origin',(-1.49199590676139,2.24958065361715,8.75658640621095));
#392318=CARTESIAN_POINT('',(-1.46041276049034,2.23251709792628,8.85049129520029));
#392319=CARTESIAN_POINT('Ctrl Pts',(-1.52331214621093,2.26650000646723,
8.78727029226991));
#392320=CARTESIAN_POINT('Ctrl Pts',(-1.50237542338154,2.25518843754,8.80838212259896));
#392321=CARTESIAN_POINT('Ctrl Pts',(-1.48140969918007,2.24386119992281,
8.82945686509571));
#392322=CARTESIAN_POINT('Ctrl Pts',(-1.46041276049034,2.23251709792628,
8.85049129520029));
#392323=CARTESIAN_POINT('',(-1.46041276049034,2.23251709792628,7.59394543036555));
#392324=CARTESIAN_POINT('',(-1.46041276049034,2.23251709792628,7.5));
#392325=CARTESIAN_POINT('',(-1.53564927699521,2.27316543860614,7.51860402984325));
#392326=CARTESIAN_POINT('Ctrl Pts',(-1.46041276049034,2.23251709792628,
7.59394543036555));
#392327=CARTESIAN_POINT('Ctrl Pts',(-1.47581327361951,2.24083759618166,
7.57858609112103));
#392328=CARTESIAN_POINT('Ctrl Pts',(-1.49119655366672,2.24914878384933,
7.56320440326857));
#392329=CARTESIAN_POINT('Ctrl Pts',(-1.50656350379345,2.25745114888401,
7.54780169004651));
#392330=CARTESIAN_POINT('Ctrl Pts',(-1.51626519221406,2.26269271979147,
7.53807742314383));
#392331=CARTESIAN_POINT('Ctrl Pts',(-1.52596037955093,2.26793077833181,
7.52834476460825));
#392332=CARTESIAN_POINT('Ctrl Pts',(-1.53564927699521,2.27316543860614,
7.51860402984325));
#392333=CARTESIAN_POINT('',(-1.53564927699521,2.27316543860614,7.5));
#392334=CARTESIAN_POINT('Origin',(-1.4571448281799,2.2385657542576,7.5));
#392335=CARTESIAN_POINT('Ctrl Pts',(-1.46041276049034,2.23251709792628,
8.85049129520029));
#392336=CARTESIAN_POINT('Ctrl Pts',(-1.46024237621486,2.23242504371647,
8.85097269580138));
#392337=CARTESIAN_POINT('Ctrl Pts',(-1.46007014340848,2.2323415513399,8.85143669361005));
#392338=CARTESIAN_POINT('Ctrl Pts',(-1.45988774993289,2.23226356296288,
8.8519052845931));
#392339=CARTESIAN_POINT('Ctrl Pts',(-1.45953099986159,2.23211102264327,
8.85282181883899));
#392340=CARTESIAN_POINT('Ctrl Pts',(-1.4591444780731,2.23198364392552,8.85372622499635));
#392341=CARTESIAN_POINT('Ctrl Pts',(-1.45871729341942,2.23189407204953,
8.8546225773507));
#392342=CARTESIAN_POINT('Ctrl Pts',(-1.4583626598921,2.23181971265937,8.85536669723986));
#392343=CARTESIAN_POINT('Ctrl Pts',(-1.45797992823562,2.2317713608387,8.85610498449051));
#392344=CARTESIAN_POINT('Ctrl Pts',(-1.45756183174182,2.23176418670402,
8.85681338218371));
#392345=CARTESIAN_POINT('Ctrl Pts',(-1.45718240851707,2.23175767616552,
8.85745625420285));
#392346=CARTESIAN_POINT('Ctrl Pts',(-1.45676911105285,2.2317843978143,8.85808743050666));
#392347=CARTESIAN_POINT('Ctrl Pts',(-1.45631128381982,2.23187089041148,
8.85866804508411));
#392348=CARTESIAN_POINT('Ctrl Pts',(-1.45610005225898,2.23191079622088,
8.85893592806396));
#392349=CARTESIAN_POINT('Ctrl Pts',(-1.4558792788259,2.23196365955264,8.85919241173849));
#392350=CARTESIAN_POINT('Ctrl Pts',(-1.45564772260897,2.23203367112446,
8.85943017985534));
#392351=CARTESIAN_POINT('Ctrl Pts',(-1.45533505316813,2.23212820747206,
8.8597512372));
#392352=CARTESIAN_POINT('Ctrl Pts',(-1.45499495061645,2.23225702953025,
8.86004599534705));
#392353=CARTESIAN_POINT('Ctrl Pts',(-1.45463519034912,2.23242832936726,
8.86026130871721));
#392354=CARTESIAN_POINT('Ctrl Pts',(-1.45450347197253,2.23249104706704,
8.86034014101235));
#392355=CARTESIAN_POINT('Ctrl Pts',(-1.45436713462983,2.23256038986721,
8.86040910639692));
#392356=CARTESIAN_POINT('Ctrl Pts',(-1.45423004525064,2.23263476838842,
8.86046313645506));
#392357=CARTESIAN_POINT('Ctrl Pts',(-1.45401611842252,2.23275083544785,
8.86054744990829));
#392358=CARTESIAN_POINT('Ctrl Pts',(-1.45379459084791,2.23288246268807,
8.86059655985668));
#392359=CARTESIAN_POINT('Ctrl Pts',(-1.45357952011842,2.23302095660015,
8.86059725258816));
#392360=CARTESIAN_POINT('Ctrl Pts',(-1.45336395248962,2.2331597704885,8.86059794692011));
#392361=CARTESIAN_POINT('Ctrl Pts',(-1.45315391929664,2.23330925598726,
8.86056369958366));
#392362=CARTESIAN_POINT('Ctrl Pts',(-1.45295869380043,2.23345819421407,
8.86048590497774));
#392363=CARTESIAN_POINT('Ctrl Pts',(-1.45290774575849,2.23349706265685,
8.86046560290182));
#392364=CARTESIAN_POINT('Ctrl Pts',(-1.45285719833681,2.23353647149836,
8.86044257503091));
#392365=CARTESIAN_POINT('Ctrl Pts',(-1.45280859330923,2.23357517708475,
8.86041778462584));
#392366=CARTESIAN_POINT('Ctrl Pts',(-1.45248154178737,2.23383561765153,
8.86025097596201));
#392367=CARTESIAN_POINT('Ctrl Pts',(-1.45219875525292,2.23409942479349,
8.8599848982295));
#392368=CARTESIAN_POINT('Ctrl Pts',(-1.45196270805473,2.23435270342851,
8.85968173251461));
#392369=CARTESIAN_POINT('Ctrl Pts',(-1.45183785261078,2.2344866733153,8.85952137522076));
#392370=CARTESIAN_POINT('Ctrl Pts',(-1.45172352753971,2.23462014970573,
8.85934740853961));
#392371=CARTESIAN_POINT('Ctrl Pts',(-1.4516201644098,2.23475023902308,8.8591675900182));
#392372=CARTESIAN_POINT('Ctrl Pts',(-1.45120510771614,2.23527261525129,
8.85844552518695));
#392373=CARTESIAN_POINT('Ctrl Pts',(-1.45094097857851,2.23576801806972,
8.85759444184124));
#392374=CARTESIAN_POINT('Ctrl Pts',(-1.45076190271768,2.23619128641436,
8.85683498915138));
#392375=CARTESIAN_POINT('Ctrl Pts',(-1.45074316290576,2.23623558031937,
8.85675551444998));
#392376=CARTESIAN_POINT('Ctrl Pts',(-1.45072537407566,2.23627908830464,
8.85667699793651));
#392377=CARTESIAN_POINT('Ctrl Pts',(-1.45070847371898,2.23632176059871,
8.85659965593547));
#392378=CARTESIAN_POINT('Ctrl Pts',(-1.45048035184219,2.23689775340153,
8.85555568965886));
#392379=CARTESIAN_POINT('Ctrl Pts',(-1.45034429734325,2.23748426348366,
8.85434650606346));
#392380=CARTESIAN_POINT('Ctrl Pts',(-1.45029358366056,2.2380827858589,8.85297329937117));
#392381=CARTESIAN_POINT('Ctrl Pts',(-1.45026506030408,2.23841941822647,
8.85220095427747));
#392382=CARTESIAN_POINT('Ctrl Pts',(-1.45026383578707,2.23876001466752,
8.85137579139183));
#392383=CARTESIAN_POINT('Ctrl Pts',(-1.45029105591254,2.23910559748223,
8.85049129520029));
#392384=CARTESIAN_POINT('Origin',(-1.4571448281799,2.2385657542576,7.59394543036555));
#392385=CARTESIAN_POINT('Ctrl Pts',(-1.45991807746004,2.232249833501,7.59443877723642));
#392386=CARTESIAN_POINT('Ctrl Pts',(-1.45482331821922,2.2294972670755,7.58783886950016));
#392387=CARTESIAN_POINT('Ctrl Pts',(-1.4491689343392,2.23583028566651,7.58559994247159));
#392388=CARTESIAN_POINT('Ctrl Pts',(-1.48773021868178,2.24727601286091,
7.56670252222133));
#392389=CARTESIAN_POINT('Ctrl Pts',(-1.4826428228145,2.24452742467542,7.56004874999029));
#392390=CARTESIAN_POINT('Ctrl Pts',(-1.47693899722921,2.25088373893362,
7.55786368756703));
#392391=CARTESIAN_POINT('Ctrl Pts',(-1.51549042350858,2.26227413233218,
7.53888913333558));
#392392=CARTESIAN_POINT('Ctrl Pts',(-1.51037279299855,2.25950920915248,
7.53222002137275));
#392393=CARTESIAN_POINT('Ctrl Pts',(-1.5046587420292,2.26590858929744,7.53005029815326));
#392394=CARTESIAN_POINT('Ctrl Pts',(-1.54319743577236,2.27724351323975,
7.51101258149734));
#392395=CARTESIAN_POINT('Ctrl Pts',(-1.5380177702816,2.27444507416711,7.5043616886572));
#392396=CARTESIAN_POINT('Ctrl Pts',(-1.53232675979281,2.28090416707255,
7.50217374673251));
#392397=CARTESIAN_POINT('',(-1.53085035931326,2.28010398287621,7.50366116523517));
#392398=CARTESIAN_POINT('Ctrl Pts',(-1.53564927699521,2.27316543860614,
7.51860402984325));
#392399=CARTESIAN_POINT('Ctrl Pts',(-1.53603780855528,2.27337535214218,
7.51734760759494));
#392400=CARTESIAN_POINT('Ctrl Pts',(-1.5363606214257,2.27361738460006,7.51608817408573));
#392401=CARTESIAN_POINT('Ctrl Pts',(-1.53660896257295,2.27390166343754,
7.5148100591312));
#392402=CARTESIAN_POINT('Ctrl Pts',(-1.53683391591844,2.27415917000159,
7.51365231206384));
#392403=CARTESIAN_POINT('Ctrl Pts',(-1.53699826944798,2.27445153882633,
7.51247773061042));
#392404=CARTESIAN_POINT('Ctrl Pts',(-1.53706699140845,2.2747918051043,7.51129758471022));
#392405=CARTESIAN_POINT('Ctrl Pts',(-1.53715240495698,2.27521471722793,
7.50983079813402));
#392406=CARTESIAN_POINT('Ctrl Pts',(-1.53707459741071,2.27570070103045,
7.50839324291155));
#392407=CARTESIAN_POINT('Ctrl Pts',(-1.53675159800195,2.27624027053725,
7.50715379678855));
#392408=CARTESIAN_POINT('Ctrl Pts',(-1.53660238158211,2.27648953610207,
7.50658120839351));
#392409=CARTESIAN_POINT('Ctrl Pts',(-1.5363714718882,2.2767807927975,7.50598221009429));
#392410=CARTESIAN_POINT('Ctrl Pts',(-1.53604653982967,2.27709297784468,
7.50545747549611));
#392411=CARTESIAN_POINT('Ctrl Pts',(-1.53587314602565,2.27725956944889,
7.50517746087247));
#392412=CARTESIAN_POINT('Ctrl Pts',(-1.53567123831364,2.27743407312487,
7.50491486231392));
#392413=CARTESIAN_POINT('Ctrl Pts',(-1.53544507284031,2.2776106057266,7.50468370960993));
#392414=CARTESIAN_POINT('Ctrl Pts',(-1.53510688411783,2.27787457765022,
7.50433806340447));
#392415=CARTESIAN_POINT('Ctrl Pts',(-1.53470397229055,2.27815056287832,
7.50405484070984));
#392416=CARTESIAN_POINT('Ctrl Pts',(-1.5342630678757,2.27841938328403,7.50385766036132));
#392417=CARTESIAN_POINT('Ctrl Pts',(-1.53421592000173,2.27844812944801,
7.50383657498791));
#392418=CARTESIAN_POINT('Ctrl Pts',(-1.53416836604275,2.27847679328435,
7.50381643264937));
#392419=CARTESIAN_POINT('Ctrl Pts',(-1.53412045929204,2.27850535137414,
7.50379723213559));
#392420=CARTESIAN_POINT('Ctrl Pts',(-1.53380066605966,2.27869598596543,
7.50366906242519));
#392421=CARTESIAN_POINT('Ctrl Pts',(-1.5334578280016,2.27888543759958,7.50358235568538));
#392422=CARTESIAN_POINT('Ctrl Pts',(-1.53312298478602,2.27906010223199,
7.5035341175365));
#392423=CARTESIAN_POINT('Ctrl Pts',(-1.5326209252812,2.27932199208007,7.50346178989176));
#392424=CARTESIAN_POINT('Ctrl Pts',(-1.53206968824904,2.27958237897119,
7.50346967198527));
#392425=CARTESIAN_POINT('Ctrl Pts',(-1.53152067885768,2.27982134720852,
7.50354272648692));
#392426=CARTESIAN_POINT('Ctrl Pts',(-1.53129485993119,2.27991963979088,
7.50357277531559));
#392427=CARTESIAN_POINT('Ctrl Pts',(-1.53106977451843,2.28001430808025,
7.50361331098761));
#392428=CARTESIAN_POINT('Ctrl Pts',(-1.53085035931405,2.28010398287738,
7.50366116523658));
#392429=CARTESIAN_POINT('',(-1.45874211355498,2.24101961352526,7.57603338622103));
#392430=CARTESIAN_POINT('Origin',(-1.46356058069551,2.2484273030446,7.58486873427627));
#392431=CARTESIAN_POINT('Ctrl Pts',(-1.53085035936601,2.2801039828987,7.50366116529969));
#392432=CARTESIAN_POINT('Ctrl Pts',(-1.50685310107526,2.26709785383092,
7.52783573079709));
#392433=CARTESIAN_POINT('Ctrl Pts',(-1.482818145483,2.25407036159425,7.55196141284068));
#392434=CARTESIAN_POINT('Ctrl Pts',(-1.45874211477943,2.24101961378671,
7.57603338728831));
#392435=CARTESIAN_POINT('Ctrl Pts',(-1.46123398723767,2.23316062115807,
7.5963967733137));
#392436=CARTESIAN_POINT('Ctrl Pts',(-1.44604747589618,2.22151724109288,
7.59974925422225));
#392437=CARTESIAN_POINT('Ctrl Pts',(-1.4505470827706,2.2401170250713,7.59639677331373));
#392438=CARTESIAN_POINT('Ctrl Pts',(-1.45856018235568,2.23032057335267,
7.5870762605742));
#392439=CARTESIAN_POINT('Ctrl Pts',(-1.45166892345349,2.23015329411126,
7.58811717123965));
#392440=CARTESIAN_POINT('Ctrl Pts',(-1.44903241888651,2.23652246009042,
7.58707626057426));
#392441=CARTESIAN_POINT('Ctrl Pts',(-1.45829905181766,2.23639160646937,
7.58015376756929));
#392442=CARTESIAN_POINT('Ctrl Pts',(-1.45543932339328,2.23594564091341,
7.58208760766041));
#392443=CARTESIAN_POINT('Ctrl Pts',(-1.45468954949516,2.23874113211161,
7.5801537675693));
#392444=CARTESIAN_POINT('Ctrl Pts',(-1.45874211310368,2.24101961283157,
7.57603338509286));
#392445=CARTESIAN_POINT('Ctrl Pts',(-1.45874211310368,2.24101961283157,
7.57603338509286));
#392446=CARTESIAN_POINT('Ctrl Pts',(-1.45874211310368,2.24101961283157,
7.57603338509286));
#392447=CARTESIAN_POINT('Origin',(-1.46356536312157,2.24842419003061,7.58486873427624));
#392448=CARTESIAN_POINT('Ctrl Pts',(-1.45768172623408,2.33293648944412,
7.51098857897448));
#392449=CARTESIAN_POINT('Ctrl Pts',(-1.4572194384267,2.32706734964727,7.50433767179956));
#392450=CARTESIAN_POINT('Ctrl Pts',(-1.4654293770884,2.32447795623306,7.50214974420965));
#392451=CARTESIAN_POINT('Ctrl Pts',(-1.4552081611692,2.30153246162716,7.53887321589171));
#392452=CARTESIAN_POINT('Ctrl Pts',(-1.45475141239016,2.29573364454093,
7.53220407452068));
#392453=CARTESIAN_POINT('Ctrl Pts',(-1.46291606210055,2.29309898801139,
7.53003438070911));
#392454=CARTESIAN_POINT('Ctrl Pts',(-1.45272984594693,2.27006812649225,
7.56669465659231));
#392455=CARTESIAN_POINT('Ctrl Pts',(-1.45227579646822,2.26430357933688,
7.56004085833297));
#392456=CARTESIAN_POINT('Ctrl Pts',(-1.46039691481123,2.2616608370139,7.55785582193789));
#392457=CARTESIAN_POINT('Ctrl Pts',(-1.45024689265155,2.23854490704546,
7.59443891967696));
#392458=CARTESIAN_POINT('Ctrl Pts',(-1.44979218485767,2.23277200201443,
7.58783901202978));
#392459=CARTESIAN_POINT('Ctrl Pts',(-1.45787197718041,2.23016506242752,
7.58560008491213));
#392460=CARTESIAN_POINT('',(-1.4652931374677,2.32277700535965,7.50366116523517));
#392461=CARTESIAN_POINT('Ctrl Pts',(-1.4652931374679,2.32277700535996,7.50366116523554));
#392462=CARTESIAN_POINT('Ctrl Pts',(-1.46474697642256,2.32330221544109,
7.50350835821027));
#392463=CARTESIAN_POINT('Ctrl Pts',(-1.46422783470213,2.32376724219866,
7.50345484956));
#392464=CARTESIAN_POINT('Ctrl Pts',(-1.46372067846696,2.32418635854707,
7.50349758195598));
#392465=CARTESIAN_POINT('Ctrl Pts',(-1.46346046970663,2.32440139631628,
7.50351950684424));
#392466=CARTESIAN_POINT('Ctrl Pts',(-1.46317785130408,2.32462564316439,
7.50357029184312));
#392467=CARTESIAN_POINT('Ctrl Pts',(-1.46289938165619,2.32483439063405,
7.50365515313924));
#392468=CARTESIAN_POINT('Ctrl Pts',(-1.46247098257424,2.32515552877258,
7.50378570417639));
#392469=CARTESIAN_POINT('Ctrl Pts',(-1.46204003528892,2.32544968913027,
7.50400001621911));
#392470=CARTESIAN_POINT('Ctrl Pts',(-1.46163806115037,2.32569260662708,
7.50428903009634));
#392471=CARTESIAN_POINT('Ctrl Pts',(-1.46159344511359,2.32571956860033,
7.50432110841318));
#392472=CARTESIAN_POINT('Ctrl Pts',(-1.46154917354528,2.3257459269341,7.50435406373354));
#392473=CARTESIAN_POINT('Ctrl Pts',(-1.46150528007181,2.32577166872305,
7.50438785222352));
#392474=CARTESIAN_POINT('Ctrl Pts',(-1.46123728931836,2.32592883471765,
7.50459414719562));
#392475=CARTESIAN_POINT('Ctrl Pts',(-1.46097886517165,2.32606507519194,
7.50483629897752));
#392476=CARTESIAN_POINT('Ctrl Pts',(-1.46074052152492,2.32617633497058,
7.5050991045531));
#392477=CARTESIAN_POINT('Ctrl Pts',(-1.46021471150088,2.32642178521725,
7.50567888004914));
#392478=CARTESIAN_POINT('Ctrl Pts',(-1.45976613099599,2.32655580102416,
7.50637912803145));
#392479=CARTESIAN_POINT('Ctrl Pts',(-1.45939558937345,2.32660928163543,
7.50710440483569));
#392480=CARTESIAN_POINT('Ctrl Pts',(-1.45930472521132,2.32662239614305,
7.50728225710685));
#392481=CARTESIAN_POINT('Ctrl Pts',(-1.45921676576371,2.32663107336785,
7.50746498566954));
#392482=CARTESIAN_POINT('Ctrl Pts',(-1.4591338051873,2.32663552533606,7.50764697238949));
#392483=CARTESIAN_POINT('Ctrl Pts',(-1.45868783195991,2.32665945789196,
7.50862528291181));
#392484=CARTESIAN_POINT('Ctrl Pts',(-1.45834605560041,2.32656759282621,
7.50965856837421));
#392485=CARTESIAN_POINT('Ctrl Pts',(-1.45807469544966,2.32641697628602,
7.51067959873202));
#392486=CARTESIAN_POINT('Ctrl Pts',(-1.45792536561643,2.32633409181398,
7.51124147302578));
#392487=CARTESIAN_POINT('Ctrl Pts',(-1.45779753440284,2.32623301549519,
7.51180065547253));
#392488=CARTESIAN_POINT('Ctrl Pts',(-1.45768697619171,2.32612092895029,
7.51235175716501));
#392489=CARTESIAN_POINT('Ctrl Pts',(-1.4573049535311,2.32573362528766,7.51425603304537));
#392490=CARTESIAN_POINT('Ctrl Pts',(-1.45708793524577,2.32516442453968,
7.51626900505183));
#392491=CARTESIAN_POINT('Ctrl Pts',(-1.45701626624483,2.32447039109802,
7.51827788969247));
#392492=CARTESIAN_POINT('Ctrl Pts',(-1.45701238738306,2.32443282869662,
7.51838661432547));
#392493=CARTESIAN_POINT('Ctrl Pts',(-1.45700894005981,2.32439489252746,
7.51849533314857));
#392494=CARTESIAN_POINT('Ctrl Pts',(-1.45700592305912,2.3243565891188,7.51860402984325));
#392495=CARTESIAN_POINT('Ctrl Pts',(-1.45874211329886,2.24101961475187,
7.57603338728985));
#392496=CARTESIAN_POINT('Ctrl Pts',(-1.46093030563708,2.26831776647326,
7.55196141284922));
#392497=CARTESIAN_POINT('Ctrl Pts',(-1.46311385931009,2.29556894514296,
7.52783573083105));
#392498=CARTESIAN_POINT('Ctrl Pts',(-1.46529313746699,2.32277700541882,
7.50366116530176));
#392499=CARTESIAN_POINT('Origin',(-5.0406283147387E-16,7.74375868966275E-16,
7.49482233047033));
#392500=CARTESIAN_POINT('Origin',(-1.52592346056196,2.27276568139055,7.49482233047033));
#392501=CARTESIAN_POINT('Origin',(0.,0.,7.50366116523517));
#392502=CARTESIAN_POINT('Origin',(-1.4605772285055,2.31530136474093,7.49482233047033));
#392503=CARTESIAN_POINT('Ctrl Pts',(-1.53564834642937,2.27316493579466,
7.51860402984325));
#392504=CARTESIAN_POINT('Ctrl Pts',(-1.54234243883857,2.27678231230909,
7.51860402984325));
#392505=CARTESIAN_POINT('Ctrl Pts',(-1.54863020028822,2.27249741534622,
7.51860402984325));
#392506=CARTESIAN_POINT('Ctrl Pts',(-1.53813390922789,2.27450809126278,
7.51041458714365));
#392507=CARTESIAN_POINT('Ctrl Pts',(-1.54383207597013,2.27576716295958,
7.51004642900441));
#392508=CARTESIAN_POINT('Ctrl Pts',(-1.54863193437817,2.27249623362252,
7.5072913648301));
#392509=CARTESIAN_POINT('Ctrl Pts',(-1.53773211669731,2.2772941817067,7.50215815450137));
#392510=CARTESIAN_POINT('Ctrl Pts',(-1.54079910519163,2.27783422435051,
7.49877163671531));
#392511=CARTESIAN_POINT('Ctrl Pts',(-1.54366359294843,2.27591104118568,
7.4948158853317));
#392512=CARTESIAN_POINT('Ctrl Pts',(-1.53085005244588,2.28010352581767,
7.50366171572174));
#392513=CARTESIAN_POINT('Ctrl Pts',(-1.53289114759616,2.28314360687656,
7.50000045605858));
#392514=CARTESIAN_POINT('Ctrl Pts',(-1.53289114759627,2.28314360687649,
7.49482233047317));
#392515=CARTESIAN_POINT('Origin',(-1.5415909721051,2.2621678816401,7.51860402984325));
#392516=CARTESIAN_POINT('Origin',(-1.5415909721051,2.2621678816401,9.));
#392517=CARTESIAN_POINT('Origin',(-1.5415909721051,2.2621678816401,8.75721825406948));
#392518=CARTESIAN_POINT('Ctrl Pts',(-1.52095641350492,2.26522723077965,
8.78942910404913));
#392519=CARTESIAN_POINT('Ctrl Pts',(-1.52584946047529,2.26789378661956,
8.79672699501691));
#392520=CARTESIAN_POINT('Ctrl Pts',(-1.5314874230971,2.26097375313284,8.79893251111267));
#392521=CARTESIAN_POINT('Ctrl Pts',(-1.53062927805545,2.27045323404477,
8.78111911759578));
#392522=CARTESIAN_POINT('Ctrl Pts',(-1.53643360398451,2.27360793064428,
8.78644465894812));
#392523=CARTESIAN_POINT('Ctrl Pts',(-1.54278266608223,2.26856760106628,
8.78817647674131));
#392524=CARTESIAN_POINT('Ctrl Pts',(-1.53665763797808,2.27371020390355,
8.76780923932034));
#392525=CARTESIAN_POINT('Ctrl Pts',(-1.54351183306585,2.27742971280518,
8.76988516158375));
#392526=CARTESIAN_POINT('Ctrl Pts',(-1.54984371438415,2.27330131609856,
8.77093053738833));
#392527=CARTESIAN_POINT('Ctrl Pts',(-1.53548219029791,2.27307513935434,
8.75371302330491));
#392528=CARTESIAN_POINT('Ctrl Pts',(-1.54216779835547,2.27670402985536,
8.75300828287558));
#392529=CARTESIAN_POINT('Ctrl Pts',(-1.54846677797149,2.27237766936051,
8.75267964240738));
#392530=CARTESIAN_POINT('Origin',(-1.52925384132081,2.25550244950119,8.78727029226991));
#392531=CARTESIAN_POINT('Ctrl Pts',(-1.46041276049034,2.23251709792628,
8.85049129520029));
#392532=CARTESIAN_POINT('Ctrl Pts',(-1.46555048104866,2.23529287523861,
8.85711686593484));
#392533=CARTESIAN_POINT('Ctrl Pts',(-1.47122360941501,2.22889628422051,
8.85933012996512));
#392534=CARTESIAN_POINT('Ctrl Pts',(-1.48140972735874,2.24386121514701,
8.82945683644724));
#392535=CARTESIAN_POINT('Ctrl Pts',(-1.48659009410405,2.24666003308931,
8.8360746990239));
#392536=CARTESIAN_POINT('Ctrl Pts',(-1.49225182125613,2.240219777803,8.8382956714852));
#392537=CARTESIAN_POINT('Ctrl Pts',(-1.50237539655485,2.25518842304624,
8.80838214965001));
#392538=CARTESIAN_POINT('Ctrl Pts',(-1.507576207446,2.25799828643086,8.81501364461992));
#392539=CARTESIAN_POINT('Ctrl Pts',(-1.51324781742241,2.25152668285288,
8.81722098428721));
#392540=CARTESIAN_POINT('Ctrl Pts',(-1.52331214621093,2.26650000646723,
8.78727029226991));
#392541=CARTESIAN_POINT('Ctrl Pts',(-1.52851382097383,2.2693103365794,8.79393457792714));
#392542=CARTESIAN_POINT('Ctrl Pts',(-1.53421404825537,2.26281827803707,
8.79610912703474));
#392543=CARTESIAN_POINT('Origin',(-1.46635445560022,2.22151954096025,8.85049129520029));
#392544=CARTESIAN_POINT('Ctrl Pts',(-1.45029105591254,2.23910559748223,
8.85049129520029));
#392545=CARTESIAN_POINT('Ctrl Pts',(-1.45074959802199,2.24492718243454,
8.85711686593484));
#392546=CARTESIAN_POINT('Ctrl Pts',(-1.44260408658468,2.24752552912783,
8.85933012996512));
#392547=CARTESIAN_POINT('Ctrl Pts',(-1.44988539032744,2.23395532531039,
8.86332496987232));
#392548=CARTESIAN_POINT('Ctrl Pts',(-1.44617396855412,2.23670800451389,
8.86648636486738));
#392549=CARTESIAN_POINT('Ctrl Pts',(-1.44148630031577,2.23311608742407,
8.87206031107458));
#392550=CARTESIAN_POINT('Ctrl Pts',(-1.45583660675252,2.2300447206183,8.86341338519875));
#392551=CARTESIAN_POINT('Ctrl Pts',(-1.45985275223894,2.22773300133036,
8.86654584966059));
#392552=CARTESIAN_POINT('Ctrl Pts',(-1.45840313270636,2.22198645836977,
8.87215952290713));
#392553=CARTESIAN_POINT('Ctrl Pts',(-1.46041276049034,2.23251709792628,
8.85049129520029));
#392554=CARTESIAN_POINT('Ctrl Pts',(-1.46555048104866,2.23529287523861,
8.85711686593484));
#392555=CARTESIAN_POINT('Ctrl Pts',(-1.47122360941501,2.22889628422051,
8.85933012996512));
#392556=CARTESIAN_POINT('Origin',(-1.43782965179007,2.24008713061793,8.85049129520029));
#392557=CARTESIAN_POINT('Ctrl Pts',(-1.45590483281685,2.31037730509331,
8.78727029226991));
#392558=CARTESIAN_POINT('Ctrl Pts',(-1.4563690828459,2.31627135697541,8.79393457792714));
#392559=CARTESIAN_POINT('Ctrl Pts',(-1.44812530550985,2.3188558395952,8.79610912703474));
#392560=CARTESIAN_POINT('Ctrl Pts',(-1.45403622567031,2.28665373636971,
8.80838214965003));
#392561=CARTESIAN_POINT('Ctrl Pts',(-1.4545003985987,2.29254680939306,8.81501364461993));
#392562=CARTESIAN_POINT('Ctrl Pts',(-1.44628690934869,2.29511340381664,
8.81722098428721));
#392563=CARTESIAN_POINT('Ctrl Pts',(-1.45216503745173,2.26289739872514,
8.82945683644723));
#392564=CARTESIAN_POINT('Ctrl Pts',(-1.45262738573793,2.26876730635234,
8.83607469902391));
#392565=CARTESIAN_POINT('Ctrl Pts',(-1.44444656216421,2.27133755306294,
8.8382956714852));
#392566=CARTESIAN_POINT('Ctrl Pts',(-1.45029105591254,2.23910559748223,
8.85049129520029));
#392567=CARTESIAN_POINT('Ctrl Pts',(-1.45074959802199,2.24492718243454,
8.85711686593484));
#392568=CARTESIAN_POINT('Ctrl Pts',(-1.44260408658468,2.24752552912783,
8.85933012996512));
#392569=CARTESIAN_POINT('Origin',(-1.44344342869438,2.31135883822901,8.78727029226991));
#392570=CARTESIAN_POINT('Ctrl Pts',(-1.45699136532626,2.32417200115391,
8.75374538247848));
#392571=CARTESIAN_POINT('Ctrl Pts',(-1.45760113795343,2.33174646851016,
8.75304829418601));
#392572=CARTESIAN_POINT('Ctrl Pts',(-1.45110520950818,2.33575565257218,
8.75272238421917));
#392573=CARTESIAN_POINT('Ctrl Pts',(-1.45709501436911,2.3254879091256,8.76769408445022));
#392574=CARTESIAN_POINT('Ctrl Pts',(-1.45771944369952,2.33325303906547,
8.76974318093972));
#392575=CARTESIAN_POINT('Ctrl Pts',(-1.45138968706044,2.33737038507602,
8.77077869880429));
#392576=CARTESIAN_POINT('Ctrl Pts',(-1.45656376843517,2.3187433144848,8.78108014887986));
#392577=CARTESIAN_POINT('Ctrl Pts',(-1.45709673696933,2.32532367783663,
8.78639403366321));
#392578=CARTESIAN_POINT('Ctrl Pts',(-1.44993759076019,2.3291010712878,8.78812224174741));
#392579=CARTESIAN_POINT('Ctrl Pts',(-1.45569317358814,2.30769041275578,
8.78944554828685));
#392580=CARTESIAN_POINT('Ctrl Pts',(-1.45614791916575,2.31323564711302,
8.79673892988687));
#392581=CARTESIAN_POINT('Ctrl Pts',(-1.44754787197038,2.31558995009989,
8.79894799272499));
#392582=CARTESIAN_POINT('Origin',(-1.44454451893666,2.3253381222545,8.75721825406948));
#392583=CARTESIAN_POINT('Origin',(-1.44454451893666,2.3253381222545,9.));
#392584=CARTESIAN_POINT('Origin',(-1.44454451893666,2.3253381222545,7.51860402984325));
#392585=CARTESIAN_POINT('Ctrl Pts',(-1.46529271774777,2.32277634002135,
7.50366195182967));
#392586=CARTESIAN_POINT('Ctrl Pts',(-1.46724653091864,2.32587351709142,
7.50000065167736));
#392587=CARTESIAN_POINT('Ctrl Pts',(-1.46724653091855,2.32587351709148,
7.49482233047108));
#392588=CARTESIAN_POINT('Ctrl Pts',(-1.45993268034609,2.32793616546986,
7.50215800491335));
#392589=CARTESIAN_POINT('Ctrl Pts',(-1.45918346602513,2.33095996689781,
7.49877273257261));
#392590=CARTESIAN_POINT('Ctrl Pts',(-1.4562637686462,2.33280184734057,7.49481816995645));
#392591=CARTESIAN_POINT('Ctrl Pts',(-1.45722758392156,2.32716644495162,
7.51043025814045));
#392592=CARTESIAN_POINT('Ctrl Pts',(-1.45607536702449,2.33289053031166,
7.5100620959452));
#392593=CARTESIAN_POINT('Ctrl Pts',(-1.45113846196593,2.33595744058183,
7.50731281821702));
#392594=CARTESIAN_POINT('Ctrl Pts',(-1.45700580428831,2.32435508238525,
7.51860402984326));
#392595=CARTESIAN_POINT('Ctrl Pts',(-1.45760422169307,2.33194078696693,
7.51860402984326));
#392596=CARTESIAN_POINT('Ctrl Pts',(-1.45114061263043,2.3359561045479,7.51860402984327));
#392597=CARTESIAN_POINT('Origin',(0.,0.,7.5));
#392598=CARTESIAN_POINT('Origin',(-1.59077126558568,2.14158464790051,7.5));
#392599=CARTESIAN_POINT('',(-1.59077126558568,2.14158464790051,7.59394543036555));
#392600=CARTESIAN_POINT('',(-1.59077126558568,2.14158464790051,8.85049129520029));
#392601=CARTESIAN_POINT('',(-1.59077126558568,2.14158464790051,7.5));
#392602=CARTESIAN_POINT('',(-1.6009399023683,2.21235024422325,8.78727029226991));
#392603=CARTESIAN_POINT('Ctrl Pts',(-1.59077126558568,2.14158464790051,
8.85049129520029));
#392604=CARTESIAN_POINT('Ctrl Pts',(-1.59416573821266,2.16520746822393,
8.82945686509571));
#392605=CARTESIAN_POINT('Ctrl Pts',(-1.59755516454564,2.1887951703685,8.80838212259894));
#392606=CARTESIAN_POINT('Ctrl Pts',(-1.6009399023683,2.21235024422325,8.78727029226991));
#392607=CARTESIAN_POINT('',(-1.60293438610527,2.22623025921639,8.75721825406948));
#392608=CARTESIAN_POINT('Origin',(-1.59693249240023,2.18446045038835,8.75937679713127));
#392609=CARTESIAN_POINT('',(-1.60293438610527,2.22623025921639,7.51860402984325));
#392610=CARTESIAN_POINT('',(-1.60293438610527,2.22623025921639,7.5));
#392611=CARTESIAN_POINT('Ctrl Pts',(-1.60293438610527,2.22623025921639,
7.51860402984325));
#392612=CARTESIAN_POINT('Ctrl Pts',(-1.60136802933078,2.21532966618994,
7.52834476460825));
#392613=CARTESIAN_POINT('Ctrl Pts',(-1.59980065570007,2.20442199665579,
7.53807742314407));
#392614=CARTESIAN_POINT('Ctrl Pts',(-1.59823223107085,2.19350701301077,
7.54780169004674));
#392615=CARTESIAN_POINT('Ctrl Pts',(-1.59574793122428,2.1762182688216,7.5632044032688));
#392616=CARTESIAN_POINT('Ctrl Pts',(-1.59326099139909,2.15891115248838,
7.57858609112103));
#392617=CARTESIAN_POINT('Ctrl Pts',(-1.59077126558568,2.14158464790051,
7.59394543036555));
#392618=CARTESIAN_POINT('Origin',(-1.85027428182726,2.24930835533596,7.5));
#392619=CARTESIAN_POINT('',(-1.67813633056181,2.17010558942599,8.75721825406948));
#392620=CARTESIAN_POINT('',(-1.66539749203247,2.16424429481555,8.78727029226991));
#392621=CARTESIAN_POINT('Origin',(-1.63306156849634,2.14936614294093,8.75658640621094));
#392622=CARTESIAN_POINT('',(-1.60045004741997,2.13436118528463,8.85049129520029));
#392623=CARTESIAN_POINT('Ctrl Pts',(-1.66539749203247,2.16424429481555,
8.78727029226991));
#392624=CARTESIAN_POINT('Ctrl Pts',(-1.64377905123609,2.15429738715721,
8.80838212259896));
#392625=CARTESIAN_POINT('Ctrl Pts',(-1.62213066475766,2.14433670112618,
8.82945686509571));
#392626=CARTESIAN_POINT('Ctrl Pts',(-1.60045004741997,2.13436118528463,
8.85049129520029));
#392627=CARTESIAN_POINT('',(-1.60045004741997,2.13436118528463,7.59394543036555));
#392628=CARTESIAN_POINT('',(-1.60045004741997,2.13436118528463,7.5));
#392629=CARTESIAN_POINT('',(-1.67813633056181,2.17010558942599,7.51860402984325));
#392630=CARTESIAN_POINT('Ctrl Pts',(-1.60045004741997,2.13436118528463,
7.59394543036555));
#392631=CARTESIAN_POINT('Ctrl Pts',(-1.61635201469679,2.14167787391996,
7.57858609112103));
#392632=CARTESIAN_POINT('Ctrl Pts',(-1.63223618776747,2.14898637522455,
7.56320440326857));
#392633=CARTESIAN_POINT('Ctrl Pts',(-1.64810349920118,2.15628711828479,
7.54780169004651));
#392634=CARTESIAN_POINT('Ctrl Pts',(-1.65812108306352,2.16089633051137,
7.53807742314383));
#392635=CARTESIAN_POINT('Ctrl Pts',(-1.66813195416115,2.16550245411323,
7.52834476460825));
#392636=CARTESIAN_POINT('Ctrl Pts',(-1.67813633056181,2.17010558942599,
7.51860402984325));
#392637=CARTESIAN_POINT('',(-1.67813633056181,2.17010558942599,7.5));
#392638=CARTESIAN_POINT('Origin',(-1.59757636816869,2.14060679114481,7.5));
#392639=CARTESIAN_POINT('Ctrl Pts',(-1.60045004741997,2.13436118528463,
8.85049129520029));
#392640=CARTESIAN_POINT('Ctrl Pts',(-1.60027411528379,2.13428023676807,
8.85097269580138));
#392641=CARTESIAN_POINT('Ctrl Pts',(-1.60009688697325,2.13420795092934,
8.85143669361005));
#392642=CARTESIAN_POINT('Ctrl Pts',(-1.59990987151214,2.13414180877791,
8.8519052845931));
#392643=CARTESIAN_POINT('Ctrl Pts',(-1.59954408113029,2.13401243892429,
8.85282181883899));
#392644=CARTESIAN_POINT('Ctrl Pts',(-1.59915019230981,2.13391008645579,
8.85372622499635));
#392645=CARTESIAN_POINT('Ctrl Pts',(-1.59871814646302,2.13384806842956,
8.8546225773507));
#392646=CARTESIAN_POINT('Ctrl Pts',(-1.59835947734583,2.13379658326685,
8.85536669723986));
#392647=CARTESIAN_POINT('Ctrl Pts',(-1.5979744341408,2.13377285249161,8.85610498449051));
#392648=CARTESIAN_POINT('Ctrl Pts',(-1.5975567370227,2.13379248063128,8.85681338218371));
#392649=CARTESIAN_POINT('Ctrl Pts',(-1.59717767623202,2.13381029319887,
8.85745625420284));
#392650=CARTESIAN_POINT('Ctrl Pts',(-1.59676693999368,2.13386344000459,
8.85808743050666));
#392651=CARTESIAN_POINT('Ctrl Pts',(-1.59631559501554,2.13397908798499,
8.85866804508411));
#392652=CARTESIAN_POINT('Ctrl Pts',(-1.59610735422658,2.1340324454562,8.85893592806396));
#392653=CARTESIAN_POINT('Ctrl Pts',(-1.59589042136149,2.134099345177,8.85919241173848));
#392654=CARTESIAN_POINT('Ctrl Pts',(-1.59566382655845,2.13418404876029,
8.85943017985534));
#392655=CARTESIAN_POINT('Ctrl Pts',(-1.5953578564951,2.13429842367268,8.8597512372));
#392656=CARTESIAN_POINT('Ctrl Pts',(-1.59502670637818,2.13444877149743,
8.86004599534705));
#392657=CARTESIAN_POINT('Ctrl Pts',(-1.59467866049515,2.13464276930003,
8.86026130871721));
#392658=CARTESIAN_POINT('Ctrl Pts',(-1.59455123108491,2.13471379736494,
8.86034014101235));
#392659=CARTESIAN_POINT('Ctrl Pts',(-1.59441961667037,2.13479173285642,
8.86040910639693));
#392660=CARTESIAN_POINT('Ctrl Pts',(-1.59428757440422,2.13487474190566,
8.86046313645507));
#392661=CARTESIAN_POINT('Ctrl Pts',(-1.59408152355374,2.13500427683181,
8.8605474499083));
#392662=CARTESIAN_POINT('Ctrl Pts',(-1.59386888451753,2.13514982695018,
8.86059655985668));
#392663=CARTESIAN_POINT('Ctrl Pts',(-1.59366312900933,2.13530181594062,
8.86059725258816));
#392664=CARTESIAN_POINT('Ctrl Pts',(-1.59345689812371,2.13545415608635,
8.86059794692011));
#392665=CARTESIAN_POINT('Ctrl Pts',(-1.59325687403524,2.13561679132399,
8.86056369958366));
#392666=CARTESIAN_POINT('Ctrl Pts',(-1.59307159215571,2.13577793168174,
8.86048590497774));
#392667=CARTESIAN_POINT('Ctrl Pts',(-1.59302323910166,2.13581998451738,
8.86046560290182));
#392668=CARTESIAN_POINT('Ctrl Pts',(-1.59297532046823,2.13586255097362,
8.86044257503091));
#392669=CARTESIAN_POINT('Ctrl Pts',(-1.59292929518032,2.13590429117004,
8.86041778462583));
#392670=CARTESIAN_POINT('Ctrl Pts',(-1.5926196021053,2.1361851508967,8.860250975962));
#392671=CARTESIAN_POINT('Ctrl Pts',(-1.59235429876773,2.13646653421406,
8.8599848982295));
#392672=CARTESIAN_POINT('Ctrl Pts',(-1.59213496417169,2.13673441605688,
8.85968173251461));
#392673=CARTESIAN_POINT('Ctrl Pts',(-1.59201894873675,2.13687611020393,
8.85952137522076));
#392674=CARTESIAN_POINT('Ctrl Pts',(-1.5919134104205,2.13701663718526,8.85934740853961));
#392675=CARTESIAN_POINT('Ctrl Pts',(-1.59181859451241,2.13715308171862,
8.8591675900182));
#392676=CARTESIAN_POINT('Ctrl Pts',(-1.59143785935708,2.13770097744252,
8.85844552518694));
#392677=CARTESIAN_POINT('Ctrl Pts',(-1.59120601346866,2.13821228521468,
8.85759444184122));
#392678=CARTESIAN_POINT('Ctrl Pts',(-1.59105442443434,2.13864615733892,
8.85683498915135));
#392679=CARTESIAN_POINT('Ctrl Pts',(-1.59103856104561,2.13869156090121,
8.85675551444996));
#392680=CARTESIAN_POINT('Ctrl Pts',(-1.59102359633076,2.13873611922891,
8.8566769979365));
#392681=CARTESIAN_POINT('Ctrl Pts',(-1.59100946472095,2.13877978665774,
8.85659965593547));
#392682=CARTESIAN_POINT('Ctrl Pts',(-1.59081871553059,2.1393692118404,8.85555568965886));
#392683=CARTESIAN_POINT('Ctrl Pts',(-1.5907205184002,2.13996323391635,8.85434650606346));
#392684=CARTESIAN_POINT('Ctrl Pts',(-1.59070825637446,2.14056377579998,
8.85297329937117));
#392685=CARTESIAN_POINT('Ctrl Pts',(-1.59070135973212,2.14090154401798,
8.85220095427747));
#392686=CARTESIAN_POINT('Ctrl Pts',(-1.59072195981991,2.14124151912217,
8.85137579139183));
#392687=CARTESIAN_POINT('Ctrl Pts',(-1.59077126558568,2.14158464790051,
8.85049129520029));
#392688=CARTESIAN_POINT('Origin',(-1.59757636816869,2.14060679114481,7.59394543036555));
#392689=CARTESIAN_POINT('Ctrl Pts',(-1.5999392570785,2.13412616443334,7.59443877723642));
#392690=CARTESIAN_POINT('Ctrl Pts',(-1.59467860803055,2.13170567579608,
7.58783886950016));
#392691=CARTESIAN_POINT('Ctrl Pts',(-1.58944159958292,2.13838796014023,
7.58559994247159));
#392692=CARTESIAN_POINT('Ctrl Pts',(-1.6286569858903,2.14733954088999,7.56670252222132));
#392693=CARTESIAN_POINT('Ctrl Pts',(-1.62340393997377,2.14492255054603,
7.56004874999026));
#392694=CARTESIAN_POINT('Ctrl Pts',(-1.61811908396269,2.15163125043487,
7.55786368756704));
#392695=CARTESIAN_POINT('Ctrl Pts',(-1.65732108721283,2.16052824268631,
7.53888913333556));
#392696=CARTESIAN_POINT('Ctrl Pts',(-1.65203682218721,2.15809688805035,
7.53222002137275));
#392697=CARTESIAN_POINT('Ctrl Pts',(-1.64674452104204,2.16484922048508,
7.53005029815326));
#392698=CARTESIAN_POINT('Ctrl Pts',(-1.68593026397609,2.17369167302459,
7.51101258149734));
#392699=CARTESIAN_POINT('Ctrl Pts',(-1.68058194405661,2.17123084595258,
7.5043616886572));
#392700=CARTESIAN_POINT('Ctrl Pts',(-1.67531646186255,2.17804129225284,
7.50217374673251));
#392701=CARTESIAN_POINT('',(-1.67379182682864,2.17733734542425,7.50366116523517));
#392702=CARTESIAN_POINT('Ctrl Pts',(-1.67813633056181,2.17010558942599,
7.51860402984325));
#392703=CARTESIAN_POINT('Ctrl Pts',(-1.67853751304855,2.17029017836963,
7.51734760759494));
#392704=CARTESIAN_POINT('Ctrl Pts',(-1.67887516973812,2.17051103085425,
7.51608817408573));
#392705=CARTESIAN_POINT('Ctrl Pts',(-1.6791412144495,2.17077881433843,7.5148100591312));
#392706=CARTESIAN_POINT('Ctrl Pts',(-1.67938220410642,2.1710213790173,7.51365231206384));
#392707=CARTESIAN_POINT('Ctrl Pts',(-1.67956495208892,2.17130261697214,
7.51247773061043));
#392708=CARTESIAN_POINT('Ctrl Pts',(-1.67965533378804,2.17163778110542,
7.51129758471022));
#392709=CARTESIAN_POINT('Ctrl Pts',(-1.67976766791807,2.1720543518459,7.50983079813401));
#392710=CARTESIAN_POINT('Ctrl Pts',(-1.67972115732488,2.17254432228918,
7.50839324291155));
#392711=CARTESIAN_POINT('Ctrl Pts',(-1.67943339189004,2.17310347783573,
7.50715379678855));
#392712=CARTESIAN_POINT('Ctrl Pts',(-1.67930045255091,2.17336179158656,
7.50658120839351));
#392713=CARTESIAN_POINT('Ctrl Pts',(-1.67908867816628,2.17366724429875,
7.50598221009429));
#392714=CARTESIAN_POINT('Ctrl Pts',(-1.67878441548016,2.17399960639674,
7.50545747549611));
#392715=CARTESIAN_POINT('Ctrl Pts',(-1.67862205149304,2.1741769650998,7.50517746087247));
#392716=CARTESIAN_POINT('Ctrl Pts',(-1.67843173911099,2.17436404651079,
7.50491486231392));
#392717=CARTESIAN_POINT('Ctrl Pts',(-1.6782173488015,2.17455470687898,7.50468370960992));
#392718=CARTESIAN_POINT('Ctrl Pts',(-1.67789676766324,2.17483980426982,
7.50433806340447));
#392719=CARTESIAN_POINT('Ctrl Pts',(-1.67751236609578,2.17514103710608,
7.50405484070984));
#392720=CARTESIAN_POINT('Ctrl Pts',(-1.67708959094887,2.17543755403429,
7.50385766036131));
#392721=CARTESIAN_POINT('Ctrl Pts',(-1.67704438171832,2.17546926191084,
7.50383657498791));
#392722=CARTESIAN_POINT('Ctrl Pts',(-1.67699876196235,2.17550091364687,
7.50381643264937));
#392723=CARTESIAN_POINT('Ctrl Pts',(-1.67695278336429,2.17553248245705,
7.50379723213559));
#392724=CARTESIAN_POINT('Ctrl Pts',(-1.67664586118161,2.17574321459188,
7.50366906242519));
#392725=CARTESIAN_POINT('Ctrl Pts',(-1.67631586572899,2.17595424268713,
7.50358235568538));
#392726=CARTESIAN_POINT('Ctrl Pts',(-1.67599290128613,2.1761500019308,7.5035341175365));
#392727=CARTESIAN_POINT('Ctrl Pts',(-1.67550865265657,2.17644352076102,
7.50346178989176));
#392728=CARTESIAN_POINT('Ctrl Pts',(-1.67497523124542,2.17673869053725,
7.50346967198527));
#392729=CARTESIAN_POINT('Ctrl Pts',(-1.67444266060026,2.17701234294118,
7.50354272648693));
#392730=CARTESIAN_POINT('Ctrl Pts',(-1.67422360327035,2.17712490183919,
7.50357277531559));
#392731=CARTESIAN_POINT('Ctrl Pts',(-1.67400504573784,2.17723379689431,
7.50361331098761));
#392732=CARTESIAN_POINT('Ctrl Pts',(-1.67379182682951,2.17733734542537,
7.50366116523659));
#392733=CARTESIAN_POINT('',(-1.59932759105274,2.14295327027008,7.57603338622103));
#392734=CARTESIAN_POINT('Origin',(-1.60461077043295,2.15003701964751,7.58486873427628));
#392735=CARTESIAN_POINT('Ctrl Pts',(-1.67379182688272,2.17733734544332,
7.50366116529969));
#392736=CARTESIAN_POINT('Ctrl Pts',(-1.64901056798236,2.16589544848023,
7.52783573079709));
#392737=CARTESIAN_POINT('Ctrl Pts',(-1.62419032049072,2.15443464751556,
7.55196141284068));
#392738=CARTESIAN_POINT('Ctrl Pts',(-1.59932759229143,2.14295327045253,
7.57603338728831));
#392739=CARTESIAN_POINT('Ctrl Pts',(-1.60131081754386,2.13495077015054,
7.59639677331371));
#392740=CARTESIAN_POINT('Ctrl Pts',(-1.58612303190611,2.12478203949354,
7.59959882295467));
#392741=CARTESIAN_POINT('Ctrl Pts',(-1.59104033438506,2.14240387109349,
7.59642833564546));
#392742=CARTESIAN_POINT('Ctrl Pts',(-1.5984605437931,2.13228786879496,7.58707626057421));
#392743=CARTESIAN_POINT('Ctrl Pts',(-1.59169006087516,2.13255778006641,
7.58809943920599));
#392744=CARTESIAN_POINT('Ctrl Pts',(-1.58940753054067,2.13892209118902,
7.58710240504253));
#392745=CARTESIAN_POINT('Ctrl Pts',(-1.59858892220314,2.13836315901399,
7.58015376756929));
#392746=CARTESIAN_POINT('Ctrl Pts',(-1.59574942482533,2.13810523259534,
7.58205880659761));
#392747=CARTESIAN_POINT('Ctrl Pts',(-1.59515444522379,2.14085715452587,
7.58020924244127));
#392748=CARTESIAN_POINT('Ctrl Pts',(-1.59932759055792,2.14295326960673,
7.57603338509286));
#392749=CARTESIAN_POINT('Ctrl Pts',(-1.59932759055792,2.14295326960673,
7.57603338509286));
#392750=CARTESIAN_POINT('Ctrl Pts',(-1.59932759055792,2.14295326960673,
7.57603338509286));
#392751=CARTESIAN_POINT('Origin',(-1.60461534358171,2.15003360661839,7.58486873427622));
#392752=CARTESIAN_POINT('Ctrl Pts',(-1.60415851687137,2.23474923235822,
7.51098857897448));
#392753=CARTESIAN_POINT('Ctrl Pts',(-1.60332114180599,2.22892177022006,
7.50433767179956));
#392754=CARTESIAN_POINT('Ctrl Pts',(-1.61134830926253,2.22581168441625,
7.50214974420965));
#392755=CARTESIAN_POINT('Ctrl Pts',(-1.59967797104069,2.20356820934231,
7.53887321589168));
#392756=CARTESIAN_POINT('Ctrl Pts',(-1.59885062921467,2.19781057054244,
7.53220407452063));
#392757=CARTESIAN_POINT('Ctrl Pts',(-1.60682970075316,2.19465821629432,
7.53003438070911));
#392758=CARTESIAN_POINT('Ctrl Pts',(-1.5951888209092,2.17232730725995,7.56669465659229));
#392759=CARTESIAN_POINT('Ctrl Pts',(-1.59436636851957,2.16660369503491,
7.56004085833293));
#392760=CARTESIAN_POINT('Ctrl Pts',(-1.60230148007192,2.16344606067078,
7.55785582193789));
#392761=CARTESIAN_POINT('Ctrl Pts',(-1.59069126950322,2.14102793901222,
7.59443891967696));
#392762=CARTESIAN_POINT('Ctrl Pts',(-1.58986762466,2.1352960282621,7.58783901202978));
#392763=CARTESIAN_POINT('Ctrl Pts',(-1.59776378899004,2.13217677084064,
7.58560008491213));
#392764=CARTESIAN_POINT('',(-1.61110336926411,2.2241229572313,7.50366116523517));
#392765=CARTESIAN_POINT('Ctrl Pts',(-1.61110336926433,2.2241229572316,7.50366116523554));
#392766=CARTESIAN_POINT('Ctrl Pts',(-1.61059198069087,2.22468208087061,
7.50350835821027));
#392767=CARTESIAN_POINT('Ctrl Pts',(-1.61010369996943,2.22517941370506,
7.50345484956));
#392768=CARTESIAN_POINT('Ctrl Pts',(-1.60962443861778,2.22563016254553,
7.50349758195598));
#392769=CARTESIAN_POINT('Ctrl Pts',(-1.60937854200143,2.2258614301291,7.50351950684424));
#392770=CARTESIAN_POINT('Ctrl Pts',(-1.60911087181359,2.22610332366123,
7.50357029184312));
#392771=CARTESIAN_POINT('Ctrl Pts',(-1.60884634880776,2.22632948384843,
7.50365515313924));
#392772=CARTESIAN_POINT('Ctrl Pts',(-1.60843940530885,2.22667740979763,
7.50378570417639));
#392773=CARTESIAN_POINT('Ctrl Pts',(-1.60802819036976,2.22699857665869,
7.50400001621911));
#392774=CARTESIAN_POINT('Ctrl Pts',(-1.60764260590765,2.22726674962693,
7.50428903009634));
#392775=CARTESIAN_POINT('Ctrl Pts',(-1.60759980899887,2.22729651476321,
7.50432110841318));
#392776=CARTESIAN_POINT('Ctrl Pts',(-1.60755731717549,2.22732565543007,
7.50435406373354));
#392777=CARTESIAN_POINT('Ctrl Pts',(-1.60751516316794,2.22735415659425,
7.50438785222352));
#392778=CARTESIAN_POINT('Ctrl Pts',(-1.60725779269008,2.22752816990098,
7.50459414719561));
#392779=CARTESIAN_POINT('Ctrl Pts',(-1.60700862846065,2.22768068774654,
7.50483629897752));
#392780=CARTESIAN_POINT('Ctrl Pts',(-1.606777902955,2.22780698965991,7.5050991045531));
#392781=CARTESIAN_POINT('Ctrl Pts',(-1.60626889931535,2.22808562436663,
7.50567888004914));
#392782=CARTESIAN_POINT('Ctrl Pts',(-1.60582982688945,2.22824810547532,
7.50637912803144));
#392783=CARTESIAN_POINT('Ctrl Pts',(-1.60546347309894,2.22832521688821,
7.50710440483569));
#392784=CARTESIAN_POINT('Ctrl Pts',(-1.60537363587636,2.22834412613752,
7.50728225710685));
#392785=CARTESIAN_POINT('Ctrl Pts',(-1.60528641310257,2.22835842111519,
7.50746498566954));
#392786=CARTESIAN_POINT('Ctrl Pts',(-1.60520390821615,2.22836817923874,
7.50764697238949));
#392787=CARTESIAN_POINT('Ctrl Pts',(-1.6047603846527,2.22842063622541,7.50862528291181));
#392788=CARTESIAN_POINT('Ctrl Pts',(-1.60441342469442,2.22835085759284,
7.50965856837421));
#392789=CARTESIAN_POINT('Ctrl Pts',(-1.60413297204735,2.22821793661504,
7.51067959873201));
#392790=CARTESIAN_POINT('Ctrl Pts',(-1.60397863860191,2.22814479003329,
7.51124147302578));
#392791=CARTESIAN_POINT('Ctrl Pts',(-1.60384459404929,2.22805211156062,
7.51180065547253));
#392792=CARTESIAN_POINT('Ctrl Pts',(-1.60372708158227,2.22794733879845,
7.51235175716501));
#392793=CARTESIAN_POINT('Ctrl Pts',(-1.60332102919732,2.22758530716864,
7.51425603304536));
#392794=CARTESIAN_POINT('Ctrl Pts',(-1.6030679879822,2.22703118031393,7.51626900505181));
#392795=CARTESIAN_POINT('Ctrl Pts',(-1.60295199935763,2.22634316468707,
7.51827788969244));
#392796=CARTESIAN_POINT('Ctrl Pts',(-1.60294572183408,2.22630592798117,
7.51838661432546));
#392797=CARTESIAN_POINT('Ctrl Pts',(-1.60293985101502,2.2262682906267,7.51849533314857));
#392798=CARTESIAN_POINT('Ctrl Pts',(-1.60293438610526,2.2262302592164,7.51860402984325));
#392799=CARTESIAN_POINT('Ctrl Pts',(-1.59932759087573,2.14295327151058,
7.57603338728985));
#392800=CARTESIAN_POINT('Ctrl Pts',(-1.60326028592398,2.17005513828706,
7.55196141284922));
#392801=CARTESIAN_POINT('Ctrl Pts',(-1.60718534226387,2.19711042572333,
7.52783573083105));
#392802=CARTESIAN_POINT('Ctrl Pts',(-1.61110336926719,2.2241229572904,7.50366116530176));
#392803=CARTESIAN_POINT('Origin',(-5.52641612598462E-16,7.404894141953E-16,
7.49482233047033));
#392804=CARTESIAN_POINT('Origin',(-1.66840488432876,2.17032978875284,7.49482233047033));
#392805=CARTESIAN_POINT('Origin',(0.,0.,7.50366116523517));
#392806=CARTESIAN_POINT('Origin',(-1.60591818370371,2.21696482544261,7.49482233047033));
#392807=CARTESIAN_POINT('Ctrl Pts',(-1.67813536969267,2.17010514726915,
7.51860402984325));
#392808=CARTESIAN_POINT('Ctrl Pts',(-1.68504747448011,2.17328619952234,
7.51860402984325));
#392809=CARTESIAN_POINT('Ctrl Pts',(-1.6910477827585,2.16860724808057,7.51860402984325));
#392810=CARTESIAN_POINT('Ctrl Pts',(-1.68070188190216,2.17128629252504,
7.51041458714365));
#392811=CARTESIAN_POINT('Ctrl Pts',(-1.68646901015029,2.17217769452733,
7.51004642900442));
#392812=CARTESIAN_POINT('Ctrl Pts',(-1.69104943757228,2.16860595768131,
7.50729136483009));
#392813=CARTESIAN_POINT('Ctrl Pts',(-1.68047942032504,2.17409240158313,
7.50215815450138));
#392814=CARTESIAN_POINT('Ctrl Pts',(-1.68357470801357,2.17443483202392,
7.49877163671531));
#392815=CARTESIAN_POINT('Ctrl Pts',(-1.68631009160461,2.17233207188445,
7.49481588533172));
#392816=CARTESIAN_POINT('Ctrl Pts',(-1.67379149130792,2.17733690896585,
7.50366171572174));
#392817=CARTESIAN_POINT('Ctrl Pts',(-1.67602317147151,2.18023997043688,
7.50000045605858));
#392818=CARTESIAN_POINT('Ctrl Pts',(-1.67602317147161,2.1802399704368,7.49482233047317));
#392819=CARTESIAN_POINT('Origin',(-1.68336120192778,2.15874994240748,7.51860402984325));
#392820=CARTESIAN_POINT('Origin',(-1.68336120192778,2.15874994240748,9.));
#392821=CARTESIAN_POINT('Origin',(-1.68336120192778,2.15874994240748,8.75721825406948));
#392822=CARTESIAN_POINT('Ctrl Pts',(-1.66296505241367,2.16312506649482,
8.78942910404913));
#392823=CARTESIAN_POINT('Ctrl Pts',(-1.66801889291352,2.165472645014,8.79672699501691));
#392824=CARTESIAN_POINT('Ctrl Pts',(-1.67320190366867,2.15820560397284,
8.79893251111267));
#392825=CARTESIAN_POINT('Ctrl Pts',(-1.67295287420539,2.16772058981616,
8.78111911759583));
#392826=CARTESIAN_POINT('Ctrl Pts',(-1.6789473966294,2.17049692031401,8.78644465894815));
#392827=CARTESIAN_POINT('Ctrl Pts',(-1.68496047887327,2.16506016082846,
8.78817647674132));
#392828=CARTESIAN_POINT('Ctrl Pts',(-1.67917752299136,2.17058462953469,
8.76780923932029));
#392829=CARTESIAN_POINT('Ctrl Pts',(-1.68625594515375,2.17385734651933,
8.76988516158372));
#392830=CARTESIAN_POINT('Ctrl Pts',(-1.69231030965761,2.16933174701751,
8.77093053738832));
#392831=CARTESIAN_POINT('Ctrl Pts',(-1.67796380166912,2.17002618098514,
8.75371302330492));
#392832=CARTESIAN_POINT('Ctrl Pts',(-1.68486817724058,2.17321926716246,
8.75300828287559));
#392833=CARTESIAN_POINT('Ctrl Pts',(-1.69087702405879,2.16849821862961,
8.75267964240737));
#392834=CARTESIAN_POINT('Origin',(-1.67062236339843,2.15288864779704,8.78727029226991));
#392835=CARTESIAN_POINT('Ctrl Pts',(-1.60045004741997,2.13436118528463,
8.85049129520029));
#392836=CARTESIAN_POINT('Ctrl Pts',(-1.60575505664341,2.13680208457839,
8.85711686593484));
#392837=CARTESIAN_POINT('Ctrl Pts',(-1.61100669796544,2.13005515746016,
8.85933012996512));
#392838=CARTESIAN_POINT('Ctrl Pts',(-1.62213069385385,2.14433671451369,
8.82945683644722));
#392839=CARTESIAN_POINT('Ctrl Pts',(-1.62747973786132,2.14679787474737,
8.83607469902389));
#392840=CARTESIAN_POINT('Ctrl Pts',(-1.63271720381484,2.14000810355219,
8.83829567148519));
#392841=CARTESIAN_POINT('Ctrl Pts',(-1.6437790235359,2.15429737441201,8.80838214965002));
#392842=CARTESIAN_POINT('Ctrl Pts',(-1.64914917736843,2.15676824753307,
8.81501364461988));
#392843=CARTESIAN_POINT('Ctrl Pts',(-1.65439449734901,2.14994655925989,
8.81722098428722));
#392844=CARTESIAN_POINT('Ctrl Pts',(-1.66539749203247,2.16424429481555,
8.78727029226991));
#392845=CARTESIAN_POINT('Ctrl Pts',(-1.6707685378652,2.16671557835677,8.79393457792714));
#392846=CARTESIAN_POINT('Ctrl Pts',(-1.6760411057995,2.15987164362912,8.79610912703474));
#392847=CARTESIAN_POINT('Origin',(-1.60567491878594,2.12300553826611,8.85049129520029));
#392848=CARTESIAN_POINT('Ctrl Pts',(-1.59077126558568,2.14158464790051,
8.85049129520029));
#392849=CARTESIAN_POINT('Ctrl Pts',(-1.59160185579971,2.14736489288835,
8.85711686593484));
#392850=CARTESIAN_POINT('Ctrl Pts',(-1.58363955683347,2.15047978570932,
8.85933012996512));
#392851=CARTESIAN_POINT('Ctrl Pts',(-1.59003645441302,2.13647094859848,
8.86332496987231));
#392852=CARTESIAN_POINT('Ctrl Pts',(-1.58650902291588,2.13945576373678,
8.86648636486736));
#392853=CARTESIAN_POINT('Ctrl Pts',(-1.5816008510766,2.13617156656111,8.87206031107456));
#392854=CARTESIAN_POINT('Ctrl Pts',(-1.59572489012279,2.13218708291763,
8.86341338519877));
#392855=CARTESIAN_POINT('Ctrl Pts',(-1.59958467164427,2.1296227979801,8.86654584966058));
#392856=CARTESIAN_POINT('Ctrl Pts',(-1.59776984823888,2.12398093935066,
8.87215952290716));
#392857=CARTESIAN_POINT('Ctrl Pts',(-1.60045004741997,2.13436118528463,
8.85049129520029));
#392858=CARTESIAN_POINT('Ctrl Pts',(-1.60575505664341,2.13680208457839,
8.85711686593484));
#392859=CARTESIAN_POINT('Ctrl Pts',(-1.61100669796544,2.13005515746016,
8.85933012996512));
#392860=CARTESIAN_POINT('Origin',(-1.57839835179838,2.1433625692745,8.85049129520029));
#392861=CARTESIAN_POINT('Ctrl Pts',(-1.6009399023683,2.21235024422325,8.78727029226991));
#392862=CARTESIAN_POINT('Ctrl Pts',(-1.60178083174653,2.21820244154214,
8.79393457792714));
#392863=CARTESIAN_POINT('Ctrl Pts',(-1.59371958050516,2.22130979469259,
8.79610912703474));
#392864=CARTESIAN_POINT('Ctrl Pts',(-1.5975551602087,2.18879514018686,8.80838214965001));
#392865=CARTESIAN_POINT('Ctrl Pts',(-1.59839594992902,2.19464636559803,
8.81501364461995));
#392866=CARTESIAN_POINT('Ctrl Pts',(-1.59036377844289,2.19773392674114,
8.81722098428721));
#392867=CARTESIAN_POINT('Ctrl Pts',(-1.59416574276817,2.16520749992664,
8.82945683644723));
#392868=CARTESIAN_POINT('Ctrl Pts',(-1.59500322738317,2.17103572444267,
8.83607469902388));
#392869=CARTESIAN_POINT('Ctrl Pts',(-1.58700388846103,2.17412483747175,
8.83829567148519));
#392870=CARTESIAN_POINT('Ctrl Pts',(-1.59077126558568,2.14158464790051,
8.85049129520029));
#392871=CARTESIAN_POINT('Ctrl Pts',(-1.59160185579971,2.14736489288835,
8.85711686593484));
#392872=CARTESIAN_POINT('Ctrl Pts',(-1.58363955683347,2.15047978570932,
8.85933012996512));
#392873=CARTESIAN_POINT('Origin',(-1.588566988581,2.21412816559724,8.78727029226991));
#392874=CARTESIAN_POINT('Ctrl Pts',(-1.60290803169131,2.22604698322442,
8.75374538247848));
#392875=CARTESIAN_POINT('Ctrl Pts',(-1.60400184926497,2.23356681975876,
8.75304829418601));
#392876=CARTESIAN_POINT('Ctrl Pts',(-1.5977761367062,2.23798396208662,8.75272238421917));
#392877=CARTESIAN_POINT('Ctrl Pts',(-1.6030957782893,2.22735354670509,8.76769408445021));
#392878=CARTESIAN_POINT('Ctrl Pts',(-1.6042164382461,2.23506271502815,8.76974318093968));
#392879=CARTESIAN_POINT('Ctrl Pts',(-1.59816348603553,2.23957715041,8.77077869880429));
#392880=CARTESIAN_POINT('Ctrl Pts',(-1.60213349619479,2.22065684660117,
8.78108014887988));
#392881=CARTESIAN_POINT('Ctrl Pts',(-1.60308697501544,2.22718954247952,
8.78639403366325));
#392882=CARTESIAN_POINT('Ctrl Pts',(-1.59618455646937,2.23141786294322,
8.78812224174742));
#392883=CARTESIAN_POINT('Ctrl Pts',(-1.60055652823305,2.20968243344755,
8.78944554828686));
#392884=CARTESIAN_POINT('Ctrl Pts',(-1.60136562387221,2.21518713887687,
8.79673892988686));
#392885=CARTESIAN_POINT('Ctrl Pts',(-1.59293408710642,2.21808761161141,
8.79894799272499));
#392886=CARTESIAN_POINT('Origin',(-1.59056147231797,2.22800818059039,8.75721825406948));
#392887=CARTESIAN_POINT('Origin',(-1.59056147231797,2.22800818059039,9.));
#392888=CARTESIAN_POINT('Origin',(-1.59056147231797,2.22800818059039,7.51860402984325));
#392889=CARTESIAN_POINT('Ctrl Pts',(-1.61110290777817,2.22412232015156,
7.50366195182966));
#392890=CARTESIAN_POINT('Ctrl Pts',(-1.61325114344654,2.22708795249951,
7.50000065167735));
#392891=CARTESIAN_POINT('Ctrl Pts',(-1.61325114344644,2.22708795249958,
7.49482233047108));
#392892=CARTESIAN_POINT('Ctrl Pts',(-1.60608447429972,2.22961496296073,
7.50215800491337));
#392893=CARTESIAN_POINT('Ctrl Pts',(-1.60553053494261,2.23268055399069,
7.49877273257265));
#392894=CARTESIAN_POINT('Ctrl Pts',(-1.60273484608023,2.23470571574589,
7.49481816995647));
#392895=CARTESIAN_POINT('Ctrl Pts',(-1.603335619623,2.22902014003883,7.51043025814043));
#392896=CARTESIAN_POINT('Ctrl Pts',(-1.60255251348732,2.23480628744166,
7.51006209594516));
#392897=CARTESIAN_POINT('Ctrl Pts',(-1.59782224944537,2.23818320500886,
7.50731281821701));
#392898=CARTESIAN_POINT('Ctrl Pts',(-1.60293417104173,2.22622876318827,
7.51860402984326));
#392899=CARTESIAN_POINT('Ctrl Pts',(-1.604017376695,2.23376054139155,7.51860402984326));
#392900=CARTESIAN_POINT('Ctrl Pts',(-1.59782431009111,2.23818173392642,
7.51860402984327));
#392901=CARTESIAN_POINT('Origin',(0.,0.,7.5));
#392902=CARTESIAN_POINT('Origin',(-1.72471465490915,2.03526346763209,7.5));
#392903=CARTESIAN_POINT('',(-1.72471465490915,2.03526346763209,7.59394543036555));
#392904=CARTESIAN_POINT('',(-1.72471465490915,2.03526346763209,8.85049129520029));
#392905=CARTESIAN_POINT('',(-1.72471465490915,2.03526346763209,7.5));
#392906=CARTESIAN_POINT('',(-1.73939636646039,2.10523216165203,8.78727029226991));
#392907=CARTESIAN_POINT('Ctrl Pts',(-1.72471465490915,2.03526346763209,
8.85049129520029));
#392908=CARTESIAN_POINT('Ctrl Pts',(-1.72961567252276,2.05862026772969,
8.82945686509571));
#392909=CARTESIAN_POINT('Ctrl Pts',(-1.73450940418106,2.0819423451197,8.80838212259897));
#392910=CARTESIAN_POINT('Ctrl Pts',(-1.73939636646039,2.10523216165203,
8.78727029226991));
#392911=CARTESIAN_POINT('',(-1.74227604793056,2.11895587165397,8.75721825406948));
#392912=CARTESIAN_POINT('Origin',(-1.7336102849198,2.07765642602853,8.7593767971315));
#392913=CARTESIAN_POINT('',(-1.74227604793056,2.11895587165397,7.51860402984325));
#392914=CARTESIAN_POINT('',(-1.74227604793056,2.11895587165397,7.5));
#392915=CARTESIAN_POINT('Ctrl Pts',(-1.74227604793056,2.11895587165397,
7.51860402984325));
#392916=CARTESIAN_POINT('Ctrl Pts',(-1.74001450601092,2.10817803188809,
7.52834476460825));
#392917=CARTESIAN_POINT('Ctrl Pts',(-1.73775149593092,2.09739319530415,
7.53807742314407));
#392918=CARTESIAN_POINT('Ctrl Pts',(-1.73548696839508,2.08660112697468,
7.54780169004674));
#392919=CARTESIAN_POINT('Ctrl Pts',(-1.7319000791656,2.06950707400232,7.5632044032688));
#392920=CARTESIAN_POINT('Ctrl Pts',(-1.7283093782743,2.05239485577747,7.57858609112103));
#392921=CARTESIAN_POINT('Ctrl Pts',(-1.72471465490915,2.03526346763209,
7.59394543036555));
#392922=CARTESIAN_POINT('Origin',(-1.99058637600479,2.12613942982103,7.5));
#392923=CARTESIAN_POINT('',(-1.81372756198701,2.0581283108927,8.75721825406948));
#392924=CARTESIAN_POINT('',(-1.8006393623326,2.05309523912753,8.78727029226991));
#392925=CARTESIAN_POINT('Origin',(-1.76741662995628,2.040319425746,8.75658640621099));
#392926=CARTESIAN_POINT('',(-1.7339107418093,2.0274347247136,8.85049129520029));
#392927=CARTESIAN_POINT('Ctrl Pts',(-1.8006393623326,2.05309523912753,8.78727029226991));
#392928=CARTESIAN_POINT('Ctrl Pts',(-1.77842803837962,2.04455386671524,
8.80838212259896));
#392929=CARTESIAN_POINT('Ctrl Pts',(-1.75618594748781,2.03600066286584,
8.82945686509571));
#392930=CARTESIAN_POINT('Ctrl Pts',(-1.7339107418093,2.0274347247136,8.85049129520029));
#392931=CARTESIAN_POINT('',(-1.7339107418093,2.0274347247136,7.59394543036555));
#392932=CARTESIAN_POINT('',(-1.7339107418093,2.0274347247136,7.5));
#392933=CARTESIAN_POINT('',(-1.81372756198701,2.0581283108927,7.51860402984325));
#392934=CARTESIAN_POINT('Ctrl Pts',(-1.7339107418093,2.0274347247136,7.59394543036555));
#392935=CARTESIAN_POINT('Ctrl Pts',(-1.75024881863927,2.03371753788587,
7.57858609112103));
#392936=CARTESIAN_POINT('Ctrl Pts',(-1.76656861325911,2.03999332062785,
7.56320440326857));
#392937=CARTESIAN_POINT('Ctrl Pts',(-1.78287108381361,2.0462624413944,7.54780169004651));
#392938=CARTESIAN_POINT('Ctrl Pts',(-1.79316339871681,2.05022035469839,
7.53807742314383));
#392939=CARTESIAN_POINT('Ctrl Pts',(-1.80344881675855,2.05417561581188,
7.52834476460825));
#392940=CARTESIAN_POINT('Ctrl Pts',(-1.81372756198701,2.0581283108927,7.51860402984325));
#392941=CARTESIAN_POINT('',(-1.81372756198701,2.0581283108927,7.5));
#392942=CARTESIAN_POINT('Origin',(-1.73144312418161,2.03385161556849,7.5));
#392943=CARTESIAN_POINT('Ctrl Pts',(-1.7339107418093,2.0274347247136,8.85049129520029));
#392944=CARTESIAN_POINT('Ctrl Pts',(-1.7337299847553,2.02736521452512,8.85097269580139));
#392945=CARTESIAN_POINT('Ctrl Pts',(-1.73354848920974,2.02730443226224,
8.85143669361005));
#392946=CARTESIAN_POINT('Ctrl Pts',(-1.73335762024976,2.02725040812869,
8.8519052845931));
#392947=CARTESIAN_POINT('Ctrl Pts',(-1.7329842926685,2.02714474034954,8.85282181883899));
#392948=CARTESIAN_POINT('Ctrl Pts',(-1.73258465538967,2.02706783471854,
8.85372622499636));
#392949=CARTESIAN_POINT('Ctrl Pts',(-1.73214952371882,2.02703362538744,
8.85462257735071));
#392950=CARTESIAN_POINT('Ctrl Pts',(-1.7317882928601,2.02700522601576,8.85536669723986));
#392951=CARTESIAN_POINT('Ctrl Pts',(-1.73140252033164,2.02700621380079,
8.85610498449051));
#392952=CARTESIAN_POINT('Ctrl Pts',(-1.7309869389963,2.02705256355859,8.85681338218371));
#392953=CARTESIAN_POINT('Ctrl Pts',(-1.73060979828179,2.02709462603658,
8.85745625420284));
#392954=CARTESIAN_POINT('Ctrl Pts',(-1.73020331107265,2.02717397960764,
8.85808743050665));
#392955=CARTESIAN_POINT('Ctrl Pts',(-1.72976030302272,2.02731830774889,
8.85866804508409));
#392956=CARTESIAN_POINT('Ctrl Pts',(-1.72955590871171,2.02738489762462,
8.85893592806395));
#392957=CARTESIAN_POINT('Ctrl Pts',(-1.72934370783828,2.02746555882915,
8.85919241173848));
#392958=CARTESIAN_POINT('Ctrl Pts',(-1.72912300557577,2.02756460635873,
8.85943017985534));
#392959=CARTESIAN_POINT('Ctrl Pts',(-1.72882499218653,2.02769834984486,
8.8597512372));
#392960=CARTESIAN_POINT('Ctrl Pts',(-1.72850415527125,2.02786960562472,
8.86004599534706));
#392961=CARTESIAN_POINT('Ctrl Pts',(-1.7281692539677,2.02808550421431,8.86026130871721));
#392962=CARTESIAN_POINT('Ctrl Pts',(-1.7280466371586,2.02816455077479,8.86034014101236));
#392963=CARTESIAN_POINT('Ctrl Pts',(-1.72792028650407,2.02825075870394,
8.86040910639693));
#392964=CARTESIAN_POINT('Ctrl Pts',(-1.72779383394097,2.02834205717922,
8.86046313645507));
#392965=CARTESIAN_POINT('Ctrl Pts',(-1.72759650577527,2.02848452768529,
8.8605474499083));
#392966=CARTESIAN_POINT('Ctrl Pts',(-1.72739362905687,2.02864340258516,
8.86059655985668));
#392967=CARTESIAN_POINT('Ctrl Pts',(-1.72719803426348,2.02880826209859,
8.86059725258816));
#392968=CARTESIAN_POINT('Ctrl Pts',(-1.72700198756798,2.02897350250336,
8.86059794692011));
#392969=CARTESIAN_POINT('Ctrl Pts',(-1.7268127945259,2.02914861917682,8.86056369958366));
#392970=CARTESIAN_POINT('Ctrl Pts',(-1.72663821762604,2.02932129950519,
8.86048590497774));
#392971=CARTESIAN_POINT('Ctrl Pts',(-1.72659265825295,2.02936636392959,
8.86046560290182));
#392972=CARTESIAN_POINT('Ctrl Pts',(-1.72654756531571,2.02941191308586,
8.86044257503091));
#392973=CARTESIAN_POINT('Ctrl Pts',(-1.72650430889525,2.0294565163729,8.86041778462583));
#392974=CARTESIAN_POINT('Ctrl Pts',(-1.72621324686234,2.02975664114657,
8.86025097596201));
#392975=CARTESIAN_POINT('Ctrl Pts',(-1.72596651690997,2.03005444437492,
8.8599848982295));
#392976=CARTESIAN_POINT('Ctrl Pts',(-1.72576479620898,2.03033582864158,
8.85968173251462));
#392977=CARTESIAN_POINT('Ctrl Pts',(-1.72565809751538,2.03048466479724,
8.85952137522077));
#392978=CARTESIAN_POINT('Ctrl Pts',(-1.72556177963352,2.03063166491396,
8.85934740853961));
#392979=CARTESIAN_POINT('Ctrl Pts',(-1.72547590056615,2.03077390398348,
8.8591675900182));
#392980=CARTESIAN_POINT('Ctrl Pts',(-1.72513105147159,2.031345067782,8.85844552518695));
#392981=CARTESIAN_POINT('Ctrl Pts',(-1.72493244153685,2.03187017943457,
8.85759444184125));
#392982=CARTESIAN_POINT('Ctrl Pts',(-1.7248089622409,2.03231287246477,8.85683498915139));
#392983=CARTESIAN_POINT('Ctrl Pts',(-1.72479604046143,2.03235919911139,
8.85675551444999));
#392984=CARTESIAN_POINT('Ctrl Pts',(-1.72478396135505,2.0324046246818,8.85667699793652));
#392985=CARTESIAN_POINT('Ctrl Pts',(-1.72477265656191,2.03244910780657,
8.85659965593547));
#392986=CARTESIAN_POINT('Ctrl Pts',(-1.72462006388734,2.03304954329457,
8.85555568965886));
#392987=CARTESIAN_POINT('Ctrl Pts',(-1.72456012763856,2.03364863640019,
8.85434650606346));
#392988=CARTESIAN_POINT('Ctrl Pts',(-1.72458636765706,2.03424873003681,
8.85297329937117));
#392989=CARTESIAN_POINT('Ctrl Pts',(-1.72460112606864,2.03458624614316,
8.85220095427747));
#392990=CARTESIAN_POINT('Ctrl Pts',(-1.72464346611106,2.03492420287989,
8.85137579139184));
#392991=CARTESIAN_POINT('Ctrl Pts',(-1.72471465490915,2.03526346763209,
8.85049129520029));
#392992=CARTESIAN_POINT('Origin',(-1.73144312418161,2.03385161556849,7.59394543036555));
#392993=CARTESIAN_POINT('Ctrl Pts',(-1.73338594310372,2.0272329131874,7.59443877723642));
#392994=CARTESIAN_POINT('Ctrl Pts',(-1.727981021384,2.02515444864539,7.58783886950016));
#392995=CARTESIAN_POINT('Ctrl Pts',(-1.72318290835979,2.03215853980296,
7.58559994247159));
#392996=CARTESIAN_POINT('Ctrl Pts',(-1.76289125219803,2.03857919014269,
7.56670252222138));
#392997=CARTESIAN_POINT('Ctrl Pts',(-1.75749414212464,2.03650372957206,
7.56004874999027));
#392998=CARTESIAN_POINT('Ctrl Pts',(-1.75264997229472,2.04353724760462,
7.55786368756705));
#392999=CARTESIAN_POINT('Ctrl Pts',(-1.79234146307548,2.04990427905938,
7.53888913333557));
#393000=CARTESIAN_POINT('Ctrl Pts',(-1.78691227771271,2.04781648392494,
7.53222002137276));
#393001=CARTESIAN_POINT('Ctrl Pts',(-1.78206347359232,2.05489402186703,
7.53005029815327));
#393002=CARTESIAN_POINT('Ctrl Pts',(-1.82173524309422,2.06120766746957,
7.51101258149734));
#393003=CARTESIAN_POINT('Ctrl Pts',(-1.81624024613979,2.05909456446447,
7.5043616886572));
#393004=CARTESIAN_POINT('Ctrl Pts',(-1.81142192923624,2.06622837857486,
7.50217374673251));
#393005=CARTESIAN_POINT('',(-1.80985532470036,2.06562356178254,7.50366116523517));
#393006=CARTESIAN_POINT('Ctrl Pts',(-1.81372756198701,2.0581283108927,7.51860402984325));
#393007=CARTESIAN_POINT('Ctrl Pts',(-1.81413974685553,2.05828681672838,
7.51734760759493));
#393008=CARTESIAN_POINT('Ctrl Pts',(-1.81449085986049,2.05848558170951,
7.51608817408572));
#393009=CARTESIAN_POINT('Ctrl Pts',(-1.81477351490122,2.05873576946062,
7.51481005913119));
#393010=CARTESIAN_POINT('Ctrl Pts',(-1.81502955059138,2.058962395504,7.51365231206383));
#393011=CARTESIAN_POINT('Ctrl Pts',(-1.81522994207618,2.05923134692187,
7.51247773061043));
#393012=CARTESIAN_POINT('Ctrl Pts',(-1.81534161211616,2.05956003164914,
7.51129758471022));
#393013=CARTESIAN_POINT('Ctrl Pts',(-1.81548040522265,2.05996854922794,
7.50983079813402));
#393014=CARTESIAN_POINT('Ctrl Pts',(-1.81546538270455,2.06046049291832,
7.50839324291155));
#393015=CARTESIAN_POINT('Ctrl Pts',(-1.81521403373353,2.06103693681455,
7.50715379678855));
#393016=CARTESIAN_POINT('Ctrl Pts',(-1.81509791775136,2.06130323728478,
7.50658120839351));
#393017=CARTESIAN_POINT('Ctrl Pts',(-1.81490614890238,2.06162163084303,
7.50598221009429));
#393018=CARTESIAN_POINT('Ctrl Pts',(-1.81462380586932,2.06197280424467,
7.50545747549611));
#393019=CARTESIAN_POINT('Ctrl Pts',(-1.81447313888754,2.06216020124162,
7.50517746087247));
#393020=CARTESIAN_POINT('Ctrl Pts',(-1.81429520386984,2.06235909162997,
7.50491486231392));
#393021=CARTESIAN_POINT('Ctrl Pts',(-1.81409346969998,2.06256309630028,
7.50468370960993));
#393022=CARTESIAN_POINT('Ctrl Pts',(-1.81379181348259,2.06286814763201,
7.50433806340447));
#393023=CARTESIAN_POINT('Ctrl Pts',(-1.81342750176346,2.06319339024608,
7.50405484070984));
#393024=CARTESIAN_POINT('Ctrl Pts',(-1.81302459315824,2.06351638524513,
7.50385766036131));
#393025=CARTESIAN_POINT('Ctrl Pts',(-1.81298150834553,2.06355092453979,
7.50383657498791));
#393026=CARTESIAN_POINT('Ctrl Pts',(-1.81293801025394,2.06358543411174,
7.50381643264937));
#393027=CARTESIAN_POINT('Ctrl Pts',(-1.81289414874446,2.0636198839193,7.50379723213559));
#393028=CARTESIAN_POINT('Ctrl Pts',(-1.81260135882055,2.06384984765412,
7.50366906242519));
#393029=CARTESIAN_POINT('Ctrl Pts',(-1.81228556199546,2.06408158505075,
7.50358235568538));
#393030=CARTESIAN_POINT('Ctrl Pts',(-1.8119758034555,2.06429763448896,7.5035341175365));
#393031=CARTESIAN_POINT('Ctrl Pts',(-1.81151135558271,2.06462157616948,
7.50346178989176));
#393032=CARTESIAN_POINT('Ctrl Pts',(-1.81099794173554,2.06495031591491,
7.50346967198527));
#393033=CARTESIAN_POINT('Ctrl Pts',(-1.81048399828362,2.06525752798902,
7.50354272648692));
#393034=CARTESIAN_POINT('Ctrl Pts',(-1.81027260270384,2.06538389067401,
7.50357277531559));
#393035=CARTESIAN_POINT('Ctrl Pts',(-1.81006147115135,2.06550656502176,
7.50361331098761));
#393036=CARTESIAN_POINT('Ctrl Pts',(-1.8098553247013,2.06562356178361,7.50366116523658));
#393037=CARTESIAN_POINT('',(-1.73334108842417,2.03608107236531,7.57603338622103));
#393038=CARTESIAN_POINT('Origin',(-1.73906727032659,2.04281177295478,7.58486873427627));
#393039=CARTESIAN_POINT('Ctrl Pts',(-1.80985532475556,2.06562356179811,
7.50366116529969));
#393040=CARTESIAN_POINT('Ctrl Pts',(-1.78439189675398,2.0557929141486,7.52783573079709));
#393041=CARTESIAN_POINT('Ctrl Pts',(-1.75888834908382,2.04594589934544,
7.55196141284069));
#393042=CARTESIAN_POINT('Ctrl Pts',(-1.73334108967201,2.03608107246803,
7.57603338728831));
#393043=CARTESIAN_POINT('Ctrl Pts',(-1.73480751822067,2.02796794848296,
7.59639677331372));
#393044=CARTESIAN_POINT('Ctrl Pts',(-1.71825676553209,2.01836216837365,
7.59974925422225));
#393045=CARTESIAN_POINT('Ctrl Pts',(-1.72509791827961,2.03623385142679,
7.59639677331371));
#393046=CARTESIAN_POINT('Ctrl Pts',(-1.73179248798738,2.02549313601005,
7.58707626057423));
#393047=CARTESIAN_POINT('Ctrl Pts',(-1.72493641503091,2.02620846475782,
7.58811717123965));
#393048=CARTESIAN_POINT('Ctrl Pts',(-1.72313602699776,2.03286248869314,
7.58707626057423));
#393049=CARTESIAN_POINT('Ctrl Pts',(-1.73230984781104,2.03154771866077,
7.58015376756929));
#393050=CARTESIAN_POINT('Ctrl Pts',(-1.72941656890807,2.03147110842991,
7.5820876076604));
#393051=CARTESIAN_POINT('Ctrl Pts',(-1.72903043012316,2.03433952764207,
7.5801537675693));
#393052=CARTESIAN_POINT('Ctrl Pts',(-1.73334108788787,2.03608107173503,
7.57603338509286));
#393053=CARTESIAN_POINT('Ctrl Pts',(-1.73334108788787,2.03608107173503,
7.57603338509286));
#393054=CARTESIAN_POINT('Ctrl Pts',(-1.73334108788787,2.03608107173503,
7.57603338509286));
#393055=CARTESIAN_POINT('Origin',(-1.73907161540578,2.04280807393547,7.58486873427622));
#393056=CARTESIAN_POINT('Ctrl Pts',(-1.74404347607192,2.12737891132436,
7.51098857897448));
#393057=CARTESIAN_POINT('Ctrl Pts',(-1.7428344547023,2.1216170731368,7.50433767179956));
#393058=CARTESIAN_POINT('Ctrl Pts',(-1.75064586560078,2.11799907495306,
7.50214974420965));
#393059=CARTESIAN_POINT('Ctrl Pts',(-1.73757436099932,2.09654902262136,
7.53887321589166));
#393060=CARTESIAN_POINT('Ctrl Pts',(-1.73637982585133,2.09085622148072,
7.53220407452062));
#393061=CARTESIAN_POINT('Ctrl Pts',(-1.74414053150148,2.08719912321378,
7.53003438070911));
#393062=CARTESIAN_POINT('Ctrl Pts',(-1.73109282283944,2.06565992915942,
7.56669465659232));
#393063=CARTESIAN_POINT('Ctrl Pts',(-1.72990534717204,2.06000077141513,
7.56004085833301));
#393064=CARTESIAN_POINT('Ctrl Pts',(-1.73762184485837,2.05634122040666,
7.55785582193789));
#393065=CARTESIAN_POINT('Ctrl Pts',(-1.72459915472629,2.03471302792852,
7.59443891967696));
#393066=CARTESIAN_POINT('Ctrl Pts',(-1.72340995736706,2.02904566511007,
7.58783901202978));
#393067=CARTESIAN_POINT('Ctrl Pts',(-1.73109004667146,2.0254269075519,7.58560008491213));
#393068=CARTESIAN_POINT('',(-1.75029323173563,2.11632951079881,7.50366116523517));
#393069=CARTESIAN_POINT('Ctrl Pts',(-1.75029323173586,2.1163295107991,7.50366116523554));
#393070=CARTESIAN_POINT('Ctrl Pts',(-1.74981871703962,2.11692025043702,
7.50350835821027));
#393071=CARTESIAN_POINT('Ctrl Pts',(-1.7493633037674,2.11744784570105,7.50345484956));
#393072=CARTESIAN_POINT('Ctrl Pts',(-1.74891390668696,2.11792837480992,
7.50349758195598));
#393073=CARTESIAN_POINT('Ctrl Pts',(-1.74868333265654,2.11817492187974,
7.50351950684424));
#393074=CARTESIAN_POINT('Ctrl Pts',(-1.74843171059763,2.11843346810349,
7.50357029184312));
#393075=CARTESIAN_POINT('Ctrl Pts',(-1.74818222121562,2.11867611166749,
7.50365515313923));
#393076=CARTESIAN_POINT('Ctrl Pts',(-1.74779840551787,2.11904939572501,
7.50378570417639));
#393077=CARTESIAN_POINT('Ctrl Pts',(-1.74740861269543,2.11939624934591,
7.50400001621911));
#393078=CARTESIAN_POINT('Ctrl Pts',(-1.74704100235902,2.11968857580534,
7.50428903009634));
#393079=CARTESIAN_POINT('Ctrl Pts',(-1.7470002004399,2.11972102179331,7.50432110841318));
#393080=CARTESIAN_POINT('Ctrl Pts',(-1.74695966296946,2.11975282504803,
7.50435406373354));
#393081=CARTESIAN_POINT('Ctrl Pts',(-1.7469194216477,2.11978396847005,7.50438785222352));
#393082=CARTESIAN_POINT('Ctrl Pts',(-1.74667372903594,2.11997411403091,
7.50459414719561));
#393083=CARTESIAN_POINT('Ctrl Pts',(-1.74643484859306,2.12014228251918,
7.50483629897752));
#393084=CARTESIAN_POINT('Ctrl Pts',(-1.74621268932908,2.12028310756563,
7.5050991045531));
#393085=CARTESIAN_POINT('Ctrl Pts',(-1.74572258367895,2.12059378176262,
7.50567888004914));
#393086=CARTESIAN_POINT('Ctrl Pts',(-1.74529482357481,2.12078406050336,
7.50637912803144));
#393087=CARTESIAN_POINT('Ctrl Pts',(-1.74493416304264,2.12088448585053,
7.50710440483569));
#393088=CARTESIAN_POINT('Ctrl Pts',(-1.74484572192004,2.12090911213938,
7.50728225710685));
#393089=CARTESIAN_POINT('Ctrl Pts',(-1.74475959423715,2.12092896612878,
7.50746498566954));
#393090=CARTESIAN_POINT('Ctrl Pts',(-1.74467788407099,2.12094399030944,
7.50764697238949));
#393091=CARTESIAN_POINT('Ctrl Pts',(-1.74423863270495,2.12102475616989,
7.50862528291181));
#393092=CARTESIAN_POINT('Ctrl Pts',(-1.74388791488077,2.12097735070585,
7.50965856837421));
#393093=CARTESIAN_POINT('Ctrl Pts',(-1.74359952217745,2.12086267149125,
7.51067959873202));
#393094=CARTESIAN_POINT('Ctrl Pts',(-1.74344081930905,2.1207995633748,7.51124147302578));
#393095=CARTESIAN_POINT('Ctrl Pts',(-1.7433011122352,2.12071566358396,7.51180065547253));
#393096=CARTESIAN_POINT('Ctrl Pts',(-1.74317712839623,2.12061863513828,
7.51235175716501));
#393097=CARTESIAN_POINT('Ctrl Pts',(-1.7427487148433,2.12028336320691,7.51425603304536));
#393098=CARTESIAN_POINT('Ctrl Pts',(-1.74246069049901,2.11974658727157,
7.51626900505181));
#393099=CARTESIAN_POINT('Ctrl Pts',(-1.74230085887294,2.11906741666329,
7.51827788969245));
#393100=CARTESIAN_POINT('Ctrl Pts',(-1.7422922084833,2.11903065866652,7.51838661432546));
#393101=CARTESIAN_POINT('Ctrl Pts',(-1.74228393829289,2.11899347478669,
7.51849533314857));
#393102=CARTESIAN_POINT('Ctrl Pts',(-1.74227604793055,2.11895587165397,
7.51860402984325));
#393103=CARTESIAN_POINT('Ctrl Pts',(-1.733341088327,2.03608107361461,7.57603338728985));
#393104=CARTESIAN_POINT('Ctrl Pts',(-1.73900212579773,2.06287528806228,
7.55196141284922));
#393105=CARTESIAN_POINT('Ctrl Pts',(-1.74465255590613,2.0896235082857,7.52783573083105));
#393106=CARTESIAN_POINT('Ctrl Pts',(-1.75029323174249,2.11632951085759,
7.50366116530176));
#393107=CARTESIAN_POINT('Origin',(-5.98949470795634E-16,7.03560129586916E-16,
7.49482233047033));
#393108=CARTESIAN_POINT('Origin',(-1.80403047455413,2.05897554547887,7.49482233047033));
#393109=CARTESIAN_POINT('Origin',(0.,0.,7.50366116523517));
#393110=CARTESIAN_POINT('Origin',(-1.74466007661672,2.10951830213908,7.49482233047033));
#393111=CARTESIAN_POINT('Ctrl Pts',(-1.81372657476299,2.05812793120741,
7.51860402984325));
#393112=CARTESIAN_POINT('Ctrl Pts',(-1.82082828860746,2.06085958757332,
7.51860402984325));
#393113=CARTESIAN_POINT('Ctrl Pts',(-1.82651648716081,2.05580580846776,
7.51860402984325));
#393114=CARTESIAN_POINT('Ctrl Pts',(-1.81636349003426,2.05914221267185,
7.51041458714367));
#393115=CARTESIAN_POINT('Ctrl Pts',(-1.82217588142127,2.0596622820176,7.51004642900443));
#393116=CARTESIAN_POINT('Ctrl Pts',(-1.82651805589842,2.05580441469549,
7.5072913648301));
#393117=CARTESIAN_POINT('Ctrl Pts',(-1.81632127355297,2.06195680944013,
7.50215815450137));
#393118=CARTESIAN_POINT('Ctrl Pts',(-1.81943214123462,2.06210022055774,
7.49877163671531));
#393119=CARTESIAN_POINT('Ctrl Pts',(-1.82202718038202,2.05982652413607,
7.4948158853317));
#393120=CARTESIAN_POINT('Ctrl Pts',(-1.80985496190502,2.06562314771778,
7.50366171572174));
#393121=CARTESIAN_POINT('Ctrl Pts',(-1.81226805662943,2.06837726029866,
7.50000045605858));
#393122=CARTESIAN_POINT('Ctrl Pts',(-1.81226805662953,2.06837726029858,
7.49482233047317));
#393123=CARTESIAN_POINT('Origin',(-1.81821413949189,2.04646123661108,7.51860402984325));
#393124=CARTESIAN_POINT('Origin',(-1.81821413949189,2.04646123661108,9.));
#393125=CARTESIAN_POINT('Origin',(-1.81821413949189,2.04646123661108,8.75721825406948));
#393126=CARTESIAN_POINT('Ctrl Pts',(-1.79814021121715,2.05213415732288,
8.78942910404912));
#393127=CARTESIAN_POINT('Ctrl Pts',(-1.80333407793182,2.05415311181765,
8.7967269950169));
#393128=CARTESIAN_POINT('Ctrl Pts',(-1.80804083871739,2.04656892505245,
8.79893251111267));
#393129=CARTESIAN_POINT('Ctrl Pts',(-1.80840194814796,2.05608031670937,
8.78111911759582));
#393130=CARTESIAN_POINT('Ctrl Pts',(-1.8145620342885,2.05846687256809,8.78644465894816));
#393131=CARTESIAN_POINT('Ctrl Pts',(-1.82021442763375,2.05265602398583,
8.78817647674131));
#393132=CARTESIAN_POINT('Ctrl Pts',(-1.81479730738017,2.05853965733411,
8.7678092393203));
#393133=CARTESIAN_POINT('Ctrl Pts',(-1.8220708698622,2.06135213410563,8.76988516158372));
#393134=CARTESIAN_POINT('Ctrl Pts',(-1.82782283886924,2.05644792846779,
8.77093053738833));
#393135=CARTESIAN_POINT('Ctrl Pts',(-1.81355029985716,2.05806011956911,
8.75371302330492));
#393136=CARTESIAN_POINT('Ctrl Pts',(-1.82064507138233,2.06080428034674,
8.75300828287559));
#393137=CARTESIAN_POINT('Ctrl Pts',(-1.82633909376226,2.05570794357694,
8.75267964240737));
#393138=CARTESIAN_POINT('Origin',(-1.80512593983748,2.04142816484592,8.78727029226991));
#393139=CARTESIAN_POINT('Ctrl Pts',(-1.7339107418093,2.0274347247136,8.85049129520029));
#393140=CARTESIAN_POINT('Ctrl Pts',(-1.73936124027703,2.02953071581004,
8.85711686593484));
#393141=CARTESIAN_POINT('Ctrl Pts',(-1.74416981443406,2.02246117716241,
8.85933012996512));
#393142=CARTESIAN_POINT('Ctrl Pts',(-1.75618597738197,2.03600067436165,
8.82945683644724));
#393143=CARTESIAN_POINT('Ctrl Pts',(-1.76168171828244,2.03811406345141,
8.83607469902391));
#393144=CARTESIAN_POINT('Ctrl Pts',(-1.76647340116633,2.03100267697357,
8.8382956714852));
#393145=CARTESIAN_POINT('Ctrl Pts',(-1.77842800991975,2.04455385577099,
8.80838214965002));
#393146=CARTESIAN_POINT('Ctrl Pts',(-1.78394543957973,2.04667558528088,
8.81501364461994));
#393147=CARTESIAN_POINT('Ctrl Pts',(-1.7887429154195,2.03953184409285,8.8172209842872));
#393148=CARTESIAN_POINT('Ctrl Pts',(-1.8006393623326,2.05309523912753,8.78727029226991));
#393149=CARTESIAN_POINT('Ctrl Pts',(-1.80615770845575,2.05521732106364,
8.79393457792714));
#393150=CARTESIAN_POINT('Ctrl Pts',(-1.81098095093021,2.04804963334648,
8.79610912703474));
#393151=CARTESIAN_POINT('Origin',(-1.73839731931418,2.01576765043199,8.85049129520029));
#393152=CARTESIAN_POINT('Ctrl Pts',(-1.72471465490915,2.03526346763209,
8.85049129520029));
#393153=CARTESIAN_POINT('Ctrl Pts',(-1.72591388015442,2.04097862038895,
8.85711686593484));
#393154=CARTESIAN_POINT('Ctrl Pts',(-1.71816751245362,2.04459725957487,
8.85933012996512));
#393155=CARTESIAN_POINT('Ctrl Pts',(-1.72365371764566,2.0302073544872,8.86332496987232));
#393156=CARTESIAN_POINT('Ctrl Pts',(-1.72032477139737,2.03341204031466,
8.86648636486737));
#393157=CARTESIAN_POINT('Ctrl Pts',(-1.71521626468801,2.03044905852376,
8.87206031107457));
#393158=CARTESIAN_POINT('Ctrl Pts',(-1.72905599763765,2.02556783114056,
8.86341338519876));
#393159=CARTESIAN_POINT('Ctrl Pts',(-1.73274355452398,2.02276151775032,
8.86654584966059));
#393160=CARTESIAN_POINT('Ctrl Pts',(-1.73057098474443,2.01724752705932,
8.87215952290714));
#393161=CARTESIAN_POINT('Ctrl Pts',(-1.7339107418093,2.0274347247136,8.85049129520029));
#393162=CARTESIAN_POINT('Ctrl Pts',(-1.73936124027703,2.02953071581004,
8.85711686593484));
#393163=CARTESIAN_POINT('Ctrl Pts',(-1.74416981443406,2.02246117716241,
8.85933012996512));
#393164=CARTESIAN_POINT('Origin',(-1.71248107441376,2.0378304713841,8.85049129520029));
#393165=CARTESIAN_POINT('Ctrl Pts',(-1.73939636646039,2.10523216165203,
8.78727029226991));
#393166=CARTESIAN_POINT('Ctrl Pts',(-1.74061051962861,2.11101845647363,
8.79393457792714));
#393167=CARTESIAN_POINT('Ctrl Pts',(-1.73276491989239,2.11463591137413,
8.79610912703474));
#393168=CARTESIAN_POINT('Ctrl Pts',(-1.73450939791929,2.08194231527793,
8.80838214965004));
#393169=CARTESIAN_POINT('Ctrl Pts',(-1.73572334944619,2.08772764913661,
8.81501364461994));
#393170=CARTESIAN_POINT('Ctrl Pts',(-1.72790550163946,2.09132348954825,
8.81722098428721));
#393171=CARTESIAN_POINT('Ctrl Pts',(-1.7296156791001,2.05862029907538,8.82945683644722));
#393172=CARTESIAN_POINT('Ctrl Pts',(-1.73082485863997,2.06438289105556,
8.83607469902388));
#393173=CARTESIAN_POINT('Ctrl Pts',(-1.72303987536891,2.06797817657505,
8.83829567148519));
#393174=CARTESIAN_POINT('Ctrl Pts',(-1.72471465490915,2.03526346763209,
8.85049129520029));
#393175=CARTESIAN_POINT('Ctrl Pts',(-1.72591388015442,2.04097862038895,
8.85711686593484));
#393176=CARTESIAN_POINT('Ctrl Pts',(-1.71816751245362,2.04459725957487,
8.85933012996512));
#393177=CARTESIAN_POINT('Origin',(-1.727162785965,2.10779916540404,8.78727029226991));
#393178=CARTESIAN_POINT('Ctrl Pts',(-1.74223800513144,2.11877466075529,
8.75374538247848));
#393179=CARTESIAN_POINT('Ctrl Pts',(-1.74381137292056,2.1262089658464,8.75304829418602));
#393180=CARTESIAN_POINT('Ctrl Pts',(-1.73788145903658,2.13101591545478,
8.75272238421917));
#393181=CARTESIAN_POINT('Ctrl Pts',(-1.74250907779354,2.12006651079531,
8.76769408445018));
#393182=CARTESIAN_POINT('Ctrl Pts',(-1.74412136334459,2.12768803887528,
8.76974318093967));
#393183=CARTESIAN_POINT('Ctrl Pts',(-1.73837008844153,2.13258101284514,
8.7707786988043));
#393184=CARTESIAN_POINT('Ctrl Pts',(-1.741119713762,2.11344522340548,8.78108014887992));
#393185=CARTESIAN_POINT('Ctrl Pts',(-1.74248978482014,2.11990340756173,
8.78639403366326));
#393186=CARTESIAN_POINT('Ctrl Pts',(-1.7358724574555,2.12456527996219,8.78812224174741));
#393187=CARTESIAN_POINT('Ctrl Pts',(-1.73884285278514,2.10259439504487,
8.78944554828685));
#393188=CARTESIAN_POINT('Ctrl Pts',(-1.74000297373832,2.10803595153093,
8.79673892988686));
#393189=CARTESIAN_POINT('Ctrl Pts',(-1.73177459439526,2.11147067534852,
8.79894799272499));
#393190=CARTESIAN_POINT('Origin',(-1.73004246743517,2.12152287540598,8.75721825406948));
#393191=CARTESIAN_POINT('Origin',(-1.73004246743517,2.12152287540598,9.));
#393192=CARTESIAN_POINT('Origin',(-1.73004246743517,2.12152287540598,7.51860402984325));
#393193=CARTESIAN_POINT('Ctrl Pts',(-1.75029273038002,2.11632890459552,
7.50366195182966));
#393194=CARTESIAN_POINT('Ctrl Pts',(-1.75262656098472,2.11915080580191,
7.50000065167735));
#393195=CARTESIAN_POINT('Ctrl Pts',(-1.75262656098463,2.11915080580198,
7.49482233047108));
#393196=CARTESIAN_POINT('Ctrl Pts',(-1.74563652264444,2.12213179431787,
7.50215800491336));
#393197=CARTESIAN_POINT('Ctrl Pts',(-1.74528013450682,2.12522657777876,
7.49877273257264));
#393198=CARTESIAN_POINT('Ctrl Pts',(-1.7426199422462,2.12742669902233,7.49481816995649));
#393199=CARTESIAN_POINT('Ctrl Pts',(-1.74285520534901,2.1217143132473,7.51043025814042));
#393200=CARTESIAN_POINT('Ctrl Pts',(-1.74244442792582,2.12753874617212,
7.51006209594515));
#393201=CARTESIAN_POINT('Ctrl Pts',(-1.73794024257004,2.13121179455774,
7.50731281821698));
#393202=CARTESIAN_POINT('Ctrl Pts',(-1.74227573745804,2.11895439247877,
7.51860402984325));
#393203=CARTESIAN_POINT('Ctrl Pts',(-1.74383928023545,2.12640129461146,
7.51860402984325));
#393204=CARTESIAN_POINT('Ctrl Pts',(-1.73794220472939,2.13121019447176,
7.51860402984325));
#393205=CARTESIAN_POINT('Origin',(0.,0.,7.5));
#393206=CARTESIAN_POINT('Origin',(-1.85157082176547,1.92057895321253,7.5));
#393207=CARTESIAN_POINT('',(-1.85157082176547,1.92057895321253,7.59394543036555));
#393208=CARTESIAN_POINT('',(-1.85157082176547,1.92057895321253,8.85049129520029));
#393209=CARTESIAN_POINT('',(-1.85157082176547,1.92057895321253,7.5));
#393210=CARTESIAN_POINT('',(-1.87070527778333,1.98946322855771,8.78727029226991));
#393211=CARTESIAN_POINT('Ctrl Pts',(-1.85157082176547,1.92057895321253,
8.85049129520029));
#393212=CARTESIAN_POINT('Ctrl Pts',(-1.85795824503306,1.94357375498269,
8.82945686509571));
#393213=CARTESIAN_POINT('Ctrl Pts',(-1.8643361726236,1.96653437219952,8.80838212259895));
#393214=CARTESIAN_POINT('Ctrl Pts',(-1.87070527778333,1.98946322855771,
8.78727029226991));
#393215=CARTESIAN_POINT('',(-1.87445832375786,2.00297423990032,8.75721825406948));
#393216=CARTESIAN_POINT('Origin',(-1.86316430092012,1.96231486575702,8.75937679713127));
#393217=CARTESIAN_POINT('',(-1.87445832375786,2.00297423990032,7.51860402984325));
#393218=CARTESIAN_POINT('',(-1.87445832375786,2.00297423990032,7.5));
#393219=CARTESIAN_POINT('Ctrl Pts',(-1.87445832375786,2.00297423990032,
7.51860402984325));
#393220=CARTESIAN_POINT('Ctrl Pts',(-1.87151088985393,1.99236344185043,
7.52834476460825));
#393221=CARTESIAN_POINT('Ctrl Pts',(-1.86856154251845,1.98174575542357,
7.53807742314407));
#393222=CARTESIAN_POINT('Ctrl Pts',(-1.86561021750539,1.9711209493333,7.54780169004674));
#393223=CARTESIAN_POINT('Ctrl Pts',(-1.86093547819022,1.95429183070809,
7.5632044032688));
#393224=CARTESIAN_POINT('Ctrl Pts',(-1.85625577119299,1.93744482836685,
7.57858609112103));
#393225=CARTESIAN_POINT('Ctrl Pts',(-1.85157082176547,1.92057895321253,
7.59394543036555));
#393226=CARTESIAN_POINT('Origin',(-2.12271872378387,1.99423374133349,7.5));
#393227=CARTESIAN_POINT('',(-1.94186579781666,1.93769374166281,8.75721825406948));
#393228=CARTESIAN_POINT('',(-1.92848201925698,1.93350957471439,8.78727029226991));
#393229=CARTESIAN_POINT('Origin',(-1.89450899737115,1.92288859838258,8.75658640621016));
#393230=CARTESIAN_POINT('',(-1.86024642503785,1.91217709997534,8.85049129520029));
#393231=CARTESIAN_POINT('Ctrl Pts',(-1.92848201925698,1.93350957471439,
8.78727029226991));
#393232=CARTESIAN_POINT('Ctrl Pts',(-1.90576908324182,1.92640883587951,
8.80838212259896));
#393233=CARTESIAN_POINT('Ctrl Pts',(-1.88302468545904,1.91929826116101,
8.82945686509571));
#393234=CARTESIAN_POINT('Ctrl Pts',(-1.86024642503785,1.91217709997534,
8.85049129520029));
#393235=CARTESIAN_POINT('',(-1.86024642503785,1.91217709997534,7.59394543036555));
#393236=CARTESIAN_POINT('',(-1.86024642503785,1.91217709997534,7.5));
#393237=CARTESIAN_POINT('',(-1.94186579781666,1.93769374166281,7.51860402984325));
#393238=CARTESIAN_POINT('Ctrl Pts',(-1.86024642503785,1.91217709997534,
7.59394543036555));
#393239=CARTESIAN_POINT('Ctrl Pts',(-1.87695347475876,1.91740022025756,
7.57858609112103));
#393240=CARTESIAN_POINT('Ctrl Pts',(-1.89364182939109,1.92261749589948,
7.56320440326857));
#393241=CARTESIAN_POINT('Ctrl Pts',(-1.910312468718,1.92782923321041,7.54780169004651));
#393242=CARTESIAN_POINT('Ctrl Pts',(-1.92083722133244,1.93111958367707,
7.53807742314383));
#393243=CARTESIAN_POINT('Ctrl Pts',(-1.93135492132932,1.93440772928588,
7.52834476460825));
#393244=CARTESIAN_POINT('Ctrl Pts',(-1.94186579781666,1.93769374166281,
7.51860402984325));
#393245=CARTESIAN_POINT('',(-1.94186579781666,1.93769374166281,7.5));
#393246=CARTESIAN_POINT('Origin',(-1.85819500900389,1.91873890744399,7.5));
#393247=CARTESIAN_POINT('Ctrl Pts',(-1.86024642503785,1.91217709997534,
8.85049129520029));
#393248=CARTESIAN_POINT('Ctrl Pts',(-1.86006158583553,1.91211931374721,
8.85097269580138));
#393249=CARTESIAN_POINT('Ctrl Pts',(-1.85987656885909,1.91207028482754,
8.85143669361005));
#393250=CARTESIAN_POINT('Ctrl Pts',(-1.85968263072173,1.91202860070861,
8.8519052845931));
#393251=CARTESIAN_POINT('Ctrl Pts',(-1.85930330002417,1.91194706921551,
8.85282181883899));
#393252=CARTESIAN_POINT('Ctrl Pts',(-1.85889955648229,1.91189592644375,
8.85372622499635));
#393253=CARTESIAN_POINT('Ctrl Pts',(-1.85846312703677,1.91188966638125,
8.85462257735071));
#393254=CARTESIAN_POINT('Ctrl Pts',(-1.85810081881159,1.91188446949971,
8.85536669723986));
#393255=CARTESIAN_POINT('Ctrl Pts',(-1.85771590218177,1.91191017178599,
8.85610498449051));
#393256=CARTESIAN_POINT('Ctrl Pts',(-1.85730414434203,1.91198305270082,
8.85681338218371));
#393257=CARTESIAN_POINT('Ctrl Pts',(-1.85693047345579,1.91204919224548,
8.85745625420284));
#393258=CARTESIAN_POINT('Ctrl Pts',(-1.85652990561897,1.91215442650103,
8.85808743050665));
#393259=CARTESIAN_POINT('Ctrl Pts',(-1.85609705491234,1.91232684172785,
8.8586680450841));
#393260=CARTESIAN_POINT('Ctrl Pts',(-1.85589734697935,1.912406390376,8.85893592806395));
#393261=CARTESIAN_POINT('Ctrl Pts',(-1.8556907500765,1.91250048161008,8.85919241173848));
#393262=CARTESIAN_POINT('Ctrl Pts',(-1.85547684726747,1.91261346607839,
8.85943017985534));
#393263=CARTESIAN_POINT('Ctrl Pts',(-1.85518801515327,1.9127660285576,8.8597512372));
#393264=CARTESIAN_POINT('Ctrl Pts',(-1.85487880982734,1.91295748856583,
8.86004599534706));
#393265=CARTESIAN_POINT('Ctrl Pts',(-1.85455842928456,1.9131944007688,8.86026130871721));
#393266=CARTESIAN_POINT('Ctrl Pts',(-1.85444112893537,1.91328114100557,
8.86034014101235));
#393267=CARTESIAN_POINT('Ctrl Pts',(-1.85432056124279,1.91337526712552,
8.86040910639693));
#393268=CARTESIAN_POINT('Ctrl Pts',(-1.85420021800343,1.91347447986183,
8.86046313645507));
#393269=CARTESIAN_POINT('Ctrl Pts',(-1.85401242338628,1.91362930050595,
8.8605474499083));
#393270=CARTESIAN_POINT('Ctrl Pts',(-1.85382014264964,1.91380084733627,
8.86059655985668));
#393271=CARTESIAN_POINT('Ctrl Pts',(-1.85363551231202,1.91397789992959,
8.86059725258816));
#393272=CARTESIAN_POINT('Ctrl Pts',(-1.85345045540457,1.91415536158513,
8.86059794692011));
#393273=CARTESIAN_POINT('Ctrl Pts',(-1.85327287084368,1.91434224010243,
8.86056369958366));
#393274=CARTESIAN_POINT('Ctrl Pts',(-1.8531097162974,1.91452575082093,8.86048590497774));
#393275=CARTESIAN_POINT('Ctrl Pts',(-1.85306713781852,1.91457364165468,
8.86046560290182));
#393276=CARTESIAN_POINT('Ctrl Pts',(-1.85302505587401,1.91462198633974,
8.86044257503091));
#393277=CARTESIAN_POINT('Ctrl Pts',(-1.85298474607093,1.91466926943291,
8.86041778462583));
#393278=CARTESIAN_POINT('Ctrl Pts',(-1.85271351111645,1.91498742597652,
8.86025097596201));
#393279=CARTESIAN_POINT('Ctrl Pts',(-1.85248636841558,1.91530042537853,
8.8599848982295));
#393280=CARTESIAN_POINT('Ctrl Pts',(-1.85230309052327,1.91559415580072,
8.85968173251461));
#393281=CARTESIAN_POINT('Ctrl Pts',(-1.85220614701881,1.91574952236531,
8.85952137522076));
#393282=CARTESIAN_POINT('Ctrl Pts',(-1.85211944536218,1.9159023915624,8.85934740853961));
#393283=CARTESIAN_POINT('Ctrl Pts',(-1.85204285603104,1.91604984067723,
8.8591675900182));
#393284=CARTESIAN_POINT('Ctrl Pts',(-1.85173531005615,1.91664192551583,
8.85844552518695));
#393285=CARTESIAN_POINT('Ctrl Pts',(-1.85157075220591,1.9171786832524,8.85759444184124));
#393286=CARTESIAN_POINT('Ctrl Pts',(-1.85147589005125,1.91762837806794,
8.85683498915138));
#393287=CARTESIAN_POINT('Ctrl Pts',(-1.8514659629794,1.91767543743275,8.85675551444998));
#393288=CARTESIAN_POINT('Ctrl Pts',(-1.85145681911712,1.91772154358246,
8.85667699793651));
#393289=CARTESIAN_POINT('Ctrl Pts',(-1.85144838759449,1.91776665961246,
8.85659965593547));
#393290=CARTESIAN_POINT('Ctrl Pts',(-1.85133457847174,1.91837563808757,
8.85555568965886));
#393291=CARTESIAN_POINT('Ctrl Pts',(-1.85131314939547,1.91897734042081,
8.85434650606346));
#393292=CARTESIAN_POINT('Ctrl Pts',(-1.85137778363235,1.91957451989693,
8.85297329937118));
#393293=CARTESIAN_POINT('Ctrl Pts',(-1.85141413645237,1.91991039696557,
8.85220095427747));
#393294=CARTESIAN_POINT('Ctrl Pts',(-1.85147804246509,1.9202449465981,8.85137579139184));
#393295=CARTESIAN_POINT('Ctrl Pts',(-1.85157082176547,1.92057895321253,
8.85049129520029));
#393296=CARTESIAN_POINT('Origin',(-1.85819500900389,1.91873890744399,7.59394543036555));
#393297=CARTESIAN_POINT('Ctrl Pts',(-1.85970977447861,1.91200932706108,
7.59443877723642));
#393298=CARTESIAN_POINT('Ctrl Pts',(-1.85418279006981,1.91028142747094,
7.58783886950016));
#393299=CARTESIAN_POINT('Ctrl Pts',(-1.84984328894464,1.917578544129,7.58559994247159));
#393300=CARTESIAN_POINT('Ctrl Pts',(-1.88988142021143,1.92144188022921,
7.56670252222137));
#393301=CARTESIAN_POINT('Ctrl Pts',(-1.88436242386422,1.91971647794457,
7.56004874999028));
#393302=CARTESIAN_POINT('Ctrl Pts',(-1.87997884594832,1.92704591188663,
7.55786368756704));
#393303=CARTESIAN_POINT('Ctrl Pts',(-1.91999672341034,1.93085681904672,
7.5388891333356));
#393304=CARTESIAN_POINT('Ctrl Pts',(-1.91444492739764,1.9291211626118,7.53222002137279));
#393305=CARTESIAN_POINT('Ctrl Pts',(-1.91005954507819,1.93649482293976,
7.53005029815327));
#393306=CARTESIAN_POINT('Ctrl Pts',(-1.9500543213375,1.94025371748126,7.51101258149734));
#393307=CARTESIAN_POINT('Ctrl Pts',(-1.94443522746927,1.93849702173658,
7.5043616886572));
#393308=CARTESIAN_POINT('Ctrl Pts',(-1.94008387535392,1.94592488928473,
7.50217374673251));
#393309=CARTESIAN_POINT('',(-1.93848173883014,1.94542168785061,7.50366116523517));
#393310=CARTESIAN_POINT('Ctrl Pts',(-1.94186579781667,1.93769374166281,
7.51860402984325));
#393311=CARTESIAN_POINT('Ctrl Pts',(-1.94228729131093,1.93782551305605,
7.51734760759494));
#393312=CARTESIAN_POINT('Ctrl Pts',(-1.94265041783263,1.93800137376575,
7.51608817408572));
#393313=CARTESIAN_POINT('Ctrl Pts',(-1.94294852171251,1.93823293770865,
7.51481005913119));
#393314=CARTESIAN_POINT('Ctrl Pts',(-1.94321855133033,1.93844269386153,
7.51365231206383));
#393315=CARTESIAN_POINT('Ctrl Pts',(-1.94343576286585,1.93869825356335,
7.51247773061042));
#393316=CARTESIAN_POINT('Ctrl Pts',(-1.94356826237053,1.93901910824857,
7.51129758471022));
#393317=CARTESIAN_POINT('Ctrl Pts',(-1.94373294412284,1.93941789397932,
7.50983079813402));
#393318=CARTESIAN_POINT('Ctrl Pts',(-1.94374947141057,1.93990978941468,
7.50839324291155));
#393319=CARTESIAN_POINT('Ctrl Pts',(-1.94353557175021,1.94050115292896,
7.50715379678855));
#393320=CARTESIAN_POINT('Ctrl Pts',(-1.94343675627049,1.94077434583283,
7.50658120839351));
#393321=CARTESIAN_POINT('Ctrl Pts',(-1.94326578097649,1.94110437188971,
7.50598221009429));
#393322=CARTESIAN_POINT('Ctrl Pts',(-1.94300651780457,1.94147291354817,
7.50545747549611));
#393323=CARTESIAN_POINT('Ctrl Pts',(-1.94286816695108,1.94166957878456,
7.50517746087247));
#393324=CARTESIAN_POINT('Ctrl Pts',(-1.9427033404709,1.941879460867,7.50491486231392));
#393325=CARTESIAN_POINT('Ctrl Pts',(-1.94251509140962,1.94209597154048,
7.50468370960992));
#393326=CARTESIAN_POINT('Ctrl Pts',(-1.94223359968321,1.94241972329174,
7.50433806340447));
#393327=CARTESIAN_POINT('Ctrl Pts',(-1.94189087484742,1.94276763919197,
7.50405484070984));
#393328=CARTESIAN_POINT('Ctrl Pts',(-1.94150948842178,1.94311578500611,
7.50385766036131));
#393329=CARTESIAN_POINT('Ctrl Pts',(-1.94146870507165,1.94315301378952,
7.50383657498791));
#393330=CARTESIAN_POINT('Ctrl Pts',(-1.94142750738742,1.94319023939014,
7.50381643264937));
#393331=CARTESIAN_POINT('Ctrl Pts',(-1.94138594320286,1.94322742863344,
7.50379723213559));
#393332=CARTESIAN_POINT('Ctrl Pts',(-1.94110848867433,1.94347567899794,
7.50366906242519));
#393333=CARTESIAN_POINT('Ctrl Pts',(-1.94080818815367,1.94372717343729,
7.50358235568538));
#393334=CARTESIAN_POINT('Ctrl Pts',(-1.94051290838087,1.94396262527655,
7.5035341175365));
#393335=CARTESIAN_POINT('Ctrl Pts',(-1.94007016978078,1.94431565866153,
7.50346178989176));
#393336=CARTESIAN_POINT('Ctrl Pts',(-1.93957887322524,1.94467661751402,
7.50346967198527));
#393337=CARTESIAN_POINT('Ctrl Pts',(-1.93908566887042,1.945016126858,7.50354272648692));
#393338=CARTESIAN_POINT('Ctrl Pts',(-1.93888280371056,1.9451557740786,7.50357277531559));
#393339=CARTESIAN_POINT('Ctrl Pts',(-1.93867996572294,1.94529172362375,
7.50361331098761));
#393340=CARTESIAN_POINT('Ctrl Pts',(-1.93848173883115,1.94542168785162,
7.50366116523658));
#393341=CARTESIAN_POINT('',(-1.86023191546276,1.92084218059618,7.57603338622103));
#393342=CARTESIAN_POINT('Origin',(-1.86637756977754,1.92719217450495,7.58486873427628));
#393343=CARTESIAN_POINT('Ctrl Pts',(-1.93848173888622,1.94542168786261,
7.50366116529968));
#393344=CARTESIAN_POINT('Ctrl Pts',(-1.91244077647095,1.93724268576656,
7.52783573079709));
#393345=CARTESIAN_POINT('Ctrl Pts',(-1.88635872817013,1.92904992062092,
7.55196141284068));
#393346=CARTESIAN_POINT('Ctrl Pts',(-1.86023191671462,1.92084218061874,
7.57603338728831));
#393347=CARTESIAN_POINT('Ctrl Pts',(-1.86117552269009,1.91265177151732,
7.59639677331371));
#393348=CARTESIAN_POINT('Ctrl Pts',(-1.84404333085321,1.90412613787907,
7.59974925422226));
#393349=CARTESIAN_POINT('Ctrl Pts',(-1.85201547038344,1.92152278748121,
7.59639677331371));
#393350=CARTESIAN_POINT('Ctrl Pts',(-1.85800812538022,1.91037521746236,
7.58707626057423));
#393351=CARTESIAN_POINT('Ctrl Pts',(-1.85121197023118,1.91152834659303,
7.58811717123965));
#393352=CARTESIAN_POINT('Ctrl Pts',(-1.84984160606564,1.91828405037989,
7.58707626057423));
#393353=CARTESIAN_POINT('Ctrl Pts',(-1.85891234067498,1.91638421296596,
7.58015376756929));
#393354=CARTESIAN_POINT('Ctrl Pts',(-1.85602009788945,1.91649313315483,
7.5820876076604));
#393355=CARTESIAN_POINT('Ctrl Pts',(-1.85581853271804,1.91938039888895,
7.58015376756929));
#393356=CARTESIAN_POINT('Ctrl Pts',(-1.86023191488718,1.92084218000156,
7.57603338509286));
#393357=CARTESIAN_POINT('Ctrl Pts',(-1.86023191488718,1.92084218000156,
7.57603338509286));
#393358=CARTESIAN_POINT('Ctrl Pts',(-1.86023191488718,1.92084218000156,
7.57603338509286));
#393359=CARTESIAN_POINT('Origin',(-1.86638166893224,1.92718820469566,7.58486873427622));
#393360=CARTESIAN_POINT('Ctrl Pts',(-1.87676178653313,2.01126673402251,
7.51098857897448));
#393361=CARTESIAN_POINT('Ctrl Pts',(-1.87518608698741,2.00559419641458,
7.50433767179956));
#393362=CARTESIAN_POINT('Ctrl Pts',(-1.88274964256491,2.00148315298151,
7.50214974420965));
#393363=CARTESIAN_POINT('Ctrl Pts',(-1.86833068520009,1.98091466625814,
7.53887321589167));
#393364=CARTESIAN_POINT('Ctrl Pts',(-1.86677386533128,1.97531009571769,
7.5322040745206));
#393365=CARTESIAN_POINT('Ctrl Pts',(-1.87428431468887,1.97116328123316,
7.53003438070911));
#393366=CARTESIAN_POINT('Ctrl Pts',(-1.85988339304239,1.95050431132728,
7.56669465659234));
#393367=CARTESIAN_POINT('Ctrl Pts',(-1.85833577368953,1.94493286275673,
7.560040858333));
#393368=CARTESIAN_POINT('Ctrl Pts',(-1.86580194876562,1.94078643298405,
7.55785582193789));
#393369=CARTESIAN_POINT('Ctrl Pts',(-1.85142029209722,1.92003704456849,
7.59443891967696));
#393370=CARTESIAN_POINT('Ctrl Pts',(-1.84987042888903,1.91445751809118,
7.58783901202978));
#393371=CARTESIAN_POINT('Ctrl Pts',(-1.85730288403345,1.91035413064732,
7.58560008491213));
#393372=CARTESIAN_POINT('',(-1.88229076388122,1.99983961245519,7.50366116523517));
#393373=CARTESIAN_POINT('Ctrl Pts',(-1.88229076388148,1.99983961245546,
7.50366116523554));
#393374=CARTESIAN_POINT('Ctrl Pts',(-1.88185507294512,2.00045954061641,
7.50350835821027));
#393375=CARTESIAN_POINT('Ctrl Pts',(-1.88143439851294,2.00101523030793,
7.50345484955999));
#393376=CARTESIAN_POINT('Ctrl Pts',(-1.88101671237271,2.00152356508801,
7.50349758195598));
#393377=CARTESIAN_POINT('Ctrl Pts',(-1.88080240840636,2.00178437852928,
7.50351950684424));
#393378=CARTESIAN_POINT('Ctrl Pts',(-1.88056786844539,2.00205851502274,
7.50357029184312));
#393379=CARTESIAN_POINT('Ctrl Pts',(-1.8803344378926,2.00231664488911,7.50365515313923));
#393380=CARTESIAN_POINT('Ctrl Pts',(-1.87997532717705,2.00271375315069,
7.50378570417639));
#393381=CARTESIAN_POINT('Ctrl Pts',(-1.87960855821355,2.00308486823551,
7.50400001621911));
#393382=CARTESIAN_POINT('Ctrl Pts',(-1.87926043259256,2.00340014695399,
7.50428903009634));
#393383=CARTESIAN_POINT('Ctrl Pts',(-1.87922179332695,2.00343514046614,
7.50432110841317));
#393384=CARTESIAN_POINT('Ctrl Pts',(-1.87918337678662,2.0034694756223,7.50435406373354));
#393385=CARTESIAN_POINT('Ctrl Pts',(-1.87914521351087,2.00350313332716,
7.50438785222352));
#393386=CARTESIAN_POINT('Ctrl Pts',(-1.87891220836884,2.00370862979325,
7.50459414719561));
#393387=CARTESIAN_POINT('Ctrl Pts',(-1.87868459332349,2.00389175788386,
7.50483629897752));
#393388=CARTESIAN_POINT('Ctrl Pts',(-1.87847191320124,2.00404652738306,
7.5050991045531));
#393389=CARTESIAN_POINT('Ctrl Pts',(-1.87800271948988,2.00438796444341,
7.50567888004914));
#393390=CARTESIAN_POINT('Ctrl Pts',(-1.87758802946553,2.00460525892004,
7.50637912803144));
#393391=CARTESIAN_POINT('Ctrl Pts',(-1.87723454422319,2.0047285855322,7.50710440483569));
#393392=CARTESIAN_POINT('Ctrl Pts',(-1.8771478626241,2.00475882766588,7.50728225710685));
#393393=CARTESIAN_POINT('Ctrl Pts',(-1.87706318394925,2.00478415908272,
7.50746498566954));
#393394=CARTESIAN_POINT('Ctrl Pts',(-1.87698260426795,2.00480438758291,
7.50764697238949));
#393395=CARTESIAN_POINT('Ctrl Pts',(-1.87654943007739,2.00491313043288,
7.50862528291182));
#393396=CARTESIAN_POINT('Ctrl Pts',(-1.87619639556209,2.0048882929366,7.50965856837422));
#393397=CARTESIAN_POINT('Ctrl Pts',(-1.87590124787,2.00479232672669,7.51067959873202));
#393398=CARTESIAN_POINT('Ctrl Pts',(-1.87573882772276,2.00473951640032,
7.51124147302578));
#393399=CARTESIAN_POINT('Ctrl Pts',(-1.87559403221403,2.00466474005356,
7.51180065547253));
#393400=CARTESIAN_POINT('Ctrl Pts',(-1.87546408647929,2.00457585463506,
7.51235175716501));
#393401=CARTESIAN_POINT('Ctrl Pts',(-1.87501507220155,2.00426872010641,
7.51425603304536));
#393402=CARTESIAN_POINT('Ctrl Pts',(-1.87469324828192,2.00375150081789,
7.5162690050518));
#393403=CARTESIAN_POINT('Ctrl Pts',(-1.87449023043679,2.00308396608592,
7.51827788969243));
#393404=CARTESIAN_POINT('Ctrl Pts',(-1.87447924272736,2.00304783784476,
7.51838661432545));
#393405=CARTESIAN_POINT('Ctrl Pts',(-1.87446860714958,2.00301126023612,
7.51849533314856));
#393406=CARTESIAN_POINT('Ctrl Pts',(-1.87445832375785,2.00297423990032,
7.51860402984325));
#393407=CARTESIAN_POINT('Ctrl Pts',(-1.86023191544584,1.92084218184914,
7.57603338728985));
#393408=CARTESIAN_POINT('Ctrl Pts',(-1.86759803292181,1.94721864079349,
7.55196141284922));
#393409=CARTESIAN_POINT('Ctrl Pts',(-1.87495061796934,1.9735498796297,7.52783573083105));
#393410=CARTESIAN_POINT('Ctrl Pts',(-1.88229076389183,1.99983961251341,
7.50366116530176));
#393411=CARTESIAN_POINT('Origin',(-6.42796117143048E-16,6.63739765492884E-16,
7.49482233047033));
#393412=CARTESIAN_POINT('Origin',(-1.93224291659624,1.93916053003965,7.49482233047033));
#393413=CARTESIAN_POINT('Origin',(0.,0.,7.50366116523517));
#393414=CARTESIAN_POINT('Origin',(-1.87623278704649,1.99340331564181,7.49482233047033));
#393415=CARTESIAN_POINT('Ctrl Pts',(-1.94186478829449,1.93769342600929,
7.51860402984325));
#393416=CARTESIAN_POINT('Ctrl Pts',(-1.94912692873048,1.93996446152597,
7.51860402984325));
#393417=CARTESIAN_POINT('Ctrl Pts',(-1.95447964353081,1.93455662181898,
7.51860402984325));
#393418=CARTESIAN_POINT('Ctrl Pts',(-1.94456127097707,1.93853667578217,
7.51041458714366));
#393419=CARTESIAN_POINT('Ctrl Pts',(-1.95039504113998,1.93868327539491,
7.51004642900443));
#393420=CARTESIAN_POINT('Ctrl Pts',(-1.954481119746,1.934555130401,7.5072913648301));
#393421=CARTESIAN_POINT('Ctrl Pts',(-1.94469947306816,1.94134819447877,
7.50215815450137));
#393422=CARTESIAN_POINT('Ctrl Pts',(-1.94781313752039,1.94129199696616,
7.49877163671529));
#393423=CARTESIAN_POINT('Ctrl Pts',(-1.95025716865163,1.93885670736862,
7.4948158853317));
#393424=CARTESIAN_POINT('Ctrl Pts',(-1.93848135025098,1.94542129788097,
7.50366171572174));
#393425=CARTESIAN_POINT('Ctrl Pts',(-1.94106594361239,1.94801514433234,
7.50000045605858));
#393426=CARTESIAN_POINT('Ctrl Pts',(-1.94106594361248,1.94801514433226,
7.49482233047317));
#393427=CARTESIAN_POINT('Origin',(-1.94559564515113,1.9257631826289,7.51860402984325));
#393428=CARTESIAN_POINT('Origin',(-1.94559564515113,1.9257631826289,9.));
#393429=CARTESIAN_POINT('Origin',(-1.94559564515113,1.9257631826289,8.75721825406948));
#393430=CARTESIAN_POINT('Ctrl Pts',(-1.92592642619289,1.93271058871712,
8.78942910404913));
#393431=CARTESIAN_POINT('Ctrl Pts',(-1.93123897640996,1.93439262287038,
8.79672699501691));
#393432=CARTESIAN_POINT('Ctrl Pts',(-1.93545014613627,1.92652245543136,
8.79893251111267));
#393433=CARTESIAN_POINT('Ctrl Pts',(-1.93641991058457,1.93599116855338,
8.78111911759582));
#393434=CARTESIAN_POINT('Ctrl Pts',(-1.94272024732632,1.937978142903,8.78644465894813));
#393435=CARTESIAN_POINT('Ctrl Pts',(-1.9479887248763,1.93181708324733,8.78817647674132));
#393436=CARTESIAN_POINT('Ctrl Pts',(-1.94295970036018,1.93803570412618,
8.7678092393203));
#393437=CARTESIAN_POINT('Ctrl Pts',(-1.95039851453345,1.94037638361425,
8.76988516158374));
#393438=CARTESIAN_POINT('Ctrl Pts',(-1.95582445196923,1.93511372427327,
8.77093053738833));
#393439=CARTESIAN_POINT('Ctrl Pts',(-1.94168453085777,1.93763704766926,
8.75371302330492));
#393440=CARTESIAN_POINT('Ctrl Pts',(-1.94894054439861,1.93992100670194,
8.75300828287559));
#393441=CARTESIAN_POINT('Ctrl Pts',(-1.95429634438094,1.93447032363616,
8.75267964240738));
#393442=CARTESIAN_POINT('Origin',(-1.93221186659144,1.92157901568048,8.78727029226991));
#393443=CARTESIAN_POINT('Ctrl Pts',(-1.86024642503785,1.91217709997534,
8.85049129520029));
#393444=CARTESIAN_POINT('Ctrl Pts',(-1.86582001548254,1.91391956999744,
8.85711686593484));
#393445=CARTESIAN_POINT('Ctrl Pts',(-1.87016576301193,1.90655647007114,
8.85933012996512));
#393446=CARTESIAN_POINT('Ctrl Pts',(-1.88302471602832,1.91929827071788,
8.82945683644722));
#393447=CARTESIAN_POINT('Ctrl Pts',(-1.88864457064355,1.92105520429467,
8.8360746990239));
#393448=CARTESIAN_POINT('Ctrl Pts',(-1.89297078040507,1.91365142474657,
8.83829567148519));
#393449=CARTESIAN_POINT('Ctrl Pts',(-1.90576905413921,1.92640882678117,
8.80838214965003));
#393450=CARTESIAN_POINT('Ctrl Pts',(-1.91141108732462,1.92817269403818,
8.81501364461988));
#393451=CARTESIAN_POINT('Ctrl Pts',(-1.91574100516639,1.92073625510017,
8.81722098428721));
#393452=CARTESIAN_POINT('Ctrl Pts',(-1.92848201925698,1.93350957471439,
8.78727029226991));
#393453=CARTESIAN_POINT('Ctrl Pts',(-1.93412498960264,1.93527373495553,
8.79393457792714));
#393454=CARTESIAN_POINT('Ctrl Pts',(-1.93847908687936,1.92781174781516,
8.79610912703474));
#393455=CARTESIAN_POINT('Origin',(-1.86397627237231,1.90024654094143,8.85049129520029));
#393456=CARTESIAN_POINT('Ctrl Pts',(-1.85157082176547,1.92057895321253,
8.85049129520029));
#393457=CARTESIAN_POINT('Ctrl Pts',(-1.85313375416821,1.92620552894983,
8.85711686593484));
#393458=CARTESIAN_POINT('Ctrl Pts',(-1.84563514921932,1.93031304473609,
8.85933012996512));
#393459=CARTESIAN_POINT('Ctrl Pts',(-1.85018811802993,1.91560120287823,
8.86332496987232));
#393460=CARTESIAN_POINT('Ctrl Pts',(-1.84707133638466,1.91901259065339,
8.86648636486738));
#393461=CARTESIAN_POINT('Ctrl Pts',(-1.84178348675509,1.91638299977499,
8.87206031107456));
#393462=CARTESIAN_POINT('Ctrl Pts',(-1.85528204317686,1.9106250866624,8.86341338519876));
#393463=CARTESIAN_POINT('Ctrl Pts',(-1.85878222246584,1.90758827656308,
8.86654584966058));
#393464=CARTESIAN_POINT('Ctrl Pts',(-1.85626083386736,1.90222481198104,
8.87215952290715));
#393465=CARTESIAN_POINT('Ctrl Pts',(-1.86024642503785,1.91217709997534,
8.85049129520029));
#393466=CARTESIAN_POINT('Ctrl Pts',(-1.86582001548254,1.91391956999744,
8.85711686593484));
#393467=CARTESIAN_POINT('Ctrl Pts',(-1.87016576301193,1.90655647007114,
8.85933012996512));
#393468=CARTESIAN_POINT('Origin',(-1.83952684496834,1.92392449097351,8.85049129520029));
#393469=CARTESIAN_POINT('Ctrl Pts',(-1.87070527778333,1.98946322855771,
8.78727029226991));
#393470=CARTESIAN_POINT('Ctrl Pts',(-1.87228766552576,1.99515984375544,
8.79393457792714));
#393471=CARTESIAN_POINT('Ctrl Pts',(-1.86468995654687,1.99927253550785,
8.79610912703474));
#393472=CARTESIAN_POINT('Ctrl Pts',(-1.86433616446272,1.96653434282026,
8.80838214965001));
#393473=CARTESIAN_POINT('Ctrl Pts',(-1.86591828940899,1.97223001194868,
8.81501364461992));
#393474=CARTESIAN_POINT('Ctrl Pts',(-1.85834689049526,1.97631935554929,
8.81722098428721));
#393475=CARTESIAN_POINT('Ctrl Pts',(-1.85795825360522,1.94357378584257,
8.82945683644724));
#393476=CARTESIAN_POINT('Ctrl Pts',(-1.85953415929187,1.94924706556038,
8.8360746990239));
#393477=CARTESIAN_POINT('Ctrl Pts',(-1.85199552183799,1.95333374977089,
8.83829567148519));
#393478=CARTESIAN_POINT('Ctrl Pts',(-1.85157082176547,1.92057895321253,
8.85049129520029));
#393479=CARTESIAN_POINT('Ctrl Pts',(-1.85313375416821,1.92620552894983,
8.85711686593484));
#393480=CARTESIAN_POINT('Ctrl Pts',(-1.84563514921932,1.93031304473609,
8.85933012996512));
#393481=CARTESIAN_POINT('Origin',(-1.8586613009862,1.99280876631869,8.78727029226991));
#393482=CARTESIAN_POINT('Ctrl Pts',(-1.87440874889961,2.00279583872935,
8.75374538247848));
#393483=CARTESIAN_POINT('Ctrl Pts',(-1.87645520159846,2.01011406322297,
8.75304829418601));
#393484=CARTESIAN_POINT('Ctrl Pts',(-1.87084545367738,2.01529106732486,
8.75272238421917));
#393485=CARTESIAN_POINT('Ctrl Pts',(-1.8747620337301,2.00406766683986,8.76769408445021));
#393486=CARTESIAN_POINT('Ctrl Pts',(-1.87685931964825,2.01157023618307,
8.7697431809397));
#393487=CARTESIAN_POINT('Ctrl Pts',(-1.87143335527489,2.01682164246132,
8.7707786988043));
#393488=CARTESIAN_POINT('Ctrl Pts',(-1.87295129695634,1.99754900045418,
8.78108014887987));
#393489=CARTESIAN_POINT('Ctrl Pts',(-1.87473233033612,2.00390613482436,
8.78639403366323));
#393490=CARTESIAN_POINT('Ctrl Pts',(-1.8684272861705,2.00898240252795,8.78812224174741));
#393491=CARTESIAN_POINT('Ctrl Pts',(-1.86998389907453,1.98686634526788,
8.78944554828685));
#393492=CARTESIAN_POINT('Ctrl Pts',(-1.87149027815589,1.99222239228786,
8.79673892988686));
#393493=CARTESIAN_POINT('Ctrl Pts',(-1.86349886841123,1.99617725317158,
8.79894799272499));
#393494=CARTESIAN_POINT('Origin',(-1.86241434696072,2.0063197776613,8.75721825406948));
#393495=CARTESIAN_POINT('Origin',(-1.86241434696072,2.0063197776613,9.));
#393496=CARTESIAN_POINT('Origin',(-1.86241434696072,2.0063197776613,7.51860402984325));
#393497=CARTESIAN_POINT('Ctrl Pts',(-1.88229022471613,1.99983903961938,
7.50366195182966));
#393498=CARTESIAN_POINT('Ctrl Pts',(-1.88480006004661,2.00250561388684,
7.50000065167735));
#393499=CARTESIAN_POINT('Ctrl Pts',(-1.88480006004652,2.00250561388692,
7.49482233047108));
#393500=CARTESIAN_POINT('Ctrl Pts',(-1.87801537607974,2.00592833093633,
7.50215800491337));
#393501=CARTESIAN_POINT('Ctrl Pts',(-1.87785800363691,2.00903958969905,
7.49877273257265));
#393502=CARTESIAN_POINT('Ctrl Pts',(-1.87534423927865,2.0114056296609,7.49481816995647));
#393503=CARTESIAN_POINT('Ctrl Pts',(-1.87521302519497,2.00568990723636,
7.51043025814042));
#393504=CARTESIAN_POINT('Ctrl Pts',(-1.87517626445679,2.01152869183891,
7.51006209594515));
#393505=CARTESIAN_POINT('Ctrl Pts',(-1.87091666645098,2.01548277769927,
7.50731281821699));
#393506=CARTESIAN_POINT('Ctrl Pts',(-1.87445791915216,2.00297278365629,
7.51860402984325));
#393507=CARTESIAN_POINT('Ctrl Pts',(-1.87649537412106,2.01030420880017,
7.51860402984325));
#393508=CARTESIAN_POINT('Ctrl Pts',(-1.870918522061,2.01548105518487,7.51860402984325));
#393509=CARTESIAN_POINT('Origin',(0.,0.,7.5));
#393510=CARTESIAN_POINT('Origin',(-1.97081848695446,1.79800236791132,7.5));
#393511=CARTESIAN_POINT('',(-1.97081848695446,1.79800236791132,7.59394543036555));
#393512=CARTESIAN_POINT('',(-1.97081848695446,1.79800236791132,8.85049129520029));
#393513=CARTESIAN_POINT('',(-1.97081848695446,1.79800236791132,7.5));
#393514=CARTESIAN_POINT('',(-1.99432705985485,1.86551916431871,8.78727029226991));
#393515=CARTESIAN_POINT('Ctrl Pts',(-1.97081848695446,1.79800236791132,
8.85049129520029));
#393516=CARTESIAN_POINT('Ctrl Pts',(-1.97866606858372,1.8205406807812,8.82945686509571));
#393517=CARTESIAN_POINT('Ctrl Pts',(-1.98650198383397,1.84304548772369,
8.80838212259895));
#393518=CARTESIAN_POINT('Ctrl Pts',(-1.99432705985485,1.86551916431871,
8.78727029226991));
#393519=CARTESIAN_POINT('',(-1.99893804826279,1.87876195735828,8.75721825406948));
#393520=CARTESIAN_POINT('Origin',(-1.98506217516061,1.83890973278755,8.7593767971313));
#393521=CARTESIAN_POINT('',(-1.99893804826279,1.87876195735828,7.51860402984325));
#393522=CARTESIAN_POINT('',(-1.99893804826279,1.87876195735828,7.5));
#393523=CARTESIAN_POINT('Ctrl Pts',(-1.99893804826279,1.87876195735828,
7.51860402984325));
#393524=CARTESIAN_POINT('Ctrl Pts',(-1.9953168340127,1.8683618030696,7.52834476460825));
#393525=CARTESIAN_POINT('Ctrl Pts',(-1.99169326892258,1.85795489715083,
7.53807742314407));
#393526=CARTESIAN_POINT('Ctrl Pts',(-1.98806727405984,1.847541012907,7.54780169004674));
#393527=CARTESIAN_POINT('Ctrl Pts',(-1.98232389416555,1.8310459830872,7.5632044032688));
#393528=CARTESIAN_POINT('Ctrl Pts',(-1.97657441098222,1.81453342457586,
7.57858609112103));
#393529=CARTESIAN_POINT('Ctrl Pts',(-1.97081848695446,1.79800236791132,
7.59394543036555));
#393530=CARTESIAN_POINT('Origin',(-2.24612836500518,1.85413331864101,7.5));
#393531=CARTESIAN_POINT('',(-2.06202449055418,1.80929677321442,8.75721825406948));
#393532=CARTESIAN_POINT('',(-2.04840012990613,1.80597870472224,8.78727029226991));
#393533=CARTESIAN_POINT('Origin',(-2.01381642094786,1.79755620931114,8.75658640621029));
#393534=CARTESIAN_POINT('',(-1.9789379566843,1.78906192937258,8.85049129520029));
#393535=CARTESIAN_POINT('Ctrl Pts',(-2.04840012990613,1.80597870472224,
8.78727029226991));
#393536=CARTESIAN_POINT('Ctrl Pts',(-2.0252789141548,1.80034777792375,8.80838212259897));
#393537=CARTESIAN_POINT('Ctrl Pts',(-2.00212567109019,1.79470905121289,
8.82945686509571));
#393538=CARTESIAN_POINT('Ctrl Pts',(-1.9789379566843,1.78906192937258,8.85049129520029));
#393539=CARTESIAN_POINT('',(-1.9789379566843,1.78906192937258,7.59394543036555));
#393540=CARTESIAN_POINT('',(-1.9789379566843,1.78906192937258,7.5));
#393541=CARTESIAN_POINT('',(-2.06202449055418,1.80929677321442,7.51860402984325));
#393542=CARTESIAN_POINT('Ctrl Pts',(-1.9789379566843,1.78906192937258,7.59394543036555));
#393543=CARTESIAN_POINT('Ctrl Pts',(-1.99594532644521,1.79320389384316,
7.57858609112103));
#393544=CARTESIAN_POINT('Ctrl Pts',(-2.0129336650612,1.79734122348031,7.56320440326857));
#393545=CARTESIAN_POINT('Ctrl Pts',(-2.02990396992769,1.80147416118908,
7.54780169004651));
#393546=CARTESIAN_POINT('Ctrl Pts',(-2.04061791178732,1.80408342806257,
7.53807742314383));
#393547=CARTESIAN_POINT('Ctrl Pts',(-2.05132467425402,1.80669094647108,
7.52834476460825));
#393548=CARTESIAN_POINT('Ctrl Pts',(-2.06202449055418,1.80929677321442,
7.51860402984324));
#393549=CARTESIAN_POINT('',(-2.06202449055418,1.80929677321442,7.5));
#393550=CARTESIAN_POINT('Origin',(-1.97731117195259,1.7957416895806,7.5));
#393551=CARTESIAN_POINT('Ctrl Pts',(-1.9789379566843,1.78906192937258,8.85049129520029));
#393552=CARTESIAN_POINT('Ctrl Pts',(-1.97874979487761,1.78901610456081,
8.85097269580138));
#393553=CARTESIAN_POINT('Ctrl Pts',(-1.97856201674471,1.78897903045469,
8.85143669361005));
#393554=CARTESIAN_POINT('Ctrl Pts',(-1.97836580636339,1.78894985763938,
8.8519052845931));
#393555=CARTESIAN_POINT('Ctrl Pts',(-1.97798203130074,1.78889279746271,
8.85282181883899));
#393556=CARTESIAN_POINT('Ctrl Pts',(-1.97757584056463,1.7888676277068,8.85372622499636));
#393557=CARTESIAN_POINT('Ctrl Pts',(-1.97713990672662,1.78888934263686,
8.85462257735071));
#393558=CARTESIAN_POINT('Ctrl Pts',(-1.97677800993721,1.78890736960055,
8.85536669723986));
#393559=CARTESIAN_POINT('Ctrl Pts',(-1.97639553091103,1.78895768077188,
8.85610498449051));
#393560=CARTESIAN_POINT('Ctrl Pts',(-1.97598928856817,1.78905679336042,
8.85681338218371));
#393561=CARTESIAN_POINT('Ctrl Pts',(-1.97562062300402,1.78914673819018,
8.85745625420284));
#393562=CARTESIAN_POINT('Ctrl Pts',(-1.97522762055868,1.78927742070009,
8.85808743050666));
#393563=CARTESIAN_POINT('Ctrl Pts',(-1.97480670587176,1.78947721452132,
8.85866804508411));
#393564=CARTESIAN_POINT('Ctrl Pts',(-1.97461250495953,1.78956939505944,
8.85893592806396));
#393565=CARTESIAN_POINT('Ctrl Pts',(-1.97441236097823,1.789676529682,8.85919241173848));
#393566=CARTESIAN_POINT('Ctrl Pts',(-1.97420613659521,1.78980298681164,
8.85943017985534));
#393567=CARTESIAN_POINT('Ctrl Pts',(-1.97392767262917,1.78997374137196,
8.8597512372));
#393568=CARTESIAN_POINT('Ctrl Pts',(-1.97363136948358,1.79018461885832,
8.86004599534705));
#393569=CARTESIAN_POINT('Ctrl Pts',(-1.97332682621395,1.79044157115162,
8.86026130871721));
#393570=CARTESIAN_POINT('Ctrl Pts',(-1.97321532433696,1.79053564863045,
8.86034014101235));
#393571=CARTESIAN_POINT('Ctrl Pts',(-1.97310103504485,1.79063730615677,
8.86040910639692));
#393572=CARTESIAN_POINT('Ctrl Pts',(-1.97298729564542,1.79074402546769,
8.86046313645506));
#393573=CARTESIAN_POINT('Ctrl Pts',(-1.97280980626518,1.79091056005862,
8.86054744990829));
#393574=CARTESIAN_POINT('Ctrl Pts',(-1.97262891163309,1.79109407389668,
8.86059655985668));
#393575=CARTESIAN_POINT('Ctrl Pts',(-1.97245600443691,1.79128259202281,
8.86059725258816));
#393576=CARTESIAN_POINT('Ctrl Pts',(-1.97228269775603,1.79147154570111,
8.86059794692011));
#393577=CARTESIAN_POINT('Ctrl Pts',(-1.97211745140937,1.79166941813833,
8.86056369958366));
#393578=CARTESIAN_POINT('Ctrl Pts',(-1.97196638965371,1.79186300516205,
8.86048590497774));
#393579=CARTESIAN_POINT('Ctrl Pts',(-1.97192696703313,1.79191352561146,
8.86046560290182));
#393580=CARTESIAN_POINT('Ctrl Pts',(-1.9718880690051,1.79196446716662,8.86044257503091));
#393581=CARTESIAN_POINT('Ctrl Pts',(-1.97185087146101,1.79201423576956,
8.86041778462583));
#393582=CARTESIAN_POINT('Ctrl Pts',(-1.97160057814757,1.79234911670963,
8.860250975962));
#393583=CARTESIAN_POINT('Ctrl Pts',(-1.97139395607629,1.79267602610361,
8.8599848982295));
#393584=CARTESIAN_POINT('Ctrl Pts',(-1.97122987412082,1.79298089568002,
8.85968173251461));
#393585=CARTESIAN_POINT('Ctrl Pts',(-1.97114308416716,1.793142154219,8.85952137522076));
#393586=CARTESIAN_POINT('Ctrl Pts',(-1.97106635501147,1.79330026432413,
8.85934740853961));
#393587=CARTESIAN_POINT('Ctrl Pts',(-1.97099937013855,1.79345231758424,
8.8591675900182));
#393588=CARTESIAN_POINT('Ctrl Pts',(-1.97073039105571,1.7940628904593,8.85844552518695));
#393589=CARTESIAN_POINT('Ctrl Pts',(-1.97060056149348,1.7946090886272,8.85759444184124));
#393590=CARTESIAN_POINT('Ctrl Pts',(-1.97053470628904,1.79506393733563,
8.85683498915138));
#393591=CARTESIAN_POINT('Ctrl Pts',(-1.97052781471729,1.79511153604161,
8.85675551444998));
#393592=CARTESIAN_POINT('Ctrl Pts',(-1.97052164367321,1.79515813331055,
8.85667699793651));
#393593=CARTESIAN_POINT('Ctrl Pts',(-1.97051612006801,1.79520369685434,
8.85659965593547));
#393594=CARTESIAN_POINT('Ctrl Pts',(-1.97044156216317,1.7958187158934,8.85555568965886));
#393595=CARTESIAN_POINT('Ctrl Pts',(-1.97045872831609,1.79642055493028,
8.85434650606346));
#393596=CARTESIAN_POINT('Ctrl Pts',(-1.9705614911754,1.79701236630735,8.85297329937117));
#393597=CARTESIAN_POINT('Ctrl Pts',(-1.97061928902233,1.79734522414735,
8.85220095427747));
#393598=CARTESIAN_POINT('Ctrl Pts',(-1.97070449840185,1.79767499193949,
8.85137579139183));
#393599=CARTESIAN_POINT('Ctrl Pts',(-1.97081848695446,1.79800236791132,
8.85049129520029));
#393600=CARTESIAN_POINT('Origin',(-1.97731117195259,1.7957416895806,7.59394543036555));
#393601=CARTESIAN_POINT('Ctrl Pts',(-1.97839165948368,1.78892888448515,
7.59443877723642));
#393602=CARTESIAN_POINT('Ctrl Pts',(-1.97276532395027,1.78755865015694,
7.58783886950016));
#393603=CARTESIAN_POINT('Ctrl Pts',(-1.96890226666507,1.7951188068979,7.58559994247159));
#393604=CARTESIAN_POINT('Ctrl Pts',(-2.00910566009089,1.79640895348187,
7.56670252222136));
#393605=CARTESIAN_POINT('Ctrl Pts',(-2.00348745620966,1.7950406995313,7.56004874999026));
#393606=CARTESIAN_POINT('Ctrl Pts',(-1.99958248326974,1.80263593116663,
7.55786368756705));
#393607=CARTESIAN_POINT('Ctrl Pts',(-2.03976230537066,1.80387505419709,
7.53888913333558));
#393608=CARTESIAN_POINT('Ctrl Pts',(-2.03411071222869,1.80249866864629,
7.53222002137278));
#393609=CARTESIAN_POINT('Ctrl Pts',(-2.03020677218684,1.81013815140819,
7.53005029815327));
#393610=CARTESIAN_POINT('Ctrl Pts',(-2.07036020808906,1.8113268487847,7.51101258149734));
#393611=CARTESIAN_POINT('Ctrl Pts',(-2.06464010736903,1.80993377894006,
7.5043616886572));
#393612=CARTESIAN_POINT('Ctrl Pts',(-2.06077360068108,1.81762517722494,
7.50217374673251));
#393613=CARTESIAN_POINT('',(-2.05914251569204,1.81722565891166,7.50366116523517));
#393614=CARTESIAN_POINT('Ctrl Pts',(-2.06202449055418,1.80929677321442,
7.51860402984325));
#393615=CARTESIAN_POINT('Ctrl Pts',(-2.06245356066701,1.80940126868831,
7.51734760759493));
#393616=CARTESIAN_POINT('Ctrl Pts',(-2.06282720854068,1.80955350247719,
7.51608817408573));
#393617=CARTESIAN_POINT('Ctrl Pts',(-2.06313953628693,1.80976549106597,
7.5148100591312));
#393618=CARTESIAN_POINT('Ctrl Pts',(-2.0634224502228,1.80995751539533,7.51365231206384));
#393619=CARTESIAN_POINT('Ctrl Pts',(-2.06365558924024,1.81019863323146,
7.51247773061042));
#393620=CARTESIAN_POINT('Ctrl Pts',(-2.06380837374074,1.81051033941392,
7.51129758471022));
#393621=CARTESIAN_POINT('Ctrl Pts',(-2.06399826742622,1.81089775460052,
7.50983079813401));
#393622=CARTESIAN_POINT('Ctrl Pts',(-2.06404627660562,1.81138758047698,
7.50839324291155));
#393623=CARTESIAN_POINT('Ctrl Pts',(-2.0638707052155,1.8119914335698,7.50715379678855));
#393624=CARTESIAN_POINT('Ctrl Pts',(-2.06378959629223,1.81227039629907,
7.50658120839351));
#393625=CARTESIAN_POINT('Ctrl Pts',(-2.06364011712737,1.81261069870671,
7.50598221009429));
#393626=CARTESIAN_POINT('Ctrl Pts',(-2.06340499918457,1.81299509420527,
7.50545747549611));
#393627=CARTESIAN_POINT('Ctrl Pts',(-2.06327953297271,1.81320021954146,
7.50517746087247));
#393628=CARTESIAN_POINT('Ctrl Pts',(-2.0631284923374,1.8134202308675,7.50491486231392));
#393629=CARTESIAN_POINT('Ctrl Pts',(-2.06295450194049,1.81364835785534,
7.50468370960992));
#393630=CARTESIAN_POINT('Ctrl Pts',(-2.06269433141494,1.81398947966074,
7.50433806340446));
#393631=CARTESIAN_POINT('Ctrl Pts',(-2.06237460179234,1.81435863918606,
7.50405484070983));
#393632=CARTESIAN_POINT('Ctrl Pts',(-2.06201630474491,1.81473050520948,
7.5038576603613));
#393633=CARTESIAN_POINT('Ctrl Pts',(-2.06197799044489,1.81477027050058,
7.50383657498791));
#393634=CARTESIAN_POINT('Ctrl Pts',(-2.06193926245814,1.8148100591619,7.50381643264937));
#393635=CARTESIAN_POINT('Ctrl Pts',(-2.06190016639466,1.81484983502236,
7.50379723213559));
#393636=CARTESIAN_POINT('Ctrl Pts',(-2.06163918738168,1.81511535190253,
7.50366906242519));
#393637=CARTESIAN_POINT('Ctrl Pts',(-2.0613556171647,1.81538556994,7.50358235568538));
#393638=CARTESIAN_POINT('Ctrl Pts',(-2.061076029527,1.81563945665821,7.5035341175365));
#393639=CARTESIAN_POINT('Ctrl Pts',(-2.06065681950748,1.81602013105773,
7.50346178989176));
#393640=CARTESIAN_POINT('Ctrl Pts',(-2.06018965908649,1.81641182575994,
7.50346967198527));
#393641=CARTESIAN_POINT('Ctrl Pts',(-2.05971922051127,1.81678223725707,
7.50354272648692));
#393642=CARTESIAN_POINT('Ctrl Pts',(-2.05952571938778,1.8169345951729,7.50357277531559));
#393643=CARTESIAN_POINT('Ctrl Pts',(-2.05933200846982,1.81708326126962,
7.50361331098761));
#393644=CARTESIAN_POINT('Ctrl Pts',(-2.05914251569311,1.8172256589126,7.50366116523659));
#393645=CARTESIAN_POINT('',(-1.97947865054223,1.79771013628763,7.57603338622103));
#393646=CARTESIAN_POINT('Origin',(-1.98601852345765,1.80365333002892,7.58486873427627));
#393647=CARTESIAN_POINT('Ctrl Pts',(-2.05914251574877,1.81722565892004,
7.50366116529969));
#393648=CARTESIAN_POINT('Ctrl Pts',(-2.03263102682016,1.81073191165144,
7.52783573079709));
#393649=CARTESIAN_POINT('Ctrl Pts',(-2.00607765461973,1.80422706199264,
7.55196141284069));
#393650=CARTESIAN_POINT('Ctrl Pts',(-1.97947865179296,1.79771013622993,
7.57603338728831));
#393651=CARTESIAN_POINT('Ctrl Pts',(-1.9798955577159,1.78947609816001,7.59639677331371));
#393652=CARTESIAN_POINT('Ctrl Pts',(-1.96304400704085,1.78239816374436,
7.59959882295464));
#393653=CARTESIAN_POINT('Ctrl Pts',(-1.97123919548053,1.7987550491153,7.59642833564546));
#393654=CARTESIAN_POINT('Ctrl Pts',(-1.97658880884441,1.78740715737193,
7.58707626057423));
#393655=CARTESIAN_POINT('Ctrl Pts',(-1.96999477520762,1.78896632748225,
7.58809943920598));
#393656=CARTESIAN_POINT('Ctrl Pts',(-1.96897092964352,1.79564960071127,
7.58710240504252));
#393657=CARTESIAN_POINT('Ctrl Pts',(-1.97787616399563,1.79334587347696,
7.58015376756929));
#393658=CARTESIAN_POINT('Ctrl Pts',(-1.97503972448267,1.79363549786387,
7.58205880659761));
#393659=CARTESIAN_POINT('Ctrl Pts',(-1.97498177042911,1.7964504075188,7.58020924244128));
#393660=CARTESIAN_POINT('Ctrl Pts',(-1.97947864992973,1.7977101357311,7.57603338509286));
#393661=CARTESIAN_POINT('Ctrl Pts',(-1.97947864992973,1.7977101357311,7.57603338509286));
#393662=CARTESIAN_POINT('Ctrl Pts',(-1.97947864992973,1.7977101357311,7.57603338509286));
#393663=CARTESIAN_POINT('Origin',(-1.9860223598435,1.80364910574226,7.58486873427621));
#393664=CARTESIAN_POINT('Ctrl Pts',(-2.00176808024934,1.88688983029521,
7.51098857897448));
#393665=CARTESIAN_POINT('Ctrl Pts',(-1.99983217741494,1.88132990294068,
7.50433767179956));
#393666=CARTESIAN_POINT('Ctrl Pts',(-2.00711679739921,1.87674270741757,
7.50214974420965));
#393667=CARTESIAN_POINT('Ctrl Pts',(-1.99140963785969,1.85714030662641,
7.53887321589169));
#393668=CARTESIAN_POINT('Ctrl Pts',(-1.98949693057684,1.85164699706871,
7.53220407452066));
#393669=CARTESIAN_POINT('Ctrl Pts',(-1.99672626159447,1.84702750651676,
7.53003438070912));
#393670=CARTESIAN_POINT('Ctrl Pts',(-1.98103130343958,1.82733365289803,
7.56669465659235));
#393671=CARTESIAN_POINT('Ctrl Pts',(-1.97912989990116,1.82187280777846,
7.56004085833298));
#393672=CARTESIAN_POINT('Ctrl Pts',(-1.98631507225213,1.81725653781094,
7.55785582193789));
#393673=CARTESIAN_POINT('Ctrl Pts',(-1.97063354635953,1.79747121714567,
7.59443891967696));
#393674=CARTESIAN_POINT('Ctrl Pts',(-1.96872938602273,1.7920024544806,7.58783901202978));
#393675=CARTESIAN_POINT('Ctrl Pts',(-1.97588366545473,1.78743129885023,
7.58560008491213));
#393676=CARTESIAN_POINT('',(-2.00655355952792,1.87513194417974,7.50366116523517));
#393677=CARTESIAN_POINT('Ctrl Pts',(-2.00655355952819,1.87513194417999,
7.50366116523554));
#393678=CARTESIAN_POINT('Ctrl Pts',(-2.00615848269924,1.87577851344619,
7.50350835821027));
#393679=CARTESIAN_POINT('Ctrl Pts',(-2.00577427574858,1.87636001411704,
7.50345484955999));
#393680=CARTESIAN_POINT('Ctrl Pts',(-2.0053900169105,1.87689406571169,7.50349758195598));
#393681=CARTESIAN_POINT('Ctrl Pts',(-2.00519286362919,1.87716807378604,
7.50351950684424));
#393682=CARTESIAN_POINT('Ctrl Pts',(-2.00497636954116,1.87745667406357,
7.50357029184312));
#393683=CARTESIAN_POINT('Ctrl Pts',(-2.0047599570338,1.87772922952131,7.50365515313923));
#393684=CARTESIAN_POINT('Ctrl Pts',(-2.0044270269634,1.87814853018392,7.50378570417639));
#393685=CARTESIAN_POINT('Ctrl Pts',(-2.0040847889912,1.87854238174117,7.50400001621911));
#393686=CARTESIAN_POINT('Ctrl Pts',(-2.00375757860848,1.87887931717084,
7.50428903009634));
#393687=CARTESIAN_POINT('Ctrl Pts',(-2.00372126077341,1.8789167144113,7.50432110841318));
#393688=CARTESIAN_POINT('Ctrl Pts',(-2.00368512302499,1.87895344037839,
7.50435406373354));
#393689=CARTESIAN_POINT('Ctrl Pts',(-2.00364919461634,1.87898947405935,
7.50438785222351));
#393690=CARTESIAN_POINT('Ctrl Pts',(-2.00342983441215,1.87920947700163,
7.50459414719561));
#393691=CARTESIAN_POINT('Ctrl Pts',(-2.00321442008337,1.87940681218196,
7.50483629897752));
#393692=CARTESIAN_POINT('Ctrl Pts',(-2.00301209305111,1.87957489015284,
7.5050991045531));
#393693=CARTESIAN_POINT('Ctrl Pts',(-2.00256573929611,1.87994568703844,
7.50567888004914));
#393694=CARTESIAN_POINT('Ctrl Pts',(-2.00216582340181,1.88018910434134,
7.50637912803145));
#393695=CARTESIAN_POINT('Ctrl Pts',(-2.00182096599598,1.88033482544298,
7.50710440483569));
#393696=CARTESIAN_POINT('Ctrl Pts',(-2.00173640011369,1.88037055915008,
7.50728225710685));
#393697=CARTESIAN_POINT('Ctrl Pts',(-2.00165351840971,1.88040126390213,
7.50746498566955));
#393698=CARTESIAN_POINT('Ctrl Pts',(-2.00157440033246,1.8804266135986,7.50764697238949));
#393699=CARTESIAN_POINT('Ctrl Pts',(-2.00114908332306,1.88056288659041,
7.50862528291181));
#393700=CARTESIAN_POINT('Ctrl Pts',(-2.00079518281119,1.88056071912448,
7.5096585683742));
#393701=CARTESIAN_POINT('Ctrl Pts',(-2.0004944929555,1.880483860265,7.510679598732));
#393702=CARTESIAN_POINT('Ctrl Pts',(-2.00032902294865,1.88044156473768,
7.51124147302577));
#393703=CARTESIAN_POINT('Ctrl Pts',(-2.00017973400083,1.88037621910703,
7.51180065547252));
#393704=CARTESIAN_POINT('Ctrl Pts',(-2.00004436034522,1.88029584196497,
7.512351757165));
#393705=CARTESIAN_POINT('Ctrl Pts',(-1.99957659043866,1.8800181069207,7.51425603304536));
#393706=CARTESIAN_POINT('Ctrl Pts',(-1.99922228938719,1.87952256964401,
7.51626900505181));
#393707=CARTESIAN_POINT('Ctrl Pts',(-1.99897691956687,1.87886941383173,
7.51827788969244));
#393708=CARTESIAN_POINT('Ctrl Pts',(-1.99896363968851,1.87883406380488,
7.51838661432546));
#393709=CARTESIAN_POINT('Ctrl Pts',(-1.99895068242723,1.87879824277267,
7.51849533314857));
#393710=CARTESIAN_POINT('Ctrl Pts',(-1.99893804826278,1.87876195735829,
7.51860402984325));
#393711=CARTESIAN_POINT('Ctrl Pts',(-1.97947865060561,1.7977101375391,7.57603338728985));
#393712=CARTESIAN_POINT('Ctrl Pts',(-1.9885195791301,1.82356045445259,7.55196141284922));
#393713=CARTESIAN_POINT('Ctrl Pts',(-1.99754410576767,1.84936651119318,
7.52783573083105));
#393714=CARTESIAN_POINT('Ctrl Pts',(-2.00655355954224,1.87513194423716,
7.50366116530176));
#393715=CARTESIAN_POINT('Origin',(-6.84001376365786E-16,6.21191952330709E-16,
7.49482233047033));
#393716=CARTESIAN_POINT('Origin',(-2.05251535802925,1.81137708803387,7.49482233047033));
#393717=CARTESIAN_POINT('Origin',(0.,0.,7.50366116523517));
#393718=CARTESIAN_POINT('Origin',(-2.00009565450363,1.86909700733689,7.49482233047033));
#393719=CARTESIAN_POINT('Ctrl Pts',(-2.06202346288219,1.80929652288975,
7.51860402984325));
#393720=CARTESIAN_POINT('Ctrl Pts',(-2.06941618821693,1.81109760538513,
7.51860402984325));
#393721=CARTESIAN_POINT('Ctrl Pts',(-2.07441142381098,1.80535792705007,
7.51860402984325));
#393722=CARTESIAN_POINT('Ctrl Pts',(-2.06476843255036,1.8099652758769,7.51041458714365));
#393723=CARTESIAN_POINT('Ctrl Pts',(-2.07059960927625,1.80973780334734,
7.51004642900442));
#393724=CARTESIAN_POINT('Ctrl Pts',(-2.07441280143765,1.80535634411492,
7.5072913648301));
#393725=CARTESIAN_POINT('Ctrl Pts',(-2.06508648531179,1.81276216336841,
7.50215815450138));
#393726=CARTESIAN_POINT('Ctrl Pts',(-2.06819015181946,1.81250658815323,
7.49877163671531));
#393727=CARTESIAN_POINT('Ctrl Pts',(-2.07047313188639,1.80991971250713,
7.49481588533171));
#393728=CARTESIAN_POINT('Ctrl Pts',(-2.05914210292581,1.8172252946396,7.50366171572174));
#393729=CARTESIAN_POINT('Ctrl Pts',(-2.0618875742757,1.81964821629003,7.50000045605858));
#393730=CARTESIAN_POINT('Ctrl Pts',(-2.06188757427578,1.81964821628993,
7.49482233047317));
#393731=CARTESIAN_POINT('Origin',(-2.06498228097548,1.79715175465438,7.51860402984325));
#393732=CARTESIAN_POINT('Origin',(-2.06498228097548,1.79715175465438,9.));
#393733=CARTESIAN_POINT('Origin',(-2.06498228097548,1.79715175465438,8.75721825406948));
#393734=CARTESIAN_POINT('Ctrl Pts',(-2.04579859637347,1.80534509773719,
8.78942910404913));
#393735=CARTESIAN_POINT('Ctrl Pts',(-2.05120799968457,1.80668329970982,
8.79672699501691));
#393736=CARTESIAN_POINT('Ctrl Pts',(-2.05490627375193,1.79855949180314,
8.79893251111267));
#393737=CARTESIAN_POINT('Ctrl Pts',(-2.05648070824783,1.807946617417,8.78111911759583));
#393738=CARTESIAN_POINT('Ctrl Pts',(-2.06289540615571,1.80952584535372,
8.78644465894813));
#393739=CARTESIAN_POINT('Ctrl Pts',(-2.06775831860606,1.80303989174029,
8.78817647674131));
#393740=CARTESIAN_POINT('Ctrl Pts',(-2.06313805516785,1.80956794650264,
8.7678092393203));
#393741=CARTESIAN_POINT('Ctrl Pts',(-2.0707115533493,1.8114272103532,8.76988516158374));
#393742=CARTESIAN_POINT('Ctrl Pts',(-2.07578916287302,1.80582772270513,
8.77093053738833));
#393743=CARTESIAN_POINT('Ctrl Pts',(-2.06183996363106,1.8092518095187,8.75371302330492));
#393744=CARTESIAN_POINT('Ctrl Pts',(-2.06922740267153,1.81106618152884,
8.75300828287559));
#393745=CARTESIAN_POINT('Ctrl Pts',(-2.07422297212531,1.80528355019297,
8.75267964240738));
#393746=CARTESIAN_POINT('Origin',(-2.05135792032742,1.7938336861622,8.78727029226991));
#393747=CARTESIAN_POINT('Ctrl Pts',(-1.9789379566843,1.78906192937258,8.85049129520029));
#393748=CARTESIAN_POINT('Ctrl Pts',(-1.98461173602729,1.79044371813727,
8.85711686593484));
#393749=CARTESIAN_POINT('Ctrl Pts',(-1.98847679932028,1.78281731348927,
8.85933012996512));
#393750=CARTESIAN_POINT('Ctrl Pts',(-2.00212570220895,1.79470905879154,
8.82945683644721));
#393751=CARTESIAN_POINT('Ctrl Pts',(-2.00784657735091,1.79610231723841,
8.83607469902387));
#393752=CARTESIAN_POINT('Ctrl Pts',(-2.01168953666616,1.78843656833835,
8.8382956714852));
#393753=CARTESIAN_POINT('Ctrl Pts',(-2.02527888452907,1.80034777070872,
8.80838214965003));
#393754=CARTESIAN_POINT('Ctrl Pts',(-2.03102233691534,1.80174652760391,
8.81501364461987));
#393755=CARTESIAN_POINT('Ctrl Pts',(-2.03486690419791,1.79404794883865,
8.81722098428721));
#393756=CARTESIAN_POINT('Ctrl Pts',(-2.04840012990613,1.80597870472224,
8.78727029226991));
#393757=CARTESIAN_POINT('Ctrl Pts',(-2.05414453629874,1.80737769395557,
8.79393457792714));
#393758=CARTESIAN_POINT('Ctrl Pts',(-2.05801159645805,1.79965207029774,
8.79610912703474));
#393759=CARTESIAN_POINT('Origin',(-1.9818957471056,1.77691691081254,8.85049129520029));
#393760=CARTESIAN_POINT('Ctrl Pts',(-1.97081848695446,1.79800236791132,
8.85049129520029));
#393761=CARTESIAN_POINT('Ctrl Pts',(-1.97273870409018,1.80351724582246,
8.85711686593484));
#393762=CARTESIAN_POINT('Ctrl Pts',(-1.96551867526938,1.80809675954563,
8.85933012996512));
#393763=CARTESIAN_POINT('Ctrl Pts',(-1.96911969857311,1.79312343503146,
8.86332496987231));
#393764=CARTESIAN_POINT('Ctrl Pts',(-1.9662278890552,1.79672750663019,8.86648636486737));
#393765=CARTESIAN_POINT('Ctrl Pts',(-1.96078242541378,1.79444211221727,
8.87206031107457));
#393766=CARTESIAN_POINT('Ctrl Pts',(-1.97388433684391,1.78783117387535,
8.86341338519877));
#393767=CARTESIAN_POINT('Ctrl Pts',(-1.97718275554803,1.78457634597106,
8.86654584966058));
#393768=CARTESIAN_POINT('Ctrl Pts',(-1.97432290905723,1.7793854471244,8.87215952290714));
#393769=CARTESIAN_POINT('Ctrl Pts',(-1.9789379566843,1.78906192937258,8.85049129520029));
#393770=CARTESIAN_POINT('Ctrl Pts',(-1.98461173602729,1.79044371813727,
8.85711686593484));
#393771=CARTESIAN_POINT('Ctrl Pts',(-1.98847679932028,1.78281731348927,
8.85933012996512));
#393772=CARTESIAN_POINT('Origin',(-1.95901360513967,1.802112692149,8.85049129520029));
#393773=CARTESIAN_POINT('Ctrl Pts',(-1.99432705985485,1.86551916431871,
8.78727029226991));
#393774=CARTESIAN_POINT('Ctrl Pts',(-1.99627117980081,1.87110269127881,
8.79393457792714));
#393775=CARTESIAN_POINT('Ctrl Pts',(-1.98895258219516,1.87569371995056,
8.79610912703474));
#393776=CARTESIAN_POINT('Ctrl Pts',(-1.98650197380753,1.84304545892766,
8.80838214965002));
#393777=CARTESIAN_POINT('Ctrl Pts',(-1.98844577088241,1.84862805859966,
8.81501364461993));
#393778=CARTESIAN_POINT('Ctrl Pts',(-1.98115193336383,1.85319410139924,
8.81722098428721));
#393779=CARTESIAN_POINT('Ctrl Pts',(-1.97866607911547,1.82054071102845,
8.82945683644723));
#393780=CARTESIAN_POINT('Ctrl Pts',(-1.98060223521441,1.8261013657606,8.83607469902389));
#393781=CARTESIAN_POINT('Ctrl Pts',(-1.97334092145604,1.83066265560014,
8.8382956714852));
#393782=CARTESIAN_POINT('Ctrl Pts',(-1.97081848695446,1.79800236791132,
8.85049129520029));
#393783=CARTESIAN_POINT('Ctrl Pts',(-1.97273870409018,1.80351724582246,
8.85711686593484));
#393784=CARTESIAN_POINT('Ctrl Pts',(-1.96551867526938,1.80809675954563,
8.85933012996512));
#393785=CARTESIAN_POINT('Origin',(-1.98252217804006,1.86962948855639,8.78727029226991));
#393786=CARTESIAN_POINT('Ctrl Pts',(-1.99887714505914,1.87858709900374,
8.75374538247848));
#393787=CARTESIAN_POINT('Ctrl Pts',(-2.0013882733546,1.88575917074566,8.75304829418602));
#393788=CARTESIAN_POINT('Ctrl Pts',(-1.99612174305392,1.89128495592073,
8.75272238421917));
#393789=CARTESIAN_POINT('Ctrl Pts',(-1.99931119033487,1.87983367897016,
8.76769408445018));
#393790=CARTESIAN_POINT('Ctrl Pts',(-2.00188485842239,1.88718645990988,
8.76974318093967));
#393791=CARTESIAN_POINT('Ctrl Pts',(-1.99680650103025,1.89277471934172,
8.7707786988043));
#393792=CARTESIAN_POINT('Ctrl Pts',(-1.99708652152471,1.87344442018717,
8.78108014887992));
#393793=CARTESIAN_POINT('Ctrl Pts',(-1.99927119857792,1.87967438194253,
8.78639403366326));
#393794=CARTESIAN_POINT('Ctrl Pts',(-1.9933043463902,1.88514418547637,8.78812224174741));
#393795=CARTESIAN_POINT('Ctrl Pts',(-1.99344078041232,1.86297383549668,
8.78944554828685));
#393796=CARTESIAN_POINT('Ctrl Pts',(-1.9952872275871,1.86822236390451,8.79673892988685));
#393797=CARTESIAN_POINT('Ctrl Pts',(-1.98756562585766,1.87268111048268,
8.79894799272499));
#393798=CARTESIAN_POINT('Origin',(-1.987133166448,1.88287228159596,8.75721825406948));
#393799=CARTESIAN_POINT('Origin',(-1.987133166448,1.88287228159596,9.));
#393800=CARTESIAN_POINT('Origin',(-1.987133166448,1.88287228159596,7.51860402984325));
#393801=CARTESIAN_POINT('Ctrl Pts',(-2.00655298476889,1.87513140706531,
7.50366195182966));
#393802=CARTESIAN_POINT('Ctrl Pts',(-2.00922851137341,1.87763169686821,
7.50000065167735));
#393803=CARTESIAN_POINT('Ctrl Pts',(-2.00922851137333,1.8776316968683,7.49482233047108));
#393804=CARTESIAN_POINT('Ctrl Pts',(-2.00267706150171,1.88148207777269,
7.50215800491337));
#393805=CARTESIAN_POINT('Ctrl Pts',(-2.00271935143079,1.88459702700764,
7.49877273257265));
#393806=CARTESIAN_POINT('Ctrl Pts',(-2.00036234457183,1.88711926312204,
7.49481816995647));
#393807=CARTESIAN_POINT('Ctrl Pts',(-1.99986519248848,1.88142369117744,
7.51043025814042));
#393808=CARTESIAN_POINT('Ctrl Pts',(-2.0002025994931,1.8872528346394,7.51006209594514));
#393809=CARTESIAN_POINT('Ctrl Pts',(-1.99620509243911,1.89147170978754,
7.50731281821699));
#393810=CARTESIAN_POINT('Ctrl Pts',(-1.99893755118652,1.87876053002944,
7.51860402984325));
#393811=CARTESIAN_POINT('Ctrl Pts',(-2.00144054600741,1.88594635178601,
7.51860402984325));
#393812=CARTESIAN_POINT('Ctrl Pts',(-1.9962068338747,1.89146987192289,7.51860402984325));
#393813=CARTESIAN_POINT('Origin',(0.,0.,7.5));
#393814=CARTESIAN_POINT('Origin',(-2.08196763624131,1.66803740521007,7.5));
#393815=CARTESIAN_POINT('',(-2.08196763624131,1.66803740521007,7.59394543036555));
#393816=CARTESIAN_POINT('',(-2.08196763624131,1.66803740521007,8.85049129520029));
#393817=CARTESIAN_POINT('',(-2.08196763624131,1.66803740521007,7.5));
#393818=CARTESIAN_POINT('',(-2.10975372425561,1.73390928168093,8.78727029226991));
#393819=CARTESIAN_POINT('Ctrl Pts',(-2.08196763624131,1.66803740521007,
8.85049129520029));
#393820=CARTESIAN_POINT('Ctrl Pts',(-2.09124312883603,1.69002661441762,
8.82945686509571));
#393821=CARTESIAN_POINT('Ctrl Pts',(-2.10050483228943,1.71198313400678,
8.80838212259895));
#393822=CARTESIAN_POINT('Ctrl Pts',(-2.10975372425561,1.73390928168093,
8.78727029226991));
#393823=CARTESIAN_POINT('',(-2.11520370755654,1.74682943894029,8.75721825406948));
#393824=CARTESIAN_POINT('Origin',(-2.09880300312866,1.70794812528068,8.75937679713103));
#393825=CARTESIAN_POINT('',(-2.11520370755654,1.74682943894029,7.51860402984325));
#393826=CARTESIAN_POINT('',(-2.11520370755654,1.74682943894029,7.5));
#393827=CARTESIAN_POINT('Ctrl Pts',(-2.11520370755654,1.74682943894029,
7.51860402984325));
#393828=CARTESIAN_POINT('Ctrl Pts',(-2.11092359330639,1.73668266487761,
7.52834476460825));
#393829=CARTESIAN_POINT('Ctrl Pts',(-2.10664070046784,1.72652930367562,
7.53807742314407));
#393830=CARTESIAN_POINT('Ctrl Pts',(-2.10235493574608,1.71636913416236,
7.54780169004674));
#393831=CARTESIAN_POINT('Ctrl Pts',(-2.09556651605262,1.70027597476367,
7.5632044032688));
#393832=CARTESIAN_POINT('Ctrl Pts',(-2.08877088254285,1.68416571372709,
7.57858609112102));
#393833=CARTESIAN_POINT('Ctrl Pts',(-2.08196763624131,1.66803740521007,
7.59394543036555));
#393834=CARTESIAN_POINT('Origin',(-2.36030818298167,1.70641386443188,7.5));
#393835=CARTESIAN_POINT('',(-2.17370988235715,1.67346501623196,8.75721825406948));
#393836=CARTESIAN_POINT('',(-2.15990092504105,1.67102668085117,8.78727029226991));
#393837=CARTESIAN_POINT('Origin',(-2.12484864088886,1.66483727620104,8.75658640621056));
#393838=CARTESIAN_POINT('',(-2.08949760778589,1.65859511954945,8.85049129520029));
#393839=CARTESIAN_POINT('Ctrl Pts',(-2.15990092504105,1.67102668085117,
8.78727029226991));
#393840=CARTESIAN_POINT('Ctrl Pts',(-2.13646643958854,1.66688870477511,
8.80838212259895));
#393841=CARTESIAN_POINT('Ctrl Pts',(-2.11299949288422,1.66274499680945,
8.82945686509571));
#393842=CARTESIAN_POINT('Ctrl Pts',(-2.08949760778589,1.65859511954945,
8.85049129520029));
#393843=CARTESIAN_POINT('',(-2.08949760778589,1.65859511954945,7.59394543036555));
#393844=CARTESIAN_POINT('',(-2.08949760778589,1.65859511954945,7.5));
#393845=CARTESIAN_POINT('',(-2.17370988235715,1.67346501623196,7.51860402984325));
#393846=CARTESIAN_POINT('Ctrl Pts',(-2.08949760778588,1.65859511954945,
7.59394543036555));
#393847=CARTESIAN_POINT('Ctrl Pts',(-2.10673541065636,1.66163890798792,
7.57858609112103));
#393848=CARTESIAN_POINT('Ctrl Pts',(-2.12395392452866,1.66467929044538,
7.56320440326857));
#393849=CARTESIAN_POINT('Ctrl Pts',(-2.14115416031192,1.66771644542443,
7.54780169004651));
#393850=CARTESIAN_POINT('Ctrl Pts',(-2.1520132655315,1.66963390666748,7.53807742314383));
#393851=CARTESIAN_POINT('Ctrl Pts',(-2.16286509408445,1.67155008302324,
7.52834476460825));
#393852=CARTESIAN_POINT('Ctrl Pts',(-2.17370988235715,1.67346501623196,
7.51860402984325));
#393853=CARTESIAN_POINT('',(-2.17370988235715,1.67346501623196,7.5));
#393854=CARTESIAN_POINT('Origin',(-2.08830213916383,1.66536538392934,7.5));
#393855=CARTESIAN_POINT('Ctrl Pts',(-2.08949760778589,1.65859511954945,
8.85049129520029));
#393856=CARTESIAN_POINT('Ctrl Pts',(-2.08930689657203,1.65856144445801,
8.85097269580138));
#393857=CARTESIAN_POINT('Ctrl Pts',(-2.08911712890332,1.65853647751091,
8.85143669361005));
#393858=CARTESIAN_POINT('Ctrl Pts',(-2.08891945254857,1.65851993587657,
8.8519052845931));
#393859=CARTESIAN_POINT('Ctrl Pts',(-2.08853281013487,1.65848758148884,
8.85282181883899));
#393860=CARTESIAN_POINT('Ctrl Pts',(-2.0881258413294,1.65848848817671,8.85372622499635));
#393861=CARTESIAN_POINT('Ctrl Pts',(-2.08769219444456,1.65853808886801,
8.8546225773507));
#393862=CARTESIAN_POINT('Ctrl Pts',(-2.08733219620245,1.65857926560028,
8.85536669723986));
#393863=CARTESIAN_POINT('Ctrl Pts',(-2.08695372646825,1.65865397891726,
8.85610498449051));
#393864=CARTESIAN_POINT('Ctrl Pts',(-2.08655466895921,1.65877891590463,
8.85681338218371));
#393865=CARTESIAN_POINT('Ctrl Pts',(-2.08619252364303,1.65889229641688,
8.85745625420284));
#393866=CARTESIAN_POINT('Ctrl Pts',(-2.08580870152052,1.65904789017868,
8.85808743050665));
#393867=CARTESIAN_POINT('Ctrl Pts',(-2.08540145248205,1.65927424159867,
8.8586680450841));
#393868=CARTESIAN_POINT('Ctrl Pts',(-2.08521355660377,1.65937867523715,
8.85893592806395));
#393869=CARTESIAN_POINT('Ctrl Pts',(-2.08502068797859,1.65949841300905,
8.85919241173848));
#393870=CARTESIAN_POINT('Ctrl Pts',(-2.08482298944179,1.65963782316054,
8.85943017985534));
#393871=CARTESIAN_POINT('Ctrl Pts',(-2.08455603789208,1.65982606813486,
8.8597512372));
#393872=CARTESIAN_POINT('Ctrl Pts',(-2.08427385450002,1.66005549655853,
8.86004599534706));
#393873=CARTESIAN_POINT('Ctrl Pts',(-2.08398639993716,1.66033143307006,
8.86026130871721));
#393874=CARTESIAN_POINT('Ctrl Pts',(-2.08388115471749,1.66043246120641,
8.86034014101235));
#393875=CARTESIAN_POINT('Ctrl Pts',(-2.08377361346506,1.66054123240653,
8.86040910639692));
#393876=CARTESIAN_POINT('Ctrl Pts',(-2.08366694528516,1.66065501975952,
8.86046313645506));
#393877=CARTESIAN_POINT('Ctrl Pts',(-2.08350049048376,1.66083258397091,
8.86054744990829));
#393878=CARTESIAN_POINT('Ctrl Pts',(-2.08333172529106,1.66102731071898,
8.86059655985669));
#393879=CARTESIAN_POINT('Ctrl Pts',(-2.08317125174907,1.66122651971649,
8.86059725258816));
#393880=CARTESIAN_POINT('Ctrl Pts',(-2.08301040744909,1.66142618896637,
8.86059794692011));
#393881=CARTESIAN_POINT('Ctrl Pts',(-2.08285817834936,1.66163424222322,
8.86056369958366));
#393882=CARTESIAN_POINT('Ctrl Pts',(-2.08271983012947,1.66183711006156,
8.86048590497774));
#393883=CARTESIAN_POINT('Ctrl Pts',(-2.0826837253632,1.66189005252726,8.86046560290182));
#393884=CARTESIAN_POINT('Ctrl Pts',(-2.08264817109199,1.66194338162274,
8.86044257503091));
#393885=CARTESIAN_POINT('Ctrl Pts',(-2.08261423865958,1.66199543122558,
8.86041778462583));
#393886=CARTESIAN_POINT('Ctrl Pts',(-2.08238591549609,1.66234566046449,
8.86025097596201));
#393887=CARTESIAN_POINT('Ctrl Pts',(-2.0822006631088,1.66268513650962,8.8599848982295));
#393888=CARTESIAN_POINT('Ctrl Pts',(-2.08205645133814,1.66299989246577,
8.85968173251461));
#393889=CARTESIAN_POINT('Ctrl Pts',(-2.08198017157381,1.66316638033321,
8.85952137522076));
#393890=CARTESIAN_POINT('Ctrl Pts',(-2.08191373021562,1.66332908163806,
8.85934740853961));
#393891=CARTESIAN_POINT('Ctrl Pts',(-2.08185662505612,1.66348511422399,
8.8591675900182));
#393892=CARTESIAN_POINT('Ctrl Pts',(-2.08162731815807,1.66411166616059,
8.85844552518696));
#393893=CARTESIAN_POINT('Ctrl Pts',(-2.08153275038138,1.66466506031438,
8.85759444184126));
#393894=CARTESIAN_POINT('Ctrl Pts',(-2.08149617274033,1.66512319384479,
8.85683498915141));
#393895=CARTESIAN_POINT('Ctrl Pts',(-2.08149234498761,1.66517113629864,
8.85675551445));
#393896=CARTESIAN_POINT('Ctrl Pts',(-2.08148917211987,1.66521803320866,
8.85667699793652));
#393897=CARTESIAN_POINT('Ctrl Pts',(-2.08148657912978,1.66526385703586,
8.85659965593547));
#393898=CARTESIAN_POINT('Ctrl Pts',(-2.08145157881728,1.6658823893937,8.85555568965886));
#393899=CARTESIAN_POINT('Ctrl Pts',(-2.08150726965999,1.66648189204855,
8.85434650606346));
#393900=CARTESIAN_POINT('Ctrl Pts',(-2.08164773886709,1.66706590344667,
8.85297329937118));
#393901=CARTESIAN_POINT('Ctrl Pts',(-2.08172674423718,1.66739437427377,
8.85220095427748));
#393902=CARTESIAN_POINT('Ctrl Pts',(-2.08183290683987,1.66771800513893,
8.85137579139184));
#393903=CARTESIAN_POINT('Ctrl Pts',(-2.08196763624131,1.66803740521007,
8.85049129520029));
#393904=CARTESIAN_POINT('Origin',(-2.08830213916383,1.66536538392934,7.59394543036555));
#393905=CARTESIAN_POINT('Ctrl Pts',(-2.08894390879624,1.65849734939882,
7.59443877723642));
#393906=CARTESIAN_POINT('Ctrl Pts',(-2.08324134195778,1.65749041091931,
7.58783886950016));
#393907=CARTESIAN_POINT('Ctrl Pts',(-2.07987060264357,1.66528254143749,
7.58559994247159));
#393908=CARTESIAN_POINT('Ctrl Pts',(-2.12007405386119,1.66399419701616,
7.56670252222133));
#393909=CARTESIAN_POINT('Ctrl Pts',(-2.11437972885083,1.66298871384862,
7.56004874999027));
#393910=CARTESIAN_POINT('Ctrl Pts',(-2.11096940725828,1.6708185327413,7.55786368756704));
#393911=CARTESIAN_POINT('Ctrl Pts',(-2.1511460664906,1.66948077981979,7.5388891333356));
#393912=CARTESIAN_POINT('Ctrl Pts',(-2.14541789982786,1.66846932101657,
7.53222002137279));
#393913=CARTESIAN_POINT('Ctrl Pts',(-2.1420114441906,1.67634323393907,7.53005029815327));
#393914=CARTESIAN_POINT('Ctrl Pts',(-2.18215854065472,1.67495684953809,
7.51101258149734));
#393915=CARTESIAN_POINT('Ctrl Pts',(-2.17636093820369,1.6739331300163,7.5043616886572));
#393916=CARTESIAN_POINT('Ctrl Pts',(-2.17299516524849,1.68185645343256,
7.50217374673251));
#393917=CARTESIAN_POINT('',(-2.17134183427228,1.68156225994656,7.50366116523517));
#393918=CARTESIAN_POINT('Ctrl Pts',(-2.17370988235715,1.67346501623196,
7.51860402984325));
#393919=CARTESIAN_POINT('Ctrl Pts',(-2.17414476594741,1.67354180639217,
7.51734760759493));
#393920=CARTESIAN_POINT('Ctrl Pts',(-2.17452739977379,1.67366978769894,
7.51608817408572));
#393921=CARTESIAN_POINT('Ctrl Pts',(-2.17485266796471,1.67386132982703,
7.51481005913119));
#393922=CARTESIAN_POINT('Ctrl Pts',(-2.17514730366458,1.6740348332637,7.51365231206383));
#393923=CARTESIAN_POINT('Ctrl Pts',(-2.1753954121457,1.67426051842925,7.51247773061042));
#393924=CARTESIAN_POINT('Ctrl Pts',(-2.17556785381774,1.67456179524136,
7.51129758471022));
#393925=CARTESIAN_POINT('Ctrl Pts',(-2.17578217912251,1.67493624791171,
7.50983079813402));
#393926=CARTESIAN_POINT('Ctrl Pts',(-2.17586147291356,1.67542199142969,
7.50839324291155));
#393927=CARTESIAN_POINT('Ctrl Pts',(-2.17572495125418,1.67603585273915,
7.50715379678855));
#393928=CARTESIAN_POINT('Ctrl Pts',(-2.17566188218132,1.67631943897613,
7.50658120839351));
#393929=CARTESIAN_POINT('Ctrl Pts',(-2.17553451338756,1.67666861935896,
7.50598221009429));
#393930=CARTESIAN_POINT('Ctrl Pts',(-2.17532450682394,1.67706728913406,
7.50545747549611));
#393931=CARTESIAN_POINT('Ctrl Pts',(-2.17521244082128,1.67728003166603,
7.50517746087247));
#393932=CARTESIAN_POINT('Ctrl Pts',(-2.17507580668921,1.67750926816194,
7.50491486231392));
#393933=CARTESIAN_POINT('Ctrl Pts',(-2.17491678992052,1.67774807404142,
7.50468370960992));
#393934=CARTESIAN_POINT('Ctrl Pts',(-2.17467900969234,1.67810516415829,
7.50433806340446));
#393935=CARTESIAN_POINT('Ctrl Pts',(-2.17438358912053,1.67849405035303,
7.50405484070983));
#393936=CARTESIAN_POINT('Ctrl Pts',(-2.17404985377074,1.67888810850847,
7.5038576603613));
#393937=CARTESIAN_POINT('Ctrl Pts',(-2.1740141659625,1.67893024690314,7.50383657498791));
#393938=CARTESIAN_POINT('Ctrl Pts',(-2.17397806681484,1.67897243512502,
7.50381643264937));
#393939=CARTESIAN_POINT('Ctrl Pts',(-2.17394159952654,1.67901463415509,
7.50379723213559));
#393940=CARTESIAN_POINT('Ctrl Pts',(-2.17369816844786,1.67929632648513,
7.50366906242519));
#393941=CARTESIAN_POINT('Ctrl Pts',(-2.1734324937854,1.67958415773685,7.50358235568538));
#393942=CARTESIAN_POINT('Ctrl Pts',(-2.17316974716838,1.67985543605901,
7.5035341175365));
#393943=CARTESIAN_POINT('Ctrl Pts',(-2.17277578835333,1.68026218720033,
7.50346178989176));
#393944=CARTESIAN_POINT('Ctrl Pts',(-2.17233468372925,1.6806830081947,7.50346967198527));
#393945=CARTESIAN_POINT('Ctrl Pts',(-2.17188894406665,1.68108279974468,
7.50354272648692));
#393946=CARTESIAN_POINT('Ctrl Pts',(-2.17170560211715,1.68124724228438,
7.50357277531559));
#393947=CARTESIAN_POINT('Ctrl Pts',(-2.17152181426857,1.68140801403178,
7.50361331098761));
#393948=CARTESIAN_POINT('Ctrl Pts',(-2.1713418342734,1.68156225994742,7.50366116523658));
#393949=CARTESIAN_POINT('',(-2.09059128324977,1.66719091542145,7.57603338622103));
#393950=CARTESIAN_POINT('Origin',(-2.09749850102583,1.67270288713818,7.58486873427626));
#393951=CARTESIAN_POINT('Ctrl Pts',(-2.17134183432943,1.68156225995128,
7.50366116529969));
#393952=CARTESIAN_POINT('Ctrl Pts',(-2.14446876028216,1.67678045171058,
7.52783573079709));
#393953=CARTESIAN_POINT('Ctrl Pts',(-2.11755317768418,1.67199024736118,
7.55196141284068));
#393954=CARTESIAN_POINT('Ctrl Pts',(-2.09059128449423,1.66719091528374,
7.57603338728831));
#393955=CARTESIAN_POINT('Ctrl Pts',(-2.09047977720881,1.65894708367395,
7.59639677331371));
#393956=CARTESIAN_POINT('Ctrl Pts',(-2.07239800659894,1.65268226143542,
7.59974925422225));
#393957=CARTESIAN_POINT('Ctrl Pts',(-2.08252932914762,1.6689166302092,7.59639677331372));
#393958=CARTESIAN_POINT('Ctrl Pts',(-2.08704726491611,1.6570942578742,7.58707626057421));
#393959=CARTESIAN_POINT('Ctrl Pts',(-2.08045436498717,1.65910699286144,
7.58811717123966));
#393960=CARTESIAN_POINT('Ctrl Pts',(-2.0799591517179,1.66598247069354,7.58707626057424));
#393961=CARTESIAN_POINT('Ctrl Pts',(-2.08871246990531,1.66293829112236,
7.5801537675693));
#393962=CARTESIAN_POINT('Ctrl Pts',(-2.08585790079769,1.66341616887628,
7.5820876076604));
#393963=CARTESIAN_POINT('Ctrl Pts',(-2.08602720582064,1.66630550578067,
7.5801537675693));
#393964=CARTESIAN_POINT('Ctrl Pts',(-2.09059128260288,1.66719091490531,
7.57603338509286));
#393965=CARTESIAN_POINT('Ctrl Pts',(-2.09059128260288,1.66719091490531,
7.57603338509286));
#393966=CARTESIAN_POINT('Ctrl Pts',(-2.09059128260288,1.66719091490531,
7.57603338509286));
#393967=CARTESIAN_POINT('Origin',(-2.09750205887831,1.67269842573215,7.5848687342762));
#393968=CARTESIAN_POINT('Ctrl Pts',(-2.1185486795459,1.75475929151862,7.51098857897448));
#393969=CARTESIAN_POINT('Ctrl Pts',(-2.11626052846282,1.74933482135161,
7.50433767179956));
#393970=CARTESIAN_POINT('Ctrl Pts',(-2.1232362787878,1.74429032350881,7.50214974420965));
#393971=CARTESIAN_POINT('Ctrl Pts',(-2.1063054611613,1.72573455911939,7.53887321589169));
#393972=CARTESIAN_POINT('Ctrl Pts',(-2.10404472618889,1.72037508373168,
7.53220407452062));
#393973=CARTESIAN_POINT('Ctrl Pts',(-2.11096323199479,1.71530189958991,
7.53003438070911));
#393974=CARTESIAN_POINT('Ctrl Pts',(-2.09403873128105,1.69665408852716,
7.56669465659233));
#393975=CARTESIAN_POINT('Ctrl Pts',(-2.09179135683204,1.69132628664258,
7.560040858333));
#393976=CARTESIAN_POINT('Ctrl Pts',(-2.09866600104349,1.68625914572365,
7.55785582193789));
#393977=CARTESIAN_POINT('Ctrl Pts',(-2.08174904468027,1.66751919493523,
7.59443891967696));
#393978=CARTESIAN_POINT('Ctrl Pts',(-2.07949841181813,1.66218366840124,
7.58783901202978));
#393979=CARTESIAN_POINT('Ctrl Pts',(-2.08634511706894,1.65716352844335,
7.58560008491213));
#393980=CARTESIAN_POINT('',(-2.12257099619414,1.74271895653111,7.50366116523517));
#393981=CARTESIAN_POINT('Ctrl Pts',(-2.12257099619443,1.74271895653135,
7.50366116523554));
#393982=CARTESIAN_POINT('Ctrl Pts',(-2.1222181569283,1.74338951001098,7.50350835821027));
#393983=CARTESIAN_POINT('Ctrl Pts',(-2.12187199624793,1.74399443215019,
7.50345484956));
#393984=CARTESIAN_POINT('Ctrl Pts',(-2.121522743714,1.74455200602684,7.50349758195598));
#393985=CARTESIAN_POINT('Ctrl Pts',(-2.12134355126285,1.74483808277632,
7.50351950684424));
#393986=CARTESIAN_POINT('Ctrl Pts',(-2.12114599266841,1.74513996091748,
7.50357029184312));
#393987=CARTESIAN_POINT('Ctrl Pts',(-2.12094748749189,1.74542582197775,
7.50365515313924));
#393988=CARTESIAN_POINT('Ctrl Pts',(-2.12064210614772,1.74586559204503,
7.50378570417639));
#393989=CARTESIAN_POINT('Ctrl Pts',(-2.12032580549605,1.74628056165417,
7.50400001621911));
#393990=CARTESIAN_POINT('Ctrl Pts',(-2.12002085492926,1.74663776925506,
7.50428903009634));
#393991=CARTESIAN_POINT('Ctrl Pts',(-2.11998700776249,1.74667741655057,
7.50432110841318));
#393992=CARTESIAN_POINT('Ctrl Pts',(-2.11995329730374,1.74671638241371,
7.50435406373354));
#393993=CARTESIAN_POINT('Ctrl Pts',(-2.11991975139973,1.74675464400066,
7.50438785222352));
#393994=CARTESIAN_POINT('Ctrl Pts',(-2.11971493753151,1.74698824937983,
7.50459414719561));
#393995=CARTESIAN_POINT('Ctrl Pts',(-2.11951260910298,1.7471989807573,7.50483629897752));
#393996=CARTESIAN_POINT('Ctrl Pts',(-2.11932146656588,1.74737967653143,
7.5050991045531));
#393997=CARTESIAN_POINT('Ctrl Pts',(-2.11889978693057,1.74777830955833,
7.50567888004914));
#393998=CARTESIAN_POINT('Ctrl Pts',(-2.11851628850651,1.7480468494336,7.50637912803144));
#393999=CARTESIAN_POINT('Ctrl Pts',(-2.11818147603024,1.74821436622547,
7.50710440483569));
#394000=CARTESIAN_POINT('Ctrl Pts',(-2.11809937336411,1.74825544466851,
7.50728225710685));
#394001=CARTESIAN_POINT('Ctrl Pts',(-2.11801862920969,1.74829139658336,
7.50746498566954));
#394002=CARTESIAN_POINT('Ctrl Pts',(-2.11794129784965,1.74832176330878,
7.50764697238949));
#394003=CARTESIAN_POINT('Ctrl Pts',(-2.11752558574022,1.74848500646746,
7.50862528291181));
#394004=CARTESIAN_POINT('Ctrl Pts',(-2.11717227348488,1.74850551793847,
7.50965856837421));
#394005=CARTESIAN_POINT('Ctrl Pts',(-2.11686727706472,1.74844808225896,
7.51067959873201));
#394006=CARTESIAN_POINT('Ctrl Pts',(-2.11669943715,1.74841647533207,7.51124147302577));
#394007=CARTESIAN_POINT('Ctrl Pts',(-2.11654626822341,1.74836082893676,
7.51180065547252));
#394008=CARTESIAN_POINT('Ctrl Pts',(-2.11640602292632,1.74828929035805,
7.512351757165));
#394009=CARTESIAN_POINT('Ctrl Pts',(-2.11592141955782,1.74804209607103,
7.51425603304536));
#394010=CARTESIAN_POINT('Ctrl Pts',(-2.11553609727353,1.74757027707513,
7.51626900505181));
#394011=CARTESIAN_POINT('Ctrl Pts',(-2.11524938375525,1.74693418413988,
7.51827788969245));
#394012=CARTESIAN_POINT('Ctrl Pts',(-2.11523386627782,1.74689975758818,
7.51838661432546));
#394013=CARTESIAN_POINT('Ctrl Pts',(-2.11521864057722,1.7468648403287,7.51849533314857));
#394014=CARTESIAN_POINT('Ctrl Pts',(-2.11520370755653,1.74682943894029,
7.51860402984325));
#394015=CARTESIAN_POINT('Ctrl Pts',(-2.09059128339321,1.66719091666629,
7.57603338728985));
#394016=CARTESIAN_POINT('Ctrl Pts',(-2.10126987185163,1.69240886705185,
7.55196141284922));
#394017=CARTESIAN_POINT('Ctrl Pts',(-2.11192925636356,1.71758369907427,
7.52783573083105));
#394018=CARTESIAN_POINT('Ctrl Pts',(-2.12257099621211,1.7427189565875,7.50366116530176));
#394019=CARTESIAN_POINT('Origin',(-7.22395927215202E-16,5.76091528191151E-16,
7.49482233047033));
#394020=CARTESIAN_POINT('Origin',(-2.16435357359295,1.6761503090342,7.49482233047033));
#394021=CARTESIAN_POINT('Origin',(0.,0.,7.50366116523517));
#394022=CARTESIAN_POINT('Origin',(-2.11573969989723,1.73711017850878,7.49482233047033));
#394023=CARTESIAN_POINT('Ctrl Pts',(-2.17370884075826,1.67346483226478,
7.51860402984325));
#394024=CARTESIAN_POINT('Ctrl Pts',(-2.18120177269762,1.67478856070455,
7.51860402984325));
#394025=CARTESIAN_POINT('Ctrl Pts',(-2.18581900259086,1.66874062931084,
7.51860402984325));
#394026=CARTESIAN_POINT('Ctrl Pts',(-2.17649101774283,1.67395634041671,
7.51041458714366));
#394027=CARTESIAN_POINT('Ctrl Pts',(-2.18229563947574,1.6733557304783,7.51004642900443));
#394028=CARTESIAN_POINT('Ctrl Pts',(-2.18582027596804,1.66873896136317,
7.5072913648301));
#394029=CARTESIAN_POINT('Ctrl Pts',(-2.17698761422762,1.67672710369252,
7.50215815450137));
#394030=CARTESIAN_POINT('Ctrl Pts',(-2.18006852915933,1.67627320098812,
7.49877163671529));
#394031=CARTESIAN_POINT('Ctrl Pts',(-2.18218107690715,1.67354536932039,
7.4948158853317));
#394032=CARTESIAN_POINT('Ctrl Pts',(-2.17134139901513,1.68156192286896,
7.50366171572174));
#394033=CARTESIAN_POINT('Ctrl Pts',(-2.17423646662282,1.68380396341366,
7.50000045605858));
#394034=CARTESIAN_POINT('Ctrl Pts',(-2.17423646662289,1.68380396341356,
7.49482233047317));
#394035=CARTESIAN_POINT('Origin',(-2.17588346166999,1.66115544463215,7.51860402984325));
#394036=CARTESIAN_POINT('Origin',(-2.17588346166999,1.66115544463215,9.));
#394037=CARTESIAN_POINT('Origin',(-2.17588346166999,1.66115544463215,8.75721825406948));
#394038=CARTESIAN_POINT('Ctrl Pts',(-2.15726414129913,1.67056105650535,
8.78942910404913));
#394039=CARTESIAN_POINT('Ctrl Pts',(-2.16274816930574,1.6715499273384,8.79672699501691));
#394040=CARTESIAN_POINT('Ctrl Pts',(-2.16591835071273,1.66320586143329,
8.79893251111267));
#394041=CARTESIAN_POINT('Ctrl Pts',(-2.16809098556717,1.67247282582632,
8.78111911759582));
#394042=CARTESIAN_POINT('Ctrl Pts',(-2.17459368527152,1.67363781796381,
8.78644465894813));
#394043=CARTESIAN_POINT('Ctrl Pts',(-2.1790310498719,1.66685362256725,8.78817647674131));
#394044=CARTESIAN_POINT('Ctrl Pts',(-2.17483853316512,1.67366428603581,
8.76780923932031));
#394045=CARTESIAN_POINT('Ctrl Pts',(-2.18251559422621,1.67503449413488,
8.76988516158375));
#394046=CARTESIAN_POINT('Ctrl Pts',(-2.1872240108512,1.66912118767556,8.77093053738833));
#394047=CARTESIAN_POINT('Ctrl Pts',(-2.17352285373051,1.67343196759953,
8.75371302330491));
#394048=CARTESIAN_POINT('Ctrl Pts',(-2.18101136169898,1.67476929694336,
8.75300828287559));
#394049=CARTESIAN_POINT('Ctrl Pts',(-2.18562617275779,1.66867847940992,
8.75267964240737));
#394050=CARTESIAN_POINT('Origin',(-2.16207450435389,1.65871710925137,8.78727029226991));
#394051=CARTESIAN_POINT('Ctrl Pts',(-2.08949760778589,1.65859511954945,
8.85049129520029));
#394052=CARTESIAN_POINT('Ctrl Pts',(-2.09524826125082,1.6596105489903,8.85711686593484));
#394053=CARTESIAN_POINT('Ctrl Pts',(-2.09861675793329,1.65175217815315,
8.85933012996512));
#394054=CARTESIAN_POINT('Ctrl Pts',(-2.11299952442463,1.66274500237874,
8.82945683644724));
#394055=CARTESIAN_POINT('Ctrl Pts',(-2.11879791179024,1.66376886049789,
8.8360746990239));
#394056=CARTESIAN_POINT('Ctrl Pts',(-2.12214182911504,1.65587264245237,
8.8382956714852));
#394057=CARTESIAN_POINT('Ctrl Pts',(-2.1364664095614,1.66688869947303,8.80838214965002));
#394058=CARTESIAN_POINT('Ctrl Pts',(-2.14228768007071,1.66791659821434,
8.81501364461985));
#394059=CARTESIAN_POINT('Ctrl Pts',(-2.14563109864249,1.6599875147333,8.81722098428721));
#394060=CARTESIAN_POINT('Ctrl Pts',(-2.15990092504105,1.67102668085117,
8.78727029226991));
#394061=CARTESIAN_POINT('Ctrl Pts',(-2.16572316248257,1.67205475032985,
8.79393457792714));
#394062=CARTESIAN_POINT('Ctrl Pts',(-2.1690872949448,1.66409723639931,8.79610912703474));
#394063=CARTESIAN_POINT('Origin',(-2.09167118709872,1.64628554794964,8.85049129520029));
#394064=CARTESIAN_POINT('Ctrl Pts',(-2.08196763624131,1.66803740521007,
8.85049129520029));
#394065=CARTESIAN_POINT('Ctrl Pts',(-2.08423724752592,1.67341792347878,
8.85711686593484));
#394066=CARTESIAN_POINT('Ctrl Pts',(-2.07732546348033,1.67845061693467,
8.85933012996512));
#394067=CARTESIAN_POINT('Ctrl Pts',(-2.0799597439,1.66327733836635,8.86332496987233));
#394068=CARTESIAN_POINT('Ctrl Pts',(-2.07730478957506,1.66705928388543,
8.86648636486738));
#394069=CARTESIAN_POINT('Ctrl Pts',(-2.07172408849992,1.66512747711384,
8.87206031107457));
#394070=CARTESIAN_POINT('Ctrl Pts',(-2.08437551637401,1.65769067930626,
8.86341338519875));
#394071=CARTESIAN_POINT('Ctrl Pts',(-2.08745862058333,1.654231208383,8.86654584966058));
#394072=CARTESIAN_POINT('Ctrl Pts',(-2.08427206792284,1.64923420578852,
8.87215952290715));
#394073=CARTESIAN_POINT('Ctrl Pts',(-2.08949760778589,1.65859511954945,
8.85049129520029));
#394074=CARTESIAN_POINT('Ctrl Pts',(-2.09524826125082,1.6596105489903,8.85711686593484));
#394075=CARTESIAN_POINT('Ctrl Pts',(-2.09861675793329,1.65175217815315,
8.85933012996512));
#394076=CARTESIAN_POINT('Origin',(-2.07045035820038,1.67289562572049,8.85049129520029));
#394077=CARTESIAN_POINT('Ctrl Pts',(-2.10975372425561,1.73390928168093,
8.78727029226991));
#394078=CARTESIAN_POINT('Ctrl Pts',(-2.11205158759923,1.73935677649345,
8.79393457792714));
#394079=CARTESIAN_POINT('Ctrl Pts',(-2.10504217505422,1.74440727656295,
8.79610912703474));
#394080=CARTESIAN_POINT('Ctrl Pts',(-2.10050482043861,1.71198310591231,
8.80838214965002));
#394081=CARTESIAN_POINT('Ctrl Pts',(-2.10280230216296,1.71742969602831,
8.81501364461987));
#394082=CARTESIAN_POINT('Ctrl Pts',(-2.09581599798247,1.72245367517763,
8.81722098428721));
#394083=CARTESIAN_POINT('Ctrl Pts',(-2.09124314128409,1.69002664392797,
8.82945683644723));
#394084=CARTESIAN_POINT('Ctrl Pts',(-2.0935315917146,1.69545182375143,8.8360746990239));
#394085=CARTESIAN_POINT('Ctrl Pts',(-2.08657743994753,1.70046897590163,
8.8382956714852));
#394086=CARTESIAN_POINT('Ctrl Pts',(-2.08196763624131,1.66803740521007,
8.85049129520029));
#394087=CARTESIAN_POINT('Ctrl Pts',(-2.08423724752592,1.67341792347878,
8.85711686593484));
#394088=CARTESIAN_POINT('Ctrl Pts',(-2.07732546348033,1.67845061693467,
8.85933012996512));
#394089=CARTESIAN_POINT('Origin',(-2.09823644621467,1.73876750219135,8.78727029226991));
#394090=CARTESIAN_POINT('Ctrl Pts',(-2.11513172627181,1.74665884193264,
8.75374538247847));
#394091=CARTESIAN_POINT('Ctrl Pts',(-2.1180972113991,1.75365528934167,8.75304829418601));
#394092=CARTESIAN_POINT('Ctrl Pts',(-2.11319554002148,1.75950714895337,
8.75272238421917));
#394093=CARTESIAN_POINT('Ctrl Pts',(-2.11564474840764,1.74787505129053,
8.76769408445022));
#394094=CARTESIAN_POINT('Ctrl Pts',(-2.11868422291034,1.75504782967271,
8.7697431809397));
#394095=CARTESIAN_POINT('Ctrl Pts',(-2.11397434055921,1.76094997890146,
8.7707786988043));
#394096=CARTESIAN_POINT('Ctrl Pts',(-2.1130152892024,1.74164145494498,8.78108014887987));
#394097=CARTESIAN_POINT('Ctrl Pts',(-2.11559463262246,1.74771864383638,
8.78639403366323));
#394098=CARTESIAN_POINT('Ctrl Pts',(-2.10999049148816,1.75355950660449,
8.78812224174741));
#394099=CARTESIAN_POINT('Ctrl Pts',(-2.10870618599169,1.73142596662879,
8.78944554828686));
#394100=CARTESIAN_POINT('Ctrl Pts',(-2.11088511381239,1.73654540909543,
8.79673892988686));
#394101=CARTESIAN_POINT('Ctrl Pts',(-2.10346504981594,1.74148971942198,
8.79894799272499));
#394102=CARTESIAN_POINT('Origin',(-2.1036864295156,1.75168765945071,8.75721825406948));
#394103=CARTESIAN_POINT('Origin',(-2.1036864295156,1.75168765945071,9.));
#394104=CARTESIAN_POINT('Origin',(-2.1036864295156,1.75168765945071,7.51860402984325));
#394105=CARTESIAN_POINT('Ctrl Pts',(-2.12257038820296,1.74271845734518,
7.50366195182966));
#394106=CARTESIAN_POINT('Ctrl Pts',(-2.12540061176882,1.74504218845641,
7.50000065167735));
#394107=CARTESIAN_POINT('Ctrl Pts',(-2.12540061176874,1.7450421884565,7.49482233047108));
#394108=CARTESIAN_POINT('Ctrl Pts',(-2.11910931730508,1.74930441117484,
7.50215800491336));
#394109=CARTESIAN_POINT('Ctrl Pts',(-2.11935109582765,1.75241025088745,
7.49877273257265));
#394110=CARTESIAN_POINT('Ctrl Pts',(-2.11716053191478,1.7550783187452,7.49481816995649));
#394111=CARTESIAN_POINT('Ctrl Pts',(-2.1162994847363,1.74942630160733,7.51043025814042));
#394112=CARTESIAN_POINT('Ctrl Pts',(-2.11700967300595,1.75522185072787,
7.51006209594514));
#394113=CARTESIAN_POINT('Ctrl Pts',(-2.11329068351776,1.75968817890087,
7.50731281821698));
#394114=CARTESIAN_POINT('Ctrl Pts',(-2.11520312005229,1.74682804639183,
7.51860402984325));
#394115=CARTESIAN_POINT('Ctrl Pts',(-2.11816136938257,1.75383873667814,
7.51860402984324));
#394116=CARTESIAN_POINT('Ctrl Pts',(-2.11329230362298,1.75968623323816,
7.51860402984325));
#394117=CARTESIAN_POINT('Origin',(0.,0.,7.5));
#394118=CARTESIAN_POINT('Origin',(-2.18456153393019,1.53121811901791,7.5));
#394119=CARTESIAN_POINT('',(-2.18456153393019,1.53121811901791,7.59394543036555));
#394120=CARTESIAN_POINT('',(-2.18456153393019,1.53121811901791,8.85049129520029));
#394121=CARTESIAN_POINT('',(-2.18456153393019,1.53121811901791,7.5));
#394122=CARTESIAN_POINT('',(-2.21651095806264,1.59517439388234,8.78727029226991));
#394123=CARTESIAN_POINT('Ctrl Pts',(-2.18456153393019,1.53121811901791,
8.85049129520029));
#394124=CARTESIAN_POINT('Ctrl Pts',(-2.19522682250171,1.55256786618584,
8.82945686509571));
#394125=CARTESIAN_POINT('Ctrl Pts',(-2.20587625583214,1.57388587437302,
8.80838212259895));
#394126=CARTESIAN_POINT('Ctrl Pts',(-2.21651095806264,1.59517439388234,
8.78727029226991));
#394127=CARTESIAN_POINT('',(-2.22277754110617,1.60771882366395,8.75721825406948));
#394128=CARTESIAN_POINT('Origin',(-2.20391939936566,1.56996819257471,8.75937679713137));
#394129=CARTESIAN_POINT('',(-2.22277754110617,1.60771882366395,7.51860402984325));
#394130=CARTESIAN_POINT('',(-2.22277754110617,1.60771882366395,7.5));
#394131=CARTESIAN_POINT('Ctrl Pts',(-2.22277754110617,1.60771882366395,
7.51860402984325));
#394132=CARTESIAN_POINT('Ctrl Pts',(-2.2178561147635,1.59786712509837,7.52834476460825));
#394133=CARTESIAN_POINT('Ctrl Pts',(-2.21293149350187,1.58800903095223,
7.53807742314407));
#394134=CARTESIAN_POINT('Ctrl Pts',(-2.20800357004761,1.57814432648542,
7.54780169004674));
#394135=CARTESIAN_POINT('Ctrl Pts',(-2.20019800562761,1.56251916775178,
7.5632044032688));
#394136=CARTESIAN_POINT('Ctrl Pts',(-2.19238414650716,1.54687740470821,
7.57858609112103));
#394137=CARTESIAN_POINT('Ctrl Pts',(-2.18456153393019,1.53121811901791,
7.59394543036555));
#394138=CARTESIAN_POINT('Origin',(-2.46478898834976,1.55168238962918,7.5));
#394139=CARTESIAN_POINT('',(-2.2764630339942,1.53075663254068,8.75721825406948));
#394140=CARTESIAN_POINT('',(-2.26252622397768,1.52920804991439,8.78727029226991));
#394141=CARTESIAN_POINT('Origin',(-2.22714940198531,1.5252771696164,8.75658640621067));
#394142=CARTESIAN_POINT('',(-2.19147106502124,1.52131278661255,8.85049129520029));
#394143=CARTESIAN_POINT('Ctrl Pts',(-2.26252622397768,1.52920804991439,
8.78727029226991));
#394144=CARTESIAN_POINT('Ctrl Pts',(-2.2388747661514,1.52658002839205,8.80838212259895));
#394145=CARTESIAN_POINT('Ctrl Pts',(-2.21519054652501,1.52394836655644,
8.82945686509571));
#394146=CARTESIAN_POINT('Ctrl Pts',(-2.19147106502124,1.52131278661255,
8.85049129520029));
#394147=CARTESIAN_POINT('',(-2.19147106502124,1.52131278661255,7.59394543036555));
#394148=CARTESIAN_POINT('',(-2.19147106502124,1.52131278661255,7.5));
#394149=CARTESIAN_POINT('',(-2.2764630339942,1.53075663254068,7.51860402984325));
#394150=CARTESIAN_POINT('Ctrl Pts',(-2.19147106502124,1.52131278661255,
7.59394543036555));
#394151=CARTESIAN_POINT('Ctrl Pts',(-2.2088684671718,1.52324589143933,7.57858609112103));
#394152=CARTESIAN_POINT('Ctrl Pts',(-2.22624640173355,1.52517683313341,
7.56320440326857));
#394153=CARTESIAN_POINT('Ctrl Pts',(-2.24360588897529,1.52710572506147,
7.54780169004651));
#394154=CARTESIAN_POINT('Ctrl Pts',(-2.25456553516221,1.52832350141454,
7.53807742314383));
#394155=CARTESIAN_POINT('Ctrl Pts',(-2.26551783731018,1.52954046173788,
7.52834476460825));
#394156=CARTESIAN_POINT('Ctrl Pts',(-2.2764630339942,1.53075663254068,7.51860402984325));
#394157=CARTESIAN_POINT('',(-2.2764630339942,1.53075663254068,7.5));
#394158=CARTESIAN_POINT('Origin',(-2.19071182494583,1.52814573469576,7.5));
#394159=CARTESIAN_POINT('Ctrl Pts',(-2.19147106502124,1.52131278661255,
8.85049129520029));
#394160=CARTESIAN_POINT('Ctrl Pts',(-2.19127858807352,1.52129139961963,
8.85097269580138));
#394161=CARTESIAN_POINT('Ctrl Pts',(-2.19108761066503,1.52127864242607,
8.85143669361005));
#394162=CARTESIAN_POINT('Ctrl Pts',(-2.19088928063141,1.52127479994583,
8.8519052845931));
#394163=CARTESIAN_POINT('Ctrl Pts',(-2.19050135966328,1.52126728429815,
8.85282181883899));
#394164=CARTESIAN_POINT('Ctrl Pts',(-2.19009528511055,1.52129426370403,
8.85372622499636));
#394165=CARTESIAN_POINT('Ctrl Pts',(-2.18966570712695,1.5213715463367,8.85462257735071));
#394166=CARTESIAN_POINT('Ctrl Pts',(-2.18930908674213,1.52143570363352,
8.85536669723986));
#394167=CARTESIAN_POINT('Ctrl Pts',(-2.18893618151325,1.5215345120831,8.85610498449051));
#394168=CARTESIAN_POINT('Ctrl Pts',(-2.18854594865093,1.52168476007642,
8.85681338218371));
#394169=CARTESIAN_POINT('Ctrl Pts',(-2.1881918117155,1.52182111036632,8.85745625420284));
#394170=CARTESIAN_POINT('Ctrl Pts',(-2.18781874712325,1.52200097601188,
8.85808743050666));
#394171=CARTESIAN_POINT('Ctrl Pts',(-2.18742683720687,1.52225295490408,
8.85866804508411));
#394172=CARTESIAN_POINT('Ctrl Pts',(-2.18724601846702,1.5223692125027,8.85893592806396));
#394173=CARTESIAN_POINT('Ctrl Pts',(-2.1870612177365,1.52250106139575,8.85919241173848));
#394174=CARTESIAN_POINT('Ctrl Pts',(-2.18687285743162,1.52265285170287,
8.85943017985534));
#394175=CARTESIAN_POINT('Ctrl Pts',(-2.18661851525942,1.52285781355222,
8.8597512372));
#394176=CARTESIAN_POINT('Ctrl Pts',(-2.18635161117297,1.52310485014259,
8.86004599534705));
#394177=CARTESIAN_POINT('Ctrl Pts',(-2.18608242652933,1.52339863699004,
8.86026130871721));
#394178=CARTESIAN_POINT('Ctrl Pts',(-2.18598387044218,1.52350620063762,
8.86034014101235));
#394179=CARTESIAN_POINT('Ctrl Pts',(-2.1858835191395,1.52362163854734,8.86040910639693));
#394180=CARTESIAN_POINT('Ctrl Pts',(-2.18578436050156,1.52374202636577,
8.86046313645507));
#394181=CARTESIAN_POINT('Ctrl Pts',(-2.18562962427748,1.52392989054819,
8.8605474499083));
#394182=CARTESIAN_POINT('Ctrl Pts',(-2.18547368201656,1.52413503003229,
8.86059655985668));
#394183=CARTESIAN_POINT('Ctrl Pts',(-2.18532630154896,1.52434411130868,
8.86059725258815));
#394184=CARTESIAN_POINT('Ctrl Pts',(-2.18517858057361,1.52455367564636,
8.86059794692011));
#394185=CARTESIAN_POINT('Ctrl Pts',(-2.18503999426282,1.52477105478739,
8.86056369958366));
#394186=CARTESIAN_POINT('Ctrl Pts',(-2.18491492808122,1.52498236981287,
8.86048590497774));
#394187=CARTESIAN_POINT('Ctrl Pts',(-2.18488228953149,1.52503751674292,
8.86046560290182));
#394188=CARTESIAN_POINT('Ctrl Pts',(-2.18485022511722,1.52509301423803,
8.86044257503091));
#394189=CARTESIAN_POINT('Ctrl Pts',(-2.18481969723213,1.52514713095779,
8.86041778462583));
#394190=CARTESIAN_POINT('Ctrl Pts',(-2.18461428244746,1.52551126932848,
8.86025097596201));
#394191=CARTESIAN_POINT('Ctrl Pts',(-2.18445116098595,1.52586191704487,
8.8599848982295));
#394192=CARTESIAN_POINT('Ctrl Pts',(-2.18432741199719,1.52618526598102,
8.85968173251461));
#394193=CARTESIAN_POINT('Ctrl Pts',(-2.18426195587211,1.52635629904256,
8.85952137522076));
#394194=CARTESIAN_POINT('Ctrl Pts',(-2.18420607533321,1.52652292297257,
8.85934740853961));
#394195=CARTESIAN_POINT('Ctrl Pts',(-2.18415908454449,1.52668229371294,
8.8591675900182));
#394196=CARTESIAN_POINT('Ctrl Pts',(-2.18397039210246,1.52732225007481,
8.85844552518694));
#394197=CARTESIAN_POINT('Ctrl Pts',(-2.18391147471058,1.52788056619923,
8.85759444184121));
#394198=CARTESIAN_POINT('Ctrl Pts',(-2.18390432493829,1.52834010198268,
8.85683498915135));
#394199=CARTESIAN_POINT('Ctrl Pts',(-2.18390357673366,1.52838819117857,
8.85675551444995));
#394200=CARTESIAN_POINT('Ctrl Pts',(-2.18390341508026,1.52843519502018,
8.8566769979365));
#394201=CARTESIAN_POINT('Ctrl Pts',(-2.18390376336044,1.52848109083085,
8.85659965593547));
#394202=CARTESIAN_POINT('Ctrl Pts',(-2.18390846446407,1.52910059482535,
8.85555568965886));
#394203=CARTESIAN_POINT('Ctrl Pts',(-2.18400245115094,1.52969529761315,
8.85434650606346));
#394204=CARTESIAN_POINT('Ctrl Pts',(-2.18418004948775,1.53026910920421,
8.85297329937117));
#394205=CARTESIAN_POINT('Ctrl Pts',(-2.18427993773097,1.53059184326133,
8.85220095427747));
#394206=CARTESIAN_POINT('Ctrl Pts',(-2.18440661731194,1.53090800733086,
8.85137579139183));
#394207=CARTESIAN_POINT('Ctrl Pts',(-2.18456153393019,1.53121811901791,
8.85049129520029));
#394208=CARTESIAN_POINT('Origin',(-2.19071182494583,1.52814573469576,7.59394543036555));
#394209=CARTESIAN_POINT('Ctrl Pts',(-2.1909122395105,1.52125069295726,7.59443877723642));
#394210=CARTESIAN_POINT('Ctrl Pts',(-2.18515687443731,1.52061118805264,
7.58783886950016));
#394211=CARTESIAN_POINT('Ctrl Pts',(-2.18229230418495,1.52860327281232,
7.58559994247159));
#394212=CARTESIAN_POINT('Ctrl Pts',(-2.22233060858978,1.52474173146929,
7.56670252222134));
#394213=CARTESIAN_POINT('Ctrl Pts',(-2.21658356165307,1.52410315083086,
7.56004874999022));
#394214=CARTESIAN_POINT('Ctrl Pts',(-2.2136819051509,1.53213538257546,7.55786368756704));
#394215=CARTESIAN_POINT('Ctrl Pts',(-2.25369030700392,1.52822625081569,
7.53888913333559));
#394216=CARTESIAN_POINT('Ctrl Pts',(-2.24790910508591,1.52758387506124,
7.53222002137278));
#394217=CARTESIAN_POINT('Ctrl Pts',(-2.24501413171015,1.53565986254721,
7.53005029815326));
#394218=CARTESIAN_POINT('Ctrl Pts',(-2.28498991570528,1.53170409331962,
7.51101258149734));
#394219=CARTESIAN_POINT('Ctrl Pts',(-2.27913863511532,1.53105393080378,
7.5043616886572));
#394220=CARTESIAN_POINT('Ctrl Pts',(-2.27628742657589,1.53917662071595,
7.50217374673251));
#394221=CARTESIAN_POINT('',(-2.27461864350412,1.53898896096136,7.50366116523517));
#394222=CARTESIAN_POINT('Ctrl Pts',(-2.2764630339942,1.53075663254068,7.51860402984325));
#394223=CARTESIAN_POINT('Ctrl Pts',(-2.27690194403194,1.53080540183998,
7.51734760759494));
#394224=CARTESIAN_POINT('Ctrl Pts',(-2.27729199148657,1.530908604762,7.51608817408573));
#394225=CARTESIAN_POINT('Ctrl Pts',(-2.27762886352539,1.53107891334169,
7.5148100591312));
#394226=CARTESIAN_POINT('Ctrl Pts',(-2.27793401026797,1.53123318292284,
7.51365231206384));
#394227=CARTESIAN_POINT('Ctrl Pts',(-2.27819606868181,1.53144250802905,
7.51247773061043));
#394228=CARTESIAN_POINT('Ctrl Pts',(-2.27838745892557,1.53173211745978,
7.51129758471022));
#394229=CARTESIAN_POINT('Ctrl Pts',(-2.27862533514097,1.53209206890753,
7.50983079813402));
#394230=CARTESIAN_POINT('Ctrl Pts',(-2.27873558770847,1.53257173404272,
7.50839324291155));
#394231=CARTESIAN_POINT('Ctrl Pts',(-2.27863867677662,1.53319308108103,
7.50715379678855));
#394232=CARTESIAN_POINT('Ctrl Pts',(-2.27859390671852,1.53348012550905,
7.50658120839351));
#394233=CARTESIAN_POINT('Ctrl Pts',(-2.27848917168155,1.53383674900996,
7.50598221009429));
#394234=CARTESIAN_POINT('Ctrl Pts',(-2.27830513945913,1.53424805484198,
7.50545747549611));
#394235=CARTESIAN_POINT('Ctrl Pts',(-2.27820693416891,1.53446754036505,
7.50517746087247));
#394236=CARTESIAN_POINT('Ctrl Pts',(-2.27808526799904,1.53470506004889,
7.50491486231392));
#394237=CARTESIAN_POINT('Ctrl Pts',(-2.27794187829259,1.53495356351543,
7.50468370960992));
#394238=CARTESIAN_POINT('Ctrl Pts',(-2.27772746545172,1.53532515458389,
7.50433806340446));
#394239=CARTESIAN_POINT('Ctrl Pts',(-2.27745756787721,1.53573216943126,
7.50405484070983));
#394240=CARTESIAN_POINT('Ctrl Pts',(-2.27714976561519,1.53614680044923,
7.5038576603613));
#394241=CARTESIAN_POINT('Ctrl Pts',(-2.2771168509476,1.53619113879177,7.5038365749879));
#394242=CARTESIAN_POINT('Ctrl Pts',(-2.27708352897817,1.53623555321376,
7.50381643264937));
#394243=CARTESIAN_POINT('Ctrl Pts',(-2.27704984031696,1.53628000200858,
7.50379723213559));
#394244=CARTESIAN_POINT('Ctrl Pts',(-2.27682495748309,1.53657671225428,
7.50366906242519));
#394245=CARTESIAN_POINT('Ctrl Pts',(-2.27657827008934,1.53688097395988,
7.50358235568538));
#394246=CARTESIAN_POINT('Ctrl Pts',(-2.2763334441752,1.53716852914519,7.5035341175365));
#394247=CARTESIAN_POINT('Ctrl Pts',(-2.27596635542588,1.5375996856006,7.50346178989176));
#394248=CARTESIAN_POINT('Ctrl Pts',(-2.27555311919225,1.53804790364341,
7.50346967198526));
#394249=CARTESIAN_POINT('Ctrl Pts',(-2.27513391008214,1.53847543241701,
7.50354272648692));
#394250=CARTESIAN_POINT('Ctrl Pts',(-2.27496148069803,1.53865128385091,
7.50357277531559));
#394251=CARTESIAN_POINT('Ctrl Pts',(-2.27478837114252,1.53882350060341,
7.50361331098761));
#394252=CARTESIAN_POINT('Ctrl Pts',(-2.2746186435053,1.53898896096215,7.50366116523658));
#394253=CARTESIAN_POINT('',(-2.19311322794402,1.52982084947248,7.57603338622103));
#394254=CARTESIAN_POINT('Origin',(-2.20035940734066,1.53487894928966,7.58486873427627));
#394255=CARTESIAN_POINT('Ctrl Pts',(-2.27461864356146,1.53898896096242,
7.50366116529969));
#394256=CARTESIAN_POINT('Ctrl Pts',(-2.24749441162106,1.53593874122536,
7.52783573079709));
#394257=CARTESIAN_POINT('Ctrl Pts',(-2.2203272205278,1.5328828661625,7.55196141284068));
#394258=CARTESIAN_POINT('Ctrl Pts',(-2.1931132291771,1.52982084925532,7.57603338728831));
#394259=CARTESIAN_POINT('Ctrl Pts',(-2.19147106502124,1.52131278661255,
7.59394543036555));
#394260=CARTESIAN_POINT('Ctrl Pts',(-2.1789164401766,1.51991778489473,7.59394543036555));
#394261=CARTESIAN_POINT('Ctrl Pts',(-2.18456153393019,1.53121811901791,
7.59394543036555));
#394262=CARTESIAN_POINT('Ctrl Pts',(-2.18915221929748,1.52105512907136,
7.58587155981958));
#394263=CARTESIAN_POINT('Ctrl Pts',(-2.18371352266056,1.52326402197318,
7.58685956158229));
#394264=CARTESIAN_POINT('Ctrl Pts',(-2.1835188821845,1.52913094144129,7.58587155981959));
#394265=CARTESIAN_POINT('Ctrl Pts',(-2.19108705088142,1.5260901058675,7.57982961904599));
#394266=CARTESIAN_POINT('Ctrl Pts',(-2.18864592315195,1.52670465103599,
7.58148017275034));
#394267=CARTESIAN_POINT('Ctrl Pts',(-2.18891227212867,1.52920781474972,
7.57982961904595));
#394268=CARTESIAN_POINT('Ctrl Pts',(-2.19311322726539,1.52982084899885,
7.57603338509286));
#394269=CARTESIAN_POINT('Ctrl Pts',(-2.19311322726539,1.52982084899885,
7.57603338509286));
#394270=CARTESIAN_POINT('Ctrl Pts',(-2.19311322726539,1.52982084899885,
7.57603338509286));
#394271=CARTESIAN_POINT('Origin',(-2.20036267203999,1.53487426909781,7.5848687342762));
#394272=CARTESIAN_POINT('Ctrl Pts',(-2.22662370789094,1.6154180704185,7.51098857897448));
#394273=CARTESIAN_POINT('Ctrl Pts',(-2.22399271106278,1.61015134775046,
7.50433767179957));
#394274=CARTESIAN_POINT('Ctrl Pts',(-2.23063092687409,1.60467027651165,
7.50214974420965));
#394275=CARTESIAN_POINT('Ctrl Pts',(-2.21254602352188,1.58723739814004,
7.53887321589168));
#394276=CARTESIAN_POINT('Ctrl Pts',(-2.2099465507049,1.5820337801563,7.53220407452062));
#394277=CARTESIAN_POINT('Ctrl Pts',(-2.21652580167462,1.57652774922654,
7.53003438070912));
#394278=CARTESIAN_POINT('Ctrl Pts',(-2.19844130480579,1.55900260857537,
7.5666946565923));
#394279=CARTESIAN_POINT('Ctrl Pts',(-2.19585719438986,1.55382974300644,
7.56004085833292));
#394280=CARTESIAN_POINT('Ctrl Pts',(-2.20239306107414,1.54833255310514,
7.55785582193789));
#394281=CARTESIAN_POINT('Ctrl Pts',(-2.18431018964265,1.53071497867106,
7.59443891967696));
#394282=CARTESIAN_POINT('Ctrl Pts',(-2.18172233258836,1.52553461309114,
7.58783901202978));
#394283=CARTESIAN_POINT('Ctrl Pts',(-2.18823332907749,1.52008611763764,
7.58560008491213));
#394284=CARTESIAN_POINT('',(-2.22986633334694,1.60314476287806,7.50366116523517));
#394285=CARTESIAN_POINT('Ctrl Pts',(-2.22986633334724,1.60314476287828,
7.50366116523554));
#394286=CARTESIAN_POINT('Ctrl Pts',(-2.22955718153618,1.60383654512327,
7.50350835821027));
#394287=CARTESIAN_POINT('Ctrl Pts',(-2.22925048957458,1.60446240297601,
7.50345484956));
#394288=CARTESIAN_POINT('Ctrl Pts',(-2.22893767849837,1.60504120794401,
7.50349758195598));
#394289=CARTESIAN_POINT('Ctrl Pts',(-2.2287771832176,1.60533817781789,7.50351950684424));
#394290=CARTESIAN_POINT('Ctrl Pts',(-2.22859937192739,1.60565209334063,
7.50357029184312));
#394291=CARTESIAN_POINT('Ctrl Pts',(-2.22841958978206,1.60595008533902,
7.50365515313923));
#394292=CARTESIAN_POINT('Ctrl Pts',(-2.22814301204157,1.60640851770143,
7.50378570417639));
#394293=CARTESIAN_POINT('Ctrl Pts',(-2.22785394845765,1.60684290016334,
7.50400001621911));
#394294=CARTESIAN_POINT('Ctrl Pts',(-2.22757251081407,1.6072189120928,7.50428903009635));
#394295=CARTESIAN_POINT('Ctrl Pts',(-2.22754127340089,1.60726064652411,
7.50432110841318));
#394296=CARTESIAN_POINT('Ctrl Pts',(-2.22751012875531,1.60730169216422,
7.50435406373354));
#394297=CARTESIAN_POINT('Ctrl Pts',(-2.22747910320325,1.60734202443208,
7.50438785222352));
#394298=CARTESIAN_POINT('Ctrl Pts',(-2.22728967729513,1.60758827231354,
7.50459414719561));
#394299=CARTESIAN_POINT('Ctrl Pts',(-2.22710126617777,1.60781153394771,
7.50483629897752));
#394300=CARTESIAN_POINT('Ctrl Pts',(-2.2269220935815,1.60800410500739,7.5050991045531));
#394301=CARTESIAN_POINT('Ctrl Pts',(-2.22652682083796,1.60842893610698,
7.50567888004914));
#394302=CARTESIAN_POINT('Ctrl Pts',(-2.22616131576142,1.60872149506667,
7.50637912803144));
#394303=CARTESIAN_POINT('Ctrl Pts',(-2.225837924031,1.60891011918632,7.50710440483569));
#394304=CARTESIAN_POINT('Ctrl Pts',(-2.22575862195848,1.60895637356518,
7.50728225710685));
#394305=CARTESIAN_POINT('Ctrl Pts',(-2.22568034714868,1.60899742490871,
7.50746498566954));
#394306=CARTESIAN_POINT('Ctrl Pts',(-2.22560512027699,1.60903268387968,
7.50764697238949));
#394307=CARTESIAN_POINT('Ctrl Pts',(-2.22520072131776,1.60922222640408,
7.50862528291182));
#394308=CARTESIAN_POINT('Ctrl Pts',(-2.2248494491548,1.609265332526,7.50965856837422));
#394309=CARTESIAN_POINT('Ctrl Pts',(-2.22454139946587,1.60922755604198,
7.51067959873202));
#394310=CARTESIAN_POINT('Ctrl Pts',(-2.2243718793335,1.60920676759517,7.51124147302578));
#394311=CARTESIAN_POINT('Ctrl Pts',(-2.22421545983211,1.60916104909817,
7.51180065547253));
#394312=CARTESIAN_POINT('Ctrl Pts',(-2.22407091919156,1.60909864305018,
7.51235175716501));
#394313=CARTESIAN_POINT('Ctrl Pts',(-2.22357147370029,1.60888300529476,
7.51425603304536));
#394314=CARTESIAN_POINT('Ctrl Pts',(-2.2231567135551,1.6084368433851,7.51626900505181));
#394315=CARTESIAN_POINT('Ctrl Pts',(-2.22282983450621,1.60782042716919,
7.51827788969245));
#394316=CARTESIAN_POINT('Ctrl Pts',(-2.22281214319437,1.60778706555872,
7.51838661432546));
#394317=CARTESIAN_POINT('Ctrl Pts',(-2.2227947116201,1.60775319555449,7.51849533314857));
#394318=CARTESIAN_POINT('Ctrl Pts',(-2.22277754110616,1.60771882366395,
7.51860402984325));
#394319=CARTESIAN_POINT('Ctrl Pts',(-2.19311322816692,1.52982085070557,
7.57603338728985));
#394320=CARTESIAN_POINT('Ctrl Pts',(-2.20538559594875,1.55430280859583,
7.55196141284922));
#394321=CARTESIAN_POINT('Ctrl Pts',(-2.21763603663764,1.57874296711533,
7.52783573083105));
#394322=CARTESIAN_POINT('Ctrl Pts',(-2.22986633336848,1.60314476293318,
7.50366116530176));
#394323=CARTESIAN_POINT('Origin',(-7.5782199824625E-16,5.28623820391011E-16,
7.49482233047033));
#394324=CARTESIAN_POINT('Origin',(-2.26729799607037,1.53403586888159,7.49482233047033));
#394325=CARTESIAN_POINT('Origin',(0.,0.,7.50366116523517));
#394326=CARTESIAN_POINT('Origin',(-2.22268971703921,1.59798519134821,7.49482233047033));
#394327=CARTESIAN_POINT('Ctrl Pts',(-2.27646198274857,1.53075651568695,
7.51860402984325));
#394328=CARTESIAN_POINT('Ctrl Pts',(-2.28402433122797,1.53159745058702,
7.51860402984325));
#394329=CARTESIAN_POINT('Ctrl Pts',(-2.28824458223238,1.52526611838203,
7.51860402984325));
#394330=CARTESIAN_POINT('Ctrl Pts',(-2.27926993448757,1.53106875929124,
7.51041458714366));
#394331=CARTESIAN_POINT('Ctrl Pts',(-2.28502414879171,1.53009747997903,
7.51004642900442));
#394332=CARTESIAN_POINT('Ctrl Pts',(-2.2882457461275,1.52526437227578,7.50729136483009));
#394333=CARTESIAN_POINT('Ctrl Pts',(-2.2799430340742,1.53380201269071,7.50215815450138));
#394334=CARTESIAN_POINT('Ctrl Pts',(-2.28298853728963,1.53315164768069,
7.4987716367153));
#394335=CARTESIAN_POINT('Ctrl Pts',(-2.28492197180652,1.53029406923675,
7.49481588533172));
#394336=CARTESIAN_POINT('Ctrl Pts',(-2.27461818754462,1.53898865246334,
7.50366171572174));
#394337=CARTESIAN_POINT('Ctrl Pts',(-2.27765095495632,1.5410405988768,7.50000045605858));
#394338=CARTESIAN_POINT('Ctrl Pts',(-2.27765095495639,1.5410405988767,7.49482233047317));
#394339=CARTESIAN_POINT('Origin',(-2.27784347049496,1.5183330905712,7.51860402984325));
#394340=CARTESIAN_POINT('Origin',(-2.27784347049496,1.5183330905712,9.));
#394341=CARTESIAN_POINT('Origin',(-2.27784347049496,1.5183330905712,8.75721825406948));
#394342=CARTESIAN_POINT('Ctrl Pts',(-2.25986502513649,1.52891232155811,
8.78942910404912));
#394343=CARTESIAN_POINT('Ctrl Pts',(-2.2654011427912,1.52954779776922,8.79672699501689));
#394344=CARTESIAN_POINT('Ctrl Pts',(-2.26803020458242,1.52101776142228,
8.79893251111266));
#394345=CARTESIAN_POINT('Ctrl Pts',(-2.27079211197273,1.53012648465002,
8.78111911759583));
#394346=CARTESIAN_POINT('Ctrl Pts',(-2.27735609248566,1.5308724537857,8.78644465894817));
#394347=CARTESIAN_POINT('Ctrl Pts',(-2.28134967515312,1.5238178943201,8.78817647674132));
#394348=CARTESIAN_POINT('Ctrl Pts',(-2.27760213312821,1.5308831800178,8.76780923932029));
#394349=CARTESIAN_POINT('Ctrl Pts',(-2.28535121037833,1.53175870188639,
8.7698851615837));
#394350=CARTESIAN_POINT('Ctrl Pts',(-2.28967108621071,1.52555587566046,
8.77093053738832));
#394351=CARTESIAN_POINT('Ctrl Pts',(-2.27627427220477,1.53073563477546,
8.75371302330492));
#394352=CARTESIAN_POINT('Ctrl Pts',(-2.28383307721573,1.53159042607986,
8.7530082828756));
#394353=CARTESIAN_POINT('Ctrl Pts',(-2.28804816663106,1.52521645082458,
8.75267964240738));
#394354=CARTESIAN_POINT('Origin',(-2.26390666047844,1.51678450794491,8.78727029226991));
#394355=CARTESIAN_POINT('Ctrl Pts',(-2.19147106502124,1.52131278661255,
8.85049129520029));
#394356=CARTESIAN_POINT('Ctrl Pts',(-2.19727496193953,1.52195768411218,
8.85711686593484));
#394357=CARTESIAN_POINT('Ctrl Pts',(-2.20013305013607,1.51389963881728,
8.85933012996512));
#394358=CARTESIAN_POINT('Ctrl Pts',(-2.21519057835742,1.52394837009348,
8.8294568364472));
#394359=CARTESIAN_POINT('Ctrl Pts',(-2.2210426511292,1.52459862063228,8.83607469902385));
#394360=CARTESIAN_POINT('Ctrl Pts',(-2.2238737855901,1.516504380695,8.83829567148519));
#394361=CARTESIAN_POINT('Ctrl Pts',(-2.23887473584625,1.52658002502471,
8.80838214965002));
#394362=CARTESIAN_POINT('Ctrl Pts',(-2.24474990362954,1.52723284175572,
8.81501364461992));
#394363=CARTESIAN_POINT('Ctrl Pts',(-2.24757843466631,1.51910583586367,
8.81722098428721));
#394364=CARTESIAN_POINT('Ctrl Pts',(-2.26252622397768,1.52920804991439,
8.78727029226991));
#394365=CARTESIAN_POINT('Ctrl Pts',(-2.2684023676456,1.5298609750804,8.79393457792714));
#394366=CARTESIAN_POINT('Ctrl Pts',(-2.27124974846885,1.52170427000877,
8.79610912703474));
#394367=CARTESIAN_POINT('Origin',(-2.192851501522,1.50888924464307,8.85049129520029));
#394368=CARTESIAN_POINT('Ctrl Pts',(-2.18456153393019,1.53121811901791,
8.85049129520029));
#394369=CARTESIAN_POINT('Ctrl Pts',(-2.18717121304409,1.5364421679405,8.85711686593484));
#394370=CARTESIAN_POINT('Ctrl Pts',(-2.18059607577692,1.54190736071219,
8.85933012996512));
#394371=CARTESIAN_POINT('Ctrl Pts',(-2.18225278848925,1.52659647834605,
8.86332496987231));
#394372=CARTESIAN_POINT('Ctrl Pts',(-2.17984559913406,1.53054075696006,
8.86648636486738));
#394373=CARTESIAN_POINT('Ctrl Pts',(-2.174152592923,1.52897047603821,8.87206031107457));
#394374=CARTESIAN_POINT('Ctrl Pts',(-2.18630154981016,1.52073837816236,
8.86341338519877));
#394375=CARTESIAN_POINT('Ctrl Pts',(-2.18915667038817,1.51708847992824,
8.86654584966059));
#394376=CARTESIAN_POINT('Ctrl Pts',(-2.1856565057864,1.51230590734145,8.87215952290715));
#394377=CARTESIAN_POINT('Ctrl Pts',(-2.19147106502124,1.52131278661255,
8.85049129520029));
#394378=CARTESIAN_POINT('Ctrl Pts',(-2.19727496193953,1.52195768411218,
8.85711686593484));
#394379=CARTESIAN_POINT('Ctrl Pts',(-2.20013305013607,1.51389963881728,
8.85933012996512));
#394380=CARTESIAN_POINT('Origin',(-2.17337918662904,1.53680427233091,8.85049129520029));
#394381=CARTESIAN_POINT('Ctrl Pts',(-2.21651095806264,1.59517439388234,
8.78727029226991));
#394382=CARTESIAN_POINT('Ctrl Pts',(-2.21915312239057,1.60046347162262,
8.79393457792714));
#394383=CARTESIAN_POINT('Ctrl Pts',(-2.21248169808585,1.60595268950176,
8.79610912703474));
#394384=CARTESIAN_POINT('Ctrl Pts',(-2.20587624220566,1.57388584709556,
8.80838214965002));
#394385=CARTESIAN_POINT('Ctrl Pts',(-2.2085179677343,1.57917404644853,8.81501364461987));
#394386=CARTESIAN_POINT('Ctrl Pts',(-2.20186790511427,1.58463531733957,
8.81722098428721));
#394387=CARTESIAN_POINT('Ctrl Pts',(-2.19522683681493,1.552567894838,8.82945683644722));
#394388=CARTESIAN_POINT('Ctrl Pts',(-2.19785817784333,1.55783530652516,
8.83607469902391));
#394389=CARTESIAN_POINT('Ctrl Pts',(-2.19123976416883,1.56328770443168,
8.8382956714852));
#394390=CARTESIAN_POINT('Ctrl Pts',(-2.18456153393019,1.53121811901791,
8.85049129520029));
#394391=CARTESIAN_POINT('Ctrl Pts',(-2.18717121304409,1.5364421679405,8.85711686593484));
#394392=CARTESIAN_POINT('Ctrl Pts',(-2.18059607577692,1.54190736071219,
8.85933012996512));
#394393=CARTESIAN_POINT('Origin',(-2.20532861076149,1.60076054719534,8.78727029226991));
#394394=CARTESIAN_POINT('Ctrl Pts',(-2.2226947775269,1.60755318902291,8.75374538247848));
#394395=CARTESIAN_POINT('Ctrl Pts',(-2.22610243367153,1.61434526219592,
8.75304829418602));
#394396=CARTESIAN_POINT('Ctrl Pts',(-2.22158576323608,1.62049914969785,
8.75272238421917));
#394397=CARTESIAN_POINT('Ctrl Pts',(-2.22328466840483,1.60873403010711,
8.7676940844502));
#394398=CARTESIAN_POINT('Ctrl Pts',(-2.22677745946999,1.6156973314468,8.76974318093968));
#394399=CARTESIAN_POINT('Ctrl Pts',(-2.22245540607675,1.6218891172753,8.7707786988043));
#394400=CARTESIAN_POINT('Ctrl Pts',(-2.22026122381643,1.60268171138357,
8.78108014887991));
#394401=CARTESIAN_POINT('Ctrl Pts',(-2.22322463452793,1.60858115493827,
8.78639403366325));
#394402=CARTESIAN_POINT('Ctrl Pts',(-2.21800623306505,1.61476907558264,
8.78812224174741));
#394403=CARTESIAN_POINT('Ctrl Pts',(-2.21530646553677,1.59276329707432,
8.78944554828686));
#394404=CARTESIAN_POINT('Ctrl Pts',(-2.21780892032157,1.59773261671256,
8.79673892988686));
#394405=CARTESIAN_POINT('Ctrl Pts',(-2.21072088469269,1.60314217355579,
8.79894799272499));
#394406=CARTESIAN_POINT('Origin',(-2.21159519380501,1.61330497697695,8.75721825406948));
#394407=CARTESIAN_POINT('Origin',(-2.21159519380501,1.61330497697695,9.));
#394408=CARTESIAN_POINT('Origin',(-2.21159519380501,1.61330497697695,7.51860402984325));
#394409=CARTESIAN_POINT('Ctrl Pts',(-2.22986569462199,1.60314430367188,
7.50366195182966));
#394410=CARTESIAN_POINT('Ctrl Pts',(-2.23283898515346,1.60528192738187,
7.50000065167735));
#394411=CARTESIAN_POINT('Ctrl Pts',(-2.2328389851534,1.60528192738197,7.49482233047108));
#394412=CARTESIAN_POINT('Ctrl Pts',(-2.22683369837612,1.60993847752686,
7.50215800491336));
#394413=CARTESIAN_POINT('Ctrl Pts',(-2.22727397197241,1.61302244515553,
7.49877273257266));
#394414=CARTESIAN_POINT('Ctrl Pts',(-2.22525885250261,1.6158253810935,7.49481816995649));
#394415=CARTESIAN_POINT('Ctrl Pts',(-2.22403744845653,1.61024014411319,
7.51043025814043));
#394416=CARTESIAN_POINT('Ctrl Pts',(-2.22511749967526,1.61597828373783,
7.51006209594513));
#394417=CARTESIAN_POINT('Ctrl Pts',(-2.22169230987838,1.62067371183521,
7.50731281821698));
#394418=CARTESIAN_POINT('Ctrl Pts',(-2.22277686558813,1.60771747161815,
7.51860402984325));
#394419=CARTESIAN_POINT('Ctrl Pts',(-2.22617821334674,1.61452422200403,
7.51860402984324));
#394420=CARTESIAN_POINT('Ctrl Pts',(-2.2216938019959,1.62067166636954,7.51860402984325));
#394421=CARTESIAN_POINT('Origin',(0.,0.,7.5));
#394422=CARTESIAN_POINT('Origin',(-2.27817859968918,1.38810672912945,7.5));
#394423=CARTESIAN_POINT('',(-2.27817859968918,1.38810672912945,7.59394543036555));
#394424=CARTESIAN_POINT('',(-2.27817859968918,1.38810672912945,8.85049129520029));
#394425=CARTESIAN_POINT('',(-2.27817859968918,1.38810672912945,7.5));
#394426=CARTESIAN_POINT('',(-2.31416007290289,1.44988459233546,8.78727029226991));
#394427=CARTESIAN_POINT('Ctrl Pts',(-2.27817859968918,1.38810672912945,
8.85049129520029));
#394428=CARTESIAN_POINT('Ctrl Pts',(-2.29018985827906,1.40872928356713,
8.82945686509571));
#394429=CARTESIAN_POINT('Ctrl Pts',(-2.30218326068067,1.429321180084,8.80838212259896));
#394430=CARTESIAN_POINT('Ctrl Pts',(-2.31416007290289,1.44988459233546,
8.78727029226991));
#394431=CARTESIAN_POINT('',(-2.3212175049551,1.46200174688657,8.75721825406948));
#394432=CARTESIAN_POINT('Origin',(-2.29997941805091,1.42553692380718,8.7593767971313));
#394433=CARTESIAN_POINT('',(-2.3212175049551,1.46200174688657,7.51860402984325));
#394434=CARTESIAN_POINT('',(-2.3212175049551,1.46200174688657,7.5));
#394435=CARTESIAN_POINT('Ctrl Pts',(-2.3212175049551,1.46200174688657,7.51860402984325));
#394436=CARTESIAN_POINT('Ctrl Pts',(-2.31567498971639,1.45248560656067,
7.52834476460825));
#394437=CARTESIAN_POINT('Ctrl Pts',(-2.31012887635678,1.44296328849379,
7.53807742314407));
#394438=CARTESIAN_POINT('Ctrl Pts',(-2.30457904406455,1.43343458526006,
7.54780169004674));
#394439=CARTESIAN_POINT('Ctrl Pts',(-2.29578840965649,1.41834163432029,
7.5632044032688));
#394440=CARTESIAN_POINT('Ctrl Pts',(-2.28698843374855,1.40323264462921,
7.57858609112103));
#394441=CARTESIAN_POINT('Ctrl Pts',(-2.27817859968918,1.38810672912945,
7.59394543036555));
#394442=CARTESIAN_POINT('Origin',(-2.55914144706915,1.39057471905267,7.5));
#394443=CARTESIAN_POINT('',(-2.36986171072478,1.38175804150002,8.75721825406948));
#394444=CARTESIAN_POINT('',(-2.35585431734964,1.38110557508641,8.78727029226991));
#394445=CARTESIAN_POINT('Origin',(-2.32029832846756,1.37944937197089,8.75658640621095));
#394446=CARTESIAN_POINT('',(-2.28443929758136,1.37777905311489,8.85049129520029));
#394447=CARTESIAN_POINT('Ctrl Pts',(-2.35585431734964,1.38110557508641,
8.78727029226991));
#394448=CARTESIAN_POINT('Ctrl Pts',(-2.33208307606302,1.37999830722194,
8.80838212259896));
#394449=CARTESIAN_POINT('Ctrl Pts',(-2.30827890705325,1.37888950557934,
8.82945686509571));
#394450=CARTESIAN_POINT('Ctrl Pts',(-2.28443929758136,1.37777905311489,
8.85049129520029));
#394451=CARTESIAN_POINT('',(-2.28443929758136,1.37777905311489,7.59394543036555));
#394452=CARTESIAN_POINT('',(-2.28443929758136,1.37777905311489,7.5));
#394453=CARTESIAN_POINT('',(-2.36986171072478,1.38175804150002,7.51860402984325));
#394454=CARTESIAN_POINT('Ctrl Pts',(-2.28443929758136,1.37777905311489,
7.59394543036555));
#394455=CARTESIAN_POINT('Ctrl Pts',(-2.30192480935483,1.37859353078761,
7.57858609112103));
#394456=CARTESIAN_POINT('Ctrl Pts',(-2.31939075494535,1.3794070970647,7.56320440326857));
#394457=CARTESIAN_POINT('Ctrl Pts',(-2.3368381597889,1.38021979971109,7.54780169004651));
#394458=CARTESIAN_POINT('Ctrl Pts',(-2.34785331140614,1.38073288706993,
7.53807742314383));
#394459=CARTESIAN_POINT('Ctrl Pts',(-2.35886108179035,1.38124563060985,
7.52834476460825));
#394460=CARTESIAN_POINT('Ctrl Pts',(-2.36986171072478,1.38175804150002,
7.51860402984325));
#394461=CARTESIAN_POINT('',(-2.36986171072478,1.38175804150002,7.5));
#394462=CARTESIAN_POINT('Origin',(-2.28411940593292,1.38464660685209,7.5));
#394463=CARTESIAN_POINT('Ctrl Pts',(-2.28443929758136,1.37777905311489,
8.85049129520029));
#394464=CARTESIAN_POINT('Ctrl Pts',(-2.28424584582882,1.37777004210422,
8.85097269580138));
#394465=CARTESIAN_POINT('Ctrl Pts',(-2.28405444344771,1.37776954708626,
8.85143669361005));
#394466=CARTESIAN_POINT('Ctrl Pts',(-2.28385627471586,1.37777841954969,
8.8519052845931));
#394467=CARTESIAN_POINT('Ctrl Pts',(-2.28346866924376,1.37779577352548,
8.85282181883899));
#394468=CARTESIAN_POINT('Ctrl Pts',(-2.28306515759123,1.3778487147852,8.85372622499636));
#394469=CARTESIAN_POINT('Ctrl Pts',(-2.28264141373694,1.37795336178832,
8.85462257735071));
#394470=CARTESIAN_POINT('Ctrl Pts',(-2.28228963663907,1.3780402360136,8.85536669723986));
#394471=CARTESIAN_POINT('Ctrl Pts',(-2.28192382826308,1.37816273357066,
8.85610498449051));
#394472=CARTESIAN_POINT('Ctrl Pts',(-2.281544023598,1.3783376751687,8.85681338218371));
#394473=CARTESIAN_POINT('Ctrl Pts',(-2.28119935026796,1.37849643494367,
8.85745625420284));
#394474=CARTESIAN_POINT('Ctrl Pts',(-2.2808385762084,1.37869983336645,8.85808743050665));
#394475=CARTESIAN_POINT('Ctrl Pts',(-2.28046361585604,1.37897640429555,
8.8586680450841));
#394476=CARTESIAN_POINT('Ctrl Pts',(-2.2802906172776,1.37910400812691,8.85893592806395));
#394477=CARTESIAN_POINT('Ctrl Pts',(-2.28011464382758,1.37924742634572,
8.85919241173848));
#394478=CARTESIAN_POINT('Ctrl Pts',(-2.27993639576751,1.37941097306954,
8.85943017985534));
#394479=CARTESIAN_POINT('Ctrl Pts',(-2.27969570811935,1.37963180956172,
8.8597512372));
#394480=CARTESIAN_POINT('Ctrl Pts',(-2.27944518010467,1.37989543919245,
8.86004599534705));
#394481=CARTESIAN_POINT('Ctrl Pts',(-2.2791953715177,1.38020586914265,8.86026130871721));
#394482=CARTESIAN_POINT('Ctrl Pts',(-2.27910390955115,1.38031952629937,
8.86034014101235));
#394483=CARTESIAN_POINT('Ctrl Pts',(-2.27901116056326,1.38044115655956,
8.86040910639693));
#394484=CARTESIAN_POINT('Ctrl Pts',(-2.27891991893138,1.38056765014405,
8.86046313645507));
#394485=CARTESIAN_POINT('Ctrl Pts',(-2.27877753712897,1.38076504232326,
8.8605474499083));
#394486=CARTESIAN_POINT('Ctrl Pts',(-2.27863505860002,1.38097975158126,
8.86059655985668));
#394487=CARTESIAN_POINT('Ctrl Pts',(-2.27850137682477,1.38119784597673,
8.86059725258816));
#394488=CARTESIAN_POINT('Ctrl Pts',(-2.27836738619122,1.38141644425738,
8.86059794692012));
#394489=CARTESIAN_POINT('Ctrl Pts',(-2.27824301215026,1.38164225602507,
8.86056369958366));
#394490=CARTESIAN_POINT('Ctrl Pts',(-2.27813174193071,1.38186114989894,
8.86048590497774));
#394491=CARTESIAN_POINT('Ctrl Pts',(-2.27810270371632,1.38191827468276,
8.86046560290182));
#394492=CARTESIAN_POINT('Ctrl Pts',(-2.27807426091854,1.3819757125264,8.86044257503091));
#394493=CARTESIAN_POINT('Ctrl Pts',(-2.27804726302641,1.38203167398586,
8.86041778462583));
#394494=CARTESIAN_POINT('Ctrl Pts',(-2.27786560071395,1.38240822516566,
8.86025097596201));
#394495=CARTESIAN_POINT('Ctrl Pts',(-2.27772528047931,1.38276860366663,
8.8599848982295));
#394496=CARTESIAN_POINT('Ctrl Pts',(-2.27762250278359,1.38309921687265,
8.85968173251462));
#394497=CARTESIAN_POINT('Ctrl Pts',(-2.27756813927101,1.38327409231675,
8.85952137522077));
#394498=CARTESIAN_POINT('Ctrl Pts',(-2.27752304917652,1.38344395417844,
8.85934740853961));
#394499=CARTESIAN_POINT('Ctrl Pts',(-2.27748636585381,1.38360600818471,
8.8591675900182));
#394500=CARTESIAN_POINT('Ctrl Pts',(-2.27733906324553,1.38425673925387,
8.85844552518694));
#394501=CARTESIAN_POINT('Ctrl Pts',(-2.27731603834265,1.38481768310818,
8.85759444184122));
#394502=CARTESIAN_POINT('Ctrl Pts',(-2.27733834581908,1.38527673281356,
8.85683498915136));
#394503=CARTESIAN_POINT('Ctrl Pts',(-2.27734068023707,1.38532477114268,
8.85675551444996));
#394504=CARTESIAN_POINT('Ctrl Pts',(-2.27734353046228,1.38537168876702,
8.85667699793651));
#394505=CARTESIAN_POINT('Ctrl Pts',(-2.27734681858157,1.38541746796544,
8.85659965593547));
#394506=CARTESIAN_POINT('Ctrl Pts',(-2.27739120178348,1.3860353979218,8.85555568965886));
#394507=CARTESIAN_POINT('Ctrl Pts',(-2.27752309810306,1.38662285708124,
8.85434650606346));
#394508=CARTESIAN_POINT('Ctrl Pts',(-2.2777370957799,1.38718411095034,8.85297329937117));
#394509=CARTESIAN_POINT('Ctrl Pts',(-2.27785745643406,1.38749978205401,
8.85220095427747));
#394510=CARTESIAN_POINT('Ctrl Pts',(-2.27800413243972,1.38780718014193,
8.85137579139183));
#394511=CARTESIAN_POINT('Ctrl Pts',(-2.27817859968918,1.38810672912945,
8.85049129520029));
#394512=CARTESIAN_POINT('Origin',(-2.28411940593292,1.38464660685209,7.59394543036555));
#394513=CARTESIAN_POINT('Ctrl Pts',(-2.28387764188341,1.37775289111108,
7.59443877723642));
#394514=CARTESIAN_POINT('Ctrl Pts',(-2.27809312860511,1.37748344764418,
7.58783886950016));
#394515=CARTESIAN_POINT('Ctrl Pts',(-2.27574649854821,1.38564264545479,
7.58559994247159));
#394516=CARTESIAN_POINT('Ctrl Pts',(-2.31545513015923,1.37922377509172,
7.56670252222134));
#394517=CARTESIAN_POINT('Ctrl Pts',(-2.30967897714489,1.37895472104714,
7.56004874999028));
#394518=CARTESIAN_POINT('Ctrl Pts',(-2.30729790926197,1.38715635948061,
7.55786368756704));
#394519=CARTESIAN_POINT('Ctrl Pts',(-2.34697365063074,1.3806919123435,7.5388891333356));
#394520=CARTESIAN_POINT('Ctrl Pts',(-2.34116316965618,1.38042125929756,
7.53222002137278));
#394521=CARTESIAN_POINT('Ctrl Pts',(-2.3387915746085,1.38866613538212,7.53005029815326));
#394522=CARTESIAN_POINT('Ctrl Pts',(-2.37843177706341,1.3821572364322,7.51101258149734));
#394523=CARTESIAN_POINT('Ctrl Pts',(-2.37255086250156,1.38188330257954,
7.5043616886572));
#394524=CARTESIAN_POINT('Ctrl Pts',(-2.37022593460537,1.39017198111247,
7.50217374673251));
#394525=CARTESIAN_POINT('',(-2.36854855682564,1.39009162622348,7.50366116523517));
#394526=CARTESIAN_POINT('Ctrl Pts',(-2.36986171072478,1.38175804150002,
7.51860402984325));
#394527=CARTESIAN_POINT('Ctrl Pts',(-2.37030284363451,1.38177858953489,
7.51734760759494));
#394528=CARTESIAN_POINT('Ctrl Pts',(-2.37069870192873,1.38185658998922,
7.51608817408573));
#394529=CARTESIAN_POINT('Ctrl Pts',(-2.37104579353598,1.38200496518604,
7.5148100591312));
#394530=CARTESIAN_POINT('Ctrl Pts',(-2.37136019740785,1.38213936698486,
7.51365231206384));
#394531=CARTESIAN_POINT('Ctrl Pts',(-2.37163512890018,1.38233147186997,
7.51247773061043));
#394532=CARTESIAN_POINT('Ctrl Pts',(-2.37184468125209,1.38260822385204,
7.51129758471022));
#394533=CARTESIAN_POINT('Ctrl Pts',(-2.37210513089373,1.38295219495949,
7.50983079813402));
#394534=CARTESIAN_POINT('Ctrl Pts',(-2.37224588918624,1.38342381066497,
7.50839324291155));
#394535=CARTESIAN_POINT('Ctrl Pts',(-2.37218898720972,1.38405009018387,
7.50715379678855));
#394536=CARTESIAN_POINT('Ctrl Pts',(-2.37216270013615,1.38433941327579,
7.50658120839351));
#394537=CARTESIAN_POINT('Ctrl Pts',(-2.3720810292347,1.38470201445234,7.50598221009429));
#394538=CARTESIAN_POINT('Ctrl Pts',(-2.37192372758135,1.38512426619738,
7.50545747549611));
#394539=CARTESIAN_POINT('Ctrl Pts',(-2.37183978655018,1.38534959279845,
7.50517746087247));
#394540=CARTESIAN_POINT('Ctrl Pts',(-2.3717335882949,1.3855944196509,7.50491486231392));
#394541=CARTESIAN_POINT('Ctrl Pts',(-2.37160641486975,1.38585159955045,
7.50468370960992));
#394542=CARTESIAN_POINT('Ctrl Pts',(-2.37141625048456,1.38623616462308,
7.50433806340446));
#394543=CARTESIAN_POINT('Ctrl Pts',(-2.37117298497437,1.38665963561176,
7.50405484070983));
#394544=CARTESIAN_POINT('Ctrl Pts',(-2.37089238062564,1.38709313568448,
7.5038576603613));
#394545=CARTESIAN_POINT('Ctrl Pts',(-2.37086237435212,1.38713949177914,
7.5038365749879));
#394546=CARTESIAN_POINT('Ctrl Pts',(-2.37083196648804,1.38718594989284,
7.50381643264937));
#394547=CARTESIAN_POINT('Ctrl Pts',(-2.37080119488786,1.38723246580278,
7.50379723213559));
#394548=CARTESIAN_POINT('Ctrl Pts',(-2.37059578439061,1.38754297471809,
7.50366906242519));
#394549=CARTESIAN_POINT('Ctrl Pts',(-2.37036909795697,1.38786241660097,
7.50358235568538));
#394550=CARTESIAN_POINT('Ctrl Pts',(-2.3701431987879,1.38816506702349,7.5035341175365));
#394551=CARTESIAN_POINT('Ctrl Pts',(-2.36980448855074,1.38861885707865,
7.50346178989176));
#394552=CARTESIAN_POINT('Ctrl Pts',(-2.36942081878387,1.38909263034581,
7.50346967198527));
#394553=CARTESIAN_POINT('Ctrl Pts',(-2.36902986284641,1.38954613953559,
7.50354272648692));
#394554=CARTESIAN_POINT('Ctrl Pts',(-2.36886905457702,1.38973267725243,
7.50357277531559));
#394555=CARTESIAN_POINT('Ctrl Pts',(-2.36870733465887,1.38991563133445,
7.50361331098761));
#394556=CARTESIAN_POINT('Ctrl Pts',(-2.36854855682687,1.39009162622419,
7.50366116523659));
#394557=CARTESIAN_POINT('',(-2.28662319996334,1.38616442150748,7.57603338622103));
#394558=CARTESIAN_POINT('Origin',(-2.29417856487493,1.39074786460783,7.58486873427627));
#394559=CARTESIAN_POINT('Ctrl Pts',(-2.36854855688293,1.39009162622086,
7.50366116529968));
#394560=CARTESIAN_POINT('Ctrl Pts',(-2.34128462633658,1.38878552899461,
7.52783573079709));
#394561=CARTESIAN_POINT('Ctrl Pts',(-2.31397746256357,1.38747654046441,
7.55196141284068));
#394562=CARTESIAN_POINT('Ctrl Pts',(-2.28662320117997,1.38616442121176,
7.57603338728831));
#394563=CARTESIAN_POINT('Ctrl Pts',(-2.2854584115801,1.37800253058068,7.59639677331372));
#394564=CARTESIAN_POINT('Ctrl Pts',(-2.26756460946867,1.37427643856106,
7.59959882295461));
#394565=CARTESIAN_POINT('Ctrl Pts',(-2.27873543150216,1.38876510819258,
7.59642833564546));
#394566=CARTESIAN_POINT('Ctrl Pts',(-2.2818171460615,1.37660385638462,7.58707626057424));
#394567=CARTESIAN_POINT('Ctrl Pts',(-2.27564276078402,1.37939478051135,
7.58809943920598));
#394568=CARTESIAN_POINT('Ctrl Pts',(-2.27591536114094,1.38615052546198,
7.58710240504252));
#394569=CARTESIAN_POINT('Ctrl Pts',(-2.2842159981254,1.3821869685129,7.5801537675693));
#394570=CARTESIAN_POINT('Ctrl Pts',(-2.28148722914889,1.3830134618696,7.5820588065976));
#394571=CARTESIAN_POINT('Ctrl Pts',(-2.28196843808644,1.38578754063495,
7.58020924244129));
#394572=CARTESIAN_POINT('Ctrl Pts',(-2.28662319925575,1.3861644210783,7.57603338509286));
#394573=CARTESIAN_POINT('Ctrl Pts',(-2.28662319925575,1.3861644210783,7.57603338509286));
#394574=CARTESIAN_POINT('Ctrl Pts',(-2.28662319925575,1.3861644210783,7.57603338509286));
#394575=CARTESIAN_POINT('Origin',(-2.29418152300553,1.39074298486212,7.58486873427623));
#394576=CARTESIAN_POINT('Ctrl Pts',(-2.32554906181097,1.46943874996094,
7.51098857897448));
#394577=CARTESIAN_POINT('Ctrl Pts',(-2.32258603056804,1.46435141688502,
7.50433767179956));
#394578=CARTESIAN_POINT('Ctrl Pts',(-2.32885943401302,1.4584562951476,7.50214974420965));
#394579=CARTESIAN_POINT('Ctrl Pts',(-2.30969475968219,1.44221793823038,
7.53887321589168));
#394580=CARTESIAN_POINT('Ctrl Pts',(-2.30676723081199,1.4371915604331,7.53220407452061));
#394581=CARTESIAN_POINT('Ctrl Pts',(-2.31298019139209,1.43127530817746,
7.53003438070911));
#394582=CARTESIAN_POINT('Ctrl Pts',(-2.29381001144491,1.41494485249997,
7.56669465659232));
#394583=CARTESIAN_POINT('Ctrl Pts',(-2.29089978372601,1.40994817966099,
7.56004085833298));
#394584=CARTESIAN_POINT('Ctrl Pts',(-2.29707001560499,1.40404352990962,
7.55785582193789));
#394585=CARTESIAN_POINT('Ctrl Pts',(-2.27789553550272,1.3876207262222,7.59443891967696));
#394586=CARTESIAN_POINT('Ctrl Pts',(-2.27498108831601,1.3826168088297,7.58783901202978));
#394587=CARTESIAN_POINT('Ctrl Pts',(-2.28112962096229,1.3767623469171,7.58560008491213));
#394588=CARTESIAN_POINT('',(-2.32799867143119,1.45698290352087,7.50366116523517));
#394589=CARTESIAN_POINT('Ctrl Pts',(-2.3279986714315,1.45698290352106,7.50366116523554));
#394590=CARTESIAN_POINT('Ctrl Pts',(-2.32773447744661,1.45769307184978,
7.50350835821027));
#394591=CARTESIAN_POINT('Ctrl Pts',(-2.32746851446684,1.45833729363188,
7.50345484956));
#394592=CARTESIAN_POINT('Ctrl Pts',(-2.32719343025616,1.45893495125746,
7.50349758195598));
#394593=CARTESIAN_POINT('Ctrl Pts',(-2.32705229165531,1.45924159394283,
7.50351950684424));
#394594=CARTESIAN_POINT('Ctrl Pts',(-2.32689495833406,1.45956625690094,
7.50357029184312));
#394595=CARTESIAN_POINT('Ctrl Pts',(-2.32673463798332,1.45987515532442,
7.50365515313923));
#394596=CARTESIAN_POINT('Ctrl Pts',(-2.32648800036376,1.46035036618505,
7.50378570417639));
#394597=CARTESIAN_POINT('Ctrl Pts',(-2.32622736167187,1.46080237652902,
7.50400001621911));
#394598=CARTESIAN_POINT('Ctrl Pts',(-2.32597059343915,1.46119564767338,
7.50428903009635));
#394599=CARTESIAN_POINT('Ctrl Pts',(-2.32594209414077,1.46123929774475,
7.50432110841318));
#394600=CARTESIAN_POINT('Ctrl Pts',(-2.3259136432884,1.46128225449648,7.50435406373354));
#394601=CARTESIAN_POINT('Ctrl Pts',(-2.32588526557894,1.46132449171132,
7.50438785222351));
#394602=CARTESIAN_POINT('Ctrl Pts',(-2.32571200602259,1.46158237020969,
7.50459414719561));
#394603=CARTESIAN_POINT('Ctrl Pts',(-2.3255382864381,1.46181724467064,7.50483629897752));
#394604=CARTESIAN_POINT('Ctrl Pts',(-2.3253718200413,1.46202089970008,7.5050991045531));
#394605=CARTESIAN_POINT('Ctrl Pts',(-2.32500457845001,1.46247018315024,
7.50567888004914));
#394606=CARTESIAN_POINT('Ctrl Pts',(-2.32465856865975,1.46278555900683,
7.50637912803144));
#394607=CARTESIAN_POINT('Ctrl Pts',(-2.32434792656117,1.46299451535731,
7.50710440483569));
#394608=CARTESIAN_POINT('Ctrl Pts',(-2.32427175095149,1.46304575560281,
7.50728225710685));
#394609=CARTESIAN_POINT('Ctrl Pts',(-2.32419626713429,1.46309173768623,
7.50746498566954));
#394610=CARTESIAN_POINT('Ctrl Pts',(-2.3241234538743,1.46313174401608,7.50764697238949));
#394611=CARTESIAN_POINT('Ctrl Pts',(-2.32373202982733,1.46334680703533,
7.50862528291182));
#394612=CARTESIAN_POINT('Ctrl Pts',(-2.32338424120943,1.46341233067584,
7.50965856837422));
#394613=CARTESIAN_POINT('Ctrl Pts',(-2.32307440409398,1.46339436861899,
7.51067959873203));
#394614=CARTESIAN_POINT('Ctrl Pts',(-2.32290390033854,1.46338448407646,
7.51124147302579));
#394615=CARTESIAN_POINT('Ctrl Pts',(-2.32274487302363,1.46334888134487,
7.51180065547253));
#394616=CARTESIAN_POINT('Ctrl Pts',(-2.32259663098811,1.46329586426744,
7.51235175716501));
#394617=CARTESIAN_POINT('Ctrl Pts',(-2.32208439570275,1.4631126691454,7.51425603304535));
#394618=CARTESIAN_POINT('Ctrl Pts',(-2.32164190203507,1.46269399769698,
7.51626900505179));
#394619=CARTESIAN_POINT('Ctrl Pts',(-2.32127620067168,1.46209979118688,
7.51827788969242));
#394620=CARTESIAN_POINT('Ctrl Pts',(-2.32125640822281,1.46206763160766,
7.51838661432544));
#394621=CARTESIAN_POINT('Ctrl Pts',(-2.32123684240496,1.46203494803777,
7.51849533314856));
#394622=CARTESIAN_POINT('Ctrl Pts',(-2.3212175049551,1.46200174688657,7.51860402984325));
#394623=CARTESIAN_POINT('Ctrl Pts',(-2.28662320026479,1.38616442272375,
7.57603338728984));
#394624=CARTESIAN_POINT('Ctrl Pts',(-2.30043891757839,1.40980978650237,
7.55196141284922));
#394625=CARTESIAN_POINT('Ctrl Pts',(-2.31423007475574,1.4334148416652,7.52783573083104));
#394626=CARTESIAN_POINT('Ctrl Pts',(-2.32799867145622,1.45698290357449,
7.50366116530176));
#394627=CARTESIAN_POINT('Origin',(-7.90134016134196E-16,4.7898388392343E-16,
7.49482233047033));
#394628=CARTESIAN_POINT('Origin',(-2.36092560474804,1.38561774629408,7.49482233047033));
#394629=CARTESIAN_POINT('Origin',(0.,0.,7.50366116523517));
#394630=CARTESIAN_POINT('Origin',(-2.32050622536843,1.45229374026964,7.49482233047033));
#394631=CARTESIAN_POINT('Ctrl Pts',(-2.36986065415221,1.38175799223992,
7.51860402984325));
#394632=CARTESIAN_POINT('Ctrl Pts',(-2.37746134385964,1.38211267801839,
7.51860402984325));
#394633=CARTESIAN_POINT('Ctrl Pts',(-2.38126727405859,1.37552396180423,
7.51860402984325));
#394634=CARTESIAN_POINT('Ctrl Pts',(-2.37268284216962,1.38188968822062,
7.51041458714365));
#394635=CARTESIAN_POINT('Ctrl Pts',(-2.37836300374412,1.38055173072964,
7.51004642900441));
#394636=CARTESIAN_POINT('Ctrl Pts',(-2.38126832368895,1.37552214471453,
7.50729136483009));
#394637=CARTESIAN_POINT('Ctrl Pts',(-2.37352967894752,1.38457420021926,
7.50215815450138));
#394638=CARTESIAN_POINT('Ctrl Pts',(-2.37652725582071,1.38373004539293,
7.49877163671531));
#394639=CARTESIAN_POINT('Ctrl Pts',(-2.37827363220951,1.38075446257557,
7.49481588533172));
#394640=CARTESIAN_POINT('Ctrl Pts',(-2.36854808203743,1.39009134757273,
7.50366171572174));
#394641=CARTESIAN_POINT('Ctrl Pts',(-2.37170608696131,1.39194476796699,
7.50000045605858));
#394642=CARTESIAN_POINT('Ctrl Pts',(-2.37170608696137,1.39194476796689,
7.49482233047317));
#394643=CARTESIAN_POINT('Origin',(-2.37044333190377,1.36927158015967,7.51860402984325));
#394644=CARTESIAN_POINT('Origin',(-2.37044333190377,1.36927158015967,9.));
#394645=CARTESIAN_POINT('Origin',(-2.37044333190377,1.36927158015967,8.75721825406948));
#394646=CARTESIAN_POINT('Ctrl Pts',(-2.35317963884603,1.38098095793092,
8.78942910404913));
#394647=CARTESIAN_POINT('Ctrl Pts',(-2.35874509705392,1.38126042821203,
8.7967269950169));
#394648=CARTESIAN_POINT('Ctrl Pts',(-2.36082223585053,1.37257947317229,
8.79893251111267));
#394649=CARTESIAN_POINT('Ctrl Pts',(-2.36416206650684,1.3814925255372,8.78111911759576));
#394650=CARTESIAN_POINT('Ctrl Pts',(-2.37076035502444,1.38181640632387,
8.78644465894814));
#394651=CARTESIAN_POINT('Ctrl Pts',(-2.37429374527117,1.37452047148728,
8.78817647674131));
#394652=CARTESIAN_POINT('Ctrl Pts',(-2.37100657738213,1.38181134663968,
8.76780923932034));
#394653=CARTESIAN_POINT('Ctrl Pts',(-2.37879582820066,1.38218858457062,
8.76988516158373));
#394654=CARTESIAN_POINT('Ctrl Pts',(-2.38270941194407,1.37572172732156,
8.77093053738834));
#394655=CARTESIAN_POINT('Ctrl Pts',(-2.36967199143526,1.38174918088633,
8.75371302330491));
#394656=CARTESIAN_POINT('Ctrl Pts',(-2.37727003273756,1.38211792163049,
8.75300828287559));
#394657=CARTESIAN_POINT('Ctrl Pts',(-2.38106807980286,1.37548698068488,
8.75267964240737));
#394658=CARTESIAN_POINT('Origin',(-2.35643593852862,1.36861911374606,8.78727029226991));
#394659=CARTESIAN_POINT('Ctrl Pts',(-2.28443929758136,1.37777905311489,
8.85049129520029));
#394660=CARTESIAN_POINT('Ctrl Pts',(-2.29027258849563,1.37805076865114,
8.85711686593484));
#394661=CARTESIAN_POINT('Ctrl Pts',(-2.29260852370878,1.36982616113504,
8.85933012996512));
#394662=CARTESIAN_POINT('Ctrl Pts',(-2.3082789390469,1.37888950706961,8.82945683644723));
#394663=CARTESIAN_POINT('Ctrl Pts',(-2.31416064980263,1.37916347800909,
8.83607469902389));
#394664=CARTESIAN_POINT('Ctrl Pts',(-2.31646736766073,1.37090447714819,
8.8382956714852));
#394665=CARTESIAN_POINT('Ctrl Pts',(-2.3320830456044,1.37999830580317,8.80838214965002));
#394666=CARTESIAN_POINT('Ctrl Pts',(-2.33798796833688,1.3802733579599,8.8150136446199));
#394667=CARTESIAN_POINT('Ctrl Pts',(-2.34028998879803,1.37198182526734,
8.81722098428721));
#394668=CARTESIAN_POINT('Ctrl Pts',(-2.35585431734964,1.38110557508641,
8.78727029226991));
#394669=CARTESIAN_POINT('Ctrl Pts',(-2.36176022090919,1.3813806729302,8.79393457792714));
#394670=CARTESIAN_POINT('Ctrl Pts',(-2.36407914959491,1.37305829436823,
8.79610912703474));
#394671=CARTESIAN_POINT('Origin',(-2.28502091876035,1.36529259177454,8.85049129520029));
#394672=CARTESIAN_POINT('Ctrl Pts',(-2.27817859968918,1.38810672912945,
8.85049129520029));
#394673=CARTESIAN_POINT('Ctrl Pts',(-2.28111762290111,1.39315284196834,
8.85711686593484));
#394674=CARTESIAN_POINT('Ctrl Pts',(-2.27490615106175,1.39902807640646,
8.85933012996512));
#394675=CARTESIAN_POINT('Ctrl Pts',(-2.27557848827882,1.38364250594229,
8.86332496987234));
#394676=CARTESIAN_POINT('Ctrl Pts',(-2.27342895555081,1.38773290976439,
8.86648636486737));
#394677=CARTESIAN_POINT('Ctrl Pts',(-2.26764703798749,1.38653060731341,
8.87206031107457));
#394678=CARTESIAN_POINT('Ctrl Pts',(-2.27924360121796,1.37753703682523,
8.86341338519875));
#394679=CARTESIAN_POINT('Ctrl Pts',(-2.28185900586174,1.37371170949497,
8.86654584966057));
#394680=CARTESIAN_POINT('Ctrl Pts',(-2.27805961224584,1.3691632195325,8.87215952290714));
#394681=CARTESIAN_POINT('Ctrl Pts',(-2.28443929758136,1.37777905311489,
8.85049129520029));
#394682=CARTESIAN_POINT('Ctrl Pts',(-2.29027258849563,1.37805076865114,
8.85711686593484));
#394683=CARTESIAN_POINT('Ctrl Pts',(-2.29260852370878,1.36982616113504,
8.85933012996512));
#394684=CARTESIAN_POINT('Origin',(-2.26737713379146,1.39439786054284,8.85049129520029));
#394685=CARTESIAN_POINT('Ctrl Pts',(-2.31416007290289,1.44988459233546,
8.78727029226991));
#394686=CARTESIAN_POINT('Ctrl Pts',(-2.31713568099515,1.45499351904855,
8.79393457792714));
#394687=CARTESIAN_POINT('Ctrl Pts',(-2.31082965924421,1.46089889836363,
8.79610912703474));
#394688=CARTESIAN_POINT('Ctrl Pts',(-2.30218324533451,1.42932115373564,
8.80838214965002));
#394689=CARTESIAN_POINT('Ctrl Pts',(-2.30515835925056,1.43442923198015,
8.81501364461988));
#394690=CARTESIAN_POINT('Ctrl Pts',(-2.29887186472477,1.44030535307934,
8.81722098428722));
#394691=CARTESIAN_POINT('Ctrl Pts',(-2.29018987439861,1.40872931124336,
8.82945683644723));
#394692=CARTESIAN_POINT('Ctrl Pts',(-2.29315329328018,1.41381730986974,
8.83607469902389));
#394693=CARTESIAN_POINT('Ctrl Pts',(-2.2868978141797,1.41968254846007,8.8382956714852));
#394694=CARTESIAN_POINT('Ctrl Pts',(-2.27817859968918,1.38810672912945,
8.85049129520029));
#394695=CARTESIAN_POINT('Ctrl Pts',(-2.28111762290111,1.39315284196834,
8.85711686593484));
#394696=CARTESIAN_POINT('Ctrl Pts',(-2.27490615106175,1.39902807640646,
8.85933012996512));
#394697=CARTESIAN_POINT('Origin',(-2.30335860700518,1.45617572374885,8.78727029226991));
#394698=CARTESIAN_POINT('Ctrl Pts',(-2.3211242991746,1.46184175524038,8.75374538247848));
#394699=CARTESIAN_POINT('Ctrl Pts',(-2.32496012354653,1.4684015440918,8.75304829418601));
#394700=CARTESIAN_POINT('Ctrl Pts',(-2.32084701402088,1.47483217184025,
8.75272238421917));
#394701=CARTESIAN_POINT('Ctrl Pts',(-2.32178863480649,1.46298237572165,
8.7676940844502));
#394702=CARTESIAN_POINT('Ctrl Pts',(-2.32572038980645,1.46970758632004,
8.76974318093969));
#394703=CARTESIAN_POINT('Ctrl Pts',(-2.32180392561551,1.47616356537214,
8.7707786988043));
#394704=CARTESIAN_POINT('Ctrl Pts',(-2.31838362881722,1.45713620489586,
8.78108014887988));
#394705=CARTESIAN_POINT('Ctrl Pts',(-2.32171892952989,1.4628336610349,8.78639403366325));
#394706=CARTESIAN_POINT('Ctrl Pts',(-2.31690771126942,1.46934321206235,
8.78812224174741));
#394707=CARTESIAN_POINT('Ctrl Pts',(-2.31280357563321,1.44755562148552,
8.78944554828685));
#394708=CARTESIAN_POINT('Ctrl Pts',(-2.31561927425866,1.45235439829505,
8.79673892988686));
#394709=CARTESIAN_POINT('Ctrl Pts',(-2.30889239325609,1.45820697262554,
8.79894799272499));
#394710=CARTESIAN_POINT('Origin',(-2.31041603905739,1.46829287829996,8.75721825406948));
#394711=CARTESIAN_POINT('Origin',(-2.31041603905739,1.46829287829996,9.));
#394712=CARTESIAN_POINT('Origin',(-2.31041603905739,1.46829287829996,7.51860402984325));
#394713=CARTESIAN_POINT('Ctrl Pts',(-2.32799800459713,1.45698248618143,
7.50366195182966));
#394714=CARTESIAN_POINT('Ctrl Pts',(-2.33110214420566,1.45892521853583,
7.50000065167735));
#394715=CARTESIAN_POINT('Ctrl Pts',(-2.33110214420559,1.45892521853592,
7.49482233047108));
#394716=CARTESIAN_POINT('Ctrl Pts',(-2.32540754212619,1.46395696134399,
7.50215800491338));
#394717=CARTESIAN_POINT('Ctrl Pts',(-2.32604450161754,1.46700638420426,
7.49877273257267));
#394718=CARTESIAN_POINT('Ctrl Pts',(-2.32421310714895,1.46993267035745,
7.49481816995647));
#394719=CARTESIAN_POINT('Ctrl Pts',(-2.32263636524651,1.46443716447144,
7.5104302581404));
#394720=CARTESIAN_POINT('Ctrl Pts',(-2.32408184125221,1.47009431535362,
7.51006209594513));
#394721=CARTESIAN_POINT('Ctrl Pts',(-2.32096452598623,1.47499954885415,
7.50731281821699));
#394722=CARTESIAN_POINT('Ctrl Pts',(-2.32121674419912,1.46200044089929,
7.51860402984325));
#394723=CARTESIAN_POINT('Ctrl Pts',(-2.32504721351854,1.46857528098735,
7.51860402984324));
#394724=CARTESIAN_POINT('Ctrl Pts',(-2.32096588398459,1.47499741199083,
7.51860402984325));
#394725=CARTESIAN_POINT('Origin',(0.,0.,7.5));
#394726=CARTESIAN_POINT('Origin',(-2.36243414091426,1.23929131094303,7.5));
#394727=CARTESIAN_POINT('',(-2.36243414091426,1.23929131094303,7.59394543036555));
#394728=CARTESIAN_POINT('',(-2.36243414091426,1.23929131094303,8.85049129520029));
#394729=CARTESIAN_POINT('',(-2.36243414091426,1.23929131094303,7.5));
#394730=CARTESIAN_POINT('',(-2.4022998076178,1.2986369039994,8.78727029226991));
#394731=CARTESIAN_POINT('Ctrl Pts',(-2.36243414091426,1.23929131094303,
8.85049129520029));
#394732=CARTESIAN_POINT('Ctrl Pts',(-2.37574201268455,1.25910193015076,
8.82945686509571));
#394733=CARTESIAN_POINT('Ctrl Pts',(-2.38903010069429,1.27888309847756,
8.80838212259894));
#394734=CARTESIAN_POINT('Ctrl Pts',(-2.4022998076178,1.2986369039994,8.78727029226991));
#394735=CARTESIAN_POINT('',(-2.41011908817658,1.31027699133284,8.75721825406948));
#394736=CARTESIAN_POINT('Origin',(-2.38658832796283,1.27524781804229,8.75937679713088));
#394737=CARTESIAN_POINT('',(-2.41011908817658,1.31027699133284,7.51860402984325));
#394738=CARTESIAN_POINT('',(-2.41011908817658,1.31027699133284,7.5));
#394739=CARTESIAN_POINT('Ctrl Pts',(-2.41011908817658,1.31027699133284,
7.51860402984325));
#394740=CARTESIAN_POINT('Ctrl Pts',(-2.40397825942582,1.30113551310844,
7.52834476460825));
#394741=CARTESIAN_POINT('Ctrl Pts',(-2.39783344413765,1.29198810036828,
7.53807742314407));
#394742=CARTESIAN_POINT('Ctrl Pts',(-2.39168450845876,1.28283455385311,
7.54780169004674));
#394743=CARTESIAN_POINT('Ctrl Pts',(-2.38194492666502,1.26833583088006,
7.5632044032688));
#394744=CARTESIAN_POINT('Ctrl Pts',(-2.37219499495818,1.25382170062098,
7.57858609112103));
#394745=CARTESIAN_POINT('Ctrl Pts',(-2.36243414091426,1.23929131094303,
7.59394543036555));
#394746=CARTESIAN_POINT('Origin',(-2.64297784464841,1.22375287867822,7.5));
#394747=CARTESIAN_POINT('',(-2.45352211735225,1.22708151028067,8.75721825406948));
#394748=CARTESIAN_POINT('',(-2.43950170000243,1.22732784120418,8.78727029226991));
#394749=CARTESIAN_POINT('Origin',(-2.4039126514152,1.22795312096489,8.75658640621105));
#394750=CARTESIAN_POINT('',(-2.36802027905702,1.2285837299553,8.85049129520029));
#394751=CARTESIAN_POINT('Ctrl Pts',(-2.43950170000243,1.22732784120418,
8.78727029226991));
#394752=CARTESIAN_POINT('Ctrl Pts',(-2.41570835638484,1.22774587699874,
8.80838212259895));
#394753=CARTESIAN_POINT('Ctrl Pts',(-2.39188205442814,1.22816449185295,
8.82945686509571));
#394754=CARTESIAN_POINT('Ctrl Pts',(-2.36802027905702,1.2285837299553,8.85049129520029));
#394755=CARTESIAN_POINT('',(-2.36802027905702,1.2285837299553,7.59394543036555));
#394756=CARTESIAN_POINT('',(-2.36802027905702,1.2285837299553,7.5));
#394757=CARTESIAN_POINT('',(-2.45352211735225,1.22708151028067,7.51860402984325));
#394758=CARTESIAN_POINT('Ctrl Pts',(-2.36802027905702,1.2285837299553,7.59394543036555));
#394759=CARTESIAN_POINT('Ctrl Pts',(-2.3855220487349,1.22827623361048,7.57858609112103));
#394760=CARTESIAN_POINT('Ctrl Pts',(-2.40300423403733,1.22796908135225,
7.56320440326857));
#394761=CARTESIAN_POINT('Ctrl Pts',(-2.42046786135374,1.22766225514747,
7.54780169004651));
#394762=CARTESIAN_POINT('Ctrl Pts',(-2.43149325478056,1.22746854512606,
7.53807742314383));
#394763=CARTESIAN_POINT('Ctrl Pts',(-2.44251126011132,1.22727496490938,
7.52834476460825));
#394764=CARTESIAN_POINT('Ctrl Pts',(-2.45352211735225,1.22708151028067,
7.51860402984325));
#394765=CARTESIAN_POINT('',(-2.45352211735225,1.22708151028067,7.5));
#394766=CARTESIAN_POINT('Origin',(-2.36814105033895,1.23545766909509,7.5));
#394767=CARTESIAN_POINT('Ctrl Pts',(-2.36802027905702,1.2285837299553,8.85049129520029));
#394768=CARTESIAN_POINT('Ctrl Pts',(-2.36782664743442,1.22858713195506,
8.85097269580138));
#394769=CARTESIAN_POINT('Ctrl Pts',(-2.36763560659412,1.22859890114683,
8.85143669361005));
#394770=CARTESIAN_POINT('Ctrl Pts',(-2.36743841348187,1.22862045209507,
8.8519052845931));
#394771=CARTESIAN_POINT('Ctrl Pts',(-2.36705271625983,1.22866260438312,
8.85282181883899));
#394772=CARTESIAN_POINT('Ctrl Pts',(-2.36665342562341,1.22874128994969,
8.85372622499635));
#394773=CARTESIAN_POINT('Ctrl Pts',(-2.36623725715283,1.22887287130628,
8.85462257735071));
#394774=CARTESIAN_POINT('Ctrl Pts',(-2.36589176886946,1.22898210547519,
8.85536669723986));
#394775=CARTESIAN_POINT('Ctrl Pts',(-2.36553456053144,1.22912778877101,
8.85610498449051));
#394776=CARTESIAN_POINT('Ctrl Pts',(-2.36516674476246,1.22932670510121,
8.85681338218371));
#394777=CARTESIAN_POINT('Ctrl Pts',(-2.36483295137444,1.22950722198327,
8.85745625420284));
#394778=CARTESIAN_POINT('Ctrl Pts',(-2.36448595034557,1.22973331737554,
8.85808743050666));
#394779=CARTESIAN_POINT('Ctrl Pts',(-2.36412948034973,1.23003334385226,
8.8586680450841));
#394780=CARTESIAN_POINT('Ctrl Pts',(-2.36396501282097,1.23017176956484,
8.85893592806395));
#394781=CARTESIAN_POINT('Ctrl Pts',(-2.36379858976411,1.23032616777319,
8.85919241173848));
#394782=CARTESIAN_POINT('Ctrl Pts',(-2.36363118640837,1.23050079886515,
8.85943017985534));
#394783=CARTESIAN_POINT('Ctrl Pts',(-2.36340514232143,1.23073660253563,
8.8597512372));
#394784=CARTESIAN_POINT('Ctrl Pts',(-2.36317201985186,1.23101574189602,
8.86004599534706));
#394785=CARTESIAN_POINT('Ctrl Pts',(-2.36294261383862,1.23134153932572,
8.86026130871721));
#394786=CARTESIAN_POINT('Ctrl Pts',(-2.36285862182953,1.23146082294993,
8.86034014101235));
#394787=CARTESIAN_POINT('Ctrl Pts',(-2.36277385628191,1.23158814575577,
8.86040910639693));
#394788=CARTESIAN_POINT('Ctrl Pts',(-2.36269090658753,1.23172022531705,
8.86046313645507));
#394789=CARTESIAN_POINT('Ctrl Pts',(-2.36256146428415,1.23192633436627,
8.8605474499083));
#394790=CARTESIAN_POINT('Ctrl Pts',(-2.36243303496201,1.23214973111175,
8.86059655985669));
#394791=CARTESIAN_POINT('Ctrl Pts',(-2.3623136012062,1.23237594242964,8.86059725258816));
#394792=CARTESIAN_POINT('Ctrl Pts',(-2.3621938915107,1.23260267638605,8.86059794692012));
#394793=CARTESIAN_POINT('Ctrl Pts',(-2.36208424081917,1.23283599287141,
8.86056369958366));
#394794=CARTESIAN_POINT('Ctrl Pts',(-2.36198722379487,1.23306156611178,
8.86048590497774));
#394795=CARTESIAN_POINT('Ctrl Pts',(-2.36196190524008,1.23312043401139,
8.86046560290182));
#394796=CARTESIAN_POINT('Ctrl Pts',(-2.36193720093636,1.23317957617913,
8.8604425750309));
#394797=CARTESIAN_POINT('Ctrl Pts',(-2.36191384397731,1.23323715242066,
8.86041778462583));
#394798=CARTESIAN_POINT('Ctrl Pts',(-2.36175668062648,1.23362456908,8.860250975962));
#394799=CARTESIAN_POINT('Ctrl Pts',(-2.36163973822464,1.23399319749299,
8.8599848982295));
#394800=CARTESIAN_POINT('Ctrl Pts',(-2.36155835415756,1.23432971640829,
8.85968173251461));
#394801=CARTESIAN_POINT('Ctrl Pts',(-2.36151530664882,1.23450771563425,
8.85952137522076));
#394802=CARTESIAN_POINT('Ctrl Pts',(-2.36148119228361,1.2346801174288,8.85934740853961));
#394803=CARTESIAN_POINT('Ctrl Pts',(-2.36145496716655,1.23484418878629,
8.8591675900182));
#394804=CARTESIAN_POINT('Ctrl Pts',(-2.36134965969002,1.23550302056918,
8.85844552518695));
#394805=CARTESIAN_POINT('Ctrl Pts',(-2.36136262189042,1.23606428711478,
8.85759444184123));
#394806=CARTESIAN_POINT('Ctrl Pts',(-2.36141429494935,1.23652096440839,
8.85683498915137));
#394807=CARTESIAN_POINT('Ctrl Pts',(-2.36141970239735,1.23656875447093,
8.85675551444997));
#394808=CARTESIAN_POINT('Ctrl Pts',(-2.36142555278897,1.23661539308343,
8.85667699793651));
#394809=CARTESIAN_POINT('Ctrl Pts',(-2.36143176723578,1.23666086755305,
8.85659965593547));
#394810=CARTESIAN_POINT('Ctrl Pts',(-2.36151565015588,1.23727468426453,
8.85555568965886));
#394811=CARTESIAN_POINT('Ctrl Pts',(-2.3616849141179,1.23785248579991,8.85434650606346));
#394812=CARTESIAN_POINT('Ctrl Pts',(-2.36193443177242,1.23839887563451,
8.85297329937117));
#394813=CARTESIAN_POINT('Ctrl Pts',(-2.36207477024976,1.23870618662446,
8.85220095427747));
#394814=CARTESIAN_POINT('Ctrl Pts',(-2.36224083995695,1.23900355556609,
8.85137579139183));
#394815=CARTESIAN_POINT('Ctrl Pts',(-2.36243414091426,1.23929131094303,
8.85049129520029));
#394816=CARTESIAN_POINT('Origin',(-2.36814105033895,1.23545766909509,7.59394543036555));
#394817=CARTESIAN_POINT('Ctrl Pts',(-2.3674581011356,1.22859360710825,7.59443877723642));
#394818=CARTESIAN_POINT('Ctrl Pts',(-2.36166820945802,1.22869533228008,
7.58783886950016));
#394819=CARTESIAN_POINT('Ctrl Pts',(-2.35984916240284,1.23698811524768,
7.58559994247159));
#394820=CARTESIAN_POINT('Ctrl Pts',(-2.39906494993531,1.22803829237974,
7.56670252222137));
#394821=CARTESIAN_POINT('Ctrl Pts',(-2.39328342629498,1.22813987052983,
7.56004874999026));
#394822=CARTESIAN_POINT('Ctrl Pts',(-2.39143273135004,1.23647721336054,
7.55786368756704));
#394823=CARTESIAN_POINT('Ctrl Pts',(-2.43061277610281,1.227484014646,7.5388891333356));
#394824=CARTESIAN_POINT('Ctrl Pts',(-2.4247968925844,1.22758619647999,7.53222002137278));
#394825=CARTESIAN_POINT('Ctrl Pts',(-2.42295842125755,1.23596608119879,
7.53005029815327));
#394826=CARTESIAN_POINT('Ctrl Pts',(-2.46210015207757,1.22693079898848,
7.51101258149734));
#394827=CARTESIAN_POINT('Ctrl Pts',(-2.45621376948321,1.22703421945197,
7.5043616886572));
#394828=CARTESIAN_POINT('Ctrl Pts',(-2.45442467585769,1.23545482664764,
7.50217374673251));
#394829=CARTESIAN_POINT('',(-2.45274559607509,1.23548210681972,7.50366116523517));
#394830=CARTESIAN_POINT('Ctrl Pts',(-2.45352211735225,1.22708151028067,
7.51860402984325));
#394831=CARTESIAN_POINT('Ctrl Pts',(-2.45396366042422,1.22707375261483,
7.51734760759494));
#394832=CARTESIAN_POINT('Ctrl Pts',(-2.45436370289138,1.22712623008087,
7.51608817408573));
#394833=CARTESIAN_POINT('Ctrl Pts',(-2.4547195877932,1.22725206218931,7.5148100591312));
#394834=CARTESIAN_POINT('Ctrl Pts',(-2.45504195684141,1.22736604391998,
7.51365231206384));
#394835=CARTESIAN_POINT('Ctrl Pts',(-2.45532863165975,1.2275401391838,7.51247773061043));
#394836=CARTESIAN_POINT('Ctrl Pts',(-2.45555548502425,1.22780289648397,
7.51129758471022));
#394837=CARTESIAN_POINT('Ctrl Pts',(-2.45583743784869,1.22812947380005,
7.50983079813402));
#394838=CARTESIAN_POINT('Ctrl Pts',(-2.45600812346019,1.22859110210571,
7.50839324291155));
#394839=CARTESIAN_POINT('Ctrl Pts',(-2.45599146426143,1.22921974058833,
7.50715379678855));
#394840=CARTESIAN_POINT('Ctrl Pts',(-2.45598376819163,1.22951015345352,
7.50658120839351));
#394841=CARTESIAN_POINT('Ctrl Pts',(-2.45592549702894,1.22987724229968,
7.50598221009429));
#394842=CARTESIAN_POINT('Ctrl Pts',(-2.45579557233091,1.23030870483476,
7.50545747549611));
#394843=CARTESIAN_POINT('Ctrl Pts',(-2.45572624049049,1.2305389465985,7.50517746087247));
#394844=CARTESIAN_POINT('Ctrl Pts',(-2.4556359465412,1.23079007457349,7.50491486231392));
#394845=CARTESIAN_POINT('Ctrl Pts',(-2.45552551198023,1.23105487409868,
7.50468370960993));
#394846=CARTESIAN_POINT('Ctrl Pts',(-2.45536037747697,1.23145083291511,
7.50433806340447));
#394847=CARTESIAN_POINT('Ctrl Pts',(-2.45514474366126,1.23188901991197,
7.50405484070984));
#394848=CARTESIAN_POINT('Ctrl Pts',(-2.45489249028929,1.23233960769464,
7.50385766036131));
#394849=CARTESIAN_POINT('Ctrl Pts',(-2.45486551571206,1.23238779105428,
7.50383657498791));
#394850=CARTESIAN_POINT('Ctrl Pts',(-2.45483814690575,1.23243610195336,
7.50381643264937));
#394851=CARTESIAN_POINT('Ctrl Pts',(-2.45481041881371,1.23248449383457,
7.50379723213559));
#394852=CARTESIAN_POINT('Ctrl Pts',(-2.45462532472886,1.23280752547176,
7.50366906242519));
#394853=CARTESIAN_POINT('Ctrl Pts',(-2.45441957075851,1.2331408348767,7.50358235568538));
#394854=CARTESIAN_POINT('Ctrl Pts',(-2.45421352660267,1.23345733688093,
7.5035341175365));
#394855=CARTESIAN_POINT('Ctrl Pts',(-2.45390458671067,1.23393189581515,
7.50346178989176));
#394856=CARTESIAN_POINT('Ctrl Pts',(-2.45355205999194,1.23442927747068,
7.50346967198527));
#394857=CARTESIAN_POINT('Ctrl Pts',(-2.45319096374893,1.23490690351011,
7.50354272648692));
#394858=CARTESIAN_POINT('Ctrl Pts',(-2.45304243738993,1.2351033609864,7.50357277531559));
#394859=CARTESIAN_POINT('Ctrl Pts',(-2.45289277165098,1.23529630060036,
7.50361331098761));
#394860=CARTESIAN_POINT('Ctrl Pts',(-2.45274559607636,1.23548210682036,
7.50366116523658));
#394861=CARTESIAN_POINT('',(-2.37073694677487,1.23681194660317,7.57603338622103));
#394862=CARTESIAN_POINT('Origin',(-2.37857045058673,1.24090189863625,7.58486873427629));
#394863=CARTESIAN_POINT('Ctrl Pts',(-2.45274559613209,1.23548210681344,
7.50366116529969));
#394864=CARTESIAN_POINT('Ctrl Pts',(-2.4254540003185,1.23592549913166,7.52783573079709));
#394865=CARTESIAN_POINT('Ctrl Pts',(-2.39811907485907,1.23636877604877,
7.55196141284068));
#394866=CARTESIAN_POINT('Ctrl Pts',(-2.37073694797006,1.23681194623011,
7.57603338728831));
#394867=CARTESIAN_POINT('Ctrl Pts',(-2.36887194462182,1.22871860183693,
7.59642833564546));
#394868=CARTESIAN_POINT('Ctrl Pts',(-2.35069119251645,1.22667677287982,
7.59959882295468));
#394869=CARTESIAN_POINT('Ctrl Pts',(-2.36315354717508,1.24004694984633,
7.59639677331371));
#394870=CARTESIAN_POINT('Ctrl Pts',(-2.3651741996041,1.22766241933315,7.58710240504253));
#394871=CARTESIAN_POINT('Ctrl Pts',(-2.35925575920166,1.23093143508659,
7.58809943920599));
#394872=CARTESIAN_POINT('Ctrl Pts',(-2.36006987607439,1.23765821029868,
7.58707626057422));
#394873=CARTESIAN_POINT('Ctrl Pts',(-2.3680016658602,1.2330268329137,7.58020924244127));
#394874=CARTESIAN_POINT('Ctrl Pts',(-2.36537997734295,1.23405339238908,
7.58205880659761));
#394875=CARTESIAN_POINT('Ctrl Pts',(-2.36608778108834,1.23681532744518,
7.58015376756929));
#394876=CARTESIAN_POINT('Ctrl Pts',(-2.37073694604124,1.23681194622021,
7.57603338509286));
#394877=CARTESIAN_POINT('Ctrl Pts',(-2.37073694604124,1.23681194622021,
7.57603338509286));
#394878=CARTESIAN_POINT('Ctrl Pts',(-2.37073694604124,1.23681194622021,
7.57603338509286));
#394879=CARTESIAN_POINT('Origin',(-2.37857308999325,1.24089683938839,7.58486873427622));
#394880=CARTESIAN_POINT('Ctrl Pts',(-2.4149182358073,1.31742119048616,7.51098857897448));
#394881=CARTESIAN_POINT('Ctrl Pts',(-2.41163534588056,1.31253415194521,
7.50433767179957));
#394882=CARTESIAN_POINT('Ctrl Pts',(-2.41751815819881,1.3062492040289,7.50214974420965));
#394883=CARTESIAN_POINT('Ctrl Pts',(-2.39735246464699,1.29127209545777,
7.53887321589167));
#394884=CARTESIAN_POINT('Ctrl Pts',(-2.39410890956764,1.28644361231146,
7.53220407452061));
#394885=CARTESIAN_POINT('Ctrl Pts',(-2.39993004937042,1.2801414498795,7.53003438070911));
#394886=CARTESIAN_POINT('Ctrl Pts',(-2.3797529607263,1.26507278452091,7.56669465659233));
#394887=CARTESIAN_POINT('Ctrl Pts',(-2.37652857445444,1.26027283681232,
7.56004085833301));
#394888=CARTESIAN_POINT('Ctrl Pts',(-2.38230781672175,1.25398499068331,
7.55785582193789));
#394889=CARTESIAN_POINT('Ctrl Pts',(-2.36212052000036,1.23882444256557,
7.59443891967696));
#394890=CARTESIAN_POINT('Ctrl Pts',(-2.35889145876986,1.2340175355304,7.58783901202978));
#394891=CARTESIAN_POINT('Ctrl Pts',(-2.36465226193378,1.22778116439849,
7.58560008491213));
#394892=CARTESIAN_POINT('',(-2.41656476362038,1.30483398889125,7.50366116523517));
#394893=CARTESIAN_POINT('Ctrl Pts',(-2.41656476362071,1.30483398889143,
7.50366116523554));
#394894=CARTESIAN_POINT('Ctrl Pts',(-2.41634661309173,1.30555962506988,
7.50350835821027));
#394895=CARTESIAN_POINT('Ctrl Pts',(-2.41612247199273,1.30621956353586,
7.50345484956));
#394896=CARTESIAN_POINT('Ctrl Pts',(-2.41588624502761,1.30683361791564,
7.50349758195598));
#394897=CARTESIAN_POINT('Ctrl Pts',(-2.41576504307545,1.30714867335193,
7.50351950684424));
#394898=CARTESIAN_POINT('Ctrl Pts',(-2.41562883423953,1.30748274963568,
7.50357029184312));
#394899=CARTESIAN_POINT('Ctrl Pts',(-2.41548863447409,1.30780128515435,
7.50365515313924));
#394900=CARTESIAN_POINT('Ctrl Pts',(-2.41527295046235,1.30829132176983,
7.50378570417639));
#394901=CARTESIAN_POINT('Ctrl Pts',(-2.41504180768278,1.30875910258839,
7.5040000162191));
#394902=CARTESIAN_POINT('Ctrl Pts',(-2.41481076397667,1.30916801691215,
7.50428903009634));
#394903=CARTESIAN_POINT('Ctrl Pts',(-2.41478511990283,1.3092134032561,7.50432110841317));
#394904=CARTESIAN_POINT('Ctrl Pts',(-2.41475947975432,1.30925809460095,
7.50435406373354));
#394905=CARTESIAN_POINT('Ctrl Pts',(-2.41473386649755,1.30930206320099,
7.50438785222352));
#394906=CARTESIAN_POINT('Ctrl Pts',(-2.41457748525366,1.30957051263823,
7.50459414719561));
#394907=CARTESIAN_POINT('Ctrl Pts',(-2.41441917105306,1.30981603477639,
7.50483629897752));
#394908=CARTESIAN_POINT('Ctrl Pts',(-2.41426609490187,1.3100299369134,7.5050991045531));
#394909=CARTESIAN_POINT('Ctrl Pts',(-2.4139283935373,1.31050182651207,7.50567888004914));
#394910=CARTESIAN_POINT('Ctrl Pts',(-2.41360330086178,1.31083872331851,
7.50637912803144));
#394911=CARTESIAN_POINT('Ctrl Pts',(-2.41330668489004,1.31106715325335,
7.50710440483569));
#394912=CARTESIAN_POINT('Ctrl Pts',(-2.41323394876512,1.31112316880834,
7.50728225710685));
#394913=CARTESIAN_POINT('Ctrl Pts',(-2.41316156611972,1.31117389268141,
7.50746498566954));
#394914=CARTESIAN_POINT('Ctrl Pts',(-2.41309146567674,1.31121848197555,
7.50764697238949));
#394915=CARTESIAN_POINT('Ctrl Pts',(-2.41271462498741,1.31145818174955,
7.50862528291181));
#394916=CARTESIAN_POINT('Ctrl Pts',(-2.41237174905258,1.31154585365798,
7.50965856837421));
#394917=CARTESIAN_POINT('Ctrl Pts',(-2.41206139769779,1.31154777983825,
7.51067959873202));
#394918=CARTESIAN_POINT('Ctrl Pts',(-2.41189061095578,1.31154883981768,
7.51124147302578));
#394919=CARTESIAN_POINT('Ctrl Pts',(-2.4117296293047,1.31152349915077,7.51180065547253));
#394920=CARTESIAN_POINT('Ctrl Pts',(-2.41157829503252,1.31148008890244,
7.51235175716501));
#394921=CARTESIAN_POINT('Ctrl Pts',(-2.41105537483772,1.31133008920184,
7.51425603304537));
#394922=CARTESIAN_POINT('Ctrl Pts',(-2.41058696594893,1.31094062862544,
7.51626900505183));
#394923=CARTESIAN_POINT('Ctrl Pts',(-2.4101839450164,1.31037107354313,7.51827788969247));
#394924=CARTESIAN_POINT('Ctrl Pts',(-2.41016213276193,1.31034024814577,
7.51838661432548));
#394925=CARTESIAN_POINT('Ctrl Pts',(-2.41014051310064,1.31030888531404,
7.51849533314857));
#394926=CARTESIAN_POINT('Ctrl Pts',(-2.41011908817658,1.31027699133284,
7.51860402984325));
#394927=CARTESIAN_POINT('Ctrl Pts',(-2.37073694715362,1.23681194779763,
7.57603338728985));
#394928=CARTESIAN_POINT('Ctrl Pts',(-2.38603924225309,1.25952355359294,
7.55196141284922));
#394929=CARTESIAN_POINT('Ctrl Pts',(-2.40131444509586,1.28219650716416,
7.52783573083104));
#394930=CARTESIAN_POINT('Ctrl Pts',(-2.4165647636488,1.30483398894316,7.50366116530176));
#394931=CARTESIAN_POINT('Origin',(-8.19199203866632E-16,4.27375699935086E-16,
7.49482233047033));
#394932=CARTESIAN_POINT('Origin',(-2.44485166369885,1.23150582317298,7.49482233047033));
#394933=CARTESIAN_POINT('Origin',(0.,0.,7.50366116523517));
#394934=CARTESIAN_POINT('Origin',(-2.40878727587059,1.30063450269627,7.49482233047033));
#394935=CARTESIAN_POINT('Ctrl Pts',(-2.45352105979441,1.22708152881661,
7.51860402984325));
#394936=CARTESIAN_POINT('Ctrl Pts',(-2.46112885786552,1.22694850799356,
7.51860402984325));
#394937=CARTESIAN_POINT('Ctrl Pts',(-2.46450482787546,1.22012948221841,
7.51860402984325));
#394938=CARTESIAN_POINT('Ctrl Pts',(-2.45634588711432,1.22703213600669,
7.51041458714366));
#394939=CARTESIAN_POINT('Ctrl Pts',(-2.4619286549569,1.22533299829127,7.51004642900443));
#394940=CARTESIAN_POINT('Ctrl Pts',(-2.46450575892791,1.22012760161206,
7.5072913648301));
#394941=CARTESIAN_POINT('Ctrl Pts',(-2.45736298124953,1.22965687536887,
7.50215815450137));
#394942=CARTESIAN_POINT('Ctrl Pts',(-2.46030031409413,1.2286223995395,7.49877163671529));
#394943=CARTESIAN_POINT('Ctrl Pts',(-2.46185245611965,1.22554103965677,
7.4948158853317));
#394944=CARTESIAN_POINT('Ctrl Pts',(-2.45274510440916,1.23548185916128,
7.50366171572174));
#394945=CARTESIAN_POINT('Ctrl Pts',(-2.45601536992562,1.23712913743439,
7.50000045605858));
#394946=CARTESIAN_POINT('Ctrl Pts',(-2.45601536992567,1.23712913743428,
7.49482233047317));
#394947=CARTESIAN_POINT('Origin',(-2.4533025332033,1.21458343911742,7.51860402984325));
#394948=CARTESIAN_POINT('Origin',(-2.4533025332033,1.21458343911742,9.));
#394949=CARTESIAN_POINT('Origin',(-2.4533025332033,1.21458343911742,8.75721825406948));
#394950=CARTESIAN_POINT('Ctrl Pts',(-2.43682453266412,1.22737484732811,
8.78942910404912));
#394951=CARTESIAN_POINT('Ctrl Pts',(-2.4423964617636,1.22729716327587,8.7967269950169));
#394952=CARTESIAN_POINT('Ctrl Pts',(-2.44391314215674,1.21850096144968,
8.79893251111267));
#394953=CARTESIAN_POINT('Ctrl Pts',(-2.44781717199849,1.22718171730772,
8.78111911759584));
#394954=CARTESIAN_POINT('Ctrl Pts',(-2.45442265473791,1.22708217884976,
8.78644465894815));
#394955=CARTESIAN_POINT('Ctrl Pts',(-2.45748133310548,1.2195748492034,8.78817647674132));
#394956=CARTESIAN_POINT('Ctrl Pts',(-2.45466804703032,1.22706135404061,
8.76780923932029));
#394957=CARTESIAN_POINT('Ctrl Pts',(-2.46246546371488,1.22693875788234,
8.76988516158373));
#394958=CARTESIAN_POINT('Ctrl Pts',(-2.46595667361419,1.22023444331371,
8.77093053738832));
#394959=CARTESIAN_POINT('Ctrl Pts',(-2.45333222015989,1.22708482322868,
8.75371302330492));
#394960=CARTESIAN_POINT('Ctrl Pts',(-2.46093827577203,1.22696599817776,
8.75300828287559));
#394961=CARTESIAN_POINT('Ctrl Pts',(-2.46430367349724,1.22010533950053,
8.75267964240738));
#394962=CARTESIAN_POINT('Origin',(-2.43928211585347,1.21482977004094,8.78727029226991));
#394963=CARTESIAN_POINT('Ctrl Pts',(-2.36802027905702,1.2285837299553,8.85049129520029));
#394964=CARTESIAN_POINT('Ctrl Pts',(-2.37385899372367,1.22848114699075,
8.85711686593484));
#394965=CARTESIAN_POINT('Ctrl Pts',(-2.37566317709459,1.22012377392992,
8.85933012996512));
#394966=CARTESIAN_POINT('Ctrl Pts',(-2.39188208645152,1.22816449129032,
8.82945683644721));
#394967=CARTESIAN_POINT('Ctrl Pts',(-2.39776926598005,1.22806105682515,
8.83607469902388));
#394968=CARTESIAN_POINT('Ctrl Pts',(-2.39954208843695,1.21967123304667,
8.8382956714852));
#394969=CARTESIAN_POINT('Ctrl Pts',(-2.41570832589789,1.22774587753438,
8.80838214965002));
#394970=CARTESIAN_POINT('Ctrl Pts',(-2.42161873898548,1.2276420348685,8.81501364461985));
#394971=CARTESIAN_POINT('Ctrl Pts',(-2.42338478937515,1.2192200470618,8.81722098428721));
#394972=CARTESIAN_POINT('Ctrl Pts',(-2.43950170000243,1.22732784120418,
8.78727029226991));
#394973=CARTESIAN_POINT('Ctrl Pts',(-2.44541309482909,1.2272239812897,8.79393457792714));
#394974=CARTESIAN_POINT('Ctrl Pts',(-2.44719404240189,1.21877012767605,
8.79610912703474));
#394975=CARTESIAN_POINT('Origin',(-2.36780069490807,1.21608565879206,8.85049129520029));
#394976=CARTESIAN_POINT('Ctrl Pts',(-2.36243414091426,1.23929131094304,
8.85049129520029));
#394977=CARTESIAN_POINT('Ctrl Pts',(-2.36569043114742,1.24413875213819,
8.85711686593484));
#394978=CARTESIAN_POINT('Ctrl Pts',(-2.35986814900603,1.25039988564418,
8.85933012996512));
#394979=CARTESIAN_POINT('Ctrl Pts',(-2.35955334795002,1.23500284969123,
8.86332496987233));
#394980=CARTESIAN_POINT('Ctrl Pts',(-2.35767030474023,1.23922257037475,
8.86648636486738));
#394981=CARTESIAN_POINT('Ctrl Pts',(-2.35182323496412,1.23839318691327,
8.87206031107457));
#394982=CARTESIAN_POINT('Ctrl Pts',(-2.36281975177212,1.22867510032302,
8.86341338519876));
#394983=CARTESIAN_POINT('Ctrl Pts',(-2.36518469322302,1.22469006298717,
8.86654584966059));
#394984=CARTESIAN_POINT('Ctrl Pts',(-2.3611016831163,1.22039434636991,8.87215952290714));
#394985=CARTESIAN_POINT('Ctrl Pts',(-2.36802027905702,1.2285837299553,8.85049129520029));
#394986=CARTESIAN_POINT('Ctrl Pts',(-2.37385899372367,1.22848114699075,
8.85711686593484));
#394987=CARTESIAN_POINT('Ctrl Pts',(-2.37566317709459,1.22012377392992,
8.85933012996512));
#394988=CARTESIAN_POINT('Origin',(-2.35205794196027,1.24626156884839,8.85049129520029));
#394989=CARTESIAN_POINT('Ctrl Pts',(-2.4022998076178,1.2986369039994,8.78727029226991));
#394990=CARTESIAN_POINT('Ctrl Pts',(-2.40559663206247,1.30354468600958,
8.79393457792714));
#394991=CARTESIAN_POINT('Ctrl Pts',(-2.39968192566133,1.30984196029029,
8.79610912703474));
#394992=CARTESIAN_POINT('Ctrl Pts',(-2.38903008369151,1.27888307316657,
8.80838214965001));
#394993=CARTESIAN_POINT('Ctrl Pts',(-2.39232636061377,1.28379004011346,
8.81501364461993));
#394994=CARTESIAN_POINT('Ctrl Pts',(-2.38642926673666,1.29005686517878,
8.81722098428721));
#394995=CARTESIAN_POINT('Ctrl Pts',(-2.3757420305442,1.25910195673734,8.82945683644722));
#394996=CARTESIAN_POINT('Ctrl Pts',(-2.37902534995512,1.26398963462523,
8.83607469902389));
#394997=CARTESIAN_POINT('Ctrl Pts',(-2.37315851053408,1.27024361237586,
8.83829567148519));
#394998=CARTESIAN_POINT('Ctrl Pts',(-2.36243414091426,1.23929131094303,
8.85049129520029));
#394999=CARTESIAN_POINT('Ctrl Pts',(-2.36569043114742,1.24413875213819,
8.85711686593484));
#395000=CARTESIAN_POINT('Ctrl Pts',(-2.35986814900603,1.25039988564418,
8.85933012996512));
#395001=CARTESIAN_POINT('Origin',(-2.39192360866381,1.30560716190476,8.78727029226991));
#395002=CARTESIAN_POINT('Ctrl Pts',(-2.41001582319738,1.31012330012151,
8.75374538247848));
#395003=CARTESIAN_POINT('Ctrl Pts',(-2.41426405357149,1.31642384907189,
8.75304829418601));
#395004=CARTESIAN_POINT('Ctrl Pts',(-2.41057140660495,1.32310479223806,
8.75272238421917));
#395005=CARTESIAN_POINT('Ctrl Pts',(-2.41075187368563,1.31121901294559,
8.76769408445018));
#395006=CARTESIAN_POINT('Ctrl Pts',(-2.4151064361957,1.31767849746975,8.76974318093969));
#395007=CARTESIAN_POINT('Ctrl Pts',(-2.41161165479856,1.32437214074276,
8.7707786988043));
#395008=CARTESIAN_POINT('Ctrl Pts',(-2.4069792981955,1.30560301318754,8.78108014887992));
#395009=CARTESIAN_POINT('Ctrl Pts',(-2.41067278344333,1.31107506984152,
8.78639403366326));
#395010=CARTESIAN_POINT('Ctrl Pts',(-2.40628851871305,1.31787950211056,
8.78812224174741));
#395011=CARTESIAN_POINT('Ctrl Pts',(-2.40079687974256,1.29639962934832,
8.78944554828684));
#395012=CARTESIAN_POINT('Ctrl Pts',(-2.40391425189901,1.3010081441259,8.79673892988686));
#395013=CARTESIAN_POINT('Ctrl Pts',(-2.39757616771974,1.30727968646036,
8.79894799272499));
#395014=CARTESIAN_POINT('Origin',(-2.39974288922259,1.3172472492382,8.75721825406948));
#395015=CARTESIAN_POINT('Origin',(-2.39974288922259,1.3172472492382,9.));
#395016=CARTESIAN_POINT('Origin',(-2.39974288922259,1.3172472492382,7.51860402984325));
#395017=CARTESIAN_POINT('Ctrl Pts',(-2.41656407141737,1.30483361513348,
7.50366195182967));
#395018=CARTESIAN_POINT('Ctrl Pts',(-2.41978630452746,1.30657347302834,
7.50000065167736));
#395019=CARTESIAN_POINT('Ctrl Pts',(-2.41978630452741,1.30657347302844,
7.49482233047108));
#395020=CARTESIAN_POINT('Ctrl Pts',(-2.41442578748734,1.31195973198919,
7.50215800491335));
#395021=CARTESIAN_POINT('Ctrl Pts',(-2.41525681547057,1.31496207934841,
7.49877273257265));
#395022=CARTESIAN_POINT('Ctrl Pts',(-2.41361667159588,1.31799969097933,
7.49481816995647));
#395023=CARTESIAN_POINT('Ctrl Pts',(-2.41169107100776,1.31261649840007,
7.51043025814043));
#395024=CARTESIAN_POINT('Ctrl Pts',(-2.41349603202947,1.3181694140934,7.51006209594515));
#395025=CARTESIAN_POINT('Ctrl Pts',(-2.41069940101147,1.32326429634045,
7.507312818217));
#395026=CARTESIAN_POINT('Ctrl Pts',(-2.41011824530876,1.31027573677064,
7.51860402984325));
#395027=CARTESIAN_POINT('Ctrl Pts',(-2.41436209596894,1.31659164913267,
7.51860402984325));
#395028=CARTESIAN_POINT('Ctrl Pts',(-2.41070061931037,1.3232620768603,7.51860402984325));
#395029=CARTESIAN_POINT('Origin',(0.,0.,7.5));
#395030=CARTESIAN_POINT('Origin',(-2.43698193351379,1.0853833789328,7.5));
#395031=CARTESIAN_POINT('',(-2.43698193351379,1.0853833789328,7.59394543036555));
#395032=CARTESIAN_POINT('',(-2.43698193351379,1.0853833789328,8.85049129520029));
#395033=CARTESIAN_POINT('',(-2.43698193351379,1.0853833789328,7.5));
#395034=CARTESIAN_POINT('',(-2.48056797713152,1.14205283806807,8.78727029226991));
#395035=CARTESIAN_POINT('Ctrl Pts',(-2.43698193351379,1.0853833789328,8.85049129520029));
#395036=CARTESIAN_POINT('Ctrl Pts',(-2.45153173356486,1.10430065682689,
8.82945686509571));
#395037=CARTESIAN_POINT('Ctrl Pts',(-2.46605990357881,1.12318981189994,
8.80838212259895));
#395038=CARTESIAN_POINT('Ctrl Pts',(-2.48056797713152,1.14205283806807,
8.78727029226991));
#395039=CARTESIAN_POINT('',(-2.48911697509583,1.15316802656819,8.75721825406948));
#395040=CARTESIAN_POINT('Origin',(-2.4633902345141,1.11971844545421,8.75937679713085));
#395041=CARTESIAN_POINT('',(-2.48911697509583,1.15316802656819,7.51860402984325));
#395042=CARTESIAN_POINT('',(-2.48911697509583,1.15316802656819,7.5));
#395043=CARTESIAN_POINT('Ctrl Pts',(-2.48911697509583,1.15316802656819,
7.51860402984325));
#395044=CARTESIAN_POINT('Ctrl Pts',(-2.48240306681555,1.14443877474015,
7.52834476460825));
#395045=CARTESIAN_POINT('Ctrl Pts',(-2.4756847999629,1.13570385600777,7.53807742314407));
#395046=CARTESIAN_POINT('Ctrl Pts',(-2.468962028193,1.12696308009723,7.54780169004674));
#395047=CARTESIAN_POINT('Ctrl Pts',(-2.4583135210443,1.11311816345355,7.5632044032688));
#395048=CARTESIAN_POINT('Ctrl Pts',(-2.4476536980993,1.09925853430098,7.57858609112103));
#395049=CARTESIAN_POINT('Ctrl Pts',(-2.43698193351379,1.0853833789328,7.59394543036555));
#395050=CARTESIAN_POINT('Origin',(-2.71595367934704,1.05190237523112,7.5));
#395051=CARTESIAN_POINT('',(-2.52710047532068,1.06736263792741,8.75721825406948));
#395052=CARTESIAN_POINT('',(-2.51312464689845,1.06850675396145,8.78727029226991));
#395053=CARTESIAN_POINT('Origin',(-2.47764878163776,1.07141094718992,8.75658640621009));
#395054=CARTESIAN_POINT('',(-2.44187055726728,1.07433989271894,8.85049129520029));
#395055=CARTESIAN_POINT('Ctrl Pts',(-2.51312464689845,1.06850675396145,
8.78727029226991));
#395056=CARTESIAN_POINT('Ctrl Pts',(-2.48940697290247,1.07044837561629,
8.80838212259896));
#395057=CARTESIAN_POINT('Ctrl Pts',(-2.46565644538429,1.07239268678908,
8.82945686509571));
#395058=CARTESIAN_POINT('Ctrl Pts',(-2.44187055726729,1.07433989271894,
8.85049129520029));
#395059=CARTESIAN_POINT('',(-2.44187055726728,1.07433989271894,7.59394543036555));
#395060=CARTESIAN_POINT('',(-2.44187055726728,1.07433989271894,7.5));
#395061=CARTESIAN_POINT('',(-2.52710047532068,1.06736263792741,7.51860402984325));
#395062=CARTESIAN_POINT('Ctrl Pts',(-2.44187055726728,1.07433989271894,
7.59394543036555));
#395063=CARTESIAN_POINT('Ctrl Pts',(-2.45931666632384,1.07291168592503,
7.57858609112103));
#395064=CARTESIAN_POINT('Ctrl Pts',(-2.47674325328886,1.07148507728598,
7.56320440326857));
#395065=CARTESIAN_POINT('Ctrl Pts',(-2.49415134128754,1.07005998304473,
7.54780169004651));
#395066=CARTESIAN_POINT('Ctrl Pts',(-2.50514167081741,1.0691602716391,7.53807742314383));
#395067=CARTESIAN_POINT('Ctrl Pts',(-2.51612463574748,1.06826116312845,
7.52834476460825));
#395068=CARTESIAN_POINT('Ctrl Pts',(-2.52710047532068,1.06736263792741,
7.51860402984325));
#395069=CARTESIAN_POINT('',(-2.52710047532068,1.06736263792741,7.5));
#395070=CARTESIAN_POINT('Origin',(-2.44243149520448,1.08119197077094,7.5));
#395071=CARTESIAN_POINT('Ctrl Pts',(-2.44187055726728,1.07433989271894,
8.85049129520029));
#395072=CARTESIAN_POINT('Ctrl Pts',(-2.44167754144849,1.07435569374958,
8.85097269580138));
#395073=CARTESIAN_POINT('Ctrl Pts',(-2.44148764717679,1.07437967878895,
8.85143669361005));
#395074=CARTESIAN_POINT('Ctrl Pts',(-2.44129223999293,1.07441381966454,
8.8519052845931));
#395075=CARTESIAN_POINT('Ctrl Pts',(-2.44091003593357,1.07448059705206,
8.85282181883899));
#395076=CARTESIAN_POINT('Ctrl Pts',(-2.44051660708415,1.07458470358959,
8.85372622499635));
#395077=CARTESIAN_POINT('Ctrl Pts',(-2.44010972412279,1.07474267860363,
8.8546225773507));
#395078=CARTESIAN_POINT('Ctrl Pts',(-2.43977194433938,1.07487382384955,
8.85536669723986));
#395079=CARTESIAN_POINT('Ctrl Pts',(-2.43942480388501,1.0750420942402,8.85610498449051));
#395080=CARTESIAN_POINT('Ctrl Pts',(-2.439070488446,1.0752641679127,8.85681338218371));
#395081=CARTESIAN_POINT('Ctrl Pts',(-2.43874894662864,1.07546570011927,
8.85745625420285));
#395082=CARTESIAN_POINT('Ctrl Pts',(-2.43841714453212,1.07571356340656,
8.85808743050666));
#395083=CARTESIAN_POINT('Ctrl Pts',(-2.43808062970449,1.07603581255776,
8.85866804508411));
#395084=CARTESIAN_POINT('Ctrl Pts',(-2.43792536905776,1.07618449133062,
8.85893592806396));
#395085=CARTESIAN_POINT('Ctrl Pts',(-2.43776918026209,1.07634923507315,
8.85919241173848));
#395086=CARTESIAN_POINT('Ctrl Pts',(-2.43761330950698,1.07653423293663,
8.85943017985534));
#395087=CARTESIAN_POINT('Ctrl Pts',(-2.4374028378449,1.07678403481755,8.8597512372));
#395088=CARTESIAN_POINT('Ctrl Pts',(-2.43718807887067,1.0770775368641,8.86004599534706));
#395089=CARTESIAN_POINT('Ctrl Pts',(-2.43698001810968,1.07741736300177,
8.86026130871721));
#395090=CARTESIAN_POINT('Ctrl Pts',(-2.43690384119922,1.07754178293148,
8.86034014101235));
#395091=CARTESIAN_POINT('Ctrl Pts',(-2.43682740741169,1.07767427508624,
8.86040910639692));
#395092=CARTESIAN_POINT('Ctrl Pts',(-2.4367530905129,1.07781139788106,8.86046313645506));
#395093=CARTESIAN_POINT('Ctrl Pts',(-2.43663711961473,1.07802537685398,
8.86054744990829));
#395094=CARTESIAN_POINT('Ctrl Pts',(-2.43652326724304,1.07825654310182,
8.86059655985668));
#395095=CARTESIAN_POINT('Ctrl Pts',(-2.43641857228559,1.07848994179131,
8.86059725258816));
#395096=CARTESIAN_POINT('Ctrl Pts',(-2.43631363544096,1.07872387972501,
8.86059794692011));
#395097=CARTESIAN_POINT('Ctrl Pts',(-2.43621915867709,1.07896374218055,
8.86056369958366));
#395098=CARTESIAN_POINT('Ctrl Pts',(-2.4361367935118,1.0791950678586,8.86048590497774));
#395099=CARTESIAN_POINT('Ctrl Pts',(-2.43611529865597,1.07925543697317,
8.86046560290182));
#395100=CARTESIAN_POINT('Ctrl Pts',(-2.43609443436159,1.07931604043715,
8.86044257503091));
#395101=CARTESIAN_POINT('Ctrl Pts',(-2.43607481431438,1.07937499486763,
8.86041778462584));
#395102=CARTESIAN_POINT('Ctrl Pts',(-2.43594279574309,1.07977168502834,
8.86025097596201));
#395103=CARTESIAN_POINT('Ctrl Pts',(-2.43584971171547,1.08014704858014,
8.8599848982295));
#395104=CARTESIAN_POINT('Ctrl Pts',(-2.43579005570161,1.08048809037632,
8.85968173251461));
#395105=CARTESIAN_POINT('Ctrl Pts',(-2.43575850108816,1.08066848194713,
8.85952137522076));
#395106=CARTESIAN_POINT('Ctrl Pts',(-2.43573550263548,1.08084271523859,
8.85934740853961));
#395107=CARTESIAN_POINT('Ctrl Pts',(-2.4357198434887,1.08100812974289,8.8591675900182));
#395108=CARTESIAN_POINT('Ctrl Pts',(-2.43565696387494,1.08167235495841,
8.85844552518696));
#395109=CARTESIAN_POINT('Ctrl Pts',(-2.43570585991415,1.08223163783065,
8.85759444184126));
#395110=CARTESIAN_POINT('Ctrl Pts',(-2.43578668621989,1.08268406612752,
8.85683498915141));
#395111=CARTESIAN_POINT('Ctrl Pts',(-2.43579514447753,1.08273141154388,
8.85675551445));
#395112=CARTESIAN_POINT('Ctrl Pts',(-2.43580397099506,1.08277757949648,
8.85667699793652));
#395113=CARTESIAN_POINT('Ctrl Pts',(-2.4358130862329,1.08282256237296,8.85659965593547));
#395114=CARTESIAN_POINT('Ctrl Pts',(-2.43593612417827,1.08342974353503,
8.85555568965886));
#395115=CARTESIAN_POINT('Ctrl Pts',(-2.43614206024081,1.08399551313591,
8.85434650606346));
#395116=CARTESIAN_POINT('Ctrl Pts',(-2.43642607255145,1.08452479370298,
8.85297329937117));
#395117=CARTESIAN_POINT('Ctrl Pts',(-2.43658581217106,1.08482248177242,
8.85220095427747));
#395118=CARTESIAN_POINT('Ctrl Pts',(-2.43677059316373,1.085108599615,8.85137579139183));
#395119=CARTESIAN_POINT('Ctrl Pts',(-2.43698193351379,1.0853833789328,8.85049129520029));
#395120=CARTESIAN_POINT('Origin',(-2.44243149520448,1.08119197077094,7.59394543036555));
#395121=CARTESIAN_POINT('Ctrl Pts',(-2.44131016723206,1.07438576844132,
7.59443877723642));
#395122=CARTESIAN_POINT('Ctrl Pts',(-2.43553868906203,1.07485824424131,
7.58783886950016));
#395123=CARTESIAN_POINT('Ctrl Pts',(-2.4342546998631,1.08325053554189,7.58559994247159));
#395124=CARTESIAN_POINT('Ctrl Pts',(-2.47281649723427,1.07180653691098,
7.56670252222137));
#395125=CARTESIAN_POINT('Ctrl Pts',(-2.46705336048875,1.07227832984935,
7.56004874999027));
#395126=CARTESIAN_POINT('Ctrl Pts',(-2.46574064338428,1.08071711714724,
7.55786368756704));
#395127=CARTESIAN_POINT('Ctrl Pts',(-2.50426399231304,1.06923212183783,
7.53888913333556));
#395128=CARTESIAN_POINT('Ctrl Pts',(-2.49846660496366,1.0697067186647,7.53222002137274));
#395129=CARTESIAN_POINT('Ctrl Pts',(-2.49716881203071,1.07818717727394,
7.53005029815327));
#395130=CARTESIAN_POINT('Ctrl Pts',(-2.53565122944802,1.06666263971588,
7.51101258149734));
#395131=CARTESIAN_POINT('Ctrl Pts',(-2.52978356722986,1.06714298951865,
7.5043616886572));
#395132=CARTESIAN_POINT('Ctrl Pts',(-2.52853765964446,1.07566092329588,
7.50217374673251));
#395133=CARTESIAN_POINT('',(-2.52686377755799,1.07579572642896,7.50366116523517));
#395134=CARTESIAN_POINT('Ctrl Pts',(-2.52710047532068,1.06736263792741,
7.51860402984325));
#395135=CARTESIAN_POINT('Ctrl Pts',(-2.52754061415969,1.06732660643878,
7.51734760759493));
#395136=CARTESIAN_POINT('Ctrl Pts',(-2.5279431969395,1.06735334527536,7.51608817408572));
#395137=CARTESIAN_POINT('Ctrl Pts',(-2.52830641272848,1.06745611722429,
7.51481005913119));
#395138=CARTESIAN_POINT('Ctrl Pts',(-2.52863542226947,1.06754921051145,
7.51365231206383));
#395139=CARTESIAN_POINT('Ctrl Pts',(-2.5289326624055,1.0677045807592,7.51247773061042));
#395140=CARTESIAN_POINT('Ctrl Pts',(-2.52917588459346,1.06795226365134,
7.51129758471022));
#395141=CARTESIAN_POINT('Ctrl Pts',(-2.52947818199606,1.06826010519982,
7.50983079813402));
#395142=CARTESIAN_POINT('Ctrl Pts',(-2.52967809354276,1.06870984917595,
7.50839324291155));
#395143=CARTESIAN_POINT('Ctrl Pts',(-2.52970174557798,1.06933826341191,
7.50715379678855));
#395144=CARTESIAN_POINT('Ctrl Pts',(-2.52971267213673,1.0696285726816,7.50658120839351));
#395145=CARTESIAN_POINT('Ctrl Pts',(-2.52967804016153,1.06999864075057,
7.50598221009429));
#395146=CARTESIAN_POINT('Ctrl Pts',(-2.52957602630725,1.07043754110358,
7.50545747549611));
#395147=CARTESIAN_POINT('Ctrl Pts',(-2.52952158855699,1.07067175191719,
7.50517746087247));
#395148=CARTESIAN_POINT('Ctrl Pts',(-2.5294475699509,1.07092814907601,7.50491486231392));
#395149=CARTESIAN_POINT('Ctrl Pts',(-2.52935432805341,1.0711994801088,7.50468370960993));
#395150=CARTESIAN_POINT('Ctrl Pts',(-2.52921490200517,1.07160520558933,
7.50433806340447));
#395151=CARTESIAN_POINT('Ctrl Pts',(-2.52902778596954,1.07205630799002,
7.50405484070984));
#395152=CARTESIAN_POINT('Ctrl Pts',(-2.52880492013753,1.0725221319208,7.50385766036131));
#395153=CARTESIAN_POINT('Ctrl Pts',(-2.52878108810092,1.07257194454966,
7.50383657498791));
#395154=CARTESIAN_POINT('Ctrl Pts',(-2.52875687081669,1.07262190971424,
7.50381643264937));
#395155=CARTESIAN_POINT('Ctrl Pts',(-2.52873230017346,1.0726719787141,7.50379723213559));
#395156=CARTESIAN_POINT('Ctrl Pts',(-2.52856828309231,1.07300620566688,
7.50366906242519));
#395157=CARTESIAN_POINT('Ctrl Pts',(-2.52838430707247,1.07335201295404,
7.50358235568538));
#395158=CARTESIAN_POINT('Ctrl Pts',(-2.52819896460947,1.07368106596535,
7.5035341175365));
#395159=CARTESIAN_POINT('Ctrl Pts',(-2.52792106456293,1.07417444371418,
7.50346178989176));
#395160=CARTESIAN_POINT('Ctrl Pts',(-2.52760112950023,1.07469338991018,
7.50346967198527));
#395161=CARTESIAN_POINT('Ctrl Pts',(-2.5272713767736,1.07519317013141,7.50354272648692));
#395162=CARTESIAN_POINT('Ctrl Pts',(-2.52713574265166,1.07539874008124,
7.50357277531559));
#395163=CARTESIAN_POINT('Ctrl Pts',(-2.52699874610053,1.07560087239689,
7.50361331098761));
#395164=CARTESIAN_POINT('Ctrl Pts',(-2.5268637775593,1.07579572642952,7.50366116523659));
#395165=CARTESIAN_POINT('',(-2.44510882695062,1.08237714611494,7.57603338622103));
#395166=CARTESIAN_POINT('Origin',(-2.45318828011502,1.08595680059032,7.58486873427628));
#395167=CARTESIAN_POINT('Ctrl Pts',(-2.52686377761447,1.07579572641904,
7.50366116529969));
#395168=CARTESIAN_POINT('Ctrl Pts',(-2.49965666355485,1.0779867862876,7.52783573079709));
#395169=CARTESIAN_POINT('Ctrl Pts',(-2.47240630148104,1.08018050713207,
7.55196141284069));
#395170=CARTESIAN_POINT('Ctrl Pts',(-2.44510882811945,1.08237714566607,
7.57603338728831));
#395171=CARTESIAN_POINT('Ctrl Pts',(-2.44290988201821,1.07443121403224,
7.59639677331372));
#395172=CARTESIAN_POINT('Ctrl Pts',(-2.42383037731441,1.07295780766364,
7.59974925422225));
#395173=CARTESIAN_POINT('Ctrl Pts',(-2.43774827562803,1.08609137277752,
7.59639677331371));
#395174=CARTESIAN_POINT('Ctrl Pts',(-2.43911965275287,1.07350965763145,
7.58707626057423));
#395175=CARTESIAN_POINT('Ctrl Pts',(-2.43325291397481,1.07712888513353,
7.58811717123965));
#395176=CARTESIAN_POINT('Ctrl Pts',(-2.43451789319206,1.08390511263723,
7.58707626057423));
#395177=CARTESIAN_POINT('Ctrl Pts',(-2.44221276280681,1.0787401740931,7.5801537675693));
#395178=CARTESIAN_POINT('Ctrl Pts',(-2.43957276865564,1.07992649732889,
7.5820876076604));
#395179=CARTESIAN_POINT('Ctrl Pts',(-2.4404694300849,1.08267839307892,7.5801537675693));
#395180=CARTESIAN_POINT('Ctrl Pts',(-2.44510882619396,1.08237714577977,
7.57603338509286));
#395181=CARTESIAN_POINT('Ctrl Pts',(-2.44510882619396,1.08237714577977,
7.57603338509286));
#395182=CARTESIAN_POINT('Ctrl Pts',(-2.44510882619396,1.08237714577977,
7.57603338509286));
#395183=CARTESIAN_POINT('Origin',(-2.4531905899516,1.08595158263,7.5848687342762));
#395184=CARTESIAN_POINT('Ctrl Pts',(-2.49436399277437,1.15999006475372,
7.51098857897448));
#395185=CARTESIAN_POINT('Ctrl Pts',(-2.4907747342627,1.15532340263736,7.50433767179956));
#395186=CARTESIAN_POINT('Ctrl Pts',(-2.49624278171655,1.14867445474127,
7.50214974420965));
#395187=CARTESIAN_POINT('Ctrl Pts',(-2.47515893410406,1.13502013866792,
7.53887321589168));
#395188=CARTESIAN_POINT('Ctrl Pts',(-2.47161268127916,1.13040939144553,
7.53220407452062));
#395189=CARTESIAN_POINT('Ctrl Pts',(-2.47701807999249,1.1237472157745,7.53003438070911));
#395190=CARTESIAN_POINT('Ctrl Pts',(-2.45591699463667,1.11000226111302,
7.56669465659236));
#395191=CARTESIAN_POINT('Ctrl Pts',(-2.45239169950658,1.10541876254954,
7.56004085833301));
#395192=CARTESIAN_POINT('Ctrl Pts',(-2.45775620401614,1.09877355815139,
7.5578558219379));
#395193=CARTESIAN_POINT('Ctrl Pts',(-2.43663904460805,1.08493756354744,
7.59443891967696));
#395194=CARTESIAN_POINT('Ctrl Pts',(-2.43310863823899,1.08034741948168,
7.58783901202978));
#395195=CARTESIAN_POINT('Ctrl Pts',(-2.43845803954466,1.07375476571713,
7.58560008491213));
#395196=CARTESIAN_POINT('',(-2.49520067284433,1.14732323151527,7.50366116523517));
#395197=CARTESIAN_POINT('Ctrl Pts',(-2.49520067284467,1.14732323151543,
7.50366116523554));
#395198=CARTESIAN_POINT('Ctrl Pts',(-2.49502946219894,1.1480613537489,7.50350835821027));
#395199=CARTESIAN_POINT('Ctrl Pts',(-2.49484806402455,1.14873429707004,
7.50345484956));
#395200=CARTESIAN_POINT('Ctrl Pts',(-2.49465166501225,1.14936222492287,
7.50349758195598));
#395201=CARTESIAN_POINT('Ctrl Pts',(-2.49455089775362,1.14968439847971,
7.50351950684424));
#395202=CARTESIAN_POINT('Ctrl Pts',(-2.49443637311435,1.15002651529798,
7.50357029184312));
#395203=CARTESIAN_POINT('Ctrl Pts',(-2.49431687004512,1.15035337898108,
7.50365515313923));
#395204=CARTESIAN_POINT('Ctrl Pts',(-2.49413302593306,1.15085622768587,
7.50378570417639));
#395205=CARTESIAN_POINT('Ctrl Pts',(-2.49393232888106,1.15133785676731,
7.50400001621911));
#395206=CARTESIAN_POINT('Ctrl Pts',(-2.4937279591097,1.15176073395383,7.50428903009635));
#395207=CARTESIAN_POINT('Ctrl Pts',(-2.4937052756374,1.1518076700681,7.50432110841318));
#395208=CARTESIAN_POINT('Ctrl Pts',(-2.49368255155363,1.15185391235974,
7.50435406373355));
#395209=CARTESIAN_POINT('Ctrl Pts',(-2.49365980799992,1.15189943166856,
7.50438785222352));
#395210=CARTESIAN_POINT('Ctrl Pts',(-2.49352094767257,1.15217734892834,
7.50459414719561));
#395211=CARTESIAN_POINT('Ctrl Pts',(-2.49337868940288,1.1524325098406,7.50483629897752));
#395212=CARTESIAN_POINT('Ctrl Pts',(-2.49323963252003,1.1526557801154,7.5050991045531));
#395213=CARTESIAN_POINT('Ctrl Pts',(-2.49293285906952,1.15314833676699,
7.50567888004914));
#395214=CARTESIAN_POINT('Ctrl Pts',(-2.49263001938426,1.15350537014205,
7.50637912803144));
#395215=CARTESIAN_POINT('Ctrl Pts',(-2.49234864839803,1.15375233499365,
7.50710440483569));
#395216=CARTESIAN_POINT('Ctrl Pts',(-2.49227965064621,1.1538128956782,7.50728225710685));
#395217=CARTESIAN_POINT('Ctrl Pts',(-2.49221066660843,1.15386815290565,
7.50746498566954));
#395218=CARTESIAN_POINT('Ctrl Pts',(-2.4921435670402,1.1539171419371,7.50764697238949));
#395219=CARTESIAN_POINT('Ctrl Pts',(-2.49178285822774,1.15418049348807,
7.50862528291181));
#395220=CARTESIAN_POINT('Ctrl Pts',(-2.49144630392675,1.15428995340173,
7.50965856837422));
#395221=CARTESIAN_POINT('Ctrl Pts',(-2.49113671363289,1.15431175990403,
7.51067959873202));
#395222=CARTESIAN_POINT('Ctrl Pts',(-2.49096634570368,1.15432376004975,
7.51124147302578));
#395223=CARTESIAN_POINT('Ctrl Pts',(-2.49080407122456,1.15430878557776,
7.51180065547253));
#395224=CARTESIAN_POINT('Ctrl Pts',(-2.49065026658072,1.15427516054054,
7.512351757165));
#395225=CARTESIAN_POINT('Ctrl Pts',(-2.49011881026773,1.15415897264233,
7.51425603304536));
#395226=CARTESIAN_POINT('Ctrl Pts',(-2.48962641095044,1.15380032331501,
7.5162690050518));
#395227=CARTESIAN_POINT('Ctrl Pts',(-2.48918772654822,1.15325776008451,
7.51827788969244));
#395228=CARTESIAN_POINT('Ctrl Pts',(-2.48916398411938,1.15322839553717,
7.51838661432545));
#395229=CARTESIAN_POINT('Ctrl Pts',(-2.48914039945447,1.1531984823202,7.51849533314857));
#395230=CARTESIAN_POINT('Ctrl Pts',(-2.48911697509582,1.15316802656819,
7.51860402984325));
#395231=CARTESIAN_POINT('Ctrl Pts',(-2.44510882740512,1.08237714728269,
7.57603338728985));
#395232=CARTESIAN_POINT('Ctrl Pts',(-2.46183481987753,1.10406166823487,
7.55196141284923));
#395233=CARTESIAN_POINT('Ctrl Pts',(-2.47853129930075,1.1257093521849,7.52783573083105));
#395234=CARTESIAN_POINT('Ctrl Pts',(-2.49520067287602,1.14732323156525,
7.50366116530176));
#395235=CARTESIAN_POINT('Origin',(-8.44898126352701E-16,3.74011337523909E-16,
7.49482233047033));
#395236=CARTESIAN_POINT('Origin',(-2.51873130274449,1.07233337846729,7.49482233047033));
#395237=CARTESIAN_POINT('Origin',(0.,0.,7.50366116523517));
#395238=CARTESIAN_POINT('Origin',(-2.48717010277294,1.14363067896609,7.49482233047033));
#395239=CARTESIAN_POINT('Ctrl Pts',(-2.5270994211233,1.06736272418324,7.51860402984325));
#395240=CARTESIAN_POINT('Ctrl Pts',(-2.53468306548394,1.06674254336975,
7.51860402984325));
#395241=CARTESIAN_POINT('Ctrl Pts',(-2.53761520271996,1.05972122887321,
7.51860402984325));
#395242=CARTESIAN_POINT('Ctrl Pts',(-2.52991527992432,1.06713244554835,
7.51041458714367));
#395243=CARTESIAN_POINT('Ctrl Pts',(-2.53537771324442,1.06507910972982,
7.51004642900442));
#395244=CARTESIAN_POINT('Ctrl Pts',(-2.5376160113686,1.05971929247804,7.5072913648301));
#395245=CARTESIAN_POINT('Ctrl Pts',(-2.53109845195889,1.06968662665703,
7.50215815450137));
#395246=CARTESIAN_POINT('Ctrl Pts',(-2.53396347064417,1.06846608070768,
7.4987716367153));
#395247=CARTESIAN_POINT('Ctrl Pts',(-2.53531500022191,1.06529160572828,
7.49481588533171));
#395248=CARTESIAN_POINT('Ctrl Pts',(-2.52686327103471,1.0757955107805,7.50366171572174));
#395249=CARTESIAN_POINT('Ctrl Pts',(-2.53023235892125,1.0772298779127,7.50000045605858));
#395250=CARTESIAN_POINT('Ctrl Pts',(-2.5302323589213,1.07722987791258,7.49482233047317));
#395251=CARTESIAN_POINT('Origin',(-2.52608058816214,1.05490431419651,7.51860402984325));
#395252=CARTESIAN_POINT('Origin',(-2.52608058816214,1.05490431419651,9.));
#395253=CARTESIAN_POINT('Origin',(-2.52608058816214,1.05490431419651,8.75721825406948));
#395254=CARTESIAN_POINT('Ctrl Pts',(-2.51045599178025,1.06872519020655,
8.78942910404912));
#395255=CARTESIAN_POINT('Ctrl Pts',(-2.5160114955195,1.0682906710414,8.7967269950169));
#395256=CARTESIAN_POINT('Ctrl Pts',(-2.51696148514411,1.05941536790882,
8.79893251111267));
#395257=CARTESIAN_POINT('Ctrl Pts',(-2.52141367167526,1.06782815617218,
8.78111911759584));
#395258=CARTESIAN_POINT('Ctrl Pts',(-2.52799920529106,1.06730560749445,
8.78644465894814));
#395259=CARTESIAN_POINT('Ctrl Pts',(-2.53057060301398,1.05961773226615,
8.78817647674132));
#395260=CARTESIAN_POINT('Ctrl Pts',(-2.5282427591486,1.06726910313396,8.76780923932029));
#395261=CARTESIAN_POINT('Ctrl Pts',(-2.53601630044146,1.06664717666037,
8.76988516158373));
#395262=CARTESIAN_POINT('Ctrl Pts',(-2.53907079036638,1.05973295423882,
8.77093053738833));
#395263=CARTESIAN_POINT('Ctrl Pts',(-2.52691118055377,1.0673781108235,8.75371302330492));
#395264=CARTESIAN_POINT('Ctrl Pts',(-2.53449399556176,1.06677220825514,
8.75300828287559));
#395265=CARTESIAN_POINT('Ctrl Pts',(-2.53741291480574,1.05971002376439,
8.75267964240738));
#395266=CARTESIAN_POINT('Origin',(-2.51210475973991,1.05604843023055,8.78727029226991));
#395267=CARTESIAN_POINT('Ctrl Pts',(-2.44187055726728,1.07433989271894,
8.85049129520029));
#395268=CARTESIAN_POINT('Ctrl Pts',(-2.44769070315534,1.073863432789,8.85711686593484));
#395269=CARTESIAN_POINT('Ctrl Pts',(-2.44895572090756,1.06540763642198,
8.85933012996512));
#395270=CARTESIAN_POINT('Ctrl Pts',(-2.46565647730584,1.07239268417586,
8.82945683644723));
#395271=CARTESIAN_POINT('Ctrl Pts',(-2.4715249339237,1.07191226934043,8.8360746990239));
#395272=CARTESIAN_POINT('Ctrl Pts',(-2.47275657607163,1.06342609822992,
8.83829567148519));
#395273=CARTESIAN_POINT('Ctrl Pts',(-2.48940694251248,1.07044837810413,
8.80838214965003));
#395274=CARTESIAN_POINT('Ctrl Pts',(-2.49529855880007,1.06996606732746,
8.81501364461988));
#395275=CARTESIAN_POINT('Ctrl Pts',(-2.49652138203832,1.06144823216098,
8.81722098428721));
#395276=CARTESIAN_POINT('Ctrl Pts',(-2.51312464689845,1.06850675396145,
8.78727029226991));
#395277=CARTESIAN_POINT('Ctrl Pts',(-2.51901724180287,1.06802436307137,
8.79393457792714));
#395278=CARTESIAN_POINT('Ctrl Pts',(-2.52025288996716,1.05947377310387,
8.79610912703474));
#395279=CARTESIAN_POINT('Origin',(-2.44085067010875,1.06188156898805,8.85049129520029));
#395280=CARTESIAN_POINT('Ctrl Pts',(-2.43698193351379,1.0853833789328,8.85049129520029));
#395281=CARTESIAN_POINT('Ctrl Pts',(-2.44054210997315,1.09001222930857,
8.85711686593484));
#395282=CARTESIAN_POINT('Ctrl Pts',(-2.43513294253591,1.09663353354187,
8.85933012996512));
#395283=CARTESIAN_POINT('Ctrl Pts',(-2.43383229679188,1.08128830182353,
8.86332496987231));
#395284=CARTESIAN_POINT('Ctrl Pts',(-2.43222348092876,1.08561999963099,
8.86648636486737));
#395285=CARTESIAN_POINT('Ctrl Pts',(-2.42633528580379,1.08516694327359,
8.87206031107457));
#395286=CARTESIAN_POINT('Ctrl Pts',(-2.436686569143,1.07476427428361,8.86341338519877));
#395287=CARTESIAN_POINT('Ctrl Pts',(-2.4387913293493,1.07063590231536,8.86654584966059));
#395288=CARTESIAN_POINT('Ctrl Pts',(-2.43444148071611,1.06661061106433,
8.87215952290714));
#395289=CARTESIAN_POINT('Ctrl Pts',(-2.44187055726728,1.07433989271894,
8.85049129520029));
#395290=CARTESIAN_POINT('Ctrl Pts',(-2.44769070315534,1.073863432789,8.85711686593484));
#395291=CARTESIAN_POINT('Ctrl Pts',(-2.44895572090756,1.06540763642198,
8.85933012996512));
#395292=CARTESIAN_POINT('Origin',(-2.42707363953071,1.09300412104528,8.85049129520029));
#395293=CARTESIAN_POINT('Ctrl Pts',(-2.48056797713152,1.14205283806807,
8.78727029226991));
#395294=CARTESIAN_POINT('Ctrl Pts',(-2.48417247056979,1.14673930824634,
8.79393457792714));
#395295=CARTESIAN_POINT('Ctrl Pts',(-2.47867338431574,1.1534026006419,8.79610912703474));
#395296=CARTESIAN_POINT('Ctrl Pts',(-2.46605988498929,1.12318978773032,
8.80838214965001));
#395297=CARTESIAN_POINT('Ctrl Pts',(-2.46966377980882,1.12787547959983,
8.81501364461993));
#395298=CARTESIAN_POINT('Ctrl Pts',(-2.46418031900403,1.1345072569029,8.81722098428721));
#395299=CARTESIAN_POINT('Ctrl Pts',(-2.45153175309122,1.10430068221457,
8.82945683644722));
#395300=CARTESIAN_POINT('Ctrl Pts',(-2.4551214811677,1.10896795484712,8.83607469902389));
#395301=CARTESIAN_POINT('Ctrl Pts',(-2.44966738952775,1.11558497282201,
8.83829567148519));
#395302=CARTESIAN_POINT('Ctrl Pts',(-2.43698193351379,1.0853833789328,8.85049129520029));
#395303=CARTESIAN_POINT('Ctrl Pts',(-2.44054210997315,1.09001222930857,
8.85711686593484));
#395304=CARTESIAN_POINT('Ctrl Pts',(-2.43513294253591,1.09663353354187,
8.85933012996512));
#395305=CARTESIAN_POINT('Origin',(-2.47065968314844,1.14967358018055,8.78727029226991));
#395306=CARTESIAN_POINT('Ctrl Pts',(-2.48900407525588,1.15302126734187,
8.75374538247849));
#395307=CARTESIAN_POINT('Ctrl Pts',(-2.49364725474231,1.1590366860841,8.75304829418602));
#395308=CARTESIAN_POINT('Ctrl Pts',(-2.49039024421334,1.16594049123946,
8.75272238421917));
#395309=CARTESIAN_POINT('Ctrl Pts',(-2.48980881601113,1.15406756998975,
8.76769408445016));
#395310=CARTESIAN_POINT('Ctrl Pts',(-2.49456829219992,1.16023478503224,
8.76974318093967));
#395311=CARTESIAN_POINT('Ctrl Pts',(-2.49150955440295,1.16713858691016,
8.7707786988043));
#395312=CARTESIAN_POINT('Ctrl Pts',(-2.48568417334204,1.14870481864704,
8.78108014887994));
#395313=CARTESIAN_POINT('Ctrl Pts',(-2.48972066580186,1.15392898996144,
8.78639403366327));
#395314=CARTESIAN_POINT('Ctrl Pts',(-2.48578137048602,1.16100034260033,
8.78812224174741));
#395315=CARTESIAN_POINT('Ctrl Pts',(-2.47892479450374,1.13991645305729,
8.78944554828685));
#395316=CARTESIAN_POINT('Ctrl Pts',(-2.48233103024034,1.14431576842716,
8.79673892988685));
#395317=CARTESIAN_POINT('Ctrl Pts',(-2.47640778743176,1.1509805076529,8.79894799272499));
#395318=CARTESIAN_POINT('Origin',(-2.47920868111275,1.16078876868067,8.75721825406948));
#395319=CARTESIAN_POINT('Origin',(-2.47920868111275,1.16078876868067,9.));
#395320=CARTESIAN_POINT('Origin',(-2.47920868111275,1.16078876868067,7.51860402984325));
#395321=CARTESIAN_POINT('Ctrl Pts',(-2.49519995811679,1.14732290287503,
7.50366195182966));
#395322=CARTESIAN_POINT('Ctrl Pts',(-2.49852704388144,1.14885273686104,
7.50000065167735));
#395323=CARTESIAN_POINT('Ctrl Pts',(-2.49852704388139,1.14885273686115,
7.49482233047108));
#395324=CARTESIAN_POINT('Ctrl Pts',(-2.49352263939497,1.15457137868116,
7.50215800491337));
#395325=CARTESIAN_POINT('Ctrl Pts',(-2.49454432099783,1.15751431325004,
7.49877273257264));
#395326=CARTESIAN_POINT('Ctrl Pts',(-2.49310216742007,1.16065076816093,
7.49481816995647));
#395327=CARTESIAN_POINT('Ctrl Pts',(-2.49083562085213,1.15540200958145,
7.51043025814042));
#395328=CARTESIAN_POINT('Ctrl Pts',(-2.49299264991784,1.1608278719642,7.51006209594515));
#395329=CARTESIAN_POINT('Ctrl Pts',(-2.49052819510454,1.16609146699379,
7.50731281821699));
#395330=CARTESIAN_POINT('Ctrl Pts',(-2.48911605357969,1.15316682858636,
7.51860402984325));
#395331=CARTESIAN_POINT('Ctrl Pts',(-2.49375584668794,1.1591978597837,7.51860402984325));
#395332=CARTESIAN_POINT('Ctrl Pts',(-2.49052926869774,1.16608917401712,
7.51860402984325));
#395333=CARTESIAN_POINT('Origin',(0.,0.,7.5));
#395334=CARTESIAN_POINT('Origin',(-2.50151564461753,0.927015373804532,7.5));
#395335=CARTESIAN_POINT('',(-2.50151564461753,0.927015373804532,7.59394543036555));
#395336=CARTESIAN_POINT('',(-2.50151564461753,0.927015373804532,8.85049129520029));
#395337=CARTESIAN_POINT('',(-2.50151564461753,0.927015373804532,7.5));
#395338=CARTESIAN_POINT('',(-2.54864296074704,0.980775832055543,8.78727029226991));
#395339=CARTESIAN_POINT('Ctrl Pts',(-2.50151564461753,0.927015373804532,
8.85049129520029));
#395340=CARTESIAN_POINT('Ctrl Pts',(-2.51724758470004,0.944961575232364,
8.82945686509571));
#395341=CARTESIAN_POINT('Ctrl Pts',(-2.53295613735134,0.96288109746175,
8.80838212259895));
#395342=CARTESIAN_POINT('Ctrl Pts',(-2.54864296074704,0.980775832055543,
8.78727029226991));
#395343=CARTESIAN_POINT('',(-2.55788654645048,0.991320447028606,8.75721825406948));
#395344=CARTESIAN_POINT('Origin',(-2.53006954219739,0.959587909596253,8.75937679713144));
#395345=CARTESIAN_POINT('',(-2.55788654645048,0.991320447028606,7.51860402984325));
#395346=CARTESIAN_POINT('',(-2.55788654645048,0.991320447028606,7.5));
#395347=CARTESIAN_POINT('Ctrl Pts',(-2.55788654645048,0.991320447028606,
7.51860402984325));
#395348=CARTESIAN_POINT('Ctrl Pts',(-2.55062714752994,0.9830392919651,7.52834476460825));
#395349=CARTESIAN_POINT('Ctrl Pts',(-2.54336303591238,0.974752760895221,
7.53807742314407));
#395350=CARTESIAN_POINT('Ctrl Pts',(-2.53609405336271,0.966460673312405,
7.54780169004674));
#395351=CARTESIAN_POINT('Ctrl Pts',(-2.52458037785902,0.953326454730319,
7.5632044032688));
#395352=CARTESIAN_POINT('Ctrl Pts',(-2.51305446717486,0.94017827887332,
7.57858609112103));
#395353=CARTESIAN_POINT('Ctrl Pts',(-2.50151564461753,0.927015373804532,
7.59394543036555));
#395354=CARTESIAN_POINT('Origin',(-2.77776907780699,0.87572937929184,7.5));
#395355=CARTESIAN_POINT('',(-2.59029443537466,0.903257743546346,8.75721825406948));
#395356=CARTESIAN_POINT('',(-2.57642062555681,0.905294943272712,8.78727029226991));
#395357=CARTESIAN_POINT('Origin',(-2.54120372156563,0.910466116015902,8.75658640621026));
#395358=CARTESIAN_POINT('',(-2.50568666557814,0.91568136241822,8.85049129520029));
#395359=CARTESIAN_POINT('Ctrl Pts',(-2.57642062555681,0.905294943272712,
8.78727029226991));
#395360=CARTESIAN_POINT('Ctrl Pts',(-2.5528760821923,0.908752172247975,
8.80838212259895));
#395361=CARTESIAN_POINT('Ctrl Pts',(-2.52929892512471,0.912214190147685,
8.82945686509571));
#395362=CARTESIAN_POINT('Ctrl Pts',(-2.50568666557814,0.91568136241822,
8.85049129520029));
#395363=CARTESIAN_POINT('',(-2.50568666557814,0.91568136241822,7.59394543036555));
#395364=CARTESIAN_POINT('',(-2.50568666557814,0.91568136241822,7.5));
#395365=CARTESIAN_POINT('',(-2.59029443537466,0.903257743546346,7.51860402984325));
#395366=CARTESIAN_POINT('Ctrl Pts',(-2.50568666557814,0.91568136241822,
7.59394543036555));
#395367=CARTESIAN_POINT('Ctrl Pts',(-2.52300542420909,0.913138313983279,
7.57858609112103));
#395368=CARTESIAN_POINT('Ctrl Pts',(-2.54030480325286,0.910598111204322,
7.56320440326857));
#395369=CARTESIAN_POINT('Ctrl Pts',(-2.5575858183662,0.908060604944507,
7.54780169004651));
#395370=CARTESIAN_POINT('Ctrl Pts',(-2.56849592237767,0.906458589261821,
7.53807742314383));
#395371=CARTESIAN_POINT('Ctrl Pts',(-2.57939871554831,0.904857647086919,
7.52834476460825));
#395372=CARTESIAN_POINT('Ctrl Pts',(-2.59029443537466,0.903257743546347,
7.51860402984324));
#395373=CARTESIAN_POINT('',(-2.59029443537466,0.903257743546346,7.5));
#395374=CARTESIAN_POINT('Origin',(-2.5066854651563,0.922483422723941,7.5));
#395375=CARTESIAN_POINT('Ctrl Pts',(-2.50568666557814,0.91568136241822,
8.85049129520029));
#395376=CARTESIAN_POINT('Ctrl Pts',(-2.50549505870656,0.915709497549917,
8.85097269580138));
#395377=CARTESIAN_POINT('Ctrl Pts',(-2.50530709131976,0.915745599877208,
8.85143669361005));
#395378=CARTESIAN_POINT('Ctrl Pts',(-2.50511427303432,0.915792190387963,
8.8519052845931));
#395379=CARTESIAN_POINT('Ctrl Pts',(-2.5047371326961,0.915883318472337,
8.85282181883899));
#395380=CARTESIAN_POINT('Ctrl Pts',(-2.50435118231721,0.916012418184756,
8.85372622499635));
#395381=CARTESIAN_POINT('Ctrl Pts',(-2.50395525683443,0.916196137703026,
8.8546225773507));
#395382=CARTESIAN_POINT('Ctrl Pts',(-2.50362657356056,0.916348655121995,
8.85536669723986));
#395383=CARTESIAN_POINT('Ctrl Pts',(-2.50329092746443,0.916538821148363,
8.8561049844905));
#395384=CARTESIAN_POINT('Ctrl Pts',(-2.50295156831354,0.916783139614805,
8.8568133821837));
#395385=CARTESIAN_POINT('Ctrl Pts',(-2.50264359935114,0.91700485900681,
8.85745625420284));
#395386=CARTESIAN_POINT('Ctrl Pts',(-2.50232835963296,0.917273471665707,
8.85808743050666));
#395387=CARTESIAN_POINT('Ctrl Pts',(-2.50201318278513,0.917616619300495,
8.8586680450841));
#395388=CARTESIAN_POINT('Ctrl Pts',(-2.50186776701974,0.917774940180657,
8.85893592806395));
#395389=CARTESIAN_POINT('Ctrl Pts',(-2.50172245429852,0.917949352490005,
8.85919241173848));
#395390=CARTESIAN_POINT('Ctrl Pts',(-2.50157875665041,0.918143956929098,
8.85943017985534));
#395391=CARTESIAN_POINT('Ctrl Pts',(-2.50138472228639,0.918406730530955,
8.8597512372));
#395392=CARTESIAN_POINT('Ctrl Pts',(-2.50118920929819,0.918713389200792,
8.86004599534705));
#395393=CARTESIAN_POINT('Ctrl Pts',(-2.50100334875574,0.91906584762794,
8.86026130871721));
#395394=CARTESIAN_POINT('Ctrl Pts',(-2.50093529997118,0.919194892594974,
8.86034014101235));
#395395=CARTESIAN_POINT('Ctrl Pts',(-2.50086751202657,0.919332009659972,
8.86040910639693));
#395396=CARTESIAN_POINT('Ctrl Pts',(-2.50080213330744,0.919473612221358,
8.86046313645507));
#395397=CARTESIAN_POINT('Ctrl Pts',(-2.50070011036379,0.91969458183249,
8.8605474499083));
#395398=CARTESIAN_POINT('Ctrl Pts',(-2.50060130278636,0.919932567670979,
8.86059655985669));
#395399=CARTESIAN_POINT('Ctrl Pts',(-2.5005117768413,0.920172194646778,
8.86059725258816));
#395400=CARTESIAN_POINT('Ctrl Pts',(-2.50042204405555,0.920412375256622,
8.86059794692011));
#395401=CARTESIAN_POINT('Ctrl Pts',(-2.50034312944461,0.920657798036075,
8.86056369958366));
#395402=CARTESIAN_POINT('Ctrl Pts',(-2.50027575459447,0.920893925584962,
8.86048590497774));
#395403=CARTESIAN_POINT('Ctrl Pts',(-2.50025817176458,0.920955547844857,
8.86046560290182));
#395404=CARTESIAN_POINT('Ctrl Pts',(-2.5002412332154,0.921017363572455,
8.86044257503091));
#395405=CARTESIAN_POINT('Ctrl Pts',(-2.50022543070301,0.921077453935466,
8.86041778462584));
#395406=CARTESIAN_POINT('Ctrl Pts',(-2.5001190994039,0.921481787512609,
8.86025097596201));
#395407=CARTESIAN_POINT('Ctrl Pts',(-2.50005025625273,0.921862343753855,
8.8599848982295));
#395408=CARTESIAN_POINT('Ctrl Pts',(-2.50001257343146,0.922206507017019,
8.85968173251461));
#395409=CARTESIAN_POINT('Ctrl Pts',(-2.49999264137797,0.922388549665028,
8.85952137522076));
#395410=CARTESIAN_POINT('Ctrl Pts',(-2.49998085334338,0.922563898491426,
8.85934740853961));
#395411=CARTESIAN_POINT('Ctrl Pts',(-2.49997582451368,0.922729976418867,
8.8591675900182));
#395412=CARTESIAN_POINT('Ctrl Pts',(-2.49995563114851,0.923396865623127,
8.85844552518696));
#395413=CARTESIAN_POINT('Ctrl Pts',(-2.50004026010221,0.923951866608739,
8.85759444184126));
#395414=CARTESIAN_POINT('Ctrl Pts',(-2.50014990752215,0.924398186783963,
8.85683498915141));
#395415=CARTESIAN_POINT('Ctrl Pts',(-2.50016138183263,0.924444893001657,
8.85675551445));
#395416=CARTESIAN_POINT('Ctrl Pts',(-2.50017314820602,0.924490400580325,
8.85667699793652));
#395417=CARTESIAN_POINT('Ctrl Pts',(-2.50018512677841,0.92453470701937,
8.85659965593547));
#395418=CARTESIAN_POINT('Ctrl Pts',(-2.50034681415975,0.925132757594396,
8.85555568965886));
#395419=CARTESIAN_POINT('Ctrl Pts',(-2.50058857608735,0.925684170392119,
8.85434650606345));
#395420=CARTESIAN_POINT('Ctrl Pts',(-2.5009059159866,0.926194166764285,
8.85297329937116));
#395421=CARTESIAN_POINT('Ctrl Pts',(-2.50108440034412,0.926481008649092,
8.85220095427747));
#395422=CARTESIAN_POINT('Ctrl Pts',(-2.50128713331755,0.926754699673022,
8.85137579139183));
#395423=CARTESIAN_POINT('Ctrl Pts',(-2.50151564461753,0.927015373804532,
8.85049129520029));
#395424=CARTESIAN_POINT('Origin',(-2.5066854651563,0.922483422723941,7.59394543036555));
#395425=CARTESIAN_POINT('Ctrl Pts',(-2.50513036619197,0.915763048196833,
7.59443877723642));
#395426=CARTESIAN_POINT('Ctrl Pts',(-2.49940101777127,0.916604333120594,
7.58783886950016));
#395427=CARTESIAN_POINT('Ctrl Pts',(-2.49865736261563,0.925061647029049,
7.58559994247159));
#395428=CARTESIAN_POINT('Ctrl Pts',(-2.5364067111286,0.911170498480271,
7.56670252222134));
#395429=CARTESIAN_POINT('Ctrl Pts',(-2.53068564324298,0.912010567508487,
7.56004874999028));
#395430=CARTESIAN_POINT('Ctrl Pts',(-2.52991629821513,0.920516122486533,
7.55786368756704));
#395431=CARTESIAN_POINT('Ctrl Pts',(-2.56762465061597,0.906586524891448,
7.53888913333557));
#395432=CARTESIAN_POINT('Ctrl Pts',(-2.5618695821438,0.907431586491008,
7.53222002137279));
#395433=CARTESIAN_POINT('Ctrl Pts',(-2.56111780051421,0.915977770967222,
7.53005029815326));
#395434=CARTESIAN_POINT('Ctrl Pts',(-2.59878277202118,0.902011334858278,
7.51101258149734));
#395435=CARTESIAN_POINT('Ctrl Pts',(-2.59295794166188,0.902866640139947,
7.5043616886572));
#395436=CARTESIAN_POINT('Ctrl Pts',(-2.59226033981814,0.911446898481761,
7.50217374673251));
#395437=CARTESIAN_POINT('',(-2.59059853376832,0.911688670640849,7.50366116523517));
#395438=CARTESIAN_POINT('Ctrl Pts',(-2.59029443537466,0.903257743546346,
7.51860402984325));
#395439=CARTESIAN_POINT('Ctrl Pts',(-2.59073136135582,0.903193586296034,
7.51734760759493));
#395440=CARTESIAN_POINT('Ctrl Pts',(-2.59113483014927,0.903194476627547,
7.51608817408572));
#395441=CARTESIAN_POINT('Ctrl Pts',(-2.59150388429384,0.903273766104983,
7.51481005913119));
#395442=CARTESIAN_POINT('Ctrl Pts',(-2.59183818235682,0.903345588408327,
7.51365231206383));
#395443=CARTESIAN_POINT('Ctrl Pts',(-2.59214476638707,0.903481595190344,
7.51247773061042));
#395444=CARTESIAN_POINT('Ctrl Pts',(-2.59240335794634,0.903713185892332,
7.51129758471022));
#395445=CARTESIAN_POINT('Ctrl Pts',(-2.59272475772224,0.904001026686246,
7.50983079813402));
#395446=CARTESIAN_POINT('Ctrl Pts',(-2.59295307372471,0.904437038238365,
7.50839324291155));
#395447=CARTESIAN_POINT('Ctrl Pts',(-2.59301693980262,0.905062645938782,
7.50715379678855));
#395448=CARTESIAN_POINT('Ctrl Pts',(-2.59304644409036,0.905351658669921,
7.50658120839351));
#395449=CARTESIAN_POINT('Ctrl Pts',(-2.59303559361285,0.905723185272621,
7.50598221009429));
#395450=CARTESIAN_POINT('Ctrl Pts',(-2.59296190979915,0.906167719907874,
7.50545747549611));
#395451=CARTESIAN_POINT('Ctrl Pts',(-2.59292258983543,0.906404937348878,
7.50517746087247));
#395452=CARTESIAN_POINT('Ctrl Pts',(-2.59286515073088,0.906665550100618,
7.50491486231392));
#395453=CARTESIAN_POINT('Ctrl Pts',(-2.59278948464782,0.906942297683577,
7.50468370960993));
#395454=CARTESIAN_POINT('Ctrl Pts',(-2.59267633998614,0.907356122615175,
7.50433806340447));
#395455=CARTESIAN_POINT('Ctrl Pts',(-2.59251851063052,0.907818286743171,
7.50405484070984));
#395456=CARTESIAN_POINT('Ctrl Pts',(-2.59232594814198,0.908297432651606,
7.50385766036131));
#395457=CARTESIAN_POINT('Ctrl Pts',(-2.59230535657693,0.908348669858901,
7.50383657498791));
#395458=CARTESIAN_POINT('Ctrl Pts',(-2.59228439032879,0.90840008397143,
7.50381643264937));
#395459=CARTESIAN_POINT('Ctrl Pts',(-2.59226307810043,0.908451624345678,
7.50379723213559));
#395460=CARTESIAN_POINT('Ctrl Pts',(-2.59212081200435,0.908795673203805,
7.50366906242519));
#395461=CARTESIAN_POINT('Ctrl Pts',(-2.59195936993193,0.909152557376872,
7.50358235568538));
#395462=CARTESIAN_POINT('Ctrl Pts',(-2.59179549077372,0.909492809245847,
7.5035341175365));
#395463=CARTESIAN_POINT('Ctrl Pts',(-2.59154977252353,0.910002978414299,
7.50346178989176));
#395464=CARTESIAN_POINT('Ctrl Pts',(-2.59126374379866,0.910541356689525,
7.50346967198527));
#395465=CARTESIAN_POINT('Ctrl Pts',(-2.59096668961309,0.911061237388423,
7.50354272648692));
#395466=CARTESIAN_POINT('Ctrl Pts',(-2.59084450507791,0.911275075080774,
7.50357277531559));
#395467=CARTESIAN_POINT('Ctrl Pts',(-2.59072074066281,0.911485569493069,
7.50361331098761));
#395468=CARTESIAN_POINT('Ctrl Pts',(-2.59059853376966,0.91168867064132,
7.50366116523659));
#395469=CARTESIAN_POINT('',(-2.50943323048223,0.923494625764158,7.57603338622103));
#395470=CARTESIAN_POINT('Origin',(-2.51772543279346,0.926549273114053,7.58486873427626));
#395471=CARTESIAN_POINT('Ctrl Pts',(-2.59059853382405,0.911688670627326,
7.50366116529969));
#395472=CARTESIAN_POINT('Ctrl Pts',(-2.56358770138599,0.915618394511231,
7.52783573079709));
#395473=CARTESIAN_POINT('Ctrl Pts',(-2.53653388028073,0.919553544813599,
7.55196141284068));
#395474=CARTESIAN_POINT('Ctrl Pts',(-2.5094332316199,0.923494625241324,
7.57603338728831));
#395475=CARTESIAN_POINT('Ctrl Pts',(-2.50672970590163,0.915705906336666,
7.5963967733137));
#395476=CARTESIAN_POINT('Ctrl Pts',(-2.48759500061638,0.915457955302635,
7.59974925422226));
#395477=CARTESIAN_POINT('Ctrl Pts',(-2.502325773521,0.927672813292059,7.59639677331373));
#395478=CARTESIAN_POINT('Ctrl Pts',(-2.50288821974749,0.915029084195064,
7.58707626057421));
#395479=CARTESIAN_POINT('Ctrl Pts',(-2.49726541951563,0.919016758850096,
7.58811717123965));
#395480=CARTESIAN_POINT('Ctrl Pts',(-2.49896195408413,0.925698016370938,
7.58707626057425));
#395481=CARTESIAN_POINT('Ctrl Pts',(-2.5063100950153,0.920050677758216,
7.58015376756929));
#395482=CARTESIAN_POINT('Ctrl Pts',(-2.50375153300591,0.921403708571725,
7.58208760766041));
#395483=CARTESIAN_POINT('Ctrl Pts',(-2.50482266671417,0.924092500961744,
7.58015376756931));
#395484=CARTESIAN_POINT('Ctrl Pts',(-2.50943322970565,0.923494625478152,
7.57603338509286));
#395485=CARTESIAN_POINT('Ctrl Pts',(-2.50943322970565,0.923494625478151,
7.57603338509286));
#395486=CARTESIAN_POINT('Ctrl Pts',(-2.50943322970565,0.923494625478151,
7.57603338509286));
#395487=CARTESIAN_POINT('Origin',(-2.51772740356828,0.926543917882751,7.58486873427622));
#395488=CARTESIAN_POINT('Ctrl Pts',(-2.56355987305573,0.997792291028113,
7.51098857897448));
#395489=CARTESIAN_POINT('Ctrl Pts',(-2.55967899499225,0.993365181651979,
7.50433767179956));
#395490=CARTESIAN_POINT('Ctrl Pts',(-2.56470980820181,0.986379555729206,
7.50214974420965));
#395491=CARTESIAN_POINT('Ctrl Pts',(-2.54279444458098,0.974104140667222,
7.53887321589168));
#395492=CARTESIAN_POINT('Ctrl Pts',(-2.53896006632403,0.969730075918122,
7.53220407452065));
#395493=CARTESIAN_POINT('Ctrl Pts',(-2.54392751200518,0.962735263316863,
7.53003438070911));
#395494=CARTESIAN_POINT('Ctrl Pts',(-2.52198913882351,0.950370500319441,
7.56669465659234));
#395495=CARTESIAN_POINT('Ctrl Pts',(-2.51817742102916,0.9460222854798,7.56004085833302));
#395496=CARTESIAN_POINT('Ctrl Pts',(-2.52310514388124,0.939047029382759,
7.55785582193789));
#395497=CARTESIAN_POINT('Ctrl Pts',(-2.501144896724,0.926592443362311,7.59443891967696));
#395498=CARTESIAN_POINT('Ctrl Pts',(-2.49732765241344,0.922237924152511,
7.58783901202978));
#395499=CARTESIAN_POINT('Ctrl Pts',(-2.50224367002345,0.915316078383761,
7.58560008491213));
#395500=CARTESIAN_POINT('',(-2.56358326728471,0.985097876880933,7.50366116523517));
#395501=CARTESIAN_POINT('Ctrl Pts',(-2.56358326728506,0.985097876881066,
7.50366116523554));
#395502=CARTESIAN_POINT('Ctrl Pts',(-2.56345970006383,0.985845452066986,
7.50350835821027));
#395503=CARTESIAN_POINT('Ctrl Pts',(-2.56332179021806,0.98652863497484,
7.50345484956));
#395504=CARTESIAN_POINT('Ctrl Pts',(-2.56316602620426,0.987167856010466,
7.50349758195598));
#395505=CARTESIAN_POINT('Ctrl Pts',(-2.56308610771343,0.987495823807609,
7.50351950684424));
#395506=CARTESIAN_POINT('Ctrl Pts',(-2.56299373787712,0.987844575329019,
7.50357029184312));
#395507=CARTESIAN_POINT('Ctrl Pts',(-2.56289542256784,0.98817842402356,
7.50365515313923));
#395508=CARTESIAN_POINT('Ctrl Pts',(-2.56274417381036,0.98869201850445,
7.50378570417639));
#395509=CARTESIAN_POINT('Ctrl Pts',(-2.56257474719318,0.989185516731555,
7.50400001621911));
#395510=CARTESIAN_POINT('Ctrl Pts',(-2.5623978911558,0.989620619087741,
7.50428903009634));
#395511=CARTESIAN_POINT('Ctrl Pts',(-2.56237826149629,0.989668912101802,
7.50432110841318));
#395512=CARTESIAN_POINT('Ctrl Pts',(-2.56235854685538,0.989716515320739,
7.50435406373354));
#395513=CARTESIAN_POINT('Ctrl Pts',(-2.56233876646287,0.989763398289759,
7.50438785222352));
#395514=CARTESIAN_POINT('Ctrl Pts',(-2.56221799765893,0.990049641350433,
7.50459414719561));
#395515=CARTESIAN_POINT('Ctrl Pts',(-2.56209237988989,0.990313392525865,
7.50483629897752));
#395516=CARTESIAN_POINT('Ctrl Pts',(-2.56196791368994,0.990545113473018,
7.5050991045531));
#395517=CARTESIAN_POINT('Ctrl Pts',(-2.56169332875141,0.991056313156602,
7.50567888004914));
#395518=CARTESIAN_POINT('Ctrl Pts',(-2.56141398648965,0.991432015973551,
7.50637912803144));
#395519=CARTESIAN_POINT('Ctrl Pts',(-2.56114901670265,0.991696500910359,
7.50710440483569));
#395520=CARTESIAN_POINT('Ctrl Pts',(-2.56108404085049,0.991761357867625,
7.50728225710685));
#395521=CARTESIAN_POINT('Ctrl Pts',(-2.56101873889053,0.99182092138565,
7.50746498566954));
#395522=CARTESIAN_POINT('Ctrl Pts',(-2.56095491592359,0.991874108847984,
7.50764697238949));
#395523=CARTESIAN_POINT('Ctrl Pts',(-2.56061182121787,0.992160030007908,
7.50862528291182));
#395524=CARTESIAN_POINT('Ctrl Pts',(-2.56028297152453,0.992290828132535,
7.50965856837421));
#395525=CARTESIAN_POINT('Ctrl Pts',(-2.55997541446453,0.992332425349267,
7.51067959873202));
#395526=CARTESIAN_POINT('Ctrl Pts',(-2.55980616542648,0.992355316350103,
7.51124147302578));
#395527=CARTESIAN_POINT('Ctrl Pts',(-2.55964326493997,0.992350769606349,
7.51180065547253));
#395528=CARTESIAN_POINT('Ctrl Pts',(-2.55948762194073,0.992327067952742,
7.51235175716501));
#395529=CARTESIAN_POINT('Ctrl Pts',(-2.55894981337754,0.992245169297914,
7.51425603304536));
#395530=CARTESIAN_POINT('Ctrl Pts',(-2.55843544700615,0.991918804986669,
7.51626900505181));
#395531=CARTESIAN_POINT('Ctrl Pts',(-2.55796290178256,0.991405463116667,
7.51827788969244));
#395532=CARTESIAN_POINT('Ctrl Pts',(-2.55793732674207,0.991377680084582,
7.51838661432546));
#395533=CARTESIAN_POINT('Ctrl Pts',(-2.557911873988,0.991349339402192,7.51849533314857));
#395534=CARTESIAN_POINT('Ctrl Pts',(-2.55788654645048,0.991320447028609,
7.51860402984325));
#395535=CARTESIAN_POINT('Ctrl Pts',(-2.50943323101062,0.923494626900376,
7.57603338728985));
#395536=CARTESIAN_POINT('Ctrl Pts',(-2.52751419016524,0.944062956661482,
7.55196141284922));
#395537=CARTESIAN_POINT('Ctrl Pts',(-2.54556333675352,0.964596416013609,
7.52783573083105));
#395538=CARTESIAN_POINT('Ctrl Pts',(-2.56358326731953,0.985097876928784,
7.50366116530176));
#395539=CARTESIAN_POINT('Origin',(-8.67125181207506E-16,3.19110082301667E-16,
7.49482233047033));
#395540=CARTESIAN_POINT('Origin',(-2.58226093460097,0.908754485894685,7.49482233047033));
#395541=CARTESIAN_POINT('Origin',(0.,0.,7.50366116523517));
#395542=CARTESIAN_POINT('Origin',(-2.55533261422669,0.981927431468037,7.49482233047033));
#395543=CARTESIAN_POINT('Ctrl Pts',(-2.59029338886968,0.903257897167606,
7.51860402984325));
#395544=CARTESIAN_POINT('Ctrl Pts',(-2.59782171669849,0.902153104819671,
7.51860402984325));
#395545=CARTESIAN_POINT('Ctrl Pts',(-2.60029797237973,0.894958353689076,
7.51860402984325));
#395546=CARTESIAN_POINT('Ctrl Pts',(-2.59308870818399,0.902847678972059,
7.51041458714366));
#395547=CARTESIAN_POINT('Ctrl Pts',(-2.59840836067141,0.90044858264775,
7.51004642900443));
#395548=CARTESIAN_POINT('Ctrl Pts',(-2.60029865530165,0.894956369462144,
7.5072913648301));
#395549=CARTESIAN_POINT('Ctrl Pts',(-2.59443309621022,0.905320806149179,
7.50215815450137));
#395550=CARTESIAN_POINT('Ctrl Pts',(-2.59721402775987,0.903919205564972,
7.49877163671529));
#395551=CARTESIAN_POINT('Ctrl Pts',(-2.59835939116489,0.900664660087521,
7.4948158853317));
#395552=CARTESIAN_POINT('Ctrl Pts',(-2.5905980144691,0.911688487888521,
7.50366171572174));
#395553=CARTESIAN_POINT('Ctrl Pts',(-2.59405208042094,0.912904049757583,
7.50000045605858));
#395554=CARTESIAN_POINT('Ctrl Pts',(-2.59405208042098,0.912904049757465,
7.49482233047317));
#395555=CARTESIAN_POINT('Origin',(-2.58847843614164,0.890890361172308,7.51860402984325));
#395556=CARTESIAN_POINT('Origin',(-2.58847843614164,0.890890361172308,9.));
#395557=CARTESIAN_POINT('Origin',(-2.58847843614164,0.890890361172308,8.75721825406948));
#395558=CARTESIAN_POINT('Ctrl Pts',(-2.57377144873504,0.905683912037591,
8.78942910404912));
#395559=CARTESIAN_POINT('Ctrl Pts',(-2.57928769835754,0.904894343291997,
8.79672699501691));
#395560=CARTESIAN_POINT('Ctrl Pts',(-2.57966709350247,0.895976409377347,
8.79893251111267));
#395561=CARTESIAN_POINT('Ctrl Pts',(-2.58464914173359,0.904086660094499,
8.78111911759583));
#395562=CARTESIAN_POINT('Ctrl Pts',(-2.59118766485554,0.903143248461625,
8.78644465894812));
#395563=CARTESIAN_POINT('Ctrl Pts',(-2.593261215509,0.895306418779735,8.78817647674132));
#395564=CARTESIAN_POINT('Ctrl Pts',(-2.59142837946314,0.903091214554023,
8.76780923932029));
#395565=CARTESIAN_POINT('Ctrl Pts',(-2.59914610221573,0.901972513394419,
8.76988516158374));
#395566=CARTESIAN_POINT('Ctrl Pts',(-2.60175132061197,0.894876795142954,
8.77093053738833));
#395567=CARTESIAN_POINT('Ctrl Pts',(-2.59010652088601,0.90328531280907,
8.75371302330492));
#395568=CARTESIAN_POINT('Ctrl Pts',(-2.59763493587647,0.902194822506885,
8.75300828287559));
#395569=CARTESIAN_POINT('Ctrl Pts',(-2.60009538217394,0.89496013223352,
8.75267964240738));
#395570=CARTESIAN_POINT('Origin',(-2.57460462632379,0.892927560898673,8.78727029226991));
#395571=CARTESIAN_POINT('Ctrl Pts',(-2.50568666557814,0.91568136241822,
8.85049129520029));
#395572=CARTESIAN_POINT('Ctrl Pts',(-2.51146432645974,0.914832983398935,
8.85711686593484));
#395573=CARTESIAN_POINT('Ctrl Pts',(-2.51218498036397,0.90631351040677,
8.85933012996512));
#395574=CARTESIAN_POINT('Ctrl Pts',(-2.52929895681326,0.912214185494608,
8.82945683644725));
#395575=CARTESIAN_POINT('Ctrl Pts',(-2.5351245757734,0.911358764416525,
8.8360746990239));
#395576=CARTESIAN_POINT('Ctrl Pts',(-2.5358099765306,0.90281111747134,8.83829567148519));
#395577=CARTESIAN_POINT('Ctrl Pts',(-2.55287605202415,0.9087521766778,8.80838214965001));
#395578=CARTESIAN_POINT('Ctrl Pts',(-2.5587246615967,0.907893379708743,
8.81501364461994));
#395579=CARTESIAN_POINT('Ctrl Pts',(-2.55939923284053,0.899314698794289,
8.81722098428721));
#395580=CARTESIAN_POINT('Ctrl Pts',(-2.57642062555681,0.905294943272712,
8.78727029226991));
#395581=CARTESIAN_POINT('Ctrl Pts',(-2.58227020660257,0.904436003654666,
8.79393457792714));
#395582=CARTESIAN_POINT('Ctrl Pts',(-2.58295547781501,0.895823813541599,
8.79610912703474));
#395583=CARTESIAN_POINT('Origin',(-2.50387066634512,0.903313980044182,8.85049129520029));
#395584=CARTESIAN_POINT('Ctrl Pts',(-2.50151564461753,0.927015373804532,
8.85049129520029));
#395585=CARTESIAN_POINT('Ctrl Pts',(-2.50536507777436,0.931406612421841,
8.85711686593484));
#395586=CARTESIAN_POINT('Ctrl Pts',(-2.50039125247054,0.93836087902307,
8.85933012996512));
#395587=CARTESIAN_POINT('Ctrl Pts',(-2.49811010667082,0.923130508387991,
8.86332496987231));
#395588=CARTESIAN_POINT('Ctrl Pts',(-2.49678212912387,0.927556383444011,
8.86648636486738));
#395589=CARTESIAN_POINT('Ctrl Pts',(-2.4908770045068,0.927481515896442,
8.87206031107457));
#395590=CARTESIAN_POINT('Ctrl Pts',(-2.50054051873363,0.916437011304943,
8.86341338519877));
#395591=CARTESIAN_POINT('Ctrl Pts',(-2.5023764487842,0.912182269070248,
8.86654584966059));
#395592=CARTESIAN_POINT('Ctrl Pts',(-2.49777763608561,0.908443943970601,
8.87215952290714));
#395593=CARTESIAN_POINT('Ctrl Pts',(-2.50568666557814,0.91568136241822,
8.85049129520029));
#395594=CARTESIAN_POINT('Ctrl Pts',(-2.51146432645974,0.914832983398934,
8.85711686593484));
#395595=CARTESIAN_POINT('Ctrl Pts',(-2.51218498036396,0.90631351040677,
8.85933012996512));
#395596=CARTESIAN_POINT('Origin',(-2.49211597091066,0.93525528486015,8.85049129520029));
#395597=CARTESIAN_POINT('Ctrl Pts',(-2.54864296074704,0.980775832055543,
8.78727029226991));
#395598=CARTESIAN_POINT('Ctrl Pts',(-2.55254031154222,0.985221732690706,
8.79393457792714));
#395599=CARTESIAN_POINT('Ctrl Pts',(-2.54747944236023,0.992223662303395,
8.79610912703474));
#395600=CARTESIAN_POINT('Ctrl Pts',(-2.53295611725146,0.962881074532825,
8.80838214965002));
#395601=CARTESIAN_POINT('Ctrl Pts',(-2.53685282079141,0.967326236811945,
8.81501364461993));
#395602=CARTESIAN_POINT('Ctrl Pts',(-2.53180552577562,0.974295714957313,
8.81722098428721));
#395603=CARTESIAN_POINT('Ctrl Pts',(-2.51724760581289,0.944961599316835,
8.82945683644723));
#395604=CARTESIAN_POINT('Ctrl Pts',(-2.52112899159234,0.94938928786966,
8.8360746990239));
#395605=CARTESIAN_POINT('Ctrl Pts',(-2.51611005976584,0.956342155322624,
8.83829567148519));
#395606=CARTESIAN_POINT('Ctrl Pts',(-2.50151564461753,0.927015373804532,
8.85049129520029));
#395607=CARTESIAN_POINT('Ctrl Pts',(-2.50536507777436,0.931406612421841,
8.85711686593484));
#395608=CARTESIAN_POINT('Ctrl Pts',(-2.50039125247054,0.93836087902307,
8.85933012996512));
#395609=CARTESIAN_POINT('Origin',(-2.53924328704018,0.989015743111162,8.78727029226991));
#395610=CARTESIAN_POINT('Ctrl Pts',(-2.55776447567946,0.991181222852442,
8.75374538247848));
#395611=CARTESIAN_POINT('Ctrl Pts',(-2.56278352445774,0.996886792740612,
8.75304829418602));
#395612=CARTESIAN_POINT('Ctrl Pts',(-2.55997553412122,1.00398509066891,
8.75272238421917));
#395613=CARTESIAN_POINT('Ctrl Pts',(-2.55863459984932,0.99217381584208,
8.76769408445019));
#395614=CARTESIAN_POINT('Ctrl Pts',(-2.56377943200827,0.998023418993422,
8.76974318093969));
#395615=CARTESIAN_POINT('Ctrl Pts',(-2.56116930682118,1.00510901027348,
8.7707786988043));
#395616=CARTESIAN_POINT('Ctrl Pts',(-2.55417483904275,0.987086349610347,
8.78108014887992));
#395617=CARTESIAN_POINT('Ctrl Pts',(-2.55853775190122,0.992041168344635,
8.78639403366325));
#395618=CARTESIAN_POINT('Ctrl Pts',(-2.55505961340922,0.999350383648577,
8.78812224174741));
#395619=CARTESIAN_POINT('Ctrl Pts',(-2.54686627555659,0.978749115549326,
8.78944554828685));
#395620=CARTESIAN_POINT('Ctrl Pts',(-2.55054737792007,0.982921153781,8.79673892988686));
#395621=CARTESIAN_POINT('Ctrl Pts',(-2.54506331635741,0.989951703054951,
8.79894799272499));
#395622=CARTESIAN_POINT('Origin',(-2.54848687274362,0.999560358084225,8.75721825406948));
#395623=CARTESIAN_POINT('Origin',(-2.54848687274362,0.999560358084225,9.));
#395624=CARTESIAN_POINT('Origin',(-2.54848687274362,0.999560358084225,7.51860402984325));
#395625=CARTESIAN_POINT('Ctrl Pts',(-2.5635825329696,0.985097594708666,
7.50366195182966));
#395626=CARTESIAN_POINT('Ctrl Pts',(-2.56700079967973,0.986411118369848,
7.50000065167735));
#395627=CARTESIAN_POINT('Ctrl Pts',(-2.56700079967969,0.986411118369957,
7.49482233047108));
#395628=CARTESIAN_POINT('Ctrl Pts',(-2.56237307191841,0.99243864392334,
7.50215800491336));
#395629=CARTESIAN_POINT('Ctrl Pts',(-2.56358120883208,0.995310072552473,
7.49877273257264));
#395630=CARTESIAN_POINT('Ctrl Pts',(-2.56234297166959,0.998532482377338,
7.49481816995647));
#395631=CARTESIAN_POINT('Ctrl Pts',(-2.55974479284784,0.993439726072497,
7.51043025814042));
#395632=CARTESIAN_POINT('Ctrl Pts',(-2.56224502626245,0.998716239112324,
7.51006209594515));
#395633=CARTESIAN_POINT('Ctrl Pts',(-2.56012287462731,1.00412691768342,
7.50731281821699));
#395634=CARTESIAN_POINT('Ctrl Pts',(-2.55788555007274,0.9913193105499,7.51860402984325));
#395635=CARTESIAN_POINT('Ctrl Pts',(-2.56290221972396,0.997040677781703,
7.51860402984324));
#395636=CARTESIAN_POINT('Ctrl Pts',(-2.56012379910318,1.00412456063256,
7.51860402984325));
#395637=CARTESIAN_POINT('Origin',(0.,0.,7.5));
#395638=CARTESIAN_POINT('Origin',(-2.55577009136411,0.764838063661123,7.5));
#395639=CARTESIAN_POINT('',(-2.55577009136411,0.764838063661123,7.59394543036555));
#395640=CARTESIAN_POINT('',(-2.55577009136411,0.764838063661123,8.85049129520029));
#395641=CARTESIAN_POINT('',(-2.55577009136411,0.764838063661123,7.5));
#395642=CARTESIAN_POINT('',(-2.60624502375465,0.815468607773348,8.78727029226991));
#395643=CARTESIAN_POINT('Ctrl Pts',(-2.55577009136411,0.764838063661123,
8.85049129520029));
#395644=CARTESIAN_POINT('Ctrl Pts',(-2.57261952556177,0.781739443831588,
8.82945686509571));
#395645=CARTESIAN_POINT('Ctrl Pts',(-2.5894439110381,0.798615698056739,
8.80838212259895));
#395646=CARTESIAN_POINT('Ctrl Pts',(-2.60624502375465,0.815468607773348,
8.78727029226991));
#395647=CARTESIAN_POINT('',(-2.61614521332083,0.825399319134613,8.75721825406948));
#395648=CARTESIAN_POINT('Origin',(-2.58635225143102,0.795514221183931,8.75937679713083));
#395649=CARTESIAN_POINT('',(-2.61614521332083,0.825399319134613,7.51860402984325));
#395650=CARTESIAN_POINT('',(-2.61614521332083,0.825399319134613,7.5));
#395651=CARTESIAN_POINT('Ctrl Pts',(-2.61614521332083,0.825399319134613,
7.51860402984325));
#395652=CARTESIAN_POINT('Ctrl Pts',(-2.60837015418732,0.817600289878103,
7.52834476460825));
#395653=CARTESIAN_POINT('Ctrl Pts',(-2.60059004759763,0.809796197604334,
7.53807742314407));
#395654=CARTESIAN_POINT('Ctrl Pts',(-2.59280472407667,0.801986872315774,
7.54780169004674));
#395655=CARTESIAN_POINT('Ctrl Pts',(-2.58047319238031,0.789617323116712,
7.5632044032688));
#395656=CARTESIAN_POINT('Ctrl Pts',(-2.56812855639631,0.777234629230163,
7.57858609112103));
#395657=CARTESIAN_POINT('Ctrl Pts',(-2.55577009136411,0.764838063661123,
7.59394543036555));
#395658=CARTESIAN_POINT('Origin',(-2.82817002729664,0.695957823489687,7.5));
#395659=CARTESIAN_POINT('',(-2.64284431997727,0.73544116934887,8.75721825406948));
#395660=CARTESIAN_POINT('',(-2.62912953922427,0.738363081476909,8.78727029226991));
#395661=CARTESIAN_POINT('Origin',(-2.59431631031274,0.745779984277226,8.75658640620964));
#395662=CARTESIAN_POINT('',(-2.55920636991203,0.753260100986283,8.85049129520029));
#395663=CARTESIAN_POINT('Ctrl Pts',(-2.62912953922427,0.738363081476909,
8.78727029226991));
#395664=CARTESIAN_POINT('Ctrl Pts',(-2.60585487607022,0.743321711277163,
8.80838212259895));
#395665=CARTESIAN_POINT('Ctrl Pts',(-2.58254797304887,0.74828720972964,
8.82945686509571));
#395666=CARTESIAN_POINT('Ctrl Pts',(-2.55920636991203,0.753260100986283,
8.85049129520029));
#395667=CARTESIAN_POINT('',(-2.55920636991203,0.753260100986283,7.59394543036555));
#395668=CARTESIAN_POINT('',(-2.55920636991203,0.753260100986283,7.5));
#395669=CARTESIAN_POINT('',(-2.64284431997727,0.73544116934887,7.51860402984325));
#395670=CARTESIAN_POINT('Ctrl Pts',(-2.55920636991203,0.753260100986283,
7.59394543036555));
#395671=CARTESIAN_POINT('Ctrl Pts',(-2.5763266116233,0.749612660841815,
7.57858609112103));
#395672=CARTESIAN_POINT('Ctrl Pts',(-2.59342769588662,0.745969302161038,
7.56320440326857));
#395673=CARTESIAN_POINT('Ctrl Pts',(-2.61051062671677,0.742329811040179,
7.54780169004651));
#395674=CARTESIAN_POINT('Ctrl Pts',(-2.62129567325223,0.740032074106501,
7.53807742314383));
#395675=CARTESIAN_POINT('Ctrl Pts',(-2.63207349274766,0.737735876882151,
7.52834476460825));
#395676=CARTESIAN_POINT('Ctrl Pts',(-2.64284431997727,0.73544116934887,
7.51860402984325));
#395677=CARTESIAN_POINT('',(-2.64284431997727,0.73544116934887,7.5));
#395678=CARTESIAN_POINT('Origin',(-2.56063892684945,0.759984192420898,7.5));
#395679=CARTESIAN_POINT('Ctrl Pts',(-2.55920636991203,0.753260100986283,
8.85049129520029));
#395680=CARTESIAN_POINT('Ctrl Pts',(-2.55901695934139,0.753300454605746,
8.85097269580138));
#395681=CARTESIAN_POINT('Ctrl Pts',(-2.5588316912378,0.753348525868755,
8.85143669361005));
#395682=CARTESIAN_POINT('Ctrl Pts',(-2.55864225418248,0.753407374564274,
8.8519052845931));
#395683=CARTESIAN_POINT('Ctrl Pts',(-2.55827172731594,0.753522478880658,
8.85282181883899));
#395684=CARTESIAN_POINT('Ctrl Pts',(-2.55789484136047,0.75367604126955,
8.85372622499635));
#395685=CARTESIAN_POINT('Ctrl Pts',(-2.55751150029901,0.753884750349144,
8.8546225773507));
#395686=CARTESIAN_POINT('Ctrl Pts',(-2.55719326416477,0.754058013214378,
8.85536669723986));
#395687=CARTESIAN_POINT('Ctrl Pts',(-2.55687049166869,0.754269293443464,
8.85610498449051));
#395688=CARTESIAN_POINT('Ctrl Pts',(-2.55654748330546,0.754534852746864,
8.85681338218371));
#395689=CARTESIAN_POINT('Ctrl Pts',(-2.55625435270854,0.754775848231767,
8.85745625420284));
#395690=CARTESIAN_POINT('Ctrl Pts',(-2.55595697075631,0.755064106475237,
8.85808743050666));
#395691=CARTESIAN_POINT('Ctrl Pts',(-2.55566442701757,0.75542674252638,
8.8586680450841));
#395692=CARTESIAN_POINT('Ctrl Pts',(-2.55552945367808,0.755594054939391,
8.85893592806395));
#395693=CARTESIAN_POINT('Ctrl Pts',(-2.55539561415247,0.755777419117959,
8.85919241173848));
#395694=CARTESIAN_POINT('Ctrl Pts',(-2.5552646800958,0.755980830461287,
8.85943017985535));
#395695=CARTESIAN_POINT('Ctrl Pts',(-2.55508788035867,0.756255495990983,
8.85975123720001));
#395696=CARTESIAN_POINT('Ctrl Pts',(-2.55491241676131,0.756574051157857,
8.86004599534706));
#395697=CARTESIAN_POINT('Ctrl Pts',(-2.55474952017824,0.756937693547207,
8.86026130871721));
#395698=CARTESIAN_POINT('Ctrl Pts',(-2.55468987914663,0.757070833278112,
8.86034014101236));
#395699=CARTESIAN_POINT('Ctrl Pts',(-2.55463101560014,0.757212011809917,
8.86040910639693));
#395700=CARTESIAN_POINT('Ctrl Pts',(-2.55457484371586,0.757357512262571,
8.86046313645507));
#395701=CARTESIAN_POINT('Ctrl Pts',(-2.55448718796089,0.75758456450038,
8.8605474499083));
#395702=CARTESIAN_POINT('Ctrl Pts',(-2.55440383119924,0.757828391994662,
8.86059655985668));
#395703=CARTESIAN_POINT('Ctrl Pts',(-2.55432984214789,0.758073262578132,
8.86059725258816));
#395704=CARTESIAN_POINT('Ctrl Pts',(-2.55425568215228,0.758318698910477,
8.86059794692011));
#395705=CARTESIAN_POINT('Ctrl Pts',(-2.55419265397134,0.75856867351899,
8.86056369958366));
#395706=CARTESIAN_POINT('Ctrl Pts',(-2.55414054629406,0.758808632639973,
8.86048590497774));
#395707=CARTESIAN_POINT('Ctrl Pts',(-2.55412694774172,0.758871254826106,
8.86046560290182));
#395708=CARTESIAN_POINT('Ctrl Pts',(-2.55411400454187,0.758934028803233,
8.8604425750309));
#395709=CARTESIAN_POINT('Ctrl Pts',(-2.55410208450021,0.758995008174594,
8.86041778462583));
#395710=CARTESIAN_POINT('Ctrl Pts',(-2.5540218774114,0.759405323674763,
8.860250975962));
#395711=CARTESIAN_POINT('Ctrl Pts',(-2.55397755802796,0.759789508818236,
8.8599848982295));
#395712=CARTESIAN_POINT('Ctrl Pts',(-2.55396200324606,0.760135379307712,
8.85968173251461));
#395713=CARTESIAN_POINT('Ctrl Pts',(-2.55395377565762,0.760318324980629,
8.85952137522076));
#395714=CARTESIAN_POINT('Ctrl Pts',(-2.55395324648069,0.760494068796026,
8.85934740853961));
#395715=CARTESIAN_POINT('Ctrl Pts',(-2.55395886863261,0.760660127696779,
8.8591675900182));
#395716=CARTESIAN_POINT('Ctrl Pts',(-2.55398144449489,0.761326940499001,
8.85844552518695));
#395717=CARTESIAN_POINT('Ctrl Pts',(-2.55410145860457,0.761875378979888,
8.85759444184124));
#395718=CARTESIAN_POINT('Ctrl Pts',(-2.55423947657393,0.762313757008131,
8.85683498915138));
#395719=CARTESIAN_POINT('Ctrl Pts',(-2.55425391978686,0.76235963210129,
8.85675551444998));
#395720=CARTESIAN_POINT('Ctrl Pts',(-2.55426857766554,0.76240429230562,
8.85667699793651));
#395721=CARTESIAN_POINT('Ctrl Pts',(-2.55428337034997,0.762447740242562,
8.85659965593547));
#395722=CARTESIAN_POINT('Ctrl Pts',(-2.55448304275914,0.76303420271245,
8.85555568965886));
#395723=CARTESIAN_POINT('Ctrl Pts',(-2.55475963710018,0.763568992833556,
8.85434650606346));
#395724=CARTESIAN_POINT('Ctrl Pts',(-2.55510900057033,0.764057609326325,
8.85297329937117));
#395725=CARTESIAN_POINT('Ctrl Pts',(-2.55530549623525,0.764332426331667,
8.85220095427747));
#395726=CARTESIAN_POINT('Ctrl Pts',(-2.55552534811615,0.764592565881831,
8.85137579139183));
#395727=CARTESIAN_POINT('Ctrl Pts',(-2.55577009136411,0.764838063661123,
8.85049129520029));
#395728=CARTESIAN_POINT('Origin',(-2.56063892684945,0.759984192420898,7.59394543036555));
#395729=CARTESIAN_POINT('Ctrl Pts',(-2.55865644712841,0.75337726115675,
7.59443877723642));
#395730=CARTESIAN_POINT('Ctrl Pts',(-2.55299277157865,0.754583898184068,
7.58783886950016));
#395731=CARTESIAN_POINT('Ctrl Pts',(-2.55279250630485,0.763071481783466,
7.58559994247159));
#395732=CARTESIAN_POINT('Ctrl Pts',(-2.58957428578941,0.746790265025842,
7.56670252222137));
#395733=CARTESIAN_POINT('Ctrl Pts',(-2.58391879585875,0.747995158120122,
7.56004874999027));
#395734=CARTESIAN_POINT('Ctrl Pts',(-2.58369598431129,0.756532529628374,
7.55786368756704));
#395735=CARTESIAN_POINT('Ctrl Pts',(-2.62043438847577,0.740215569452088,
7.5388891333356));
#395736=CARTESIAN_POINT('Ctrl Pts',(-2.61474528769158,0.741427623284989,
7.5322200213728));
#395737=CARTESIAN_POINT('Ctrl Pts',(-2.61454260659733,0.750004415522996,
7.53005029815327));
#395738=CARTESIAN_POINT('Ctrl Pts',(-2.65123535874695,0.733653471944914,
7.51101258149734));
#395739=CARTESIAN_POINT('Ctrl Pts',(-2.64547729572389,0.734880218072622,
7.5043616886572));
#395740=CARTESIAN_POINT('Ctrl Pts',(-2.6453308662174,0.74348754285703,7.50217374673251));
#395741=CARTESIAN_POINT('',(-2.64368796492176,0.743835290548465,7.50366116523517));
#395742=CARTESIAN_POINT('Ctrl Pts',(-2.64284431997727,0.735441169348869,
7.51860402984325));
#395743=CARTESIAN_POINT('Ctrl Pts',(-2.643276237678,0.735349149972781,7.51734760759494));
#395744=CARTESIAN_POINT('Ctrl Pts',(-2.64367893454528,0.735324188140661,
7.51608817408573));
#395745=CARTESIAN_POINT('Ctrl Pts',(-2.64405231052279,0.735379669329133,
7.5148100591312));
#395746=CARTESIAN_POINT('Ctrl Pts',(-2.64439052340533,0.735429925515418,
7.51365231206384));
#395747=CARTESIAN_POINT('Ctrl Pts',(-2.64470519151024,0.735546009950654,
7.51247773061043));
#395748=CARTESIAN_POINT('Ctrl Pts',(-2.64497808983264,0.735760556806619,
7.51129758471022));
#395749=CARTESIAN_POINT('Ctrl Pts',(-2.64531727128122,0.736027214046408,
7.50983079813402));
#395750=CARTESIAN_POINT('Ctrl Pts',(-2.64557305354003,0.736447701509528,
7.50839324291155));
#395751=CARTESIAN_POINT('Ctrl Pts',(-2.64567687122122,0.737067931918167,
7.50715379678855));
#395752=CARTESIAN_POINT('Ctrl Pts',(-2.6457248319985,0.737354460495448,
7.50658120839351));
#395753=CARTESIAN_POINT('Ctrl Pts',(-2.64573780760563,0.737725918949378,
7.50598221009429));
#395754=CARTESIAN_POINT('Ctrl Pts',(-2.64569275661509,0.738174261178699,
7.50545747549611));
#395755=CARTESIAN_POINT('Ctrl Pts',(-2.64566871601208,0.738413510469755,
7.50517746087247));
#395756=CARTESIAN_POINT('Ctrl Pts',(-2.64562809243867,0.738677267900709,
7.50491486231392));
#395757=CARTESIAN_POINT('Ctrl Pts',(-2.64557031309821,0.738958294818664,
7.50468370960993));
#395758=CARTESIAN_POINT('Ctrl Pts',(-2.64548391475877,0.739378518705923,
7.50433806340447));
#395759=CARTESIAN_POINT('Ctrl Pts',(-2.64535602063784,0.739849845429687,
7.50405484070984));
#395760=CARTESIAN_POINT('Ctrl Pts',(-2.64519455277334,0.740340344402469,
7.50385766036131));
#395761=CARTESIAN_POINT('Ctrl Pts',(-2.64517728629501,0.740392795643526,
7.50383657498791));
#395762=CARTESIAN_POINT('Ctrl Pts',(-2.64515965723778,0.740445447432375,
7.50381643264937));
#395763=CARTESIAN_POINT('Ctrl Pts',(-2.64514169100079,0.740498247390553,
7.50379723213559));
#395764=CARTESIAN_POINT('Ctrl Pts',(-2.64502176049169,0.740850704383473,
7.50366906242519));
#395765=CARTESIAN_POINT('Ctrl Pts',(-2.6448835157668,0.741217198928826,
7.50358235568538));
#395766=CARTESIAN_POINT('Ctrl Pts',(-2.64474177332799,0.741567251487561,
7.5035341175365));
#395767=CARTESIAN_POINT('Ctrl Pts',(-2.64452924658315,0.742092115681084,
7.50346178989176));
#395768=CARTESIAN_POINT('Ctrl Pts',(-2.6442782995495,0.742647713723726,
7.50346967198527));
#395769=CARTESIAN_POINT('Ctrl Pts',(-2.64401516456435,0.743185558598988,
7.50354272648693));
#395770=CARTESIAN_POINT('Ctrl Pts',(-2.64390693169839,0.743406785328913,
7.50357277531559));
#395771=CARTESIAN_POINT('Ctrl Pts',(-2.64379690799386,0.743624776871163,
7.50361331098761));
#395772=CARTESIAN_POINT('Ctrl Pts',(-2.64368796492312,0.743835290548849,
7.50366116523659));
#395773=CARTESIAN_POINT('',(-2.56344583459805,0.760817267907127,7.57603338622103));
#395774=CARTESIAN_POINT('Origin',(-2.57191671161806,0.763334355930278,7.58486873427629));
#395775=CARTESIAN_POINT('Ctrl Pts',(-2.64368796497651,0.743835290531399,
7.50366116529968));
#395776=CARTESIAN_POINT('Ctrl Pts',(-2.6169844074643,0.749487530352289,
7.52783573079709));
#395777=CARTESIAN_POINT('Ctrl Pts',(-2.59023829728154,0.755147939735831,
7.55196141284069));
#395778=CARTESIAN_POINT('Ctrl Pts',(-2.56344583569988,0.760817267312471,
7.57603338728831));
#395779=CARTESIAN_POINT('Ctrl Pts',(-2.5602488397315,0.753217766653644,
7.59639677331371));
#395780=CARTESIAN_POINT('Ctrl Pts',(-2.54113756247317,0.754196289838703,
7.59974925422225));
#395781=CARTESIAN_POINT('Ctrl Pts',(-2.5566206780635,0.765442247231691,
7.59639677331372));
#395782=CARTESIAN_POINT('Ctrl Pts',(-2.55637188217917,0.752788459978717,
7.58707626057422));
#395783=CARTESIAN_POINT('Ctrl Pts',(-2.55101612578582,0.757128195576277,
7.58811717123966));
#395784=CARTESIAN_POINT('Ctrl Pts',(-2.55313724428125,0.763687028393967,
7.58707626057424));
#395785=CARTESIAN_POINT('Ctrl Pts',(-2.56010846144155,0.757580495838095,
7.5801537675693));
#395786=CARTESIAN_POINT('Ctrl Pts',(-2.55764184525408,0.759094674335491,
7.5820876076604));
#395787=CARTESIAN_POINT('Ctrl Pts',(-2.55888304972318,0.761709314540829,
7.5801537675693));
#395788=CARTESIAN_POINT('Ctrl Pts',(-2.56344583380474,0.760817267671466,
7.57603338509286));
#395789=CARTESIAN_POINT('Ctrl Pts',(-2.56344583380474,0.760817267671466,
7.57603338509286));
#395790=CARTESIAN_POINT('Ctrl Pts',(-2.56344583380474,0.760817267671466,
7.57603338509286));
#395791=CARTESIAN_POINT('Origin',(-2.57191833523281,0.763328885433854,7.58486873427624));
#395792=CARTESIAN_POINT('Ctrl Pts',(-2.62222153593683,0.831494374752899,
7.51098857897448));
#395793=CARTESIAN_POINT('Ctrl Pts',(-2.61806498568195,0.82732501005903,
7.50433767179956));
#395794=CARTESIAN_POINT('Ctrl Pts',(-2.62263789195665,0.820031411544902,
7.50214974420965));
#395795=CARTESIAN_POINT('Ctrl Pts',(-2.59998106725738,0.809185339807811,
7.53887321589163));
#395796=CARTESIAN_POINT('Ctrl Pts',(-2.5958743198511,0.805065931502258,
7.53220407452058));
#395797=CARTESIAN_POINT('Ctrl Pts',(-2.6003834002003,0.797767225156164,
7.53003438070911));
#395798=CARTESIAN_POINT('Ctrl Pts',(-2.57769788867395,0.786833463286226,
7.56669465659234));
#395799=CARTESIAN_POINT('Ctrl Pts',(-2.57361541138129,0.782738399917917,
7.560040858333));
#395800=CARTESIAN_POINT('Ctrl Pts',(-2.57808610350574,0.77546175494548,
7.55785582193789));
#395801=CARTESIAN_POINT('Ctrl Pts',(-2.55537300796543,0.76443975607395,
7.59443891967696));
#395802=CARTESIAN_POINT('Ctrl Pts',(-2.55128461158901,0.760338755373586,
7.58783901202978));
#395803=CARTESIAN_POINT('Ctrl Pts',(-2.55574704453252,0.753116160949631,
7.58560008491213));
#395804=CARTESIAN_POINT('',(-2.62143154819292,0.818824543767658,7.50366116523517));
#395805=CARTESIAN_POINT('Ctrl Pts',(-2.62143154819328,0.81882454376777,
7.50366116523554));
#395806=CARTESIAN_POINT('Ctrl Pts',(-2.62135613216077,0.819578499959339,
7.50350835821027));
#395807=CARTESIAN_POINT('Ctrl Pts',(-2.62126227734477,0.820269115108793,
7.50345484956));
#395808=CARTESIAN_POINT('Ctrl Pts',(-2.62114778839721,0.820917002630874,
7.50349758195598));
#395809=CARTESIAN_POINT('Ctrl Pts',(-2.6210890470764,0.821249416978292,
7.50351950684424));
#395810=CARTESIAN_POINT('Ctrl Pts',(-2.62101921161052,0.821603370108029,
7.50357029184312));
#395811=CARTESIAN_POINT('Ctrl Pts',(-2.62094248805988,0.821942831958116,
7.50365515313923));
#395812=CARTESIAN_POINT('Ctrl Pts',(-2.62082445617057,0.822465061745227,
7.50378570417639));
#395813=CARTESIAN_POINT('Ctrl Pts',(-2.62068699619852,0.822968401227933,
7.50400001621911));
#395814=CARTESIAN_POINT('Ctrl Pts',(-2.6205383806345,0.823413940824885,
7.50428903009634));
#395815=CARTESIAN_POINT('Ctrl Pts',(-2.62052188545027,0.82346339229237,
7.50432110841318));
#395816=CARTESIAN_POINT('Ctrl Pts',(-2.62050526126392,0.823512160826767,
7.50435406373354));
#395817=CARTESIAN_POINT('Ctrl Pts',(-2.62048852531448,0.823560214803795,
7.50438785222351));
#395818=CARTESIAN_POINT('Ctrl Pts',(-2.62038634429886,0.823853607431238,
7.50459414719561));
#395819=CARTESIAN_POINT('Ctrl Pts',(-2.62027788322083,0.824124865059689,
7.50483629897752));
#395820=CARTESIAN_POINT('Ctrl Pts',(-2.6201685191621,0.824364084488115,
7.5050991045531));
#395821=CARTESIAN_POINT('Ctrl Pts',(-2.61992725106395,0.824891826574538,
7.50567888004914));
#395822=CARTESIAN_POINT('Ctrl Pts',(-2.61967255410296,0.825284654989918,
7.50637912803144));
#395823=CARTESIAN_POINT('Ctrl Pts',(-2.61942507433289,0.825565573186598,
7.50710440483569));
#395824=CARTESIAN_POINT('Ctrl Pts',(-2.6193643873801,0.825634459905432,
7.50728225710685));
#395825=CARTESIAN_POINT('Ctrl Pts',(-2.61930303583773,0.825698084954761,
7.50746498566954));
#395826=CARTESIAN_POINT('Ctrl Pts',(-2.61924275173433,0.825755252289281,
7.50764697238949));
#395827=CARTESIAN_POINT('Ctrl Pts',(-2.61891868098509,0.826062568146788,
7.50862528291182));
#395828=CARTESIAN_POINT('Ctrl Pts',(-2.61859888721333,0.826214167004833,
7.50965856837423));
#395829=CARTESIAN_POINT('Ctrl Pts',(-2.61829462720512,0.826275384004112,
7.51067959873204));
#395830=CARTESIAN_POINT('Ctrl Pts',(-2.61812719253884,0.82630907179603,
7.5112414730258));
#395831=CARTESIAN_POINT('Ctrl Pts',(-2.61796433543798,0.826314971464054,
7.51180065547253));
#395832=CARTESIAN_POINT('Ctrl Pts',(-2.61780749365381,0.826301290589236,
7.512351757165));
#395833=CARTESIAN_POINT('Ctrl Pts',(-2.61726554281117,0.826254017716928,
7.51425603304535));
#395834=CARTESIAN_POINT('Ctrl Pts',(-2.61673132302744,0.825961279522731,
7.51626900505178));
#395835=CARTESIAN_POINT('Ctrl Pts',(-2.61622685877216,0.825479268445089,
7.51827788969241));
#395836=CARTESIAN_POINT('Ctrl Pts',(-2.61619955621336,0.82545318109469,
7.51838661432543));
#395837=CARTESIAN_POINT('Ctrl Pts',(-2.61617233996094,0.825426529404821,
7.51849533314855));
#395838=CARTESIAN_POINT('Ctrl Pts',(-2.61614521332083,0.825399319134616,
7.51860402984325));
#395839=CARTESIAN_POINT('Ctrl Pts',(-2.56344583519815,0.760817269007159,
7.57603338728985));
#395840=CARTESIAN_POINT('Ctrl Pts',(-2.58280746249544,0.780184887898324,
7.55196141284922));
#395841=CARTESIAN_POINT('Ctrl Pts',(-2.60213510843396,0.799519746263615,
7.52783573083104));
#395842=CARTESIAN_POINT('Ctrl Pts',(-2.62143154823074,0.818824543813179,
7.50366116530176));
#395843=CARTESIAN_POINT('Origin',(-8.85789032694963E-16,2.62897535302348E-16,
7.49482233047033));
#395844=CARTESIAN_POINT('Origin',(-2.63517950238395,0.741441326212315,7.49482233047033));
#395845=CARTESIAN_POINT('Origin',(0.,0.,7.50366116523517));
#395846=CARTESIAN_POINT('Origin',(-2.61299471585145,0.816189233531305,7.49482233047033));
#395847=CARTESIAN_POINT('Ctrl Pts',(-2.64284328546499,0.735441389704302,
7.51860402984325));
#395848=CARTESIAN_POINT('Ctrl Pts',(-2.6502853612481,0.733856525650656,
7.51860402984325));
#395849=CARTESIAN_POINT('Ctrl Pts',(-2.65229555990883,0.726517902661667,
7.51860402984325));
#395850=CARTESIAN_POINT('Ctrl Pts',(-2.64560657872596,0.734852917622648,
7.51041458714366));
#395851=CARTESIAN_POINT('Ctrl Pts',(-2.65076159078754,0.732117919193946,
7.51004642900443));
#395852=CARTESIAN_POINT('Ctrl Pts',(-2.65229611429775,0.726515878756583,
7.5072913648301));
#395853=CARTESIAN_POINT('Ctrl Pts',(-2.64710665836507,0.737234828258163,
7.50215815450137));
#395854=CARTESIAN_POINT('Ctrl Pts',(-2.64979207533485,0.735657932516545,
7.49877163671529));
#395855=CARTESIAN_POINT('Ctrl Pts',(-2.65072656602323,0.732336690166504,
7.4948158853317));
#395856=CARTESIAN_POINT('Ctrl Pts',(-2.64368743498051,0.743835141443236,
7.50366171572174));
#395857=CARTESIAN_POINT('Ctrl Pts',(-2.64721228549976,0.744826903044707,
7.50000045605858));
#395858=CARTESIAN_POINT('Ctrl Pts',(-2.64721228549979,0.744826903044587,
7.49482233047317));
#395859=CARTESIAN_POINT('Origin',(-2.64023967100015,0.72321554855866,7.51860402984325));
#395860=CARTESIAN_POINT('Origin',(-2.64023967100015,0.72321554855866,9.));
#395861=CARTESIAN_POINT('Origin',(-2.64023967100015,0.72321554855866,8.75721825406948));
#395862=CARTESIAN_POINT('Ctrl Pts',(-2.62651072673473,0.738920984405482,
8.78942910404912));
#395863=CARTESIAN_POINT('Ctrl Pts',(-2.63196505478754,0.737779610586776,
8.79672699501691));
#395864=CARTESIAN_POINT('Ctrl Pts',(-2.63177229643678,0.728855691593404,
8.79893251111266));
#395865=CARTESIAN_POINT('Ctrl Pts',(-2.63726373406303,0.736630078004512,
8.78111911759583));
#395866=CARTESIAN_POINT('Ctrl Pts',(-2.64372837849713,0.735269680097243,
8.78644465894813));
#395867=CARTESIAN_POINT('Ctrl Pts',(-2.64529556141671,0.727316099175921,
8.78817647674132));
#395868=CARTESIAN_POINT('Ctrl Pts',(-2.64396526470684,0.735202330461026,
8.76780923932029));
#395869=CARTESIAN_POINT('Ctrl Pts',(-2.65159545514092,0.733591451598431,
8.76988516158374));
#395870=CARTESIAN_POINT('Ctrl Pts',(-2.65374069660727,0.726343395345381,
8.77093053738833));
#395871=CARTESIAN_POINT('Ctrl Pts',(-2.64265855794782,0.735480721690211,
8.75371302330492));
#395872=CARTESIAN_POINT('Ctrl Pts',(-2.65010163704872,0.733910124712761,
8.75300828287559));
#395873=CARTESIAN_POINT('Ctrl Pts',(-2.65209349989808,0.72653265755095,
8.75267964240738));
#395874=CARTESIAN_POINT('Origin',(-2.62652489024715,0.726137460686699,8.78727029226991));
#395875=CARTESIAN_POINT('Ctrl Pts',(-2.55920636991203,0.753260100986283,
8.85049129520029));
#395876=CARTESIAN_POINT('Ctrl Pts',(-2.5649178041393,0.752043289049023,
8.85711686593484));
#395877=CARTESIAN_POINT('Ctrl Pts',(-2.56509113287407,0.743495147773657,
8.85933012996512));
#395878=CARTESIAN_POINT('Ctrl Pts',(-2.58254800437417,0.748287203055835,
8.82945683644722));
#395879=CARTESIAN_POINT('Ctrl Pts',(-2.58830684695874,0.747060290843812,
8.8360746990239));
#395880=CARTESIAN_POINT('Ctrl Pts',(-2.58844318986647,0.738486292178717,
8.83829567148519));
#395881=CARTESIAN_POINT('Ctrl Pts',(-2.60585484624787,0.743321717630768,
8.80838214965002));
#395882=CARTESIAN_POINT('Ctrl Pts',(-2.61163641591407,0.742089963450301,
8.81501364461994));
#395883=CARTESIAN_POINT('Ctrl Pts',(-2.61175996320559,0.733485688427861,
8.81722098428721));
#395884=CARTESIAN_POINT('Ctrl Pts',(-2.62912953922427,0.738363081476909,
8.78727029226991));
#395885=CARTESIAN_POINT('Ctrl Pts',(-2.63491206922813,0.737131122698032,
8.79393457792714));
#395886=CARTESIAN_POINT('Ctrl Pts',(-2.6350441475623,0.728492721775879,
8.79610912703474));
#395887=CARTESIAN_POINT('Origin',(-2.55660172093491,0.741034480196073,8.85049129520029));
#395888=CARTESIAN_POINT('Ctrl Pts',(-2.55577009136411,0.764838063661123,
8.85049129520029));
#395889=CARTESIAN_POINT('Ctrl Pts',(-2.55989296307187,0.768973645978575,
8.85711686593484));
#395890=CARTESIAN_POINT('Ctrl Pts',(-2.55537491841652,0.776232298374591,
8.85933012996512));
#395891=CARTESIAN_POINT('Ctrl Pts',(-2.55212264627854,0.761179373682638,
8.86332496987231));
#395892=CARTESIAN_POINT('Ctrl Pts',(-2.55108096399231,0.765681239117246,
8.86648636486738));
#395893=CARTESIAN_POINT('Ctrl Pts',(-2.54518317530685,0.765984868026305,
8.87206031107457));
#395894=CARTESIAN_POINT('Ctrl Pts',(-2.55411921096854,0.754343912071706,
8.86341338519876));
#395895=CARTESIAN_POINT('Ctrl Pts',(-2.55567876663298,0.749980283219038,
8.8665458496606));
#395896=CARTESIAN_POINT('Ctrl Pts',(-2.5508498873768,0.746544285850494,
8.87215952290715));
#395897=CARTESIAN_POINT('Ctrl Pts',(-2.55920636991203,0.753260100986283,
8.85049129520029));
#395898=CARTESIAN_POINT('Ctrl Pts',(-2.5649178041393,0.752043289049023,
8.85711686593484));
#395899=CARTESIAN_POINT('Ctrl Pts',(-2.56509113287407,0.743495147773658,
8.85933012996512));
#395900=CARTESIAN_POINT('Origin',(-2.54691766320894,0.773663284097895,8.85049129520029));
#395901=CARTESIAN_POINT('Ctrl Pts',(-2.60624502375465,0.815468607773348,
8.78727029226991));
#395902=CARTESIAN_POINT('Ctrl Pts',(-2.61041921685634,0.819655669706046,
8.79393457792714));
#395903=CARTESIAN_POINT('Ctrl Pts',(-2.60581736094344,0.826967464105174,
8.79610912703474));
#395904=CARTESIAN_POINT('Ctrl Pts',(-2.58944388951045,0.798615676462725,
8.80838214965001));
#395905=CARTESIAN_POINT('Ctrl Pts',(-2.59361738938011,0.802802043026238,
8.81501364461992));
#395906=CARTESIAN_POINT('Ctrl Pts',(-2.5890270005712,0.810080582933235,
8.81722098428721));
#395907=CARTESIAN_POINT('Ctrl Pts',(-2.57261954817434,0.781739466513871,
8.82945683644723));
#395908=CARTESIAN_POINT('Ctrl Pts',(-2.57677664221002,0.785909376664977,
8.83607469902391));
#395909=CARTESIAN_POINT('Ctrl Pts',(-2.57221349406444,0.793169522772258,
8.8382956714852));
#395910=CARTESIAN_POINT('Ctrl Pts',(-2.55577009136411,0.764838063661123,
8.85049129520029));
#395911=CARTESIAN_POINT('Ctrl Pts',(-2.55989296307187,0.768973645978575,
8.85711686593484));
#395912=CARTESIAN_POINT('Ctrl Pts',(-2.55537491841652,0.776232298374591,
8.85933012996512));
#395913=CARTESIAN_POINT('Origin',(-2.59739259559948,0.824293828210121,8.78727029226991));
#395914=CARTESIAN_POINT('Ctrl Pts',(-2.61601447323369,0.825268202110593,
8.75374538247848));
#395915=CARTESIAN_POINT('Ctrl Pts',(-2.62138876695583,0.830640477734187,
8.75304829418601));
#395916=CARTESIAN_POINT('Ctrl Pts',(-2.61904133544637,0.83790410000668,
8.75272238421917));
#395917=CARTESIAN_POINT('Ctrl Pts',(-2.61694640529134,0.826203006664529,
8.7676940844502));
#395918=CARTESIAN_POINT('Ctrl Pts',(-2.62245545220154,0.831710960650642,
8.76974318093971));
#395919=CARTESIAN_POINT('Ctrl Pts',(-2.62030466518858,0.83894922511839,
8.7707786988043));
#395920=CARTESIAN_POINT('Ctrl Pts',(-2.61216985246101,0.82141173103369,
8.78108014887988));
#395921=CARTESIAN_POINT('Ctrl Pts',(-2.61684125757339,0.826076836774891,
8.78639403366323));
#395922=CARTESIAN_POINT('Ctrl Pts',(-2.61383856832237,0.833593879610395,
8.78812224174741));
#395923=CARTESIAN_POINT('Ctrl Pts',(-2.60434213678208,0.81355988798455,
8.78944554828686));
#395924=CARTESIAN_POINT('Ctrl Pts',(-2.60828297933323,0.817487505278025,
8.79673892988686));
#395925=CARTESIAN_POINT('Ctrl Pts',(-2.60326063420178,0.824854974565179,
8.79894799272499));
#395926=CARTESIAN_POINT('Origin',(-2.60729278516566,0.834224539571385,8.75721825406948));
#395927=CARTESIAN_POINT('Origin',(-2.60729278516566,0.834224539571385,9.));
#395928=CARTESIAN_POINT('Origin',(-2.60729278516566,0.834224539571385,7.51860402984325));
#395929=CARTESIAN_POINT('Ctrl Pts',(-2.62143079730771,0.818824309222877,
7.50366195182966));
#395930=CARTESIAN_POINT('Ctrl Pts',(-2.62492619857219,0.81991612500875,
7.50000065167735));
#395931=CARTESIAN_POINT('Ctrl Pts',(-2.62492619857216,0.819916125008861,
7.49482233047108));
#395932=CARTESIAN_POINT('Ctrl Pts',(-2.62069416386201,0.826227765900225,
7.50215800491338));
#395933=CARTESIAN_POINT('Ctrl Pts',(-2.62208379159276,0.829015889273454,
7.49877273257264));
#395934=CARTESIAN_POINT('Ctrl Pts',(-2.62105455902767,0.83231101243912,
7.49481816995647));
#395935=CARTESIAN_POINT('Ctrl Pts',(-2.61813542442621,0.827395185636962,
7.5104302581404));
#395936=CARTESIAN_POINT('Ctrl Pts',(-2.62096858819431,0.832500667009961,
7.51006209594514));
#395937=CARTESIAN_POINT('Ctrl Pts',(-2.61919746011361,0.838036195483735,
7.50731281821699));
#395938=CARTESIAN_POINT('Ctrl Pts',(-2.61614414617581,0.825398248829071,
7.51860402984325));
#395939=CARTESIAN_POINT('Ctrl Pts',(-2.62151707779833,0.830786441770156,
7.51860402984325));
#395940=CARTESIAN_POINT('Ctrl Pts',(-2.61919823167327,0.83803378404432,
7.51860402984325));
#395941=CARTESIAN_POINT('Origin',(0.,0.,7.5));
#395942=CARTESIAN_POINT('Origin',(-2.59952233059431,0.59951786985688,7.5));
#395943=CARTESIAN_POINT('',(-2.59952233059431,0.59951786985688,7.59394543036555));
#395944=CARTESIAN_POINT('',(-2.59952233059431,0.59951786985688,8.85049129520029));
#395945=CARTESIAN_POINT('',(-2.59952233059431,0.59951786985688,7.5));
#395946=CARTESIAN_POINT('',(-2.65313746692185,0.646810448064345,8.78727029226991));
#395947=CARTESIAN_POINT('Ctrl Pts',(-2.59952233059431,0.59951786985688,
8.85049129520029));
#395948=CARTESIAN_POINT('Ctrl Pts',(-2.61742002096782,0.615304977373523,
8.82945686509571));
#395949=CARTESIAN_POINT('Ctrl Pts',(-2.63529110426044,0.631068615445895,
8.80838212259896));
#395950=CARTESIAN_POINT('Ctrl Pts',(-2.65313746692185,0.646810448064345,
8.78727029226991));
#395951=CARTESIAN_POINT('',(-2.66365357834825,0.656086448390696,8.75721825406948));
#395952=CARTESIAN_POINT('Origin',(-2.63200708449499,0.628171594201884,8.75937679713114));
#395953=CARTESIAN_POINT('',(-2.66365357834825,0.656086448390696,7.51860402984325));
#395954=CARTESIAN_POINT('',(-2.66365357834825,0.656086448390696,7.5));
#395955=CARTESIAN_POINT('Ctrl Pts',(-2.66365357834825,0.656086448390696,
7.51860402984325));
#395956=CARTESIAN_POINT('Ctrl Pts',(-2.65539480838751,0.648801592825284,
7.52834476460825));
#395957=CARTESIAN_POINT('Ctrl Pts',(-2.64713067695249,0.641512008036755,
7.53807742314407));
#395958=CARTESIAN_POINT('Ctrl Pts',(-2.63886100402454,0.634217535235156,
7.54780169004674));
#395959=CARTESIAN_POINT('Ctrl Pts',(-2.62576228904436,0.622663484550039,
7.5632044032688));
#395960=CARTESIAN_POINT('Ctrl Pts',(-2.61264965451767,0.611097155779194,
7.57858609112102));
#395961=CARTESIAN_POINT('Ctrl Pts',(-2.59952233059431,0.59951786985688,
7.59394543036555));
#395962=CARTESIAN_POINT('Origin',(-2.86694941950356,0.51332642770833,7.5));
#395963=CARTESIAN_POINT('',(-2.68453419038077,0.564602509634903,8.75721825406948));
#395964=CARTESIAN_POINT('',(-2.67103479566853,0.568397127400933,8.78727029226991));
#395965=CARTESIAN_POINT('Origin',(-2.63676829686931,0.578029282611961,8.75658640621177));
#395966=CARTESIAN_POINT('',(-2.60220974632391,0.587743532225608,8.85049129520029));
#395967=CARTESIAN_POINT('Ctrl Pts',(-2.67103479566853,0.568397127400933,
8.78727029226991));
#395968=CARTESIAN_POINT('Ctrl Pts',(-2.64812565330825,0.574836781952707,
8.80838212259896));
#395969=CARTESIAN_POINT('Ctrl Pts',(-2.62518477739697,0.581285356659713,
8.82945686509571));
#395970=CARTESIAN_POINT('Ctrl Pts',(-2.60220974632391,0.587743532225608,
8.85049129520029));
#395971=CARTESIAN_POINT('',(-2.60220974632391,0.587743532225608,7.59394543036555));
#395972=CARTESIAN_POINT('',(-2.60220974632391,0.587743532225608,7.5));
#395973=CARTESIAN_POINT('',(-2.68453419038077,0.564602509634903,7.51860402984325));
#395974=CARTESIAN_POINT('Ctrl Pts',(-2.60220974632391,0.587743532225608,
7.59394543036555));
#395975=CARTESIAN_POINT('Ctrl Pts',(-2.61906112037001,0.58300668848554,
7.57858609112103));
#395976=CARTESIAN_POINT('Ctrl Pts',(-2.63589363782949,0.578275145245262,
7.56320440326857));
#395977=CARTESIAN_POINT('Ctrl Pts',(-2.65270828694937,0.573548624713042,
7.54780169004651));
#395978=CARTESIAN_POINT('Ctrl Pts',(-2.66332395793924,0.570564608422297,
7.53807742314383));
#395979=CARTESIAN_POINT('Ctrl Pts',(-2.67393251538731,0.567582591715426,
7.52834476460825));
#395980=CARTESIAN_POINT('Ctrl Pts',(-2.68453419038077,0.564602509634903,
7.51860402984325));
#395981=CARTESIAN_POINT('',(-2.68453419038077,0.564602509634903,7.5));
#395982=CARTESIAN_POINT('Origin',(-2.60407017393684,0.594362024055099,7.5));
#395983=CARTESIAN_POINT('Ctrl Pts',(-2.60220974632391,0.587743532225608,
8.85049129520029));
#395984=CARTESIAN_POINT('Ctrl Pts',(-2.60202331038288,0.587795938511159,
8.85097269580138));
#395985=CARTESIAN_POINT('Ctrl Pts',(-2.60184150286887,0.587855781174756,
8.85143669361005));
#395986=CARTESIAN_POINT('Ctrl Pts',(-2.60165622548117,0.587926646233124,
8.8519052845931));
#395987=CARTESIAN_POINT('Ctrl Pts',(-2.60129383466069,0.588065253793194,
8.85282181883899));
#395988=CARTESIAN_POINT('Ctrl Pts',(-2.60092756183387,0.588242647837763,
8.85372622499635));
#395989=CARTESIAN_POINT('Ctrl Pts',(-2.60055838042438,0.588475488848304,
8.8546225773507));
#395990=CARTESIAN_POINT('Ctrl Pts',(-2.60025189913029,0.588668785185525,
8.85536669723986));
#395991=CARTESIAN_POINT('Ctrl Pts',(-2.59994332657567,0.588900311421549,
8.85610498449051));
#395992=CARTESIAN_POINT('Ctrl Pts',(-2.59963799631076,0.589186020321766,
8.85681338218371));
#395993=CARTESIAN_POINT('Ctrl Pts',(-2.59936090861582,0.589445301597426,
8.85745625420284));
#395994=CARTESIAN_POINT('Ctrl Pts',(-2.59908260643578,0.589752020910516,
8.85808743050665));
#395995=CARTESIAN_POINT('Ctrl Pts',(-2.59881389793109,0.590132655228693,
8.8586680450841));
#395996=CARTESIAN_POINT('Ctrl Pts',(-2.59868992165191,0.59030827165196,
8.85893592806395));
#395997=CARTESIAN_POINT('Ctrl Pts',(-2.59856810529721,0.590499834217007,
8.85919241173848));
#395998=CARTESIAN_POINT('Ctrl Pts',(-2.59845047286812,0.590711216603729,
8.85943017985534));
#395999=CARTESIAN_POINT('Ctrl Pts',(-2.59829163426592,0.590996645401686,
8.8597512372));
#396000=CARTESIAN_POINT('Ctrl Pts',(-2.59813694107696,0.591325788054087,
8.86004599534705));
#396001=CARTESIAN_POINT('Ctrl Pts',(-2.59799767783027,0.591699120121058,
8.86026130871721));
#396002=CARTESIAN_POINT('Ctrl Pts',(-2.5979466896294,0.591835807516122,
8.86034014101235));
#396003=CARTESIAN_POINT('Ctrl Pts',(-2.59789699236396,0.591980467381866,
8.86040910639693));
#396004=CARTESIAN_POINT('Ctrl Pts',(-2.59785025813686,0.592129267833217,
8.86046313645507));
#396005=CARTESIAN_POINT('Ctrl Pts',(-2.59777732976686,0.592361469691356,
8.8605474499083));
#396006=CARTESIAN_POINT('Ctrl Pts',(-2.59770976635181,0.592610136901956,
8.86059655985668));
#396007=CARTESIAN_POINT('Ctrl Pts',(-2.59765161823106,0.592859244867346,
8.86059725258816));
#396008=CARTESIAN_POINT('Ctrl Pts',(-2.59759333576492,0.593108928371656,
8.86059794692011));
#396009=CARTESIAN_POINT('Ctrl Pts',(-2.59754645301029,0.593362427609944,
8.86056369958366));
#396010=CARTESIAN_POINT('Ctrl Pts',(-2.59750982662749,0.593605232259524,
8.86048590497774));
#396011=CARTESIAN_POINT('Ctrl Pts',(-2.59750026823207,0.593668597043899,
8.86046560290182));
#396012=CARTESIAN_POINT('Ctrl Pts',(-2.59749137356794,0.59373207131882,
8.86044257503091));
#396013=CARTESIAN_POINT('Ctrl Pts',(-2.59748338497902,0.593793689121214,
8.86041778462583));
#396014=CARTESIAN_POINT('Ctrl Pts',(-2.59742963168863,0.594208300470006,
8.86025097596201));
#396015=CARTESIAN_POINT('Ctrl Pts',(-2.59741001819078,0.594594535816544,
8.8599848982295));
#396016=CARTESIAN_POINT('Ctrl Pts',(-2.59741665536619,0.594940692276304,
8.85968173251462));
#396017=CARTESIAN_POINT('Ctrl Pts',(-2.59742016605172,0.595123789211116,
8.85952137522077));
#396018=CARTESIAN_POINT('Ctrl Pts',(-2.59743089790696,0.595299205846478,
8.85934740853961));
#396019=CARTESIAN_POINT('Ctrl Pts',(-2.59744714793786,0.595464563348899,
8.8591675900182));
#396020=CARTESIAN_POINT('Ctrl Pts',(-2.59751240025853,0.596128559672241,
8.85844552518695));
#396021=CARTESIAN_POINT('Ctrl Pts',(-2.59766730636048,0.59666818199704,
8.85759444184124));
#396022=CARTESIAN_POINT('Ctrl Pts',(-2.59783312773382,0.597096816488949,
8.85683498915139));
#396023=CARTESIAN_POINT('Ctrl Pts',(-2.59785048049892,0.59714167194698,
8.85675551444998));
#396024=CARTESIAN_POINT('Ctrl Pts',(-2.59786796965054,0.59718530125862,
8.85667699793651));
#396025=CARTESIAN_POINT('Ctrl Pts',(-2.59788551566069,0.597227712156571,
8.85659965593547));
#396026=CARTESIAN_POINT('Ctrl Pts',(-2.59812235260094,0.597800176621236,
8.85555568965886));
#396027=CARTESIAN_POINT('Ctrl Pts',(-2.59843264276994,0.598316146498407,
8.85434650606346));
#396028=CARTESIAN_POINT('Ctrl Pts',(-2.59881259420155,0.598781375281802,
8.85297329937117));
#396029=CARTESIAN_POINT('Ctrl Pts',(-2.59902629373105,0.599043038125655,
8.85220095427747));
#396030=CARTESIAN_POINT('Ctrl Pts',(-2.59926236110088,0.599288557232841,
8.85137579139183));
#396031=CARTESIAN_POINT('Ctrl Pts',(-2.59952233059431,0.59951786985688,
8.85049129520029));
#396032=CARTESIAN_POINT('Origin',(-2.60407017393684,0.594362024055099,7.59394543036555));
#396033=CARTESIAN_POINT('Ctrl Pts',(-2.60166845989353,0.587895685351658,
7.59443877723642));
#396034=CARTESIAN_POINT('Ctrl Pts',(-2.59609373047238,0.589462716152165,
7.58783886950016));
#396035=CARTESIAN_POINT('Ctrl Pts',(-2.59643767801338,0.597945692140914,
7.58559994247159));
#396036=CARTESIAN_POINT('Ctrl Pts',(-2.63210074424794,0.579341310186416,
7.56670252222136));
#396037=CARTESIAN_POINT('Ctrl Pts',(-2.6265340718935,0.580906076182574,
7.56004874999025));
#396038=CARTESIAN_POINT('Ctrl Pts',(-2.62685870940684,0.589440182330292,
7.55786368756705));
#396039=CARTESIAN_POINT('Ctrl Pts',(-2.66247619935184,0.57080290946212,
7.53888913333556));
#396040=CARTESIAN_POINT('Ctrl Pts',(-2.65687644399105,0.572376974939169,
7.53222002137275));
#396041=CARTESIAN_POINT('Ctrl Pts',(-2.65722369629234,0.580949131059962,
7.53005029815326));
#396042=CARTESIAN_POINT('Ctrl Pts',(-2.69279345069543,0.562280869547154,
7.51101258149734));
#396043=CARTESIAN_POINT('Ctrl Pts',(-2.68712581612466,0.563874015557924,
7.5043616886572));
#396044=CARTESIAN_POINT('Ctrl Pts',(-2.68753116066568,0.572473037441123,
7.50217374673251));
#396045=CARTESIAN_POINT('',(-2.68591391515804,0.572925331695047,7.50366116523517));
#396046=CARTESIAN_POINT('Ctrl Pts',(-2.68453419038077,0.564602509634902,
7.51860402984325));
#396047=CARTESIAN_POINT('Ctrl Pts',(-2.68495932495859,0.564483006260392,
7.51734760759494));
#396048=CARTESIAN_POINT('Ctrl Pts',(-2.68535959513189,0.564432294838161,
7.51608817408573));
#396049=CARTESIAN_POINT('Ctrl Pts',(-2.68573575866036,0.564463739753566,
7.5148100591312));
#396050=CARTESIAN_POINT('Ctrl Pts',(-2.68607649657317,0.564492223309341,
7.51365231206384));
#396051=CARTESIAN_POINT('Ctrl Pts',(-2.68639795571401,0.564587908381951,
7.51247773061043));
#396052=CARTESIAN_POINT('Ctrl Pts',(-2.6866840394018,0.564784529772842,
7.51129758471022));
#396053=CARTESIAN_POINT('Ctrl Pts',(-2.68703960875373,0.565028907706709,
7.50983079813402));
#396054=CARTESIAN_POINT('Ctrl Pts',(-2.68732180620472,0.565432143207649,
7.50839324291155));
#396055=CARTESIAN_POINT('Ctrl Pts',(-2.68746514888007,0.566044447664722,
7.50715379678855));
#396056=CARTESIAN_POINT('Ctrl Pts',(-2.68753136906576,0.566327314680761,
7.50658120839351));
#396057=CARTESIAN_POINT('Ctrl Pts',(-2.68756811743797,0.566697178583455,
7.50598221009429));
#396058=CARTESIAN_POINT('Ctrl Pts',(-2.68755188439478,0.567147486072456,
7.50545747549611));
#396059=CARTESIAN_POINT('Ctrl Pts',(-2.68754322194048,0.567387784086907,
7.50517746087247));
#396060=CARTESIAN_POINT('Ctrl Pts',(-2.68751958082918,0.567653602361217,
7.50491486231392));
#396061=CARTESIAN_POINT('Ctrl Pts',(-2.68747992565903,0.567937753814282,
7.50468370960992));
#396062=CARTESIAN_POINT('Ctrl Pts',(-2.68742062867114,0.568362649867107,
7.50433806340447));
#396063=CARTESIAN_POINT('Ctrl Pts',(-2.68732319532927,0.568841202404026,
7.50405484070984));
#396064=CARTESIAN_POINT('Ctrl Pts',(-2.68719348559491,0.569341038875656,
7.50385766036131));
#396065=CARTESIAN_POINT('Ctrl Pts',(-2.68717961515496,0.569394488617083,
7.50383657498791));
#396066=CARTESIAN_POINT('Ctrl Pts',(-2.68716539573021,0.569448161724763,
7.50381643264937));
#396067=CARTESIAN_POINT('Ctrl Pts',(-2.68715084931171,0.569502004300525,
7.50379723213559));
#396068=CARTESIAN_POINT('Ctrl Pts',(-2.68705374720978,0.569861421106853,
7.50366906242519));
#396069=CARTESIAN_POINT('Ctrl Pts',(-2.68693926790964,0.570236020019791,
7.50358235568538));
#396070=CARTESIAN_POINT('Ctrl Pts',(-2.68682024464032,0.570594434827236,
7.5035341175365));
#396071=CARTESIAN_POINT('Ctrl Pts',(-2.68664178271881,0.571131837266276,
7.50346178989176));
#396072=CARTESIAN_POINT('Ctrl Pts',(-2.68642694857157,0.571702372004801,
7.50346967198527));
#396073=CARTESIAN_POINT('Ctrl Pts',(-2.68619881406494,0.572255970936466,
7.50354272648692));
#396074=CARTESIAN_POINT('Ctrl Pts',(-2.68610497762026,0.572483677635879,
7.50357277531559));
#396075=CARTESIAN_POINT('Ctrl Pts',(-2.6860091467373,0.572708270534078,
7.50361331098761));
#396076=CARTESIAN_POINT('Ctrl Pts',(-2.68591391515943,0.572925331695343,
7.50366116523659));
#396077=CARTESIAN_POINT('',(-2.6069246899221,0.595013548701475,7.57603338622103));
#396078=CARTESIAN_POINT('Origin',(-2.61553943299995,0.596982734143139,7.58486873427628));
#396079=CARTESIAN_POINT('Ctrl Pts',(-2.68591391521158,0.57292533167451,
7.50366116529969));
#396080=CARTESIAN_POINT('Ctrl Pts',(-2.65962736327094,0.580276861166578,
7.52783573079709));
#396081=CARTESIAN_POINT('Ctrl Pts',(-2.63329886951444,0.587639269794993,
7.55196141284068));
#396082=CARTESIAN_POINT('Ctrl Pts',(-2.60692469098357,0.59501354803745,
7.57603338728831));
#396083=CARTESIAN_POINT('Ctrl Pts',(-2.60324736190728,0.587634493602744,
7.59639677331372));
#396084=CARTESIAN_POINT('Ctrl Pts',(-2.58509102396111,0.589736708654646,
7.59959882295461));
#396085=CARTESIAN_POINT('Ctrl Pts',(-2.60025825567991,0.599967246010122,
7.59642833564546));
#396086=CARTESIAN_POINT('Ctrl Pts',(-2.59935086420695,0.587454466507696,
7.58707626057424));
#396087=CARTESIAN_POINT('Ctrl Pts',(-2.59437047150332,0.592048808631819,
7.58809943920598));
#396088=CARTESIAN_POINT('Ctrl Pts',(-2.5967579751915,0.598374488589847,
7.58710240504252));
#396089=CARTESIAN_POINT('Ctrl Pts',(-2.60338679305819,0.591997253160073,
7.5801537675693));
#396090=CARTESIAN_POINT('Ctrl Pts',(-2.60105747402761,0.593641498959686,
7.5820588065976));
#396091=CARTESIAN_POINT('Ctrl Pts',(-2.60238830315171,0.596122621463806,
7.58020924244129));
#396092=CARTESIAN_POINT('Ctrl Pts',(-2.60692468911532,0.595013548517127,
7.57603338509286));
#396093=CARTESIAN_POINT('Ctrl Pts',(-2.60692468911532,0.595013548517126,
7.57603338509286));
#396094=CARTESIAN_POINT('Ctrl Pts',(-2.60692468911532,0.595013548517126,
7.57603338509286));
#396095=CARTESIAN_POINT('Origin',(-2.61554070278294,0.596977170861169,7.58486873427623));
#396096=CARTESIAN_POINT('Ctrl Pts',(-2.67010792806202,0.661779669736841,
7.51098857897448));
#396097=CARTESIAN_POINT('Ctrl Pts',(-2.6656927857723,0.657885182539089,
7.50433767179956));
#396098=CARTESIAN_POINT('Ctrl Pts',(-2.66978899405937,0.650313582394374,
7.50214974420965));
#396099=CARTESIAN_POINT('Ctrl Pts',(-2.64648381003428,0.64094142281747,
7.53887321589167));
#396100=CARTESIAN_POINT('Ctrl Pts',(-2.64212156898465,0.637093598487822,
7.53220407452062));
#396101=CARTESIAN_POINT('Ctrl Pts',(-2.6461537552235,0.629520990346805,
7.53003438070911));
#396102=CARTESIAN_POINT('Ctrl Pts',(-2.62281432498534,0.620063158777091,
7.56669465659229));
#396103=CARTESIAN_POINT('Ctrl Pts',(-2.61847786396929,0.616238074373824,
7.56004085833292));
#396104=CARTESIAN_POINT('Ctrl Pts',(-2.62247315433322,0.60868994182108,
7.55785582193789));
#396105=CARTESIAN_POINT('Ctrl Pts',(-2.59910054339133,0.599145821856068,
7.59443891967696));
#396106=CARTESIAN_POINT('Ctrl Pts',(-2.59475779504673,0.595315191556679,
7.58783901202978));
#396107=CARTESIAN_POINT('Ctrl Pts',(-2.59874830622959,0.587821527667248,
7.58560008491213));
#396108=CARTESIAN_POINT('',(-2.66850780457431,0.649186484966729,7.50366116523517));
#396109=CARTESIAN_POINT('Ctrl Pts',(-2.66850780457467,0.649186484966817,
7.50366116523554));
#396110=CARTESIAN_POINT('Ctrl Pts',(-2.66848084963154,0.649943723996322,
7.50350835821027));
#396111=CARTESIAN_POINT('Ctrl Pts',(-2.66843143551487,0.650638933501591,
7.50345484956));
#396112=CARTESIAN_POINT('Ctrl Pts',(-2.6683586920932,0.651292825201327,
7.50349758195598));
#396113=CARTESIAN_POINT('Ctrl Pts',(-2.66832136932309,0.651628320137165,
7.50351950684424));
#396114=CARTESIAN_POINT('Ctrl Pts',(-2.66827435519655,0.651986020405896,
7.50357029184312));
#396115=CARTESIAN_POINT('Ctrl Pts',(-2.66821953867809,0.652329700489972,
7.50365515313923));
#396116=CARTESIAN_POINT('Ctrl Pts',(-2.6681352086753,0.652858419629088,
7.50378570417639));
#396117=CARTESIAN_POINT('Ctrl Pts',(-2.66803028020088,0.65336953203749,
7.50400001621911));
#396118=CARTESIAN_POINT('Ctrl Pts',(-2.66791051580347,0.653823678057434,
7.50428903009635));
#396119=CARTESIAN_POINT('Ctrl Pts',(-2.66789722287677,0.653874084771659,
7.50432110841318));
#396120=CARTESIAN_POINT('Ctrl Pts',(-2.66788375745731,0.653923818221149,
7.50435406373354));
#396121=CARTESIAN_POINT('Ctrl Pts',(-2.66787013472256,0.653972845742091,
7.50438785222352));
#396122=CARTESIAN_POINT('Ctrl Pts',(-2.66778696137897,0.654272182323062,
7.50459414719561));
#396123=CARTESIAN_POINT('Ctrl Pts',(-2.66769610268179,0.654549831748752,
7.50483629897752));
#396124=CARTESIAN_POINT('Ctrl Pts',(-2.66760229016464,0.654795566654507,
7.5050991045531));
#396125=CARTESIAN_POINT('Ctrl Pts',(-2.66739533032925,0.655337682538336,
7.50567888004914));
#396126=CARTESIAN_POINT('Ctrl Pts',(-2.66716632527347,0.655746022335924,
7.50637912803144));
#396127=CARTESIAN_POINT('Ctrl Pts',(-2.66693735246779,0.65604221943935,
7.50710440483569));
#396128=CARTESIAN_POINT('Ctrl Pts',(-2.66688120379009,0.656114852849446,
7.50728225710685));
#396129=CARTESIAN_POINT('Ctrl Pts',(-2.66682405477194,0.656182277981104,
7.50746498566954));
#396130=CARTESIAN_POINT('Ctrl Pts',(-2.66676755725239,0.65624319027497,
7.50764697238949));
#396131=CARTESIAN_POINT('Ctrl Pts',(-2.66646384213586,0.65657063800328,
7.50862528291182));
#396132=CARTESIAN_POINT('Ctrl Pts',(-2.66615441838689,0.656742414642516,
7.50965856837422));
#396133=CARTESIAN_POINT('Ctrl Pts',(-2.66585470570012,0.656822999870563,
7.51067959873202));
#396134=CARTESIAN_POINT('Ctrl Pts',(-2.66568977343054,0.656867346023202,
7.51124147302579));
#396135=CARTESIAN_POINT('Ctrl Pts',(-2.66552762893009,0.656883667860003,
7.51180065547253));
#396136=CARTESIAN_POINT('Ctrl Pts',(-2.66537023285753,0.656880063981624,
7.512351757165));
#396137=CARTESIAN_POINT('Ctrl Pts',(-2.66482636672768,0.656867611146211,
7.51425603304536));
#396138=CARTESIAN_POINT('Ctrl Pts',(-2.6642744887553,0.65660970199309,7.5162690050518));
#396139=CARTESIAN_POINT('Ctrl Pts',(-2.66374017842015,0.656161002394707,
7.51827788969243));
#396140=CARTESIAN_POINT('Ctrl Pts',(-2.66371126053511,0.656136717924517,
7.51838661432545));
#396141=CARTESIAN_POINT('Ctrl Pts',(-2.66368239262177,0.656111864744685,
7.51849533314856));
#396142=CARTESIAN_POINT('Ctrl Pts',(-2.66365357834825,0.6560864483907,7.51860402984325));
#396143=CARTESIAN_POINT('Ctrl Pts',(-2.60692469059145,0.595013549760795,
7.57603338728985));
#396144=CARTESIAN_POINT('Ctrl Pts',(-2.62748742495179,0.613100872081649,
7.55196141284922));
#396145=CARTESIAN_POINT('Ctrl Pts',(-2.64801414879759,0.631157678379805,
7.52783573083105));
#396146=CARTESIAN_POINT('Ctrl Pts',(-2.66850780461497,0.649186485009733,
7.50366116530176));
#396147=CARTESIAN_POINT('Origin',(-9.00812987045924E-16,2.05604685939128E-16,
7.49482233047033));
#396148=CARTESIAN_POINT('Origin',(-2.6772695523474,0.571081425081873,7.49482233047033));
#396149=CARTESIAN_POINT('Origin',(0.,0.,7.50366116523517));
#396150=CARTESIAN_POINT('Origin',(-2.65991946170317,0.647097138961951,7.49482233047033));
#396151=CARTESIAN_POINT('Ctrl Pts',(-2.68453317211223,0.56460279581902,
7.51860402984325));
#396152=CARTESIAN_POINT('Ctrl Pts',(-2.69185841476393,0.56254437260601,
7.51860402984325));
#396153=CARTESIAN_POINT('Ctrl Pts',(-2.69339429606665,0.555092033734621,
7.51860402984325));
#396154=CARTESIAN_POINT('Ctrl Pts',(-2.68725308435509,0.563838488009272,
7.51041458714365));
#396155=CARTESIAN_POINT('Ctrl Pts',(-2.69222227294056,0.560778826171376,
7.51004642900443));
#396156=CARTESIAN_POINT('Ctrl Pts',(-2.69339471964448,0.555089978468046,
7.5072913648301));
#396157=CARTESIAN_POINT('Ctrl Pts',(-2.68890269145811,0.566119394321452,
7.50215815450137));
#396158=CARTESIAN_POINT('Ctrl Pts',(-2.69148155889365,0.564373683225266,
7.4987716367153));
#396159=CARTESIAN_POINT('Ctrl Pts',(-2.69220133684272,0.560999391699865,
7.49481588533171));
#396160=CARTESIAN_POINT('Ctrl Pts',(-2.68591337675241,0.572925216849624,
7.50366171572174));
#396161=CARTESIAN_POINT('Ctrl Pts',(-2.6894945274722,0.573689102822351,
7.50000045605858));
#396162=CARTESIAN_POINT('Ctrl Pts',(-2.68949452747222,0.57368910282223,
7.49482233047317));
#396163=CARTESIAN_POINT('Origin',(-2.68115159472089,0.552568888126737,7.51860402984325));
#396164=CARTESIAN_POINT('Origin',(-2.68115159472089,0.552568888126737,9.));
#396165=CARTESIAN_POINT('Origin',(-2.68115159472089,0.552568888126737,8.75721825406948));
#396166=CARTESIAN_POINT('Ctrl Pts',(-2.66845710877349,0.569121671950397,
8.78942910404912));
#396167=CARTESIAN_POINT('Ctrl Pts',(-2.67382710225269,0.567633183208423,
8.79672699501691));
#396168=CARTESIAN_POINT('Ctrl Pts',(-2.67306298249164,0.558739949433648,
8.79893251111267));
#396169=CARTESIAN_POINT('Ctrl Pts',(-2.67904124401791,0.566146524917349,
8.78111911759583));
#396170=CARTESIAN_POINT('Ctrl Pts',(-2.68540544515351,0.564374730902493,
8.78644465894813));
#396171=CARTESIAN_POINT('Ctrl Pts',(-2.68645982044843,0.556337081711785,
8.78817647674132));
#396172=CARTESIAN_POINT('Ctrl Pts',(-2.68563752954908,0.564292342291762,
8.76780923932029));
#396173=CARTESIAN_POINT('Ctrl Pts',(-2.69314883357549,0.562195905172953,
8.76988516158374));
#396174=CARTESIAN_POINT('Ctrl Pts',(-2.69482528285461,0.554825294736158,
8.77093053738833));
#396175=CARTESIAN_POINT('Ctrl Pts',(-2.68435134414654,0.564653882525808,
8.75371302330492));
#396176=CARTESIAN_POINT('Ctrl Pts',(-2.69167850214931,0.562609632792963,
8.75300828287559));
#396177=CARTESIAN_POINT('Ctrl Pts',(-2.69319359655887,0.555119704337743,
8.75267964240738));
#396178=CARTESIAN_POINT('Origin',(-2.66765220000866,0.556363505892767,8.78727029226991));
#396179=CARTESIAN_POINT('Ctrl Pts',(-2.60220974632391,0.587743532225608,
8.85049129520029));
#396180=CARTESIAN_POINT('Ctrl Pts',(-2.60783148438852,0.586163287511629,
8.85711686593484));
#396181=CARTESIAN_POINT('Ctrl Pts',(-2.60745677570887,0.577621604099134,
8.85933012996512));
#396182=CARTESIAN_POINT('Ctrl Pts',(-2.62518480823032,0.581285347992601,
8.82945683644724));
#396183=CARTESIAN_POINT('Ctrl Pts',(-2.63085321011983,0.579691986292063,
8.8360746990239));
#396184=CARTESIAN_POINT('Ctrl Pts',(-2.63043993491586,0.571126868306685,
8.8382956714852));
#396185=CARTESIAN_POINT('Ctrl Pts',(-2.64812562395425,0.57483679020398,
8.80838214965002));
#396186=CARTESIAN_POINT('Ctrl Pts',(-2.6538163960042,0.573237140354248,
8.81501364461995));
#396187=CARTESIAN_POINT('Ctrl Pts',(-2.65338841166109,0.564642628035487,
8.81722098428721));
#396188=CARTESIAN_POINT('Ctrl Pts',(-2.67103479566853,0.568397127400933,
8.78727029226991));
#396189=CARTESIAN_POINT('Ctrl Pts',(-2.67672651297436,0.566797211844102,
8.79393457792714));
#396190=CARTESIAN_POINT('Ctrl Pts',(-2.67630485569206,0.558168097155184,
8.79610912703474));
#396191=CARTESIAN_POINT('Origin',(-2.59882715066404,0.575709910717442,8.85049129520029));
#396192=CARTESIAN_POINT('Ctrl Pts',(-2.59952233059431,0.59951786985688,
8.85049129520029));
#396193=CARTESIAN_POINT('Ctrl Pts',(-2.6039016990888,0.603380801879653,
8.85711686593484));
#396194=CARTESIAN_POINT('Ctrl Pts',(-2.59985800069653,0.610914012710784,
8.85933012996512));
#396195=CARTESIAN_POINT('Ctrl Pts',(-2.59564796650408,0.596100389658347,
8.86332496987231));
#396196=CARTESIAN_POINT('Ctrl Pts',(-2.59489685997454,0.600659746340822,
8.86648636486737));
#396197=CARTESIAN_POINT('Ctrl Pts',(-2.58903064249948,0.601340624030199,
8.87206031107457));
#396198=CARTESIAN_POINT('Ctrl Pts',(-2.59720247950872,0.589151051897506,
8.86341338519877));
#396199=CARTESIAN_POINT('Ctrl Pts',(-2.59847925223829,0.584696467513824,
8.86654584966059));
#396200=CARTESIAN_POINT('Ctrl Pts',(-2.59344014932518,0.581576917126584,
8.87215952290714));
#396201=CARTESIAN_POINT('Ctrl Pts',(-2.60220974632391,0.587743532225608,
8.85049129520029));
#396202=CARTESIAN_POINT('Ctrl Pts',(-2.60783148438852,0.586163287511629,
8.85711686593484));
#396203=CARTESIAN_POINT('Ctrl Pts',(-2.60745677570887,0.577621604099134,
8.85933012996512));
#396204=CARTESIAN_POINT('Origin',(-2.59125352451697,0.608892134951029,8.85049129520029));
#396205=CARTESIAN_POINT('Ctrl Pts',(-2.65313746692185,0.646810448064345,
8.78727029226991));
#396206=CARTESIAN_POINT('Ctrl Pts',(-2.65757134967523,0.650721465758973,
8.79393457792714));
#396207=CARTESIAN_POINT('Ctrl Pts',(-2.65344741704445,0.65831307921298,
8.79610912703474));
#396208=CARTESIAN_POINT('Ctrl Pts',(-2.63529108139349,0.631068595275529,
8.80838214965003));
#396209=CARTESIAN_POINT('Ctrl Pts',(-2.63972422778674,0.634978963445187,
8.81501364461995));
#396210=CARTESIAN_POINT('Ctrl Pts',(-2.63560960807689,0.642536656032112,
8.81722098428721));
#396211=CARTESIAN_POINT('Ctrl Pts',(-2.61742004498719,0.615304998560408,
8.82945683644722));
#396212=CARTESIAN_POINT('Ctrl Pts',(-2.62183576488799,0.619199995254543,
8.83607469902389));
#396213=CARTESIAN_POINT('Ctrl Pts',(-2.61774715137787,0.626737586518493,
8.8382956714852));
#396214=CARTESIAN_POINT('Ctrl Pts',(-2.59952233059431,0.59951786985688,
8.85049129520029));
#396215=CARTESIAN_POINT('Ctrl Pts',(-2.6039016990888,0.603380801879653,
8.85711686593484));
#396216=CARTESIAN_POINT('Ctrl Pts',(-2.59985800069653,0.610914012710784,
8.85933012996512));
#396217=CARTESIAN_POINT('Origin',(-2.64486866084451,0.656184713158493,8.78727029226991));
#396218=CARTESIAN_POINT('Ctrl Pts',(-2.66351470618408,0.655963977306816,
8.75374538247848));
#396219=CARTESIAN_POINT('Ctrl Pts',(-2.66922216072437,0.660980882832946,
8.75304829418602));
#396220=CARTESIAN_POINT('Ctrl Pts',(-2.66734493414156,0.668379981667657,
8.75272238421917));
#396221=CARTESIAN_POINT('Ctrl Pts',(-2.66450461662075,0.65683715211257,
8.76769408445019));
#396222=CARTESIAN_POINT('Ctrl Pts',(-2.67035524042678,0.661980823569082,
8.76974318093969));
#396223=CARTESIAN_POINT('Ctrl Pts',(-2.66867262963315,0.669342017643231,
8.7707786988043));
#396224=CARTESIAN_POINT('Ctrl Pts',(-2.65943089964689,0.652361755462014,
8.78108014887991));
#396225=CARTESIAN_POINT('Ctrl Pts',(-2.66439160120751,0.656717978289954,
8.78639403366325));
#396226=CARTESIAN_POINT('Ctrl Pts',(-2.66187669989166,0.664411959515594,
8.78812224174741));
#396227=CARTESIAN_POINT('Ctrl Pts',(-2.6511161975379,0.645027568331988,
8.78944554828685));
#396228=CARTESIAN_POINT('Ctrl Pts',(-2.65530058650936,0.648694625265341,
8.79673892988685));
#396229=CARTESIAN_POINT('Ctrl Pts',(-2.65076059570256,0.656368740054075,
8.79894799272499));
#396230=CARTESIAN_POINT('Origin',(-2.65538477227091,0.665460713484845,8.75721825406948));
#396231=CARTESIAN_POINT('Origin',(-2.65538477227091,0.665460713484845,9.));
#396232=CARTESIAN_POINT('Origin',(-2.65538477227091,0.665460713484844,7.51860402984325));
#396233=CARTESIAN_POINT('Ctrl Pts',(-2.66850704020453,0.649186299013225,
7.50366195182966));
#396234=CARTESIAN_POINT('Ctrl Pts',(-2.67206521266982,0.650051920418533,
7.50000065167735));
#396235=CARTESIAN_POINT('Ctrl Pts',(-2.67206521266979,0.650051920418647,
7.49482233047108));
#396236=CARTESIAN_POINT('Ctrl Pts',(-2.6682462613492,0.656621740761716,
7.50215800491337));
#396237=CARTESIAN_POINT('Ctrl Pts',(-2.6698116696186,0.65931510188205,7.49877273257264));
#396238=CARTESIAN_POINT('Ctrl Pts',(-2.66899567098828,0.662669398020626,
7.49481816995647));
#396239=CARTESIAN_POINT('Ctrl Pts',(-2.66576757595734,0.657950700907936,
7.51043025814041));
#396240=CARTESIAN_POINT('Ctrl Pts',(-2.66892202800129,0.662864171096034,
7.51006209594515));
#396241=CARTESIAN_POINT('Ctrl Pts',(-2.6675092014202,0.66850180279862,7.50731281821699));
#396242=CARTESIAN_POINT('Ctrl Pts',(-2.66365244482109,0.656085448656425,
7.51860402984325));
#396243=CARTESIAN_POINT('Ctrl Pts',(-2.66935955988637,0.661118326066235,
7.51860402984324));
#396244=CARTESIAN_POINT('Ctrl Pts',(-2.66750981689315,0.668499346879757,
7.51860402984325));
#396245=CARTESIAN_POINT('Origin',(0.,0.,7.5));
#396246=CARTESIAN_POINT('Origin',(-2.6325925749723,0.431734128529216,7.5));
#396247=CARTESIAN_POINT('',(-2.6325925749723,0.431734128529216,7.59394543036555));
#396248=CARTESIAN_POINT('',(-2.6325925749723,0.431734128529216,8.85049129520029));
#396249=CARTESIAN_POINT('',(-2.6325925749723,0.431734128529216,7.5));
#396250=CARTESIAN_POINT('',(-2.68912759914126,0.475494405483839,8.78727029226991));
#396251=CARTESIAN_POINT('Ctrl Pts',(-2.63259257497231,0.431734128529216,
8.85049129520029));
#396252=CARTESIAN_POINT('Ctrl Pts',(-2.65146497607287,0.446342090780926,
8.82945686509571));
#396253=CARTESIAN_POINT('Ctrl Pts',(-2.6703093210672,0.460928336530387,
8.80838212259897));
#396254=CARTESIAN_POINT('Ctrl Pts',(-2.68912759914126,0.475494405483838,
8.78727029226991));
#396255=CARTESIAN_POINT('',(-2.70021641947034,0.48407757770024,8.75721825406948));
#396256=CARTESIAN_POINT('Origin',(-2.66684643588357,0.45824767539555,8.75937679713099));
#396257=CARTESIAN_POINT('',(-2.70021641947034,0.48407757770024,7.51860402984325));
#396258=CARTESIAN_POINT('',(-2.70021641947034,0.48407757770024,7.5));
#396259=CARTESIAN_POINT('Ctrl Pts',(-2.70021641947034,0.48407757770024,
7.51860402984325));
#396260=CARTESIAN_POINT('Ctrl Pts',(-2.69150787573963,0.47733683086004,
7.52834476460825));
#396261=CARTESIAN_POINT('Ctrl Pts',(-2.68279367854799,0.470591708024255,
7.53807742314407));
#396262=CARTESIAN_POINT('Ctrl Pts',(-2.67407363807296,0.463842062263019,
7.54780169004674));
#396263=CARTESIAN_POINT('Ctrl Pts',(-2.66026156523847,0.453150988164448,
7.5632044032688));
#396264=CARTESIAN_POINT('Ctrl Pts',(-2.64643481479703,0.4424485530352,7.57858609112103));
#396265=CARTESIAN_POINT('Ctrl Pts',(-2.6325925749723,0.431734128529216,
7.59394543036555));
#396266=CARTESIAN_POINT('Origin',(-2.89394790158701,0.328585663527346,7.5));
#396267=CARTESIAN_POINT('',(-2.71519273396521,0.391443777101987,8.75721825406948));
#396268=CARTESIAN_POINT('',(-2.70196419720223,0.396095507607665,8.78727029226991));
#396269=CARTESIAN_POINT('Origin',(-2.66838523689962,0.40790333464003,8.75658640621052));
#396270=CARTESIAN_POINT('',(-2.6345200847159,0.419811799220425,8.85049129520029));
#396271=CARTESIAN_POINT('Ctrl Pts',(-2.70196419720223,0.396095507607665,
8.78727029226991));
#396272=CARTESIAN_POINT('Ctrl Pts',(-2.67951471421566,0.403989724989103,
8.80838212259896));
#396273=CARTESIAN_POINT('Ctrl Pts',(-2.65703413439438,0.411894877373953,
8.82945686509571));
#396274=CARTESIAN_POINT('Ctrl Pts',(-2.63452008471591,0.419811799220425,
8.85049129520029));
#396275=CARTESIAN_POINT('',(-2.6345200847159,0.419811799220425,7.59394543036555));
#396276=CARTESIAN_POINT('',(-2.6345200847159,0.419811799220425,7.5));
#396277=CARTESIAN_POINT('',(-2.71519273396521,0.391443777101987,7.51860402984325));
#396278=CARTESIAN_POINT('Ctrl Pts',(-2.63452008471591,0.419811799220425,
7.59394543036555));
#396279=CARTESIAN_POINT('Ctrl Pts',(-2.65103334518629,0.414005016591735,
7.57858609112103));
#396280=CARTESIAN_POINT('Ctrl Pts',(-2.66752812741711,0.408204731718043,
7.56320440326857));
#396281=CARTESIAN_POINT('Ctrl Pts',(-2.68400539982677,0.402410604061165,
7.54780169004651));
#396282=CARTESIAN_POINT('Ctrl Pts',(-2.69440807320188,0.39875257037636,
7.53807742314383));
#396283=CARTESIAN_POINT('Ctrl Pts',(-2.70480377576452,0.395096987933257,
7.52834476460825));
#396284=CARTESIAN_POINT('Ctrl Pts',(-2.71519273396521,0.391443777101987,
7.51860402984325));
#396285=CARTESIAN_POINT('',(-2.71519273396521,0.391443777101987,7.5));
#396286=CARTESIAN_POINT('Origin',(-2.63680073810823,0.426297494642203,7.5));
#396287=CARTESIAN_POINT('Ctrl Pts',(-2.6345200847159,0.419811799220425,
8.85049129520029));
#396288=CARTESIAN_POINT('Ctrl Pts',(-2.63433738950975,0.419876042823397,
8.85097269580139));
#396289=CARTESIAN_POINT('Ctrl Pts',(-2.6341597896714,0.41994741098124,8.85143669361005));
#396290=CARTESIAN_POINT('Ctrl Pts',(-2.63397943329584,0.420030001202733,
8.8519052845931));
#396291=CARTESIAN_POINT('Ctrl Pts',(-2.63362666766303,0.420191542438292,
8.85282181883899));
#396292=CARTESIAN_POINT('Ctrl Pts',(-2.63327251305848,0.420392039188358,
8.85372622499635));
#396293=CARTESIAN_POINT('Ctrl Pts',(-2.63291900834655,0.420648055336189,
8.8546225773507));
#396294=CARTESIAN_POINT('Ctrl Pts',(-2.63262554129001,0.420860590849287,
8.85536669723986));
#396295=CARTESIAN_POINT('Ctrl Pts',(-2.63233243666767,0.421111411701283,
8.85610498449051));
#396296=CARTESIAN_POINT('Ctrl Pts',(-2.63204603916861,0.421416096159162,
8.85681338218371));
#396297=CARTESIAN_POINT('Ctrl Pts',(-2.63178613298843,0.421692597783202,
8.85745625420284));
#396298=CARTESIAN_POINT('Ctrl Pts',(-2.63152805418393,0.422016517790465,
8.85808743050665));
#396299=CARTESIAN_POINT('Ctrl Pts',(-2.63128428509418,0.422413586267619,
8.8586680450841));
#396300=CARTESIAN_POINT('Ctrl Pts',(-2.63117181532044,0.422596785055589,
8.85893592806395));
#396301=CARTESIAN_POINT('Ctrl Pts',(-2.63106252270618,0.422795758835443,
8.85919241173848));
#396302=CARTESIAN_POINT('Ctrl Pts',(-2.63095867528155,0.42301424364999,
8.85943017985534));
#396303=CARTESIAN_POINT('Ctrl Pts',(-2.63081845051617,0.423309262828054,
8.8597512372));
#396304=CARTESIAN_POINT('Ctrl Pts',(-2.6306851634031,0.42364764044822,8.86004599534706));
#396305=CARTESIAN_POINT('Ctrl Pts',(-2.63057010575534,0.424029128091272,
8.86026130871721));
#396306=CARTESIAN_POINT('Ctrl Pts',(-2.63052797990667,0.424168801472668,
8.86034014101235));
#396307=CARTESIAN_POINT('Ctrl Pts',(-2.63048765313902,0.424316348233932,
8.86040910639692));
#396308=CARTESIAN_POINT('Ctrl Pts',(-2.63045054861005,0.424467837231008,
8.86046313645506));
#396309=CARTESIAN_POINT('Ctrl Pts',(-2.63039264730333,0.424704234542235,
8.86054744990829));
#396310=CARTESIAN_POINT('Ctrl Pts',(-2.63034115486745,0.424956719642246,
8.86059655985668));
#396311=CARTESIAN_POINT('Ctrl Pts',(-2.63029908662039,0.425209041351492,
8.86059725258816));
#396312=CARTESIAN_POINT('Ctrl Pts',(-2.63025692117888,0.425461946024691,
8.86059794692011));
#396313=CARTESIAN_POINT('Ctrl Pts',(-2.63022637650186,0.425717928210008,
8.86056369958366));
#396314=CARTESIAN_POINT('Ctrl Pts',(-2.6302053819192,0.425962580651799,
8.86048590497774));
#396315=CARTESIAN_POINT('Ctrl Pts',(-2.63019990295821,0.426026427654925,
8.86046560290182));
#396316=CARTESIAN_POINT('Ctrl Pts',(-2.63019509337987,0.426090341398228,
8.86044257503091));
#396317=CARTESIAN_POINT('Ctrl Pts',(-2.63019106907052,0.426152344430887,
8.86041778462584));
#396318=CARTESIAN_POINT('Ctrl Pts',(-2.63016399046235,0.426569547901336,
8.86025097596201));
#396319=CARTESIAN_POINT('Ctrl Pts',(-2.63016916344615,0.426956246327054,
8.8599848982295));
#396320=CARTESIAN_POINT('Ctrl Pts',(-2.6301979653053,0.427301266325953,
8.85968173251462));
#396321=CARTESIAN_POINT('Ctrl Pts',(-2.63021319983864,0.427483762138081,
8.85952137522077));
#396322=CARTESIAN_POINT('Ctrl Pts',(-2.63023514862655,0.427658130768826,
8.85934740853961));
#396323=CARTESIAN_POINT('Ctrl Pts',(-2.63026195976158,0.42782210738347,
8.8591675900182));
#396324=CARTESIAN_POINT('Ctrl Pts',(-2.63036962040486,0.428480558724614,
8.85844552518695));
#396325=CARTESIAN_POINT('Ctrl Pts',(-2.63055878195666,0.429009147469447,
8.85759444184123));
#396326=CARTESIAN_POINT('Ctrl Pts',(-2.6307517253384,0.429426277073954,
8.85683498915138));
#396327=CARTESIAN_POINT('Ctrl Pts',(-2.63077191634944,0.429469928576157,
8.85675551444997));
#396328=CARTESIAN_POINT('Ctrl Pts',(-2.63079216490732,0.429512347712904,
8.85667699793651));
#396329=CARTESIAN_POINT('Ctrl Pts',(-2.63081239214286,0.429553547296386,
8.85659965593547));
#396330=CARTESIAN_POINT('Ctrl Pts',(-2.63108542040041,0.43010966137655,
8.85555568965886));
#396331=CARTESIAN_POINT('Ctrl Pts',(-2.63142813134851,0.430604690778885,
8.85434650606346));
#396332=CARTESIAN_POINT('Ctrl Pts',(-2.63183710943965,0.431044620128043,
8.85297329937117));
#396333=CARTESIAN_POINT('Ctrl Pts',(-2.63206713469651,0.431292053581656,
8.85220095427747));
#396334=CARTESIAN_POINT('Ctrl Pts',(-2.63231844750382,0.431521943355189,
8.85137579139183));
#396335=CARTESIAN_POINT('Ctrl Pts',(-2.6325925749723,0.431734128529216,
8.85049129520029));
#396336=CARTESIAN_POINT('Origin',(-2.63680073810823,0.426297494642203,7.59394543036555));
#396337=CARTESIAN_POINT('Ctrl Pts',(-2.6339896589008,0.419998320072227,
7.59443877723642));
#396338=CARTESIAN_POINT('Ctrl Pts',(-2.62852678336725,0.421919305380237,
7.58783886950016));
#396339=CARTESIAN_POINT('Ctrl Pts',(-2.62941353036882,0.430362815390407,
7.58559994247159));
#396340=CARTESIAN_POINT('Ctrl Pts',(-2.66381133616454,0.409511717635108,
7.56670252222138));
#396341=CARTESIAN_POINT('Ctrl Pts',(-2.65835635603707,0.411429926574002,
7.56004874999029));
#396342=CARTESIAN_POINT('Ctrl Pts',(-2.65922710860603,0.419925698888489,
7.55786368756704));
#396343=CARTESIAN_POINT('Ctrl Pts',(-2.69357732442549,0.399044697880317,
7.53888913333559));
#396344=CARTESIAN_POINT('Ctrl Pts',(-2.68808992508402,0.400974306828835,
7.53222002137275));
#396345=CARTESIAN_POINT('Ctrl Pts',(-2.68898568384657,0.409506602004173,
7.53005029815327));
#396346=CARTESIAN_POINT('Ctrl Pts',(-2.72328627675262,0.388597734447555,
7.51101258149734));
#396347=CARTESIAN_POINT('Ctrl Pts',(-2.7177323601603,0.390550733762701,
7.5043616886572));
#396348=CARTESIAN_POINT('Ctrl Pts',(-2.71868781310115,0.399106117519288,
7.50217374673251));
#396349=CARTESIAN_POINT('',(-2.71710286899021,0.399661099761597,7.50366116523517));
#396350=CARTESIAN_POINT('Ctrl Pts',(-2.71519273396521,0.391443777101986,
7.51860402984325));
#396351=CARTESIAN_POINT('Ctrl Pts',(-2.71560933845096,0.391297280794053,
7.51734760759494));
#396352=CARTESIAN_POINT('Ctrl Pts',(-2.71600553713428,0.391221028165823,
7.51608817408573));
#396353=CARTESIAN_POINT('Ctrl Pts',(-2.71638294247708,0.39122830759426,
7.5148100591312));
#396354=CARTESIAN_POINT('Ctrl Pts',(-2.71672480525499,0.391234901474485,
7.51365231206384));
#396355=CARTESIAN_POINT('Ctrl Pts',(-2.7170517344872,0.391309793993984,
7.51247773061042));
#396356=CARTESIAN_POINT('Ctrl Pts',(-2.71734982796114,0.39148768196033,
7.51129758471022));
#396357=CARTESIAN_POINT('Ctrl Pts',(-2.71772032410568,0.391708776386926,
7.50983079813401));
#396358=CARTESIAN_POINT('Ctrl Pts',(-2.71802777713899,0.39209310294452,
7.50839324291155));
#396359=CARTESIAN_POINT('Ctrl Pts',(-2.7182100557827,0.392694965359674,
7.50715379678855));
#396360=CARTESIAN_POINT('Ctrl Pts',(-2.71829426326387,0.392973008453226,
7.50658120839351));
#396361=CARTESIAN_POINT('Ctrl Pts',(-2.71835463339421,0.393339757954573,
7.50598221009429));
#396362=CARTESIAN_POINT('Ctrl Pts',(-2.71836728500343,0.39379018029319,
7.50545747549611));
#396363=CARTESIAN_POINT('Ctrl Pts',(-2.71837403629372,0.394030539594952,
7.50517746087247));
#396364=CARTESIAN_POINT('Ctrl Pts',(-2.71836747479092,0.39429732640831,
7.50491486231392));
#396365=CARTESIAN_POINT('Ctrl Pts',(-2.71834610674268,0.394583434757215,
7.50468370960992));
#396366=CARTESIAN_POINT('Ctrl Pts',(-2.71831415477038,0.395011256986588,
7.50433806340447));
#396367=CARTESIAN_POINT('Ctrl Pts',(-2.71824758258208,0.395495068861645,
7.50405484070984));
#396368=CARTESIAN_POINT('Ctrl Pts',(-2.71815016398297,0.396002188896854,
7.50385766036131));
#396369=CARTESIAN_POINT('Ctrl Pts',(-2.71813974657802,0.39605641750219,
7.50383657498791));
#396370=CARTESIAN_POINT('Ctrl Pts',(-2.71812899521642,0.396110891374383,
7.50381643264937));
#396371=CARTESIAN_POINT('Ctrl Pts',(-2.71811792839077,0.39616555531703,
7.50379723213559));
#396372=CARTESIAN_POINT('Ctrl Pts',(-2.71804405370936,0.396530455016013,
7.50366906242519));
#396373=CARTESIAN_POINT('Ctrl Pts',(-2.71795381025398,0.396911618989251,
7.50358235568538));
#396374=CARTESIAN_POINT('Ctrl Pts',(-2.71785799524629,0.397276923242083,
7.5035341175365));
#396375=CARTESIAN_POINT('Ctrl Pts',(-2.71771433148642,0.397824655624746,
7.50346178989176));
#396376=CARTESIAN_POINT('Ctrl Pts',(-2.71753649302518,0.398407782609535,
7.50346967198527));
#396377=CARTESIAN_POINT('Ctrl Pts',(-2.7173442964507,0.398974860740847,
7.50354272648692));
#396378=CARTESIAN_POINT('Ctrl Pts',(-2.71726524202138,0.399208111714077,
7.50357277531559));
#396379=CARTESIAN_POINT('Ctrl Pts',(-2.71718399774964,0.39943838306783,
7.50361331098761));
#396380=CARTESIAN_POINT('Ctrl Pts',(-2.71710286899161,0.399661099761803,
7.50366116523659));
#396381=CARTESIAN_POINT('',(-2.63969113251167,0.426764791194204,7.57603338622103));
#396382=CARTESIAN_POINT('Origin',(-2.64841434182066,0.428177982249233,7.58486873427627));
#396383=CARTESIAN_POINT('Ctrl Pts',(-2.71710286904232,0.399661099737671,
7.50366116529969));
#396384=CARTESIAN_POINT('Ctrl Pts',(-2.69134133975362,0.408681709889307,
7.52783573079709));
#396385=CARTESIAN_POINT('Ctrl Pts',(-2.66553865185168,0.417715864046332,
7.55196141284068));
#396386=CARTESIAN_POINT('Ctrl Pts',(-2.63969113352841,0.426764790463535,
7.57603338728831));
#396387=CARTESIAN_POINT('Ctrl Pts',(-2.6355485822783,0.419636504370411,
7.59639677331371));
#396388=CARTESIAN_POINT('Ctrl Pts',(-2.61671933910964,0.42305088978551,
7.59974925422225));
#396389=CARTESIAN_POINT('Ctrl Pts',(-2.63351343964677,0.43222458114812,
7.59639677331372));
#396390=CARTESIAN_POINT('Ctrl Pts',(-2.63164855597479,0.419706496625095,
7.58707626057422));
#396391=CARTESIAN_POINT('Ctrl Pts',(-2.62689172333806,0.424695481979636,
7.58811717123965));
#396392=CARTESIAN_POINT('Ctrl Pts',(-2.62983415240462,0.430929224257757,
7.58707626057423));
#396393=CARTESIAN_POINT('Ctrl Pts',(-2.63596724991744,0.423981366785865,
7.58015376756929));
#396394=CARTESIAN_POINT('Ctrl Pts',(-2.63371451346331,0.425798537775723,
7.5820876076604));
#396395=CARTESIAN_POINT('Ctrl Pts',(-2.63527988042915,0.428232990116566,
7.5801537675693));
#396396=CARTESIAN_POINT('Ctrl Pts',(-2.63969113169474,0.426764791061924,
7.57603338509286));
#396397=CARTESIAN_POINT('Ctrl Pts',(-2.63969113169474,0.426764791061924,
7.57603338509286));
#396398=CARTESIAN_POINT('Ctrl Pts',(-2.63969113169474,0.426764791061924,
7.57603338509286));
#396399=CARTESIAN_POINT('Origin',(-2.64841525255382,0.428172349042207,7.5848687342762));
#396400=CARTESIAN_POINT('Ctrl Pts',(-2.70702227397444,0.489345570106541,
7.51098857897448));
#396401=CARTESIAN_POINT('Ctrl Pts',(-2.70236668241661,0.485741963688167,
7.50433767179956));
#396402=CARTESIAN_POINT('Ctrl Pts',(-2.70596936051755,0.477923475241962,
7.50214974420965));
#396403=CARTESIAN_POINT('Ctrl Pts',(-2.68211158316672,0.470063740039235,
7.53887321589164));
#396404=CARTESIAN_POINT('Ctrl Pts',(-2.67751177385793,0.466503311220993,
7.53220407452058));
#396405=CARTESIAN_POINT('Ctrl Pts',(-2.6810504968683,0.458687918756245,
7.53003438070911));
#396406=CARTESIAN_POINT('Ctrl Pts',(-2.65715305464352,0.450744881745466,
7.56669465659234));
#396407=CARTESIAN_POINT('Ctrl Pts',(-2.65258042935257,0.447205494399617,
7.56004085833301));
#396408=CARTESIAN_POINT('Ctrl Pts',(-2.6560839004508,0.439416891162178,
7.55785582193789));
#396409=CARTESIAN_POINT('Ctrl Pts',(-2.63214781717911,0.431389868939804,
7.59443891967696));
#396410=CARTESIAN_POINT('Ctrl Pts',(-2.6275685621508,0.427845349922958,
7.58783901202978));
#396411=CARTESIAN_POINT('Ctrl Pts',(-2.6310707537066,0.420111409640359,
7.58560008491213));
#396412=CARTESIAN_POINT('',(-2.70461858999357,0.476880779649006,7.50366116523517));
#396413=CARTESIAN_POINT('Ctrl Pts',(-2.70461858999394,0.476880779649071,
7.50366116523554));
#396414=CARTESIAN_POINT('Ctrl Pts',(-2.70464020690383,0.477638189858912,
7.50350835821027));
#396415=CARTESIAN_POINT('Ctrl Pts',(-2.70463543653969,0.478335136955017,
7.50345484956));
#396416=CARTESIAN_POINT('Ctrl Pts',(-2.70460473756223,0.478992345851155,
7.50349758195598));
#396417=CARTESIAN_POINT('Ctrl Pts',(-2.7045889867101,0.479329542754757,
7.50351950684424));
#396418=CARTESIAN_POINT('Ctrl Pts',(-2.70456498711403,0.479689520295352,
7.50357029184312));
#396419=CARTESIAN_POINT('Ctrl Pts',(-2.70453230288058,0.480036006358231,
7.50365515313923));
#396420=CARTESIAN_POINT('Ctrl Pts',(-2.70448202129437,0.480569042228999,
7.50378570417639));
#396421=CARTESIAN_POINT('Ctrl Pts',(-2.7044100554912,0.481085827292577,
7.50400001621911));
#396422=CARTESIAN_POINT('Ctrl Pts',(-2.70431963439798,0.481546713552103,
7.50428903009634));
#396423=CARTESIAN_POINT('Ctrl Pts',(-2.70430959835229,0.481597868381067,
7.50432110841318));
#396424=CARTESIAN_POINT('Ctrl Pts',(-2.70429934703203,0.48164836238024,
7.50435406373354));
#396425=CARTESIAN_POINT('Ctrl Pts',(-2.7042888934907,0.481698161980497,
7.50438785222352));
#396426=CARTESIAN_POINT('Ctrl Pts',(-2.70422506959627,0.482002212476779,
7.50459414719561));
#396427=CARTESIAN_POINT('Ctrl Pts',(-2.7041521866378,0.482285112778662,
7.50483629897752));
#396428=CARTESIAN_POINT('Ctrl Pts',(-2.704074311158,0.482536353384309,7.5050991045531));
#396429=CARTESIAN_POINT('Ctrl Pts',(-2.70390251002772,0.483090615395093,
7.50567888004914));
#396430=CARTESIAN_POINT('Ctrl Pts',(-2.70370013790804,0.483512788619073,
7.50637912803145));
#396431=CARTESIAN_POINT('Ctrl Pts',(-2.70349061296512,0.483823047491813,
7.50710440483569));
#396432=CARTESIAN_POINT('Ctrl Pts',(-2.70343923328946,0.48389912912691,
7.50728225710685));
#396433=CARTESIAN_POINT('Ctrl Pts',(-2.70338652163312,0.483970077276568,
7.50746498566954));
#396434=CARTESIAN_POINT('Ctrl Pts',(-2.70333404285786,0.484034484228099,
7.50764697238949));
#396435=CARTESIAN_POINT('Ctrl Pts',(-2.70305193140459,0.48438071827426,
7.50862528291182));
#396436=CARTESIAN_POINT('Ctrl Pts',(-2.70275414916696,0.484571966827631,
7.50965856837422));
#396437=CARTESIAN_POINT('Ctrl Pts',(-2.70246021538533,0.484671589142456,
7.51067959873202));
#396438=CARTESIAN_POINT('Ctrl Pts',(-2.70229846325455,0.484726411427962,
7.51124147302579));
#396439=CARTESIAN_POINT('Ctrl Pts',(-2.70213769764104,0.484753088363612,
7.51180065547253));
#396440=CARTESIAN_POINT('Ctrl Pts',(-2.70198039405431,0.484759576290781,
7.51235175716501));
#396441=CARTESIAN_POINT('Ctrl Pts',(-2.70143684749985,0.484781994663633,
7.51425603304536));
#396442=CARTESIAN_POINT('Ctrl Pts',(-2.70086957912378,0.484559974355621,
7.5162690050518));
#396443=CARTESIAN_POINT('Ctrl Pts',(-2.70030761830454,0.484146430039397,
7.51827788969244));
#396444=CARTESIAN_POINT('Ctrl Pts',(-2.70027720392305,0.484124048239512,
7.51838661432545));
#396445=CARTESIAN_POINT('Ctrl Pts',(-2.70024680297323,0.484101095696761,
7.51849533314856));
#396446=CARTESIAN_POINT('Ctrl Pts',(-2.70021641947034,0.484077577700244,
7.51860402984325));
#396447=CARTESIAN_POINT('Ctrl Pts',(-2.63969113324751,0.426764792208463,
7.57603338728985));
#396448=CARTESIAN_POINT('Ctrl Pts',(-2.66137047798473,0.443497493271876,
7.55196141284922));
#396449=CARTESIAN_POINT('Ctrl Pts',(-2.68301193102658,0.460202048212608,
7.52783573083104));
#396450=CARTESIAN_POINT('Ctrl Pts',(-2.7046185900369,0.476880779689317,
7.50366116530176));
#396451=CARTESIAN_POINT('Origin',(-9.12135307609333E-16,1.47466962819317E-16,
7.49482233047033));
#396452=CARTESIAN_POINT('Origin',(-2.70835812744774,0.398374827879188,7.49482233047033));
#396453=CARTESIAN_POINT('Origin',(0.,0.,7.50366116523517));
#396454=CARTESIAN_POINT('Origin',(-2.69591402793581,0.475345983446701,7.49482233047033));
#396455=CARTESIAN_POINT('Ctrl Pts',(-2.7151917361247,0.391444127938797,
7.51860402984325));
#396456=CARTESIAN_POINT('Ctrl Pts',(-2.72237004465166,0.388920604068936,
7.51860402984325));
#396457=CARTESIAN_POINT('Ctrl Pts',(-2.72342529733067,0.381385172574091,
7.51860402984325));
#396458=CARTESIAN_POINT('Ctrl Pts',(-2.71785709064666,0.390507125105682,
7.51041458714365));
#396459=CARTESIAN_POINT('Ctrl Pts',(-2.7226200362942,0.387135372665384,
7.51004642900441));
#396460=CARTESIAN_POINT('Ctrl Pts',(-2.72342558835683,0.381383094391554,
7.50729136483009));
#396461=CARTESIAN_POINT('Ctrl Pts',(-2.71964944662411,0.392677654361255,
7.50215815450138));
#396462=CARTESIAN_POINT('Ctrl Pts',(-2.72211116740598,0.390770301411846,
7.49877163671532));
#396463=CARTESIAN_POINT('Ctrl Pts',(-2.72261327489375,0.387356826398741,
7.49481588533172));
#396464=CARTESIAN_POINT('Ctrl Pts',(-2.71710232433262,0.399661019647903,
7.50366171572174));
#396465=CARTESIAN_POINT('Ctrl Pts',(-2.72072505953649,0.400193891020572,
7.50000045605858));
#396466=CARTESIAN_POINT('Ctrl Pts',(-2.72072505953651,0.400193891020448,
7.49482233047317));
#396467=CARTESIAN_POINT('Origin',(-2.71104609143371,0.379651603607846,7.51860402984325));
#396468=CARTESIAN_POINT('Origin',(-2.71104609143371,0.379651603607846,9.));
#396469=CARTESIAN_POINT('Origin',(-2.71104609143371,0.379651603607846,8.75721825406948));
#396470=CARTESIAN_POINT('Ctrl Pts',(-2.69943822817004,0.396983716469052,
8.78942910404912));
#396471=CARTESIAN_POINT('Ctrl Pts',(-2.70470182062058,0.395154229323329,
8.7967269950169));
#396472=CARTESIAN_POINT('Ctrl Pts',(-2.70336947938123,0.386328224972321,
8.79893251111267));
#396473=CARTESIAN_POINT('Ctrl Pts',(-2.70980999884857,0.393336554321251,
8.78111911759583));
#396474=CARTESIAN_POINT('Ctrl Pts',(-2.71604760481807,0.391160644880466,
8.78644465894814));
#396475=CARTESIAN_POINT('Ctrl Pts',(-2.71658483983411,0.383071955844967,
8.78817647674132));
#396476=CARTESIAN_POINT('Ctrl Pts',(-2.71627393371497,0.391063555847688,
8.76780923932029));
#396477=CARTESIAN_POINT('Ctrl Pts',(-2.72363548577431,0.388490175182464,
8.76988516158374));
#396478=CARTESIAN_POINT('Ctrl Pts',(-2.72483625397649,0.381027297981215,
8.77093053738832));
#396479=CARTESIAN_POINT('Ctrl Pts',(-2.7150135548806,0.391506759440228,
8.75371302330492));
#396480=CARTESIAN_POINT('Ctrl Pts',(-2.72219468292134,0.388997257212635,
8.75300828287559));
#396481=CARTESIAN_POINT('Ctrl Pts',(-2.72322678304317,0.381425645186602,
8.75267964240738));
#396482=CARTESIAN_POINT('Origin',(-2.69781755467073,0.384303334113524,8.78727029226991));
#396483=CARTESIAN_POINT('Ctrl Pts',(-2.63452008471591,0.419811799220425,
8.85049129520029));
#396484=CARTESIAN_POINT('Ctrl Pts',(-2.64002902569028,0.417874615294219,
8.85711686593484));
#396485=CARTESIAN_POINT('Ctrl Pts',(-2.63910781935456,0.409374489353921,
8.85933012996512));
#396486=CARTESIAN_POINT('Ctrl Pts',(-2.65703416460908,0.411894866749149,
8.82945683644722));
#396487=CARTESIAN_POINT('Ctrl Pts',(-2.66258883312432,0.409941603025127,
8.83607469902391));
#396488=CARTESIAN_POINT('Ctrl Pts',(-2.66162763804508,0.401420561626479,
8.8382956714852));
#396489=CARTESIAN_POINT('Ctrl Pts',(-2.67951468545063,0.403989735104143,
8.80838214965003));
#396490=CARTESIAN_POINT('Ctrl Pts',(-2.68509127528126,0.402028762889477,
8.8150136446199));
#396491=CARTESIAN_POINT('Ctrl Pts',(-2.68411351798304,0.393479329969056,
8.81722098428721));
#396492=CARTESIAN_POINT('Ctrl Pts',(-2.70196419720223,0.396095507607664,
8.78727029226991));
#396493=CARTESIAN_POINT('Ctrl Pts',(-2.70754171332274,0.394134209669084,
8.79393457792714));
#396494=CARTESIAN_POINT('Ctrl Pts',(-2.7065680531042,0.385549840096597,
8.79610912703474));
#396495=CARTESIAN_POINT('Origin',(-2.6303734421844,0.408019625726284,8.85049129520029));
#396496=CARTESIAN_POINT('Ctrl Pts',(-2.6325925749723,0.431734128529216,
8.85049129520029));
#396497=CARTESIAN_POINT('Ctrl Pts',(-2.63721044448901,0.435308536641031,
8.85711686593484));
#396498=CARTESIAN_POINT('Ctrl Pts',(-2.63365770878388,0.443085350328103,
8.85933012996512));
#396499=CARTESIAN_POINT('Ctrl Pts',(-2.62850721247053,0.428571901269819,
8.86332496987231));
#396500=CARTESIAN_POINT('Ctrl Pts',(-2.62804976815553,0.433170013825585,
8.86648636486736));
#396501=CARTESIAN_POINT('Ctrl Pts',(-2.62223922743675,0.434225342422805,
8.87206031107457));
#396502=CARTESIAN_POINT('Ctrl Pts',(-2.62961328596242,0.42153724367855,
8.86341338519877));
#396503=CARTESIAN_POINT('Ctrl Pts',(-2.63060202922408,0.417010008606594,
8.86654584966058));
#396504=CARTESIAN_POINT('Ctrl Pts',(-2.62537340940882,0.414219724102341,
8.87215952290714));
#396505=CARTESIAN_POINT('Ctrl Pts',(-2.6345200847159,0.419811799220425,
8.85049129520029));
#396506=CARTESIAN_POINT('Ctrl Pts',(-2.64002902569028,0.417874615294219,
8.85711686593485));
#396507=CARTESIAN_POINT('Ctrl Pts',(-2.63910781935455,0.409374489353921,
8.85933012996512));
#396508=CARTESIAN_POINT('Origin',(-2.62494136927062,0.441618917414695,8.85049129520029));
#396509=CARTESIAN_POINT('Ctrl Pts',(-2.68912759914126,0.475494405483839,
8.78727029226991));
#396510=CARTESIAN_POINT('Ctrl Pts',(-2.69380295177104,0.479113307729781,
8.79393457792714));
#396511=CARTESIAN_POINT('Ctrl Pts',(-2.69017388854615,0.486953544670587,
8.79610912703474));
#396512=CARTESIAN_POINT('Ctrl Pts',(-2.67030929695491,0.460928317866552,
8.80838214965004));
#396513=CARTESIAN_POINT('Ctrl Pts',(-2.67498387312222,0.464546619100771,
8.81501364461989));
#396514=CARTESIAN_POINT('Ctrl Pts',(-2.6713619303665,0.472352408187695,
8.81722098428721));
#396515=CARTESIAN_POINT('Ctrl Pts',(-2.65146500140035,0.44634211038536,
8.82945683644723));
#396516=CARTESIAN_POINT('Ctrl Pts',(-2.65612120202605,0.449946188245617,
8.83607469902389));
#396517=CARTESIAN_POINT('Ctrl Pts',(-2.65252392414128,0.457730251086941,
8.8382956714852));
#396518=CARTESIAN_POINT('Ctrl Pts',(-2.63259257497231,0.431734128529216,
8.85049129520029));
#396519=CARTESIAN_POINT('Ctrl Pts',(-2.63721044448901,0.435308536641031,
8.85711686593484));
#396520=CARTESIAN_POINT('Ctrl Pts',(-2.63365770878388,0.443085350328103,
8.85933012996512));
#396521=CARTESIAN_POINT('Origin',(-2.68147639343958,0.485379194369317,8.78727029226991));
#396522=CARTESIAN_POINT('Ctrl Pts',(-2.70006998588464,0.483964255816441,
8.75374538247848));
#396523=CARTESIAN_POINT('Ctrl Pts',(-2.70608714808814,0.488605175704185,
8.75304829418602));
#396524=CARTESIAN_POINT('Ctrl Pts',(-2.70468784035867,0.496109346616901,
8.75272238421917));
#396525=CARTESIAN_POINT('Ctrl Pts',(-2.70111380694607,0.484772212811493,
8.76769408445017));
#396526=CARTESIAN_POINT('Ctrl Pts',(-2.70728196617972,0.489530465289048,
8.76974318093969));
#396527=CARTESIAN_POINT('Ctrl Pts',(-2.70607444581406,0.496984340244175,
8.77077869880429));
#396528=CARTESIAN_POINT('Ctrl Pts',(-2.69576377481994,0.480631085505944,
8.78108014887993));
#396529=CARTESIAN_POINT('Ctrl Pts',(-2.70099338824204,0.484660524766653,
8.78639403366326));
#396530=CARTESIAN_POINT('Ctrl Pts',(-2.69897660913032,0.492499828163215,
8.78812224174742));
#396531=CARTESIAN_POINT('Ctrl Pts',(-2.68699625317539,0.47384469204318,
8.78944554828685));
#396532=CARTESIAN_POINT('Ctrl Pts',(-2.69140699401534,0.477236119892881,
8.79673892988686));
#396533=CARTESIAN_POINT('Ctrl Pts',(-2.68736801332924,0.485185345599439,
8.79894799272499));
#396534=CARTESIAN_POINT('Origin',(-2.69256521376866,0.493962366585719,8.75721825406948));
#396535=CARTESIAN_POINT('Origin',(-2.69256521376866,0.493962366585719,9.));
#396536=CARTESIAN_POINT('Origin',(-2.69256521376866,0.493962366585719,7.51860402984325));
#396537=CARTESIAN_POINT('Ctrl Pts',(-2.70461781528019,0.476880643050904,
7.50366195182966));
#396538=CARTESIAN_POINT('Ctrl Pts',(-2.70822413765239,0.477516513051618,
7.50000065167735));
#396539=CARTESIAN_POINT('Ctrl Pts',(-2.70822413765237,0.477516513051733,
7.49482233047108));
#396540=CARTESIAN_POINT('Ctrl Pts',(-2.70483396261147,0.484317516045507,
7.50215800491337));
#396541=CARTESIAN_POINT('Ctrl Pts',(-2.70656871882114,0.486905047314383,
7.49877273257267));
#396542=CARTESIAN_POINT('Ctrl Pts',(-2.70596930723901,0.490304732903542,
7.49481816995649));
#396543=CARTESIAN_POINT('Ctrl Pts',(-2.70244551671349,0.48580255561889,
7.51043025814043));
#396544=CARTESIAN_POINT('Ctrl Pts',(-2.70590829471324,0.490503824119143,
7.51006209594515));
#396545=CARTESIAN_POINT('Ctrl Pts',(-2.70485957523922,0.496220392812616,
7.50731281821699));
#396546=CARTESIAN_POINT('Ctrl Pts',(-2.70021522421893,0.48407665264536,
7.51860402984326));
#396547=CARTESIAN_POINT('Ctrl Pts',(-2.70623307096702,0.488733533351069,
7.51860402984327));
#396548=CARTESIAN_POINT('Ctrl Pts',(-2.70486003209637,0.496217902506207,
7.51860402984327));
#396549=CARTESIAN_POINT('Origin',(0.,0.,7.5));
#396550=CARTESIAN_POINT('Origin',(-2.6548449317704,0.262176299060745,7.5));
#396551=CARTESIAN_POINT('',(-2.6548449317704,0.262176299060745,7.59394543036555));
#396552=CARTESIAN_POINT('',(-2.6548449317704,0.262176299060745,8.85049129520029));
#396553=CARTESIAN_POINT('',(-2.6548449317704,0.262176299060745,7.5));
#396554=CARTESIAN_POINT('',(-2.71406752923974,0.30222445439797,8.78727029226991));
#396555=CARTESIAN_POINT('Ctrl Pts',(-2.6548449317704,0.262176299060745,
8.85049129520029));
#396556=CARTESIAN_POINT('Ctrl Pts',(-2.67461449285379,0.275545088797232,
8.82945686509571));
#396557=CARTESIAN_POINT('Ctrl Pts',(-2.69435466409413,0.288894004211245,
8.80838212259896));
#396558=CARTESIAN_POINT('Ctrl Pts',(-2.71406752923974,0.30222445439797,
8.78727029226991));
#396559=CARTESIAN_POINT('',(-2.72568349213022,0.310079528408699,8.75721825406948));
#396560=CARTESIAN_POINT('Origin',(-2.69072714323187,0.286440718598347,8.75937679713131));
#396561=CARTESIAN_POINT('',(-2.72568349213022,0.310079528408699,7.51860402984325));
#396562=CARTESIAN_POINT('',(-2.72568349213022,0.310079528408699,7.5));
#396563=CARTESIAN_POINT('Ctrl Pts',(-2.72568349213022,0.3100795284087,7.51860402984325));
#396564=CARTESIAN_POINT('Ctrl Pts',(-2.71656095990371,0.303910589468364,
7.52834476460825));
#396565=CARTESIAN_POINT('Ctrl Pts',(-2.70743250546091,0.297737645741883,
7.53807742314407));
#396566=CARTESIAN_POINT('Ctrl Pts',(-2.69829792995554,0.291560562763236,
7.54780169004674));
#396567=CARTESIAN_POINT('Ctrl Pts',(-2.6838292560367,0.28177639716791,7.5632044032688));
#396568=CARTESIAN_POINT('Ctrl Pts',(-2.6693452067639,0.271981834281868,
7.57858609112103));
#396569=CARTESIAN_POINT('Ctrl Pts',(-2.6548449317704,0.262176299060745,
7.59394543036555));
#396570=CARTESIAN_POINT('Origin',(-2.90905453099297,0.142494670373524,7.5));
#396571=CARTESIAN_POINT('',(-2.73469396819878,0.216676518124532,8.75721825406948));
#396572=CARTESIAN_POINT('',(-2.72179064828012,0.222166246411417,8.78727029226991));
#396573=CARTESIAN_POINT('Origin',(-2.68903720962739,0.236101224370437,8.7565864062101));
#396574=CARTESIAN_POINT('',(-2.65600461497701,0.250154969482898,8.85049129520029));
#396575=CARTESIAN_POINT('Ctrl Pts',(-2.72179064828012,0.222166246411417,
8.78727029226991));
#396576=CARTESIAN_POINT('Ctrl Pts',(-2.69989307440825,0.231482587589998,
8.80838212259895));
#396577=CARTESIAN_POINT('Ctrl Pts',(-2.67796516820153,0.240811833685889,
8.82945686509571));
#396578=CARTESIAN_POINT('Ctrl Pts',(-2.65600461497701,0.250154969482898,
8.85049129520029));
#396579=CARTESIAN_POINT('',(-2.65600461497701,0.250154969482898,7.59394543036555));
#396580=CARTESIAN_POINT('',(-2.65600461497701,0.250154969482898,7.5));
#396581=CARTESIAN_POINT('',(-2.73469396819878,0.216676518124532,7.51860402984325));
#396582=CARTESIAN_POINT('Ctrl Pts',(-2.65600461497701,0.250154969482899,
7.59394543036555));
#396583=CARTESIAN_POINT('Ctrl Pts',(-2.67211190534232,0.243302109280958,
7.57858609112103));
#396584=CARTESIAN_POINT('Ctrl Pts',(-2.68820117174618,0.236456917388554,
7.56320440326857));
#396585=CARTESIAN_POINT('Ctrl Pts',(-2.70427335879892,0.229618991920397,
7.54780169004651));
#396586=CARTESIAN_POINT('Ctrl Pts',(-2.71442028774302,0.225301972486589,
7.53807742314383));
#396587=CARTESIAN_POINT('Ctrl Pts',(-2.72456041724852,0.220987845879634,
7.52834476460825));
#396588=CARTESIAN_POINT('Ctrl Pts',(-2.73469396819878,0.216676518124533,
7.51860402984325));
#396589=CARTESIAN_POINT('',(-2.73469396819878,0.216676518124532,7.5));
#396590=CARTESIAN_POINT('Origin',(-2.65869612245475,0.256481217383297,7.5));
#396591=CARTESIAN_POINT('Ctrl Pts',(-2.65600461497701,0.250154969482898,
8.85049129520029));
#396592=CARTESIAN_POINT('Ctrl Pts',(-2.65582641123953,0.250230786412545,
8.85097269580138));
#396593=CARTESIAN_POINT('Ctrl Pts',(-2.65565374887267,0.250313386797565,
8.85143669361005));
#396594=CARTESIAN_POINT('Ctrl Pts',(-2.65547905463228,0.250407362801248,
8.8519052845931));
#396595=CARTESIAN_POINT('Ctrl Pts',(-2.6551373637768,0.250591173904709,
8.85282181883899));
#396596=CARTESIAN_POINT('Ctrl Pts',(-2.65479678269175,0.25081394947612,
8.85372622499635));
#396597=CARTESIAN_POINT('Ctrl Pts',(-2.65446040730407,0.251092088735977,
8.85462257735071));
#396598=CARTESIAN_POINT('Ctrl Pts',(-2.65418116040415,0.251322990070938,
8.85536669723986));
#396599=CARTESIAN_POINT('Ctrl Pts',(-2.65390472814385,0.251592074862224,
8.85610498449051));
#396600=CARTESIAN_POINT('Ctrl Pts',(-2.65363844027942,0.251914482863972,
8.8568133821837));
#396601=CARTESIAN_POINT('Ctrl Pts',(-2.65339678362424,0.252207068631909,
8.85745625420284));
#396602=CARTESIAN_POINT('Ctrl Pts',(-2.65315998869644,0.252546858276553,
8.85808743050665));
#396603=CARTESIAN_POINT('Ctrl Pts',(-2.65294216072111,0.252958729273139,
8.85866804508409));
#396604=CARTESIAN_POINT('Ctrl Pts',(-2.65284165961522,0.253148757622697,
8.85893592806395));
#396605=CARTESIAN_POINT('Ctrl Pts',(-2.65274533984821,0.253354324991418,
8.85919241173848));
#396606=CARTESIAN_POINT('Ctrl Pts',(-2.65265570415938,0.253579014432822,
8.85943017985534));
#396607=CARTESIAN_POINT('Ctrl Pts',(-2.65253466944446,0.253882411693908,
8.8597512372));
#396608=CARTESIAN_POINT('Ctrl Pts',(-2.65242333611262,0.254228633815619,
8.86004599534705));
#396609=CARTESIAN_POINT('Ctrl Pts',(-2.65233295686034,0.254616709420195,
8.86026130871721));
#396610=CARTESIAN_POINT('Ctrl Pts',(-2.65229986646803,0.254758794840041,
8.86034014101235));
#396611=CARTESIAN_POINT('Ctrl Pts',(-2.65226907590949,0.254908622195534,
8.86040910639692));
#396612=CARTESIAN_POINT('Ctrl Pts',(-2.65224175354912,0.255062177237551,
8.86046313645506));
#396613=CARTESIAN_POINT('Ctrl Pts',(-2.65219911723458,0.255301798594607,
8.86054744990829));
#396614=CARTESIAN_POINT('Ctrl Pts',(-2.65216390737134,0.255557064068595,
8.86059655985668));
#396615=CARTESIAN_POINT('Ctrl Pts',(-2.65213809186542,0.255811562677672,
8.86059725258816));
#396616=CARTESIAN_POINT('Ctrl Pts',(-2.65211221671537,0.256066649280209,
8.86059794692011));
#396617=CARTESIAN_POINT('Ctrl Pts',(-2.65209813563059,0.256324062526848,
8.86056369958366));
#396618=CARTESIAN_POINT('Ctrl Pts',(-2.65209285911932,0.256569557431487,
8.86048590497774));
#396619=CARTESIAN_POINT('Ctrl Pts',(-2.65209148210697,0.256633624292334,
8.86046560290182));
#396620=CARTESIAN_POINT('Ctrl Pts',(-2.65209077737803,0.256697714868739,
8.86044257503091));
#396621=CARTESIAN_POINT('Ctrl Pts',(-2.65209073388499,0.256759848347903,
8.86041778462583));
#396622=CARTESIAN_POINT('Ctrl Pts',(-2.65209044123086,0.257177929561459,
8.86025097596201));
#396623=CARTESIAN_POINT('Ctrl Pts',(-2.65212037943941,0.257563502039578,
8.8599848982295));
#396624=CARTESIAN_POINT('Ctrl Pts',(-2.65217122762928,0.257905967816434,
8.85968173251461));
#396625=CARTESIAN_POINT('Ctrl Pts',(-2.65219812340846,0.258087112591441,
8.85952137522076));
#396626=CARTESIAN_POINT('Ctrl Pts',(-2.65223119893676,0.258259716699464,
8.85934740853961));
#396627=CARTESIAN_POINT('Ctrl Pts',(-2.65226846100321,0.258421638611247,
8.8591675900182));
#396628=CARTESIAN_POINT('Ctrl Pts',(-2.65241808756843,0.2590718392524,8.85844552518694));
#396629=CARTESIAN_POINT('Ctrl Pts',(-2.65264072726469,0.259587222332733,
8.85759444184122));
#396630=CARTESIAN_POINT('Ctrl Pts',(-2.65285999980908,0.259991132974821,
8.85683498915136));
#396631=CARTESIAN_POINT('Ctrl Pts',(-2.65288294609688,0.260033401147807,
8.85675551444996));
#396632=CARTESIAN_POINT('Ctrl Pts',(-2.65290587085534,0.260074435800327,
8.8566769979365));
#396633=CARTESIAN_POINT('Ctrl Pts',(-2.65292869619824,0.260114254771412,
8.85659965593547));
#396634=CARTESIAN_POINT('Ctrl Pts',(-2.65323679384139,0.260651733275033,
8.85555568965886));
#396635=CARTESIAN_POINT('Ctrl Pts',(-2.6536105172958,0.261123788020533,
8.85434650606346));
#396636=CARTESIAN_POINT('Ctrl Pts',(-2.65404684146776,0.261536610171395,
8.85297329937117));
#396637=CARTESIAN_POINT('Ctrl Pts',(-2.65429224722887,0.261768797477633,
8.85220095427747));
#396638=CARTESIAN_POINT('Ctrl Pts',(-2.65455777277542,0.261982113251123,
8.85137579139184));
#396639=CARTESIAN_POINT('Ctrl Pts',(-2.6548449317704,0.262176299060745,
8.85049129520029));
#396640=CARTESIAN_POINT('Origin',(-2.65869612245475,0.256481217383297,7.59394543036555));
#396641=CARTESIAN_POINT('Ctrl Pts',(-2.65548722941064,0.250375091606262,
7.59443877723642));
#396642=CARTESIAN_POINT('Ctrl Pts',(-2.65015865589203,0.252642137681094,
7.58783886950016));
#396643=CARTESIAN_POINT('Ctrl Pts',(-2.65158455852055,0.261011485518926,
7.58559994247159));
#396644=CARTESIAN_POINT('Ctrl Pts',(-2.68457575591505,0.237999353596066,
7.56670252222135));
#396645=CARTESIAN_POINT('Ctrl Pts',(-2.67925488369801,0.24026312314568,
7.5600487499903));
#396646=CARTESIAN_POINT('Ctrl Pts',(-2.68066817321352,0.248685650676173,
7.55786368756704));
#396647=CARTESIAN_POINT('Ctrl Pts',(-2.71360996250253,0.225646726040107,
7.53888913333558));
#396648=CARTESIAN_POINT('Ctrl Pts',(-2.70825746808134,0.227923949283006,
7.53222002137277));
#396649=CARTESIAN_POINT('Ctrl Pts',(-2.70969805244026,0.236381322481881,
7.53005029815326));
#396650=CARTESIAN_POINT('Ctrl Pts',(-2.74258853535555,0.213317767903159,
7.51101258149734));
#396651=CARTESIAN_POINT('Ctrl Pts',(-2.73717115897627,0.215622595229579,
7.5043616886572));
#396652=CARTESIAN_POINT('Ctrl Pts',(-2.73867279415589,0.224099184952573,
7.50217374673251));
#396653=CARTESIAN_POINT('',(-2.73712666431696,0.224754574642189,7.50366116523517));
#396654=CARTESIAN_POINT('Ctrl Pts',(-2.73469396819878,0.216676518124532,
7.51860402984325));
#396655=CARTESIAN_POINT('Ctrl Pts',(-2.73510033067525,0.216503630867928,
7.51734760759493));
#396656=CARTESIAN_POINT('Ctrl Pts',(-2.73549082980322,0.216402150372104,
7.51608817408572));
#396657=CARTESIAN_POINT('Ctrl Pts',(-2.73586792612086,0.21638523440084,
7.51481005913118));
#396658=CARTESIAN_POINT('Ctrl Pts',(-2.73620950897638,0.216369911509849,
7.51365231206383));
#396659=CARTESIAN_POINT('Ctrl Pts',(-2.73654056487762,0.216423703726808,
7.51247773061042));
#396660=CARTESIAN_POINT('Ctrl Pts',(-2.73684944320768,0.216582127288799,
7.51129758471022));
#396661=CARTESIAN_POINT('Ctrl Pts',(-2.7372333436967,0.216779029683701,
7.50983079813402));
#396662=CARTESIAN_POINT('Ctrl Pts',(-2.73756478892187,0.217142868017685,
7.50839324291155));
#396663=CARTESIAN_POINT('Ctrl Pts',(-2.7377852545119,0.217731815209157,
7.50715379678855));
#396664=CARTESIAN_POINT('Ctrl Pts',(-2.73788710326193,0.218003891841511,
7.50658120839351));
#396665=CARTESIAN_POINT('Ctrl Pts',(-2.73797084707659,0.218366019889142,
7.50598221009429));
#396666=CARTESIAN_POINT('Ctrl Pts',(-2.73801233135005,0.218814706195371,
7.50545747549611));
#396667=CARTESIAN_POINT('Ctrl Pts',(-2.73803446864242,0.219054139096515,
7.50517746087247));
#396668=CARTESIAN_POINT('Ctrl Pts',(-2.73804501371076,0.21932079816468,
7.50491486231392));
#396669=CARTESIAN_POINT('Ctrl Pts',(-2.73804202059031,0.219607687728848,
7.50468370960993));
#396670=CARTESIAN_POINT('Ctrl Pts',(-2.73803754493112,0.220036678121463,
7.50433806340447));
#396671=CARTESIAN_POINT('Ctrl Pts',(-2.73800210745578,0.220523761247884,
7.50405484070984));
#396672=CARTESIAN_POINT('Ctrl Pts',(-2.73793738030584,0.221036080981669,
7.50385766036131));
#396673=CARTESIAN_POINT('Ctrl Pts',(-2.73793045874324,0.221090865613945,
7.50383657498791));
#396674=CARTESIAN_POINT('Ctrl Pts',(-2.73792321962444,0.221145916405826,
7.50381643264937));
#396675=CARTESIAN_POINT('Ctrl Pts',(-2.7379156778676,0.221201177089492,
7.50379723213559));
#396676=CARTESIAN_POINT('Ctrl Pts',(-2.73786533417364,0.221570060229997,
7.50366906242519));
#396677=CARTESIAN_POINT('Ctrl Pts',(-2.73779969739273,0.22195622297901,
7.50358235568538));
#396678=CARTESIAN_POINT('Ctrl Pts',(-2.73772748437109,0.222326915563695,
7.5035341175365));
#396679=CARTESIAN_POINT('Ctrl Pts',(-2.73761920911807,0.22288272714013,
7.50346178989176));
#396680=CARTESIAN_POINT('Ctrl Pts',(-2.73747909711921,0.223476050177319,
7.50346967198527));
#396681=CARTESIAN_POINT('Ctrl Pts',(-2.73732362825383,0.224054277262595,
7.50354272648692));
#396682=CARTESIAN_POINT('Ctrl Pts',(-2.73725968069148,0.224292114031364,
7.50357277531559));
#396683=CARTESIAN_POINT('Ctrl Pts',(-2.73719335688109,0.22452711760629,
7.50361331098761));
#396684=CARTESIAN_POINT('Ctrl Pts',(-2.73712666431837,0.224754574642305,
7.50366116523659));
#396685=CARTESIAN_POINT('',(-2.66161051802577,0.256762365619155,7.57603338622103));
#396686=CARTESIAN_POINT('Origin',(-2.67040634802763,0.257613755182305,7.58486873427626));
#396687=CARTESIAN_POINT('Ctrl Pts',(-2.73712666436743,0.224754574614973,
7.50366116529969));
#396688=CARTESIAN_POINT('Ctrl Pts',(-2.71199601738034,0.235407197804172,
7.52783573079709));
#396689=CARTESIAN_POINT('Ctrl Pts',(-2.68682516411221,0.246075974212539,
7.55196141284068));
#396690=CARTESIAN_POINT('Ctrl Pts',(-2.66161051899361,0.256762364824846,
7.57603338728831));
#396691=CARTESIAN_POINT('Ctrl Pts',(-2.65701976820119,0.249914138729897,
7.59639677331372));
#396692=CARTESIAN_POINT('Ctrl Pts',(-2.63844797215671,0.254527902676073,
7.59974925422226));
#396693=CARTESIAN_POINT('Ctrl Pts',(-2.65579532783688,0.262606743989909,
7.59639677331371));
#396694=CARTESIAN_POINT('Ctrl Pts',(-2.65313223933917,0.250233862721232,
7.58707626057423));
#396695=CARTESIAN_POINT('Ctrl Pts',(-2.64870482551445,0.25551736898378,
7.58811717123965));
#396696=CARTESIAN_POINT('Ctrl Pts',(-2.65204060628403,0.26154978129223,
7.58707626057423));
#396697=CARTESIAN_POINT('Ctrl Pts',(-2.65771595193357,0.254223250031748,
7.5801537675693));
#396698=CARTESIAN_POINT('Ctrl Pts',(-2.65558427051316,0.256181020769049,
7.58208760766041));
#396699=CARTESIAN_POINT('Ctrl Pts',(-2.6573023971617,0.258510177860652,
7.5801537675693));
#396700=CARTESIAN_POINT('Ctrl Pts',(-2.66161051720204,0.256762365539488,
7.57603338509286));
#396701=CARTESIAN_POINT('Ctrl Pts',(-2.66161051720204,0.256762365539488,
7.57603338509286));
#396702=CARTESIAN_POINT('Ctrl Pts',(-2.66161051720204,0.256762365539488,
7.57603338509286));
#396703=CARTESIAN_POINT('Origin',(-2.67040689596895,0.257608075198315,7.58486873427623));
#396704=CARTESIAN_POINT('Ctrl Pts',(-2.73281288470864,0.314900644564376,
7.51098857897448));
#396705=CARTESIAN_POINT('Ctrl Pts',(-2.72793597470703,0.311602726917125,
7.50433767179956));
#396706=CARTESIAN_POINT('Ctrl Pts',(-2.73103031844476,0.303569478015516,
7.50214974420965));
#396707=CARTESIAN_POINT('Ctrl Pts',(-2.70671798449284,0.297254464524858,
7.53887321589169));
#396708=CARTESIAN_POINT('Ctrl Pts',(-2.701899508528,0.293996061783762,7.53220407452062));
#396709=CARTESIAN_POINT('Ctrl Pts',(-2.70493022693791,0.285970000119303,
7.53003438070912));
#396710=CARTESIAN_POINT('Ctrl Pts',(-2.68057297244259,0.279574397310247,
7.56669465659233));
#396711=CARTESIAN_POINT('Ctrl Pts',(-2.67578297277486,0.276335251123581,
7.56004085833301));
#396712=CARTESIAN_POINT('Ctrl Pts',(-2.67878022809323,0.26833818224285,
7.55785582193788));
#396713=CARTESIAN_POINT('Ctrl Pts',(-2.65437903099217,0.261861242519229,
7.59443891967696));
#396714=CARTESIAN_POINT('Ctrl Pts',(-2.64958208642131,0.258617399973863,
7.58783901202978));
#396715=CARTESIAN_POINT('Ctrl Pts',(-2.65258156709372,0.250674963717643,
7.58560008491213));
#396716=CARTESIAN_POINT('',(-2.72961551748768,0.3026154689171,7.50366116523517));
#396717=CARTESIAN_POINT('Ctrl Pts',(-2.72961551748805,0.302615468917141,
7.50366116523554));
#396718=CARTESIAN_POINT('Ctrl Pts',(-2.72968561742244,0.303369937946302,
7.50350835821027));
#396719=CARTESIAN_POINT('Ctrl Pts',(-2.72972551041329,0.30406575872813,
7.50345484955999));
#396720=CARTESIAN_POINT('Ctrl Pts',(-2.72973698202872,0.304723584208345,
7.50349758195598));
#396721=CARTESIAN_POINT('Ctrl Pts',(-2.72974286781819,0.305061097465305,
7.50351950684424));
#396722=CARTESIAN_POINT('Ctrl Pts',(-2.72974198137209,0.305421873052835,
7.50357029184312));
#396723=CARTESIAN_POINT('Ctrl Pts',(-2.72973156373016,0.305769741308966,
7.50365515313923));
#396724=CARTESIAN_POINT('Ctrl Pts',(-2.72971553717836,0.306304903552658,
7.50378570417639));
#396725=CARTESIAN_POINT('Ctrl Pts',(-2.72967682976936,0.306825237690739,
7.50400001621911));
#396726=CARTESIAN_POINT('Ctrl Pts',(-2.72961612354001,0.307290970309348,
7.50428903009634));
#396727=CARTESIAN_POINT('Ctrl Pts',(-2.7296093856156,0.307342663046885,
7.50432110841318));
#396728=CARTESIAN_POINT('Ctrl Pts',(-2.72960239051941,0.307393710105065,
7.50435406373354));
#396729=CARTESIAN_POINT('Ctrl Pts',(-2.72959514912735,0.307444077147395,
7.50438785222352));
#396730=CARTESIAN_POINT('Ctrl Pts',(-2.72955093694813,0.30775159215028,
7.50459414719561));
#396731=CARTESIAN_POINT('Ctrl Pts',(-2.72949632922009,0.308038580830333,
7.50483629897752));
#396732=CARTESIAN_POINT('Ctrl Pts',(-2.72943471078469,0.308294294734331,
7.5050991045531));
#396733=CARTESIAN_POINT('Ctrl Pts',(-2.72929877432721,0.308858425290581,
7.50567888004914));
#396734=CARTESIAN_POINT('Ctrl Pts',(-2.72912386673409,0.309292697140621,
7.50637912803144));
#396735=CARTESIAN_POINT('Ctrl Pts',(-2.72893465063686,0.309615742862416,
7.50710440483569));
#396736=CARTESIAN_POINT('Ctrl Pts',(-2.72888825109336,0.309694960086756,
7.50728225710685));
#396737=CARTESIAN_POINT('Ctrl Pts',(-2.72884019340232,0.309769139713248,
7.50746498566954));
#396738=CARTESIAN_POINT('Ctrl Pts',(-2.72879194901788,0.309836776660465,
7.50764697238949));
#396739=CARTESIAN_POINT('Ctrl Pts',(-2.72853260048435,0.310200374274514,
7.50862528291181));
#396740=CARTESIAN_POINT('Ctrl Pts',(-2.72824768340916,0.310410308860692,
7.50965856837421));
#396741=CARTESIAN_POINT('Ctrl Pts',(-2.72796073636963,0.310528558892836,
7.51067959873201));
#396742=CARTESIAN_POINT('Ctrl Pts',(-2.72780282905185,0.310593632034678,
7.51124147302578));
#396743=CARTESIAN_POINT('Ctrl Pts',(-2.72764410294566,0.310630554447926,
7.51180065547252));
#396744=CARTESIAN_POINT('Ctrl Pts',(-2.72748753823894,0.310647107520359,
7.512351757165));
#396745=CARTESIAN_POINT('Ctrl Pts',(-2.72694654480926,0.310704304979572,
7.51425603304535));
#396746=CARTESIAN_POINT('Ctrl Pts',(-2.72636621705693,0.310519085845738,
7.51626900505179));
#396747=CARTESIAN_POINT('Ctrl Pts',(-2.72577891497116,0.310142396153974,
7.51827788969242));
#396748=CARTESIAN_POINT('Ctrl Pts',(-2.72574712907243,0.31012200899601,
7.51838661432544));
#396749=CARTESIAN_POINT('Ctrl Pts',(-2.72571532001016,0.310101051407261,
7.51849533314856));
#396750=CARTESIAN_POINT('Ctrl Pts',(-2.72568349213022,0.310079528408703,
7.51860402984325));
#396751=CARTESIAN_POINT('Ctrl Pts',(-2.66161051882509,0.256762366584182,
7.57603338728985));
#396752=CARTESIAN_POINT('Ctrl Pts',(-2.68431738886144,0.272071688132332,
7.55196141284922));
#396753=CARTESIAN_POINT('Ctrl Pts',(-2.7069846417267,0.287355349116307,
7.52783573083105));
#396754=CARTESIAN_POINT('Ctrl Pts',(-2.7296155175335,0.302615468954552,
7.50366116530176));
#396755=CARTESIAN_POINT('Origin',(-9.19709468541367E-16,8.87232663177171E-17,
7.49482233047033));
#396756=CARTESIAN_POINT('Origin',(-2.7283174780614,0.224031223057615,7.49482233047033));
#396757=CARTESIAN_POINT('Origin',(0.,0.,7.50366116523517));
#396758=CARTESIAN_POINT('Origin',(-2.72083050515592,0.301641529324075,7.49482233047033));
#396759=CARTESIAN_POINT('Ctrl Pts',(-2.73469299488662,0.216676932172375,
7.51860402984325));
#396760=CARTESIAN_POINT('Ctrl Pts',(-2.74169487207938,0.213698677346542,
7.51860402984325));
#396761=CARTESIAN_POINT('Ctrl Pts',(-2.74226515987506,0.206111117932591,
7.51860402984325));
#396762=CARTESIAN_POINT('Ctrl Pts',(-2.7372928391742,0.215571084661534,
7.51041458714367));
#396763=CARTESIAN_POINT('Ctrl Pts',(-2.74182996991853,0.211901096872849,
7.51004642900444));
#396764=CARTESIAN_POINT('Ctrl Pts',(-2.74226531715366,0.206109025373795,
7.50729136483012));
#396765=CARTESIAN_POINT('Ctrl Pts',(-2.73922057885099,0.217622317690195,
7.50215815450136));
#396766=CARTESIAN_POINT('Ctrl Pts',(-2.74155503724043,0.215561160609954,
7.49877163671529));
#396767=CARTESIAN_POINT('Ctrl Pts',(-2.74183741099952,0.212122528810162,
7.49481588533168));
#396768=CARTESIAN_POINT('Ctrl Pts',(-2.73712611564552,0.224754529589428,
7.50366171572174));
#396769=CARTESIAN_POINT('Ctrl Pts',(-2.74077554873745,0.225054196679268,
7.50000045605858));
#396770=CARTESIAN_POINT('Ctrl Pts',(-2.74077554873746,0.225054196679144,
7.49482233047317));
#396771=CARTESIAN_POINT('Origin',(-2.72980031823926,0.205174249214716,7.51860402984325));
#396772=CARTESIAN_POINT('Origin',(-2.72980031823926,0.205174249214716,9.));
#396773=CARTESIAN_POINT('Origin',(-2.72980031823926,0.205174249214716,8.75721825406948));
#396774=CARTESIAN_POINT('Ctrl Pts',(-2.71932677685935,0.223214469743997,
8.78942910404912));
#396775=CARTESIAN_POINT('Ctrl Pts',(-2.7244623390508,0.221051501949632,
8.79672699501691));
#396776=CARTESIAN_POINT('Ctrl Pts',(-2.72256725120911,0.212328994967445,
8.79893251111267));
#396777=CARTESIAN_POINT('Ctrl Pts',(-2.72944356314156,0.218910279453015,
8.78111911759583));
#396778=CARTESIAN_POINT('Ctrl Pts',(-2.73552894228411,0.216339195864926,
8.78644465894814));
#396779=CARTESIAN_POINT('Ctrl Pts',(-2.73554682940729,0.2082327051429,8.78817647674132));
#396780=CARTESIAN_POINT('Ctrl Pts',(-2.73574858564827,0.216227805369778,
8.76780923932029));
#396781=CARTESIAN_POINT('Ctrl Pts',(-2.74293013554405,0.21318805573127,
8.76988516158375));
#396782=CARTESIAN_POINT('Ctrl Pts',(-2.74365028845523,0.205663578328771,
8.77093053738833));
#396783=CARTESIAN_POINT('Ctrl Pts',(-2.73451919254909,0.216750851102169,
8.75371302330492));
#396784=CARTESIAN_POINT('Ctrl Pts',(-2.74152478183233,0.213786408462771,
8.75300828287558));
#396785=CARTESIAN_POINT('Ctrl Pts',(-2.74206964654565,0.206164226243848,
8.75267964240738));
#396786=CARTESIAN_POINT('Origin',(-2.71689699832061,0.210663977501601,8.78727029226991));
#396787=CARTESIAN_POINT('Ctrl Pts',(-2.65600461497701,0.250154969482898,
8.85049129520029));
#396788=CARTESIAN_POINT('Ctrl Pts',(-2.66137812144103,0.247868806648742,
8.85711686593484));
#396789=CARTESIAN_POINT('Ctrl Pts',(-2.65991420288366,0.239445167021401,
8.85933012996512));
#396790=CARTESIAN_POINT('Ctrl Pts',(-2.67796519767341,0.240811821147055,
8.82945683644724));
#396791=CARTESIAN_POINT('Ctrl Pts',(-2.68338330748995,0.238506681779115,
8.83607469902389));
#396792=CARTESIAN_POINT('Ctrl Pts',(-2.68187814229224,0.230064731754094,
8.8382956714852));
#396793=CARTESIAN_POINT('Ctrl Pts',(-2.6998930463504,0.231482599527234,
8.80838214965001));
#396794=CARTESIAN_POINT('Ctrl Pts',(-2.70533253855799,0.22916836300311,
8.81501364461993));
#396795=CARTESIAN_POINT('Ctrl Pts',(-2.70380902611905,0.220699140934728,
8.81722098428721));
#396796=CARTESIAN_POINT('Ctrl Pts',(-2.72179064828012,0.222166246411417,
8.78727029226991));
#396797=CARTESIAN_POINT('Ctrl Pts',(-2.7272310440052,0.219851625485012,
8.79393457792714));
#396798=CARTESIAN_POINT('Ctrl Pts',(-2.7257093818291,0.211347276044871,
8.79610912703474));
#396799=CARTESIAN_POINT('Origin',(-2.6511109650175,0.238652700573082,8.85049129520029));
#396800=CARTESIAN_POINT('Ctrl Pts',(-2.6548449317704,0.262176299060745,
8.85049129520029));
#396801=CARTESIAN_POINT('Ctrl Pts',(-2.65968232649294,0.265447495251963,
8.85711686593484));
#396802=CARTESIAN_POINT('Ctrl Pts',(-2.65663515242803,0.273435955199415,
8.85933012996512));
#396803=CARTESIAN_POINT('Ctrl Pts',(-2.65056535848791,0.259282319010592,
8.86332496987233));
#396804=CARTESIAN_POINT('Ctrl Pts',(-2.65040345612426,0.263900292808847,
8.86648636486737));
#396805=CARTESIAN_POINT('Ctrl Pts',(-2.64467246891994,0.265325735742342,
8.87206031107457));
#396806=CARTESIAN_POINT('Ctrl Pts',(-2.65121844737383,0.252191248505865,
8.86341338519875));
#396807=CARTESIAN_POINT('Ctrl Pts',(-2.65191509820944,0.247609966125634,
8.86654584966058));
#396808=CARTESIAN_POINT('Ctrl Pts',(-2.64651844701235,0.24516041338191,
8.87215952290714));
#396809=CARTESIAN_POINT('Ctrl Pts',(-2.65600461497701,0.250154969482898,
8.85049129520029));
#396810=CARTESIAN_POINT('Ctrl Pts',(-2.66137812144103,0.247868806648741,
8.85711686593484));
#396811=CARTESIAN_POINT('Ctrl Pts',(-2.65991420288366,0.239445167021401,
8.85933012996512));
#396812=CARTESIAN_POINT('Origin',(-2.64784276688978,0.272530993019743,8.85049129520029));
#396813=CARTESIAN_POINT('Ctrl Pts',(-2.71406752923974,0.30222445439797,
8.78727029226991));
#396814=CARTESIAN_POINT('Ctrl Pts',(-2.7189651397191,0.305536370349644,
8.79393457792714));
#396815=CARTESIAN_POINT('Ctrl Pts',(-2.71584585849932,0.313593013561936,
8.79610912703474));
#396816=CARTESIAN_POINT('Ctrl Pts',(-2.69435463883559,0.288893987130641,
8.80838214965001));
#396817=CARTESIAN_POINT('Ctrl Pts',(-2.69925143594083,0.292205353053551,
8.81501364461986));
#396818=CARTESIAN_POINT('Ctrl Pts',(-2.6961370534789,0.300227162978756,
8.81722098428721));
#396819=CARTESIAN_POINT('Ctrl Pts',(-2.67461451938528,0.275545106738646,
8.82945683644724));
#396820=CARTESIAN_POINT('Ctrl Pts',(-2.67949206740876,0.278843455836047,
8.83607469902389));
#396821=CARTESIAN_POINT('Ctrl Pts',(-2.6764009071358,0.286842003870814,
8.83829567148519));
#396822=CARTESIAN_POINT('Ctrl Pts',(-2.6548449317704,0.262176299060745,
8.85049129520029));
#396823=CARTESIAN_POINT('Ctrl Pts',(-2.65968232649294,0.265447495251963,
8.85711686593484));
#396824=CARTESIAN_POINT('Ctrl Pts',(-2.65663515242803,0.273435955199415,
8.85933012996512));
#396825=CARTESIAN_POINT('Origin',(-2.70706536435912,0.312579148356967,8.78727029226991));
#396826=CARTESIAN_POINT('Ctrl Pts',(-2.72553009885001,0.309975821388915,
8.75374538247848));
#396827=CARTESIAN_POINT('Ctrl Pts',(-2.73183224290654,0.314221685102973,
8.75304829418602));
#396828=CARTESIAN_POINT('Ctrl Pts',(-2.73091660408602,0.321800091845777,
8.75272238421917));
#396829=CARTESIAN_POINT('Ctrl Pts',(-2.7266235412515,0.310715240504627,
8.76769408445017));
#396830=CARTESIAN_POINT('Ctrl Pts',(-2.73308388962344,0.315068521323175,
8.76974318093968));
#396831=CARTESIAN_POINT('Ctrl Pts',(-2.73235642164598,0.322584447588244,
8.77077869880429));
#396832=CARTESIAN_POINT('Ctrl Pts',(-2.72101917840275,0.306925399324504,
8.78108014887992));
#396833=CARTESIAN_POINT('Ctrl Pts',(-2.72649621408304,0.310611497187727,
8.78639403366327));
#396834=CARTESIAN_POINT('Ctrl Pts',(-2.72498584455341,0.318563909376041,
8.78812224174742));
#396835=CARTESIAN_POINT('Ctrl Pts',(-2.7118348648497,0.300714686275392,
8.78944554828685));
#396836=CARTESIAN_POINT('Ctrl Pts',(-2.71645383287792,0.303816548936953,
8.79673892988685));
#396837=CARTESIAN_POINT('Ctrl Pts',(-2.71293245935051,0.312008220487802,
8.79894799272499));
#396838=CARTESIAN_POINT('Origin',(-2.7186813272496,0.320434222367697,8.75721825406948));
#396839=CARTESIAN_POINT('Origin',(-2.7186813272496,0.320434222367697,9.));
#396840=CARTESIAN_POINT('Origin',(-2.7186813272496,0.320434222367697,7.51860402984325));
#396841=CARTESIAN_POINT('Ctrl Pts',(-2.72961473561416,0.30261538223571,
7.50366195182966));
#396842=CARTESIAN_POINT('Ctrl Pts',(-2.7332543887411,0.303018887905602,
7.50000065167735));
#396843=CARTESIAN_POINT('Ctrl Pts',(-2.73325438874108,0.303018887905718,
7.49482233047108));
#396844=CARTESIAN_POINT('Ctrl Pts',(-2.73030692093629,0.310023126770085,
7.50215800491338));
#396845=CARTESIAN_POINT('Ctrl Pts',(-2.73220389660087,0.312494195466482,
7.49877273257266));
#396846=CARTESIAN_POINT('Ctrl Pts',(-2.7318235351777,0.315925300468913,
7.49481816995647));
#396847=CARTESIAN_POINT('Ctrl Pts',(-2.72801852916872,0.311658143424489,
7.51043025814042));
#396848=CARTESIAN_POINT('Ctrl Pts',(-2.73177540382666,0.316127891716211,
7.51006209594515));
#396849=CARTESIAN_POINT('Ctrl Pts',(-2.73109510087304,0.321899906793596,
7.507312818217));
#396850=CARTESIAN_POINT('Ctrl Pts',(-2.72568224006612,0.310078681834469,
7.51860402984326));
#396851=CARTESIAN_POINT('Ctrl Pts',(-2.73198608987389,0.31434042971436,
7.51860402984327));
#396852=CARTESIAN_POINT('Ctrl Pts',(-2.73109539723704,0.321897392332852,
7.51860402984327));
#396853=CARTESIAN_POINT('Origin',(0.,0.,7.5));
#396854=CARTESIAN_POINT('Origin',(-2.66618796128141,0.0915411309427941,
7.5));
#396855=CARTESIAN_POINT('',(-2.66618796128141,0.0915411309427941,7.59394543036555));
#396856=CARTESIAN_POINT('',(-2.66618796128141,0.0915411309427941,8.85049129520029));
#396857=CARTESIAN_POINT('',(-2.66618796128141,0.0915411309427941,7.5));
#396858=CARTESIAN_POINT('',(-2.72785477369492,0.127712598202037,8.78727029226991));
#396859=CARTESIAN_POINT('Ctrl Pts',(-2.66618796128141,0.0915411309427944,
8.85049129520029));
#396860=CARTESIAN_POINT('Ctrl Pts',(-2.68677344498056,0.103615812939434,
8.82945686509571));
#396861=CARTESIAN_POINT('Ctrl Pts',(-2.70732832586904,0.115672544461242,
8.80838212259897));
#396862=CARTESIAN_POINT('Ctrl Pts',(-2.72785477369492,0.127712598202037,
8.78727029226991));
#396863=CARTESIAN_POINT('',(-2.73995014666367,0.134807295823077,8.75721825406948));
#396864=CARTESIAN_POINT('Origin',(-2.70355107558758,0.113456715445809,8.75937679713089));
#396865=CARTESIAN_POINT('',(-2.73995014666367,0.134807295823077,7.51860402984325));
#396866=CARTESIAN_POINT('',(-2.73995014666367,0.134807295823077,7.5));
#396867=CARTESIAN_POINT('Ctrl Pts',(-2.73995014666367,0.134807295823077,
7.51860402984325));
#396868=CARTESIAN_POINT('Ctrl Pts',(-2.73045111238304,0.129235514275945,
7.52834476460825));
#396869=CARTESIAN_POINT('Ctrl Pts',(-2.72094591146644,0.123660115608629,
7.53807742314407));
#396870=CARTESIAN_POINT('Ctrl Pts',(-2.71143433686084,0.118080978371512,
7.54780169004674));
#396871=CARTESIAN_POINT('Ctrl Pts',(-2.69636851674231,0.109243926514559,
7.5632044032688));
#396872=CARTESIAN_POINT('Ctrl Pts',(-2.68128668670342,0.100397483831551,
7.57858609112103));
#396873=CARTESIAN_POINT('Ctrl Pts',(-2.66618796128141,0.0915411309427943,
7.59394543036555));
#396874=CARTESIAN_POINT('Origin',(-2.91220723134083,-0.0441818639458735,
7.5));
#396875=CARTESIAN_POINT('',(-2.742957758327,0.0410188888571364,8.75721825406948));
#396876=CARTESIAN_POINT('',(-2.73043267776197,0.0473240564541541,8.78727029226991));
#396877=CARTESIAN_POINT('Origin',(-2.69863935166689,0.0633289235250963,
8.75658640621089));
#396878=CARTESIAN_POINT('',(-2.66657505256398,0.0794701993176923,8.85049129520029));
#396879=CARTESIAN_POINT('Ctrl Pts',(-2.73043267776197,0.0473240564541541,
8.78727029226991));
#396880=CARTESIAN_POINT('Ctrl Pts',(-2.70917699483285,0.0580242385856248,
8.80838212259895));
#396881=CARTESIAN_POINT('Ctrl Pts',(-2.68789186871081,0.0687392425192337,
8.82945686509571));
#396882=CARTESIAN_POINT('Ctrl Pts',(-2.66657505256398,0.0794701993176922,
8.85049129520029));
#396883=CARTESIAN_POINT('',(-2.66657505256398,0.0794701993176923,7.59394543036555));
#396884=CARTESIAN_POINT('',(-2.66657505256398,0.0794701993176923,7.5));
#396885=CARTESIAN_POINT('',(-2.742957758327,0.0410188888571365,7.51860402984325));
#396886=CARTESIAN_POINT('Ctrl Pts',(-2.66657505256398,0.0794701993176932,
7.59394543036555));
#396887=CARTESIAN_POINT('Ctrl Pts',(-2.68221018451309,0.071599421415006,
7.57858609112103));
#396888=CARTESIAN_POINT('Ctrl Pts',(-2.6978278208432,0.0637374508656658,
7.56320440326857));
#396889=CARTESIAN_POINT('Ctrl Pts',(-2.71342887847494,0.0558838260887081,
7.54780169004651));
#396890=CARTESIAN_POINT('Ctrl Pts',(-2.72327836708049,0.0509255604647482,
7.53807742314383));
#396891=CARTESIAN_POINT('Ctrl Pts',(-2.73312125556166,0.0459706173655463,
7.52834476460825));
#396892=CARTESIAN_POINT('Ctrl Pts',(-2.742957758327,0.0410188888571374,
7.51860402984325));
#396893=CARTESIAN_POINT('',(-2.742957758327,0.0410188888571364,7.5));
#396894=CARTESIAN_POINT('Origin',(-2.66966635414557,0.0856110037871136,
7.5));
#396895=CARTESIAN_POINT('Ctrl Pts',(-2.66657505256398,0.0794701993176923,
8.85049129520029));
#396896=CARTESIAN_POINT('Ctrl Pts',(-2.66640207257255,0.0795572780259876,
8.85097269580138));
#396897=CARTESIAN_POINT('Ctrl Pts',(-2.66623505718387,0.0796507712154861,
8.85143669361005));
#396898=CARTESIAN_POINT('Ctrl Pts',(-2.66606674293477,0.0797557468338007,
8.8519052845931));
#396899=CARTESIAN_POINT('Ctrl Pts',(-2.66573753093763,0.0799610724859122,
8.85282181883899));
#396900=CARTESIAN_POINT('Ctrl Pts',(-2.66541192289281,0.0802052114460603,
8.85372622499636));
#396901=CARTESIAN_POINT('Ctrl Pts',(-2.66509405906801,0.0805043308840623,
8.85462257735071));
#396902=CARTESIAN_POINT('Ctrl Pts',(-2.66483017981012,0.0807526492177738,
8.85536669723986));
#396903=CARTESIAN_POINT('Ctrl Pts',(-2.66457155583132,0.0810388922212234,
8.85610498449051));
#396904=CARTESIAN_POINT('Ctrl Pts',(-2.66432647183546,0.0813776989232064,
8.85681338218371));
#396905=CARTESIAN_POINT('Ctrl Pts',(-2.66410405772431,0.0816851665373628,
8.85745625420284));
#396906=CARTESIAN_POINT('Ctrl Pts',(-2.66388951971436,0.0820394295508556,
8.85808743050666));
#396907=CARTESIAN_POINT('Ctrl Pts',(-2.66369852795532,0.0824644106006063,
8.8586680450841));
#396908=CARTESIAN_POINT('Ctrl Pts',(-2.6636104084979,0.0826604876445001,
8.85893592806395));
#396909=CARTESIAN_POINT('Ctrl Pts',(-2.66352745737671,0.0828718038816741,
8.85919241173848));
#396910=CARTESIAN_POINT('Ctrl Pts',(-2.66345240175596,0.0831017746528214,
8.85943017985534));
#396911=CARTESIAN_POINT('Ctrl Pts',(-2.6633510544491,0.0834123032725063,
8.8597512372));
#396912=CARTESIAN_POINT('Ctrl Pts',(-2.66326213239103,0.0837649471947974,
8.86004599534706));
#396913=CARTESIAN_POINT('Ctrl Pts',(-2.66319680292198,0.0841580160749979,
8.86026130871721));
#396914=CARTESIAN_POINT('Ctrl Pts',(-2.66317288396152,0.0843019296738245,
8.86034014101235));
#396915=CARTESIAN_POINT('Ctrl Pts',(-2.66315175613712,0.0844534219508058,
8.86040910639692));
#396916=CARTESIAN_POINT('Ctrl Pts',(-2.66313432821879,0.08460841204716,
8.86046313645506));
#396917=CARTESIAN_POINT('Ctrl Pts',(-2.66310713209819,0.0848502727944896,
8.86054744990829));
#396918=CARTESIAN_POINT('Ctrl Pts',(-2.66308834949246,0.085107269701868,
8.86059655985668));
#396919=CARTESIAN_POINT('Ctrl Pts',(-2.66307889280913,0.0853628994214006,
8.86059725258815));
#396920=CARTESIAN_POINT('Ctrl Pts',(-2.66306941427709,0.0856191197477102,
8.86059794692011));
#396921=CARTESIAN_POINT('Ctrl Pts',(-2.66307185464676,0.0858769062894261,
8.86056369958366));
#396922=CARTESIAN_POINT('Ctrl Pts',(-2.66308231788918,0.0861222348656925,
8.86048590497774));
#396923=CARTESIAN_POINT('Ctrl Pts',(-2.66308504848393,0.0861862583197862,
8.86046560290182));
#396924=CARTESIAN_POINT('Ctrl Pts',(-2.66308845150025,0.0862502623673663,
8.86044257503091));
#396925=CARTESIAN_POINT('Ctrl Pts',(-2.66309238900226,0.0863122709732421,
8.86041778462583));
#396926=CARTESIAN_POINT('Ctrl Pts',(-2.66311888350473,0.0867295119445202,
8.860250975962));
#396927=CARTESIAN_POINT('Ctrl Pts',(-2.66317346391551,0.0871123740750228,
8.8599848982295));
#396928=CARTESIAN_POINT('Ctrl Pts',(-2.66324614948998,0.0874508783645,8.85968173251461));
#396929=CARTESIAN_POINT('Ctrl Pts',(-2.66328459599449,0.08762992773965,
8.85952137522076));
#396930=CARTESIAN_POINT('Ctrl Pts',(-2.66332866234873,0.0878000580576475,
8.85934740853961));
#396931=CARTESIAN_POINT('Ctrl Pts',(-2.66337622222878,0.0879592598947022,
8.8591675900182));
#396932=CARTESIAN_POINT('Ctrl Pts',(-2.66356719986828,0.0885985380219589,
8.85844552518694));
#396933=CARTESIAN_POINT('Ctrl Pts',(-2.66382240283475,0.0890985976181652,
8.85759444184121));
#396934=CARTESIAN_POINT('Ctrl Pts',(-2.66406710350387,0.0894876295423664,
8.85683498915134));
#396935=CARTESIAN_POINT('Ctrl Pts',(-2.6640927107772,0.0895283406971491,
8.85675551444995));
#396936=CARTESIAN_POINT('Ctrl Pts',(-2.6641182175335,0.0895678222452543,
8.8566769979365));
#396937=CARTESIAN_POINT('Ctrl Pts',(-2.66414354718951,0.0896060969792497,
8.85659965593547));
#396938=CARTESIAN_POINT('Ctrl Pts',(-2.66448544817898,0.090122731291868,
8.85555568965886));
#396939=CARTESIAN_POINT('Ctrl Pts',(-2.66488864842986,0.0905698716063301,
8.85434650606346));
#396940=CARTESIAN_POINT('Ctrl Pts',(-2.66535052573303,0.0909538901841275,
8.85297329937118));
#396941=CARTESIAN_POINT('Ctrl Pts',(-2.66561030357346,0.0911698772355441,
8.85220095427748));
#396942=CARTESIAN_POINT('Ctrl Pts',(-2.66588895075784,0.0913657424487217,
8.85137579139184));
#396943=CARTESIAN_POINT('Ctrl Pts',(-2.66618796128141,0.0915411309427942,
8.85049129520029));
#396944=CARTESIAN_POINT('Origin',(-2.66966635414557,0.0856110037871136,
7.59394543036555));
#396945=CARTESIAN_POINT('Ctrl Pts',(-2.66607283329461,0.0797230181835987,
7.59443877723642));
#396946=CARTESIAN_POINT('Ctrl Pts',(-2.6609004580425,0.0823268092466506,
7.58783886950016));
#396947=CARTESIAN_POINT('Ctrl Pts',(-2.6628596569582,0.0905876034666598,
7.58559994247159));
#396948=CARTESIAN_POINT('Ctrl Pts',(-2.69430867804486,0.0655089991623795,
7.56670252222136));
#396949=CARTESIAN_POINT('Ctrl Pts',(-2.68914377834347,0.0681090270081165,
7.5600487499903));
#396950=CARTESIAN_POINT('Ctrl Pts',(-2.69109379729577,0.0764236997823088,
7.55786368756704));
#396951=CARTESIAN_POINT('Ctrl Pts',(-2.72249179517612,0.0513215234015378,
7.53888913333557));
#396952=CARTESIAN_POINT('Ctrl Pts',(-2.71729620022289,0.0539370033400496,
7.53222002137277));
#396953=CARTESIAN_POINT('Ctrl Pts',(-2.71927569050806,0.0622847014018697,
7.53005029815327));
#396954=CARTESIAN_POINT('Ctrl Pts',(-2.75062090938332,0.0371612328939311,
7.51101258149734));
#396955=CARTESIAN_POINT('Ctrl Pts',(-2.74536233437864,0.0398084172017556,
7.5043616886572));
#396956=CARTESIAN_POINT('Ctrl Pts',(-2.74740398125597,0.0481713807657634,
7.50217374673251));
#396957=CARTESIAN_POINT('',(-2.7459030190682,0.0489244847658708,7.50366116523517));
#396958=CARTESIAN_POINT('Ctrl Pts',(-2.742957758327,0.0410188888571359,
7.51860402984325));
#396959=CARTESIAN_POINT('Ctrl Pts',(-2.74335220896362,0.0408203210826832,
7.51734760759493));
#396960=CARTESIAN_POINT('Ctrl Pts',(-2.74373540389156,0.040694029724391,
7.51608817408572));
#396961=CARTESIAN_POINT('Ctrl Pts',(-2.74411064161436,0.0406529878647785,
7.51481005913119));
#396962=CARTESIAN_POINT('Ctrl Pts',(-2.74445054091028,0.0406158111676145,
7.51365231206383));
#396963=CARTESIAN_POINT('Ctrl Pts',(-2.74478436310084,0.0406482820382755,
7.51247773061043));
#396964=CARTESIAN_POINT('Ctrl Pts',(-2.74510275703971,0.0407865901995139,
7.51129758471022));
#396965=CARTESIAN_POINT('Ctrl Pts',(-2.74549848434376,0.040958491448545,
7.50983079813402));
#396966=CARTESIAN_POINT('Ctrl Pts',(-2.74585255978126,0.0413003464691624,
7.50839324291155));
#396967=CARTESIAN_POINT('Ctrl Pts',(-2.74611030637721,0.0418739583266141,
7.50715379678855));
#396968=CARTESIAN_POINT('Ctrl Pts',(-2.74622937787774,0.0421389504765283,
7.50658120839351));
#396969=CARTESIAN_POINT('Ctrl Pts',(-2.74633615125543,0.0424949690086202,
7.50598221009429));
#396970=CARTESIAN_POINT('Ctrl Pts',(-2.74640629772534,0.0429400755341853,
7.50545747549611));
#396971=CARTESIAN_POINT('Ctrl Pts',(-2.74644373005291,0.0431775981535625,
7.50517746087247));
#396972=CARTESIAN_POINT('Ctrl Pts',(-2.74647133836043,0.0434430337172244,
7.50491486231392));
#396973=CARTESIAN_POINT('Ctrl Pts',(-2.74648673246716,0.0437295256058998,
7.50468370960992));
#396974=CARTESIAN_POINT('Ctrl Pts',(-2.74650975151252,0.0441579213482125,
7.50433806340446));
#396975=CARTESIAN_POINT('Ctrl Pts',(-2.74650559437033,0.0446462741969512,
7.50405484070984));
#396976=CARTESIAN_POINT('Ctrl Pts',(-2.74647382464731,0.0451616883976327,
7.50385766036131));
#396977=CARTESIAN_POINT('Ctrl Pts',(-2.74647042736924,0.0452168039350443,
7.50383657498791));
#396978=CARTESIAN_POINT('Ctrl Pts',(-2.74646673024033,0.0452722054311037,
7.50381643264937));
#396979=CARTESIAN_POINT('Ctrl Pts',(-2.746462744543,0.0453278357777885,
7.50379723213559));
#396980=CARTESIAN_POINT('Ctrl Pts',(-2.74643613870952,0.0456991865398658,
7.50366906242519));
#396981=CARTESIAN_POINT('Ctrl Pts',(-2.74639537831869,0.0460887612390877,
7.50358235568538));
#396982=CARTESIAN_POINT('Ctrl Pts',(-2.74634706402189,0.0464633189002832,
7.5035341175365));
#396983=CARTESIAN_POINT('Ctrl Pts',(-2.74627462220196,0.0470249257215047,
7.50346178989176));
#396984=CARTESIAN_POINT('Ctrl Pts',(-2.74617281241575,0.0476260067194705,
7.50346967198527));
#396985=CARTESIAN_POINT('Ctrl Pts',(-2.74605471011437,0.0482130066995933,
7.50354272648692));
#396986=CARTESIAN_POINT('Ctrl Pts',(-2.74600613219324,0.0484544519415974,
7.50357277531559));
#396987=CARTESIAN_POINT('Ctrl Pts',(-2.74595500138298,0.0486932220575937,
7.50361331098761));
#396988=CARTESIAN_POINT('Ctrl Pts',(-2.74590301906962,0.048924484765896,
7.50366116523658));
#396989=CARTESIAN_POINT('',(-2.67259277500764,0.0857048484084221,7.57603338622103));
#396990=CARTESIAN_POINT('Origin',(-2.68142508174932,0.0859909379370601,
7.58486873427631));
#396991=CARTESIAN_POINT('Ctrl Pts',(-2.74590301911683,0.0489244847354774,
7.50366116529969));
#396992=CARTESIAN_POINT('Ctrl Pts',(-2.72150652165033,0.0611653470485632,
7.52783573079709));
#396993=CARTESIAN_POINT('Ctrl Pts',(-2.69707093545121,0.0734249054175621,
7.55196141284069));
#396994=CARTESIAN_POINT('Ctrl Pts',(-2.6725927759226,0.0857048475537328,
7.57603338728831));
#396995=CARTESIAN_POINT('Ctrl Pts',(-2.66757268996772,0.0791648222868977,
7.59639677331371));
#396996=CARTESIAN_POINT('Ctrl Pts',(-2.65015302674541,0.0846990113849867,
7.59959882295467));
#396997=CARTESIAN_POINT('Ctrl Pts',(-2.66699621741726,0.0918415417907545,
7.59642833564546));
#396998=CARTESIAN_POINT('Ctrl Pts',(-2.66371363323712,0.0797329642003343,
7.58707626057421));
#396999=CARTESIAN_POINT('Ctrl Pts',(-2.65970333131362,0.0851946278222303,
7.58809943920599));
#397000=CARTESIAN_POINT('Ctrl Pts',(-2.66325601572751,0.0909472649782365,
7.58710240504252));
#397001=CARTESIAN_POINT('Ctrl Pts',(-2.66854352902493,0.08342047541259,
7.58015376756929));
#397002=CARTESIAN_POINT('Ctrl Pts',(-2.6665714763732,0.0854796693653381,
7.58205880659761));
#397003=CARTESIAN_POINT('Ctrl Pts',(-2.66835205186191,0.0876606384084056,
7.58020924244127));
#397004=CARTESIAN_POINT('Ctrl Pts',(-2.6725927741805,0.0857048483816951,
7.57603338509286));
#397005=CARTESIAN_POINT('Ctrl Pts',(-2.6725927741805,0.0857048483816951,
7.57603338509286));
#397006=CARTESIAN_POINT('Ctrl Pts',(-2.6725927741805,0.0857048483816951,
7.57603338509286));
#397007=CARTESIAN_POINT('Origin',(-2.68142526464777,0.0859852345166785,
7.58486873427621));
#397008=CARTESIAN_POINT('Ctrl Pts',(-2.74737378111305,0.139161724727721,
7.51098857897448));
#397009=CARTESIAN_POINT('Ctrl Pts',(-2.74229559293695,0.136183047702606,
7.50433767179956));
#397010=CARTESIAN_POINT('Ctrl Pts',(-2.74486888698932,0.127968048688456,
7.50214974420965));
#397011=CARTESIAN_POINT('Ctrl Pts',(-2.72020190103144,0.123223706654827,
7.53887321589166));
#397012=CARTESIAN_POINT('Ctrl Pts',(-2.71518455856185,0.120280719466672,
7.5322040745206));
#397013=CARTESIAN_POINT('Ctrl Pts',(-2.71769481849935,0.112076969411473,
7.53003438070911));
#397014=CARTESIAN_POINT('Ctrl Pts',(-2.69297784091682,0.107255081707971,
7.56669465659235));
#397015=CARTESIAN_POINT('Ctrl Pts',(-2.68799015000839,0.104329487026961,
7.56004085833303));
#397016=CARTESIAN_POINT('Ctrl Pts',(-2.69046887318185,0.0961568141743418,
7.55785582193789));
#397017=CARTESIAN_POINT('Ctrl Pts',(-2.66570283200437,0.0912565720840829,
7.59443891967696));
#397018=CARTESIAN_POINT('Ctrl Pts',(-2.66070790956513,0.088326735655018,
7.58783901202978));
#397019=CARTESIAN_POINT('Ctrl Pts',(-2.6631923538447,0.0802084405994005,
7.58560008491213));
#397020=CARTESIAN_POINT('',(-2.74339586931974,0.127106646312599,7.50366116523517));
#397021=CARTESIAN_POINT('Ctrl Pts',(-2.74339586932012,0.127106646312616,
7.50366116523554));
#397022=CARTESIAN_POINT('Ctrl Pts',(-2.74351416422334,0.127855073886023,
7.50350835821027));
#397023=CARTESIAN_POINT('Ctrl Pts',(-2.74359855664032,0.128546909076729,
7.50345484955999));
#397024=CARTESIAN_POINT('Ctrl Pts',(-2.74365215170931,0.129202647995019,
7.50349758195598));
#397025=CARTESIAN_POINT('Ctrl Pts',(-2.74367964995442,0.129539090690968,
7.50351950684424));
#397026=CARTESIAN_POINT('Ctrl Pts',(-2.74370188030086,0.129899181821158,
7.50357029184312));
#397027=CARTESIAN_POINT('Ctrl Pts',(-2.7437137720588,0.130247002805257,
7.50365515313923));
#397028=CARTESIAN_POINT('Ctrl Pts',(-2.74373206639795,0.130782092325426,
7.50378570417639));
#397029=CARTESIAN_POINT('Ctrl Pts',(-2.74372677644016,0.131303837373427,
7.50400001621911));
#397030=CARTESIAN_POINT('Ctrl Pts',(-2.7436960345296,0.131772502555892,
7.50428903009634));
#397031=CARTESIAN_POINT('Ctrl Pts',(-2.74369262241404,0.131824520785452,
7.50432110841318));
#397032=CARTESIAN_POINT('Ctrl Pts',(-2.74368891228627,0.131875911139325,
7.50435406373354));
#397033=CARTESIAN_POINT('Ctrl Pts',(-2.7436849127999,0.131926638654744,
7.50438785222352));
#397034=CARTESIAN_POINT('Ctrl Pts',(-2.74366049401323,0.132236354519123,
7.50459414719561));
#397035=CARTESIAN_POINT('Ctrl Pts',(-2.74362438591049,0.132526252279303,
7.50483629897752));
#397036=CARTESIAN_POINT('Ctrl Pts',(-2.74357927772285,0.132785388698371,
7.5050991045531));
#397037=CARTESIAN_POINT('Ctrl Pts',(-2.74347976453025,0.133357069666624,
7.50567888004914));
#397038=CARTESIAN_POINT('Ctrl Pts',(-2.7433330401965,0.133801655626539,
7.50637912803145));
#397039=CARTESIAN_POINT('Ctrl Pts',(-2.74316491047449,0.134136160733225,
7.50710440483569));
#397040=CARTESIAN_POINT('Ctrl Pts',(-2.74312368172882,0.134218188026241,
7.50728225710685));
#397041=CARTESIAN_POINT('Ctrl Pts',(-2.74308047548245,0.134295294309571,
7.50746498566954));
#397042=CARTESIAN_POINT('Ctrl Pts',(-2.74303666373536,0.13436588331775,
7.50764697238949));
#397043=CARTESIAN_POINT('Ctrl Pts',(-2.74280114384032,0.134745350399101,
7.50862528291182));
#397044=CARTESIAN_POINT('Ctrl Pts',(-2.74253026271293,0.134973108351841,
7.50965856837422));
#397045=CARTESIAN_POINT('Ctrl Pts',(-2.74225148154245,0.135109500186557,
7.51067959873203));
#397046=CARTESIAN_POINT('Ctrl Pts',(-2.74209806791269,0.135184556785237,
7.51124147302579));
#397047=CARTESIAN_POINT('Ctrl Pts',(-2.74194203355346,0.135231572953966,
7.51180065547253));
#397048=CARTESIAN_POINT('Ctrl Pts',(-2.74178685108471,0.135258123151537,
7.51235175716501));
#397049=CARTESIAN_POINT('Ctrl Pts',(-2.74125063383784,0.135349864660484,
7.51425603304535));
#397050=CARTESIAN_POINT('Ctrl Pts',(-2.74065963140047,0.135202207805979,
7.51626900505179));
#397051=CARTESIAN_POINT('Ctrl Pts',(-2.74004940139841,0.134863920637417,
7.51827788969242));
#397052=CARTESIAN_POINT('Ctrl Pts',(-2.74001637459752,0.134845611896579,
7.51838661432544));
#397053=CARTESIAN_POINT('Ctrl Pts',(-2.73998328813306,0.13482673538106,
7.51849533314856));
#397054=CARTESIAN_POINT('Ctrl Pts',(-2.73995014666366,0.134807295823081,
7.51860402984325));
#397055=CARTESIAN_POINT('Ctrl Pts',(-2.67259277586714,0.0857048493202557,
7.57603338728985));
#397056=CARTESIAN_POINT('Ctrl Pts',(-2.69623386380305,0.0995278820670658,
7.55196141284922));
#397057=CARTESIAN_POINT('Ctrl Pts',(-2.7198337718876,0.113327845252936,
7.52783573083105));
#397058=CARTESIAN_POINT('Ctrl Pts',(-2.74339586936787,0.127106646347039,
7.50366116530176));
#397059=CARTESIAN_POINT('Origin',(-9.23504345990101E-16,2.96149868837368E-17,
7.49482233047033));
#397060=CARTESIAN_POINT('Origin',(-2.73706558693544,0.0487670258859518,
7.49482233047033));
#397061=CARTESIAN_POINT('Origin',(0.,0.,7.50366116523517));
#397062=CARTESIAN_POINT('Origin',(-2.73456650621404,0.126697565455551,7.49482233047033));
#397063=CARTESIAN_POINT('Ctrl Pts',(-2.74295681354276,0.0410193644145955,
7.51860402984325));
#397064=CARTESIAN_POINT('Ctrl Pts',(-2.74975348718602,0.0375986169206993,
7.51860402984324));
#397065=CARTESIAN_POINT('Ctrl Pts',(-2.74983646666349,0.0299901084968098,
7.51860402984325));
#397066=CARTESIAN_POINT('Ctrl Pts',(-2.74548046427814,0.0397492163906409,
7.51041458714366));
#397067=CARTESIAN_POINT('Ctrl Pts',(-2.74977313607579,0.0357960740206069,
7.51004642900442));
#397068=CARTESIAN_POINT('Ctrl Pts',(-2.74983648954825,0.0299880101605301,
7.50729136483009));
#397069=CARTESIAN_POINT('Ctrl Pts',(-2.74753566615836,0.0416727242358977,
7.50215815450138));
#397070=CARTESIAN_POINT('Ctrl Pts',(-2.74973326936515,0.0394662327613908,
7.49877163671531));
#397071=CARTESIAN_POINT('Ctrl Pts',(-2.74979474906121,0.0360165742505611,
7.49481588533172));
#397072=CARTESIAN_POINT('Ctrl Pts',(-2.74590246863753,0.0489244749591755,
7.50366171572174));
#397073=CARTESIAN_POINT('Ctrl Pts',(-2.74956360331414,0.0489897063698358,
7.50000045605858));
#397074=CARTESIAN_POINT('Ctrl Pts',(-2.74956360331414,0.0489897063697111,
7.49482233047317));
#397075=CARTESIAN_POINT('Origin',(-2.73733720999684,0.0298537898218249,
7.51860402984325));
#397076=CARTESIAN_POINT('Origin',(-2.73733720999684,0.0298537898218249,
9.));
#397077=CARTESIAN_POINT('Origin',(-2.73733720999684,0.029853789821825,8.75721825406948));
#397078=CARTESIAN_POINT('Ctrl Pts',(-2.72804102852879,0.0485279868834066,
8.78942910404913));
#397079=CARTESIAN_POINT('Ctrl Pts',(-2.73302745733453,0.0460404265390274,
8.7967269950169));
#397080=CARTESIAN_POINT('Ctrl Pts',(-2.73057741021293,0.0374572595778216,
8.79893251111267));
#397081=CARTESIAN_POINT('Ctrl Pts',(-2.73786125836976,0.0435844552904106,
8.78111911759583));
#397082=CARTESIAN_POINT('Ctrl Pts',(-2.74376940455713,0.0406287626889506,
8.78644465894815));
#397083=CARTESIAN_POINT('Ctrl Pts',(-2.74326787028547,0.0325377815896275,
8.78817647674132));
#397084=CARTESIAN_POINT('Ctrl Pts',(-2.74398145982695,0.0405035284588668,
8.76780923932029));
#397085=CARTESIAN_POINT('Ctrl Pts',(-2.75095349703021,0.0370099008303957,
8.76988516158372));
#397086=CARTESIAN_POINT('Ctrl Pts',(-2.75119007538758,0.0294547429182708,
8.77093053738833));
#397087=CARTESIAN_POINT('Ctrl Pts',(-2.74278810430285,0.0411042670240238,
8.75371302330492));
#397088=CARTESIAN_POINT('Ctrl Pts',(-2.74958936735954,0.0376970655034874,
8.75300828287559));
#397089=CARTESIAN_POINT('Ctrl Pts',(-2.74964475769837,0.0300556342733736,
8.75267964240738));
#397090=CARTESIAN_POINT('Origin',(-2.72481212943181,0.0361589574188426,
8.78727029226991));
#397091=CARTESIAN_POINT('Ctrl Pts',(-2.66657505256398,0.0794701993176923,
8.85049129520029));
#397092=CARTESIAN_POINT('Ctrl Pts',(-2.67179104362696,0.0768444519090519,
8.85711686593484));
#397093=CARTESIAN_POINT('Ctrl Pts',(-2.66979042840331,0.0685319131367625,
8.85933012996512));
#397094=CARTESIAN_POINT('Ctrl Pts',(-2.68789189731877,0.0687392281178933,
8.82945683644722));
#397095=CARTESIAN_POINT('Ctrl Pts',(-2.69315118426123,0.0660916854182248,
8.83607469902389));
#397096=CARTESIAN_POINT('Ctrl Pts',(-2.69110823399166,0.0577635165502321,
8.83829567148519));
#397097=CARTESIAN_POINT('Ctrl Pts',(-2.70917696759746,0.0580242522960096,
8.80838214965002));
#397098=CARTESIAN_POINT('Ctrl Pts',(-2.71445701014171,0.0553662611567229,
8.81501364461988));
#397099=CARTESIAN_POINT('Ctrl Pts',(-2.71239400300152,0.0470120517904829,
8.81722098428721));
#397100=CARTESIAN_POINT('Ctrl Pts',(-2.73043267776197,0.047324056454154,
8.78727029226991));
#397101=CARTESIAN_POINT('Ctrl Pts',(-2.73571359733862,0.0446656238137969,
8.79393457792714));
#397102=CARTESIAN_POINT('Ctrl Pts',(-2.73365018604124,0.0362762407020289,
8.79610912703474));
#397103=CARTESIAN_POINT('Origin',(-2.66095450423382,0.0683051002823809,
8.85049129520029));
#397104=CARTESIAN_POINT('Ctrl Pts',(-2.66618796128141,0.0915411309427942,
8.85049129520029));
#397105=CARTESIAN_POINT('Ctrl Pts',(-2.67122500331725,0.0944956731665959,
8.85711686593485));
#397106=CARTESIAN_POINT('Ctrl Pts',(-2.66869591238441,0.102662953078985,
8.85933012996512));
#397107=CARTESIAN_POINT('Ctrl Pts',(-2.66173176290277,0.0889272900866667,
8.86332496987232));
#397108=CARTESIAN_POINT('Ctrl Pts',(-2.66186606778202,0.0935461488825231,
8.86648636486737));
#397109=CARTESIAN_POINT('Ctrl Pts',(-2.65623818394787,0.095335848701524,
8.87206031107457));
#397110=CARTESIAN_POINT('Ctrl Pts',(-2.6619291835004,0.0818089453982159,
8.86341338519876));
#397111=CARTESIAN_POINT('Ctrl Pts',(-2.66233087922226,0.0771924411816848,
8.8665458496606));
#397112=CARTESIAN_POINT('Ctrl Pts',(-2.65678837264069,0.075093685936153,
8.87215952290714));
#397113=CARTESIAN_POINT('Ctrl Pts',(-2.66657505256398,0.0794701993176923,
8.85049129520029));
#397114=CARTESIAN_POINT('Ctrl Pts',(-2.67179104362696,0.0768444519090517,
8.85711686593484));
#397115=CARTESIAN_POINT('Ctrl Pts',(-2.66979042840331,0.0685319131367627,
8.85933012996512));
#397116=CARTESIAN_POINT('Origin',(-2.65986361061929,0.102323180316759,8.85049129520029));
#397117=CARTESIAN_POINT('Ctrl Pts',(-2.72785477369492,0.127712598202037,
8.78727029226991));
#397118=CARTESIAN_POINT('Ctrl Pts',(-2.73295451669186,0.130703918486395,
8.79393457792714));
#397119=CARTESIAN_POINT('Ctrl Pts',(-2.73035783527281,0.138943861495067,
8.79610912703474));
#397120=CARTESIAN_POINT('Ctrl Pts',(-2.70732829956804,0.115672529034048,
8.80838214965003));
#397121=CARTESIAN_POINT('Ctrl Pts',(-2.71242719562158,0.1186633525328,8.81501364461989));
#397122=CARTESIAN_POINT('Ctrl Pts',(-2.70983317111897,0.126868219958618,
8.81722098428721));
#397123=CARTESIAN_POINT('Ctrl Pts',(-2.68677347260706,0.103615829144114,
8.82945683644724));
#397124=CARTESIAN_POINT('Ctrl Pts',(-2.69185232513724,0.106594895854727,
8.8360746990239));
#397125=CARTESIAN_POINT('Ctrl Pts',(-2.6892799847167,0.114775061333389,
8.8382956714852));
#397126=CARTESIAN_POINT('Ctrl Pts',(-2.66618796128141,0.0915411309427942,
8.85049129520029));
#397127=CARTESIAN_POINT('Ctrl Pts',(-2.67122500331725,0.0944956731665958,
8.85711686593484));
#397128=CARTESIAN_POINT('Ctrl Pts',(-2.66869591238441,0.102662953078985,
8.85933012996512));
#397129=CARTESIAN_POINT('Origin',(-2.72153042303281,0.138494647576002,8.78727029226991));
#397130=CARTESIAN_POINT('Ctrl Pts',(-2.73979042401482,0.134713629821695,
8.75374538247848));
#397131=CARTESIAN_POINT('Ctrl Pts',(-2.74635165306265,0.138546990197332,
8.75304829418602));
#397132=CARTESIAN_POINT('Ctrl Pts',(-2.74592344570741,0.146168491471352,
8.75272238421917));
#397133=CARTESIAN_POINT('Ctrl Pts',(-2.74092899456704,0.135381472626339,
8.76769408445018));
#397134=CARTESIAN_POINT('Ctrl Pts',(-2.74765498512005,0.13931189322122,
8.76974318093969));
#397135=CARTESIAN_POINT('Ctrl Pts',(-2.74741055885273,0.146858986243038,
8.7707786988043));
#397136=CARTESIAN_POINT('Ctrl Pts',(-2.73509333052472,0.131958490841943,
8.78108014887993));
#397137=CARTESIAN_POINT('Ctrl Pts',(-2.74079528214875,0.135286100340894,
8.78639403366325));
#397138=CARTESIAN_POINT('Ctrl Pts',(-2.7397975286336,0.143318943153492,
8.78812224174742));
#397139=CARTESIAN_POINT('Ctrl Pts',(-2.72552996537758,0.126348979358604,
8.78944554828685));
#397140=CARTESIAN_POINT('Ctrl Pts',(-2.73033818026369,0.129148530613003,
8.79673892988686));
#397141=CARTESIAN_POINT('Ctrl Pts',(-2.72734888397413,0.137548986672627,
8.79894799272499));
#397142=CARTESIAN_POINT('Origin',(-2.73362579600155,0.145589345197042,8.75721825406948));
#397143=CARTESIAN_POINT('Origin',(-2.73362579600155,0.145589345197042,9.));
#397144=CARTESIAN_POINT('Origin',(-2.73362579600155,0.145589345197042,7.51860402984325));
#397145=CARTESIAN_POINT('Ctrl Pts',(-2.74339508349897,0.127106609904114,
7.50366195182966));
#397146=CARTESIAN_POINT('Ctrl Pts',(-2.74705311126524,0.127276093151834,
7.50000065167735));
#397147=CARTESIAN_POINT('Ctrl Pts',(-2.74705311126523,0.127276093151951,
7.49482233047108));
#397148=CARTESIAN_POINT('Ctrl Pts',(-2.744560462474,0.134454785967003,7.50215800491337));
#397149=CARTESIAN_POINT('Ctrl Pts',(-2.74661186251359,0.136799237939623,
7.49877273257265));
#397150=CARTESIAN_POINT('Ctrl Pts',(-2.74645211423604,0.140247663208896,
7.49481816995649));
#397151=CARTESIAN_POINT('Ctrl Pts',(-2.74238152832947,0.136233061068291,
7.51043025814043));
#397152=CARTESIAN_POINT('Ctrl Pts',(-2.74641706184182,0.140452921996988,
7.51006209594515));
#397153=CARTESIAN_POINT('Ctrl Pts',(-2.7461079709193,0.146256665010245,
7.50731281821699));
#397154=CARTESIAN_POINT('Ctrl Pts',(-2.73994884293186,0.134806531208245,
7.51860402984326));
#397155=CARTESIAN_POINT('Ctrl Pts',(-2.74651279192828,0.138655633826135,
7.51860402984327));
#397156=CARTESIAN_POINT('Ctrl Pts',(-2.74610810557233,0.146254136727627,
7.51860402984327));
#397157=CARTESIAN_POINT('Origin',(0.,0.,7.5));
#397158=CARTESIAN_POINT('Origin',(-2.66657505256398,-0.0794701993177115,
7.5));
#397159=CARTESIAN_POINT('',(-2.66657505256398,-0.0794701993177115,7.59394543036555));
#397160=CARTESIAN_POINT('',(-2.66657505256398,-0.0794701993177115,8.85049129520029));
#397161=CARTESIAN_POINT('',(-2.66657505256398,-0.0794701993177115,7.5));
#397162=CARTESIAN_POINT('',(-2.73043267776197,-0.0473240564541737,8.78727029226991));
#397163=CARTESIAN_POINT('Ctrl Pts',(-2.66657505256398,-0.0794701993177114,
8.85049129520029));
#397164=CARTESIAN_POINT('Ctrl Pts',(-2.68789186871081,-0.0687392425192531,
8.82945686509571));
#397165=CARTESIAN_POINT('Ctrl Pts',(-2.70917699483285,-0.0580242385856441,
8.80838212259895));
#397166=CARTESIAN_POINT('Ctrl Pts',(-2.73043267776197,-0.0473240564541735,
8.78727029226991));
#397167=CARTESIAN_POINT('',(-2.742957758327,-0.0410188888571562,8.75721825406948));
#397168=CARTESIAN_POINT('Origin',(-2.70526553666451,-0.0599935056863788,
8.75937679713089));
#397169=CARTESIAN_POINT('',(-2.742957758327,-0.0410188888571562,7.51860402984325));
#397170=CARTESIAN_POINT('',(-2.742957758327,-0.0410188888571562,7.5));
#397171=CARTESIAN_POINT('Ctrl Pts',(-2.742957758327,-0.0410188888571564,
7.51860402984325));
#397172=CARTESIAN_POINT('Ctrl Pts',(-2.73312125556167,-0.0459706173655643,
7.52834476460825));
#397173=CARTESIAN_POINT('Ctrl Pts',(-2.72327836708068,-0.0509255604646721,
7.53807742314407));
#397174=CARTESIAN_POINT('Ctrl Pts',(-2.71342887847514,-0.0558838260886309,
7.54780169004674));
#397175=CARTESIAN_POINT('Ctrl Pts',(-2.69782782084339,-0.0637374508655898,
7.5632044032688));
#397176=CARTESIAN_POINT('Ctrl Pts',(-2.68221018451309,-0.0715994214150238,
7.57858609112103));
#397177=CARTESIAN_POINT('Ctrl Pts',(-2.66657505256398,-0.0794701993177118,
7.59394543036555));
#397178=CARTESIAN_POINT('Origin',(-2.90339304750863,-0.230676845509337,
7.5));
#397179=CARTESIAN_POINT('',(-2.73995014666366,-0.134807295823097,8.75721825406948));
#397180=CARTESIAN_POINT('',(-2.72785477369492,-0.127712598202056,8.78727029226991));
#397181=CARTESIAN_POINT('Origin',(-2.6971522057511,-0.109703609449603,8.75658640621057));
#397182=CARTESIAN_POINT('',(-2.66618796128141,-0.0915411309428133,8.85049129520029));
#397183=CARTESIAN_POINT('Ctrl Pts',(-2.72785477369492,-0.127712598202057,
8.78727029226991));
#397184=CARTESIAN_POINT('Ctrl Pts',(-2.70732832586903,-0.115672544461257,
8.80838212259895));
#397185=CARTESIAN_POINT('Ctrl Pts',(-2.68677344498056,-0.103615812939454,
8.82945686509571));
#397186=CARTESIAN_POINT('Ctrl Pts',(-2.66618796128141,-0.0915411309428135,
8.85049129520029));
#397187=CARTESIAN_POINT('',(-2.66618796128141,-0.0915411309428133,7.59394543036555));
#397188=CARTESIAN_POINT('',(-2.66618796128141,-0.0915411309428133,7.5));
#397189=CARTESIAN_POINT('',(-2.73995014666366,-0.134807295823097,7.51860402984325));
#397190=CARTESIAN_POINT('Ctrl Pts',(-2.66618796128141,-0.0915411309428125,
7.59394543036555));
#397191=CARTESIAN_POINT('Ctrl Pts',(-2.68128668670342,-0.100397483831567,
7.57858609112103));
#397192=CARTESIAN_POINT('Ctrl Pts',(-2.69636851674213,-0.109243926514469,
7.56320440326857));
#397193=CARTESIAN_POINT('Ctrl Pts',(-2.71143433686065,-0.118080978371422,
7.54780169004651));
#397194=CARTESIAN_POINT('Ctrl Pts',(-2.72094591146625,-0.12366011560854,
7.53807742314383));
#397195=CARTESIAN_POINT('Ctrl Pts',(-2.73045111238304,-0.129235514275963,
7.52834476460825));
#397196=CARTESIAN_POINT('Ctrl Pts',(-2.73995014666366,-0.134807295823096,
7.51860402984325));
#397197=CARTESIAN_POINT('',(-2.73995014666366,-0.134807295823097,7.5));
#397198=CARTESIAN_POINT('Origin',(-2.66966635414557,-0.0856110037871328,
7.5));
#397199=CARTESIAN_POINT('Ctrl Pts',(-2.66618796128141,-0.0915411309428132,
8.85049129520029));
#397200=CARTESIAN_POINT('Ctrl Pts',(-2.66602091584792,-0.0914431482809603,
8.85097269580138));
#397201=CARTESIAN_POINT('Ctrl Pts',(-2.66586023373949,-0.0913391464705544,
8.85143669361005));
#397202=CARTESIAN_POINT('Ctrl Pts',(-2.66569899112102,-0.0912236026049402,
8.8519052845931));
#397203=CARTESIAN_POINT('Ctrl Pts',(-2.66538361078493,-0.0909976061313247,
8.85282181883899));
#397204=CARTESIAN_POINT('Ctrl Pts',(-2.66507431377364,-0.0907331070017954,
8.85372622499635));
#397205=CARTESIAN_POINT('Ctrl Pts',(-2.66477626768236,-0.0904142365315805,
8.85462257735071));
#397206=CARTESIAN_POINT('Ctrl Pts',(-2.66452884040296,-0.0901495215924163,
8.85536669723986));
#397207=CARTESIAN_POINT('Ctrl Pts',(-2.66428908744707,-0.0898472966107034,
8.85610498449051));
#397208=CARTESIAN_POINT('Ctrl Pts',(-2.66406621442249,-0.0894934834378981,
8.85681338218371));
#397209=CARTESIAN_POINT('Ctrl Pts',(-2.66386395680266,-0.0891723974279031,
8.85745625420285));
#397210=CARTESIAN_POINT('Ctrl Pts',(-2.66367255729327,-0.0888051167882754,
8.85808743050666));
#397211=CARTESIAN_POINT('Ctrl Pts',(-2.66350918657663,-0.0883687720236555,
8.8586680450841));
#397212=CARTESIAN_POINT('Ctrl Pts',(-2.66343381086941,-0.0881674520080548,
8.85893592806396));
#397213=CARTESIAN_POINT('Ctrl Pts',(-2.66336456925801,-0.0879512552461709,
8.85919241173848));
#397214=CARTESIAN_POINT('Ctrl Pts',(-2.66330440212497,-0.0877169481445036,
8.85943017985534));
#397215=CARTESIAN_POINT('Ctrl Pts',(-2.66322315868399,-0.0874005641949268,
8.8597512372));
#397216=CARTESIAN_POINT('Ctrl Pts',(-2.6631570132995,-0.0870429475615733,
8.86004599534705));
#397217=CARTESIAN_POINT('Ctrl Pts',(-2.66311700206647,-0.08664650061009,
8.86026130871721));
#397218=CARTESIAN_POINT('Ctrl Pts',(-2.66310235282603,-0.0865013502041289,
8.86034014101235));
#397219=CARTESIAN_POINT('Ctrl Pts',(-2.66309097455451,-0.0863488155199207,
8.86040910639693));
#397220=CARTESIAN_POINT('Ctrl Pts',(-2.66308351269328,-0.0861930272567808,
8.86046313645507));
#397221=CARTESIAN_POINT('Ctrl Pts',(-2.66307186852132,-0.0859499209768667,
8.8605474499083));
#397222=CARTESIAN_POINT('Ctrl Pts',(-2.66306959035485,-0.0856922486915159,
8.86059655985668));
#397223=CARTESIAN_POINT('Ctrl Pts',(-2.66307653135366,-0.0854365382988774,
8.86059725258816));
#397224=CARTESIAN_POINT('Ctrl Pts',(-2.66308348838895,-0.0851802371130747,
8.86059794692011));
#397225=CARTESIAN_POINT('Ctrl Pts',(-2.66310244018505,-0.0849231365764772,
8.86056369958366));
#397226=CARTESIAN_POINT('Ctrl Pts',(-2.66312860018547,-0.0846789824363259,
8.86048590497774));
#397227=CARTESIAN_POINT('Ctrl Pts',(-2.6631354271667,-0.0846152654750911,
8.86046560290182));
#397228=CARTESIAN_POINT('Ctrl Pts',(-2.66314292394457,-0.0845516109626956,
8.86044257503091));
#397229=CARTESIAN_POINT('Ctrl Pts',(-2.66315082626158,-0.0844899820367707,
8.86041778462583));
#397230=CARTESIAN_POINT('Ctrl Pts',(-2.66320399904907,-0.0840752958404186,
8.86025097596201));
#397231=CARTESIAN_POINT('Ctrl Pts',(-2.66328299737946,-0.0836967173201501,
8.8599848982295));
#397232=CARTESIAN_POINT('Ctrl Pts',(-2.66337722165792,-0.0833635655047856,
8.85968173251461));
#397233=CARTESIAN_POINT('Ctrl Pts',(-2.66342706090281,-0.083187347281781,
8.85952137522076));
#397234=CARTESIAN_POINT('Ctrl Pts',(-2.66348193700491,-0.0830203898557786,
8.85934740853961));
#397235=CARTESIAN_POINT('Ctrl Pts',(-2.66353959926479,-0.0828645622879489,
8.8591675900182));
#397236=CARTESIAN_POINT('Ctrl Pts',(-2.6637711432105,-0.0822388336055553,
8.85844552518695));
#397237=CARTESIAN_POINT('Ctrl Pts',(-2.66405786076342,-0.0817561523456297,
8.85759444184125));
#397238=CARTESIAN_POINT('Ctrl Pts',(-2.66432698402973,-0.0813835977549439,
8.85683498915139));
#397239=CARTESIAN_POINT('Ctrl Pts',(-2.66435514706282,-0.0813446109092215,
8.85675551444999));
#397240=CARTESIAN_POINT('Ctrl Pts',(-2.66438313100423,-0.0813068447036701,
8.85667699793651));
#397241=CARTESIAN_POINT('Ctrl Pts',(-2.66441086088839,-0.081270271485846,
8.85659965593547));
#397242=CARTESIAN_POINT('Ctrl Pts',(-2.66478516027966,-0.0807766043254381,
8.85555568965886));
#397243=CARTESIAN_POINT('Ctrl Pts',(-2.66521618049069,-0.0803562158374777,
8.85434650606346));
#397244=CARTESIAN_POINT('Ctrl Pts',(-2.66570171297216,-0.0800025788474523,
8.85297329937118));
#397245=CARTESIAN_POINT('Ctrl Pts',(-2.66597479540906,-0.079803679587981,
8.85220095427748));
#397246=CARTESIAN_POINT('Ctrl Pts',(-2.6662654192102,-0.0796260697872908,
8.85137579139184));
#397247=CARTESIAN_POINT('Ctrl Pts',(-2.66657505256398,-0.0794701993177116,
8.85049129520029));
#397248=CARTESIAN_POINT('Origin',(-2.66966635414557,-0.0856110037871328,
7.59394543036555));
#397249=CARTESIAN_POINT('Ctrl Pts',(-2.66570297203574,-0.0912566542213146,
7.59443877723642));
#397250=CARTESIAN_POINT('Ctrl Pts',(-2.66070804944951,-0.0883268177060317,
7.58783886950016));
#397251=CARTESIAN_POINT('Ctrl Pts',(-2.66319249388382,-0.0802085224792304,
7.58559994247159));
#397252=CARTESIAN_POINT('Ctrl Pts',(-2.69297010788915,-0.107250545800486,
7.56670252222133));
#397253=CARTESIAN_POINT('Ctrl Pts',(-2.68798240438414,-0.104324943730775,
7.56004874999027));
#397254=CARTESIAN_POINT('Ctrl Pts',(-2.69046113972712,-0.0961522924867714,
7.55786368756704));
#397255=CARTESIAN_POINT('Ctrl Pts',(-2.7201863250907,-0.123214570385138,
7.53888913333561));
#397256=CARTESIAN_POINT('Ctrl Pts',(-2.71516897941958,-0.120271581319056,
7.53222002137279));
#397257=CARTESIAN_POINT('Ctrl Pts',(-2.71767924148075,-0.112067860876243,
7.53005029815327));
#397258=CARTESIAN_POINT('Ctrl Pts',(-2.74735039208809,-0.139148005592317,
7.51101258149734));
#397259=CARTESIAN_POINT('Ctrl Pts',(-2.74227222707067,-0.136169342151228,
7.5043616886572));
#397260=CARTESIAN_POINT('Ctrl Pts',(-2.74484549608077,-0.127954369957341,
7.50217374673251));
#397261=CARTESIAN_POINT('',(-2.74339586931974,-0.127106646312618,7.50366116523517));
#397262=CARTESIAN_POINT('Ctrl Pts',(-2.73995014666366,-0.134807295823097,
7.51860402984325));
#397263=CARTESIAN_POINT('Ctrl Pts',(-2.74033106457815,-0.13503072815782,
7.51734760759494));
#397264=CARTESIAN_POINT('Ctrl Pts',(-2.74070538067591,-0.1351813114203,
7.51608817408573));
#397265=CARTESIAN_POINT('Ctrl Pts',(-2.74107721787159,-0.135246310518456,
7.51481005913121));
#397266=CARTESIAN_POINT('Ctrl Pts',(-2.74141403688878,-0.13530518825477,
7.51365231206384));
#397267=CARTESIAN_POINT('Ctrl Pts',(-2.74174925362168,-0.13529417216018,
7.51247773061043));
#397268=CARTESIAN_POINT('Ctrl Pts',(-2.74207585482037,-0.135176547737596,
7.51129758471022));
#397269=CARTESIAN_POINT('Ctrl Pts',(-2.74248178281107,-0.13503035401354,
7.50983079813402));
#397270=CARTESIAN_POINT('Ctrl Pts',(-2.74285703348899,-0.134711887061897,
7.50839324291155));
#397271=CARTESIAN_POINT('Ctrl Pts',(-2.74315100195479,-0.134155967632627,
7.50715379678855));
#397272=CARTESIAN_POINT('Ctrl Pts',(-2.7432868069155,-0.133899148874738,
7.50658120839351));
#397273=CARTESIAN_POINT('Ctrl Pts',(-2.7434161711015,-0.1335507028147,7.50598221009429));
#397274=CARTESIAN_POINT('Ctrl Pts',(-2.74351469152097,-0.133111005107987,
7.50545747549611));
#397275=CARTESIAN_POINT('Ctrl Pts',(-2.74356726506629,-0.132876368801768,
7.50517746087247));
#397276=CARTESIAN_POINT('Ctrl Pts',(-2.74361182316454,-0.132613247474275,
7.50491486231392));
#397277=CARTESIAN_POINT('Ctrl Pts',(-2.74364554124075,-0.132328330517715,
7.50468370960992));
#397278=CARTESIAN_POINT('Ctrl Pts',(-2.74369596040046,-0.131902289795704,
7.50433806340447));
#397279=CARTESIAN_POINT('Ctrl Pts',(-2.74372310067401,-0.131414673971259,
7.50405484070984));
#397280=CARTESIAN_POINT('Ctrl Pts',(-2.74372441892651,-0.130898283251192,
7.50385766036131));
#397281=CARTESIAN_POINT('Ctrl Pts',(-2.74372455989313,-0.130843063290206,
7.50383657498791));
#397282=CARTESIAN_POINT('Ctrl Pts',(-2.74372441994641,-0.130787538746595,
7.50381643264937));
#397283=CARTESIAN_POINT('Ctrl Pts',(-2.74372400668667,-0.130731767333915,
7.50379723213559));
#397284=CARTESIAN_POINT('Ctrl Pts',(-2.74372124804273,-0.130359474910201,
7.50366906242519));
#397285=CARTESIAN_POINT('Ctrl Pts',(-2.74370553153518,-0.129968089106774,
7.50358235568538));
#397286=CARTESIAN_POINT('Ctrl Pts',(-2.74368131449704,-0.129591205506841,
7.5035341175365));
#397287=CARTESIAN_POINT('Ctrl Pts',(-2.74364500378917,-0.129026111203727,
7.50346178989176));
#397288=CARTESIAN_POINT('Ctrl Pts',(-2.74358191457385,-0.128419742215738,
7.50346967198527));
#397289=CARTESIAN_POINT('Ctrl Pts',(-2.74350166414417,-0.127826381449601,
7.50354272648692));
#397290=CARTESIAN_POINT('Ctrl Pts',(-2.74346865548136,-0.127582319884648,
7.50357277531559));
#397291=CARTESIAN_POINT('Ctrl Pts',(-2.74343292777869,-0.127340764385202,
7.50361331098761));
#397292=CARTESIAN_POINT('Ctrl Pts',(-2.74339586932116,-0.127106646312684,
7.50366116523658));
#397293=CARTESIAN_POINT('',(-2.67259277500765,-0.0857048484080524,7.57603338622103));
#397294=CARTESIAN_POINT('Origin',(-2.68142526464731,-0.0859852345168127,
7.58486873427627));
#397295=CARTESIAN_POINT('Ctrl Pts',(-2.74339586936632,-0.127106646346066,
7.50366116529969));
#397296=CARTESIAN_POINT('Ctrl Pts',(-2.71983377186154,-0.113327845238004,
7.52783573079709));
#397297=CARTESIAN_POINT('Ctrl Pts',(-2.69623386379654,-0.0995278820633557,
7.55196141284068));
#397298=CARTESIAN_POINT('Ctrl Pts',(-2.67259277586597,-0.0857048493196056,
7.57603338728831));
#397299=CARTESIAN_POINT('Ctrl Pts',(-2.66716398335853,-0.0919097993916527,
7.59639677331372));
#397300=CARTESIAN_POINT('Ctrl Pts',(-2.64933465654095,-0.0849590058182218,
7.59974925422226));
#397301=CARTESIAN_POINT('Ctrl Pts',(-2.66757268996767,-0.0791648222869322,
7.59639677331371));
#397302=CARTESIAN_POINT('Ctrl Pts',(-2.66334925645125,-0.0910955741730429,
7.58707626057422));
#397303=CARTESIAN_POINT('Ctrl Pts',(-2.65963383141741,-0.0852892803103875,
7.58811717123965));
#397304=CARTESIAN_POINT('Ctrl Pts',(-2.66371363323709,-0.0797329642003973,
7.58707626057424));
#397305=CARTESIAN_POINT('Ctrl Pts',(-2.66840548835473,-0.0877250918337127,
7.5801537675693));
#397306=CARTESIAN_POINT('Ctrl Pts',(-2.66654166217443,-0.0855108009973929,
7.58208760766041));
#397307=CARTESIAN_POINT('Ctrl Pts',(-2.66854352902492,-0.0834204754125948,
7.5801537675693));
#397308=CARTESIAN_POINT('Ctrl Pts',(-2.6725927741805,-0.0857048483817295,
7.57603338509286));
#397309=CARTESIAN_POINT('Ctrl Pts',(-2.6725927741805,-0.0857048483817295,
7.57603338509286));
#397310=CARTESIAN_POINT('Ctrl Pts',(-2.6725927741805,-0.0857048483817295,
7.57603338509286));
#397311=CARTESIAN_POINT('Origin',(-2.6814250817504,-0.0859909379374167,
7.5848687342762));
#397312=CARTESIAN_POINT('Ctrl Pts',(-2.75064512934104,-0.0371490404859369,
7.51098857897448));
#397313=CARTESIAN_POINT('Ctrl Pts',(-2.74538653035493,-0.0397962368660951,
7.50433767179956));
#397314=CARTESIAN_POINT('Ctrl Pts',(-2.74742820050471,-0.0481592287997251,
7.50214974420965));
#397315=CARTESIAN_POINT('Ctrl Pts',(-2.72250792447726,-0.0513134038572253,
7.53887321589168));
#397316=CARTESIAN_POINT('Ctrl Pts',(-2.71731233283933,-0.0539288821268316,
7.53220407452062));
#397317=CARTESIAN_POINT('Ctrl Pts',(-2.71929181910785,-0.062276609604089,
7.53003438070911));
#397318=CARTESIAN_POINT('Ctrl Pts',(-2.69431668580073,-0.065504968031212,
7.5666946565923));
#397319=CARTESIAN_POINT('Ctrl Pts',(-2.6891517991434,-0.0681049893104966,
7.56004085833295));
#397320=CARTESIAN_POINT('Ctrl Pts',(-2.69110180456681,-0.0764196828691923,
7.55785582193789));
#397321=CARTESIAN_POINT('Ctrl Pts',(-2.6660726882884,-0.0797230911802304,
7.59443891967696));
#397322=CARTESIAN_POINT('Ctrl Pts',(-2.6609003131885,-0.0823268821666591,
7.58783901202978));
#397323=CARTESIAN_POINT('Ctrl Pts',(-2.66285951196075,-0.0905876762059219,
7.58560008491213));
#397324=CARTESIAN_POINT('',(-2.7459030190682,-0.0489244847658906,7.50366116523517));
#397325=CARTESIAN_POINT('Ctrl Pts',(-2.74590301906857,-0.0489244847658972,
7.50366116523554));
#397326=CARTESIAN_POINT('Ctrl Pts',(-2.7460690228415,-0.0481851740976808,
7.50350835821027));
#397327=CARTESIAN_POINT('Ctrl Pts',(-2.74619756789807,-0.0475001673972941,
7.50345484956));
#397328=CARTESIAN_POINT('Ctrl Pts',(-2.74629306618699,-0.0468492096127992,
7.50349758195598));
#397329=CARTESIAN_POINT('Ctrl Pts',(-2.74634206389154,-0.0465152199930655,
7.50351950684424));
#397330=CARTESIAN_POINT('Ctrl Pts',(-2.74638731968128,-0.046157293011909,
7.50357029184312));
#397331=CARTESIAN_POINT('Ctrl Pts',(-2.74642147197328,-0.0458109485708723,
7.50365515313923));
#397332=CARTESIAN_POINT('Ctrl Pts',(-2.74647401202802,-0.0452781305718466,
7.50378570417639));
#397333=CARTESIAN_POINT('Ctrl Pts',(-2.74650216125901,-0.0447571185762471,
7.50400001621911));
#397334=CARTESIAN_POINT('Ctrl Pts',(-2.74650150999234,-0.0442874466756935,
7.50428903009634));
#397335=CARTESIAN_POINT('Ctrl Pts',(-2.74650143770675,-0.0442353167081682,
7.50432110841318));
#397336=CARTESIAN_POINT('Ctrl Pts',(-2.74650102779312,-0.044183794232584,
7.50435406373354));
#397337=CARTESIAN_POINT('Ctrl Pts',(-2.7465002866472,-0.0441329146943119,
7.50438785222352));
#397338=CARTESIAN_POINT('Ctrl Pts',(-2.7464957615951,-0.0438222706573593,
7.50459414719561));
#397339=CARTESIAN_POINT('Ctrl Pts',(-2.7464783014936,-0.0435306550691341,
7.50483629897752));
#397340=CARTESIAN_POINT('Ctrl Pts',(-2.74644988891295,-0.0432691609821266,
7.5050991045531));
#397341=CARTESIAN_POINT('Ctrl Pts',(-2.74638720790626,-0.0426922787615938,
7.50567888004914));
#397342=CARTESIAN_POINT('Ctrl Pts',(-2.74626926975364,-0.0422392055908742,
7.50637912803144));
#397343=CARTESIAN_POINT('Ctrl Pts',(-2.74612291728795,-0.0418946156525315,
7.50710440483569));
#397344=CARTESIAN_POINT('Ctrl Pts',(-2.74608702875786,-0.0418101153585814,
7.50728225710685));
#397345=CARTESIAN_POINT('Ctrl Pts',(-2.7460488514999,-0.0417303992646702,
7.50746498566954));
#397346=CARTESIAN_POINT('Ctrl Pts',(-2.74600965242202,-0.0416571482609055,
7.50764697238949));
#397347=CARTESIAN_POINT('Ctrl Pts',(-2.74579892896725,-0.0412633710238883,
7.50862528291181));
#397348=CARTESIAN_POINT('Ctrl Pts',(-2.74554319689632,-0.041018725610869,
7.50965856837421));
#397349=CARTESIAN_POINT('Ctrl Pts',(-2.74527372716651,-0.0408647524368866,
7.51067959873201));
#397350=CARTESIAN_POINT('Ctrl Pts',(-2.7451254376343,-0.0407800208050308,
7.51124147302578));
#397351=CARTESIAN_POINT('Ctrl Pts',(-2.74497273620066,-0.0407231040803407,
7.51180065547252));
#397352=CARTESIAN_POINT('Ctrl Pts',(-2.74481957364794,-0.0406866658580891,
7.51235175716501));
#397353=CARTESIAN_POINT('Ctrl Pts',(-2.74429033601557,-0.0405607572849474,
7.51425603304535));
#397354=CARTESIAN_POINT('Ctrl Pts',(-2.74369108744894,-0.0406702451064386,
7.5162690050518));
#397355=CARTESIAN_POINT('Ctrl Pts',(-2.74306043709656,-0.0409687396572608,
7.51827788969243));
#397356=CARTESIAN_POINT('Ctrl Pts',(-2.74302630510772,-0.0409848947464281,
7.51838661432545));
#397357=CARTESIAN_POINT('Ctrl Pts',(-2.74299207720045,-0.0410016126210649,
7.51849533314856));
#397358=CARTESIAN_POINT('Ctrl Pts',(-2.742957758327,-0.0410188888571523,
7.51860402984325));
#397359=CARTESIAN_POINT('Ctrl Pts',(-2.67259277592381,-0.0857048475531615,
7.57603338728985));
#397360=CARTESIAN_POINT('Ctrl Pts',(-2.69707093545794,-0.0734249054142831,
7.55196141284922));
#397361=CARTESIAN_POINT('Ctrl Pts',(-2.7215065216773,-0.0611653470353149,
7.52783573083105));
#397362=CARTESIAN_POINT('Ctrl Pts',(-2.74590301911844,-0.0489244847346051,
7.50366116530176));
#397363=CARTESIAN_POINT('Origin',(-9.23504345990101E-16,-2.96149868837434E-17,
7.49482233047033));
#397364=CARTESIAN_POINT('Origin',(-2.73456650621404,-0.126697565455571,
7.49482233047033));
#397365=CARTESIAN_POINT('Origin',(0.,0.,7.50366116523517));
#397366=CARTESIAN_POINT('Origin',(-2.73706558693544,-0.0487670258859716,
7.49482233047033));
#397367=CARTESIAN_POINT('Ctrl Pts',(-2.73994923428965,-0.134806760710188,
7.51860402984325));
#397368=CARTESIAN_POINT('Ctrl Pts',(-2.74651277539354,-0.138655944286946,
7.51860402984325));
#397369=CARTESIAN_POINT('Ctrl Pts',(-2.74610810557233,-0.146254136727642,
7.51860402984325));
#397370=CARTESIAN_POINT('Ctrl Pts',(-2.74238632125063,-0.136235989936575,
7.51041458714365));
#397371=CARTESIAN_POINT('Ctrl Pts',(-2.74641689459241,-0.140456042578019,
7.51004642900442));
#397372=CARTESIAN_POINT('Ctrl Pts',(-2.7461079939692,-0.146256232218901,
7.50729136483009));
#397373=CARTESIAN_POINT('Ctrl Pts',(-2.74456054006895,-0.134448111381053,
7.50215815450138));
#397374=CARTESIAN_POINT('Ctrl Pts',(-2.7466122576701,-0.136790870303067,
7.4987716367153));
#397375=CARTESIAN_POINT('Ctrl Pts',(-2.74645259066989,-0.14023738013816,
7.49481588533172));
#397376=CARTESIAN_POINT('Ctrl Pts',(-2.74339531939168,-0.127106620832951,
7.50366171572174));
#397377=CARTESIAN_POINT('Ctrl Pts',(-2.74705311126526,-0.127276093151329,
7.50000045605858));
#397378=CARTESIAN_POINT('Ctrl Pts',(-2.74705311126525,-0.127276093151453,
7.49482233047317));
#397379=CARTESIAN_POINT('Origin',(-2.73362579600155,-0.145589345197061,
7.51860402984325));
#397380=CARTESIAN_POINT('Origin',(-2.73362579600155,-0.145589345197061,
9.));
#397381=CARTESIAN_POINT('Origin',(-2.73362579600155,-0.145589345197061,
8.75721825406948));
#397382=CARTESIAN_POINT('Ctrl Pts',(-2.72554517444904,-0.126357907884503,
8.78942910404912));
#397383=CARTESIAN_POINT('Ctrl Pts',(-2.73036197956352,-0.129159838859871,
8.79672699501691));
#397384=CARTESIAN_POINT('Ctrl Pts',(-2.72736704093116,-0.137568395725972,
8.79893251111267));
#397385=CARTESIAN_POINT('Ctrl Pts',(-2.73502849441794,-0.131920466747828,
8.78111911759583));
#397386=CARTESIAN_POINT('Ctrl Pts',(-2.74073512981015,-0.135248622787726,
8.78644465894813));
#397387=CARTESIAN_POINT('Ctrl Pts',(-2.73971623505555,-0.143290846687523,
8.78817647674132));
#397388=CARTESIAN_POINT('Ctrl Pts',(-2.74093872560498,-0.135387186138442,
8.76780923932029));
#397389=CARTESIAN_POINT('Ctrl Pts',(-2.74767260051939,-0.139320335691599,
8.76988516158374));
#397390=CARTESIAN_POINT('Ctrl Pts',(-2.74742463217173,-0.146875128348903,
8.77093053738833));
#397391=CARTESIAN_POINT('Ctrl Pts',(-2.73978631140984,-0.134711223304163,
8.75371302330492));
#397392=CARTESIAN_POINT('Ctrl Pts',(-2.7463553003912,-0.13854718278394,
8.75300828287559));
#397393=CARTESIAN_POINT('Ctrl Pts',(-2.74592098874476,-0.14617646274525,
8.75267964240738));
#397394=CARTESIAN_POINT('Origin',(-2.7215304230328,-0.138494647576021,8.78727029226991));
#397395=CARTESIAN_POINT('Ctrl Pts',(-2.66618796128141,-0.0915411309428134,
8.85049129520029));
#397396=CARTESIAN_POINT('Ctrl Pts',(-2.67122500331725,-0.0944956731666149,
8.85711686593484));
#397397=CARTESIAN_POINT('Ctrl Pts',(-2.66869591238441,-0.102662953079004,
8.85933012996512));
#397398=CARTESIAN_POINT('Ctrl Pts',(-2.68677347260704,-0.103615829144124,
8.82945683644723));
#397399=CARTESIAN_POINT('Ctrl Pts',(-2.69185232513724,-0.106594895854732,
8.83607469902389));
#397400=CARTESIAN_POINT('Ctrl Pts',(-2.6892799847167,-0.114775061333413,
8.8382956714852));
#397401=CARTESIAN_POINT('Ctrl Pts',(-2.70732829956804,-0.115672529034066,
8.80838214965002));
#397402=CARTESIAN_POINT('Ctrl Pts',(-2.71242719562158,-0.118663352532825,
8.81501364461988));
#397403=CARTESIAN_POINT('Ctrl Pts',(-2.70983317111897,-0.126868219958614,
8.81722098428721));
#397404=CARTESIAN_POINT('Ctrl Pts',(-2.72785477369492,-0.127712598202057,
8.78727029226991));
#397405=CARTESIAN_POINT('Ctrl Pts',(-2.73295451669185,-0.130703918486415,
8.79393457792714));
#397406=CARTESIAN_POINT('Ctrl Pts',(-2.7303578352728,-0.138943861495087,
8.79610912703474));
#397407=CARTESIAN_POINT('Origin',(-2.65986361061929,-0.102323180316778,
8.85049129520029));
#397408=CARTESIAN_POINT('Ctrl Pts',(-2.66657505256398,-0.0794701993177115,
8.85049129520029));
#397409=CARTESIAN_POINT('Ctrl Pts',(-2.67179104362696,-0.0768444519090711,
8.85711686593485));
#397410=CARTESIAN_POINT('Ctrl Pts',(-2.66979042840331,-0.0685319131367817,
8.85933012996512));
#397411=CARTESIAN_POINT('Ctrl Pts',(-2.66196054056419,-0.0817931601470715,
8.86332496987233));
#397412=CARTESIAN_POINT('Ctrl Pts',(-2.66239050079877,-0.0771923962351356,
8.86648636486738));
#397413=CARTESIAN_POINT('Ctrl Pts',(-2.65688884651665,-0.0750457937910786,
8.87206031107457));
#397414=CARTESIAN_POINT('Ctrl Pts',(-2.66170148162993,-0.0889095282140341,
8.86341338519875));
#397415=CARTESIAN_POINT('Ctrl Pts',(-2.66180657158416,-0.093542284060803,
8.86654584966058));
#397416=CARTESIAN_POINT('Ctrl Pts',(-2.65614098496653,-0.095281617572672,
8.87215952290715));
#397417=CARTESIAN_POINT('Ctrl Pts',(-2.66618796128141,-0.0915411309428132,
8.85049129520029));
#397418=CARTESIAN_POINT('Ctrl Pts',(-2.67122500331725,-0.0944956731666149,
8.85711686593484));
#397419=CARTESIAN_POINT('Ctrl Pts',(-2.66869591238441,-0.102662953079003,
8.85933012996512));
#397420=CARTESIAN_POINT('Origin',(-2.66095450423382,-0.0683051002824,8.85049129520029));
#397421=CARTESIAN_POINT('Ctrl Pts',(-2.73043267776197,-0.0473240564541735,
8.78727029226991));
#397422=CARTESIAN_POINT('Ctrl Pts',(-2.73571359733862,-0.0446656238138165,
8.79393457792714));
#397423=CARTESIAN_POINT('Ctrl Pts',(-2.73365018604124,-0.0362762407020484,
8.79610912703474));
#397424=CARTESIAN_POINT('Ctrl Pts',(-2.70917696759746,-0.0580242522960278,
8.80838214965002));
#397425=CARTESIAN_POINT('Ctrl Pts',(-2.71445701014171,-0.0553662611567412,
8.81501364461988));
#397426=CARTESIAN_POINT('Ctrl Pts',(-2.71239400300153,-0.0470120517905022,
8.81722098428721));
#397427=CARTESIAN_POINT('Ctrl Pts',(-2.68789189731876,-0.0687392281179148,
8.82945683644722));
#397428=CARTESIAN_POINT('Ctrl Pts',(-2.69315118426122,-0.066091685418231,
8.8360746990239));
#397429=CARTESIAN_POINT('Ctrl Pts',(-2.69110823399166,-0.0577635165502493,
8.8382956714852));
#397430=CARTESIAN_POINT('Ctrl Pts',(-2.66657505256398,-0.0794701993177114,
8.85049129520029));
#397431=CARTESIAN_POINT('Ctrl Pts',(-2.67179104362696,-0.076844451909071,
8.85711686593484));
#397432=CARTESIAN_POINT('Ctrl Pts',(-2.66979042840331,-0.0685319131367817,
8.85933012996512));
#397433=CARTESIAN_POINT('Origin',(-2.72481212943181,-0.0361589574188621,
8.78727029226991));
#397434=CARTESIAN_POINT('Ctrl Pts',(-2.74279236264415,-0.0411021289464491,
8.75374538247847));
#397435=CARTESIAN_POINT('Ctrl Pts',(-2.74958571518575,-0.0376970240092693,
8.75304829418601));
#397436=CARTESIAN_POINT('Ctrl Pts',(-2.74964669889166,-0.0300637465875672,
8.75272238421917));
#397437=CARTESIAN_POINT('Ctrl Pts',(-2.74397138271647,-0.0405086067622189,
8.76769408445022));
#397438=CARTESIAN_POINT('Ctrl Pts',(-2.75093537691269,-0.0370171973323106,
8.76974318093971));
#397439=CARTESIAN_POINT('Ctrl Pts',(-2.75117499675545,-0.0294699501778062,
8.7707786988043));
#397440=CARTESIAN_POINT('Ctrl Pts',(-2.73792839747587,-0.0435506633845036,
8.78108014887987));
#397441=CARTESIAN_POINT('Ctrl Pts',(-2.74383183450136,-0.04059521611103,
8.78639403366323));
#397442=CARTESIAN_POINT('Ctrl Pts',(-2.74335079698391,-0.0325149513483094,
8.78812224174741));
#397443=CARTESIAN_POINT('Ctrl Pts',(-2.72802527865339,-0.0485359226161412,
8.78944554828685));
#397444=CARTESIAN_POINT('Ctrl Pts',(-2.73300298241105,-0.0460501867255157,
8.79673892988686));
#397445=CARTESIAN_POINT('Ctrl Pts',(-2.73055804701899,-0.0374754654329442,
8.79894799272499));
#397446=CARTESIAN_POINT('Origin',(-2.73733720999684,-0.0298537898218447,
8.75721825406948));
#397447=CARTESIAN_POINT('Origin',(-2.73733720999684,-0.0298537898218447,
9.));
#397448=CARTESIAN_POINT('Origin',(-2.73733720999684,-0.0298537898218447,
7.51860402984325));
#397449=CARTESIAN_POINT('Ctrl Pts',(-2.74590223252928,-0.0489244707518609,
7.50366195182966));
#397450=CARTESIAN_POINT('Ctrl Pts',(-2.74956360331414,-0.0489897063693297,
7.50000065167735));
#397451=CARTESIAN_POINT('Ctrl Pts',(-2.74956360331415,-0.0489897063692129,
7.49482233047108));
#397452=CARTESIAN_POINT('Ctrl Pts',(-2.74753601636503,-0.0416660583920684,
7.50215800491337));
#397453=CARTESIAN_POINT('Ctrl Pts',(-2.74973341113685,-0.039457856999275,
7.49877273257264));
#397454=CARTESIAN_POINT('Ctrl Pts',(-2.74979493244485,-0.0360062817822748,
7.49481816995647));
#397455=CARTESIAN_POINT('Ctrl Pts',(-2.7454754935513,-0.0397518321577423,
7.51043025814042));
#397456=CARTESIAN_POINT('Ctrl Pts',(-2.74977310304523,-0.0357991989057771,
7.51006209594516));
#397457=CARTESIAN_POINT('Ctrl Pts',(-2.74983649427474,-0.0299875767815907,
7.50731281821701));
#397458=CARTESIAN_POINT('Ctrl Pts',(-2.74295640828481,-0.0410195683706217,
7.51860402984326));
#397459=CARTESIAN_POINT('Ctrl Pts',(-2.7497534837955,-0.0375989278030173,
7.51860402984327));
#397460=CARTESIAN_POINT('Ctrl Pts',(-2.74983646666349,-0.0299901084968249,
7.51860402984327));
#397461=CARTESIAN_POINT('Origin',(0.,0.,7.5));
#397462=CARTESIAN_POINT('Origin',(-2.65600461497701,-0.250154969482917,
7.5));
#397463=CARTESIAN_POINT('',(-2.65600461497701,-0.250154969482917,7.59394543036555));
#397464=CARTESIAN_POINT('',(-2.65600461497701,-0.250154969482917,8.85049129520029));
#397465=CARTESIAN_POINT('',(-2.65600461497701,-0.250154969482917,7.5));
#397466=CARTESIAN_POINT('',(-2.72179064828012,-0.222166246411436,8.78727029226991));
#397467=CARTESIAN_POINT('Ctrl Pts',(-2.65600461497701,-0.250154969482917,
8.85049129520029));
#397468=CARTESIAN_POINT('Ctrl Pts',(-2.67796516820153,-0.240811833685908,
8.82945686509571));
#397469=CARTESIAN_POINT('Ctrl Pts',(-2.69989307440825,-0.231482587590015,
8.80838212259896));
#397470=CARTESIAN_POINT('Ctrl Pts',(-2.72179064828012,-0.222166246411436,
8.78727029226991));
#397471=CARTESIAN_POINT('',(-2.73469396819878,-0.216676518124552,8.75721825406948));
#397472=CARTESIAN_POINT('Origin',(-2.69586348137444,-0.23319720063476,8.75937679713098));
#397473=CARTESIAN_POINT('',(-2.73469396819878,-0.216676518124552,7.51860402984325));
#397474=CARTESIAN_POINT('',(-2.73469396819878,-0.216676518124552,7.5));
#397475=CARTESIAN_POINT('Ctrl Pts',(-2.73469396819878,-0.216676518124552,
7.51860402984325));
#397476=CARTESIAN_POINT('Ctrl Pts',(-2.72456041724852,-0.220987845879652,
7.52834476460825));
#397477=CARTESIAN_POINT('Ctrl Pts',(-2.71442028774322,-0.225301972486524,
7.53807742314407));
#397478=CARTESIAN_POINT('Ctrl Pts',(-2.70427335879911,-0.229618991920331,
7.54780169004675));
#397479=CARTESIAN_POINT('Ctrl Pts',(-2.68820117174638,-0.236456917388489,
7.5632044032688));
#397480=CARTESIAN_POINT('Ctrl Pts',(-2.67211190534232,-0.243302109280976,
7.57858609112102));
#397481=CARTESIAN_POINT('Ctrl Pts',(-2.65600461497701,-0.250154969482917,
7.59394543036555));
#397482=CARTESIAN_POINT('Origin',(-2.88264819886835,-0.416223926434574,
7.5));
#397483=CARTESIAN_POINT('',(-2.72568349213022,-0.310079528408719,8.75721825406948));
#397484=CARTESIAN_POINT('',(-2.71406752923974,-0.302224454397989,8.78727029226991));
#397485=CARTESIAN_POINT('Origin',(-2.68458188288295,-0.282285346760464,
8.75658640620939));
#397486=CARTESIAN_POINT('',(-2.6548449317704,-0.262176299060764,8.85049129520029));
#397487=CARTESIAN_POINT('Ctrl Pts',(-2.71406752923974,-0.302224454397989,
8.78727029226991));
#397488=CARTESIAN_POINT('Ctrl Pts',(-2.69435466409413,-0.288894004211271,
8.80838212259897));
#397489=CARTESIAN_POINT('Ctrl Pts',(-2.67461449285379,-0.275545088797251,
8.82945686509571));
#397490=CARTESIAN_POINT('Ctrl Pts',(-2.6548449317704,-0.262176299060765,
8.85049129520029));
#397491=CARTESIAN_POINT('',(-2.6548449317704,-0.262176299060764,7.59394543036555));
#397492=CARTESIAN_POINT('',(-2.6548449317704,-0.262176299060764,7.5));
#397493=CARTESIAN_POINT('',(-2.72568349213022,-0.310079528408719,7.51860402984325));
#397494=CARTESIAN_POINT('Ctrl Pts',(-2.6548449317704,-0.262176299060764,
7.59394543036555));
#397495=CARTESIAN_POINT('Ctrl Pts',(-2.6693452067639,-0.271981834281885,
7.57858609112103));
#397496=CARTESIAN_POINT('Ctrl Pts',(-2.68382925603652,-0.281776397167808,
7.56320440326857));
#397497=CARTESIAN_POINT('Ctrl Pts',(-2.69829792995536,-0.291560562763133,
7.54780169004651));
#397498=CARTESIAN_POINT('Ctrl Pts',(-2.70743250546073,-0.297737645741781,
7.53807742314383));
#397499=CARTESIAN_POINT('Ctrl Pts',(-2.7165609599037,-0.303910589468382,
7.52834476460825));
#397500=CARTESIAN_POINT('Ctrl Pts',(-2.72568349213022,-0.310079528408719,
7.51860402984325));
#397501=CARTESIAN_POINT('',(-2.72568349213022,-0.310079528408719,7.5));
#397502=CARTESIAN_POINT('Origin',(-2.65869612245475,-0.256481217383316,
7.5));
#397503=CARTESIAN_POINT('Ctrl Pts',(-2.6548449317704,-0.262176299060764,
8.85049129520029));
#397504=CARTESIAN_POINT('Ctrl Pts',(-2.65468450732037,-0.262067815077129,
8.85097269580138));
#397505=CARTESIAN_POINT('Ctrl Pts',(-2.65453081876944,-0.261953732011562,
8.85143669361005));
#397506=CARTESIAN_POINT('Ctrl Pts',(-2.65437731036211,-0.261828094693177,
8.8519052845931));
#397507=CARTESIAN_POINT('Ctrl Pts',(-2.65407705765253,-0.261582356066044,
8.85282181883899));
#397508=CARTESIAN_POINT('Ctrl Pts',(-2.65378534264253,-0.261298583650791,
8.85372622499635));
#397509=CARTESIAN_POINT('Ctrl Pts',(-2.65350833902008,-0.260961272455523,
8.8546225773507));
#397510=CARTESIAN_POINT('Ctrl Pts',(-2.65327838045095,-0.260681248681371,
8.85536669723986));
#397511=CARTESIAN_POINT('Ctrl Pts',(-2.65305848371428,-0.260364283628671,
8.85610498449051));
#397512=CARTESIAN_POINT('Ctrl Pts',(-2.65285873749405,-0.259996917879263,
8.8568133821837));
#397513=CARTESIAN_POINT('Ctrl Pts',(-2.65267746748548,-0.259663532884715,
8.85745625420284));
#397514=CARTESIAN_POINT('Ctrl Pts',(-2.65250999297829,-0.25928474385388,
8.85808743050666));
#397515=CARTESIAN_POINT('Ctrl Pts',(-2.65237491462936,-0.258838828408621,
8.85866804508411));
#397516=CARTESIAN_POINT('Ctrl Pts',(-2.65231259240731,-0.258633092688443,
8.85893592806396));
#397517=CARTESIAN_POINT('Ctrl Pts',(-2.65225734483431,-0.258412903800721,
8.85919241173849));
#397518=CARTESIAN_POINT('Ctrl Pts',(-2.65221231342865,-0.258175223186676,
8.85943017985534));
#397519=CARTESIAN_POINT('Ctrl Pts',(-2.65215150770028,-0.25785428399672,
8.8597512372));
#397520=CARTESIAN_POINT('Ctrl Pts',(-2.65210841079495,-0.257493164175759,
8.86004599534705));
#397521=CARTESIAN_POINT('Ctrl Pts',(-2.65209388221268,-0.257094968238555,
8.86026130871721));
#397522=CARTESIAN_POINT('Ctrl Pts',(-2.65208856288911,-0.256949177479612,
8.86034014101235));
#397523=CARTESIAN_POINT('Ctrl Pts',(-2.65208698092624,-0.256796227185913,
8.86040910639693));
#397524=CARTESIAN_POINT('Ctrl Pts',(-2.65208951578449,-0.256640280923377,
8.86046313645507));
#397525=CARTESIAN_POINT('Ctrl Pts',(-2.65209347140956,-0.256396928086729,
8.8605474499083));
#397526=CARTESIAN_POINT('Ctrl Pts',(-2.65210770704384,-0.256139639254097,
8.86059655985668));
#397527=CARTESIAN_POINT('Ctrl Pts',(-2.65213101720273,-0.255884898957206,
8.86059725258816));
#397528=CARTESIAN_POINT('Ctrl Pts',(-2.6521543812174,-0.255629570108459,
8.86059794692011));
#397529=CARTESIAN_POINT('Ctrl Pts',(-2.65218976656294,-0.255374212058233,
8.86056369958366));
#397530=CARTESIAN_POINT('Ctrl Pts',(-2.6522315158243,-0.25513223563593,
8.86048590497774));
#397531=CARTESIAN_POINT('Ctrl Pts',(-2.65224241113849,-0.255069086994215,
8.86046560290182));
#397532=CARTESIAN_POINT('Ctrl Pts',(-2.65225397087204,-0.255006043587049,
8.86044257503091));
#397533=CARTESIAN_POINT('Ctrl Pts',(-2.65226580553173,-0.254945047587551,
8.86041778462583));
#397534=CARTESIAN_POINT('Ctrl Pts',(-2.65234543810585,-0.254534620200656,
8.860250975962));
#397535=CARTESIAN_POINT('Ctrl Pts',(-2.65244852973478,-0.254161880950966,
8.8599848982295));
#397536=CARTESIAN_POINT('Ctrl Pts',(-2.65256390552944,-0.253835450601984,
8.85968173251461));
#397537=CARTESIAN_POINT('Ctrl Pts',(-2.65262493271457,-0.253662787649602,
8.85952137522076));
#397538=CARTESIAN_POINT('Ctrl Pts',(-2.65269039306684,-0.253499689179471,
8.85934740853961));
#397539=CARTESIAN_POINT('Ctrl Pts',(-2.65275792075998,-0.253347876209768,
8.8591675900182));
#397540=CARTESIAN_POINT('Ctrl Pts',(-2.65302907954814,-0.252738268225599,
8.85844552518696));
#397541=CARTESIAN_POINT('Ctrl Pts',(-2.65334613350361,-0.252274948742778,
8.85759444184125));
#397542=CARTESIAN_POINT('Ctrl Pts',(-2.65363857348189,-0.25192040239233,
8.8568349891514));
#397543=CARTESIAN_POINT('Ctrl Pts',(-2.65366917654679,-0.251883300060988,
8.85675551444999));
#397544=CARTESIAN_POINT('Ctrl Pts',(-2.65369952268129,-0.251847404387438,
8.85667699793652));
#397545=CARTESIAN_POINT('Ctrl Pts',(-2.65372953884553,-0.251812682972989,
8.85659965593547));
#397546=CARTESIAN_POINT('Ctrl Pts',(-2.65413469856212,-0.251344011549046,
8.85555568965886));
#397547=CARTESIAN_POINT('Ctrl Pts',(-2.65459176757881,-0.250952102354057,
8.85434650606346));
#397548=CARTESIAN_POINT('Ctrl Pts',(-2.65509896008146,-0.250630300122051,
8.85297329937118));
#397549=CARTESIAN_POINT('Ctrl Pts',(-2.65538422496052,-0.250449305974245,
8.85220095427748));
#397550=CARTESIAN_POINT('Ctrl Pts',(-2.65568563114289,-0.25029068142281,
8.85137579139184));
#397551=CARTESIAN_POINT('Ctrl Pts',(-2.65600461497701,-0.250154969482917,
8.85049129520029));
#397552=CARTESIAN_POINT('Origin',(-2.65869612245475,-0.256481217383316,
7.59394543036555));
#397553=CARTESIAN_POINT('Ctrl Pts',(-2.65437916547328,-0.261861333459542,
7.59443877723642));
#397554=CARTESIAN_POINT('Ctrl Pts',(-2.64958222076125,-0.258617490818717,
7.58783886950015));
#397555=CARTESIAN_POINT('Ctrl Pts',(-2.65258170159906,-0.25067505440158,
7.58559994247159));
#397556=CARTESIAN_POINT('Ctrl Pts',(-2.68056554591988,-0.279569375265508,
7.56670252222136));
#397557=CARTESIAN_POINT('Ctrl Pts',(-2.67577553415485,-0.276330220898249,
7.56004874999029));
#397558=CARTESIAN_POINT('Ctrl Pts',(-2.6787728002332,-0.268333174361455,
7.55786368756705));
#397559=CARTESIAN_POINT('Ctrl Pts',(-2.70670302591733,-0.297244349072653,
7.53888913333561));
#397560=CARTESIAN_POINT('Ctrl Pts',(-2.70188454687783,-0.293985944252403,
7.5322200213728));
#397561=CARTESIAN_POINT('Ctrl Pts',(-2.70491526550984,-0.285959912275527,
7.53005029815327));
#397562=CARTESIAN_POINT('Ctrl Pts',(-2.73279042272696,-0.314885455076433,
7.51101258149734));
#397563=CARTESIAN_POINT('Ctrl Pts',(-2.72791353496612,-0.311587552469079,
7.5043616886572));
#397564=CARTESIAN_POINT('Ctrl Pts',(-2.73100785199465,-0.303554328728165,
7.50217374673251));
#397565=CARTESIAN_POINT('',(-2.72961551748768,-0.30261546891712,7.50366116523517));
#397566=CARTESIAN_POINT('Ctrl Pts',(-2.72568349213022,-0.310079528408719,
7.51860402984325));
#397567=CARTESIAN_POINT('Ctrl Pts',(-2.72604931204917,-0.310326907172325,
7.51734760759494));
#397568=CARTESIAN_POINT('Ctrl Pts',(-2.7264132111716,-0.310501163560067,
7.51608817408572));
#397569=CARTESIAN_POINT('Ctrl Pts',(-2.72678011988137,-0.310589852801529,
7.51481005913119));
#397570=CARTESIAN_POINT('Ctrl Pts',(-2.72711247455825,-0.310670189635742,
7.51365231206383));
#397571=CARTESIAN_POINT('Ctrl Pts',(-2.72744770835602,-0.310680673584717,
7.51247773061042));
#397572=CARTESIAN_POINT('Ctrl Pts',(-2.72778117474015,-0.31058421624477,
7.51129758471022));
#397573=CARTESIAN_POINT('Ctrl Pts',(-2.72819563537232,-0.310464330787061,
7.50983079813402));
#397574=CARTESIAN_POINT('Ctrl Pts',(-2.72859051930512,-0.310170560553407,
7.50839324291155));
#397575=CARTESIAN_POINT('Ctrl Pts',(-2.72891950166131,-0.309634617944499,
7.50715379678855));
#397576=CARTESIAN_POINT('Ctrl Pts',(-2.72907148203047,-0.309387027901999,
7.50658120839351));
#397577=CARTESIAN_POINT('Ctrl Pts',(-2.7292229054396,-0.309047586153617,
7.50598221009429));
#397578=CARTESIAN_POINT('Ctrl Pts',(-2.72934939496709,-0.308615104077948,
7.50545747549611));
#397579=CARTESIAN_POINT('Ctrl Pts',(-2.72941689369418,-0.308384318255798,
7.50517746087247));
#397580=CARTESIAN_POINT('Ctrl Pts',(-2.72947821848437,-0.308124592386449,
7.50491486231392));
#397581=CARTESIAN_POINT('Ctrl Pts',(-2.72953012197526,-0.307842421146894,
7.50468370960993));
#397582=CARTESIAN_POINT('Ctrl Pts',(-2.72960773406618,-0.307420486137888,
7.50433806340447));
#397583=CARTESIAN_POINT('Ctrl Pts',(-2.72966606023027,-0.306935611055743,
7.50405484070984));
#397584=CARTESIAN_POINT('Ctrl Pts',(-2.7297004610413,-0.306420365776516,
7.50385766036131));
#397585=CARTESIAN_POINT('Ctrl Pts',(-2.72970413967333,-0.306365268302629,
7.50383657498791));
#397586=CARTESIAN_POINT('Ctrl Pts',(-2.72970755748387,-0.306309848873736,
7.50381643264937));
#397587=CARTESIAN_POINT('Ctrl Pts',(-2.7297107183599,-0.306254165571768,
7.50379723213559));
#397588=CARTESIAN_POINT('Ctrl Pts',(-2.72973181824138,-0.305882461315843,
7.50366906242519));
#397589=CARTESIAN_POINT('Ctrl Pts',(-2.7297412101996,-0.305490872696429,
7.50358235568538));
#397590=CARTESIAN_POINT('Ctrl Pts',(-2.72974118993311,-0.30511321185331,
7.5035341175365));
#397591=CARTESIAN_POINT('Ctrl Pts',(-2.72974115954581,-0.304546952162009,
7.50346178989176));
#397592=CARTESIAN_POINT('Ctrl Pts',(-2.72971705014849,-0.303937786884236,
7.50346967198527));
#397593=CARTESIAN_POINT('Ctrl Pts',(-2.72967498135674,-0.303340503578748,
7.50354272648692));
#397594=CARTESIAN_POINT('Ctrl Pts',(-2.72965767759192,-0.303094828592168,
7.50357277531559));
#397595=CARTESIAN_POINT('Ctrl Pts',(-2.72963749980964,-0.302851480312632,
7.50361331098761));
#397596=CARTESIAN_POINT('Ctrl Pts',(-2.72961551748909,-0.302615468917276,
7.50366116523658));
#397597=CARTESIAN_POINT('',(-2.66161051802581,-0.256762365618787,7.57603338622103));
#397598=CARTESIAN_POINT('Origin',(-2.67040689596866,-0.257608075198384,
7.58486873427625));
#397599=CARTESIAN_POINT('Ctrl Pts',(-2.72961551753202,-0.302615468953483,
7.50366116529968));
#397600=CARTESIAN_POINT('Ctrl Pts',(-2.70698464170165,-0.287355349099734,
7.52783573079709));
#397601=CARTESIAN_POINT('Ctrl Pts',(-2.68431738885518,-0.272071688128237,
7.55196141284069));
#397602=CARTESIAN_POINT('Ctrl Pts',(-2.66161051882396,-0.256762366583466,
7.57603338728831));
#397603=CARTESIAN_POINT('Ctrl Pts',(-2.65579532783697,-0.262606743989967,
7.5963967733137));
#397604=CARTESIAN_POINT('Ctrl Pts',(-2.63922637620262,-0.254890413417566,
7.59959882295472));
#397605=CARTESIAN_POINT('Ctrl Pts',(-2.65684465102774,-0.249960382504432,
7.59642833564545));
#397606=CARTESIAN_POINT('Ctrl Pts',(-2.65204060628407,-0.261549781292344,
7.58707626057419));
#397607=CARTESIAN_POINT('Ctrl Pts',(-2.64876165092592,-0.255620131825776,
7.58809943920599));
#397608=CARTESIAN_POINT('Ctrl Pts',(-2.65302079876161,-0.250369030940479,
7.58710240504253));
#397609=CARTESIAN_POINT('Ctrl Pts',(-2.65730239716171,-0.258510177860639,
7.58015376756929));
#397610=CARTESIAN_POINT('Ctrl Pts',(-2.655609858913,-0.25621570936601,7.58205880659762));
#397611=CARTESIAN_POINT('Ctrl Pts',(-2.65765471203255,-0.254280340988251,
7.58020924244125));
#397612=CARTESIAN_POINT('Ctrl Pts',(-2.66161051720204,-0.256762365539522,
7.57603338509286));
#397613=CARTESIAN_POINT('Ctrl Pts',(-2.66161051720204,-0.256762365539522,
7.57603338509286));
#397614=CARTESIAN_POINT('Ctrl Pts',(-2.66161051720204,-0.256762365539522,
7.57603338509286));
#397615=CARTESIAN_POINT('Origin',(-2.67040634802769,-0.257613755182354,
7.58486873427622));
#397616=CARTESIAN_POINT('Ctrl Pts',(-2.74261348672104,-0.213307152323794,
7.51098857897448));
#397617=CARTESIAN_POINT('Ctrl Pts',(-2.73719608563612,-0.215611990161248,
7.50433767179957));
#397618=CARTESIAN_POINT('Ctrl Pts',(-2.73869774222272,-0.224088609686646,
7.50214974420965));
#397619=CARTESIAN_POINT('Ctrl Pts',(-2.71362657888527,-0.225639656586148,
7.53887321589168));
#397620=CARTESIAN_POINT('Ctrl Pts',(-2.7082740878795,-0.227916878375978,
7.53220407452062));
#397621=CARTESIAN_POINT('Ctrl Pts',(-2.70971466634537,-0.236374280672515,
7.53003438070911));
#397622=CARTESIAN_POINT('Ctrl Pts',(-2.68458400549364,-0.237995843805953,
7.56669465659234));
#397623=CARTESIAN_POINT('Ctrl Pts',(-2.67926314671457,-0.24025960763831,
7.56004085833301));
#397624=CARTESIAN_POINT('Ctrl Pts',(-2.68067642139727,-0.248682155043822,
7.5578558219379));
#397625=CARTESIAN_POINT('Ctrl Pts',(-2.65548708002545,-0.250375155162335,
7.59443891967696));
#397626=CARTESIAN_POINT('Ctrl Pts',(-2.65015850666364,-0.252642201170453,
7.58783901202978));
#397627=CARTESIAN_POINT('Ctrl Pts',(-2.65158440916059,-0.261011548818718,
7.58560008491213));
#397628=CARTESIAN_POINT('',(-2.73712666431696,-0.224754574642208,7.50366116523517));
#397629=CARTESIAN_POINT('Ctrl Pts',(-2.73712666431733,-0.224754574642239,
7.50366116523554));
#397630=CARTESIAN_POINT('Ctrl Pts',(-2.73733969481485,-0.22402741886533,
7.50350835821027));
#397631=CARTESIAN_POINT('Ctrl Pts',(-2.73751186429179,-0.223352055494728,
7.50345484956));
#397632=CARTESIAN_POINT('Ctrl Pts',(-2.73764887337768,-0.222708553769195,
7.50349758195598));
#397633=CARTESIAN_POINT('Ctrl Pts',(-2.7377191691996,-0.222378389660665,
7.50351950684424));
#397634=CARTESIAN_POINT('Ctrl Pts',(-2.73778726446689,-0.222024097627282,
7.50357029184312));
#397635=CARTESIAN_POINT('Ctrl Pts',(-2.73784353695387,-0.221680652932907,
7.50365515313924));
#397636=CARTESIAN_POINT('Ctrl Pts',(-2.73793010682584,-0.221152295918462,
7.50378570417639));
#397637=CARTESIAN_POINT('Ctrl Pts',(-2.73799157957439,-0.220634157925302,
7.50400001621911));
#397638=CARTESIAN_POINT('Ctrl Pts',(-2.73802102162781,-0.220165409289237,
7.50428903009635));
#397639=CARTESIAN_POINT('Ctrl Pts',(-2.73802428946922,-0.220113381796974,
7.50432110841319));
#397640=CARTESIAN_POINT('Ctrl Pts',(-2.73802718145414,-0.220061938916591,
7.50435406373355));
#397641=CARTESIAN_POINT('Ctrl Pts',(-2.7380297016942,-0.220011116430411,
7.50438785222352));
#397642=CARTESIAN_POINT('Ctrl Pts',(-2.73804508897109,-0.219700820723866,
7.50459414719561));
#397643=CARTESIAN_POINT('Ctrl Pts',(-2.73804634861812,-0.219408685618597,
7.50483629897752));
#397644=CARTESIAN_POINT('Ctrl Pts',(-2.73803474839784,-0.219145908398944,
7.5050991045531));
#397645=CARTESIAN_POINT('Ctrl Pts',(-2.73800915714678,-0.218566195458917,
7.50567888004914));
#397646=CARTESIAN_POINT('Ctrl Pts',(-2.73792048980846,-0.218106496852237,
7.50637912803144));
#397647=CARTESIAN_POINT('Ctrl Pts',(-2.73779651599276,-0.217753238076209,
7.50710440483569));
#397648=CARTESIAN_POINT('Ctrl Pts',(-2.73776611515193,-0.217666612011158,
7.50728225710685));
#397649=CARTESIAN_POINT('Ctrl Pts',(-2.73773312376091,-0.217584613677195,
7.50746498566954));
#397650=CARTESIAN_POINT('Ctrl Pts',(-2.73769869842967,-0.217509001681931,
7.50764697238949));
#397651=CARTESIAN_POINT('Ctrl Pts',(-2.73751363732303,-0.217102532404377,
7.50862528291181));
#397652=CARTESIAN_POINT('Ctrl Pts',(-2.7372741051665,-0.216842004831557,
7.50965856837421));
#397653=CARTESIAN_POINT('Ctrl Pts',(-2.73701505418627,-0.216671083027106,
7.51067959873201));
#397654=CARTESIAN_POINT('Ctrl Pts',(-2.7368724981051,-0.216577024542526,
7.51124147302578));
#397655=CARTESIAN_POINT('Ctrl Pts',(-2.73672375708001,-0.216510441144906,
7.51180065547252));
#397656=CARTESIAN_POINT('Ctrl Pts',(-2.73657324382109,-0.216464264630444,
7.51235175716501));
#397657=CARTESIAN_POINT('Ctrl Pts',(-2.73605316055418,-0.216304706378441,
7.51425603304536));
#397658=CARTESIAN_POINT('Ctrl Pts',(-2.73544812829919,-0.216375575257973,
7.51626900505181));
#397659=CARTESIAN_POINT('Ctrl Pts',(-2.73479964907405,-0.21663305061292,
7.51827788969244));
#397660=CARTESIAN_POINT('Ctrl Pts',(-2.73476455215294,-0.216646985665691,
7.51838661432546));
#397661=CARTESIAN_POINT('Ctrl Pts',(-2.73472932345267,-0.216661476202113,
7.51849533314857));
#397662=CARTESIAN_POINT('Ctrl Pts',(-2.73469396819878,-0.216676518124548,
7.51860402984325));
#397663=CARTESIAN_POINT('Ctrl Pts',(-2.66161051899485,-0.256762364824346,
7.57603338728985));
#397664=CARTESIAN_POINT('Ctrl Pts',(-2.68682516411913,-0.246075974209679,
7.55196141284922));
#397665=CARTESIAN_POINT('Ctrl Pts',(-2.7119960174081,-0.235407197792685,
7.52783573083105));
#397666=CARTESIAN_POINT('Ctrl Pts',(-2.73712666436909,-0.224754574614206,
7.50366116530176));
#397667=CARTESIAN_POINT('Origin',(-9.19709468541366E-16,-8.87232663177237E-17,
7.49482233047033));
#397668=CARTESIAN_POINT('Origin',(-2.72083050515592,-0.301641529324094,
7.49482233047033));
#397669=CARTESIAN_POINT('Origin',(0.,0.,7.50366116523517));
#397670=CARTESIAN_POINT('Origin',(-2.7283174780614,-0.224031223057635,7.49482233047033));
#397671=CARTESIAN_POINT('Ctrl Pts',(-2.72568261591557,-0.31007893593925,
7.51860402984325));
#397672=CARTESIAN_POINT('Ctrl Pts',(-2.73198605348183,-0.314340738477903,
7.51860402984325));
#397673=CARTESIAN_POINT('Ctrl Pts',(-2.73109539723703,-0.321897392332867,
7.51860402984325));
#397674=CARTESIAN_POINT('Ctrl Pts',(-2.72802312458908,-0.311661373358606,
7.51041458714366));
#397675=CARTESIAN_POINT('Ctrl Pts',(-2.7317750369846,-0.31613099516997,
7.51004642900443));
#397676=CARTESIAN_POINT('Ctrl Pts',(-2.73109515160462,-0.321899476368271,
7.5072913648301));
#397677=CARTESIAN_POINT('Ctrl Pts',(-2.73030742601402,-0.310016470869305,
7.50215815450137));
#397678=CARTESIAN_POINT('Ctrl Pts',(-2.7322048270618,-0.312485870339889,
7.49877163671529));
#397679=CARTESIAN_POINT('Ctrl Pts',(-2.73182466947127,-0.315915069051078,
7.4948158853317));
#397680=CARTESIAN_POINT('Ctrl Pts',(-2.72961497032199,-0.30261540825579,
7.50366171572174));
#397681=CARTESIAN_POINT('Ctrl Pts',(-2.73325438874115,-0.303018887905099,
7.50000045605858));
#397682=CARTESIAN_POINT('Ctrl Pts',(-2.73325438874114,-0.303018887905223,
7.49482233047317));
#397683=CARTESIAN_POINT('Origin',(-2.71868132724959,-0.320434222367717,
7.51860402984325));
#397684=CARTESIAN_POINT('Origin',(-2.71868132724959,-0.320434222367717,
9.));
#397685=CARTESIAN_POINT('Origin',(-2.71868132724959,-0.320434222367717,
8.75721825406948));
#397686=CARTESIAN_POINT('Ctrl Pts',(-2.71184947061986,-0.300724570905234,
8.78942910404912));
#397687=CARTESIAN_POINT('Ctrl Pts',(-2.71647685875768,-0.30382935877619,
8.79672699501689));
#397688=CARTESIAN_POINT('Ctrl Pts',(-2.71294933545981,-0.31202875298339,
8.79893251111266));
#397689=CARTESIAN_POINT('Ctrl Pts',(-2.72095691172078,-0.306883299291342,
8.78111911759583));
#397690=CARTESIAN_POINT('Ctrl Pts',(-2.72643858652894,-0.310570242662659,
8.78644465894818));
#397691=CARTESIAN_POINT('Ctrl Pts',(-2.72490651814849,-0.318530662139858,
8.78817647674132));
#397692=CARTESIAN_POINT('Ctrl Pts',(-2.72663288623001,-0.31072156574746,
8.76780923932029));
#397693=CARTESIAN_POINT('Ctrl Pts',(-2.73310092791911,-0.315078075070106,
8.7698851615837));
#397694=CARTESIAN_POINT('Ctrl Pts',(-2.73236943182156,-0.322601458209069,
8.77093053738833));
#397695=CARTESIAN_POINT('Ctrl Pts',(-2.72552614888092,-0.309973156320326,
8.75371302330492));
#397696=CARTESIAN_POINT('Ctrl Pts',(-2.73183587040219,-0.314222110979036,
8.7530082828756));
#397697=CARTESIAN_POINT('Ctrl Pts',(-2.73091364145019,-0.321807889323696,
8.75267964240738));
#397698=CARTESIAN_POINT('Origin',(-2.70706536435911,-0.312579148356987,
8.78727029226991));
#397699=CARTESIAN_POINT('Ctrl Pts',(-2.6548449317704,-0.262176299060765,
8.85049129520029));
#397700=CARTESIAN_POINT('Ctrl Pts',(-2.65968232649294,-0.265447495251982,
8.85711686593484));
#397701=CARTESIAN_POINT('Ctrl Pts',(-2.65663515242803,-0.273435955199434,
8.85933012996512));
#397702=CARTESIAN_POINT('Ctrl Pts',(-2.67461451938527,-0.275545106738663,
8.82945683644722));
#397703=CARTESIAN_POINT('Ctrl Pts',(-2.67949206740875,-0.278843455836075,
8.8360746990239));
#397704=CARTESIAN_POINT('Ctrl Pts',(-2.6764009071358,-0.286842003870841,
8.8382956714852));
#397705=CARTESIAN_POINT('Ctrl Pts',(-2.69435463883559,-0.288893987130663,
8.80838214965004));
#397706=CARTESIAN_POINT('Ctrl Pts',(-2.69925143594086,-0.292205353053579,
8.81501364461989));
#397707=CARTESIAN_POINT('Ctrl Pts',(-2.6961370534789,-0.300227162978778,
8.81722098428721));
#397708=CARTESIAN_POINT('Ctrl Pts',(-2.71406752923974,-0.302224454397989,
8.78727029226991));
#397709=CARTESIAN_POINT('Ctrl Pts',(-2.71896513971909,-0.305536370349664,
8.79393457792714));
#397710=CARTESIAN_POINT('Ctrl Pts',(-2.71584585849932,-0.313593013561955,
8.79610912703474));
#397711=CARTESIAN_POINT('Origin',(-2.64784276688977,-0.272530993019762,
8.85049129520029));
#397712=CARTESIAN_POINT('Ctrl Pts',(-2.65600461497701,-0.250154969482917,
8.85049129520029));
#397713=CARTESIAN_POINT('Ctrl Pts',(-2.66137812144103,-0.247868806648761,
8.85711686593484));
#397714=CARTESIAN_POINT('Ctrl Pts',(-2.65991420288366,-0.23944516702142,
8.85933012996512));
#397715=CARTESIAN_POINT('Ctrl Pts',(-2.65125075137568,-0.252177504741186,
8.86332496987232));
#397716=CARTESIAN_POINT('Ctrl Pts',(-2.65197460016677,-0.247613741238949,
8.86648636486738));
#397717=CARTESIAN_POINT('Ctrl Pts',(-2.64662178291423,-0.245119057019721,
8.87206031107457));
#397718=CARTESIAN_POINT('Ctrl Pts',(-2.65053627743828,-0.259262653503821,
8.86341338519876));
#397719=CARTESIAN_POINT('Ctrl Pts',(-2.65034432978771,-0.263892623993324,
8.86654584966058));
#397720=CARTESIAN_POINT('Ctrl Pts',(-2.6445789442447,-0.265265388477037,
8.87215952290714));
#397721=CARTESIAN_POINT('Ctrl Pts',(-2.6548449317704,-0.262176299060764,
8.85049129520029));
#397722=CARTESIAN_POINT('Ctrl Pts',(-2.65968232649294,-0.265447495251982,
8.85711686593484));
#397723=CARTESIAN_POINT('Ctrl Pts',(-2.65663515242803,-0.273435955199434,
8.85933012996512));
#397724=CARTESIAN_POINT('Origin',(-2.6511109650175,-0.238652700573101,8.85049129520029));
#397725=CARTESIAN_POINT('Ctrl Pts',(-2.72179064828012,-0.222166246411436,
8.78727029226991));
#397726=CARTESIAN_POINT('Ctrl Pts',(-2.7272310440052,-0.219851625485032,
8.79393457792714));
#397727=CARTESIAN_POINT('Ctrl Pts',(-2.7257093818291,-0.211347276044891,
8.79610912703474));
#397728=CARTESIAN_POINT('Ctrl Pts',(-2.69989304635039,-0.231482599527254,
8.80838214965003));
#397729=CARTESIAN_POINT('Ctrl Pts',(-2.70533253855794,-0.229168363003135,
8.81501364461988));
#397730=CARTESIAN_POINT('Ctrl Pts',(-2.70380902611904,-0.220699140934737,
8.81722098428722));
#397731=CARTESIAN_POINT('Ctrl Pts',(-2.67796519767341,-0.240811821147071,
8.82945683644723));
#397732=CARTESIAN_POINT('Ctrl Pts',(-2.68338330748996,-0.238506681779171,
8.83607469902389));
#397733=CARTESIAN_POINT('Ctrl Pts',(-2.68187814229224,-0.230064731754116,
8.83829567148519));
#397734=CARTESIAN_POINT('Ctrl Pts',(-2.65600461497701,-0.250154969482917,
8.85049129520029));
#397735=CARTESIAN_POINT('Ctrl Pts',(-2.66137812144103,-0.247868806648761,
8.85711686593484));
#397736=CARTESIAN_POINT('Ctrl Pts',(-2.65991420288366,-0.23944516702142,
8.85933012996512));
#397737=CARTESIAN_POINT('Origin',(-2.71689699832061,-0.21066397750162,8.78727029226991));
#397738=CARTESIAN_POINT('Ctrl Pts',(-2.73452357912827,-0.216748990250367,
8.75374538247848));
#397739=CARTESIAN_POINT('Ctrl Pts',(-2.74152113982087,-0.213786133058224,
8.75304829418603));
#397740=CARTESIAN_POINT('Ctrl Pts',(-2.74207106399279,-0.206172446263106,
8.75272238421917));
#397741=CARTESIAN_POINT('Ctrl Pts',(-2.7357382038743,-0.216232227596518,
8.76769408445017));
#397742=CARTESIAN_POINT('Ctrl Pts',(-2.74291158516777,-0.213194176281819,
8.76974318093965));
#397743=CARTESIAN_POINT('Ctrl Pts',(-2.74363426647131,-0.205677788252088,
8.77077869880429));
#397744=CARTESIAN_POINT('Ctrl Pts',(-2.72951272935803,-0.218880858593496,
8.78108014887993));
#397745=CARTESIAN_POINT('Ctrl Pts',(-2.73559339329596,-0.216309718112288,
8.78639403366329));
#397746=CARTESIAN_POINT('Ctrl Pts',(-2.73563104846251,-0.208215234940551,
8.78812224174742));
#397747=CARTESIAN_POINT('Ctrl Pts',(-2.71931055089962,-0.223221380073934,
8.78944554828685));
#397748=CARTESIAN_POINT('Ctrl Pts',(-2.72443728907637,-0.221059673969037,
8.79673892988685));
#397749=CARTESIAN_POINT('Ctrl Pts',(-2.72254676134579,-0.212345922812599,
8.79894799272499));
#397750=CARTESIAN_POINT('Origin',(-2.72980031823926,-0.205174249214736,
8.75721825406948));
#397751=CARTESIAN_POINT('Origin',(-2.72980031823926,-0.205174249214736,
9.));
#397752=CARTESIAN_POINT('Origin',(-2.72980031823926,-0.205174249214736,
7.51860402984325));
#397753=CARTESIAN_POINT('Ctrl Pts',(-2.73712588029195,-0.22475451026325,
7.50366195182966));
#397754=CARTESIAN_POINT('Ctrl Pts',(-2.74077554873749,-0.225054196678764,
7.50000065167735));
#397755=CARTESIAN_POINT('Ctrl Pts',(-2.7407755487375,-0.225054196678647,
7.49482233047108));
#397756=CARTESIAN_POINT('Ctrl Pts',(-2.73922135542018,-0.217615687979874,
7.50215800491337));
#397757=CARTESIAN_POINT('Ctrl Pts',(-2.74155571535778,-0.215552811140091,
7.49877273257265));
#397758=CARTESIAN_POINT('Ctrl Pts',(-2.74183825344709,-0.212112269238285,
7.49481816995647));
#397759=CARTESIAN_POINT('Ctrl Pts',(-2.7372877110675,-0.21557337657869,
7.51043025814043));
#397760=CARTESIAN_POINT('Ctrl Pts',(-2.74182973674376,-0.211904213221319,
7.51006209594515));
#397761=CARTESIAN_POINT('Ctrl Pts',(-2.74226534963713,-0.20610859318811,
7.50731281821701));
#397762=CARTESIAN_POINT('Ctrl Pts',(-2.73469257739382,-0.216677109744384,
7.51860402984326));
#397763=CARTESIAN_POINT('Ctrl Pts',(-2.74169484877752,-0.213698987372884,
7.51860402984326));
#397764=CARTESIAN_POINT('Ctrl Pts',(-2.74226515987506,-0.206111117932606,
7.51860402984327));
#397765=CARTESIAN_POINT('Origin',(0.,0.,7.5));
#397766=CARTESIAN_POINT('Origin',(-2.6345200847159,-0.419811799220444,7.5));
#397767=CARTESIAN_POINT('',(-2.6345200847159,-0.419811799220444,7.59394543036555));
#397768=CARTESIAN_POINT('',(-2.6345200847159,-0.419811799220444,8.85049129520029));
#397769=CARTESIAN_POINT('',(-2.6345200847159,-0.419811799220444,7.5));
#397770=CARTESIAN_POINT('',(-2.70196419720223,-0.396095507607684,8.78727029226991));
#397771=CARTESIAN_POINT('Ctrl Pts',(-2.6345200847159,-0.419811799220444,
8.85049129520029));
#397772=CARTESIAN_POINT('Ctrl Pts',(-2.65703413439438,-0.411894877373972,
8.82945686509571));
#397773=CARTESIAN_POINT('Ctrl Pts',(-2.67951471421565,-0.403989724989127,
8.80838212259895));
#397774=CARTESIAN_POINT('Ctrl Pts',(-2.70196419720223,-0.396095507607684,
8.78727029226991));
#397775=CARTESIAN_POINT('',(-2.71519273396521,-0.391443777102006,8.75721825406948));
#397776=CARTESIAN_POINT('Origin',(-2.6753835447784,-0.405442638265208,8.75937679713125));
#397777=CARTESIAN_POINT('',(-2.71519273396521,-0.391443777102006,7.51860402984325));
#397778=CARTESIAN_POINT('',(-2.71519273396521,-0.391443777102006,7.5));
#397779=CARTESIAN_POINT('Ctrl Pts',(-2.71519273396521,-0.391443777102006,
7.51860402984325));
#397780=CARTESIAN_POINT('Ctrl Pts',(-2.70480377576452,-0.395096987933276,
7.52834476460825));
#397781=CARTESIAN_POINT('Ctrl Pts',(-2.69440807320208,-0.398752570376309,
7.53807742314407));
#397782=CARTESIAN_POINT('Ctrl Pts',(-2.68400539982697,-0.402410604061113,
7.54780169004674));
#397783=CARTESIAN_POINT('Ctrl Pts',(-2.66752812741731,-0.408204731717991,
7.5632044032688));
#397784=CARTESIAN_POINT('Ctrl Pts',(-2.65103334518629,-0.414005016591753,
7.57858609112103));
#397785=CARTESIAN_POINT('Ctrl Pts',(-2.6345200847159,-0.419811799220444,
7.59394543036555));
#397786=CARTESIAN_POINT('Origin',(-2.85005793045283,-0.60006065396634,7.5));
#397787=CARTESIAN_POINT('',(-2.70021641947034,-0.48407757770026,8.75721825406948));
#397788=CARTESIAN_POINT('',(-2.68912759914126,-0.475494405483858,8.78727029226991));
#397789=CARTESIAN_POINT('Origin',(-2.66098003722165,-0.453707113034527,
8.75658640621012));
#397790=CARTESIAN_POINT('',(-2.6325925749723,-0.431734128529235,8.85049129520029));
#397791=CARTESIAN_POINT('Ctrl Pts',(-2.68912759914126,-0.475494405483858,
8.78727029226991));
#397792=CARTESIAN_POINT('Ctrl Pts',(-2.67030932106718,-0.460928336530396,
8.80838212259895));
#397793=CARTESIAN_POINT('Ctrl Pts',(-2.65146497607287,-0.446342090780945,
8.82945686509571));
#397794=CARTESIAN_POINT('Ctrl Pts',(-2.6325925749723,-0.431734128529236,
8.85049129520029));
#397795=CARTESIAN_POINT('',(-2.6325925749723,-0.431734128529235,7.59394543036555));
#397796=CARTESIAN_POINT('',(-2.6325925749723,-0.431734128529235,7.5));
#397797=CARTESIAN_POINT('',(-2.70021641947034,-0.48407757770026,7.51860402984325));
#397798=CARTESIAN_POINT('Ctrl Pts',(-2.6325925749723,-0.431734128529234,
7.59394543036555));
#397799=CARTESIAN_POINT('Ctrl Pts',(-2.64643481479702,-0.442448553035217,
7.57858609112103));
#397800=CARTESIAN_POINT('Ctrl Pts',(-2.6602615652383,-0.453150988164337,
7.56320440326857));
#397801=CARTESIAN_POINT('Ctrl Pts',(-2.67407363807278,-0.463842062262906,
7.54780169004651));
#397802=CARTESIAN_POINT('Ctrl Pts',(-2.68279367854782,-0.470591708024144,
7.53807742314383));
#397803=CARTESIAN_POINT('Ctrl Pts',(-2.69150787573962,-0.477336830860056,
7.52834476460825));
#397804=CARTESIAN_POINT('Ctrl Pts',(-2.70021641947034,-0.484077577700258,
7.51860402984324));
#397805=CARTESIAN_POINT('',(-2.70021641947034,-0.48407757770026,7.5));
#397806=CARTESIAN_POINT('Origin',(-2.63680073810823,-0.426297494642222,
7.5));
#397807=CARTESIAN_POINT('Ctrl Pts',(-2.6325925749723,-0.431734128529235,
8.85049129520029));
#397808=CARTESIAN_POINT('Ctrl Pts',(-2.6324394307242,-0.431615589007775,
8.85097269580138));
#397809=CARTESIAN_POINT('Ctrl Pts',(-2.63229336726999,-0.431491893478835,
8.85143669361005));
#397810=CARTESIAN_POINT('Ctrl Pts',(-2.63214822387277,-0.431356678978368,
8.8519052845931));
#397811=CARTESIAN_POINT('Ctrl Pts',(-2.63186433259248,-0.431092207990448,
8.85282181883899));
#397812=CARTESIAN_POINT('Ctrl Pts',(-2.63159139830333,-0.430790328371194,
8.85372622499635));
#397813=CARTESIAN_POINT('Ctrl Pts',(-2.63133657541701,-0.430435962534927,
8.8546225773507));
#397814=CARTESIAN_POINT('Ctrl Pts',(-2.63112503050724,-0.430141780603542,
8.85536669723986));
#397815=CARTESIAN_POINT('Ctrl Pts',(-2.63092589359265,-0.429811377957245,
8.85610498449051));
#397816=CARTESIAN_POINT('Ctrl Pts',(-2.63075009497682,-0.429431969215898,
8.85681338218371));
#397817=CARTESIAN_POINT('Ctrl Pts',(-2.63059055745687,-0.429087655187255,
8.85745625420284));
#397818=CARTESIAN_POINT('Ctrl Pts',(-2.63044769614055,-0.428698914290595,
8.85808743050665));
#397819=CARTESIAN_POINT('Ctrl Pts',(-2.63034146522525,-0.428245260526917,
8.85866804508409));
#397820=CARTESIAN_POINT('Ctrl Pts',(-2.63029245258373,-0.428035954514361,
8.85893592806395));
#397821=CARTESIAN_POINT('Ctrl Pts',(-2.63025142607327,-0.427812678304165,
8.85919241173848));
#397822=CARTESIAN_POINT('Ctrl Pts',(-2.63022171543869,-0.427572600858362,
8.85943017985534));
#397823=CARTESIAN_POINT('Ctrl Pts',(-2.63018159728671,-0.427248425236,8.8597512372));
#397824=CARTESIAN_POINT('Ctrl Pts',(-2.63016172595496,-0.426885286146236,
8.86004599534706));
#397825=CARTESIAN_POINT('Ctrl Pts',(-2.63017273972452,-0.426486977495829,
8.86026130871721));
#397826=CARTESIAN_POINT('Ctrl Pts',(-2.63017677217606,-0.426341145469406,
8.86034014101235));
#397827=CARTESIAN_POINT('Ctrl Pts',(-2.63018499302248,-0.42618840807178,
8.86040910639692));
#397828=CARTESIAN_POINT('Ctrl Pts',(-2.63019751418393,-0.426032944626492,
8.86046313645506));
#397829=CARTESIAN_POINT('Ctrl Pts',(-2.63021705335152,-0.425790345222114,
8.86054744990829));
#397830=CARTESIAN_POINT('Ctrl Pts',(-2.63024774428927,-0.425534497097203,
8.86059655985668));
#397831=CARTESIAN_POINT('Ctrl Pts',(-2.6302873278218,-0.42528177367858,
8.86059725258816));
#397832=CARTESIAN_POINT('Ctrl Pts',(-2.6303270028081,-0.425028466367897,
8.86059794692011));
#397833=CARTESIAN_POINT('Ctrl Pts',(-2.6303786762971,-0.424775900125044,
8.86056369958366));
#397834=CARTESIAN_POINT('Ctrl Pts',(-2.63043584326274,-0.424537095753612,
8.86048590497774));
#397835=CARTESIAN_POINT('Ctrl Pts',(-2.6304507621387,-0.424474774922731,
8.86046560290182));
#397836=CARTESIAN_POINT('Ctrl Pts',(-2.6304663373265,-0.424412601679678,
8.86044257503091));
#397837=CARTESIAN_POINT('Ctrl Pts',(-2.63048205569772,-0.424352489252253,
8.86041778462583));
#397838=CARTESIAN_POINT('Ctrl Pts',(-2.63058782083114,-0.423948007208984,
8.86025097596201));
#397839=CARTESIAN_POINT('Ctrl Pts',(-2.63071458213299,-0.423582638895403,
8.8599848982295));
#397840=CARTESIAN_POINT('Ctrl Pts',(-2.63085063533997,-0.423264271385127,
8.85968173251462));
#397841=CARTESIAN_POINT('Ctrl Pts',(-2.63092259969155,-0.423095873212475,
8.85952137522077));
#397842=CARTESIAN_POINT('Ctrl Pts',(-2.63099837530336,-0.422937303904813,
8.85934740853961));
#397843=CARTESIAN_POINT('Ctrl Pts',(-2.63107549094398,-0.422790129365292,
8.8591675900182));
#397844=CARTESIAN_POINT('Ctrl Pts',(-2.63138515032498,-0.422199147089306,
8.85844552518695));
#397845=CARTESIAN_POINT('Ctrl Pts',(-2.63173123784028,-0.421757093262724,
8.85759444184123));
#397846=CARTESIAN_POINT('Ctrl Pts',(-2.63204579283193,-0.421422012059516,
8.85683498915137));
#397847=CARTESIAN_POINT('Ctrl Pts',(-2.63207871017408,-0.421386946703997,
8.85675551444997));
#397848=CARTESIAN_POINT('Ctrl Pts',(-2.63211129380289,-0.421353069065475,
8.85667699793651));
#397849=CARTESIAN_POINT('Ctrl Pts',(-2.63214347290436,-0.421320342132146,
8.85659965593547));
#397850=CARTESIAN_POINT('Ctrl Pts',(-2.63257782805809,-0.420878592316076,
8.85555568965886));
#397851=CARTESIAN_POINT('Ctrl Pts',(-2.6330590676858,-0.420516772853006,
8.85434650606346));
#397852=CARTESIAN_POINT('Ctrl Pts',(-2.63358583604686,-0.420228127733416,
8.85297329937117));
#397853=CARTESIAN_POINT('Ctrl Pts',(-2.63388211115349,-0.420065782441052,
8.85220095427747));
#397854=CARTESIAN_POINT('Ctrl Pts',(-2.63419306117444,-0.419926794961179,
8.85137579139183));
#397855=CARTESIAN_POINT('Ctrl Pts',(-2.6345200847159,-0.419811799220444,
8.85049129520029));
#397856=CARTESIAN_POINT('Origin',(-2.63680073810823,-0.426297494642222,
7.59394543036555));
#397857=CARTESIAN_POINT('Ctrl Pts',(-2.63214794555735,-0.431389968309504,
7.59443877723642));
#397858=CARTESIAN_POINT('Ctrl Pts',(-2.62756869039428,-0.427845449188351,
7.58783886950016));
#397859=CARTESIAN_POINT('Ctrl Pts',(-2.63107088212544,-0.420111508755763,
7.58559994247159));
#397860=CARTESIAN_POINT('Ctrl Pts',(-2.65714596514287,-0.45073939420009,
7.56670252222133));
#397861=CARTESIAN_POINT('Ctrl Pts',(-2.65257332830362,-0.447199997915386,
7.56004874999028));
#397862=CARTESIAN_POINT('Ctrl Pts',(-2.6560768087082,-0.439411417665357,
7.55786368756704));
#397863=CARTESIAN_POINT('Ctrl Pts',(-2.68209730342447,-0.470052686971096,
7.53888913333557));
#397864=CARTESIAN_POINT('Ctrl Pts',(-2.67749749118057,-0.466492255880973,
7.53222002137277));
#397865=CARTESIAN_POINT('Ctrl Pts',(-2.68103621251044,-0.458676893057046,
7.53005029815327));
#397866=CARTESIAN_POINT('Ctrl Pts',(-2.70700083133714,-0.489328972682922,
7.51101258149734));
#397867=CARTESIAN_POINT('Ctrl Pts',(-2.70234526101078,-0.485725382698516,
7.5043616886572));
#397868=CARTESIAN_POINT('Ctrl Pts',(-2.70594791084535,-0.477906917650045,
7.50217374673251));
#397869=CARTESIAN_POINT('',(-2.70461858999357,-0.476880779649026,7.50366116523517));
#397870=CARTESIAN_POINT('Ctrl Pts',(-2.70021641947034,-0.48407757770026,
7.51860402984325));
#397871=CARTESIAN_POINT('Ctrl Pts',(-2.70056563816122,-0.484347886360344,
7.51734760759493));
#397872=CARTESIAN_POINT('Ctrl Pts',(-2.70091762496879,-0.484545099816474,
7.51608817408573));
#397873=CARTESIAN_POINT('Ctrl Pts',(-2.70127809748605,-0.484657114758125,
7.5148100591312));
#397874=CARTESIAN_POINT('Ctrl Pts',(-2.70160462210596,-0.484758580568956,
7.51365231206384));
#397875=CARTESIAN_POINT('Ctrl Pts',(-2.70193849542102,-0.484790521480701,
7.51247773061042));
#397876=CARTESIAN_POINT('Ctrl Pts',(-2.70227745670569,-0.484715627587292,
7.51129758471022));
#397877=CARTESIAN_POINT('Ctrl Pts',(-2.70269874687169,-0.48462254303099,
7.50983079813402));
#397878=CARTESIAN_POINT('Ctrl Pts',(-2.70311164139659,-0.484354676680229,
7.50839324291155));
#397879=CARTESIAN_POINT('Ctrl Pts',(-2.7034742857841,-0.483840913194821,
7.50715379678855));
#397880=CARTESIAN_POINT('Ctrl Pts',(-2.70364181704178,-0.483603569268302,
7.50658120839351));
#397881=CARTESIAN_POINT('Ctrl Pts',(-2.70381467744276,-0.48327452667053,
7.50598221009429));
#397882=CARTESIAN_POINT('Ctrl Pts',(-2.70396861630568,-0.48285103738752,
7.50545747549611));
#397883=CARTESIAN_POINT('Ctrl Pts',(-2.70405076284779,-0.482625050397887,
7.50517746087247));
#397884=CARTESIAN_POINT('Ctrl Pts',(-2.7041286023332,-0.48236978725599,
7.50491486231392));
#397885=CARTESIAN_POINT('Ctrl Pts',(-2.7041984779562,-0.48209152123559,
7.50468370960993));
#397886=CARTESIAN_POINT('Ctrl Pts',(-2.7043029640536,-0.481675425761052,
7.50433806340447));
#397887=CARTESIAN_POINT('Ctrl Pts',(-2.7043922364335,-0.481195283876931,
7.50405484070984));
#397888=CARTESIAN_POINT('Ctrl Pts',(-2.70445957844277,-0.480683301291921,
7.50385766036131));
#397889=CARTESIAN_POINT('Ctrl Pts',(-2.70446677962393,-0.480628552712466,
7.50383657498791));
#397890=CARTESIAN_POINT('Ctrl Pts',(-2.70447374114721,-0.480573466128605,
7.50381643264937));
#397891=CARTESIAN_POINT('Ctrl Pts',(-2.70448046317028,-0.480518099751973,
7.50379723213559));
#397892=CARTESIAN_POINT('Ctrl Pts',(-2.70452533487324,-0.480148511076355,
7.50366906242519));
#397893=CARTESIAN_POINT('Ctrl Pts',(-2.70455979670366,-0.479758328762587,
7.50358235568538));
#397894=CARTESIAN_POINT('Ctrl Pts',(-2.70458397329211,-0.479381442565697,
7.5035341175365));
#397895=CARTESIAN_POINT('Ctrl Pts',(-2.70462022335022,-0.47881634436874,
7.50346178989176));
#397896=CARTESIAN_POINT('Ctrl Pts',(-2.7046351928416,-0.478206885991972,
7.50346967198527));
#397897=CARTESIAN_POINT('Ctrl Pts',(-2.70463147855747,-0.477608134512351,
7.50354272648692));
#397898=CARTESIAN_POINT('Ctrl Pts',(-2.70462995079553,-0.477361855635362,
7.50357277531559));
#397899=CARTESIAN_POINT('Ctrl Pts',(-2.70462540584846,-0.477117714546017,
7.50361331098761));
#397900=CARTESIAN_POINT('Ctrl Pts',(-2.70461858999497,-0.476880779649272,
7.50366116523658));
#397901=CARTESIAN_POINT('',(-2.63969113251173,-0.426764791193839,7.57603338622103));
#397902=CARTESIAN_POINT('Origin',(-2.64841525255386,-0.428172349042246,
7.58486873427628));
#397903=CARTESIAN_POINT('Ctrl Pts',(-2.70461859003549,-0.476880779688155,
7.50366116529968));
#397904=CARTESIAN_POINT('Ctrl Pts',(-2.68301193100263,-0.460202048194472,
7.52783573079709));
#397905=CARTESIAN_POINT('Ctrl Pts',(-2.66137047797874,-0.443497493267363,
7.55196141284068));
#397906=CARTESIAN_POINT('Ctrl Pts',(-2.63969113324643,-0.426764792207667,
7.57603338728831));
#397907=CARTESIAN_POINT('Ctrl Pts',(-2.63351343964692,-0.432224581148218,
7.5963967733137));
#397908=CARTESIAN_POINT('Ctrl Pts',(-2.61671933910955,-0.423050889786067,
7.59974925422224));
#397909=CARTESIAN_POINT('Ctrl Pts',(-2.63554858227812,-0.419636504370458,
7.59639677331373));
#397910=CARTESIAN_POINT('Ctrl Pts',(-2.62983415240469,-0.430929224257954,
7.5870762605742));
#397911=CARTESIAN_POINT('Ctrl Pts',(-2.62689172333802,-0.424695481979904,
7.58811717123965));
#397912=CARTESIAN_POINT('Ctrl Pts',(-2.63164855597466,-0.41970649662526,
7.58707626057426));
#397913=CARTESIAN_POINT('Ctrl Pts',(-2.63527988042917,-0.428232990116521,
7.58015376756929));
#397914=CARTESIAN_POINT('Ctrl Pts',(-2.63371451346334,-0.425798537775517,
7.5820876076604));
#397915=CARTESIAN_POINT('Ctrl Pts',(-2.63596724991743,-0.423981366785814,
7.58015376756931));
#397916=CARTESIAN_POINT('Ctrl Pts',(-2.63969113169473,-0.426764791061958,
7.57603338509286));
#397917=CARTESIAN_POINT('Ctrl Pts',(-2.63969113169473,-0.426764791061958,
7.57603338509286));
#397918=CARTESIAN_POINT('Ctrl Pts',(-2.63969113169473,-0.426764791061958,
7.57603338509286));
#397919=CARTESIAN_POINT('Origin',(-2.64841434182015,-0.428177982249053,
7.58486873427621));
#397920=CARTESIAN_POINT('Ctrl Pts',(-2.72331185699535,-0.388588739318512,
7.51098857897448));
#397921=CARTESIAN_POINT('Ctrl Pts',(-2.71775791507471,-0.390541747540201,
7.50433767179956));
#397922=CARTESIAN_POINT('Ctrl Pts',(-2.71871338746912,-0.399097162409509,
7.50214974420965));
#397923=CARTESIAN_POINT('Ctrl Pts',(-2.69359435960954,-0.399038707566613,
7.53887321589164));
#397924=CARTESIAN_POINT('Ctrl Pts',(-2.68810696376955,-0.40096831528384,
7.53220407452058));
#397925=CARTESIAN_POINT('Ctrl Pts',(-2.68900271478691,-0.409500639119532,
7.53003438070911));
#397926=CARTESIAN_POINT('Ctrl Pts',(-2.66381979366646,-0.409508743608567,
7.56669465659232));
#397927=CARTESIAN_POINT('Ctrl Pts',(-2.65836482731572,-0.411426947702915,
7.56004085833301));
#397928=CARTESIAN_POINT('Ctrl Pts',(-2.65923556380894,-0.419922738901258,
7.55785582193789));
#397929=CARTESIAN_POINT('Ctrl Pts',(-2.63398950575049,-0.419998373926575,
7.59443891967696));
#397930=CARTESIAN_POINT('Ctrl Pts',(-2.62852663037769,-0.421919359178055,
7.58783901202978));
#397931=CARTESIAN_POINT('Ctrl Pts',(-2.62941337726011,-0.430362868990617,
7.58560008491213));
#397932=CARTESIAN_POINT('',(-2.7171028689902,-0.399661099761616,7.50366116523517));
#397933=CARTESIAN_POINT('Ctrl Pts',(-2.71710286899057,-0.399661099761671,
7.50366116523554));
#397934=CARTESIAN_POINT('Ctrl Pts',(-2.71736205082467,-0.398949086915132,
7.50350835821027));
#397935=CARTESIAN_POINT('Ctrl Pts',(-2.71757713724069,-0.398286142087269,
7.50345484956));
#397936=CARTESIAN_POINT('Ctrl Pts',(-2.71775509412383,-0.397652740707318,
7.50349758195598));
#397937=CARTESIAN_POINT('Ctrl Pts',(-2.71784639920251,-0.397327758825133,
7.50351950684424));
#397938=CARTESIAN_POINT('Ctrl Pts',(-2.71793705412928,-0.396978557601486,
7.50357029184312));
#397939=CARTESIAN_POINT('Ctrl Pts',(-2.71801521557553,-0.39663942394169,
7.50365515313924));
#397940=CARTESIAN_POINT('Ctrl Pts',(-2.71813545953055,-0.396117699044139,
7.50378570417639));
#397941=CARTESIAN_POINT('Ctrl Pts',(-2.71823000319195,-0.395604564193579,
7.50400001621911));
#397942=CARTESIAN_POINT('Ctrl Pts',(-2.71828941758173,-0.395138665010699,
7.50428903009635));
#397943=CARTESIAN_POINT('Ctrl Pts',(-2.71829601212189,-0.395086953785816,
7.50432110841318));
#397944=CARTESIAN_POINT('Ctrl Pts',(-2.71830219412158,-0.395035801890458,
7.50435406373354));
#397945=CARTESIAN_POINT('Ctrl Pts',(-2.7183079653914,-0.39498524529686,
7.50438785222352));
#397946=CARTESIAN_POINT('Ctrl Pts',(-2.71834320176766,-0.394676572992338,
7.50459414719561));
#397947=CARTESIAN_POINT('Ctrl Pts',(-2.71836317598707,-0.394385118815837,
7.50483629897752));
#397948=CARTESIAN_POINT('Ctrl Pts',(-2.71836843579496,-0.394122138271499,
7.5050991045531));
#397949=CARTESIAN_POINT('Ctrl Pts',(-2.71838003945946,-0.393541976776796,
7.50567888004914));
#397950=CARTESIAN_POINT('Ctrl Pts',(-2.71832100728855,-0.393077541734335,
7.50637912803144));
#397951=CARTESIAN_POINT('Ctrl Pts',(-2.71821992155784,-0.392717065736705,
7.50710440483569));
#397952=CARTESIAN_POINT('Ctrl Pts',(-2.71819513332984,-0.392628669865636,
7.50728225710685));
#397953=CARTESIAN_POINT('Ctrl Pts',(-2.71816746337447,-0.392544726240364,
7.50746498566954));
#397954=CARTESIAN_POINT('Ctrl Pts',(-2.71813795325093,-0.392467063959509,
7.50764697238949));
#397955=CARTESIAN_POINT('Ctrl Pts',(-2.71797931494821,-0.392049572910864,
7.50862528291182));
#397956=CARTESIAN_POINT('Ctrl Pts',(-2.71775696699509,-0.391774233741921,
7.50965856837422));
#397957=CARTESIAN_POINT('Ctrl Pts',(-2.71750939926049,-0.391587065661359,
7.51067959873203));
#397958=CARTESIAN_POINT('Ctrl Pts',(-2.71737316242388,-0.391484066830545,
7.51124147302579));
#397959=CARTESIAN_POINT('Ctrl Pts',(-2.71722899301611,-0.39140809036546,
7.51180065547253));
#397960=CARTESIAN_POINT('Ctrl Pts',(-2.71708174754227,-0.391352365307991,
7.512351757165));
#397961=CARTESIAN_POINT('Ctrl Pts',(-2.71657295577451,-0.391159813036211,
7.51425603304535));
#397962=CARTESIAN_POINT('Ctrl Pts',(-2.71596462603848,-0.391191771758356,
7.51626900505179));
#397963=CARTESIAN_POINT('Ctrl Pts',(-2.71530098268083,-0.391407169895963,
7.51827788969242));
#397964=CARTESIAN_POINT('Ctrl Pts',(-2.71526506504821,-0.391418827650217,
7.51838661432544));
#397965=CARTESIAN_POINT('Ctrl Pts',(-2.71522898031722,-0.391431031303703,
7.51849533314856));
#397966=CARTESIAN_POINT('Ctrl Pts',(-2.71519273396521,-0.391443777102002,
7.51860402984325));
#397967=CARTESIAN_POINT('Ctrl Pts',(-2.63969113352968,-0.426764790463122,
7.57603338728985));
#397968=CARTESIAN_POINT('Ctrl Pts',(-2.66553865185878,-0.417715864043942,
7.55196141284922));
#397969=CARTESIAN_POINT('Ctrl Pts',(-2.69134133978206,-0.40868170987964,
7.52783573083104));
#397970=CARTESIAN_POINT('Ctrl Pts',(-2.71710286904403,-0.399661099737013,
7.50366116530176));
#397971=CARTESIAN_POINT('Origin',(-9.12135307609332E-16,-1.47466962819323E-16,
7.49482233047033));
#397972=CARTESIAN_POINT('Origin',(-2.69591402793581,-0.47534598344672,7.49482233047033));
#397973=CARTESIAN_POINT('Origin',(0.,0.,7.50366116523517));
#397974=CARTESIAN_POINT('Origin',(-2.70835812744774,-0.398374827879208,
7.49482233047033));
#397975=CARTESIAN_POINT('Ctrl Pts',(-2.70021558301562,-0.484076930308821,
7.51860402984325));
#397976=CARTESIAN_POINT('Ctrl Pts',(-2.70623301486718,-0.488733839148586,
7.51860402984325));
#397977=CARTESIAN_POINT('Ctrl Pts',(-2.70486003209636,-0.496217902506222,
7.51860402984325));
#397978=CARTESIAN_POINT('Ctrl Pts',(-2.70244989574948,-0.485806073346367,
7.51041458714366));
#397979=CARTESIAN_POINT('Ctrl Pts',(-2.7059077297859,-0.490506897692872,
7.51004642900443));
#397980=CARTESIAN_POINT('Ctrl Pts',(-2.70485965344402,-0.496219966522037,
7.5072913648301));
#397981=CARTESIAN_POINT('Ctrl Pts',(-2.70483489309648,-0.484310906180435,
7.50215815450138));
#397982=CARTESIAN_POINT('Ctrl Pts',(-2.70657018076302,-0.486896798907495,
7.4987716367153));
#397983=CARTESIAN_POINT('Ctrl Pts',(-2.70597109473124,-0.490294595181685,
7.49481588533171));
#397984=CARTESIAN_POINT('Ctrl Pts',(-2.70461804783867,-0.476880684055306,
7.50366171572174));
#397985=CARTESIAN_POINT('Ctrl Pts',(-2.70822413765248,-0.477516513051119,
7.50000045605858));
#397986=CARTESIAN_POINT('Ctrl Pts',(-2.70822413765246,-0.477516513051242,
7.49482233047317));
#397987=CARTESIAN_POINT('Origin',(-2.69256521376865,-0.493962366585738,
7.51860402984325));
#397988=CARTESIAN_POINT('Origin',(-2.69256521376865,-0.493962366585738,
9.));
#397989=CARTESIAN_POINT('Origin',(-2.69256521376865,-0.493962366585738,
8.75721825406948));
#397990=CARTESIAN_POINT('Ctrl Pts',(-2.68701019562603,-0.473855492158896,
8.78942910404912));
#397991=CARTESIAN_POINT('Ctrl Pts',(-2.69142915185674,-0.47725037868611,
8.7967269950169));
#397992=CARTESIAN_POINT('Ctrl Pts',(-2.68738353924326,-0.485206917164847,
8.79893251111267));
#397993=CARTESIAN_POINT('Ctrl Pts',(-2.69570433342993,-0.480585082531806,
8.78111911759583));
#397994=CARTESIAN_POINT('Ctrl Pts',(-2.70093852227643,-0.484615662793361,
8.78644465894816));
#397995=CARTESIAN_POINT('Ctrl Pts',(-2.69889957586774,-0.492461566776834,
8.78817647674132));
#397996=CARTESIAN_POINT('Ctrl Pts',(-2.70112272746461,-0.484779123793258,
8.7678092393203));
#397997=CARTESIAN_POINT('Ctrl Pts',(-2.70729835735771,-0.489541091054135,
8.76988516158372));
#397998=CARTESIAN_POINT('Ctrl Pts',(-2.70608633938462,-0.497002149479666,
8.77093053738832));
#397999=CARTESIAN_POINT('Ctrl Pts',(-2.70006621478272,-0.483961343148133,
8.75371302330492));
#398000=CARTESIAN_POINT('Ctrl Pts',(-2.70609074084473,-0.488605833119682,
8.75300828287559));
#398001=CARTESIAN_POINT('Ctrl Pts',(-2.70468438422376,-0.496116938257335,
8.75267964240738));
#398002=CARTESIAN_POINT('Origin',(-2.68147639343957,-0.485379194369336,
8.78727029226991));
#398003=CARTESIAN_POINT('Ctrl Pts',(-2.6325925749723,-0.431734128529235,
8.85049129520029));
#398004=CARTESIAN_POINT('Ctrl Pts',(-2.637210444489,-0.43530853664105,8.85711686593484));
#398005=CARTESIAN_POINT('Ctrl Pts',(-2.63365770878388,-0.443085350328122,
8.85933012996512));
#398006=CARTESIAN_POINT('Ctrl Pts',(-2.65146500140032,-0.446342110385364,
8.82945683644722));
#398007=CARTESIAN_POINT('Ctrl Pts',(-2.65612120202604,-0.449946188245629,
8.83607469902387));
#398008=CARTESIAN_POINT('Ctrl Pts',(-2.65252392414128,-0.457730251086948,
8.83829567148519));
#398009=CARTESIAN_POINT('Ctrl Pts',(-2.6703092969549,-0.460928317866566,
8.80838214965001));
#398010=CARTESIAN_POINT('Ctrl Pts',(-2.6749838731222,-0.464546619100782,
8.81501364461988));
#398011=CARTESIAN_POINT('Ctrl Pts',(-2.6713619303665,-0.472352408187708,
8.81722098428721));
#398012=CARTESIAN_POINT('Ctrl Pts',(-2.68912759914126,-0.475494405483858,
8.78727029226991));
#398013=CARTESIAN_POINT('Ctrl Pts',(-2.69380295177103,-0.4791133077298,
8.79393457792714));
#398014=CARTESIAN_POINT('Ctrl Pts',(-2.69017388854615,-0.486953544670607,
8.79610912703474));
#398015=CARTESIAN_POINT('Origin',(-2.62494136927061,-0.441618917414714,
8.85049129520029));
#398016=CARTESIAN_POINT('Ctrl Pts',(-2.6345200847159,-0.419811799220444,
8.85049129520029));
#398017=CARTESIAN_POINT('Ctrl Pts',(-2.64002902569028,-0.417874615294239,
8.85711686593484));
#398018=CARTESIAN_POINT('Ctrl Pts',(-2.63910781935455,-0.40937448935394,
8.85933012996512));
#398019=CARTESIAN_POINT('Ctrl Pts',(-2.62964640415828,-0.421525597876414,
8.86332496987231));
#398020=CARTESIAN_POINT('Ctrl Pts',(-2.63066116705591,-0.417017588267029,
8.86648636486737));
#398021=CARTESIAN_POINT('Ctrl Pts',(-2.62547918270721,-0.414185073465195,
8.87206031107457));
#398022=CARTESIAN_POINT('Ctrl Pts',(-2.62847945114439,-0.428550412938697,
8.86341338519877));
#398023=CARTESIAN_POINT('Ctrl Pts',(-2.6279912546431,-0.43315857252908,
8.8665458496606));
#398024=CARTESIAN_POINT('Ctrl Pts',(-2.62214976138055,-0.434159127000912,
8.87215952290714));
#398025=CARTESIAN_POINT('Ctrl Pts',(-2.6325925749723,-0.431734128529235,
8.85049129520029));
#398026=CARTESIAN_POINT('Ctrl Pts',(-2.637210444489,-0.43530853664105,8.85711686593484));
#398027=CARTESIAN_POINT('Ctrl Pts',(-2.63365770878388,-0.443085350328122,
8.85933012996512));
#398028=CARTESIAN_POINT('Origin',(-2.6303734421844,-0.408019625726303,8.85049129520029));
#398029=CARTESIAN_POINT('Ctrl Pts',(-2.70196419720223,-0.396095507607684,
8.78727029226991));
#398030=CARTESIAN_POINT('Ctrl Pts',(-2.70754171332274,-0.394134209669103,
8.79393457792714));
#398031=CARTESIAN_POINT('Ctrl Pts',(-2.7065680531042,-0.385549840096616,
8.79610912703474));
#398032=CARTESIAN_POINT('Ctrl Pts',(-2.67951468545062,-0.403989735104165,
8.80838214965001));
#398033=CARTESIAN_POINT('Ctrl Pts',(-2.68509127528122,-0.402028762889512,
8.81501364461987));
#398034=CARTESIAN_POINT('Ctrl Pts',(-2.68411351798304,-0.393479329969075,
8.81722098428721));
#398035=CARTESIAN_POINT('Ctrl Pts',(-2.65703416460907,-0.411894866749169,
8.82945683644722));
#398036=CARTESIAN_POINT('Ctrl Pts',(-2.66258883312429,-0.409941603025111,
8.83607469902388));
#398037=CARTESIAN_POINT('Ctrl Pts',(-2.66162763804508,-0.401420561626501,
8.8382956714852));
#398038=CARTESIAN_POINT('Ctrl Pts',(-2.6345200847159,-0.419811799220444,
8.85049129520029));
#398039=CARTESIAN_POINT('Ctrl Pts',(-2.64002902569028,-0.417874615294238,
8.85711686593484));
#398040=CARTESIAN_POINT('Ctrl Pts',(-2.63910781935455,-0.40937448935394,
8.85933012996512));
#398041=CARTESIAN_POINT('Origin',(-2.69781755467073,-0.384303334113543,
8.78727029226991));
#398042=CARTESIAN_POINT('Ctrl Pts',(-2.71501805167228,-0.391505183460838,
8.75374538247847));
#398043=CARTESIAN_POINT('Ctrl Pts',(-2.72219106603802,-0.388996749029462,
8.75304829418601));
#398044=CARTESIAN_POINT('Ctrl Pts',(-2.72322767091958,-0.381433939133099,
8.75272238421917));
#398045=CARTESIAN_POINT('Ctrl Pts',(-2.7162632899384,-0.391067303825958,
8.76769408445021));
#398046=CARTESIAN_POINT('Ctrl Pts',(-2.7236165813667,-0.388495094631014,
8.76974318093971));
#398047=CARTESIAN_POINT('Ctrl Pts',(-2.72481935447853,-0.38104045217669,
8.7707786988043));
#398048=CARTESIAN_POINT('Ctrl Pts',(-2.70988090795657,-0.393311625404748,
8.78108014887987));
#398049=CARTESIAN_POINT('Ctrl Pts',(-2.71611381205453,-0.39113535708353,
8.78639403366322));
#398050=CARTESIAN_POINT('Ctrl Pts',(-2.71667000517196,-0.383059917470429,
8.78812224174741));
#398051=CARTESIAN_POINT('Ctrl Pts',(-2.69942159280191,-0.396989573000167,
8.78944554828685));
#398052=CARTESIAN_POINT('Ctrl Pts',(-2.70467629853093,-0.395160779595081,
8.79673892988686));
#398053=CARTESIAN_POINT('Ctrl Pts',(-2.70334794704577,-0.38634380524735,
8.79894799272499));
#398054=CARTESIAN_POINT('Origin',(-2.71104609143371,-0.379651603607865,
8.75721825406948));
#398055=CARTESIAN_POINT('Origin',(-2.71104609143371,-0.379651603607865,
9.));
#398056=CARTESIAN_POINT('Origin',(-2.71104609143371,-0.379651603607865,
7.51860402984325));
#398057=CARTESIAN_POINT('Ctrl Pts',(-2.71710209070084,-0.399660985282277,
7.50366195182966));
#398058=CARTESIAN_POINT('Ctrl Pts',(-2.72072505953656,-0.400193891020071,
7.50000065167735));
#398059=CARTESIAN_POINT('Ctrl Pts',(-2.72072505953658,-0.400193891019955,
7.49482233047108));
#398060=CARTESIAN_POINT('Ctrl Pts',(-2.71965064636477,-0.392671088027347,
7.50215800491338));
#398061=CARTESIAN_POINT('Ctrl Pts',(-2.72211237908244,-0.390762012543981,
7.49877273257264));
#398062=CARTESIAN_POINT('Ctrl Pts',(-2.72261477294344,-0.387346641882056,
7.49481816995647));
#398063=CARTESIAN_POINT('Ctrl Pts',(-2.71785182623255,-0.390509083754931,
7.51043025814042));
#398064=CARTESIAN_POINT('Ctrl Pts',(-2.72261960393336,-0.387138467671442,
7.51006209594516));
#398065=CARTESIAN_POINT('Ctrl Pts',(-2.72342564846379,-0.381382665175063,
7.50731281821701));
#398066=CARTESIAN_POINT('Ctrl Pts',(-2.7151913081126,-0.391444278397112,
7.51860402984326));
#398067=CARTESIAN_POINT('Ctrl Pts',(-2.72237000153422,-0.388920911965344,
7.51860402984326));
#398068=CARTESIAN_POINT('Ctrl Pts',(-2.72342529733067,-0.381385172574106,
7.51860402984327));
#398069=CARTESIAN_POINT('Origin',(0.,0.,7.5));
#398070=CARTESIAN_POINT('Origin',(-2.60220974632391,-0.587743532225626,
7.5));
#398071=CARTESIAN_POINT('',(-2.60220974632391,-0.587743532225626,7.59394543036555));
#398072=CARTESIAN_POINT('',(-2.60220974632391,-0.587743532225626,8.85049129520029));
#398073=CARTESIAN_POINT('',(-2.60220974632391,-0.587743532225626,7.5));
#398074=CARTESIAN_POINT('',(-2.67103479566853,-0.568397127400952,8.78727029226991));
#398075=CARTESIAN_POINT('Ctrl Pts',(-2.60220974632391,-0.587743532225626,
8.85049129520029));
#398076=CARTESIAN_POINT('Ctrl Pts',(-2.62518477739697,-0.581285356659731,
8.82945686509571));
#398077=CARTESIAN_POINT('Ctrl Pts',(-2.64812565330825,-0.574836781952725,
8.80838212259896));
#398078=CARTESIAN_POINT('Ctrl Pts',(-2.67103479566853,-0.568397127400952,
8.78727029226991));
#398079=CARTESIAN_POINT('',(-2.68453419038077,-0.564602509634922,8.75721825406948));
#398080=CARTESIAN_POINT('Origin',(-2.64390988332796,-0.576022025128176,
8.75937679713109));
#398081=CARTESIAN_POINT('',(-2.68453419038077,-0.564602509634922,7.51860402984325));
#398082=CARTESIAN_POINT('',(-2.68453419038077,-0.564602509634922,7.5));
#398083=CARTESIAN_POINT('Ctrl Pts',(-2.68453419038077,-0.564602509634922,
7.51860402984325));
#398084=CARTESIAN_POINT('Ctrl Pts',(-2.67393251538731,-0.567582591715445,
7.52834476460825));
#398085=CARTESIAN_POINT('Ctrl Pts',(-2.66332395793944,-0.570564608422258,
7.53807742314407));
#398086=CARTESIAN_POINT('Ctrl Pts',(-2.65270828694958,-0.573548624713003,
7.54780169004674));
#398087=CARTESIAN_POINT('Ctrl Pts',(-2.63589363782969,-0.578275145245223,
7.5632044032688));
#398088=CARTESIAN_POINT('Ctrl Pts',(-2.61906112037001,-0.583006688485557,
7.57858609112103));
#398089=CARTESIAN_POINT('Ctrl Pts',(-2.60220974632391,-0.587743532225626,
7.59394543036555));
#398090=CARTESIAN_POINT('Origin',(-2.80575616266556,-0.781431603558352,
7.5));
#398091=CARTESIAN_POINT('',(-2.66365357834825,-0.656086448390715,8.75721825406948));
#398092=CARTESIAN_POINT('',(-2.65313746692184,-0.646810448064364,8.78727029226991));
#398093=CARTESIAN_POINT('Origin',(-2.62644365380542,-0.623264499458519,
8.75658640620935));
#398094=CARTESIAN_POINT('',(-2.5995223305943,-0.599517869856899,8.85049129520029));
#398095=CARTESIAN_POINT('Ctrl Pts',(-2.65313746692184,-0.646810448064364,
8.78727029226991));
#398096=CARTESIAN_POINT('Ctrl Pts',(-2.63529110426043,-0.631068615445907,
8.80838212259895));
#398097=CARTESIAN_POINT('Ctrl Pts',(-2.61742002096782,-0.615304977373541,
8.82945686509571));
#398098=CARTESIAN_POINT('Ctrl Pts',(-2.5995223305943,-0.599517869856899,
8.85049129520029));
#398099=CARTESIAN_POINT('',(-2.5995223305943,-0.599517869856899,7.59394543036555));
#398100=CARTESIAN_POINT('',(-2.5995223305943,-0.599517869856899,7.5));
#398101=CARTESIAN_POINT('',(-2.66365357834825,-0.656086448390715,7.51860402984325));
#398102=CARTESIAN_POINT('Ctrl Pts',(-2.5995223305943,-0.599517869856899,
7.59394543036555));
#398103=CARTESIAN_POINT('Ctrl Pts',(-2.61264965451767,-0.611097155779211,
7.57858609112103));
#398104=CARTESIAN_POINT('Ctrl Pts',(-2.62576228904419,-0.622663484549916,
7.56320440326857));
#398105=CARTESIAN_POINT('Ctrl Pts',(-2.63886100402437,-0.634217535235031,
7.54780169004651));
#398106=CARTESIAN_POINT('Ctrl Pts',(-2.64713067695232,-0.641512008036632,
7.53807742314383));
#398107=CARTESIAN_POINT('Ctrl Pts',(-2.6553948083875,-0.648801592825299,
7.52834476460825));
#398108=CARTESIAN_POINT('Ctrl Pts',(-2.66365357834825,-0.656086448390714,
7.51860402984325));
#398109=CARTESIAN_POINT('',(-2.66365357834825,-0.656086448390715,7.5));
#398110=CARTESIAN_POINT('Origin',(-2.60407017393684,-0.594362024055118,
7.5));
#398111=CARTESIAN_POINT('Ctrl Pts',(-2.5995223305943,-0.599517869856899,
8.85049129520029));
#398112=CARTESIAN_POINT('Ctrl Pts',(-2.5993770958507,-0.599389761901934,
8.85097269580138));
#398113=CARTESIAN_POINT('Ctrl Pts',(-2.59923925769927,-0.599256962201082,
8.85143669361005));
#398114=CARTESIAN_POINT('Ctrl Pts',(-2.59910307573752,-0.59911272614392,
8.8519052845931));
#398115=CARTESIAN_POINT('Ctrl Pts',(-2.59883671245669,-0.59883060956323,
8.85282181883899));
#398116=CARTESIAN_POINT('Ctrl Pts',(-2.59858368043392,-0.598511863228085,
8.85372622499635));
#398117=CARTESIAN_POINT('Ctrl Pts',(-2.59835208540563,-0.598141898916052,
8.8546225773507));
#398118=CARTESIAN_POINT('Ctrl Pts',(-2.59815982343862,-0.59783476768409,
8.85536669723986));
#398119=CARTESIAN_POINT('Ctrl Pts',(-2.59798226464241,-0.597492285139542,
8.85610498449051));
#398120=CARTESIAN_POINT('Ctrl Pts',(-2.59783113602522,-0.597102392478157,
8.85681338218371));
#398121=CARTESIAN_POINT('Ctrl Pts',(-2.59769398656777,-0.596748564275613,
8.85745625420284));
#398122=CARTESIAN_POINT('Ctrl Pts',(-2.5975763254901,-0.596351468932853,
8.85808743050666));
#398123=CARTESIAN_POINT('Ctrl Pts',(-2.59749937853405,-0.595891941011372,
8.8586680450841));
#398124=CARTESIAN_POINT('Ctrl Pts',(-2.59746387687653,-0.595679924789745,
8.85893592806395));
#398125=CARTESIAN_POINT('Ctrl Pts',(-2.59743724001534,-0.59545447874692,
8.85919241173848));
#398126=CARTESIAN_POINT('Ctrl Pts',(-2.5974229722392,-0.595212990999087,
8.85943017985534));
#398127=CARTESIAN_POINT('Ctrl Pts',(-2.59740370651771,-0.594886911051487,
8.8597512372));
#398128=CARTESIAN_POINT('Ctrl Pts',(-2.59740714241511,-0.594523244909332,
8.86004599534706));
#398129=CARTESIAN_POINT('Ctrl Pts',(-2.59744365327854,-0.594126460281404,
8.86026130871721));
#398130=CARTESIAN_POINT('Ctrl Pts',(-2.597457020935,-0.593981186242577,
8.86034014101235));
#398131=CARTESIAN_POINT('Ctrl Pts',(-2.59747501080947,-0.593829289371754,
8.86040910639693));
#398132=CARTESIAN_POINT('Ctrl Pts',(-2.59749746682199,-0.593674947576356,
8.86046313645507));
#398133=CARTESIAN_POINT('Ctrl Pts',(-2.59753250924147,-0.593434098497239,
8.8605474499083));
#398134=CARTESIAN_POINT('Ctrl Pts',(-2.59757952936704,-0.593180742414873,
8.86059655985668));
#398135=CARTESIAN_POINT('Ctrl Pts',(-2.59763522361598,-0.592931074369255,
8.86059725258816));
#398136=CARTESIAN_POINT('Ctrl Pts',(-2.59769104654089,-0.592680829490709,
8.86059794692011));
#398137=CARTESIAN_POINT('Ctrl Pts',(-2.5977587958359,-0.592432092904097,
8.86056369958366));
#398138=CARTESIAN_POINT('Ctrl Pts',(-2.59783114559449,-0.592197441881922,
8.86048590497774));
#398139=CARTESIAN_POINT('Ctrl Pts',(-2.59785002672736,-0.592136204951537,
8.86046560290182));
#398140=CARTESIAN_POINT('Ctrl Pts',(-2.59786955336763,-0.592075157355788,
8.86044257503091));
#398141=CARTESIAN_POINT('Ctrl Pts',(-2.59788909086022,-0.592016175515294,
8.86041778462583));
#398142=CARTESIAN_POINT('Ctrl Pts',(-2.59802055394132,-0.591619300919128,
8.860250975962));
#398143=CARTESIAN_POINT('Ctrl Pts',(-2.5981704640267,-0.591262804918427,
8.8599848982295));
#398144=CARTESIAN_POINT('Ctrl Pts',(-2.5983266355742,-0.590953808487247,
8.85968173251462));
#398145=CARTESIAN_POINT('Ctrl Pts',(-2.59840924137526,-0.590790367078537,
8.85952137522077));
#398146=CARTESIAN_POINT('Ctrl Pts',(-2.59849502086838,-0.590636978528642,
8.85934740853961));
#398147=CARTESIAN_POINT('Ctrl Pts',(-2.59858140757177,-0.590495047191055,
8.8591675900182));
#398148=CARTESIAN_POINT('Ctrl Pts',(-2.59892829508878,-0.589925119096205,
8.85844552518695));
#398149=CARTESIAN_POINT('Ctrl Pts',(-2.59930199401607,-0.589506147419861,
8.85759444184125));
#398150=CARTESIAN_POINT('Ctrl Pts',(-2.59963737144715,-0.589191908284434,
8.8568349891514));
#398151=CARTESIAN_POINT('Ctrl Pts',(-2.59967246780213,-0.589159023995797,
8.85675551444999));
#398152=CARTESIAN_POINT('Ctrl Pts',(-2.59970715503214,-0.589127303602779,
8.85667699793652));
#398153=CARTESIAN_POINT('Ctrl Pts',(-2.59974136484002,-0.589096705632551,
8.85659965593547));
#398154=CARTESIAN_POINT('Ctrl Pts',(-2.6002031305724,-0.588683692669106,
8.85555568965886));
#398155=CARTESIAN_POINT('Ctrl Pts',(-2.60070656329426,-0.588353449731737,
8.85434650606346));
#398156=CARTESIAN_POINT('Ctrl Pts',(-2.60125074290954,-0.588099147829275,
8.85297329937117));
#398157=CARTESIAN_POINT('Ctrl Pts',(-2.60155681078578,-0.587956118503982,
8.85220095427747));
#398158=CARTESIAN_POINT('Ctrl Pts',(-2.60187602688498,-0.587837339225038,
8.85137579139183));
#398159=CARTESIAN_POINT('Ctrl Pts',(-2.60220974632391,-0.587743532225626,
8.85049129520029));
#398160=CARTESIAN_POINT('Origin',(-2.60407017393684,-0.594362024055118,
7.59394543036555));
#398161=CARTESIAN_POINT('Ctrl Pts',(-2.59910066513916,-0.599145929246824,
7.59443877723642));
#398162=CARTESIAN_POINT('Ctrl Pts',(-2.59475791666676,-0.595315298834709,
7.58783886950016));
#398163=CARTESIAN_POINT('Ctrl Pts',(-2.59874842803424,-0.587821634806831,
7.58559994247159));
#398164=CARTESIAN_POINT('Ctrl Pts',(-2.62280760163912,-0.620057228280637,
7.56670252222134));
#398165=CARTESIAN_POINT('Ctrl Pts',(-2.61847112967122,-0.616232134217014,
7.56004874999029));
#398166=CARTESIAN_POINT('Ctrl Pts',(-2.62246642784951,-0.608684025200632,
7.55786368756704));
#398167=CARTESIAN_POINT('Ctrl Pts',(-2.6464702678038,-0.640929477552819,
7.5388891333356));
#398168=CARTESIAN_POINT('Ctrl Pts',(-2.64210802397066,-0.637081650767868,
7.53222002137279));
#398169=CARTESIAN_POINT('Ctrl Pts',(-2.64614020663337,-0.629509072099121,
7.53005029815327));
#398170=CARTESIAN_POINT('Ctrl Pts',(-2.6700875928815,-0.661761732579921,
7.51101258149734));
#398171=CARTESIAN_POINT('Ctrl Pts',(-2.6656724707267,-0.657867263142676,
7.5043616886572));
#398172=CARTESIAN_POINT('Ctrl Pts',(-2.66976864930637,-0.650295684536589,
7.50217374673251));
#398173=CARTESIAN_POINT('',(-2.66850780457431,-0.649186484966748,7.50366116523517));
#398174=CARTESIAN_POINT('Ctrl Pts',(-2.66365357834825,-0.656086448390716,
7.51860402984325));
#398175=CARTESIAN_POINT('Ctrl Pts',(-2.66398476079657,-0.656378576191014,
7.51734760759493));
#398176=CARTESIAN_POINT('Ctrl Pts',(-2.66432338889996,-0.656597936323138,
7.51608817408572));
#398177=CARTESIAN_POINT('Ctrl Pts',(-2.66467594396583,-0.656732816671555,
7.51481005913119));
#398178=CARTESIAN_POINT('Ctrl Pts',(-2.66499529676907,-0.656854994514222,
7.51365231206383));
#398179=CARTESIAN_POINT('Ctrl Pts',(-2.66532643764435,-0.65690826113668,
7.51247773061042));
#398180=CARTESIAN_POINT('Ctrl Pts',(-2.66566950096493,-0.656855238444881,
7.51129758471022));
#398181=CARTESIAN_POINT('Ctrl Pts',(-2.6660958894931,-0.656789337294395,
7.50983079813402));
#398182=CARTESIAN_POINT('Ctrl Pts',(-2.66652509793794,-0.65654847554682,
7.50839324291155));
#398183=CARTESIAN_POINT('Ctrl Pts',(-2.66691991417319,-0.656059002349277,
7.50715379678855));
#398184=CARTESIAN_POINT('Ctrl Pts',(-2.66710230789752,-0.655832879835843,
7.50658120839351));
#398185=CARTESIAN_POINT('Ctrl Pts',(-2.66729589496989,-0.655515588495294,
7.50598221009429));
#398186=CARTESIAN_POINT('Ctrl Pts',(-2.66747665060042,-0.655102832213246,
7.50545747549611));
#398187=CARTESIAN_POINT('Ctrl Pts',(-2.66757310739979,-0.654882572685144,
7.50517746087247));
#398188=CARTESIAN_POINT('Ctrl Pts',(-2.66766714172129,-0.654632821201703,
7.50491486231392));
#398189=CARTESIAN_POINT('Ctrl Pts',(-2.66775470234246,-0.654359603855222,
7.50468370960993));
#398190=CARTESIAN_POINT('Ctrl Pts',(-2.66788563309055,-0.653951057740708,
7.50433806340447));
#398191=CARTESIAN_POINT('Ctrl Pts',(-2.66800548484692,-0.653477622060605,
7.50405484070984));
#398192=CARTESIAN_POINT('Ctrl Pts',(-2.66810549133165,-0.652971006016076,
7.50385766036131));
#398193=CARTESIAN_POINT('Ctrl Pts',(-2.66811618547074,-0.652916831304707,
7.50383657498791));
#398194=CARTESIAN_POINT('Ctrl Pts',(-2.66812666210037,-0.652862303928467,
7.50381643264937));
#398195=CARTESIAN_POINT('Ctrl Pts',(-2.66813691764826,-0.652807481989489,
7.50379723213559));
#398196=CARTESIAN_POINT('Ctrl Pts',(-2.66820537678524,-0.652441527613323,
7.50366906242519));
#398197=CARTESIAN_POINT('Ctrl Pts',(-2.66826476687681,-0.652054354948022,
7.50358235568538));
#398198=CARTESIAN_POINT('Ctrl Pts',(-2.6683130409734,-0.651679792103584,
7.5035341175365));
#398199=CARTESIAN_POINT('Ctrl Pts',(-2.66838542251768,-0.651118177510677,
7.50346178989176));
#398200=CARTESIAN_POINT('Ctrl Pts',(-2.6684394093849,-0.650510930430115,
7.50346967198527));
#398201=CARTESIAN_POINT('Ctrl Pts',(-2.66847406487117,-0.649913171174624,
7.50354272648692));
#398202=CARTESIAN_POINT('Ctrl Pts',(-2.66848831939001,-0.649667300419956,
7.50357277531559));
#398203=CARTESIAN_POINT('Ctrl Pts',(-2.66849942595432,-0.649423369748904,
7.50361331098761));
#398204=CARTESIAN_POINT('Ctrl Pts',(-2.66850780457568,-0.649186484967083,
7.50366116523659));
#398205=CARTESIAN_POINT('',(-2.60692468992218,-0.595013548701113,7.57603338622103));
#398206=CARTESIAN_POINT('Origin',(-2.61554070278267,-0.596977170861205,
7.58486873427627));
#398207=CARTESIAN_POINT('Ctrl Pts',(-2.66850780461363,-0.649186485008482,
7.50366116529969));
#398208=CARTESIAN_POINT('Ctrl Pts',(-2.64801414877486,-0.631157678360157,
7.52783573079709));
#398209=CARTESIAN_POINT('Ctrl Pts',(-2.62748742494612,-0.613100872076757,
7.55196141284068));
#398210=CARTESIAN_POINT('Ctrl Pts',(-2.60692469059042,-0.595013549759931,
7.57603338728831));
#398211=CARTESIAN_POINT('Ctrl Pts',(-2.60040987984642,-0.600066314790606,
7.59639677331371));
#398212=CARTESIAN_POINT('Ctrl Pts',(-2.58423804501347,-0.589835470045179,
7.59974925422226));
#398213=CARTESIAN_POINT('Ctrl Pts',(-2.60324736190728,-0.587634493602762,
7.59639677331372));
#398214=CARTESIAN_POINT('Ctrl Pts',(-2.59682114589539,-0.598537886606972,
7.58707626057422));
#398215=CARTESIAN_POINT('Ctrl Pts',(-2.59428415960393,-0.592128430143379,
7.58811717123965));
#398216=CARTESIAN_POINT('Ctrl Pts',(-2.59935086420695,-0.587454466507708,
7.58707626057423));
#398217=CARTESIAN_POINT('Ctrl Pts',(-2.60242843340217,-0.596196101160362,
7.5801537675693));
#398218=CARTESIAN_POINT('Ctrl Pts',(-2.60102225854766,-0.593666357257013,
7.58208760766041));
#398219=CARTESIAN_POINT('Ctrl Pts',(-2.60338679305818,-0.591997253160099,
7.5801537675693));
#398220=CARTESIAN_POINT('Ctrl Pts',(-2.60692468911532,-0.59501354851716,
7.57603338509286));
#398221=CARTESIAN_POINT('Ctrl Pts',(-2.60692468911532,-0.59501354851716,
7.57603338509286));
#398222=CARTESIAN_POINT('Ctrl Pts',(-2.60692468911532,-0.59501354851716,
7.57603338509286));
#398223=CARTESIAN_POINT('Origin',(-2.61553943300043,-0.596982734143423,
7.58486873427623));
#398224=CARTESIAN_POINT('Ctrl Pts',(-2.69281955470071,-0.562273531831347,
7.51098857897448));
#398225=CARTESIAN_POINT('Ctrl Pts',(-2.68715189428301,-0.563866685107569,
7.50433767179956));
#398226=CARTESIAN_POINT('Ctrl Pts',(-2.68755725624421,-0.572465739285958,
7.50214974420965));
#398227=CARTESIAN_POINT('Ctrl Pts',(-2.66249358333605,-0.570798022904131,
7.53887321589169));
#398228=CARTESIAN_POINT('Ctrl Pts',(-2.65689383154844,-0.572372087376776,
7.53220407452063));
#398229=CARTESIAN_POINT('Ctrl Pts',(-2.65724107428411,-0.580944271602769,
7.53003438070911));
#398230=CARTESIAN_POINT('Ctrl Pts',(-2.63210937491957,-0.579338884144335,
7.56669465659233));
#398231=CARTESIAN_POINT('Ctrl Pts',(-2.62654271662394,-0.580903646188561,
7.56004085833301));
#398232=CARTESIAN_POINT('Ctrl Pts',(-2.62686733688466,-0.589437770151378,
7.55785582193789));
#398233=CARTESIAN_POINT('Ctrl Pts',(-2.60166830360742,-0.587895729282982,
7.59443891967696));
#398234=CARTESIAN_POINT('Ctrl Pts',(-2.59609357435033,-0.589462760037375,
7.58783901202978));
#398235=CARTESIAN_POINT('Ctrl Pts',(-2.59643752178507,-0.597945735821288,
7.58560008491213));
#398236=CARTESIAN_POINT('',(-2.68591391515804,-0.572925331695067,7.50366116523517));
#398237=CARTESIAN_POINT('Ctrl Pts',(-2.6859139151584,-0.572925331695144,
7.50366116523554));
#398238=CARTESIAN_POINT('Ctrl Pts',(-2.68621818329533,-0.572231387592487,
7.50350835821027));
#398239=CARTESIAN_POINT('Ctrl Pts',(-2.68647530281419,-0.571583585489863,
7.50345484956));
#398240=CARTESIAN_POINT('Ctrl Pts',(-2.68669347623158,-0.57096288723763,
7.50349758195598));
#398241=CARTESIAN_POINT('Ctrl Pts',(-2.68680541537486,-0.570644423002052,
7.50351950684424));
#398242=CARTESIAN_POINT('Ctrl Pts',(-2.68691825744058,-0.570301747530871,
7.50357029184312));
#398243=CARTESIAN_POINT('Ctrl Pts',(-2.68701798666394,-0.569968318478606,
7.50365515313924));
#398244=CARTESIAN_POINT('Ctrl Pts',(-2.68717141059382,-0.569455369577467,
7.50378570417639));
#398245=CARTESIAN_POINT('Ctrl Pts',(-2.68729863666788,-0.568949346450679,
7.50400001621911));
#398246=CARTESIAN_POINT('Ctrl Pts',(-2.68738777924756,-0.568488211200666,
7.50428903009634));
#398247=CARTESIAN_POINT('Ctrl Pts',(-2.68739767338809,-0.568437028735674,
7.50432110841318));
#398248=CARTESIAN_POINT('Ctrl Pts',(-2.68740711999939,-0.568386378019446,
7.50435406373354));
#398249=CARTESIAN_POINT('Ctrl Pts',(-2.68741611858358,-0.568336295066315,
7.50438785222352));
#398250=CARTESIAN_POINT('Ctrl Pts',(-2.68747105926538,-0.568030514564526,
7.50459414719561));
#398251=CARTESIAN_POINT('Ctrl Pts',(-2.68750966597882,-0.567740938964522,
7.50483629897752));
#398252=CARTESIAN_POINT('Ctrl Pts',(-2.6875317642012,-0.567478835738966,
7.5050991045531));
#398253=CARTESIAN_POINT('Ctrl Pts',(-2.68758051509931,-0.566900609697613,
7.50567888004914));
#398254=CARTESIAN_POINT('Ctrl Pts',(-2.68755136067167,-0.566433346682581,
7.50637912803144));
#398255=CARTESIAN_POINT('Ctrl Pts',(-2.6874735784089,-0.566067134736547,
7.50710440483569));
#398256=CARTESIAN_POINT('Ctrl Pts',(-2.68745450465388,-0.565977332297053,
7.50728225710685));
#398257=CARTESIAN_POINT('Ctrl Pts',(-2.68743226983593,-0.565891788322835,
7.50746498566954));
#398258=CARTESIAN_POINT('Ctrl Pts',(-2.68740779618353,-0.565812394887358,
7.50764697238949));
#398259=CARTESIAN_POINT('Ctrl Pts',(-2.68727623256355,-0.565385597627898,
7.50862528291182));
#398260=CARTESIAN_POINT('Ctrl Pts',(-2.68707198248926,-0.565096578290538,
7.50965856837422));
#398261=CARTESIAN_POINT('Ctrl Pts',(-2.68683691530922,-0.564893933047656,
7.51067959873202));
#398262=CARTESIAN_POINT('Ctrl Pts',(-2.68670755754355,-0.564782417114894,
7.51124147302579));
#398263=CARTESIAN_POINT('Ctrl Pts',(-2.68656855217612,-0.564697359785934,
7.51180065547253));
#398264=CARTESIAN_POINT('Ctrl Pts',(-2.68642517955058,-0.564632315171672,
7.51235175716501));
#398265=CARTESIAN_POINT('Ctrl Pts',(-2.68592977001649,-0.564407560118699,
7.51425603304536));
#398266=CARTESIAN_POINT('Ctrl Pts',(-2.68532064255679,-0.564400477358213,
7.5162690050518));
#398267=CARTESIAN_POINT('Ctrl Pts',(-2.68464456211953,-0.564572913161334,
7.51827788969244));
#398268=CARTESIAN_POINT('Ctrl Pts',(-2.68460797136865,-0.564582245712857,
7.51838661432545));
#398269=CARTESIAN_POINT('Ctrl Pts',(-2.68457117888686,-0.564592112335976,
7.51849533314857));
#398270=CARTESIAN_POINT('Ctrl Pts',(-2.68453419038077,-0.564602509634918,
7.51860402984325));
#398271=CARTESIAN_POINT('Ctrl Pts',(-2.60692469098487,-0.595013548037117,
7.57603338728985));
#398272=CARTESIAN_POINT('Ctrl Pts',(-2.63329886952168,-0.587639269793053,
7.55196141284922));
#398273=CARTESIAN_POINT('Ctrl Pts',(-2.65962736329994,-0.580276861158725,
7.52783573083105));
#398274=CARTESIAN_POINT('Ctrl Pts',(-2.68591391521332,-0.572925331673961,
7.50366116530176));
#398275=CARTESIAN_POINT('Origin',(-9.00812987045923E-16,-2.05604685939134E-16,
7.49482233047033));
#398276=CARTESIAN_POINT('Origin',(-2.65991946170316,-0.64709713896197,7.49482233047033));
#398277=CARTESIAN_POINT('Origin',(0.,0.,7.50366116523517));
#398278=CARTESIAN_POINT('Origin',(-2.6772695523474,-0.571081425081893,7.49482233047033));
#398279=CARTESIAN_POINT('Ctrl Pts',(-2.66365278509063,-0.656085748737571,
7.51860402984325));
#398280=CARTESIAN_POINT('Ctrl Pts',(-2.66935948430929,-0.661118627641122,
7.51860402984325));
#398281=CARTESIAN_POINT('Ctrl Pts',(-2.66750981689315,-0.668499346879772,
7.51860402984325));
#398282=CARTESIAN_POINT('Ctrl Pts',(-2.66577172061455,-0.657954491973657,
7.51041458714366));
#398283=CARTESIAN_POINT('Ctrl Pts',(-2.66892126731013,-0.662867202159749,
7.51004642900442));
#398284=CARTESIAN_POINT('Ctrl Pts',(-2.66750930677684,-0.668501382394503,
7.5072913648301));
#398285=CARTESIAN_POINT('Ctrl Pts',(-2.66824761341794,-0.656615204093706,
7.50215815450137));
#398286=CARTESIAN_POINT('Ctrl Pts',(-2.66981365703397,-0.659306964089347,
7.49877163671531));
#398287=CARTESIAN_POINT('Ctrl Pts',(-2.66899810433398,-0.662659395652838,
7.4948158853317));
#398288=CARTESIAN_POINT('Ctrl Pts',(-2.66850726965803,-0.649186354833451,
7.50366171572174));
#398289=CARTESIAN_POINT('Ctrl Pts',(-2.67206521266994,-0.650051920418041,
7.50000045605858));
#398290=CARTESIAN_POINT('Ctrl Pts',(-2.67206521266991,-0.650051920418163,
7.49482233047317));
#398291=CARTESIAN_POINT('Origin',(-2.65538477227091,-0.665460713484864,
7.51860402984325));
#398292=CARTESIAN_POINT('Origin',(-2.65538477227091,-0.665460713484864,
9.));
#398293=CARTESIAN_POINT('Origin',(-2.65538477227091,-0.665460713484863,
8.75721825406948));
#398294=CARTESIAN_POINT('Ctrl Pts',(-2.65112941937648,-0.645039239553588,
8.78942910404912));
#398295=CARTESIAN_POINT('Ctrl Pts',(-2.65532178526109,-0.648710274420128,
8.79672699501691));
#398296=CARTESIAN_POINT('Ctrl Pts',(-2.65077470762198,-0.656391262047123,
8.79893251111267));
#398297=CARTESIAN_POINT('Ctrl Pts',(-2.65937452780626,-0.652312038582979,
8.78111911759582));
#398298=CARTESIAN_POINT('Ctrl Pts',(-2.6643397222864,-0.656669693215895,
8.78644465894812));
#398299=CARTESIAN_POINT('Ctrl Pts',(-2.66180227631762,-0.664368841203243,
8.78817647674132));
#398300=CARTESIAN_POINT('Ctrl Pts',(-2.66451307602302,-0.656844620434572,
8.7678092393203));
#398301=CARTESIAN_POINT('Ctrl Pts',(-2.67037091713225,-0.661992477688777,
8.76988516158375));
#398302=CARTESIAN_POINT('Ctrl Pts',(-2.66868335772546,-0.669360552311429,
8.77093053738833));
#398303=CARTESIAN_POINT('Ctrl Pts',(-2.66351112944559,-0.655960829007565,
8.75371302330492));
#398304=CARTESIAN_POINT('Ctrl Pts',(-2.66922570397851,-0.660981769086419,
8.75300828287558));
#398305=CARTESIAN_POINT('Ctrl Pts',(-2.66734099870958,-0.66838733627493,
8.75267964240738));
#398306=CARTESIAN_POINT('Origin',(-2.6448686608445,-0.656184713158512,8.78727029226991));
#398307=CARTESIAN_POINT('Ctrl Pts',(-2.5995223305943,-0.599517869856899,
8.85049129520029));
#398308=CARTESIAN_POINT('Ctrl Pts',(-2.60390169908879,-0.603380801879671,
8.85711686593484));
#398309=CARTESIAN_POINT('Ctrl Pts',(-2.59985800069652,-0.610914012710802,
8.85933012996512));
#398310=CARTESIAN_POINT('Ctrl Pts',(-2.61742004498719,-0.615304998560432,
8.82945683644723));
#398311=CARTESIAN_POINT('Ctrl Pts',(-2.62183576488801,-0.619199995254551,
8.83607469902389));
#398312=CARTESIAN_POINT('Ctrl Pts',(-2.61774715137788,-0.626737586518493,
8.83829567148519));
#398313=CARTESIAN_POINT('Ctrl Pts',(-2.63529108139348,-0.631068595275541,
8.80838214965001));
#398314=CARTESIAN_POINT('Ctrl Pts',(-2.63972422778671,-0.634978963445188,
8.81501364461993));
#398315=CARTESIAN_POINT('Ctrl Pts',(-2.6356096080769,-0.642536656032115,
8.81722098428721));
#398316=CARTESIAN_POINT('Ctrl Pts',(-2.65313746692184,-0.646810448064364,
8.78727029226991));
#398317=CARTESIAN_POINT('Ctrl Pts',(-2.65757134967522,-0.650721465758992,
8.79393457792714));
#398318=CARTESIAN_POINT('Ctrl Pts',(-2.65344741704445,-0.658313079212999,
8.79610912703474));
#398319=CARTESIAN_POINT('Origin',(-2.59125352451696,-0.608892134951047,
8.85049129520029));
#398320=CARTESIAN_POINT('Ctrl Pts',(-2.60220974632391,-0.587743532225626,
8.85049129520029));
#398321=CARTESIAN_POINT('Ctrl Pts',(-2.60783148438851,-0.586163287511648,
8.85711686593484));
#398322=CARTESIAN_POINT('Ctrl Pts',(-2.60745677570886,-0.577621604099153,
8.85933012996512));
#398323=CARTESIAN_POINT('Ctrl Pts',(-2.5972362758088,-0.589141551913008,
8.86332496987232));
#398324=CARTESIAN_POINT('Ctrl Pts',(-2.59853778293458,-0.584707820574939,
8.86648636486737));
#398325=CARTESIAN_POINT('Ctrl Pts',(-2.59354792537494,-0.581549114601394,
8.87206031107457));
#398326=CARTESIAN_POINT('Ctrl Pts',(-2.59562163897866,-0.596077166803026,
8.86341338519876));
#398327=CARTESIAN_POINT('Ctrl Pts',(-2.59483919973077,-0.600644579578075,
8.86654584966058));
#398328=CARTESIAN_POINT('Ctrl Pts',(-2.58894560269753,-0.60126881254509,
8.87215952290715));
#398329=CARTESIAN_POINT('Ctrl Pts',(-2.5995223305943,-0.599517869856899,
8.85049129520029));
#398330=CARTESIAN_POINT('Ctrl Pts',(-2.60390169908879,-0.603380801879671,
8.85711686593484));
#398331=CARTESIAN_POINT('Ctrl Pts',(-2.59985800069652,-0.610914012710802,
8.85933012996512));
#398332=CARTESIAN_POINT('Origin',(-2.59882715066403,-0.575709910717461,
8.85049129520029));
#398333=CARTESIAN_POINT('Ctrl Pts',(-2.67103479566853,-0.568397127400952,
8.78727029226991));
#398334=CARTESIAN_POINT('Ctrl Pts',(-2.67672651297436,-0.566797211844121,
8.79393457792714));
#398335=CARTESIAN_POINT('Ctrl Pts',(-2.67630485569206,-0.558168097155203,
8.79610912703474));
#398336=CARTESIAN_POINT('Ctrl Pts',(-2.64812562395424,-0.574836790204001,
8.80838214965003));
#398337=CARTESIAN_POINT('Ctrl Pts',(-2.65381639600413,-0.573237140354252,
8.81501364461989));
#398338=CARTESIAN_POINT('Ctrl Pts',(-2.65338841166108,-0.564642628035495,
8.81722098428721));
#398339=CARTESIAN_POINT('Ctrl Pts',(-2.62518480823033,-0.581285347992617,
8.82945683644723));
#398340=CARTESIAN_POINT('Ctrl Pts',(-2.63085321011983,-0.57969198629208,
8.8360746990239));
#398341=CARTESIAN_POINT('Ctrl Pts',(-2.63043993491585,-0.571126868306709,
8.8382956714852));
#398342=CARTESIAN_POINT('Ctrl Pts',(-2.60220974632391,-0.587743532225626,
8.85049129520029));
#398343=CARTESIAN_POINT('Ctrl Pts',(-2.60783148438851,-0.586163287511648,
8.85711686593484));
#398344=CARTESIAN_POINT('Ctrl Pts',(-2.60745677570886,-0.577621604099153,
8.85933012996512));
#398345=CARTESIAN_POINT('Origin',(-2.66765220000865,-0.556363505892786,
8.78727029226991));
#398346=CARTESIAN_POINT('Ctrl Pts',(-2.68435593267242,-0.564652597894868,
8.75374538247847));
#398347=CARTESIAN_POINT('Ctrl Pts',(-2.69167492525667,-0.5626088939194,
8.75304829418601));
#398348=CARTESIAN_POINT('Ctrl Pts',(-2.69319395121606,-0.55512803812987,
8.75272238421917));
#398349=CARTESIAN_POINT('Ctrl Pts',(-2.68562666750749,-0.564295400620303,
8.76769408445023));
#398350=CARTESIAN_POINT('Ctrl Pts',(-2.69312965281887,-0.56219960330441,
8.76974318093973));
#398351=CARTESIAN_POINT('Ctrl Pts',(-2.69480757528628,-0.554837339150378,
8.7707786988043));
#398352=CARTESIAN_POINT('Ctrl Pts',(-2.6791136046367,-0.566126190382126,
8.78108014887986));
#398353=CARTESIAN_POINT('Ctrl Pts',(-2.6854731365548,-0.56435373697426,
8.78639403366319));
#398354=CARTESIAN_POINT('Ctrl Pts',(-2.68654558210626,-0.556330524633315,
8.78812224174741));
#398355=CARTESIAN_POINT('Ctrl Pts',(-2.66844013235527,-0.569126450616946,
8.78944554828686));
#398356=CARTESIAN_POINT('Ctrl Pts',(-2.67380121292356,-0.56763808481604,
8.79673892988687));
#398357=CARTESIAN_POINT('Ctrl Pts',(-2.67304049616502,-0.558754118115857,
8.79894799272499));
#398358=CARTESIAN_POINT('Origin',(-2.68115159472089,-0.552568888126756,
8.75721825406948));
#398359=CARTESIAN_POINT('Origin',(-2.68115159472089,-0.552568888126756,
9.));
#398360=CARTESIAN_POINT('Origin',(-2.68115159472089,-0.552568888126756,
7.51860402984325));
#398361=CARTESIAN_POINT('Ctrl Pts',(-2.68591314580246,-0.572925167585766,
7.50366195182966));
#398362=CARTESIAN_POINT('Ctrl Pts',(-2.6894945274723,-0.573689102821856,
7.50000065167735));
#398363=CARTESIAN_POINT('Ctrl Pts',(-2.68949452747233,-0.573689102821742,
7.49482233047108));
#398364=CARTESIAN_POINT('Ctrl Pts',(-2.68890430944023,-0.566112918346439,
7.50215800491337));
#398365=CARTESIAN_POINT('Ctrl Pts',(-2.69148329915019,-0.564365489020161,
7.49877273257265));
#398366=CARTESIAN_POINT('Ctrl Pts',(-2.69220348433874,-0.560989324088742,
7.49481816995647));
#398367=CARTESIAN_POINT('Ctrl Pts',(-2.68724770526621,-0.563840105342091,
7.51043025814043));
#398368=CARTESIAN_POINT('Ctrl Pts',(-2.69222164317036,-0.560781887116949,
7.51006209594516));
#398369=CARTESIAN_POINT('Ctrl Pts',(-2.69339480712794,-0.555089553984483,
7.50731281821701));
#398370=CARTESIAN_POINT('Ctrl Pts',(-2.68453273533963,-0.564602918545373,
7.51860402984326));
#398371=CARTESIAN_POINT('Ctrl Pts',(-2.69185835200809,-0.562544677107268,
7.51860402984327));
#398372=CARTESIAN_POINT('Ctrl Pts',(-2.69339429606665,-0.555092033734636,
7.51860402984327));
#398373=CARTESIAN_POINT('Origin',(0.,0.,7.5));
#398374=CARTESIAN_POINT('Origin',(-2.55920636991203,-0.753260100986301,
7.5));
#398375=CARTESIAN_POINT('',(-2.55920636991203,-0.753260100986301,7.59394543036555));
#398376=CARTESIAN_POINT('',(-2.55920636991203,-0.753260100986301,8.85049129520029));
#398377=CARTESIAN_POINT('',(-2.55920636991203,-0.753260100986301,7.5));
#398378=CARTESIAN_POINT('',(-2.62912953922426,-0.738363081476928,8.78727029226991));
#398379=CARTESIAN_POINT('Ctrl Pts',(-2.55920636991203,-0.753260100986301,
8.85049129520029));
#398380=CARTESIAN_POINT('Ctrl Pts',(-2.58254797304887,-0.748287209729658,
8.82945686509571));
#398381=CARTESIAN_POINT('Ctrl Pts',(-2.60585487607022,-0.743321711277182,
8.80838212259895));
#398382=CARTESIAN_POINT('Ctrl Pts',(-2.62912953922426,-0.738363081476928,
8.78727029226991));
#398383=CARTESIAN_POINT('',(-2.64284431997727,-0.735441169348889,8.75721825406948));
#398384=CARTESIAN_POINT('Origin',(-2.60157182905119,-0.744234413933245,
8.75937679713137));
#398385=CARTESIAN_POINT('',(-2.64284431997727,-0.735441169348889,7.51860402984325));
#398386=CARTESIAN_POINT('',(-2.64284431997727,-0.735441169348889,7.5));
#398387=CARTESIAN_POINT('Ctrl Pts',(-2.64284431997727,-0.735441169348889,
7.51860402984325));
#398388=CARTESIAN_POINT('Ctrl Pts',(-2.63207349274766,-0.73773587688217,
7.52834476460825));
#398389=CARTESIAN_POINT('Ctrl Pts',(-2.62129567325243,-0.740032074106476,
7.53807742314407));
#398390=CARTESIAN_POINT('Ctrl Pts',(-2.61051062671697,-0.742329811040153,
7.54780169004674));
#398391=CARTESIAN_POINT('Ctrl Pts',(-2.59342769588683,-0.745969302161013,
7.5632044032688));
#398392=CARTESIAN_POINT('Ctrl Pts',(-2.57632661162329,-0.749612660841833,
7.57858609112103));
#398393=CARTESIAN_POINT('Ctrl Pts',(-2.55920636991203,-0.753260100986301,
7.59394543036555));
#398394=CARTESIAN_POINT('Origin',(-2.7499249409731,-0.959591483074788,7.5));
#398395=CARTESIAN_POINT('',(-2.61614521332082,-0.825399319134631,8.75721825406948));
#398396=CARTESIAN_POINT('',(-2.60624502375464,-0.815468607773367,8.78727029226991));
#398397=CARTESIAN_POINT('Origin',(-2.58111465004912,-0.790260758367852,
8.75658640621046));
#398398=CARTESIAN_POINT('',(-2.5557700913641,-0.764838063661141,8.85049129520029));
#398399=CARTESIAN_POINT('Ctrl Pts',(-2.60624502375464,-0.815468607773367,
8.78727029226991));
#398400=CARTESIAN_POINT('Ctrl Pts',(-2.5894439110381,-0.798615698056765,
8.80838212259896));
#398401=CARTESIAN_POINT('Ctrl Pts',(-2.57261952556177,-0.781739443831607,
8.82945686509571));
#398402=CARTESIAN_POINT('Ctrl Pts',(-2.5557700913641,-0.764838063661142,
8.85049129520029));
#398403=CARTESIAN_POINT('',(-2.5557700913641,-0.764838063661141,7.59394543036555));
#398404=CARTESIAN_POINT('',(-2.5557700913641,-0.764838063661141,7.5));
#398405=CARTESIAN_POINT('',(-2.61614521332082,-0.825399319134631,7.51860402984325));
#398406=CARTESIAN_POINT('Ctrl Pts',(-2.5557700913641,-0.764838063661141,
7.59394543036555));
#398407=CARTESIAN_POINT('Ctrl Pts',(-2.5681285563963,-0.777234629230179,
7.57858609112103));
#398408=CARTESIAN_POINT('Ctrl Pts',(-2.58047319238016,-0.789617323116581,
7.56320440326857));
#398409=CARTESIAN_POINT('Ctrl Pts',(-2.59280472407651,-0.801986872315641,
7.54780169004651));
#398410=CARTESIAN_POINT('Ctrl Pts',(-2.60059004759747,-0.809796197604203,
7.53807742314383));
#398411=CARTESIAN_POINT('Ctrl Pts',(-2.60837015418731,-0.81760028987812,
7.52834476460825));
#398412=CARTESIAN_POINT('Ctrl Pts',(-2.61614521332082,-0.825399319134632,
7.51860402984325));
#398413=CARTESIAN_POINT('',(-2.61614521332082,-0.825399319134631,7.5));
#398414=CARTESIAN_POINT('Origin',(-2.56063892684944,-0.759984192420916,
7.5));
#398415=CARTESIAN_POINT('Ctrl Pts',(-2.5557700913641,-0.764838063661142,
8.85049129520029));
#398416=CARTESIAN_POINT('Ctrl Pts',(-2.55563336292572,-0.764700913695738,
8.85097269580138));
#398417=CARTESIAN_POINT('Ctrl Pts',(-2.55550431648359,-0.76455955552543,
8.85143669361005));
#398418=CARTESIAN_POINT('Ctrl Pts',(-2.5553776555582,-0.76440689060847,
8.8519052845931));
#398419=CARTESIAN_POINT('Ctrl Pts',(-2.55512991482068,-0.764108287712554,
8.85282181883899));
#398420=CARTESIAN_POINT('Ctrl Pts',(-2.55489782482715,-0.76377398445858,
8.85372622499635));
#398421=CARTESIAN_POINT('Ctrl Pts',(-2.55469040933054,-0.763389941933495,
8.8546225773507));
#398422=CARTESIAN_POINT('Ctrl Pts',(-2.55451822035196,-0.763071123469069,
8.85536669723986));
#398423=CARTESIAN_POINT('Ctrl Pts',(-2.55436296930131,-0.762717968360507,
8.85610498449051));
#398424=CARTESIAN_POINT('Ctrl Pts',(-2.55423713170265,-0.762319193931662,
8.85681338218371));
#398425=CARTESIAN_POINT('Ctrl Pts',(-2.55412293388424,-0.761957305511198,
8.85745625420284));
#398426=CARTESIAN_POINT('Ctrl Pts',(-2.55403095653985,-0.761553487472278,
8.85808743050666));
#398427=CARTESIAN_POINT('Ctrl Pts',(-2.55398360973458,-0.761089973691792,
8.85866804508411));
#398428=CARTESIAN_POINT('Ctrl Pts',(-2.55396176494498,-0.760876118481226,
8.85893592806396));
#398429=CARTESIAN_POINT('Ctrl Pts',(-2.55394962718964,-0.76064942901192,
8.85919241173848));
#398430=CARTESIAN_POINT('Ctrl Pts',(-2.55395086090131,-0.76040752328701,
8.85943017985534));
#398431=CARTESIAN_POINT('Ctrl Pts',(-2.55395252677728,-0.76008087894662,
8.8597512372));
#398432=CARTESIAN_POINT('Ctrl Pts',(-2.55397925578498,-0.759718180134259,
8.86004599534706));
#398433=CARTESIAN_POINT('Ctrl Pts',(-2.55404111371133,-0.759324550001956,
8.86026130871721));
#398434=CARTESIAN_POINT('Ctrl Pts',(-2.55406376164213,-0.759180430912912,
8.86034014101235));
#398435=CARTESIAN_POINT('Ctrl Pts',(-2.5540914466204,-0.759029998745715,
8.86040910639692));
#398436=CARTESIAN_POINT('Ctrl Pts',(-2.55412374520742,-0.758877412823752,
8.86046313645506));
#398437=CARTESIAN_POINT('Ctrl Pts',(-2.55417414688197,-0.758639303770424,
8.86054744990829));
#398438=CARTESIAN_POINT('Ctrl Pts',(-2.55423730297958,-0.758389480825089,
8.86059655985669));
#398439=CARTESIAN_POINT('Ctrl Pts',(-2.55430887908532,-0.758143894092029,
8.86059725258816));
#398440=CARTESIAN_POINT('Ctrl Pts',(-2.55438062056046,-0.757897739955503,
8.86059794692011));
#398441=CARTESIAN_POINT('Ctrl Pts',(-2.5544641672651,-0.757653855137121,
8.86056369958366));
#398442=CARTESIAN_POINT('Ctrl Pts',(-2.55455140251595,-0.757424321695584,
8.86048590497774));
#398443=CARTESIAN_POINT('Ctrl Pts',(-2.55457416831912,-0.757364420301377,
8.86046560290182));
#398444=CARTESIAN_POINT('Ctrl Pts',(-2.5545975661727,-0.757304749210599,
8.86044257503091));
#398445=CARTESIAN_POINT('Ctrl Pts',(-2.55462084250291,-0.757247140326069,
8.86041778462583));
#398446=CARTESIAN_POINT('Ctrl Pts',(-2.55477746332169,-0.756859504019852,
8.86025097596201));
#398447=CARTESIAN_POINT('Ctrl Pts',(-2.55494990617791,-0.756513345250565,
8.8599848982295));
#398448=CARTESIAN_POINT('Ctrl Pts',(-2.55512555432353,-0.756214989631096,
8.85968173251461));
#398449=CARTESIAN_POINT('Ctrl Pts',(-2.55521846212913,-0.756057176602136,
8.85952137522076));
#398450=CARTESIAN_POINT('Ctrl Pts',(-2.55531389301721,-0.755909599116461,
8.85934740853961));
#398451=CARTESIAN_POINT('Ctrl Pts',(-2.55540919580188,-0.755773494207119,
8.8591675900182));
#398452=CARTESIAN_POINT('Ctrl Pts',(-2.55579188601969,-0.755226962250188,
8.85844552518695));
#398453=CARTESIAN_POINT('Ctrl Pts',(-2.55619166074993,-0.754832794368564,
8.85759444184125));
#398454=CARTESIAN_POINT('Ctrl Pts',(-2.55654648248264,-0.754540688576929,
8.8568349891514));
#398455=CARTESIAN_POINT('Ctrl Pts',(-2.556583613632,-0.754510120483775,
8.85675551444999));
#398456=CARTESIAN_POINT('Ctrl Pts',(-2.55662026192593,-0.754480687682163,
8.85667699793652));
#398457=CARTESIAN_POINT('Ctrl Pts',(-2.55665636186478,-0.754452344408663,
8.85659965593547));
#398458=CARTESIAN_POINT('Ctrl Pts',(-2.55714364068136,-0.7540697654567,
8.85555568965886));
#398459=CARTESIAN_POINT('Ctrl Pts',(-2.55766719778435,-0.753772456084101,
8.85434650606346));
#398460=CARTESIAN_POINT('Ctrl Pts',(-2.55822655250307,-0.753553542379831,
8.85297329937117));
#398461=CARTESIAN_POINT('Ctrl Pts',(-2.55854115545037,-0.753430416759787,
8.85220095427747));
#398462=CARTESIAN_POINT('Ctrl Pts',(-2.55886732590039,-0.753332333771308,
8.85137579139183));
#398463=CARTESIAN_POINT('Ctrl Pts',(-2.55920636991203,-0.753260100986301,
8.85049129520029));
#398464=CARTESIAN_POINT('Origin',(-2.56063892684944,-0.759984192420916,
7.59394543036555));
#398465=CARTESIAN_POINT('Ctrl Pts',(-2.55537312258256,-0.764439871044471,
7.59443877723642));
#398466=CARTESIAN_POINT('Ctrl Pts',(-2.55128472608583,-0.760338870223424,
7.58783886950016));
#398467=CARTESIAN_POINT('Ctrl Pts',(-2.55574715922245,-0.753116275673134,
7.58559994247159));
#398468=CARTESIAN_POINT('Ctrl Pts',(-2.57769155910977,-0.786827114208337,
7.56670252222139));
#398469=CARTESIAN_POINT('Ctrl Pts',(-2.57360907150671,-0.78273204049773,
7.56004874999028));
#398470=CARTESIAN_POINT('Ctrl Pts',(-2.57807976992149,-0.775455419514081,
7.55786368756704));
#398471=CARTESIAN_POINT('Ctrl Pts',(-2.59996831818662,-0.809172551432327,
7.53888913333561));
#398472=CARTESIAN_POINT('Ctrl Pts',(-2.59586156815991,-0.80505314049819,
7.53222002137285));
#398473=CARTESIAN_POINT('Ctrl Pts',(-2.60037064305195,-0.797754463334659,
7.53005029815327));
#398474=CARTESIAN_POINT('Ctrl Pts',(-2.62220239177471,-0.831475171570302,
7.51101258149734));
#398475=CARTESIAN_POINT('Ctrl Pts',(-2.61804586047546,-0.827305825890497,
7.5043616886572));
#398476=CARTESIAN_POINT('Ctrl Pts',(-2.62261873572381,-0.820012246967386,
7.50217374673251));
#398477=CARTESIAN_POINT('',(-2.62143154819292,-0.818824543767677,7.50366116523517));
#398478=CARTESIAN_POINT('Ctrl Pts',(-2.61614521332082,-0.825399319134632,
7.51860402984325));
#398479=CARTESIAN_POINT('Ctrl Pts',(-2.61645699862685,-0.825712065659352,
7.51734760759493));
#398480=CARTESIAN_POINT('Ctrl Pts',(-2.61678087653058,-0.825952671069635,
7.51608817408572));
#398481=CARTESIAN_POINT('Ctrl Pts',(-2.61712406542065,-0.826109862572535,
7.51481005913119));
#398482=CARTESIAN_POINT('Ctrl Pts',(-2.61743493411805,-0.826252250392075,
7.51365231206383));
#398483=CARTESIAN_POINT('Ctrl Pts',(-2.61776198182467,-0.826326623841268,
7.51247773061042));
#398484=CARTESIAN_POINT('Ctrl Pts',(-2.6181077374604,-0.826295690232693,
7.51129758471022));
#398485=CARTESIAN_POINT('Ctrl Pts',(-2.61853747222882,-0.826257243289985,
7.50983079813402));
#398486=CARTESIAN_POINT('Ctrl Pts',(-2.61898123088402,-0.82604437589818,
7.50839324291155));
#398487=CARTESIAN_POINT('Ctrl Pts',(-2.61940659658241,-0.825581204338862,
7.50715379678855));
#398488=CARTESIAN_POINT('Ctrl Pts',(-2.61960310327845,-0.825367232424425,
7.50658120839351));
#398489=CARTESIAN_POINT('Ctrl Pts',(-2.6198166215314,-0.825062996159276,
7.50598221009429));
#398490=CARTESIAN_POINT('Ctrl Pts',(-2.6200234511659,-0.82466266898229,
7.50545747549612));
#398491=CARTESIAN_POINT('Ctrl Pts',(-2.62013382186085,-0.824449042009365,
7.50517746087247));
#398492=CARTESIAN_POINT('Ctrl Pts',(-2.62024366461123,-0.824205828466795,
7.50491486231392));
#398493=CARTESIAN_POINT('Ctrl Pts',(-2.62034855042521,-0.823938782502916,
7.50468370960993));
#398494=CARTESIAN_POINT('Ctrl Pts',(-2.62050538780146,-0.823539464552042,
7.50433806340447));
#398495=CARTESIAN_POINT('Ctrl Pts',(-2.62065532643771,-0.823074680524712,
7.50405484070984));
#398496=CARTESIAN_POINT('Ctrl Pts',(-2.62078758644981,-0.822575512814655,
7.50385766036131));
#398497=CARTESIAN_POINT('Ctrl Pts',(-2.62080172960232,-0.822522134586887,
7.50383657498791));
#398498=CARTESIAN_POINT('Ctrl Pts',(-2.62081567828759,-0.822468390482957,
7.50381643264937));
#398499=CARTESIAN_POINT('Ctrl Pts',(-2.62082942521804,-0.822414338256744,
7.50379723213559));
#398500=CARTESIAN_POINT('Ctrl Pts',(-2.62092119047576,-0.822053521965059,
7.50366906242519));
#398501=CARTESIAN_POINT('Ctrl Pts',(-2.62100526478186,-0.821670949923754,
7.50358235568538));
#398502=CARTESIAN_POINT('Ctrl Pts',(-2.62107743801799,-0.82130024959084,
7.5035341175365));
#398503=CARTESIAN_POINT('Ctrl Pts',(-2.62118565361712,-0.820744426396813,
7.50346178989177));
#398504=CARTESIAN_POINT('Ctrl Pts',(-2.62127843601657,-0.820141885920964,
7.50346967198527));
#398505=CARTESIAN_POINT('Ctrl Pts',(-2.62135131886643,-0.819547575210604,
7.50354272648693));
#398506=CARTESIAN_POINT('Ctrl Pts',(-2.62138129709116,-0.819303122913928,
7.50357277531559));
#398507=CARTESIAN_POINT('Ctrl Pts',(-2.62140800952761,-0.819060405024619,
7.50361331098761));
#398508=CARTESIAN_POINT('Ctrl Pts',(-2.62143154819427,-0.8188245437681,
7.50366116523659));
#398509=CARTESIAN_POINT('',(-2.56344583459816,-0.760817267906771,7.57603338622103));
#398510=CARTESIAN_POINT('Origin',(-2.57191833523299,-0.763328885433893,
7.58486873427629));
#398511=CARTESIAN_POINT('Ctrl Pts',(-2.62143154822949,-0.818824543811846,
7.50366116529968));
#398512=CARTESIAN_POINT('Ctrl Pts',(-2.60213510841253,-0.799519746242561,
7.52783573079709));
#398513=CARTESIAN_POINT('Ctrl Pts',(-2.58280746249009,-0.780184887893086,
7.55196141284069));
#398514=CARTESIAN_POINT('Ctrl Pts',(-2.56344583519718,-0.760817269006234,
7.57603338728831));
#398515=CARTESIAN_POINT('Ctrl Pts',(-2.55662067806349,-0.765442247231706,
7.59639677331371));
#398516=CARTESIAN_POINT('Ctrl Pts',(-2.54113756247318,-0.754196289838708,
7.59974925422224));
#398517=CARTESIAN_POINT('Ctrl Pts',(-2.5602488397315,-0.753217766653662,
7.59639677331371));
#398518=CARTESIAN_POINT('Ctrl Pts',(-2.55313724428124,-0.76368702839398,
7.58707626057424));
#398519=CARTESIAN_POINT('Ctrl Pts',(-2.55101612578582,-0.757128195576305,
7.58811717123965));
#398520=CARTESIAN_POINT('Ctrl Pts',(-2.55637188217917,-0.752788459978733,
7.58707626057423));
#398521=CARTESIAN_POINT('Ctrl Pts',(-2.55888304972318,-0.761709314540856,
7.58015376756929));
#398522=CARTESIAN_POINT('Ctrl Pts',(-2.55764184525409,-0.759094674335462,
7.5820876076604));
#398523=CARTESIAN_POINT('Ctrl Pts',(-2.56010846144153,-0.757580495838117,
7.58015376756929));
#398524=CARTESIAN_POINT('Ctrl Pts',(-2.56344583380473,-0.760817267671499,
7.57603338509286));
#398525=CARTESIAN_POINT('Ctrl Pts',(-2.56344583380473,-0.760817267671499,
7.57603338509286));
#398526=CARTESIAN_POINT('Ctrl Pts',(-2.56344583380473,-0.760817267671499,
7.57603338509286));
#398527=CARTESIAN_POINT('Origin',(-2.57191671161821,-0.763334355930412,
7.58486873427621));
#398528=CARTESIAN_POINT('Ctrl Pts',(-2.65126187924782,-0.733647821794593,
7.51098857897448));
#398529=CARTESIAN_POINT('Ctrl Pts',(-2.64550378996544,-0.734874573516806,
7.50433767179956));
#398530=CARTESIAN_POINT('Ctrl Pts',(-2.64535737577417,-0.743481931646165,
7.50214974420965));
#398531=CARTESIAN_POINT('Ctrl Pts',(-2.62045204982553,-0.740211806729756,
7.53887321589168));
#398532=CARTESIAN_POINT('Ctrl Pts',(-2.61476295267151,-0.741423859789234,
7.53220407452063));
#398533=CARTESIAN_POINT('Ctrl Pts',(-2.61456026023066,-0.750000679461849,
7.53003438070911));
#398534=CARTESIAN_POINT('Ctrl Pts',(-2.58958305416547,-0.746788396937349,
7.56669465659237));
#398535=CARTESIAN_POINT('Ctrl Pts',(-2.58392757851793,-0.747993286988579,
7.56004085833303));
#398536=CARTESIAN_POINT('Ctrl Pts',(-2.58370474861186,-0.75653067516994,
7.5578558219379));
#398537=CARTESIAN_POINT('Ctrl Pts',(-2.55865628834872,-0.753377294984527,
7.59443891967696));
#398538=CARTESIAN_POINT('Ctrl Pts',(-2.55299261296563,-0.754583931976337,
7.58783901202978));
#398539=CARTESIAN_POINT('Ctrl Pts',(-2.55279234759891,-0.763071515364511,
7.58560008491213));
#398540=CARTESIAN_POINT('',(-2.64368796492175,-0.743835290548484,7.50366116523517));
#398541=CARTESIAN_POINT('Ctrl Pts',(-2.64368796492211,-0.743835290548585,
7.50366116523554));
#398542=CARTESIAN_POINT('Ctrl Pts',(-2.64403606905884,-0.743162266754978,
7.50350835821027));
#398543=CARTESIAN_POINT('Ctrl Pts',(-2.64433416512129,-0.742532269335384,
7.50345484956));
#398544=CARTESIAN_POINT('Ctrl Pts',(-2.64459165855155,-0.741926824793127,
7.50349758195598));
#398545=CARTESIAN_POINT('Ctrl Pts',(-2.64472377177749,-0.74161618684201,
7.50351950684424));
#398546=CARTESIAN_POINT('Ctrl Pts',(-2.6448583372899,-0.74128144525031,
7.50357029184312));
#398547=CARTESIAN_POINT('Ctrl Pts',(-2.6449792244816,-0.740955090937072,
7.50365515313924));
#398548=CARTESIAN_POINT('Ctrl Pts',(-2.64516519793449,-0.7404530258494,
7.50378570417639));
#398549=CARTESIAN_POINT('Ctrl Pts',(-2.64532458362199,-0.739956193803948,
7.50400001621911));
#398550=CARTESIAN_POINT('Ctrl Pts',(-2.64544308808559,-0.739501717390452,
7.50428903009635));
#398551=CARTESIAN_POINT('Ctrl Pts',(-2.64545624116934,-0.739451274005085,
7.50432110841318));
#398552=CARTESIAN_POINT('Ctrl Pts',(-2.64546891357409,-0.739401332602651,
7.50435406373354));
#398553=CARTESIAN_POINT('Ctrl Pts',(-2.64548110249556,-0.739351929091587,
7.50438785222352));
#398554=CARTESIAN_POINT('Ctrl Pts',(-2.64555552171985,-0.739050296910203,
7.50459414719561));
#398555=CARTESIAN_POINT('Ctrl Pts',(-2.64561260228404,-0.738763789814949,
7.50483629897752));
#398556=CARTESIAN_POINT('Ctrl Pts',(-2.64565144811457,-0.738503640946549,
7.5050991045531));
#398557=CARTESIAN_POINT('Ctrl Pts',(-2.64573714591841,-0.737929726413378,
7.50567888004914));
#398558=CARTESIAN_POINT('Ctrl Pts',(-2.64573798903582,-0.737461555509731,
7.50637912803144));
#398559=CARTESIAN_POINT('Ctrl Pts',(-2.645683829865,-0.737091112458729,
7.50710440483569));
#398560=CARTESIAN_POINT('Ctrl Pts',(-2.6456705489611,-0.737000272468299,
7.50728225710685));
#398561=CARTESIAN_POINT('Ctrl Pts',(-2.64565384064822,-0.736913479663673,
7.50746498566954));
#398562=CARTESIAN_POINT('Ctrl Pts',(-2.64563450403444,-0.736832681318231,
7.50764697238949));
#398563=CARTESIAN_POINT('Ctrl Pts',(-2.64553055572032,-0.736398331649443,
7.50862528291181));
#398564=CARTESIAN_POINT('Ctrl Pts',(-2.64534524283225,-0.736096819786121,
7.5096585683742));
#398565=CARTESIAN_POINT('Ctrl Pts',(-2.64512364214823,-0.73587953009369,
7.510679598732));
#398566=CARTESIAN_POINT('Ctrl Pts',(-2.6450016950123,-0.735759955301867,
7.51124147302577));
#398567=CARTESIAN_POINT('Ctrl Pts',(-2.64486842488808,-0.73566616662784,
7.51180065547252));
#398568=CARTESIAN_POINT('Ctrl Pts',(-2.64472951425973,-0.735592069739056,
7.512351757165));
#398569=CARTESIAN_POINT('Ctrl Pts',(-2.64424952270334,-0.735336035471616,
7.51425603304536));
#398570=CARTESIAN_POINT('Ctrl Pts',(-2.64364210055535,-0.735289940333083,
7.51626900505181));
#398571=CARTESIAN_POINT('Ctrl Pts',(-2.64295636119803,-0.735418705226013,
7.51827788969245));
#398572=CARTESIAN_POINT('Ctrl Pts',(-2.64291924768814,-0.73542567422535,
7.51838661432546));
#398573=CARTESIAN_POINT('Ctrl Pts',(-2.64288189864374,-0.735433163274031,
7.51849533314857));
#398574=CARTESIAN_POINT('Ctrl Pts',(-2.64284431997727,-0.735441169348884,
7.51860402984325));
#398575=CARTESIAN_POINT('Ctrl Pts',(-2.5634458357012,-0.760817267312222,
7.57603338728985));
#398576=CARTESIAN_POINT('Ctrl Pts',(-2.59023829728888,-0.755147939734358,
7.55196141284922));
#398577=CARTESIAN_POINT('Ctrl Pts',(-2.61698440749374,-0.749487530346323,
7.52783573083105));
#398578=CARTESIAN_POINT('Ctrl Pts',(-2.64368796497828,-0.743835290530964,
7.50366116530176));
#398579=CARTESIAN_POINT('Origin',(-8.85789032694961E-16,-2.62897535302355E-16,
7.49482233047033));
#398580=CARTESIAN_POINT('Origin',(-2.61299471585144,-0.816189233531323,
7.49482233047033));
#398581=CARTESIAN_POINT('Origin',(0.,0.,7.50366116523517));
#398582=CARTESIAN_POINT('Origin',(-2.63517950238395,-0.741441326212334,
7.49482233047033));
#398583=CARTESIAN_POINT('Ctrl Pts',(-2.61614446651996,-0.825398570094808,
7.51860402984325));
#398584=CARTESIAN_POINT('Ctrl Pts',(-2.62151698305456,-0.83078673788318,
7.51860402984325));
#398585=CARTESIAN_POINT('Ctrl Pts',(-2.61919823167326,-0.838033784044334,
7.51860402984325));
#398586=CARTESIAN_POINT('Ctrl Pts',(-2.61813931767337,-0.827399234462638,
7.51041458714367));
#398587=CARTESIAN_POINT('Ctrl Pts',(-2.62096763486516,-0.832503643108394,
7.51004642900444));
#398588=CARTESIAN_POINT('Ctrl Pts',(-2.61919759218916,-0.838035782693619,
7.50729136483012));
#398589=CARTESIAN_POINT('Ctrl Pts',(-2.62069593195856,-0.826221329289833,
7.50215815450137));
#398590=CARTESIAN_POINT('Ctrl Pts',(-2.62208629631497,-0.829007895534854,
7.49877163671527));
#398591=CARTESIAN_POINT('Ctrl Pts',(-2.62105762822771,-0.832301186527254,
7.49481588533168));
#398592=CARTESIAN_POINT('Ctrl Pts',(-2.62143102271336,-0.81882437962955,
7.50366171572174));
#398593=CARTESIAN_POINT('Ctrl Pts',(-2.62492619857234,-0.819916125008266,
7.50000045605858));
#398594=CARTESIAN_POINT('Ctrl Pts',(-2.6249261985723,-0.819916125008385,
7.49482233047317));
#398595=CARTESIAN_POINT('Origin',(-2.60729278516566,-0.834224539571404,
7.51860402984325));
#398596=CARTESIAN_POINT('Origin',(-2.60729278516566,-0.834224539571404,
9.));
#398597=CARTESIAN_POINT('Origin',(-2.60729278516566,-0.834224539571404,
8.75721825406948));
#398598=CARTESIAN_POINT('Ctrl Pts',(-2.60435458367725,-0.81357238235248,
8.78942910404912));
#398599=CARTESIAN_POINT('Ctrl Pts',(-2.60830313188505,-0.81750448048863,
8.79672699501691));
#398600=CARTESIAN_POINT('Ctrl Pts',(-2.6032732741377,-0.824878354438151,
8.79893251111267));
#398601=CARTESIAN_POINT('Ctrl Pts',(-2.61211678181377,-0.821358504547104,
8.78111911759584));
#398602=CARTESIAN_POINT('Ctrl Pts',(-2.61679257887839,-0.826025327013831,
8.78644465894814));
#398603=CARTESIAN_POINT('Ctrl Pts',(-2.6137670602593,-0.833546081554491,
8.78817647674132));
#398604=CARTESIAN_POINT('Ctrl Pts',(-2.61695436881583,-0.826211001637831,
8.76780923932029));
#398605=CARTESIAN_POINT('Ctrl Pts',(-2.62247035001554,-0.831723595235668,
8.76988516158373));
#398606=CARTESIAN_POINT('Ctrl Pts',(-2.62031418371861,-0.838968409056351,
8.77093053738832));
#398607=CARTESIAN_POINT('Ctrl Pts',(-2.61601110555622,-0.825264831117445,
8.75371302330492));
#398608=CARTESIAN_POINT('Ctrl Pts',(-2.62139224614751,-0.830641589183835,
8.75300828287559));
#398609=CARTESIAN_POINT('Ctrl Pts',(-2.61903693688884,-0.837911187359129,
8.75267964240737));
#398610=CARTESIAN_POINT('Origin',(-2.59739259559948,-0.82429382821014,8.78727029226991));
#398611=CARTESIAN_POINT('Ctrl Pts',(-2.5557700913641,-0.764838063661141,
8.85049129520029));
#398612=CARTESIAN_POINT('Ctrl Pts',(-2.55989296307186,-0.768973645978593,
8.85711686593484));
#398613=CARTESIAN_POINT('Ctrl Pts',(-2.55537491841651,-0.776232298374609,
8.85933012996512));
#398614=CARTESIAN_POINT('Ctrl Pts',(-2.57261954817435,-0.781739466513898,
8.82945683644724));
#398615=CARTESIAN_POINT('Ctrl Pts',(-2.57677664221004,-0.785909376664987,
8.83607469902391));
#398616=CARTESIAN_POINT('Ctrl Pts',(-2.57221349406445,-0.793169522772272,
8.83829567148518));
#398617=CARTESIAN_POINT('Ctrl Pts',(-2.58944388951045,-0.798615676462751,
8.80838214965003));
#398618=CARTESIAN_POINT('Ctrl Pts',(-2.59361738938013,-0.80280204302623,
8.81501364461993));
#398619=CARTESIAN_POINT('Ctrl Pts',(-2.58902700057119,-0.810080582933243,
8.81722098428722));
#398620=CARTESIAN_POINT('Ctrl Pts',(-2.60624502375464,-0.815468607773367,
8.78727029226991));
#398621=CARTESIAN_POINT('Ctrl Pts',(-2.61041921685633,-0.819655669706065,
8.79393457792714));
#398622=CARTESIAN_POINT('Ctrl Pts',(-2.60581736094343,-0.826967464105193,
8.79610912703474));
#398623=CARTESIAN_POINT('Origin',(-2.54691766320894,-0.773663284097914,
8.85049129520029));
#398624=CARTESIAN_POINT('Ctrl Pts',(-2.55920636991203,-0.753260100986301,
8.85049129520029));
#398625=CARTESIAN_POINT('Ctrl Pts',(-2.5649178041393,-0.752043289049042,
8.85711686593484));
#398626=CARTESIAN_POINT('Ctrl Pts',(-2.56509113287406,-0.743495147773676,
8.85933012996512));
#398627=CARTESIAN_POINT('Ctrl Pts',(-2.55415354649658,-0.75433659694233,
8.86332496987231));
#398628=CARTESIAN_POINT('Ctrl Pts',(-2.55573644967855,-0.749995363028656,
8.86648636486736));
#398629=CARTESIAN_POINT('Ctrl Pts',(-2.55095922330301,-0.74652344568379,
8.87206031107457));
#398630=CARTESIAN_POINT('Ctrl Pts',(-2.55209786073928,-0.76115451173082,
8.86341338519877));
#398631=CARTESIAN_POINT('Ctrl Pts',(-2.55102439395551,-0.765662409211723,
8.8665458496606));
#398632=CARTESIAN_POINT('Ctrl Pts',(-2.54510291120594,-0.765907755566773,
8.87215952290714));
#398633=CARTESIAN_POINT('Ctrl Pts',(-2.5557700913641,-0.764838063661141,
8.85049129520029));
#398634=CARTESIAN_POINT('Ctrl Pts',(-2.55989296307186,-0.768973645978593,
8.85711686593484));
#398635=CARTESIAN_POINT('Ctrl Pts',(-2.55537491841651,-0.776232298374608,
8.85933012996512));
#398636=CARTESIAN_POINT('Origin',(-2.55660172093491,-0.741034480196092,
8.85049129520029));
#398637=CARTESIAN_POINT('Ctrl Pts',(-2.62912953922426,-0.738363081476928,
8.78727029226991));
#398638=CARTESIAN_POINT('Ctrl Pts',(-2.63491206922812,-0.737131122698051,
8.79393457792714));
#398639=CARTESIAN_POINT('Ctrl Pts',(-2.6350441475623,-0.728492721775898,
8.79610912703474));
#398640=CARTESIAN_POINT('Ctrl Pts',(-2.60585484624786,-0.743321717630787,
8.80838214965002));
#398641=CARTESIAN_POINT('Ctrl Pts',(-2.61163641591405,-0.742089963450328,
8.81501364461993));
#398642=CARTESIAN_POINT('Ctrl Pts',(-2.61175996320559,-0.733485688427872,
8.81722098428721));
#398643=CARTESIAN_POINT('Ctrl Pts',(-2.58254800437418,-0.748287203055851,
8.82945683644723));
#398644=CARTESIAN_POINT('Ctrl Pts',(-2.58830684695873,-0.74706029084382,
8.83607469902391));
#398645=CARTESIAN_POINT('Ctrl Pts',(-2.58844318986647,-0.738486292178717,
8.8382956714852));
#398646=CARTESIAN_POINT('Ctrl Pts',(-2.55920636991203,-0.753260100986301,
8.85049129520029));
#398647=CARTESIAN_POINT('Ctrl Pts',(-2.5649178041393,-0.752043289049042,
8.85711686593484));
#398648=CARTESIAN_POINT('Ctrl Pts',(-2.56509113287406,-0.743495147773676,
8.85933012996512));
#398649=CARTESIAN_POINT('Origin',(-2.62652489024714,-0.726137460686718,
8.78727029226991));
#398650=CARTESIAN_POINT('Ctrl Pts',(-2.64266321935266,-0.735479733686548,
8.75374538247848));
#398651=CARTESIAN_POINT('Ctrl Pts',(-2.65009811484497,-0.733909158184994,
8.75304829418601));
#398652=CARTESIAN_POINT('Ctrl Pts',(-2.6520933198787,-0.726540996943379,
8.75272238421917));
#398653=CARTESIAN_POINT('Ctrl Pts',(-2.64395422903473,-0.735204686572502,
8.76769408445021));
#398654=CARTESIAN_POINT('Ctrl Pts',(-2.65157607685315,-0.733593913216367,
8.76974318093971));
#398655=CARTESIAN_POINT('Ctrl Pts',(-2.65372225373277,-0.726354280485249,
8.7707786988043));
#398656=CARTESIAN_POINT('Ctrl Pts',(-2.6373372488473,-0.736614421409541,
8.78108014887987));
#398657=CARTESIAN_POINT('Ctrl Pts',(-2.64379727590477,-0.73525306630627,
8.78639403366323));
#398658=CARTESIAN_POINT('Ctrl Pts',(-2.64538156698147,-0.727315050337957,
8.78812224174741));
#398659=CARTESIAN_POINT('Ctrl Pts',(-2.62649347902618,-0.738924665570897,
8.78944554828686));
#398660=CARTESIAN_POINT('Ctrl Pts',(-2.63193890460374,-0.737782843388496,
8.79673892988686));
#398661=CARTESIAN_POINT('Ctrl Pts',(-2.63174894852015,-0.728868390460644,
8.79894799272499));
#398662=CARTESIAN_POINT('Origin',(-2.64023967100015,-0.72321554855868,8.75721825406948));
#398663=CARTESIAN_POINT('Origin',(-2.64023967100015,-0.72321554855868,9.));
#398664=CARTESIAN_POINT('Origin',(-2.64023967100015,-0.72321554855868,7.51860402984325));
#398665=CARTESIAN_POINT('Ctrl Pts',(-2.64368720766142,-0.743835077483582,
7.50366195182966));
#398666=CARTESIAN_POINT('Ctrl Pts',(-2.64721228549989,-0.74482690304422,
7.50000065167735));
#398667=CARTESIAN_POINT('Ctrl Pts',(-2.64721228549992,-0.744826903044107,
7.49482233047108));
#398668=CARTESIAN_POINT('Ctrl Pts',(-2.64710868794002,-0.737228469253189,
7.50215800491337));
#398669=CARTESIAN_POINT('Ctrl Pts',(-2.64979433702036,-0.735649866645916,
7.49877273257265));
#398670=CARTESIAN_POINT('Ctrl Pts',(-2.65072935414105,-0.732326780830906,
7.49481816995647));
#398671=CARTESIAN_POINT('Ctrl Pts',(-2.6456011070661,-0.734854186993081,
7.51043025814043));
#398672=CARTESIAN_POINT('Ctrl Pts',(-2.6507607661958,-0.732120933500968,
7.51006209594516));
#398673=CARTESIAN_POINT('Ctrl Pts',(-2.65229622879822,-0.726515460750259,
7.50731281821701));
#398674=CARTESIAN_POINT('Ctrl Pts',(-2.64284284172669,-0.735441484194384,
7.51860402984326));
#398675=CARTESIAN_POINT('Ctrl Pts',(-2.65028527911174,-0.733856825505501,
7.51860402984326));
#398676=CARTESIAN_POINT('Ctrl Pts',(-2.65229555990883,-0.726517902661682,
7.51860402984327));
#398677=CARTESIAN_POINT('Origin',(0.,0.,7.5));
#398678=CARTESIAN_POINT('Origin',(-2.50568666557813,-0.915681362418238,
7.5));
#398679=CARTESIAN_POINT('',(-2.50568666557813,-0.915681362418238,7.59394543036555));
#398680=CARTESIAN_POINT('',(-2.50568666557813,-0.915681362418238,8.85049129520029));
#398681=CARTESIAN_POINT('',(-2.50568666557813,-0.915681362418238,7.5));
#398682=CARTESIAN_POINT('',(-2.5764206255568,-0.90529494327273,8.78727029226991));
#398683=CARTESIAN_POINT('Ctrl Pts',(-2.50568666557814,-0.915681362418238,
8.85049129520029));
#398684=CARTESIAN_POINT('Ctrl Pts',(-2.5292989251247,-0.912214190147702,
8.82945686509571));
#398685=CARTESIAN_POINT('Ctrl Pts',(-2.55287608219231,-0.90875217224799,
8.80838212259897));
#398686=CARTESIAN_POINT('Ctrl Pts',(-2.5764206255568,-0.90529494327273,
8.78727029226991));
#398687=CARTESIAN_POINT('',(-2.59029443537465,-0.903257743546365,8.75721825406948));
#398688=CARTESIAN_POINT('Origin',(-2.54854335809393,-0.909388583893695,
8.75937679713171));
#398689=CARTESIAN_POINT('',(-2.59029443537465,-0.903257743546365,7.51860402984325));
#398690=CARTESIAN_POINT('',(-2.59029443537465,-0.903257743546365,7.5));
#398691=CARTESIAN_POINT('Ctrl Pts',(-2.59029443537465,-0.903257743546365,
7.51860402984325));
#398692=CARTESIAN_POINT('Ctrl Pts',(-2.57939871554831,-0.904857647086937,
7.52834476460825));
#398693=CARTESIAN_POINT('Ctrl Pts',(-2.56849592237787,-0.906458589261808,
7.53807742314407));
#398694=CARTESIAN_POINT('Ctrl Pts',(-2.55758581836641,-0.908060604944494,
7.54780169004674));
#398695=CARTESIAN_POINT('Ctrl Pts',(-2.54030480325306,-0.910598111204309,
7.5632044032688));
#398696=CARTESIAN_POINT('Ctrl Pts',(-2.52300542420909,-0.913138313983296,
7.57858609112103));
#398697=CARTESIAN_POINT('Ctrl Pts',(-2.50568666557813,-0.915681362418238,
7.59394543036555));
#398698=CARTESIAN_POINT('Origin',(-2.68279368784112,-1.13380819535554,7.5));
#398699=CARTESIAN_POINT('',(-2.55788654645048,-0.991320447028624,8.75721825406948));
#398700=CARTESIAN_POINT('',(-2.54864296074703,-0.980775832055561,8.78727029226991));
#398701=CARTESIAN_POINT('Origin',(-2.52517929254661,-0.954009666309173,
8.75658640621072));
#398702=CARTESIAN_POINT('',(-2.50151564461752,-0.927015373804549,8.85049129520029));
#398703=CARTESIAN_POINT('Ctrl Pts',(-2.54864296074703,-0.980775832055561,
8.78727029226991));
#398704=CARTESIAN_POINT('Ctrl Pts',(-2.53295613735134,-0.962881097461776,
8.80838212259897));
#398705=CARTESIAN_POINT('Ctrl Pts',(-2.51724758470003,-0.944961575232382,
8.82945686509571));
#398706=CARTESIAN_POINT('Ctrl Pts',(-2.50151564461752,-0.927015373804549,
8.85049129520029));
#398707=CARTESIAN_POINT('',(-2.50151564461752,-0.927015373804549,7.59394543036555));
#398708=CARTESIAN_POINT('',(-2.50151564461752,-0.927015373804549,7.5));
#398709=CARTESIAN_POINT('',(-2.55788654645048,-0.991320447028624,7.51860402984325));
#398710=CARTESIAN_POINT('Ctrl Pts',(-2.50151564461752,-0.927015373804549,
7.59394543036555));
#398711=CARTESIAN_POINT('Ctrl Pts',(-2.51305446717486,-0.940178278873335,
7.57858609112103));
#398712=CARTESIAN_POINT('Ctrl Pts',(-2.52458037785887,-0.953326454730175,
7.56320440326857));
#398713=CARTESIAN_POINT('Ctrl Pts',(-2.53609405336256,-0.96646067331226,
7.54780169004651));
#398714=CARTESIAN_POINT('Ctrl Pts',(-2.54336303591223,-0.974752760895078,
7.53807742314384));
#398715=CARTESIAN_POINT('Ctrl Pts',(-2.55062714752993,-0.983039291965115,
7.52834476460825));
#398716=CARTESIAN_POINT('Ctrl Pts',(-2.55788654645047,-0.991320447028623,
7.51860402984325));
#398717=CARTESIAN_POINT('',(-2.55788654645048,-0.991320447028624,7.5));
#398718=CARTESIAN_POINT('Origin',(-2.50668546515629,-0.922483422723959,
7.5));
#398719=CARTESIAN_POINT('Ctrl Pts',(-2.50151564461752,-0.927015373804549,
8.85049129520029));
#398720=CARTESIAN_POINT('Ctrl Pts',(-2.50138798433083,-0.926869745407334,
8.85097269580138));
#398721=CARTESIAN_POINT('Ctrl Pts',(-2.50126825987753,-0.926720409638613,
8.85143669361005));
#398722=CARTESIAN_POINT('Ctrl Pts',(-2.50115164046541,-0.926559943194745,
8.8519052845931));
#398723=CARTESIAN_POINT('Ctrl Pts',(-2.50092354029103,-0.926246081006952,
8.85282181883899));
#398724=CARTESIAN_POINT('Ctrl Pts',(-2.50071334603431,-0.925897594557926,
8.85372622499636));
#398725=CARTESIAN_POINT('Ctrl Pts',(-2.50053096238415,-0.925501051932902,
8.85462257735071));
#398726=CARTESIAN_POINT('Ctrl Pts',(-2.50037955395544,-0.925171856329469,
8.85536669723986));
#398727=CARTESIAN_POINT('Ctrl Pts',(-2.50024724861021,-0.924809479846986,
8.85610498449051));
#398728=CARTESIAN_POINT('Ctrl Pts',(-2.50014721912378,-0.924403462300347,
8.85681338218371));
#398729=CARTESIAN_POINT('Ctrl Pts',(-2.50005644220774,-0.924035000739112,
8.85745625420284));
#398730=CARTESIAN_POINT('Ctrl Pts',(-2.49999052655125,-0.923626119378977,
8.85808743050665));
#398731=CARTESIAN_POINT('Ctrl Pts',(-2.49997297445495,-0.923160524417042,
8.85866804508409));
#398732=CARTESIAN_POINT('Ctrl Pts',(-2.4999648762982,-0.922945708994462,
8.85893592806395));
#398733=CARTESIAN_POINT('Ctrl Pts',(-2.49996728752534,-0.922718707614324,
8.85919241173848));
#398734=CARTESIAN_POINT('Ctrl Pts',(-2.49998401765523,-0.922477377954843,
8.85943017985534));
#398735=CARTESIAN_POINT('Ctrl Pts',(-2.50000660828322,-0.922151511473323,
8.8597512372));
#398736=CARTESIAN_POINT('Ctrl Pts',(-2.50005652056601,-0.921791270397976,
8.86004599534705));
#398737=CARTESIAN_POINT('Ctrl Pts',(-2.50014347136778,-0.921402412271945,
8.86026130871721));
#398738=CARTESIAN_POINT('Ctrl Pts',(-2.50017530650771,-0.921260040348933,
8.86034014101235));
#398739=CARTESIAN_POINT('Ctrl Pts',(-2.50021257282627,-0.921111691043407,
8.86040910639693));
#398740=CARTESIAN_POINT('Ctrl Pts',(-2.50025458126597,-0.92096148800316,
8.86046313645507));
#398741=CARTESIAN_POINT('Ctrl Pts',(-2.5003201350843,-0.920727097416795,
8.8605474499083));
#398742=CARTESIAN_POINT('Ctrl Pts',(-2.50039916763199,-0.920481834184562,
8.86059655985669));
#398743=CARTESIAN_POINT('Ctrl Pts',(-2.50048633147296,-0.920241337932624,
8.86059725258816));
#398744=CARTESIAN_POINT('Ctrl Pts',(-2.50057369669722,-0.920000286038266,
8.86059794692012));
#398745=CARTESIAN_POINT('Ctrl Pts',(-2.50067269750016,-0.919762255163144,
8.86056369958366));
#398746=CARTESIAN_POINT('Ctrl Pts',(-2.50077445977493,-0.919538782504393,
8.86048590497774));
#398747=CARTESIAN_POINT('Ctrl Pts',(-2.50080101669881,-0.919480462794041,
8.86046560290182));
#398748=CARTESIAN_POINT('Ctrl Pts',(-2.5008281896189,-0.919422413409545,
8.86044257503091));
#398749=CARTESIAN_POINT('Ctrl Pts',(-2.5008551091393,-0.919366414208244,
8.86041778462583));
#398750=CARTESIAN_POINT('Ctrl Pts',(-2.50103624410723,-0.918989609072704,
8.86025097596201));
#398751=CARTESIAN_POINT('Ctrl Pts',(-2.5012305111296,-0.918655209975466,
8.8599848982295));
#398752=CARTESIAN_POINT('Ctrl Pts',(-2.50142491409744,-0.918368721174945,
8.85968173251462));
#398753=CARTESIAN_POINT('Ctrl Pts',(-2.50152774212947,-0.91821718501332,
8.85952137522077));
#398754=CARTESIAN_POINT('Ctrl Pts',(-2.50163243226653,-0.91807602501941,
8.85934740853961));
#398755=CARTESIAN_POINT('Ctrl Pts',(-2.50173625951288,-0.91794630582258,
8.8591675900182));
#398756=CARTESIAN_POINT('Ctrl Pts',(-2.50215317987531,-0.917425415820611,
8.85844552518696));
#398757=CARTESIAN_POINT('Ctrl Pts',(-2.50257738764837,-0.917057671454084,
8.85759444184126));
#398758=CARTESIAN_POINT('Ctrl Pts',(-2.5029501956441,-0.916788899331596,
8.8568349891514));
#398759=CARTESIAN_POINT('Ctrl Pts',(-2.50298920900799,-0.916760773044774,
8.85675551444999));
#398760=CARTESIAN_POINT('Ctrl Pts',(-2.50302766777015,-0.916733748780263,
8.85667699793652));
#398761=CARTESIAN_POINT('Ctrl Pts',(-2.50306550949756,-0.916707776672081,
8.85659965593547));
#398762=CARTESIAN_POINT('Ctrl Pts',(-2.50357629906517,-0.916357203830577,
8.85555568965886));
#398763=CARTESIAN_POINT('Ctrl Pts',(-2.50411782914084,-0.916094049730731,
8.85434650606346));
#398764=CARTESIAN_POINT('Ctrl Pts',(-2.5046900604545,-0.915911423788021,
8.85297329937117));
#398765=CARTESIAN_POINT('Ctrl Pts',(-2.50501190570186,-0.915808707822809,
8.85220095427747));
#398766=CARTESIAN_POINT('Ctrl Pts',(-2.50534369019836,-0.915731724168832,
8.85137579139183));
#398767=CARTESIAN_POINT('Ctrl Pts',(-2.50568666557814,-0.915681362418238,
8.85049129520029));
#398768=CARTESIAN_POINT('Origin',(-2.50668546515629,-0.922483422723959,
7.59394543036555));
#398769=CARTESIAN_POINT('Ctrl Pts',(-2.50114500373946,-0.926592565440157,
7.59443877723642));
#398770=CARTESIAN_POINT('Ctrl Pts',(-2.49732775931656,-0.922238046102214,
7.58783886950016));
#398771=CARTESIAN_POINT('Ctrl Pts',(-2.50224377712737,-0.915316200219761,
7.58559994247159));
#398772=CARTESIAN_POINT('Ctrl Pts',(-2.52198322905089,-0.950363758749818,
7.56670252222135));
#398773=CARTESIAN_POINT('Ctrl Pts',(-2.51817150162991,-0.946015532928607,
7.56004874999028));
#398774=CARTESIAN_POINT('Ctrl Pts',(-2.5230992292225,-0.939040301174026,
7.55786368756704));
#398775=CARTESIAN_POINT('Ctrl Pts',(-2.54278254105856,-0.974090561731022,
7.5388891333356));
#398776=CARTESIAN_POINT('Ctrl Pts',(-2.53894816035487,-0.96971649419084,
7.53222002137278));
#398777=CARTESIAN_POINT('Ctrl Pts',(-2.54391559872046,-0.962721710362594,
7.53005029815327));
#398778=CARTESIAN_POINT('Ctrl Pts',(-2.56354199857948,-0.997771900729836,
7.51101258149734));
#398779=CARTESIAN_POINT('Ctrl Pts',(-2.55966113821444,-0.993344811543191,
7.5043616886572));
#398780=CARTESIAN_POINT('Ctrl Pts',(-2.56469191920621,-0.986359203183317,
7.50217374673251));
#398781=CARTESIAN_POINT('',(-2.5635832672847,-0.985097876880951,7.50366116523517));
#398782=CARTESIAN_POINT('Ctrl Pts',(-2.55788654645047,-0.991320447028625,
7.51860402984325));
#398783=CARTESIAN_POINT('Ctrl Pts',(-2.55817765342152,-0.99165252713521,
7.51734760759494));
#398784=CARTESIAN_POINT('Ctrl Pts',(-2.55848545024178,-0.991913389124411,
7.51608817408573));
#398785=CARTESIAN_POINT('Ctrl Pts',(-2.55881786271931,-0.992092245848193,
7.5148100591312));
#398786=CARTESIAN_POINT('Ctrl Pts',(-2.5591189698847,-0.992254258542515,
7.51365231206384));
#398787=CARTESIAN_POINT('Ctrl Pts',(-2.55944058051349,-0.992349433201989,
7.51247773061043));
#398788=CARTESIAN_POINT('Ctrl Pts',(-2.55978760768028,-0.992340715789471,
7.51129758471022));
#398789=CARTESIAN_POINT('Ctrl Pts',(-2.56021892281661,-0.992329881041276,
7.50983079813402));
#398790=CARTESIAN_POINT('Ctrl Pts',(-2.56067540818268,-0.992145882723016,
7.50839324291155));
#398791=CARTESIAN_POINT('Ctrl Pts',(-2.56112957542532,-0.991710916073209,
7.50715379678855));
#398792=CARTESIAN_POINT('Ctrl Pts',(-2.5613393876049,-0.991509974014261,
7.50658120839351));
#398793=CARTESIAN_POINT('Ctrl Pts',(-2.56157195964614,-0.991220042996585,
7.50598221009429));
#398794=CARTESIAN_POINT('Ctrl Pts',(-2.56180401337727,-0.9908337899549,
7.50545747549611));
#398795=CARTESIAN_POINT('Ctrl Pts',(-2.56192784443093,-0.990627673376206,
7.50517746087247));
#398796=CARTESIAN_POINT('Ctrl Pts',(-2.56205304424278,-0.990391997191125,
7.50491486231392));
#398797=CARTESIAN_POINT('Ctrl Pts',(-2.56217482425125,-0.990132219958992,
7.50468370960992));
#398798=CARTESIAN_POINT('Ctrl Pts',(-2.56235692377725,-0.989743771054873,
7.50433806340447));
#398799=CARTESIAN_POINT('Ctrl Pts',(-2.56253633316337,-0.989289548577583,
7.50405484070984));
#398800=CARTESIAN_POINT('Ctrl Pts',(-2.56270030321808,-0.988799880389192,
7.50385766036131));
#398801=CARTESIAN_POINT('Ctrl Pts',(-2.56271783726676,-0.98874751798761,
7.50383657498791));
#398802=CARTESIAN_POINT('Ctrl Pts',(-2.56273520068951,-0.988694778002039,
7.50381643264937));
#398803=CARTESIAN_POINT('Ctrl Pts',(-2.56275238251345,-0.98864171760078,
7.50379723213559));
#398804=CARTESIAN_POINT('Ctrl Pts',(-2.56286707680879,-0.988287522065112,
7.50366906242519));
#398805=CARTESIAN_POINT('Ctrl Pts',(-2.56297548985005,-0.987911122718383,
7.50358235568538));
#398806=CARTESIAN_POINT('Ctrl Pts',(-2.5630712656504,-0.987545808184175,
7.5035341175365));
#398807=CARTESIAN_POINT('Ctrl Pts',(-2.5632148706233,-0.986998060385753,
7.50346178989176));
#398808=CARTESIAN_POINT('Ctrl Pts',(-2.56334606729219,-0.986402702482677,
7.50346967198527));
#398809=CARTESIAN_POINT('Ctrl Pts',(-2.56345687801437,-0.985814282467633,
7.50354272648692));
#398810=CARTESIAN_POINT('Ctrl Pts',(-2.56350245675805,-0.985572253135872,
7.50357277531559));
#398811=CARTESIAN_POINT('Ctrl Pts',(-2.56354466529949,-0.985331745408178,
7.50361331098761));
#398812=CARTESIAN_POINT('Ctrl Pts',(-2.56358326728603,-0.985097876881459,
7.50366116523659));
#398813=CARTESIAN_POINT('',(-2.50943323048236,-0.923494625763807,7.57603338622103));
#398814=CARTESIAN_POINT('Origin',(-2.51772740356821,-0.926543917882773,
7.58486873427628));
#398815=CARTESIAN_POINT('Ctrl Pts',(-2.56358326731837,-0.985097876927373,
7.50366116529968));
#398816=CARTESIAN_POINT('Ctrl Pts',(-2.54556333673348,-0.96459641599123,
7.5278357307971));
#398817=CARTESIAN_POINT('Ctrl Pts',(-2.52751419016024,-0.944062956655898,
7.55196141284068));
#398818=CARTESIAN_POINT('Ctrl Pts',(-2.50943323100972,-0.923494626899385,
7.57603338728831));
#398819=CARTESIAN_POINT('Ctrl Pts',(-2.50232577352112,-0.92767281329218,
7.5963967733137));
#398820=CARTESIAN_POINT('Ctrl Pts',(-2.48759500061618,-0.915457955303132,
7.59974925422226));
#398821=CARTESIAN_POINT('Ctrl Pts',(-2.50672970590147,-0.91570590633668,
7.59639677331373));
#398822=CARTESIAN_POINT('Ctrl Pts',(-2.49896195408416,-0.925698016371134,
7.58707626057421));
#398823=CARTESIAN_POINT('Ctrl Pts',(-2.49726541951554,-0.919016758850335,
7.58811717123965));
#398824=CARTESIAN_POINT('Ctrl Pts',(-2.50288821974734,-0.915029084195192,
7.58707626057425));
#398825=CARTESIAN_POINT('Ctrl Pts',(-2.50482266671421,-0.924092500961708,
7.58015376756929));
#398826=CARTESIAN_POINT('Ctrl Pts',(-2.50375153300597,-0.921403708571554,
7.58208760766041));
#398827=CARTESIAN_POINT('Ctrl Pts',(-2.50631009501529,-0.920050677758166,
7.5801537675693));
#398828=CARTESIAN_POINT('Ctrl Pts',(-2.50943322970564,-0.923494625478183,
7.57603338509286));
#398829=CARTESIAN_POINT('Ctrl Pts',(-2.50943322970564,-0.923494625478183,
7.57603338509286));
#398830=CARTESIAN_POINT('Ctrl Pts',(-2.50943322970564,-0.923494625478183,
7.57603338509286));
#398831=CARTESIAN_POINT('Origin',(-2.51772543279396,-0.926549273114443,
7.5848687342762));
#398832=CARTESIAN_POINT('Ctrl Pts',(-2.59880960003921,-0.90200739549112,
7.51098857897448));
#398833=CARTESIAN_POINT('Ctrl Pts',(-2.5929847431161,-0.90286270467336,
7.50433767179956));
#398834=CARTESIAN_POINT('Ctrl Pts',(-2.5922871544197,-0.911442997272864,
7.50214974420965));
#398835=CARTESIAN_POINT('Ctrl Pts',(-2.56764251675709,-0.90658390146659,
7.53887321589172));
#398836=CARTESIAN_POINT('Ctrl Pts',(-2.56188745195717,-0.907428962526923,
7.53220407452065));
#398837=CARTESIAN_POINT('Ctrl Pts',(-2.5611356572465,-0.915975173654377,
7.53003438070911));
#398838=CARTESIAN_POINT('Ctrl Pts',(-2.53641558117792,-0.911169196021749,
7.56669465659233));
#398839=CARTESIAN_POINT('Ctrl Pts',(-2.53069452774099,-0.912009262928298,
7.56004085833298));
#398840=CARTESIAN_POINT('Ctrl Pts',(-2.52992516332407,-0.920514833368937,
7.55785582193789));
#398841=CARTESIAN_POINT('Ctrl Pts',(-2.50513020557115,-0.915763071782057,
7.59443891967696));
#398842=CARTESIAN_POINT('Ctrl Pts',(-2.49940085731906,-0.916604356681062,
7.58783901202978));
#398843=CARTESIAN_POINT('Ctrl Pts',(-2.49865720208423,-0.925061670372774,
7.58560008491213));
#398844=CARTESIAN_POINT('',(-2.59059853376832,-0.911688670640867,7.50366116523517));
#398845=CARTESIAN_POINT('Ctrl Pts',(-2.59059853376867,-0.911688670640991,
7.50366116523554));
#398846=CARTESIAN_POINT('Ctrl Pts',(-2.59098904347062,-0.911039332755566,
7.50350835821027));
#398847=CARTESIAN_POINT('Ctrl Pts',(-2.591326891136,-0.910429728813534,
7.50345484955999));
#398848=CARTESIAN_POINT('Ctrl Pts',(-2.5916226464834,-0.909842025882743,
7.50349758195598));
#398849=CARTESIAN_POINT('Ctrl Pts',(-2.59177439091041,-0.909540490694061,
7.50351950684424));
#398850=CARTESIAN_POINT('Ctrl Pts',(-2.59193012691097,-0.909215058506846,
7.50357029184312));
#398851=CARTESIAN_POINT('Ctrl Pts',(-2.5920716753196,-0.90889711999251,
7.50365515313923));
#398852=CARTESIAN_POINT('Ctrl Pts',(-2.5922894340907,-0.908408001811447,
7.50378570417639));
#398853=CARTESIAN_POINT('Ctrl Pts',(-2.59248032444165,-0.90792240243678,
7.50400001621911));
#398854=CARTESIAN_POINT('Ctrl Pts',(-2.59262770382892,-0.907476452400872,
7.50428903009634));
#398855=CARTESIAN_POINT('Ctrl Pts',(-2.59264406180704,-0.907426955377816,
7.50432110841318));
#398856=CARTESIAN_POINT('Ctrl Pts',(-2.59265990793162,-0.907377928509107,
7.50435406373354));
#398857=CARTESIAN_POINT('Ctrl Pts',(-2.59267523710346,-0.907329407449733,
7.50438785222352));
#398858=CARTESIAN_POINT('Ctrl Pts',(-2.59276882906569,-0.907033163060087,
7.50459414719561));
#398859=CARTESIAN_POINT('Ctrl Pts',(-2.59284414892436,-0.906750901788691,
7.50483629897752));
#398860=CARTESIAN_POINT('Ctrl Pts',(-2.59289958273719,-0.90649377628495,
7.5050991045531));
#398861=CARTESIAN_POINT('Ctrl Pts',(-2.59302187529609,-0.905926531597884,
7.50567888004914));
#398862=CARTESIAN_POINT('Ctrl Pts',(-2.59305271249401,-0.905459376620288,
7.50637912803145));
#398863=CARTESIAN_POINT('Ctrl Pts',(-2.59302239896678,-0.905086224694276,
7.50710440483569));
#398864=CARTESIAN_POINT('Ctrl Pts',(-2.5930149654881,-0.904994720433914,
7.50728225710685));
#398865=CARTESIAN_POINT('Ctrl Pts',(-2.59300385233832,-0.904907035449132,
7.50746498566954));
#398866=CARTESIAN_POINT('Ctrl Pts',(-2.59298973222145,-0.904825164211458,
7.50764697238949));
#398867=CARTESIAN_POINT('Ctrl Pts',(-2.59291382635912,-0.904385046969295,
7.50862528291181));
#398868=CARTESIAN_POINT('Ctrl Pts',(-2.59274821214766,-0.904072281556928,
7.50965856837421));
#398869=CARTESIAN_POINT('Ctrl Pts',(-2.59254098856441,-0.903841240304901,
7.51067959873201));
#398870=CARTESIAN_POINT('Ctrl Pts',(-2.59242695316517,-0.903714098012488,
7.51124147302577));
#398871=CARTESIAN_POINT('Ctrl Pts',(-2.59229996591969,-0.903611963391176,
7.51180065547252));
#398872=CARTESIAN_POINT('Ctrl Pts',(-2.59216608810208,-0.903529118707881,
7.512351757165));
#398873=CARTESIAN_POINT('Ctrl Pts',(-2.59170348691167,-0.903242857325696,
7.51425603304536));
#398874=CARTESIAN_POINT('Ctrl Pts',(-2.59110026610329,-0.903157939223925,
7.5162690050518));
#398875=CARTESIAN_POINT('Ctrl Pts',(-2.59040768567601,-0.903242504084099,
7.51827788969244));
#398876=CARTESIAN_POINT('Ctrl Pts',(-2.59037020191449,-0.903247080894137,
7.51838661432545));
#398877=CARTESIAN_POINT('Ctrl Pts',(-2.5903324497827,-0.903252161594273,
7.51849533314857));
#398878=CARTESIAN_POINT('Ctrl Pts',(-2.59029443537466,-0.90325774354636,
7.51860402984325));
#398879=CARTESIAN_POINT('Ctrl Pts',(-2.50943323162123,-0.923494625241156,
7.57603338728985));
#398880=CARTESIAN_POINT('Ctrl Pts',(-2.53653388028815,-0.919553544812591,
7.55196141284922));
#398881=CARTESIAN_POINT('Ctrl Pts',(-2.56358770141576,-0.915618394507157,
7.52783573083105));
#398882=CARTESIAN_POINT('Ctrl Pts',(-2.59059853382585,-0.911688670627004,
7.50366116530176));
#398883=CARTESIAN_POINT('Origin',(-8.67125181207504E-16,-3.19110082301673E-16,
7.49482233047033));
#398884=CARTESIAN_POINT('Origin',(-2.55533261422668,-0.981927431468055,
7.49482233047033));
#398885=CARTESIAN_POINT('Origin',(0.,0.,7.50366116523517));
#398886=CARTESIAN_POINT('Origin',(-2.58226093460097,-0.908754485894703,
7.49482233047033));
#398887=CARTESIAN_POINT('Ctrl Pts',(-2.55788584917515,-0.991319651680091,
7.51860402984325));
#398888=CARTESIAN_POINT('Ctrl Pts',(-2.56290210620282,-0.997040967216085,
7.51860402984325));
#398889=CARTESIAN_POINT('Ctrl Pts',(-2.56012379910317,-1.00412456063257,
7.51860402984325));
#398890=CARTESIAN_POINT('Ctrl Pts',(-2.55974841868675,-0.993444016020627,
7.51041458714365));
#398891=CARTESIAN_POINT('Ctrl Pts',(-2.56224388421272,-0.998719148016021,
7.51004642900443));
#398892=CARTESIAN_POINT('Ctrl Pts',(-2.56012303287906,-1.00412651420352,
7.5072913648301));
#398893=CARTESIAN_POINT('Ctrl Pts',(-2.56237524877722,-0.992432333819996,
7.50215815450137));
#398894=CARTESIAN_POINT('Ctrl Pts',(-2.56358422056865,-0.995302255715978,
7.49877163671529));
#398895=CARTESIAN_POINT('Ctrl Pts',(-2.56234666411196,-0.998522873298193,
7.4948158853317));
#398896=CARTESIAN_POINT('Ctrl Pts',(-2.56358275340116,-0.985097679412473,
7.50366171572174));
#398897=CARTESIAN_POINT('Ctrl Pts',(-2.56700079967991,-0.986411118369375,
7.50000045605858));
#398898=CARTESIAN_POINT('Ctrl Pts',(-2.56700079967986,-0.986411118369491,
7.49482233047317));
#398899=CARTESIAN_POINT('Origin',(-2.54848687274361,-0.999560358084243,
7.51860402984325));
#398900=CARTESIAN_POINT('Origin',(-2.54848687274361,-0.999560358084243,
9.));
#398901=CARTESIAN_POINT('Origin',(-2.54848687274361,-0.999560358084243,
8.75721825406948));
#398902=CARTESIAN_POINT('Ctrl Pts',(-2.54687789636137,-0.978762381721547,
8.78942910404913));
#398903=CARTESIAN_POINT('Ctrl Pts',(-2.55056640146084,-0.982939385292637,
8.7967269950169));
#398904=CARTESIAN_POINT('Ctrl Pts',(-2.54507443236962,-0.989975844734951,
8.79893251111267));
#398905=CARTESIAN_POINT('Ctrl Pts',(-2.55412528766752,-0.987029832235209,
8.78111911759576));
#398906=CARTESIAN_POINT('Ctrl Pts',(-2.55849247346357,-0.991986645561183,
8.78644465894812));
#398907=CARTESIAN_POINT('Ctrl Pts',(-2.5549913146991,-0.999298102261562,
8.78817647674132));
#398908=CARTESIAN_POINT('Ctrl Pts',(-2.55864203477218,-0.9921823046136,
8.76780923932033));
#398909=CARTESIAN_POINT('Ctrl Pts',(-2.56379348971245,-0.99803698212555,
8.76988516158375));
#398910=CARTESIAN_POINT('Ctrl Pts',(-2.56117757667524,-1.00512876465029,
8.77093053738833));
#398911=CARTESIAN_POINT('Ctrl Pts',(-2.55776133090151,-0.991177643017514,
8.75371302330491));
#398912=CARTESIAN_POINT('Ctrl Pts',(-2.56278692529024,-0.996888124819234,
8.75300828287559));
#398913=CARTESIAN_POINT('Ctrl Pts',(-2.55997069051277,-1.0039918816431,
8.75267964240738));
#398914=CARTESIAN_POINT('Origin',(-2.53924328704017,-0.989015743111179,
8.78727029226991));
#398915=CARTESIAN_POINT('Ctrl Pts',(-2.50151564461752,-0.927015373804549,
8.85049129520029));
#398916=CARTESIAN_POINT('Ctrl Pts',(-2.50536507777435,-0.931406612421859,
8.85711686593484));
#398917=CARTESIAN_POINT('Ctrl Pts',(-2.50039125247053,-0.938360879023088,
8.85933012996512));
#398918=CARTESIAN_POINT('Ctrl Pts',(-2.51724760581288,-0.944961599316854,
8.82945683644723));
#398919=CARTESIAN_POINT('Ctrl Pts',(-2.52112899159233,-0.949389287869671,
8.83607469902389));
#398920=CARTESIAN_POINT('Ctrl Pts',(-2.51611005976584,-0.956342155322635,
8.83829567148519));
#398921=CARTESIAN_POINT('Ctrl Pts',(-2.53295611725146,-0.962881074532847,
8.80838214965003));
#398922=CARTESIAN_POINT('Ctrl Pts',(-2.53685282079138,-0.967326236811942,
8.81501364461988));
#398923=CARTESIAN_POINT('Ctrl Pts',(-2.53180552577561,-0.974295714957338,
8.81722098428721));
#398924=CARTESIAN_POINT('Ctrl Pts',(-2.54864296074703,-0.980775832055561,
8.78727029226991));
#398925=CARTESIAN_POINT('Ctrl Pts',(-2.55254031154221,-0.985221732690724,
8.79393457792714));
#398926=CARTESIAN_POINT('Ctrl Pts',(-2.54747944236023,-0.992223662303413,
8.79610912703474));
#398927=CARTESIAN_POINT('Origin',(-2.49211597091066,-0.935255284860168,
8.85049129520029));
#398928=CARTESIAN_POINT('Ctrl Pts',(-2.50568666557814,-0.915681362418238,
8.85049129520029));
#398929=CARTESIAN_POINT('Ctrl Pts',(-2.51146432645973,-0.914832983398953,
8.85711686593484));
#398930=CARTESIAN_POINT('Ctrl Pts',(-2.51218498036396,-0.906313510406788,
8.85933012996512));
#398931=CARTESIAN_POINT('Ctrl Pts',(-2.5005752523976,-0.916431911090119,
8.86332496987231));
#398932=CARTESIAN_POINT('Ctrl Pts',(-2.50243304714704,-0.912201013662185,
8.86648636486737));
#398933=CARTESIAN_POINT('Ctrl Pts',(-2.4978880826035,-0.908430151799093,
8.87206031107457));
#398934=CARTESIAN_POINT('Ctrl Pts',(-2.49808696496685,-0.923104109502771,
8.86341338519876));
#398935=CARTESIAN_POINT('Ctrl Pts',(-2.49672688175245,-0.927533967771866,
8.86654584966057));
#398936=CARTESIAN_POINT('Ctrl Pts',(-2.49080184592933,-0.927399419334132,
8.87215952290714));
#398937=CARTESIAN_POINT('Ctrl Pts',(-2.50151564461752,-0.927015373804549,
8.85049129520029));
#398938=CARTESIAN_POINT('Ctrl Pts',(-2.50536507777435,-0.931406612421859,
8.85711686593484));
#398939=CARTESIAN_POINT('Ctrl Pts',(-2.50039125247053,-0.938360879023087,
8.85933012996512));
#398940=CARTESIAN_POINT('Origin',(-2.50387066634512,-0.903313980044199,
8.85049129520029));
#398941=CARTESIAN_POINT('Ctrl Pts',(-2.5764206255568,-0.90529494327273,
8.78727029226991));
#398942=CARTESIAN_POINT('Ctrl Pts',(-2.58227020660257,-0.904436003654684,
8.79393457792714));
#398943=CARTESIAN_POINT('Ctrl Pts',(-2.582955477815,-0.895823813541617,
8.79610912703474));
#398944=CARTESIAN_POINT('Ctrl Pts',(-2.55287605202416,-0.908752176677816,
8.80838214965003));
#398945=CARTESIAN_POINT('Ctrl Pts',(-2.55872466159673,-0.90789337970876,
8.81501364461996));
#398946=CARTESIAN_POINT('Ctrl Pts',(-2.55939923284052,-0.899314698794302,
8.81722098428721));
#398947=CARTESIAN_POINT('Ctrl Pts',(-2.52929895681325,-0.912214185494627,
8.82945683644723));
#398948=CARTESIAN_POINT('Ctrl Pts',(-2.53512457577338,-0.911358764416542,
8.83607469902389));
#398949=CARTESIAN_POINT('Ctrl Pts',(-2.5358099765306,-0.902811117471346,
8.8382956714852));
#398950=CARTESIAN_POINT('Ctrl Pts',(-2.50568666557814,-0.915681362418238,
8.85049129520029));
#398951=CARTESIAN_POINT('Ctrl Pts',(-2.51146432645973,-0.914832983398953,
8.85711686593484));
#398952=CARTESIAN_POINT('Ctrl Pts',(-2.51218498036396,-0.906313510406788,
8.85933012996512));
#398953=CARTESIAN_POINT('Origin',(-2.57460462632379,-0.892927560898691,
8.78727029226991));
#398954=CARTESIAN_POINT('Ctrl Pts',(-2.59011123601512,-0.903284625492598,
8.75374538247847));
#398955=CARTESIAN_POINT('Ctrl Pts',(-2.59763148283513,-0.902193632296583,
8.75304829418601));
#398956=CARTESIAN_POINT('Ctrl Pts',(-2.60009466821772,-0.894968442957884,
8.75272238421917));
#398957=CARTESIAN_POINT('Ctrl Pts',(-2.59141721550838,-0.903092858766682,
8.76769408445022));
#398958=CARTESIAN_POINT('Ctrl Pts',(-2.59912660602629,-0.901973728383557,
8.76974318093972));
#398959=CARTESIAN_POINT('Ctrl Pts',(-2.60173221821703,-0.894886476279129,
8.77077869880429));
#398960=CARTESIAN_POINT('Ctrl Pts',(-2.58472350859536,-0.904075745776078,
8.78108014887986));
#398961=CARTESIAN_POINT('Ctrl Pts',(-2.59125748515534,-0.903131083077525,
8.7863940336632));
#398962=CARTESIAN_POINT('Ctrl Pts',(-2.59334711156538,-0.895310882492168,
8.78812224174741));
#398963=CARTESIAN_POINT('Ctrl Pts',(-2.57375400061067,-0.905686480575177,
8.78944554828686));
#398964=CARTESIAN_POINT('Ctrl Pts',(-2.57926139477577,-0.904895894003556,
8.79673892988687));
#398965=CARTESIAN_POINT('Ctrl Pts',(-2.57964297993742,-0.895987586247249,
8.79894799272499));
#398966=CARTESIAN_POINT('Origin',(-2.58847843614164,-0.890890361172326,
8.75721825406948));
#398967=CARTESIAN_POINT('Origin',(-2.58847843614164,-0.890890361172326,
9.));
#398968=CARTESIAN_POINT('Origin',(-2.58847843614164,-0.890890361172326,
7.51860402984325));
#398969=CARTESIAN_POINT('Ctrl Pts',(-2.59059779171497,-0.911688409495895,
7.50366195182966));
#398970=CARTESIAN_POINT('Ctrl Pts',(-2.59405208042111,-0.912904049757105,
7.50000065167735));
#398971=CARTESIAN_POINT('Ctrl Pts',(-2.59405208042115,-0.912904049756995,
7.49482233047108));
#398972=CARTESIAN_POINT('Ctrl Pts',(-2.59443552903803,-0.90531459024478,
7.50215800491337));
#398973=CARTESIAN_POINT('Ctrl Pts',(-2.5972168015806,-0.903911301173237,
7.49877273257267));
#398974=CARTESIAN_POINT('Ctrl Pts',(-2.59836280844753,-0.90065494974704,
7.49481816995647));
#398975=CARTESIAN_POINT('Ctrl Pts',(-2.59308316643742,-0.902848595163979,
7.51043025814043));
#398976=CARTESIAN_POINT('Ctrl Pts',(-2.59840734464658,-0.900451537929768,
7.51006209594514));
#398977=CARTESIAN_POINT('Ctrl Pts',(-2.60029879634862,-0.894955959650723,
7.50731281821701));
#398978=CARTESIAN_POINT('Ctrl Pts',(-2.59029293998908,-0.903257963033136,
7.51860402984326));
#398979=CARTESIAN_POINT('Ctrl Pts',(-2.59782161551912,-0.902153398795935,
7.51860402984327));
#398980=CARTESIAN_POINT('Ctrl Pts',(-2.60029797237973,-0.89495835368909,
7.51860402984327));
#398981=CARTESIAN_POINT('Origin',(0.,0.,7.5));
#398982=CARTESIAN_POINT('Origin',(-2.44187055726728,-1.07433989271896,7.5));
#398983=CARTESIAN_POINT('',(-2.44187055726728,-1.07433989271896,7.59394543036555));
#398984=CARTESIAN_POINT('',(-2.44187055726728,-1.07433989271896,8.85049129520029));
#398985=CARTESIAN_POINT('',(-2.44187055726728,-1.07433989271896,7.5));
#398986=CARTESIAN_POINT('',(-2.51312464689844,-1.06850675396147,8.78727029226991));
#398987=CARTESIAN_POINT('Ctrl Pts',(-2.44187055726728,-1.07433989271896,
8.85049129520029));
#398988=CARTESIAN_POINT('Ctrl Pts',(-2.46565644538429,-1.0723926867891,
8.82945686509571));
#398989=CARTESIAN_POINT('Ctrl Pts',(-2.48940697290247,-1.0704483756163,
8.80838212259897));
#398990=CARTESIAN_POINT('Ctrl Pts',(-2.51312464689844,-1.06850675396147,
8.78727029226991));
#398991=CARTESIAN_POINT('',(-2.52710047532067,-1.06736263792743,8.75721825406948));
#398992=CARTESIAN_POINT('Origin',(-2.48504237581409,-1.07080588110011,8.75937679713092));
#398993=CARTESIAN_POINT('',(-2.52710047532067,-1.06736263792743,7.51860402984325));
#398994=CARTESIAN_POINT('',(-2.52710047532067,-1.06736263792743,7.5));
#398995=CARTESIAN_POINT('Ctrl Pts',(-2.52710047532067,-1.06736263792743,
7.51860402984325));
#398996=CARTESIAN_POINT('Ctrl Pts',(-2.51612463574747,-1.06826116312847,
7.52834476460825));
#398997=CARTESIAN_POINT('Ctrl Pts',(-2.50514167081761,-1.06916027163911,
7.53807742314407));
#398998=CARTESIAN_POINT('Ctrl Pts',(-2.49415134128775,-1.07005998304473,
7.54780169004674));
#398999=CARTESIAN_POINT('Ctrl Pts',(-2.47674325328907,-1.07148507728598,
7.5632044032688));
#399000=CARTESIAN_POINT('Ctrl Pts',(-2.45931666632384,-1.07291168592505,
7.57858609112103));
#399001=CARTESIAN_POINT('Ctrl Pts',(-2.44187055726728,-1.07433989271896,
7.59394543036555));
#399002=CARTESIAN_POINT('Origin',(-2.60463825998837,-1.30336584656049,7.5));
#399003=CARTESIAN_POINT('',(-2.48911697509582,-1.15316802656821,8.75721825406948));
#399004=CARTESIAN_POINT('',(-2.48056797713151,-1.14205283806808,8.78727029226991));
#399005=CARTESIAN_POINT('Origin',(-2.45886743168094,-1.11383834389628,8.75658640621053));
#399006=CARTESIAN_POINT('',(-2.43698193351378,-1.08538337893282,8.85049129520029));
#399007=CARTESIAN_POINT('Ctrl Pts',(-2.48056797713151,-1.14205283806808,
8.78727029226991));
#399008=CARTESIAN_POINT('Ctrl Pts',(-2.4660599035788,-1.12318981189995,
8.80838212259894));
#399009=CARTESIAN_POINT('Ctrl Pts',(-2.45153173356485,-1.10430065682691,
8.82945686509571));
#399010=CARTESIAN_POINT('Ctrl Pts',(-2.43698193351378,-1.08538337893282,
8.85049129520029));
#399011=CARTESIAN_POINT('',(-2.43698193351378,-1.08538337893282,7.59394543036555));
#399012=CARTESIAN_POINT('',(-2.43698193351378,-1.08538337893282,7.5));
#399013=CARTESIAN_POINT('',(-2.48911697509582,-1.15316802656821,7.51860402984325));
#399014=CARTESIAN_POINT('Ctrl Pts',(-2.43698193351378,-1.08538337893282,
7.59394543036555));
#399015=CARTESIAN_POINT('Ctrl Pts',(-2.4476536980993,-1.09925853430099,
7.57858609112103));
#399016=CARTESIAN_POINT('Ctrl Pts',(-2.45831352104417,-1.1131181634534,
7.56320440326857));
#399017=CARTESIAN_POINT('Ctrl Pts',(-2.46896202819287,-1.12696308009707,
7.54780169004651));
#399018=CARTESIAN_POINT('Ctrl Pts',(-2.47568479996276,-1.13570385600762,
7.53807742314383));
#399019=CARTESIAN_POINT('Ctrl Pts',(-2.48240306681554,-1.14443877474016,
7.52834476460825));
#399020=CARTESIAN_POINT('Ctrl Pts',(-2.48911697509582,-1.15316802656821,
7.51860402984325));
#399021=CARTESIAN_POINT('',(-2.48911697509582,-1.15316802656821,7.5));
#399022=CARTESIAN_POINT('Origin',(-2.44243149520447,-1.08119197077096,7.5));
#399023=CARTESIAN_POINT('Ctrl Pts',(-2.43698193351378,-1.08538337893282,
8.85049129520029));
#399024=CARTESIAN_POINT('Ctrl Pts',(-2.43686386596228,-1.08522987052212,
8.85097269580138));
#399025=CARTESIAN_POINT('Ctrl Pts',(-2.43675395547127,-1.08507317080769,
8.85143669361005));
#399026=CARTESIAN_POINT('Ctrl Pts',(-2.43664785678659,-1.08490556222795,
8.8519052845931));
#399027=CARTESIAN_POINT('Ctrl Pts',(-2.43644033448791,-1.08457773047533,
8.85282181883899));
#399028=CARTESIAN_POINT('Ctrl Pts',(-2.43625289970128,-1.08421649283683,
8.85372622499635));
#399029=CARTESIAN_POINT('Ctrl Pts',(-2.4360962973511,-1.08380907959057,
8.8546225773507));
#399030=CARTESIAN_POINT('Ctrl Pts',(-2.43596629164197,-1.08347085958347,
8.85536669723986));
#399031=CARTESIAN_POINT('Ctrl Pts',(-2.43585747567322,-1.08310075080976,
8.85610498449051));
#399032=CARTESIAN_POINT('Ctrl Pts',(-2.43578366534162,-1.08268915855852,
8.85681338218371));
#399033=CARTESIAN_POINT('Ctrl Pts',(-2.43571668234978,-1.0823156379441,
8.85745625420284));
#399034=CARTESIAN_POINT('Ctrl Pts',(-2.43567709924276,-1.08190337344395,
8.85808743050666));
#399035=CARTESIAN_POINT('Ctrl Pts',(-2.43568941398076,-1.08143761053013,
8.8586680450841));
#399036=CARTESIAN_POINT('Ctrl Pts',(-2.43569509573392,-1.08122271761819,
8.85893592806395));
#399037=CARTESIAN_POINT('Ctrl Pts',(-2.4357120460353,-1.08099633712459,
8.85919241173848));
#399038=CARTESIAN_POINT('Ctrl Pts',(-2.43574420383571,-1.08075657520588,
8.85943017985534));
#399039=CARTESIAN_POINT('Ctrl Pts',(-2.435787626386,-1.0804328256385,8.8597512372));
#399040=CARTESIAN_POINT('Ctrl Pts',(-2.43586051684359,-1.08007652260802,
8.86004599534705));
#399041=CARTESIAN_POINT('Ctrl Pts',(-2.43597220322129,-1.07969403438971,
8.86026130871721));
#399042=CARTESIAN_POINT('Ctrl Pts',(-2.43601309475293,-1.0795539946695,
8.86034014101235));
#399043=CARTESIAN_POINT('Ctrl Pts',(-2.43605978927648,-1.07940833782476,
8.86040910639693));
#399044=CARTESIAN_POINT('Ctrl Pts',(-2.43611133494717,-1.07926113488274,
8.86046313645507));
#399045=CARTESIAN_POINT('Ctrl Pts',(-2.43619177153458,-1.07903142592454,
8.8605474499083));
#399046=CARTESIAN_POINT('Ctrl Pts',(-2.43628635577067,-1.07879173024464,
8.86059655985669));
#399047=CARTESIAN_POINT('Ctrl Pts',(-2.43638874917194,-1.07855731272451,
8.86059725258816));
#399048=CARTESIAN_POINT('Ctrl Pts',(-2.43649137914288,-1.07832235360626,
8.86059794692012));
#399049=CARTESIAN_POINT('Ctrl Pts',(-2.43660542722858,-1.07809115479432,
8.86056369958366));
#399050=CARTESIAN_POINT('Ctrl Pts',(-2.43672129836425,-1.07787466121544,
8.86048590497774));
#399051=CARTESIAN_POINT('Ctrl Pts',(-2.43675153728076,-1.07781816283715,
8.86046560290182));
#399052=CARTESIAN_POINT('Ctrl Pts',(-2.436782373608,-1.0777619736963,8.86044257503091));
#399053=CARTESIAN_POINT('Ctrl Pts',(-2.43681282570051,-1.07770781429096,
8.86041778462583));
#399054=CARTESIAN_POINT('Ctrl Pts',(-2.43701773049514,-1.07734338869923,
8.86025097596201));
#399055=CARTESIAN_POINT('Ctrl Pts',(-2.4372330233988,-1.07702212339166,
8.85998489822951));
#399056=CARTESIAN_POINT('Ctrl Pts',(-2.43744538234537,-1.07674867865402,
8.85968173251462));
#399057=CARTESIAN_POINT('Ctrl Pts',(-2.43755770806138,-1.07660404205432,
8.85952137522077));
#399058=CARTESIAN_POINT('Ctrl Pts',(-2.43767122725319,-1.07646987960887,
8.85934740853961));
#399059=CARTESIAN_POINT('Ctrl Pts',(-2.43778315231281,-1.07634707916855,
8.8591675900182));
#399060=CARTESIAN_POINT('Ctrl Pts',(-2.43823258960465,-1.07585397157029,
8.85844552518695));
#399061=CARTESIAN_POINT('Ctrl Pts',(-2.43867948725982,-1.07551416185933,
8.85759444184122));
#399062=CARTESIAN_POINT('Ctrl Pts',(-2.43906874957056,-1.07526982784829,
8.85683498915136));
#399063=CARTESIAN_POINT('Ctrl Pts',(-2.43910948483468,-1.07524425894475,
8.85675551444997));
#399064=CARTESIAN_POINT('Ctrl Pts',(-2.43914959602975,-1.07521975426585,
8.8566769979365));
#399065=CARTESIAN_POINT('Ctrl Pts',(-2.43918902404596,-1.07519626004795,
8.85659965593547));
#399066=CARTESIAN_POINT('Ctrl Pts',(-2.43972122542069,-1.07487913389591,
8.85555568965886));
#399067=CARTESIAN_POINT('Ctrl Pts',(-2.44027850320581,-1.07465121642546,
8.85434650606345));
#399068=CARTESIAN_POINT('Ctrl Pts',(-2.44086125969318,-1.07450562869348,
8.85297329937116));
#399069=CARTESIAN_POINT('Ctrl Pts',(-2.44118902470945,-1.07442374446503,
8.85220095427747));
#399070=CARTESIAN_POINT('Ctrl Pts',(-2.44152505987876,-1.07436817648791,
8.85137579139183));
#399071=CARTESIAN_POINT('Ctrl Pts',(-2.44187055726728,-1.07433989271896,
8.85049129520029));
#399072=CARTESIAN_POINT('Origin',(-2.44243149520447,-1.08119197077096,7.59394543036555));
#399073=CARTESIAN_POINT('Ctrl Pts',(-2.43663914358208,-1.08493769223097,
7.59443877723642));
#399074=CARTESIAN_POINT('Ctrl Pts',(-2.43310873710913,-1.08034754803013,
7.58783886950016));
#399075=CARTESIAN_POINT('Ctrl Pts',(-2.43845813862247,-1.07375489416498,
7.58559994247159));
#399076=CARTESIAN_POINT('Ctrl Pts',(-2.45591152894015,-1.10999515475423,
7.56670252222134));
#399077=CARTESIAN_POINT('Ctrl Pts',(-2.45238622490689,-1.10541164461494,
7.56004874999029));
#399078=CARTESIAN_POINT('Ctrl Pts',(-2.45775073258754,-1.09876646481297,
7.55786368756704));
#399079=CARTESIAN_POINT('Ctrl Pts',(-2.4751479250441,-1.13500582496976,
7.53888913333554));
#399080=CARTESIAN_POINT('Ctrl Pts',(-2.47160166995632,-1.13039507480528,
7.53222002137272));
#399081=CARTESIAN_POINT('Ctrl Pts',(-2.47700705952568,-1.12373292737944,
7.53005029815326));
#399082=CARTESIAN_POINT('Ctrl Pts',(-2.49434746143405,-1.15996857112787,
7.51101258149734));
#399083=CARTESIAN_POINT('Ctrl Pts',(-2.49075821929091,-1.15530193029346,
7.5043616886572));
#399084=CARTESIAN_POINT('Ctrl Pts',(-2.4962262334679,-1.14865299785998,
7.50217374673251));
#399085=CARTESIAN_POINT('',(-2.49520067284433,-1.14732323151529,7.50366116523517));
#399086=CARTESIAN_POINT('Ctrl Pts',(-2.48911697509582,-1.15316802656821,
7.51860402984325));
#399087=CARTESIAN_POINT('Ctrl Pts',(-2.48938620751089,-1.15351807566827,
7.51734760759494));
#399088=CARTESIAN_POINT('Ctrl Pts',(-2.48967665844454,-1.15379812229852,
7.51608817408573));
#399089=CARTESIAN_POINT('Ctrl Pts',(-2.48999692855534,-1.15399790928254,
7.5148100591312));
#399090=CARTESIAN_POINT('Ctrl Pts',(-2.49028703687481,-1.15417888110673,
7.51365231206384));
#399091=CARTESIAN_POINT('Ctrl Pts',(-2.4906018888587,-1.1542944658834,7.51247773061043));
#399092=CARTESIAN_POINT('Ctrl Pts',(-2.49094876154749,-1.15430800048865,
7.51129758471022));
#399093=CARTESIAN_POINT('Ctrl Pts',(-2.49137988468531,-1.15432482245728,
7.50983079813402));
#399094=CARTESIAN_POINT('Ctrl Pts',(-2.49184722096597,-1.15417044930112,
7.50839324291155));
#399095=CARTESIAN_POINT('Ctrl Pts',(-2.49232832348224,-1.15376547493209,
7.50715379678855));
#399096=CARTESIAN_POINT('Ctrl Pts',(-2.49255057898211,-1.15357838844265,
7.50658120839351));
#399097=CARTESIAN_POINT('Ctrl Pts',(-2.49280124912323,-1.15330395406119,
7.50598221009429));
#399098=CARTESIAN_POINT('Ctrl Pts',(-2.49305757339243,-1.1529333623514,
7.50545747549611));
#399099=CARTESIAN_POINT('Ctrl Pts',(-2.49319435595645,-1.15273560314417,
7.50517746087247));
#399100=CARTESIAN_POINT('Ctrl Pts',(-2.49333439835688,-1.15250843276058,
7.50491486231392));
#399101=CARTESIAN_POINT('Ctrl Pts',(-2.49347257213968,-1.15225699174056,
7.50468370960992));
#399102=CARTESIAN_POINT('Ctrl Pts',(-2.49367918552941,-1.15188100810307,
7.50433806340447));
#399103=CARTESIAN_POINT('Ctrl Pts',(-2.49388732843374,-1.15143921367341,
7.50405484070984));
#399104=CARTESIAN_POINT('Ctrl Pts',(-2.49408233474293,-1.1509610571583,
7.50385766036131));
#399105=CARTESIAN_POINT('Ctrl Pts',(-2.49410318763662,-1.15090992575125,
7.50383657498791));
#399106=CARTESIAN_POINT('Ctrl Pts',(-2.49412389444684,-1.15085840660395,
7.50381643264937));
#399107=CARTESIAN_POINT('Ctrl Pts',(-2.49414444056045,-1.15080655606421,
7.50379723213559));
#399108=CARTESIAN_POINT('Ctrl Pts',(-2.49428159258995,-1.15046043674999,
7.50366906242519));
#399109=CARTESIAN_POINT('Ctrl Pts',(-2.49441389887394,-1.15009175680349,
7.50358235568538));
#399110=CARTESIAN_POINT('Ctrl Pts',(-2.4945328836752,-1.14973332922377,
7.5035341175365));
#399111=CARTESIAN_POINT('Ctrl Pts',(-2.49471128791822,-1.14919590763415,
7.50346178989176));
#399112=CARTESIAN_POINT('Ctrl Pts',(-2.4948803597413,-1.14861017875717,
7.50346967198527));
#399113=CARTESIAN_POINT('Ctrl Pts',(-2.49502864299077,-1.1480300673815,
7.50354272648692));
#399114=CARTESIAN_POINT('Ctrl Pts',(-2.49508963496056,-1.1477914555651,
7.50357277531559));
#399115=CARTESIAN_POINT('Ctrl Pts',(-2.49514716616304,-1.14755414629686,
7.50361331098761));
#399116=CARTESIAN_POINT('Ctrl Pts',(-2.49520067284562,-1.14732323151588,
7.50366116523659));
#399117=CARTESIAN_POINT('',(-2.44510882695077,-1.0823771461146,7.57603338622103));
#399118=CARTESIAN_POINT('Origin',(-2.45319058995134,-1.08595158263,7.58486873427628));
#399119=CARTESIAN_POINT('Ctrl Pts',(-2.49520067287495,-1.14732323156377,
7.50366116529968));
#399120=CARTESIAN_POINT('Ctrl Pts',(-2.47853129928221,-1.12570935216126,
7.52783573079709));
#399121=CARTESIAN_POINT('Ctrl Pts',(-2.46183481987292,-1.10406166822896,
7.55196141284068));
#399122=CARTESIAN_POINT('Ctrl Pts',(-2.44510882740428,-1.08237714728164,
7.57603338728831));
#399123=CARTESIAN_POINT('Ctrl Pts',(-2.43774827562808,-1.08609137277759,
7.5963967733137));
#399124=CARTESIAN_POINT('Ctrl Pts',(-2.42383037731431,-1.07295780766384,
7.59974925422225));
#399125=CARTESIAN_POINT('Ctrl Pts',(-2.44290988201814,-1.07443121403225,
7.59639677331373));
#399126=CARTESIAN_POINT('Ctrl Pts',(-2.43451789319206,-1.08390511263732,
7.5870762605742));
#399127=CARTESIAN_POINT('Ctrl Pts',(-2.43325291397476,-1.07712888513364,
7.58811717123966));
#399128=CARTESIAN_POINT('Ctrl Pts',(-2.4391196527528,-1.07350965763151,
7.58707626057425));
#399129=CARTESIAN_POINT('Ctrl Pts',(-2.44046943008491,-1.08267839307892,
7.58015376756929));
#399130=CARTESIAN_POINT('Ctrl Pts',(-2.43957276865569,-1.07992649732878,
7.5820876076604));
#399131=CARTESIAN_POINT('Ctrl Pts',(-2.4422127628068,-1.07874017409309,
7.58015376756931));
#399132=CARTESIAN_POINT('Ctrl Pts',(-2.44510882619395,-1.0823771457798,
7.57603338509286));
#399133=CARTESIAN_POINT('Ctrl Pts',(-2.44510882619395,-1.0823771457798,
7.57603338509286));
#399134=CARTESIAN_POINT('Ctrl Pts',(-2.44510882619395,-1.0823771457798,
7.57603338509286));
#399135=CARTESIAN_POINT('Origin',(-2.45318828011509,-1.08595680059041,7.58486873427625));
#399136=CARTESIAN_POINT('Ctrl Pts',(-2.53567825474113,-1.0666604273196,
7.51098857897448));
#399137=CARTESIAN_POINT('Ctrl Pts',(-2.52981056576383,-1.06714077931297,
7.50433767179956));
#399138=CARTESIAN_POINT('Ctrl Pts',(-2.52856466910387,-1.07565874811986,
7.50214974420965));
#399139=CARTESIAN_POINT('Ctrl Pts',(-2.50428198982964,-1.06923064849067,
7.53887321589167));
#399140=CARTESIAN_POINT('Ctrl Pts',(-2.49848460617954,-1.06970524501471,
7.53220407452059));
#399141=CARTESIAN_POINT('Ctrl Pts',(-2.49718679848484,-1.07818572938232,
7.53003438070911));
#399142=CARTESIAN_POINT('Ctrl Pts',(-2.47282543250793,-1.07180580543451,
7.56669465659234));
#399143=CARTESIAN_POINT('Ctrl Pts',(-2.46706231031738,-1.07227759718128,
7.56004085833301));
#399144=CARTESIAN_POINT('Ctrl Pts',(-2.46574957287294,-1.08071639866779,
7.55785582193789));
#399145=CARTESIAN_POINT('Ctrl Pts',(-2.44131000543014,-1.07438578168707,
7.59443891967696));
#399146=CARTESIAN_POINT('Ctrl Pts',(-2.43553852742996,-1.07485825747317,
7.58783901202978));
#399147=CARTESIAN_POINT('Ctrl Pts',(-2.43425453816589,-1.08325054855237,
7.58560008491213));
#399148=CARTESIAN_POINT('',(-2.52686377755798,-1.07579572642898,7.50366116523517));
#399149=CARTESIAN_POINT('Ctrl Pts',(-2.52686377755833,-1.07579572642913,
7.50366116523554));
#399150=CARTESIAN_POINT('Ctrl Pts',(-2.52729508813737,-1.07517274272054,
7.50350835821027));
#399151=CARTESIAN_POINT('Ctrl Pts',(-2.52767129911716,-1.07458603724943,
7.50345484956));
#399152=CARTESIAN_POINT('Ctrl Pts',(-2.52800410105954,-1.07401849092751,
7.50349758195598));
#399153=CARTESIAN_POINT('Ctrl Pts',(-2.52817485313722,-1.07372729757403,
7.50351950684424));
#399154=CARTESIAN_POINT('Ctrl Pts',(-2.52835111967328,-1.07341251206196,
7.50357029184312));
#399155=CARTESIAN_POINT('Ctrl Pts',(-2.52851274764609,-1.07310429582408,
7.50365515313923));
#399156=CARTESIAN_POINT('Ctrl Pts',(-2.52876139691789,-1.07263013444114,
7.50378570417639));
#399157=CARTESIAN_POINT('Ctrl Pts',(-2.5289830075229,-1.07215776316925,
7.50400001621911));
#399158=CARTESIAN_POINT('Ctrl Pts',(-2.52915865622031,-1.07172217201528,
7.50428903009634));
#399159=CARTESIAN_POINT('Ctrl Pts',(-2.52917815187436,-1.07167382474842,
7.50432110841318));
#399160=CARTESIAN_POINT('Ctrl Pts',(-2.52919710660364,-1.07162591387536,
7.50435406373354));
#399161=CARTESIAN_POINT('Ctrl Pts',(-2.52921551303501,-1.07157847465112,
7.50438785222352));
#399162=CARTESIAN_POINT('Ctrl Pts',(-2.52932789314572,-1.07128883538495,
7.50459414719561));
#399163=CARTESIAN_POINT('Ctrl Pts',(-2.52942114279342,-1.07101197980953,
7.50483629897752));
#399164=CARTESIAN_POINT('Ctrl Pts',(-2.52949293679912,-1.07075893425429,
7.5050991045531));
#399165=CARTESIAN_POINT('Ctrl Pts',(-2.52965132158672,-1.07020069034342,
7.50567888004914));
#399166=CARTESIAN_POINT('Ctrl Pts',(-2.5297120261485,-1.06973647093188,
7.50637912803144));
#399167=CARTESIAN_POINT('Ctrl Pts',(-2.52970568282965,-1.06936214349217,
7.50710440483569));
#399168=CARTESIAN_POINT('Ctrl Pts',(-2.52970412732194,-1.06927035097251,
7.50728225710685));
#399169=CARTESIAN_POINT('Ctrl Pts',(-2.52969865500158,-1.06918213412398,
7.50746498566954));
#399170=CARTESIAN_POINT('Ctrl Pts',(-2.52968980940421,-1.06909952642055,
7.50764697238949));
#399171=CARTESIAN_POINT('Ctrl Pts',(-2.52964225790714,-1.06865545014116,
7.50862528291182));
#399172=CARTESIAN_POINT('Ctrl Pts',(-2.52949702291661,-1.06833271639992,
7.50965856837422));
#399173=CARTESIAN_POINT('Ctrl Pts',(-2.52930502796028,-1.06808887298636,
7.51067959873203));
#399174=CARTESIAN_POINT('Ctrl Pts',(-2.52919937289364,-1.06795468564831,
7.51124147302579));
#399175=CARTESIAN_POINT('Ctrl Pts',(-2.52907919034473,-1.06784462477278,
7.51180065547253));
#399176=CARTESIAN_POINT('Ctrl Pts',(-2.52895089547054,-1.06775337272155,
7.512351757165));
#399177=CARTESIAN_POINT('Ctrl Pts',(-2.52850758557362,-1.06743806053404,
7.51425603304535));
#399178=CARTESIAN_POINT('Ctrl Pts',(-2.52791104486855,-1.06731466841573,
7.51626900505179));
#399179=CARTESIAN_POINT('Ctrl Pts',(-2.52721446933284,-1.067354685748,7.51827788969242));
#399180=CARTESIAN_POINT('Ctrl Pts',(-2.5271767693485,-1.06735685156164,
7.51838661432544));
#399181=CARTESIAN_POINT('Ctrl Pts',(-2.52713876926094,-1.06735950303554,
7.51849533314856));
#399182=CARTESIAN_POINT('Ctrl Pts',(-2.52710047532067,-1.06736263792743,
7.51860402984325));
#399183=CARTESIAN_POINT('Ctrl Pts',(-2.44510882812078,-1.08237714566599,
7.57603338728985));
#399184=CARTESIAN_POINT('Ctrl Pts',(-2.47240630148851,-1.08018050713156,
7.55196141284922));
#399185=CARTESIAN_POINT('Ctrl Pts',(-2.49965666358482,-1.07798678628545,
7.52783573083105));
#399186=CARTESIAN_POINT('Ctrl Pts',(-2.52686377761629,-1.07579572641883,
7.50366116530176));
#399187=CARTESIAN_POINT('Origin',(-8.44898126352698E-16,-3.74011337523916E-16,
7.49482233047033));
#399188=CARTESIAN_POINT('Origin',(-2.48717010277293,-1.14363067896611,7.49482233047033));
#399189=CARTESIAN_POINT('Origin',(0.,0.,7.50366116523517));
#399190=CARTESIAN_POINT('Origin',(-2.51873130274448,-1.07233337846731,7.49482233047033));
#399191=CARTESIAN_POINT('Ctrl Pts',(-2.48911633021128,-1.15316718817922,
7.51860402984325));
#399192=CARTESIAN_POINT('Ctrl Pts',(-2.49375571485592,-1.15919814135008,
7.51860402984325));
#399193=CARTESIAN_POINT('Ctrl Pts',(-2.49052926869773,-1.16608917401713,
7.51860402984325));
#399194=CARTESIAN_POINT('Ctrl Pts',(-2.49083896438345,-1.15540652302373,
7.51041458714365));
#399195=CARTESIAN_POINT('Ctrl Pts',(-2.49299132384048,-1.16083070171987,
7.51004642900442));
#399196=CARTESIAN_POINT('Ctrl Pts',(-2.4905283788822,-1.16609107448211,
7.50729136483008));
#399197=CARTESIAN_POINT('Ctrl Pts',(-2.4935252160709,-1.15456522101442,
7.50215815450138));
#399198=CARTESIAN_POINT('Ctrl Pts',(-2.49454782737291,-1.1575067054367,
7.49877163671531));
#399199=CARTESIAN_POINT('Ctrl Pts',(-2.49310646793173,-1.16064141540026,
7.49481588533172));
#399200=CARTESIAN_POINT('Ctrl Pts',(-2.49520017266847,-1.1473230015279,
7.50366171572174));
#399201=CARTESIAN_POINT('Ctrl Pts',(-2.49852704388165,-1.14885273686058,
7.50000045605858));
#399202=CARTESIAN_POINT('Ctrl Pts',(-2.49852704388159,-1.1488527368607,
7.49482233047317));
#399203=CARTESIAN_POINT('Origin',(-2.47920868111274,-1.16078876868069,7.51860402984325));
#399204=CARTESIAN_POINT('Origin',(-2.47920868111274,-1.16078876868069,9.));
#399205=CARTESIAN_POINT('Origin',(-2.47920868111274,-1.16078876868069,8.75721825406948));
#399206=CARTESIAN_POINT('Ctrl Pts',(-2.47893554146576,-1.13993043652026,
8.78942910404913));
#399207=CARTESIAN_POINT('Ctrl Pts',(-2.48234884659824,-1.14433518132265,
8.7967269950169));
#399208=CARTESIAN_POINT('Ctrl Pts',(-2.47641733384219,-1.15100531193657,
8.79893251111267));
#399209=CARTESIAN_POINT('Ctrl Pts',(-2.48563834485611,-1.14864524262544,
8.78111911759582));
#399210=CARTESIAN_POINT('Ctrl Pts',(-2.48967897368034,-1.15387167820146,
8.78644465894816));
#399211=CARTESIAN_POINT('Ctrl Pts',(-2.48571656178288,-1.16094379271766,
8.78817647674132));
#399212=CARTESIAN_POINT('Ctrl Pts',(-2.48981569178069,-1.15407651767732,
8.76780923932031));
#399213=CARTESIAN_POINT('Ctrl Pts',(-2.49458145202817,-1.16024922097765,
8.76988516158372));
#399214=CARTESIAN_POINT('Ctrl Pts',(-2.49151654159844,-1.16715883055085,
8.77093053738833));
#399215=CARTESIAN_POINT('Ctrl Pts',(-2.48900116630003,-1.15301749337549,
8.75371302330492));
#399216=CARTESIAN_POINT('Ctrl Pts',(-2.49365056324086,-1.15903823331792,
8.75300828287559));
#399217=CARTESIAN_POINT('Ctrl Pts',(-2.4903849754574,-1.16594695792979,
8.75267964240738));
#399218=CARTESIAN_POINT('Origin',(-2.47065968314844,-1.14967358018056,8.78727029226991));
#399219=CARTESIAN_POINT('Ctrl Pts',(-2.43698193351378,-1.08538337893282,
8.85049129520029));
#399220=CARTESIAN_POINT('Ctrl Pts',(-2.44054210997315,-1.09001222930859,
8.85711686593484));
#399221=CARTESIAN_POINT('Ctrl Pts',(-2.43513294253591,-1.09663353354188,
8.85933012996512));
#399222=CARTESIAN_POINT('Ctrl Pts',(-2.45153175309123,-1.1043006822146,
8.82945683644722));
#399223=CARTESIAN_POINT('Ctrl Pts',(-2.45512148116771,-1.10896795484714,
8.83607469902389));
#399224=CARTESIAN_POINT('Ctrl Pts',(-2.44966738952774,-1.11558497282202,
8.83829567148519));
#399225=CARTESIAN_POINT('Ctrl Pts',(-2.46605988498928,-1.12318978773033,
8.80838214965001));
#399226=CARTESIAN_POINT('Ctrl Pts',(-2.4696637798088,-1.12787547959982,
8.81501364461991));
#399227=CARTESIAN_POINT('Ctrl Pts',(-2.46418031900404,-1.1345072569029,
8.81722098428721));
#399228=CARTESIAN_POINT('Ctrl Pts',(-2.48056797713151,-1.14205283806808,
8.78727029226991));
#399229=CARTESIAN_POINT('Ctrl Pts',(-2.48417247056978,-1.14673930824636,
8.79393457792714));
#399230=CARTESIAN_POINT('Ctrl Pts',(-2.47867338431574,-1.15340260064192,
8.79610912703474));
#399231=CARTESIAN_POINT('Origin',(-2.4270736395307,-1.0930041210453,8.85049129520029));
#399232=CARTESIAN_POINT('Ctrl Pts',(-2.44187055726728,-1.07433989271896,
8.85049129520029));
#399233=CARTESIAN_POINT('Ctrl Pts',(-2.44769070315533,-1.07386343278902,
8.85711686593484));
#399234=CARTESIAN_POINT('Ctrl Pts',(-2.44895572090755,-1.065407636422,8.85933012996512));
#399235=CARTESIAN_POINT('Ctrl Pts',(-2.43672155821481,-1.07476140994121,
8.8633249698723));
#399236=CARTESIAN_POINT('Ctrl Pts',(-2.43884661045463,-1.07065823466408,
8.86648636486738));
#399237=CARTESIAN_POINT('Ctrl Pts',(-2.43455258397725,-1.06660392356299,
8.87206031107458));
#399238=CARTESIAN_POINT('Ctrl Pts',(-2.4338108940174,-1.08126047448357,
8.86341338519877));
#399239=CARTESIAN_POINT('Ctrl Pts',(-2.43216978324604,-1.08559409030301,
8.86654584966058));
#399240=CARTESIAN_POINT('Ctrl Pts',(-2.4262655415925,-1.08508019996089,
8.87215952290714));
#399241=CARTESIAN_POINT('Ctrl Pts',(-2.43698193351378,-1.08538337893282,
8.85049129520029));
#399242=CARTESIAN_POINT('Ctrl Pts',(-2.44054210997315,-1.09001222930859,
8.85711686593484));
#399243=CARTESIAN_POINT('Ctrl Pts',(-2.43513294253591,-1.09663353354188,
8.85933012996512));
#399244=CARTESIAN_POINT('Origin',(-2.44085067010874,-1.06188156898806,8.85049129520029));
#399245=CARTESIAN_POINT('Ctrl Pts',(-2.51312464689844,-1.06850675396147,
8.78727029226991));
#399246=CARTESIAN_POINT('Ctrl Pts',(-2.51901724180286,-1.06802436307139,
8.79393457792714));
#399247=CARTESIAN_POINT('Ctrl Pts',(-2.52025288996715,-1.05947377310389,
8.79610912703474));
#399248=CARTESIAN_POINT('Ctrl Pts',(-2.48940694251248,-1.07044837810415,
8.80838214965003));
#399249=CARTESIAN_POINT('Ctrl Pts',(-2.4952985588001,-1.06996606732748,
8.81501364461992));
#399250=CARTESIAN_POINT('Ctrl Pts',(-2.49652138203831,-1.061448232161,8.81722098428721));
#399251=CARTESIAN_POINT('Ctrl Pts',(-2.46565647730583,-1.07239268417588,
8.82945683644723));
#399252=CARTESIAN_POINT('Ctrl Pts',(-2.47152493392369,-1.07191226934045,
8.8360746990239));
#399253=CARTESIAN_POINT('Ctrl Pts',(-2.47275657607162,-1.06342609822993,
8.83829567148519));
#399254=CARTESIAN_POINT('Ctrl Pts',(-2.44187055726728,-1.07433989271896,
8.85049129520029));
#399255=CARTESIAN_POINT('Ctrl Pts',(-2.44769070315533,-1.07386343278902,
8.85711686593484));
#399256=CARTESIAN_POINT('Ctrl Pts',(-2.44895572090755,-1.065407636422,8.85933012996512));
#399257=CARTESIAN_POINT('Origin',(-2.5121047597399,-1.05604843023057,8.78727029226991));
#399258=CARTESIAN_POINT('Ctrl Pts',(-2.52691593003166,-1.06737772701856,
8.75374538247847));
#399259=CARTESIAN_POINT('Ctrl Pts',(-2.53449062587209,-1.06677079925314,
8.75304829418602));
#399260=CARTESIAN_POINT('Ctrl Pts',(-2.53741166984649,-1.05971827167015,
8.75272238421917));
#399261=CARTESIAN_POINT('Ctrl Pts',(-2.52823151278631,-1.06727002869137,
8.76769408445023));
#399262=CARTESIAN_POINT('Ctrl Pts',(-2.53599676646443,-1.06664714002804,
8.76974318093966));
#399263=CARTESIAN_POINT('Ctrl Pts',(-2.53905110694683,-1.05974139158942,
8.7707786988043));
#399264=CARTESIAN_POINT('Ctrl Pts',(-2.52148858502513,-1.06782202897959,
8.78108014887987));
#399265=CARTESIAN_POINT('Ctrl Pts',(-2.5280696615764,-1.06729794050741,
8.78639403366329));
#399266=CARTESIAN_POINT('Ctrl Pts',(-2.53065603659667,-1.05962769018663,
8.78812224174741));
#399267=CARTESIAN_POINT('Ctrl Pts',(-2.51043841493816,-1.06872663556163,
8.78944554828686));
#399268=CARTESIAN_POINT('Ctrl Pts',(-2.51598514662683,-1.06829053329059,
8.79673892988684));
#399269=CARTESIAN_POINT('Ctrl Pts',(-2.51693670501845,-1.05942497685323,
8.79894799272499));
#399270=CARTESIAN_POINT('Origin',(-2.52608058816213,-1.05490431419653,8.75721825406948));
#399271=CARTESIAN_POINT('Origin',(-2.52608058816213,-1.05490431419653,9.));
#399272=CARTESIAN_POINT('Origin',(-2.52608058816213,-1.05490431419653,7.51860402984325));
#399273=CARTESIAN_POINT('Ctrl Pts',(-2.52686305376089,-1.07579541827704,
7.50366195182966));
#399274=CARTESIAN_POINT('Ctrl Pts',(-2.53023235892145,-1.07722987791223,
7.50000065167735));
#399275=CARTESIAN_POINT('Ctrl Pts',(-2.5302323589215,-1.07722987791213,
7.49482233047108));
#399276=CARTESIAN_POINT('Ctrl Pts',(-2.53110127804255,-1.06968057939568,
7.50215800491338));
#399277=CARTESIAN_POINT('Ctrl Pts',(-2.5339667452019,-1.06845837027566,
7.49877273257264));
#399278=CARTESIAN_POINT('Ctrl Pts',(-2.53531903262703,-1.06528213428478,
7.49481816995647));
#399279=CARTESIAN_POINT('Ctrl Pts',(-2.52990969086325,-1.06713300479694,
7.51043025814042));
#399280=CARTESIAN_POINT('Ctrl Pts',(-2.53537650996154,-1.06508199384297,
7.51006209594516));
#399281=CARTESIAN_POINT('Ctrl Pts',(-2.53761617838248,-1.05971889254554,
7.50731281821701));
#399282=CARTESIAN_POINT('Ctrl Pts',(-2.52709896894496,-1.06736276115356,
7.51860402984326));
#399283=CARTESIAN_POINT('Ctrl Pts',(-2.53468294567733,-1.06674283025942,
7.51860402984327));
#399284=CARTESIAN_POINT('Ctrl Pts',(-2.53761520271996,-1.05972122887323,
7.51860402984327));
#399285=CARTESIAN_POINT('Origin',(0.,0.,7.5));
#399286=CARTESIAN_POINT('Origin',(-2.36802027905702,-1.22858372995532,7.5));
#399287=CARTESIAN_POINT('',(-2.36802027905702,-1.22858372995532,7.59394543036555));
#399288=CARTESIAN_POINT('',(-2.36802027905702,-1.22858372995532,8.85049129520029));
#399289=CARTESIAN_POINT('',(-2.36802027905702,-1.22858372995532,7.5));
#399290=CARTESIAN_POINT('',(-2.43950170000242,-1.2273278412042,8.78727029226991));
#399291=CARTESIAN_POINT('Ctrl Pts',(-2.36802027905702,-1.22858372995532,
8.85049129520029));
#399292=CARTESIAN_POINT('Ctrl Pts',(-2.39188205442813,-1.22816449185297,
8.82945686509571));
#399293=CARTESIAN_POINT('Ctrl Pts',(-2.41570835638483,-1.22774587699876,
8.80838212259895));
#399294=CARTESIAN_POINT('Ctrl Pts',(-2.43950170000242,-1.2273278412042,
8.78727029226991));
#399295=CARTESIAN_POINT('',(-2.45352211735224,-1.22708151028068,8.75721825406948));
#399296=CARTESIAN_POINT('Origin',(-2.41132982137612,-1.22782300725359,8.75937679713158));
#399297=CARTESIAN_POINT('',(-2.45352211735224,-1.22708151028068,7.51860402984325));
#399298=CARTESIAN_POINT('',(-2.45352211735224,-1.22708151028068,7.5));
#399299=CARTESIAN_POINT('Ctrl Pts',(-2.45352211735224,-1.22708151028068,
7.51860402984325));
#399300=CARTESIAN_POINT('Ctrl Pts',(-2.44251126011132,-1.2272749649094,
7.52834476460825));
#399301=CARTESIAN_POINT('Ctrl Pts',(-2.43149325478076,-1.22746854512608,
7.53807742314407));
#399302=CARTESIAN_POINT('Ctrl Pts',(-2.42046786135394,-1.22766225514749,
7.54780169004674));
#399303=CARTESIAN_POINT('Ctrl Pts',(-2.40300423403754,-1.22796908135226,
7.5632044032688));
#399304=CARTESIAN_POINT('Ctrl Pts',(-2.3855220487349,-1.2282762336105,7.57858609112103));
#399305=CARTESIAN_POINT('Ctrl Pts',(-2.36802027905702,-1.22858372995532,
7.59394543036555));
#399306=CARTESIAN_POINT('Origin',(-2.51577981483217,-1.46756768793082,7.5));
#399307=CARTESIAN_POINT('',(-2.41011908817657,-1.31027699133286,8.75721825406948));
#399308=CARTESIAN_POINT('',(-2.40229980761779,-1.29863690399942,8.78727029226991));
#399309=CARTESIAN_POINT('Origin',(-2.38245155711314,-1.2690900208107,8.75658640621029));
#399310=CARTESIAN_POINT('',(-2.36243414091425,-1.23929131094305,8.85049129520029));
#399311=CARTESIAN_POINT('Ctrl Pts',(-2.40229980761779,-1.29863690399942,
8.78727029226991));
#399312=CARTESIAN_POINT('Ctrl Pts',(-2.38903010069429,-1.27888309847759,
8.80838212259896));
#399313=CARTESIAN_POINT('Ctrl Pts',(-2.37574201268454,-1.25910193015078,
8.82945686509571));
#399314=CARTESIAN_POINT('Ctrl Pts',(-2.36243414091425,-1.23929131094305,
8.85049129520029));
#399315=CARTESIAN_POINT('',(-2.36243414091425,-1.23929131094305,7.59394543036555));
#399316=CARTESIAN_POINT('',(-2.36243414091425,-1.23929131094305,7.5));
#399317=CARTESIAN_POINT('',(-2.41011908817657,-1.31027699133286,7.51860402984325));
#399318=CARTESIAN_POINT('Ctrl Pts',(-2.36243414091425,-1.23929131094305,
7.59394543036555));
#399319=CARTESIAN_POINT('Ctrl Pts',(-2.37219499495817,-1.25382170062099,
7.57858609112103));
#399320=CARTESIAN_POINT('Ctrl Pts',(-2.3819449266649,-1.2683358308799,7.56320440326857));
#399321=CARTESIAN_POINT('Ctrl Pts',(-2.39168450845863,-1.28283455385295,
7.54780169004651));
#399322=CARTESIAN_POINT('Ctrl Pts',(-2.39783344413752,-1.29198810036812,
7.53807742314383));
#399323=CARTESIAN_POINT('Ctrl Pts',(-2.40397825942581,-1.30113551310845,
7.52834476460825));
#399324=CARTESIAN_POINT('Ctrl Pts',(-2.41011908817657,-1.31027699133286,
7.51860402984325));
#399325=CARTESIAN_POINT('',(-2.41011908817657,-1.31027699133286,7.5));
#399326=CARTESIAN_POINT('Origin',(-2.36814105033894,-1.2354576690951,7.5));
#399327=CARTESIAN_POINT('Ctrl Pts',(-2.36243414091425,-1.23929131094305,
8.85049129520029));
#399328=CARTESIAN_POINT('Ctrl Pts',(-2.36232615126284,-1.23913055331784,
8.85097269580138));
#399329=CARTESIAN_POINT('Ctrl Pts',(-2.36222650637989,-1.23896713357045,
8.85143669361005));
#399330=CARTESIAN_POINT('Ctrl Pts',(-2.36213136440492,-1.23879307159445,
8.8519052845931));
#399331=CARTESIAN_POINT('Ctrl Pts',(-2.36194527273555,-1.238452617408,8.85282181883899));
#399332=CARTESIAN_POINT('Ctrl Pts',(-2.36178136762876,-1.23808011298295,
8.85372622499636));
#399333=CARTESIAN_POINT('Ctrl Pts',(-2.36165119009122,-1.23766350326387,
8.85462257735071));
#399334=CARTESIAN_POINT('Ctrl Pts',(-2.36154312132302,-1.23731764867168,
8.85536669723986));
#399335=CARTESIAN_POINT('Ctrl Pts',(-2.36145824187889,-1.23694132846308,
8.85610498449051));
#399336=CARTESIAN_POINT('Ctrl Pts',(-2.36141095400462,-1.23652585282808,
8.85681338218371));
#399337=CARTESIAN_POINT('Ctrl Pts',(-2.36136804018445,-1.2361488080368,
8.85745625420284));
#399338=CARTESIAN_POINT('Ctrl Pts',(-2.36135495228239,-1.23573485447991,
8.85808743050665));
#399339=CARTESIAN_POINT('Ctrl Pts',(-2.36139708325078,-1.23527083753392,
8.8586680450841));
#399340=CARTESIAN_POINT('Ctrl Pts',(-2.36141652156631,-1.23505675017369,
8.85893592806395));
#399341=CARTESIAN_POINT('Ctrl Pts',(-2.3614479412895,-1.23483192081263,
8.85919241173848));
#399342=CARTESIAN_POINT('Ctrl Pts',(-2.36149539461714,-1.23459471186785,
8.85943017985534));
#399343=CARTESIAN_POINT('Ctrl Pts',(-2.36155947065714,-1.23427440957102,
8.8597512372));
#399344=CARTESIAN_POINT('Ctrl Pts',(-2.36165503976701,-1.23392350871098,
8.86004599534705));
#399345=CARTESIAN_POINT('Ctrl Pts',(-2.36179100277735,-1.23354896212652,
8.86026130871721));
#399346=CARTESIAN_POINT('Ctrl Pts',(-2.36184078266865,-1.23341183006237,
8.86034014101235));
#399347=CARTESIAN_POINT('Ctrl Pts',(-2.36189671351937,-1.23326946421363,
8.86040910639693));
#399348=CARTESIAN_POINT('Ctrl Pts',(-2.36195758460882,-1.23312586625831,
8.86046313645507));
#399349=CARTESIAN_POINT('Ctrl Pts',(-2.36205257343412,-1.23290178285164,
8.8605474499083));
#399350=CARTESIAN_POINT('Ctrl Pts',(-2.3621623206917,-1.23266863968503,
8.86059655985668));
#399351=CARTESIAN_POINT('Ctrl Pts',(-2.36227952289683,-1.23244126416859,
8.86059725258816));
#399352=CARTESIAN_POINT('Ctrl Pts',(-2.36239699588587,-1.23221336332386,
8.86059794692011));
#399353=CARTESIAN_POINT('Ctrl Pts',(-2.36252562260629,-1.23198994662061,
8.86056369958366));
#399354=CARTESIAN_POINT('Ctrl Pts',(-2.36265512646351,-1.23178132174017,
8.86048590497774));
#399355=CARTESIAN_POINT('Ctrl Pts',(-2.36268892311445,-1.23172687685788,
8.86046560290182));
#399356=CARTESIAN_POINT('Ctrl Pts',(-2.36272329613576,-1.23167277885392,
8.86044257503091));
#399357=CARTESIAN_POINT('Ctrl Pts',(-2.36275715566619,-1.23162068179715,
8.86041778462583));
#399358=CARTESIAN_POINT('Ctrl Pts',(-2.36298498828978,-1.23127013325215,
8.86025097596201));
#399359=CARTESIAN_POINT('Ctrl Pts',(-2.36322042239,-1.23096332188231,8.8599848982295));
#399360=CARTESIAN_POINT('Ctrl Pts',(-2.36344986468683,-1.23070404485063,
8.85968173251462));
#399361=CARTESIAN_POINT('Ctrl Pts',(-2.36357122651638,-1.23056690215567,
8.85952137522077));
#399362=CARTESIAN_POINT('Ctrl Pts',(-2.36369310828823,-1.23044028856094,
8.85934740853961));
#399363=CARTESIAN_POINT('Ctrl Pts',(-2.36381267123703,-1.2303249114905,
8.8591675900182));
#399364=CARTESIAN_POINT('Ctrl Pts',(-2.36429277862405,-1.22986161258083,
8.85844552518694));
#399365=CARTESIAN_POINT('Ctrl Pts',(-2.36476052976299,-1.22955113387645,
8.85759444184121));
#399366=CARTESIAN_POINT('Ctrl Pts',(-2.3651646468264,-1.22933224199772,
8.85683498915135));
#399367=CARTESIAN_POINT('Ctrl Pts',(-2.36520693660083,-1.22930933554557,
8.85675551444996));
#399368=CARTESIAN_POINT('Ctrl Pts',(-2.36524853540331,-1.22928745114724,
8.8566769979365));
#399369=CARTESIAN_POINT('Ctrl Pts',(-2.36528938769014,-1.22926653136241,
8.85659965593547));
#399370=CARTESIAN_POINT('Ctrl Pts',(-2.36584081394239,-1.22898415503921,
8.85555568965886));
#399371=CARTESIAN_POINT('Ctrl Pts',(-2.366411549463,-1.22879241075993,8.85434650606346));
#399372=CARTESIAN_POINT('Ctrl Pts',(-2.36700243645268,-1.22868445948991,
8.85297329937117));
#399373=CARTESIAN_POINT('Ctrl Pts',(-2.36733477438111,-1.22862374347808,
8.85220095427747));
#399374=CARTESIAN_POINT('Ctrl Pts',(-2.36767367938264,-1.22858981951854,
8.85137579139183));
#399375=CARTESIAN_POINT('Ctrl Pts',(-2.36802027905702,-1.22858372995532,
8.85049129520029));
#399376=CARTESIAN_POINT('Origin',(-2.36814105033894,-1.2354576690951,7.59394543036555));
#399377=CARTESIAN_POINT('Ctrl Pts',(-2.36212061052625,-1.238824577326,7.59443877723642));
#399378=CARTESIAN_POINT('Ctrl Pts',(-2.35889154920073,-1.23401767014937,
7.58783886950016));
#399379=CARTESIAN_POINT('Ctrl Pts',(-2.36465235257834,-1.22778129893036,
7.58559994247159));
#399380=CARTESIAN_POINT('Ctrl Pts',(-2.37974796156563,-1.26506534257455,
7.56670252222136));
#399381=CARTESIAN_POINT('Ctrl Pts',(-2.3765235671505,-1.26026538274347,
7.56004874999025));
#399382=CARTESIAN_POINT('Ctrl Pts',(-2.3823028110065,-1.25397756136332,
7.55786368756704));
#399383=CARTESIAN_POINT('Ctrl Pts',(-2.39734239528812,-1.29125710581576,
7.53888913333556));
#399384=CARTESIAN_POINT('Ctrl Pts',(-2.39409883813908,-1.28642861958838,
7.53222002137273));
#399385=CARTESIAN_POINT('Ctrl Pts',(-2.39991996700693,-1.28012648475776,
7.53005029815327));
#399386=CARTESIAN_POINT('Ctrl Pts',(-2.41490311553373,-1.31739868185466,
7.51101258149734));
#399387=CARTESIAN_POINT('Ctrl Pts',(-2.41162024057835,-1.31251166560067,
7.5043616886572));
#399388=CARTESIAN_POINT('Ctrl Pts',(-2.41750301869742,-1.30622673098315,
7.50217374673251));
#399389=CARTESIAN_POINT('',(-2.41656476362037,-1.30483398889127,7.50366116523517));
#399390=CARTESIAN_POINT('Ctrl Pts',(-2.41011908817657,-1.31027699133286,
7.51860402984325));
#399391=CARTESIAN_POINT('Ctrl Pts',(-2.41036533970193,-1.31064357099956,
7.51734760759493));
#399392=CARTESIAN_POINT('Ctrl Pts',(-2.41063725122379,-1.31094165149919,
7.51608817408572));
#399393=CARTESIAN_POINT('Ctrl Pts',(-2.41094406290928,-1.31116154777588,
7.51481005913119));
#399394=CARTESIAN_POINT('Ctrl Pts',(-2.4112219802655,-1.31136073507789,
7.51365231206383));
#399395=CARTESIAN_POINT('Ctrl Pts',(-2.41152877981015,-1.3114962550091,
7.51247773061042));
#399396=CARTESIAN_POINT('Ctrl Pts',(-2.41187407264667,-1.31153198601554,
7.51129758471022));
#399397=CARTESIAN_POINT('Ctrl Pts',(-2.41230323220854,-1.3115763955759,
7.50983079813402));
#399398=CARTESIAN_POINT('Ctrl Pts',(-2.41277949901876,-1.31145228193425,
7.50839324291155));
#399399=CARTESIAN_POINT('Ctrl Pts',(-2.41328555985522,-1.31107896397255,
7.50715379678855));
#399400=CARTESIAN_POINT('Ctrl Pts',(-2.41351934537987,-1.31090650183114,
7.50658120839351));
#399401=CARTESIAN_POINT('Ctrl Pts',(-2.41378708356349,-1.31064869179563,
7.50598221009429));
#399402=CARTESIAN_POINT('Ctrl Pts',(-2.41406662507935,-1.31029528425857,
7.50545747549611));
#399403=CARTESIAN_POINT('Ctrl Pts',(-2.41421579708484,-1.31010669505781,
7.50517746087247));
#399404=CARTESIAN_POINT('Ctrl Pts',(-2.41437010660959,-1.30988896396753,
7.50491486231392));
#399405=CARTESIAN_POINT('Ctrl Pts',(-2.41452410638099,-1.30964689238472,
7.50468370960993));
#399406=CARTESIAN_POINT('Ctrl Pts',(-2.41475438461572,-1.30928491901126,
7.50433806340447));
#399407=CARTESIAN_POINT('Ctrl Pts',(-2.41499040573442,-1.3088573680573,
7.50405484070983));
#399408=CARTESIAN_POINT('Ctrl Pts',(-2.41521564697535,-1.30839268806317,
7.50385766036131));
#399409=CARTESIAN_POINT('Ctrl Pts',(-2.41523973302503,-1.30834299776056,
7.50383657498791));
#399410=CARTESIAN_POINT('Ctrl Pts',(-2.41526369813398,-1.30829291115476,
7.50381643264937));
#399411=CARTESIAN_POINT('Ctrl Pts',(-2.41528752410889,-1.30824248354154,
7.50379723213559));
#399412=CARTESIAN_POINT('Ctrl Pts',(-2.41544657028544,-1.30790586272728,
7.50366906242519));
#399413=CARTESIAN_POINT('Ctrl Pts',(-2.41560222613725,-1.30754641716599,
7.50358235568538));
#399414=CARTESIAN_POINT('Ctrl Pts',(-2.41574393100536,-1.30719634939656,
7.5035341175365));
#399415=CARTESIAN_POINT('Ctrl Pts',(-2.41595640141719,-1.30667146239633,
7.50346178989176));
#399416=CARTESIAN_POINT('Ctrl Pts',(-2.41616265364207,-1.30609776943105,
7.50346967198527));
#399417=CARTESIAN_POINT('Ctrl Pts',(-2.41634780009116,-1.30552835049683,
7.50354272648692));
#399418=CARTESIAN_POINT('Ctrl Pts',(-2.41642395465797,-1.30529413670291,
7.50357277531559));
#399419=CARTESIAN_POINT('Ctrl Pts',(-2.41649657211345,-1.30506100104882,
7.50361331098761));
#399420=CARTESIAN_POINT('Ctrl Pts',(-2.41656476362162,-1.30483398889194,
7.50366116523659));
#399421=CARTESIAN_POINT('',(-2.37073694677504,-1.23681194660284,7.57603338622103));
#399422=CARTESIAN_POINT('Origin',(-2.37857308999325,-1.24089683938842,7.58486873427628));
#399423=CARTESIAN_POINT('Ctrl Pts',(-2.41656476364782,-1.30483398894162,
7.50366116529969));
#399424=CARTESIAN_POINT('Ctrl Pts',(-2.40131444507885,-1.2821965071394,
7.52783573079709));
#399425=CARTESIAN_POINT('Ctrl Pts',(-2.38603924224883,-1.25952355358678,
7.55196141284069));
#399426=CARTESIAN_POINT('Ctrl Pts',(-2.37073694715285,-1.23681194779654,
7.57603338728831));
#399427=CARTESIAN_POINT('Ctrl Pts',(-2.36243414091425,-1.23929131094305,
7.59394543036555));
#399428=CARTESIAN_POINT('Ctrl Pts',(-2.35539033864858,-1.22880563097346,
7.59394543036555));
#399429=CARTESIAN_POINT('Ctrl Pts',(-2.36802027905701,-1.22858372995532,
7.59394543036555));
#399430=CARTESIAN_POINT('Ctrl Pts',(-2.36113314698054,-1.23735460041134,
7.58587155981958));
#399431=CARTESIAN_POINT('Ctrl Pts',(-2.36057594445157,-1.23151095819934,
7.58685956158229));
#399432=CARTESIAN_POINT('Ctrl Pts',(-2.36568752250954,-1.22862471518852,
7.5858715598196));
#399433=CARTESIAN_POINT('Ctrl Pts',(-2.36649208760835,-1.23674115119295,
7.57982961904598));
#399434=CARTESIAN_POINT('Ctrl Pts',(-2.36590782788217,-1.23429259836977,
7.58148017275035));
#399435=CARTESIAN_POINT('Ctrl Pts',(-2.36825032769483,-1.2333709341234,
7.57982961904596));
#399436=CARTESIAN_POINT('Ctrl Pts',(-2.37073694604122,-1.23681194622024,
7.57603338509286));
#399437=CARTESIAN_POINT('Ctrl Pts',(-2.37073694604122,-1.23681194622024,
7.57603338509286));
#399438=CARTESIAN_POINT('Ctrl Pts',(-2.37073694604122,-1.23681194622024,
7.57603338509286));
#399439=CARTESIAN_POINT('Origin',(-2.37857045058693,-1.24090189863649,7.5848687342762));
#399440=CARTESIAN_POINT('Ctrl Pts',(-2.46212726359303,-1.22693032265427,
7.51098857897448));
#399441=CARTESIAN_POINT('Ctrl Pts',(-2.45624085415416,-1.2270337435894,
7.50433767179956));
#399442=CARTESIAN_POINT('Ctrl Pts',(-2.45445176918726,-1.23545438644275,
7.50214974420965));
#399443=CARTESIAN_POINT('Ctrl Pts',(-2.43063083103924,-1.22748369743084,
7.5388732158917));
#399444=CARTESIAN_POINT('Ctrl Pts',(-2.42481495123192,-1.22758587919962,
7.53220407452063));
#399445=CARTESIAN_POINT('Ctrl Pts',(-2.42297646352332,-1.23596578867809,
7.53003438070912));
#399446=CARTESIAN_POINT('Ctrl Pts',(-2.39907391371632,-1.22803813489112,
7.5666946565923));
#399447=CARTESIAN_POINT('Ctrl Pts',(-2.39329240467737,-1.22813971278464,
7.56004085833294));
#399448=CARTESIAN_POINT('Ctrl Pts',(-2.39144168852526,-1.23647706847156,
7.55785582193789));
#399449=CARTESIAN_POINT('Ctrl Pts',(-2.36745793881747,-1.22859360996011,
7.59443891967696));
#399450=CARTESIAN_POINT('Ctrl Pts',(-2.36166804731027,-1.22869533512894,
7.58783901202978));
#399451=CARTESIAN_POINT('Ctrl Pts',(-2.35984900020427,-1.23698811787145,
7.58560008491213));
#399452=CARTESIAN_POINT('',(-2.45274559607508,-1.23548210681974,7.50366116523517));
#399453=CARTESIAN_POINT('Ctrl Pts',(-2.45274559607542,-1.23548210681991,
7.50366116523554));
#399454=CARTESIAN_POINT('Ctrl Pts',(-2.45321593518388,-1.23488803726184,
7.50350835821027));
#399455=CARTESIAN_POINT('Ctrl Pts',(-2.45362896354645,-1.23432664116028,
7.50345484956));
#399456=CARTESIAN_POINT('Ctrl Pts',(-2.45399744452925,-1.2337815836168,
7.50349758195598));
#399457=CARTESIAN_POINT('Ctrl Pts',(-2.45418650260068,-1.23350192867448,
7.50351950684424));
#399458=CARTESIAN_POINT('Ctrl Pts',(-2.45438257535525,-1.23319908335874,
7.50357029184312));
#399459=CARTESIAN_POINT('Ctrl Pts',(-2.45456361872821,-1.23290185592395,
7.50365515313924));
#399460=CARTESIAN_POINT('Ctrl Pts',(-2.45484213674753,-1.23244459976998,
7.50378570417639));
#399461=CARTESIAN_POINT('Ctrl Pts',(-2.45509355696109,-1.23198739767573,
7.50400001621911));
#399462=CARTESIAN_POINT('Ctrl Pts',(-2.45529675319047,-1.23156395534119,
7.50428903009634));
#399463=CARTESIAN_POINT('Ctrl Pts',(-2.45531930640863,-1.23151695649982,
7.50432110841318));
#399464=CARTESIAN_POINT('Ctrl Pts',(-2.45534129185356,-1.23147035849846,
7.50435406373354));
#399465=CARTESIAN_POINT('Ctrl Pts',(-2.45536269990847,-1.2314241960473,
7.50438785222352));
#399466=CARTESIAN_POINT('Ctrl Pts',(-2.4554934063737,-1.23114235209449,
7.50459414719561));
#399467=CARTESIAN_POINT('Ctrl Pts',(-2.45560420262761,-1.23087203987398,
7.50483629897752));
#399468=CARTESIAN_POINT('Ctrl Pts',(-2.45569206180922,-1.23062411408571,
7.5050991045531));
#399469=CARTESIAN_POINT('Ctrl Pts',(-2.45588588798846,-1.23007716489501,
7.50567888004914));
#399470=CARTESIAN_POINT('Ctrl Pts',(-2.45597621046602,-1.22961778862667,
7.50637912803144));
#399471=CARTESIAN_POINT('Ctrl Pts',(-2.4559938634216,-1.22924382386499,
7.50710440483569));
#399472=CARTESIAN_POINT('Ctrl Pts',(-2.45599819227677,-1.22915212028119,
7.50728225710685));
#399473=CARTESIAN_POINT('Ctrl Pts',(-2.45599838327278,-1.22906373407087,
7.50746498566954));
#399474=CARTESIAN_POINT('Ctrl Pts',(-2.45599484854337,-1.22898072935445,
7.50764697238949));
#399475=CARTESIAN_POINT('Ctrl Pts',(-2.45597584681086,-1.22853451884254,
7.50862528291181));
#399476=CARTESIAN_POINT('Ctrl Pts',(-2.45585158784299,-1.22820314295458,
7.50965856837421));
#399477=CARTESIAN_POINT('Ctrl Pts',(-2.45567561046203,-1.22794749938438,
7.51067959873201));
#399478=CARTESIAN_POINT('Ctrl Pts',(-2.45557876988733,-1.22780681840524,
7.51124147302578));
#399479=CARTESIAN_POINT('Ctrl Pts',(-2.45546588589086,-1.22768928353924,
7.51180065547252));
#399480=CARTESIAN_POINT('Ctrl Pts',(-2.45534370115125,-1.22758999909432,
7.51235175716501));
#399481=CARTESIAN_POINT('Ctrl Pts',(-2.45492150420326,-1.2272469317869,
7.51425603304537));
#399482=CARTESIAN_POINT('Ctrl Pts',(-2.45433409491521,-1.22708557269673,
7.51626900505184));
#399483=CARTESIAN_POINT('Ctrl Pts',(-2.45363638664935,-1.22708087806129,
7.51827788969249));
#399484=CARTESIAN_POINT('Ctrl Pts',(-2.45359862535952,-1.22708062397875,
7.51838661432549));
#399485=CARTESIAN_POINT('Ctrl Pts',(-2.45356053346671,-1.22708083533095,
7.51849533314858));
#399486=CARTESIAN_POINT('Ctrl Pts',(-2.45352211735224,-1.22708151028068,
7.51860402984325));
#399487=CARTESIAN_POINT('Ctrl Pts',(-2.37073694797139,-1.23681194623012,
7.57603338728985));
#399488=CARTESIAN_POINT('Ctrl Pts',(-2.39811907486656,-1.23636877604872,
7.55196141284922));
#399489=CARTESIAN_POINT('Ctrl Pts',(-2.42545400034854,-1.23592549913143,
7.52783573083105));
#399490=CARTESIAN_POINT('Ctrl Pts',(-2.45274559613392,-1.23548210681335,
7.50366116530176));
#399491=CARTESIAN_POINT('Origin',(-8.19199203866628E-16,-4.27375699935092E-16,
7.49482233047033));
#399492=CARTESIAN_POINT('Origin',(-2.40878727587058,-1.30063450269628,7.49482233047033));
#399493=CARTESIAN_POINT('Origin',(0.,0.,7.50366116523517));
#399494=CARTESIAN_POINT('Origin',(-2.44485166369885,-1.231505823173,7.49482233047033));
#399495=CARTESIAN_POINT('Ctrl Pts',(-2.41011849833278,-1.31027611334853,
7.51860402984325));
#399496=CARTESIAN_POINT('Ctrl Pts',(-2.41436194636776,-1.31659192167404,
7.51860402984325));
#399497=CARTESIAN_POINT('Ctrl Pts',(-2.41070061931036,-1.32326207686031,
7.51860402984325));
#399498=CARTESIAN_POINT('Ctrl Pts',(-2.4116941184922,-1.31262121678979,
7.51041458714366));
#399499=CARTESIAN_POINT('Ctrl Pts',(-2.41349452737362,-1.31817215307297,
7.51004642900442));
#399500=CARTESIAN_POINT('Ctrl Pts',(-2.41069960955983,-1.32326391640991,
7.5072913648301));
#399501=CARTESIAN_POINT('Ctrl Pts',(-2.41442875339229,-1.31195375206223,
7.50215815450137));
#399502=CARTESIAN_POINT('Ctrl Pts',(-2.41526080207569,-1.31495471182036,
7.49877163671531));
#399503=CARTESIAN_POINT('Ctrl Pts',(-2.41362156250511,-1.31799063296964,
7.4948158853317));
#399504=CARTESIAN_POINT('Ctrl Pts',(-2.41656427920751,-1.30483372733004,
7.50366171572174));
#399505=CARTESIAN_POINT('Ctrl Pts',(-2.41978630452771,-1.30657347302789,
7.50000045605858));
#399506=CARTESIAN_POINT('Ctrl Pts',(-2.41978630452765,-1.306573473028,7.49482233047317));
#399507=CARTESIAN_POINT('Origin',(-2.39974288922259,-1.31724724923822,7.51860402984325));
#399508=CARTESIAN_POINT('Origin',(-2.39974288922259,-1.31724724923822,9.));
#399509=CARTESIAN_POINT('Origin',(-2.39974288922259,-1.31724724923822,8.75721825406948));
#399510=CARTESIAN_POINT('Ctrl Pts',(-2.40080670870025,-1.29641427264099,
8.78942910404913));
#399511=CARTESIAN_POINT('Ctrl Pts',(-2.40393078786281,-1.30102865863348,
8.7967269950169));
#399512=CARTESIAN_POINT('Ctrl Pts',(-2.39758410530013,-1.30730505142159,
8.79893251111266));
#399513=CARTESIAN_POINT('Ctrl Pts',(-2.40693738091791,-1.30554062333008,
8.78111911759582));
#399514=CARTESIAN_POINT('Ctrl Pts',(-2.41063484895981,-1.31101520461129,
8.78644465894813));
#399515=CARTESIAN_POINT('Ctrl Pts',(-2.40622746632977,-1.31781891610782,
8.78817647674133));
#399516=CARTESIAN_POINT('Ctrl Pts',(-2.41075816204787,-1.31122838278126,
8.76780923932031));
#399517=CARTESIAN_POINT('Ctrl Pts',(-2.41511864407147,-1.31769374690807,
8.76988516158374));
#399518=CARTESIAN_POINT('Ctrl Pts',(-2.41161733062359,-1.32439279046189,
8.77093053738832));
#399519=CARTESIAN_POINT('Ctrl Pts',(-2.41001316201716,-1.31011934753171,
8.75371302330492));
#399520=CARTESIAN_POINT('Ctrl Pts',(-2.41426725614076,-1.31642560510298,
8.75300828287559));
#399521=CARTESIAN_POINT('Ctrl Pts',(-2.41056573435197,-1.32311090807153,
8.75267964240738));
#399522=CARTESIAN_POINT('Origin',(-2.3919236086638,-1.30560716190478,8.78727029226991));
#399523=CARTESIAN_POINT('Ctrl Pts',(-2.36243414091425,-1.23929131094305,
8.85049129520029));
#399524=CARTESIAN_POINT('Ctrl Pts',(-2.36569043114742,-1.2441387521382,
8.85711686593484));
#399525=CARTESIAN_POINT('Ctrl Pts',(-2.35986814900602,-1.2503998856442,
8.85933012996512));
#399526=CARTESIAN_POINT('Ctrl Pts',(-2.37574203054419,-1.25910195673735,
8.82945683644722));
#399527=CARTESIAN_POINT('Ctrl Pts',(-2.3790253499551,-1.26398963462525,
8.83607469902389));
#399528=CARTESIAN_POINT('Ctrl Pts',(-2.37315851053407,-1.27024361237588,
8.83829567148519));
#399529=CARTESIAN_POINT('Ctrl Pts',(-2.38903008369151,-1.2788830731666,
8.80838214965002));
#399530=CARTESIAN_POINT('Ctrl Pts',(-2.39232636061376,-1.28379004011343,
8.81501364461988));
#399531=CARTESIAN_POINT('Ctrl Pts',(-2.38642926673664,-1.2900568651788,
8.81722098428721));
#399532=CARTESIAN_POINT('Ctrl Pts',(-2.40229980761779,-1.29863690399942,
8.78727029226991));
#399533=CARTESIAN_POINT('Ctrl Pts',(-2.40559663206246,-1.3035446860096,
8.79393457792714));
#399534=CARTESIAN_POINT('Ctrl Pts',(-2.39968192566132,-1.30984196029031,
8.79610912703474));
#399535=CARTESIAN_POINT('Origin',(-2.35205794196026,-1.24626156884841,8.85049129520029));
#399536=CARTESIAN_POINT('Ctrl Pts',(-2.36802027905702,-1.22858372995532,
8.85049129520029));
#399537=CARTESIAN_POINT('Ctrl Pts',(-2.37385899372366,-1.22848114699077,
8.85711686593484));
#399538=CARTESIAN_POINT('Ctrl Pts',(-2.37566317709458,-1.22012377392993,
8.85933012996512));
#399539=CARTESIAN_POINT('Ctrl Pts',(-2.36285485247417,-1.22867448362326,
8.86332496987232));
#399540=CARTESIAN_POINT('Ctrl Pts',(-2.36523842990886,-1.22471589132427,
8.86648636486737));
#399541=CARTESIAN_POINT('Ctrl Pts',(-2.36121298657355,-1.22039479101916,
8.87206031107457));
#399542=CARTESIAN_POINT('Ctrl Pts',(-2.35953377205362,-1.23497370824507,
8.86341338519875));
#399543=CARTESIAN_POINT('Ctrl Pts',(-2.3576183774015,-1.23919327385791,
8.86654584966058));
#399544=CARTESIAN_POINT('Ctrl Pts',(-2.35175919171291,-1.23830215329704,
8.87215952290714));
#399545=CARTESIAN_POINT('Ctrl Pts',(-2.36243414091425,-1.23929131094305,
8.85049129520029));
#399546=CARTESIAN_POINT('Ctrl Pts',(-2.36569043114742,-1.2441387521382,
8.85711686593484));
#399547=CARTESIAN_POINT('Ctrl Pts',(-2.35986814900602,-1.2503998856442,
8.85933012996512));
#399548=CARTESIAN_POINT('Origin',(-2.36780069490806,-1.21608565879207,8.85049129520029));
#399549=CARTESIAN_POINT('Ctrl Pts',(-2.43950170000242,-1.2273278412042,
8.78727029226991));
#399550=CARTESIAN_POINT('Ctrl Pts',(-2.44541309482908,-1.22722398128972,
8.79393457792714));
#399551=CARTESIAN_POINT('Ctrl Pts',(-2.44719404240188,-1.21877012767606,
8.79610912703474));
#399552=CARTESIAN_POINT('Ctrl Pts',(-2.41570832589788,-1.22774587753439,
8.80838214965002));
#399553=CARTESIAN_POINT('Ctrl Pts',(-2.42161873898549,-1.22764203486851,
8.81501364461987));
#399554=CARTESIAN_POINT('Ctrl Pts',(-2.42338478937514,-1.21922004706179,
8.81722098428721));
#399555=CARTESIAN_POINT('Ctrl Pts',(-2.39188208645153,-1.22816449129034,
8.82945683644722));
#399556=CARTESIAN_POINT('Ctrl Pts',(-2.39776926598008,-1.22806105682515,
8.83607469902391));
#399557=CARTESIAN_POINT('Ctrl Pts',(-2.39954208843695,-1.21967123304667,
8.8382956714852));
#399558=CARTESIAN_POINT('Ctrl Pts',(-2.36802027905702,-1.22858372995532,
8.85049129520029));
#399559=CARTESIAN_POINT('Ctrl Pts',(-2.37385899372366,-1.22848114699077,
8.85711686593484));
#399560=CARTESIAN_POINT('Ctrl Pts',(-2.37566317709458,-1.22012377392993,
8.85933012996512));
#399561=CARTESIAN_POINT('Origin',(-2.43928211585347,-1.21482977004095,8.78727029226991));
#399562=CARTESIAN_POINT('Ctrl Pts',(-2.45333698446993,-1.22708474451239,
8.75374538247849));
#399563=CARTESIAN_POINT('Ctrl Pts',(-2.46093500328082,-1.22696437617394,
8.75304829418602));
#399564=CARTESIAN_POINT('Ctrl Pts',(-2.46430190265075,-1.22011349069528,
8.75272238421917));
#399565=CARTESIAN_POINT('Ctrl Pts',(-2.45465676447428,-1.22706155713946,
8.76769408445017));
#399566=CARTESIAN_POINT('Ctrl Pts',(-2.46244597221954,-1.22693746977904,
8.76974318093968));
#399567=CARTESIAN_POINT('Ctrl Pts',(-2.46593649005344,-1.22024160220782,
8.77077869880429));
#399568=CARTESIAN_POINT('Ctrl Pts',(-2.44789232400141,-1.22718040241891,
8.78108014887994));
#399569=CARTESIAN_POINT('Ctrl Pts',(-2.45449345748878,-1.22707904176505,
8.78639403366326));
#399570=CARTESIAN_POINT('Ctrl Pts',(-2.45756595314955,-1.2195902604127,
8.78812224174742));
#399571=CARTESIAN_POINT('Ctrl Pts',(-2.43680689933132,-1.22737516356142,
8.78944554828685));
#399572=CARTESIAN_POINT('Ctrl Pts',(-2.44237017583329,-1.22729533762872,
8.79673892988686));
#399573=CARTESIAN_POINT('Ctrl Pts',(-2.44388779729733,-1.21850896298338,
8.79894799272499));
#399574=CARTESIAN_POINT('Origin',(-2.45330253320329,-1.21458343911744,8.75721825406948));
#399575=CARTESIAN_POINT('Origin',(-2.45330253320329,-1.21458343911744,9.));
#399576=CARTESIAN_POINT('Origin',(-2.45330253320329,-1.21458343911744,7.51860402984325));
#399577=CARTESIAN_POINT('Ctrl Pts',(-2.45274489350846,-1.23548175292708,
7.50366195182967));
#399578=CARTESIAN_POINT('Ctrl Pts',(-2.45601536992584,-1.23712913743394,
7.50000065167736));
#399579=CARTESIAN_POINT('Ctrl Pts',(-2.4560153699259,-1.23712913743383,
7.49482233047108));
#399580=CARTESIAN_POINT('Ctrl Pts',(-2.45736618897609,-1.22965102160009,
7.50215800491335));
#399581=CARTESIAN_POINT('Ctrl Pts',(-2.46030407593303,-1.22861491475103,
7.49877273257261));
#399582=CARTESIAN_POINT('Ctrl Pts',(-2.46185708707724,-1.22553184603044,
7.49481816995644));
#399583=CARTESIAN_POINT('Ctrl Pts',(-2.45634027370535,-1.22703233601387,
7.51043025814045));
#399584=CARTESIAN_POINT('Ctrl Pts',(-2.46192726936052,-1.22533579938412,
7.51006209594519));
#399585=CARTESIAN_POINT('Ctrl Pts',(-2.46450595122239,-1.2201272132019,
7.50731281821703));
#399586=CARTESIAN_POINT('Ctrl Pts',(-2.45352060617641,-1.22708153673981,
7.51860402984326));
#399587=CARTESIAN_POINT('Ctrl Pts',(-2.46112871992397,-1.22694878661776,
7.51860402984326));
#399588=CARTESIAN_POINT('Ctrl Pts',(-2.46450482787545,-1.22012948221843,
7.51860402984327));
#399589=CARTESIAN_POINT('Origin',(0.,0.,7.5));
#399590=CARTESIAN_POINT('Origin',(-2.28443929758135,-1.37777905311491,7.5));
#399591=CARTESIAN_POINT('',(-2.28443929758135,-1.37777905311491,7.59394543036555));
#399592=CARTESIAN_POINT('',(-2.28443929758135,-1.37777905311491,8.85049129520029));
#399593=CARTESIAN_POINT('',(-2.28443929758135,-1.37777905311491,7.5));
#399594=CARTESIAN_POINT('',(-2.35585431734963,-1.38110557508643,8.78727029226991));
#399595=CARTESIAN_POINT('Ctrl Pts',(-2.28443929758135,-1.37777905311491,
8.85049129520029));
#399596=CARTESIAN_POINT('Ctrl Pts',(-2.30827890705324,-1.37888950557936,
8.82945686509571));
#399597=CARTESIAN_POINT('Ctrl Pts',(-2.33208307606301,-1.37999830722195,
8.80838212259896));
#399598=CARTESIAN_POINT('Ctrl Pts',(-2.35585431734963,-1.38110557508643,
8.78727029226991));
#399599=CARTESIAN_POINT('',(-2.36986171072477,-1.38175804150004,8.75721825406948));
#399600=CARTESIAN_POINT('Origin',(-2.32770859547033,-1.37979474530314,8.75937679713115));
#399601=CARTESIAN_POINT('',(-2.36986171072477,-1.38175804150004,7.51860402984325));
#399602=CARTESIAN_POINT('',(-2.36986171072477,-1.38175804150004,7.5));
#399603=CARTESIAN_POINT('Ctrl Pts',(-2.36986171072477,-1.38175804150004,
7.51860402984325));
#399604=CARTESIAN_POINT('Ctrl Pts',(-2.35886108179034,-1.38124563060987,
7.52834476460825));
#399605=CARTESIAN_POINT('Ctrl Pts',(-2.34785331140635,-1.38073288706995,
7.53807742314407));
#399606=CARTESIAN_POINT('Ctrl Pts',(-2.33683815978911,-1.38021979971112,
7.54780169004674));
#399607=CARTESIAN_POINT('Ctrl Pts',(-2.31939075494556,-1.37940709706472,
7.5632044032688));
#399608=CARTESIAN_POINT('Ctrl Pts',(-2.30192480935483,-1.37859353078762,
7.57858609112103));
#399609=CARTESIAN_POINT('Ctrl Pts',(-2.28443929758135,-1.37777905311491,
7.59394543036555));
#399610=CARTESIAN_POINT('Origin',(-2.41658349078374,-1.62573897887916,7.5));
#399611=CARTESIAN_POINT('',(-2.32121750495509,-1.46200174688659,8.75721825406948));
#399612=CARTESIAN_POINT('',(-2.31416007290288,-1.44988459233548,8.78727029226991));
#399613=CARTESIAN_POINT('Origin',(-2.29624567806399,-1.41912673461236,8.75658640621088));
#399614=CARTESIAN_POINT('',(-2.27817859968916,-1.38810672912947,8.85049129520029));
#399615=CARTESIAN_POINT('Ctrl Pts',(-2.31416007290288,-1.44988459233548,
8.78727029226991));
#399616=CARTESIAN_POINT('Ctrl Pts',(-2.30218326068066,-1.42932118008402,
8.80838212259897));
#399617=CARTESIAN_POINT('Ctrl Pts',(-2.29018985827905,-1.40872928356715,
8.82945686509571));
#399618=CARTESIAN_POINT('Ctrl Pts',(-2.27817859968917,-1.38810672912947,
8.85049129520029));
#399619=CARTESIAN_POINT('',(-2.27817859968916,-1.38810672912947,7.59394543036555));
#399620=CARTESIAN_POINT('',(-2.27817859968916,-1.38810672912947,7.5));
#399621=CARTESIAN_POINT('',(-2.32121750495509,-1.46200174688659,7.51860402984325));
#399622=CARTESIAN_POINT('Ctrl Pts',(-2.27817859968916,-1.38810672912946,
7.59394543036555));
#399623=CARTESIAN_POINT('Ctrl Pts',(-2.28698843374854,-1.40323264462922,
7.57858609112103));
#399624=CARTESIAN_POINT('Ctrl Pts',(-2.29578840965637,-1.41834163432013,
7.56320440326857));
#399625=CARTESIAN_POINT('Ctrl Pts',(-2.30457904406443,-1.43343458525989,
7.54780169004651));
#399626=CARTESIAN_POINT('Ctrl Pts',(-2.31012887635666,-1.44296328849363,
7.53807742314383));
#399627=CARTESIAN_POINT('Ctrl Pts',(-2.31567498971638,-1.45248560656069,
7.52834476460825));
#399628=CARTESIAN_POINT('Ctrl Pts',(-2.32121750495509,-1.46200174688659,
7.51860402984325));
#399629=CARTESIAN_POINT('',(-2.32121750495509,-1.46200174688659,7.5));
#399630=CARTESIAN_POINT('Origin',(-2.28411940593291,-1.3846466068521,7.5));
#399631=CARTESIAN_POINT('Ctrl Pts',(-2.27817859968916,-1.38810672912947,
8.85049129520029));
#399632=CARTESIAN_POINT('Ctrl Pts',(-2.27808113169049,-1.38793938287732,
8.85097269580138));
#399633=CARTESIAN_POINT('Ctrl Pts',(-2.2779921618778,-1.38776991462375,
8.85143669361005));
#399634=CARTESIAN_POINT('Ctrl Pts',(-2.27790836757131,-1.38759011450948,
8.8519052845931));
#399635=CARTESIAN_POINT('Ctrl Pts',(-2.27774447122186,-1.38723843688848,
8.85282181883899));
#399636=CARTESIAN_POINT('Ctrl Pts',(-2.27760476931615,-1.38685619637747,
8.85372622499635));
#399637=CARTESIAN_POINT('Ctrl Pts',(-2.27750155151867,-1.38643210212428,
8.8546225773507));
#399638=CARTESIAN_POINT('Ctrl Pts',(-2.27741586376915,-1.38608003413768,
8.85536669723986));
#399639=CARTESIAN_POINT('Ctrl Pts',(-2.27735526963749,-1.38569904887466,
8.85610498449051));
#399640=CARTESIAN_POINT('Ctrl Pts',(-2.27733469853656,-1.3852813971344,
8.85681338218371));
#399641=CARTESIAN_POINT('Ctrl Pts',(-2.27731603023015,-1.38490237752418,
8.85745625420284));
#399642=CARTESIAN_POINT('Ctrl Pts',(-2.27732949131404,-1.38448843593451,
8.85808743050666));
#399643=CARTESIAN_POINT('Ctrl Pts',(-2.27740126538765,-1.38402807170151,
8.8586680450841));
#399644=CARTESIAN_POINT('Ctrl Pts',(-2.27743438038934,-1.38381566962388,
8.85893592806395));
#399645=CARTESIAN_POINT('Ctrl Pts',(-2.27748014042396,-1.38359331526743,
8.85919241173848));
#399646=CARTESIAN_POINT('Ctrl Pts',(-2.27754269428292,-1.38335963403901,
8.85943017985534));
#399647=CARTESIAN_POINT('Ctrl Pts',(-2.27762716051044,-1.38304409520358,
8.8597512372));
#399648=CARTESIAN_POINT('Ctrl Pts',(-2.27774501555862,-1.38270003844088,
8.86004599534705));
#399649=CARTESIAN_POINT('Ctrl Pts',(-2.27790469650044,-1.38233497258254,
8.86026130871721));
#399650=CARTESIAN_POINT('Ctrl Pts',(-2.27796316019512,-1.3822013116795,
8.86034014101235));
#399651=CARTESIAN_POINT('Ctrl Pts',(-2.27802809754116,-1.38206282183858,
8.86040910639692));
#399652=CARTESIAN_POINT('Ctrl Pts',(-2.27809804391702,-1.38192341894475,
8.86046313645506));
#399653=CARTESIAN_POINT('Ctrl Pts',(-2.27820719465075,-1.38170588189641,
8.86054744990829));
#399654=CARTESIAN_POINT('Ctrl Pts',(-2.27833165395478,-1.38148024927838,
8.86059655985668));
#399655=CARTESIAN_POINT('Ctrl Pts',(-2.27846318335477,-1.38126085010038,
8.86059725258816));
#399656=CARTESIAN_POINT('Ctrl Pts',(-2.27859501664021,-1.38104094402262,
8.86059794692011));
#399657=CARTESIAN_POINT('Ctrl Pts',(-2.27873769344056,-1.38082622749523,
8.86056369958366));
#399658=CARTESIAN_POINT('Ctrl Pts',(-2.2788802978602,-1.3806263285976,8.86048590497774));
#399659=CARTESIAN_POINT('Ctrl Pts',(-2.27891751336788,-1.38057416093702,
8.86046560290182));
#399660=CARTESIAN_POINT('Ctrl Pts',(-2.27895528183715,-1.38052237637025,
8.86044257503091));
#399661=CARTESIAN_POINT('Ctrl Pts',(-2.27899240966943,-1.38047255574004,
8.86041778462583));
#399662=CARTESIAN_POINT('Ctrl Pts',(-2.27924223390885,-1.38013732472093,
8.86025097596201));
#399663=CARTESIAN_POINT('Ctrl Pts',(-2.27949684175642,-1.37984622804254,
8.8599848982295));
#399664=CARTESIAN_POINT('Ctrl Pts',(-2.2797424245759,-1.37960218414176,
8.85968173251462));
#399665=CARTESIAN_POINT('Ctrl Pts',(-2.27987232381719,-1.3794730989003,
8.85952137522077));
#399666=CARTESIAN_POINT('Ctrl Pts',(-2.28000206733073,-1.37935455443871,
8.85934740853961));
#399667=CARTESIAN_POINT('Ctrl Pts',(-2.28012877685891,-1.37924707484726,
8.8591675900182));
#399668=CARTESIAN_POINT('Ctrl Pts',(-2.28063758147687,-1.3788154884208,
8.85844552518695));
#399669=CARTESIAN_POINT('Ctrl Pts',(-2.28112426400981,-1.37853561654659,
8.85759444184125));
#399670=CARTESIAN_POINT('Ctrl Pts',(-2.28154157522219,-1.37834306627385,
8.85683498915139));
#399671=CARTESIAN_POINT('Ctrl Pts',(-2.28158524572917,-1.37832291640061,
8.85675551444998));
#399672=CARTESIAN_POINT('Ctrl Pts',(-2.28162816120068,-1.37830374221055,
8.85667699793651));
#399673=CARTESIAN_POINT('Ctrl Pts',(-2.28167026988732,-1.37828548282266,
8.85659965593547));
#399674=CARTESIAN_POINT('Ctrl Pts',(-2.28223865508834,-1.37803901667319,
8.85555568965886));
#399675=CARTESIAN_POINT('Ctrl Pts',(-2.28282050306977,-1.37788423350345,
8.85434650606346));
#399676=CARTESIAN_POINT('Ctrl Pts',(-2.28341709248037,-1.3778143622903,
8.85297329937118));
#399677=CARTESIAN_POINT('Ctrl Pts',(-2.28375263767312,-1.37777506399021,
8.85220095427748));
#399678=CARTESIAN_POINT('Ctrl Pts',(-2.28409301987352,-1.37776292344909,
8.85137579139184));
#399679=CARTESIAN_POINT('Ctrl Pts',(-2.28443929758135,-1.37777905311491,
8.85049129520029));
#399680=CARTESIAN_POINT('Origin',(-2.28411940593291,-1.3846466068521,7.59394543036555));
#399681=CARTESIAN_POINT('Ctrl Pts',(-2.27789561720849,-1.38762086650575,
7.59443877723642));
#399682=CARTESIAN_POINT('Ctrl Pts',(-2.27498116993602,-1.382616948966,7.58783886950016));
#399683=CARTESIAN_POINT('Ctrl Pts',(-2.28112970280112,-1.37676248698019,
7.58559994247159));
#399684=CARTESIAN_POINT('Ctrl Pts',(-2.29380549936271,-1.41493710554657,
7.56670252222137));
#399685=CARTESIAN_POINT('Ctrl Pts',(-2.29089526429399,-1.40994042008827,
7.56004874999026));
#399686=CARTESIAN_POINT('Ctrl Pts',(-2.29706549617267,-1.40403579513669,
7.55786368756705));
#399687=CARTESIAN_POINT('Ctrl Pts',(-2.30968567140157,-1.44220233424018,
7.53888913333557));
#399688=CARTESIAN_POINT('Ctrl Pts',(-2.30675814066331,-1.43717595323558,
7.53222002137276));
#399689=CARTESIAN_POINT('Ctrl Pts',(-2.31297108856254,-1.43125972782393,
7.53005029815326));
#399690=CARTESIAN_POINT('Ctrl Pts',(-2.32553541473659,-1.46941531881658,
7.51101258149734));
#399691=CARTESIAN_POINT('Ctrl Pts',(-2.32257239700634,-1.46432800894105,
7.5043616886572));
#399692=CARTESIAN_POINT('Ctrl Pts',(-2.32884576547034,-1.45843289828395,
7.50217374673251));
#399693=CARTESIAN_POINT('',(-2.32799867143118,-1.45698290352088,7.50366116523517));
#399694=CARTESIAN_POINT('Ctrl Pts',(-2.32121750495509,-1.46200174688659,
7.51860402984325));
#399695=CARTESIAN_POINT('Ctrl Pts',(-2.32143976369039,-1.46238335076545,
7.51734760759494));
#399696=CARTESIAN_POINT('Ctrl Pts',(-2.32169201845768,-1.46269824025774,
7.51608817408573));
#399697=CARTESIAN_POINT('Ctrl Pts',(-2.32198411096284,-1.46293734222612,
7.51481005913121));
#399698=CARTESIAN_POINT('Ctrl Pts',(-2.32224869533379,-1.46315392650261,
7.51365231206384));
#399699=CARTESIAN_POINT('Ctrl Pts',(-2.32254618173406,-1.46330882470791,
7.51247773061043));
#399700=CARTESIAN_POINT('Ctrl Pts',(-2.32288847583598,-1.46336660528915,
7.51129758471022));
#399701=CARTESIAN_POINT('Ctrl Pts',(-2.32331390831319,-1.46343841995285,
7.50983079813401));
#399702=CARTESIAN_POINT('Ctrl Pts',(-2.3237971485705,-1.46334507583529,
7.50839324291155));
#399703=CARTESIAN_POINT('Ctrl Pts',(-2.32432608821462,-1.46300494832449,
7.50715379678855));
#399704=CARTESIAN_POINT('Ctrl Pts',(-2.32457044308918,-1.46284781921504,
7.50658120839351));
#399705=CARTESIAN_POINT('Ctrl Pts',(-2.32485414912167,-1.46260769292222,
7.50598221009429));
#399706=CARTESIAN_POINT('Ctrl Pts',(-2.32515575918815,-1.46227292178526,
7.50545747549611));
#399707=CARTESIAN_POINT('Ctrl Pts',(-2.32531670765533,-1.46209427754445,
7.50517746087247));
#399708=CARTESIAN_POINT('Ctrl Pts',(-2.32548465021346,-1.46188688045124,
7.50491486231392));
#399709=CARTESIAN_POINT('Ctrl Pts',(-2.32565384315538,-1.46165517302969,
7.50468370960992));
#399710=CARTESIAN_POINT('Ctrl Pts',(-2.32590683997245,-1.4613086973465,
7.50433806340446));
#399711=CARTESIAN_POINT('Ctrl Pts',(-2.32616976944412,-1.46089714676683,
7.50405484070983));
#399712=CARTESIAN_POINT('Ctrl Pts',(-2.32642432005221,-1.46044785276343,
7.5038576603613));
#399713=CARTESIAN_POINT('Ctrl Pts',(-2.32645154028313,-1.46039980775338,
7.5038365749879));
#399714=CARTESIAN_POINT('Ctrl Pts',(-2.32647866521305,-1.46035135950569,
7.50381643264937));
#399715=CARTESIAN_POINT('Ctrl Pts',(-2.32650567314321,-1.46030256203687,
7.50379723213559));
#399716=CARTESIAN_POINT('Ctrl Pts',(-2.32668595991195,-1.45997682296968,
7.50366906242519));
#399717=CARTESIAN_POINT('Ctrl Pts',(-2.3268643257083,-1.45962808883252,
7.50358235568538));
#399718=CARTESIAN_POINT('Ctrl Pts',(-2.32702816834756,-1.45928781937694,
7.5035341175365));
#399719=CARTESIAN_POINT('Ctrl Pts',(-2.32727383184171,-1.45877762383937,
7.50346178989176));
#399720=CARTESIAN_POINT('Ctrl Pts',(-2.32751641693377,-1.45821832421323,
7.50346967198527));
#399721=CARTESIAN_POINT('Ctrl Pts',(-2.32773766577599,-1.45766193758501,
7.50354272648692));
#399722=CARTESIAN_POINT('Ctrl Pts',(-2.32782867000438,-1.4574330842483,
7.50357277531559));
#399723=CARTESIAN_POINT('Ctrl Pts',(-2.32791607531215,-1.45720508021275,
7.50361331098761));
#399724=CARTESIAN_POINT('Ctrl Pts',(-2.32799867143238,-1.45698290352164,
7.50366116523659));
#399725=CARTESIAN_POINT('',(-2.28662319996353,-1.38616442150716,7.57603338622103));
#399726=CARTESIAN_POINT('Origin',(-2.29418152300564,-1.39074298486218,7.58486873427625));
#399727=CARTESIAN_POINT('Ctrl Pts',(-2.32799867145535,-1.45698290357288,
7.50366116529969));
#399728=CARTESIAN_POINT('Ctrl Pts',(-2.31423007474035,-1.4334148416394,
7.52783573079709));
#399729=CARTESIAN_POINT('Ctrl Pts',(-2.30043891757452,-1.40980978649596,
7.55196141284069));
#399730=CARTESIAN_POINT('Ctrl Pts',(-2.28662320026408,-1.38616442272262,
7.57603338728831));
#399731=CARTESIAN_POINT('Ctrl Pts',(-2.27884811390188,-1.38890690800894,
7.59639677331371));
#399732=CARTESIAN_POINT('Ctrl Pts',(-2.26672396437063,-1.3741013879501,
7.59974925422224));
#399733=CARTESIAN_POINT('Ctrl Pts',(-2.28545841158011,-1.37800253058071,
7.59639677331371));
#399734=CARTESIAN_POINT('Ctrl Pts',(-2.27592382560251,-1.38632550489709,
7.58707626057423));
#399735=CARTESIAN_POINT('Ctrl Pts',(-2.27553575658726,-1.37944314817564,
7.58811717123965));
#399736=CARTESIAN_POINT('Ctrl Pts',(-2.28181714606151,-1.37660385638463,
7.58707626057423));
#399737=CARTESIAN_POINT('Ctrl Pts',(-2.28198336987502,-1.38586992233497,
7.5801537675693));
#399738=CARTESIAN_POINT('Ctrl Pts',(-2.28144597464146,-1.38302595709244,
7.5820876076604));
#399739=CARTESIAN_POINT('Ctrl Pts',(-2.28421599812537,-1.38218696851292,
7.5801537675693));
#399740=CARTESIAN_POINT('Ctrl Pts',(-2.28662319925574,-1.38616442107833,
7.57603338509286));
#399741=CARTESIAN_POINT('Ctrl Pts',(-2.28662319925574,-1.38616442107833,
7.57603338509286));
#399742=CARTESIAN_POINT('Ctrl Pts',(-2.28662319925574,-1.38616442107833,
7.57603338509286));
#399743=CARTESIAN_POINT('Origin',(-2.29417856487524,-1.39074786460819,7.58486873427621));
#399744=CARTESIAN_POINT('Ctrl Pts',(-2.37845886339419,-1.38215849811743,
7.51098857897448));
#399745=CARTESIAN_POINT('Ctrl Pts',(-2.37257792201277,-1.38188456301551,
7.50433767179956));
#399746=CARTESIAN_POINT('Ctrl Pts',(-2.37025300047282,-1.39017327768762,
7.50214974420965));
#399747=CARTESIAN_POINT('Ctrl Pts',(-2.34699168879538,-1.38069275256384,
7.53887321589168));
#399748=CARTESIAN_POINT('Ctrl Pts',(-2.34118121152851,-1.38042209969059,
7.53220407452065));
#399749=CARTESIAN_POINT('Ctrl Pts',(-2.33880959854636,-1.38866699943436,
7.53003438070912));
#399750=CARTESIAN_POINT('Ctrl Pts',(-2.31546408561356,-1.3792241922381,
7.56669465659232));
#399751=CARTESIAN_POINT('Ctrl Pts',(-2.30968794718705,-1.37895513887298,
7.560040858333));
#399752=CARTESIAN_POINT('Ctrl Pts',(-2.30730685731679,-1.38715678877749,
7.55785582193789));
#399753=CARTESIAN_POINT('Ctrl Pts',(-2.28387747971606,-1.37775288355731,
7.59443891967696));
#399754=CARTESIAN_POINT('Ctrl Pts',(-2.27809296660798,-1.37748344009835,
7.58783901202978));
#399755=CARTESIAN_POINT('Ctrl Pts',(-2.27574633651479,-1.38564263768108,
7.58560008491213));
#399756=CARTESIAN_POINT('',(-2.36854855682563,-1.39009162622349,7.50366116523517));
#399757=CARTESIAN_POINT('Ctrl Pts',(-2.36854855682595,-1.39009162622368,
7.50366116523554));
#399758=CARTESIAN_POINT('Ctrl Pts',(-2.36905599173954,-1.38952891197538,
7.50350835821027));
#399759=CARTESIAN_POINT('Ctrl Pts',(-2.36950414026277,-1.38899513214037,
7.50345484956));
#399760=CARTESIAN_POINT('Ctrl Pts',(-2.36990678611858,-1.3884748031337,
7.50349758195598));
#399761=CARTESIAN_POINT('Ctrl Pts',(-2.37011337330361,-1.38820783576467,
7.50351950684424));
#399762=CARTESIAN_POINT('Ctrl Pts',(-2.37032844657167,-1.38791817510164,
7.50357029184312));
#399763=CARTESIAN_POINT('Ctrl Pts',(-2.37052816139873,-1.38763315784122,
7.50365515313924));
#399764=CARTESIAN_POINT('Ctrl Pts',(-2.37083540367529,-1.38719468587981,
7.50378570417639));
#399765=CARTESIAN_POINT('Ctrl Pts',(-2.37111560035781,-1.3867545317047,
7.50400001621911));
#399766=CARTESIAN_POINT('Ctrl Pts',(-2.37134550914226,-1.38634497820496,
7.50428903009635));
#399767=CARTESIAN_POINT('Ctrl Pts',(-2.37137102724852,-1.3862995209174,
7.50432110841318));
#399768=CARTESIAN_POINT('Ctrl Pts',(-2.3713959530662,-1.38625442726893,
7.50435406373354));
#399769=CARTESIAN_POINT('Ctrl Pts',(-2.37142027477436,-1.38620973128227,
7.50438785222352));
#399770=CARTESIAN_POINT('Ctrl Pts',(-2.37156877049319,-1.38593684080006,
7.50459414719561));
#399771=CARTESIAN_POINT('Ctrl Pts',(-2.37169665806775,-1.38567418270535,
7.50483629897752));
#399772=CARTESIAN_POINT('Ctrl Pts',(-2.37180022139304,-1.3854323954643,
7.5050991045531));
#399773=CARTESIAN_POINT('Ctrl Pts',(-2.37202869249058,-1.38489898852532,
7.50567888004914));
#399774=CARTESIAN_POINT('Ctrl Pts',(-2.37214826172948,-1.38444634307579,
7.50637912803145));
#399775=CARTESIAN_POINT('Ctrl Pts',(-2.37218983841972,-1.38407427769357,
7.50710440483569));
#399776=CARTESIAN_POINT('Ctrl Pts',(-2.37220003384959,-1.38398303987532,
7.50728225710685));
#399777=CARTESIAN_POINT('Ctrl Pts',(-2.37220588737711,-1.3838948475011,
7.50746498566954));
#399778=CARTESIAN_POINT('Ctrl Pts',(-2.37220767804062,-1.38381178685589,
7.50764697238949));
#399779=CARTESIAN_POINT('Ctrl Pts',(-2.37221730415486,-1.38336527568614,
7.50862528291182));
#399780=CARTESIAN_POINT('Ctrl Pts',(-2.3721145318164,-1.38302661934609,
7.50965856837422));
#399781=CARTESIAN_POINT('Ctrl Pts',(-2.37195529513963,-1.38276022611351,
7.51067959873202));
#399782=CARTESIAN_POINT('Ctrl Pts',(-2.37186766699555,-1.38261362958161,
7.51124147302579));
#399783=CARTESIAN_POINT('Ctrl Pts',(-2.37176254541608,-1.38248910370111,
7.51180065547253));
#399784=CARTESIAN_POINT('Ctrl Pts',(-2.37164697289435,-1.38238219484358,
7.51235175716501));
#399785=CARTESIAN_POINT('Ctrl Pts',(-2.37124762379313,-1.38201278215341,
7.51425603304536));
#399786=CARTESIAN_POINT('Ctrl Pts',(-2.37067175971287,-1.38181411915049,
7.51626900505179));
#399787=CARTESIAN_POINT('Ctrl Pts',(-2.36997578574981,-1.38176473183861,
7.51827788969242));
#399788=CARTESIAN_POINT('Ctrl Pts',(-2.36993811832372,-1.38176205890396,
7.51838661432544));
#399789=CARTESIAN_POINT('Ctrl Pts',(-2.3699000911534,-1.38175982926596,
7.51849533314856));
#399790=CARTESIAN_POINT('Ctrl Pts',(-2.36986171072477,-1.38175804150003,
7.51860402984325));
#399791=CARTESIAN_POINT('Ctrl Pts',(-2.28662320118131,-1.38616442121185,
7.57603338728985));
#399792=CARTESIAN_POINT('Ctrl Pts',(-2.31397746257106,-1.38747654046483,
7.55196141284922));
#399793=CARTESIAN_POINT('Ctrl Pts',(-2.34128462636657,-1.3887855289963,
7.52783573083105));
#399794=CARTESIAN_POINT('Ctrl Pts',(-2.36854855688476,-1.39009162622088,
7.50366116530176));
#399795=CARTESIAN_POINT('Origin',(-7.90134016134193E-16,-4.78983883923435E-16,
7.49482233047033));
#399796=CARTESIAN_POINT('Origin',(-2.32050622536842,-1.45229374026965,7.49482233047033));
#399797=CARTESIAN_POINT('Origin',(0.,0.,7.50366116523517));
#399798=CARTESIAN_POINT('Origin',(-2.36092560474803,-1.3856177462941,7.49482233047033));
#399799=CARTESIAN_POINT('Ctrl Pts',(-2.32121697257585,-1.46200083291476,
7.51860402984325));
#399800=CARTESIAN_POINT('Ctrl Pts',(-2.32504704676295,-1.46857554338377,
7.51860402984325));
#399801=CARTESIAN_POINT('Ctrl Pts',(-2.32096588398458,-1.47499741199084,
7.51860402984325));
#399802=CARTESIAN_POINT('Ctrl Pts',(-2.3226391041613,-1.46444206841971,
7.51041458714364));
#399803=CARTESIAN_POINT('Ctrl Pts',(-2.32408016420081,-1.47009695230204,
7.51004642900441));
#399804=CARTESIAN_POINT('Ctrl Pts',(-2.32096475844835,-1.47499918306595,
7.50729136483009));
#399805=CARTESIAN_POINT('Ctrl Pts',(-2.32541088507259,-1.46395118372962,
7.50215815450139));
#399806=CARTESIAN_POINT('Ctrl Pts',(-2.32604895207089,-1.46699928723625,
7.49877163671531));
#399807=CARTESIAN_POINT('Ctrl Pts',(-2.32421856835796,-1.46992394432005,
7.49481588533172));
#399808=CARTESIAN_POINT('Ctrl Pts',(-2.32799820477189,-1.45698261146062,
7.50366171572174));
#399809=CARTESIAN_POINT('Ctrl Pts',(-2.33110214420592,-1.4589252185354,
7.50000045605858));
#399810=CARTESIAN_POINT('Ctrl Pts',(-2.33110214420586,-1.4589252185355,
7.49482233047317));
#399811=CARTESIAN_POINT('Origin',(-2.31041603905738,-1.46829287829998,7.51860402984325));
#399812=CARTESIAN_POINT('Origin',(-2.31041603905738,-1.46829287829998,9.));
#399813=CARTESIAN_POINT('Origin',(-2.31041603905738,-1.46829287829998,8.75721825406948));
#399814=CARTESIAN_POINT('Ctrl Pts',(-2.31281244619727,-1.44757086443545,
8.78942910404912));
#399815=CARTESIAN_POINT('Ctrl Pts',(-2.31563446187852,-1.45237593011621,
8.7967269950169));
#399816=CARTESIAN_POINT('Ctrl Pts',(-2.30889868938922,-1.45823279403425,
8.79893251111267));
#399817=CARTESIAN_POINT('Ctrl Pts',(-2.31834579499507,-1.45707125757586,
8.78111911759583));
#399818=CARTESIAN_POINT('Ctrl Pts',(-2.32168490856532,-1.46277148833351,
8.78644465894814));
#399819=CARTESIAN_POINT('Ctrl Pts',(-2.31685066608334,-1.46927883890042,
8.78817647674132));
#399820=CARTESIAN_POINT('Ctrl Pts',(-2.32179430992119,-1.46299212920274,
8.76780923932029));
#399821=CARTESIAN_POINT('Ctrl Pts',(-2.32573159556496,-1.46972358658801,
8.76988516158374));
#399822=CARTESIAN_POINT('Ctrl Pts',(-2.32180826674691,-1.47618453631556,
8.77093053738833));
#399823=CARTESIAN_POINT('Ctrl Pts',(-2.32112189670534,-1.4618376402692,
8.75371302330492));
#399824=CARTESIAN_POINT('Ctrl Pts',(-2.32496320702648,-1.46840350170426,
8.75300828287559));
#399825=CARTESIAN_POINT('Ctrl Pts',(-2.32084096157935,-1.47483791168559,
8.75267964240737));
#399826=CARTESIAN_POINT('Origin',(-2.30335860700517,-1.45617572374887,8.78727029226991));
#399827=CARTESIAN_POINT('Ctrl Pts',(-2.27817859968917,-1.38810672912947,
8.85049129520029));
#399828=CARTESIAN_POINT('Ctrl Pts',(-2.2811176229011,-1.39315284196836,
8.85711686593484));
#399829=CARTESIAN_POINT('Ctrl Pts',(-2.27490615106174,-1.39902807640647,
8.85933012996512));
#399830=CARTESIAN_POINT('Ctrl Pts',(-2.2901898743986,-1.40872931124338,
8.82945683644721));
#399831=CARTESIAN_POINT('Ctrl Pts',(-2.29315329328014,-1.41381730986978,
8.83607469902388));
#399832=CARTESIAN_POINT('Ctrl Pts',(-2.28689781417968,-1.41968254846008,
8.8382956714852));
#399833=CARTESIAN_POINT('Ctrl Pts',(-2.3021832453345,-1.42932115373565,
8.80838214965004));
#399834=CARTESIAN_POINT('Ctrl Pts',(-2.30515835925056,-1.43442923198015,
8.81501364461989));
#399835=CARTESIAN_POINT('Ctrl Pts',(-2.29887186472477,-1.44030535307936,
8.81722098428721));
#399836=CARTESIAN_POINT('Ctrl Pts',(-2.31416007290288,-1.44988459233548,
8.78727029226991));
#399837=CARTESIAN_POINT('Ctrl Pts',(-2.31713568099513,-1.45499351904857,
8.79393457792714));
#399838=CARTESIAN_POINT('Ctrl Pts',(-2.3108296592442,-1.46089889836364,
8.79610912703474));
#399839=CARTESIAN_POINT('Origin',(-2.26737713379145,-1.39439786054286,8.85049129520029));
#399840=CARTESIAN_POINT('Ctrl Pts',(-2.28443929758135,-1.37777905311491,
8.85049129520029));
#399841=CARTESIAN_POINT('Ctrl Pts',(-2.29027258849562,-1.37805076865116,
8.85711686593484));
#399842=CARTESIAN_POINT('Ctrl Pts',(-2.29260852370877,-1.36982616113506,
8.85933012996512));
#399843=CARTESIAN_POINT('Ctrl Pts',(-2.27927866931395,-1.37753867030224,
8.86332496987232));
#399844=CARTESIAN_POINT('Ctrl Pts',(-2.28191097731258,-1.37374092768628,
8.86648636486738));
#399845=CARTESIAN_POINT('Ctrl Pts',(-2.27817065852942,-1.36917079450517,
8.87206031107457));
#399846=CARTESIAN_POINT('Ctrl Pts',(-2.27556081970208,-1.38361217013837,
8.86341338519877));
#399847=CARTESIAN_POINT('Ctrl Pts',(-2.27337901193668,-1.38770034644438,
8.86654584966059));
#399848=CARTESIAN_POINT('Ctrl Pts',(-2.26758895886383,-1.3864356574703,
8.87215952290714));
#399849=CARTESIAN_POINT('Ctrl Pts',(-2.27817859968916,-1.38810672912947,
8.85049129520029));
#399850=CARTESIAN_POINT('Ctrl Pts',(-2.2811176229011,-1.39315284196836,
8.85711686593484));
#399851=CARTESIAN_POINT('Ctrl Pts',(-2.27490615106174,-1.39902807640647,
8.85933012996512));
#399852=CARTESIAN_POINT('Origin',(-2.28502091876034,-1.36529259177455,8.85049129520029));
#399853=CARTESIAN_POINT('Ctrl Pts',(-2.35585431734963,-1.38110557508643,
8.78727029226991));
#399854=CARTESIAN_POINT('Ctrl Pts',(-2.36176022090918,-1.38138067293022,
8.79393457792714));
#399855=CARTESIAN_POINT('Ctrl Pts',(-2.3640791495949,-1.37305829436825,
8.79610912703474));
#399856=CARTESIAN_POINT('Ctrl Pts',(-2.33208304560438,-1.37999830580319,
8.80838214965003));
#399857=CARTESIAN_POINT('Ctrl Pts',(-2.33798796833693,-1.38027335795992,
8.81501364461995));
#399858=CARTESIAN_POINT('Ctrl Pts',(-2.34028998879802,-1.37198182526734,
8.81722098428721));
#399859=CARTESIAN_POINT('Ctrl Pts',(-2.30827893904688,-1.37888950706963,
8.82945683644722));
#399860=CARTESIAN_POINT('Ctrl Pts',(-2.31416064980261,-1.37916347800912,
8.83607469902389));
#399861=CARTESIAN_POINT('Ctrl Pts',(-2.31646736766072,-1.3709044771482,
8.83829567148519));
#399862=CARTESIAN_POINT('Ctrl Pts',(-2.28443929758135,-1.37777905311491,
8.85049129520029));
#399863=CARTESIAN_POINT('Ctrl Pts',(-2.29027258849562,-1.37805076865116,
8.85711686593484));
#399864=CARTESIAN_POINT('Ctrl Pts',(-2.29260852370877,-1.36982616113506,
8.85933012996512));
#399865=CARTESIAN_POINT('Origin',(-2.35643593852862,-1.36861911374607,8.78727029226991));
#399866=CARTESIAN_POINT('Ctrl Pts',(-2.36967675099988,-1.38174940758217,
8.75374538247847));
#399867=CARTESIAN_POINT('Ctrl Pts',(-2.37726687089216,-1.38211609329002,
8.75304829418601));
#399868=CARTESIAN_POINT('Ctrl Pts',(-2.38106579034592,-1.3754950016736,
8.75272238421917));
#399869=CARTESIAN_POINT('Ctrl Pts',(-2.37099530499473,-1.38181082644539,
8.76769408445023));
#399870=CARTESIAN_POINT('Ctrl Pts',(-2.37877645928179,-1.38218605028949,
8.76974318093971));
#399871=CARTESIAN_POINT('Ctrl Pts',(-2.38268881118069,-1.37572757834178,
8.7707786988043));
#399872=CARTESIAN_POINT('Ctrl Pts',(-2.3642371483471,-1.38149602835533,
8.78108014887987));
#399873=CARTESIAN_POINT('Ctrl Pts',(-2.37083121329715,-1.38181781203245,
8.78639403366322));
#399874=CARTESIAN_POINT('Ctrl Pts',(-2.37437720405471,-1.37454127265745,
8.78812224174741));
#399875=CARTESIAN_POINT('Ctrl Pts',(-2.35316202148167,-1.38098014374298,
8.78944554828686));
#399876=CARTESIAN_POINT('Ctrl Pts',(-2.35871898210048,-1.38125692217053,
8.79673892988686));
#399877=CARTESIAN_POINT('Ctrl Pts',(-2.36079643040482,-1.37258583441527,
8.79894799272499));
#399878=CARTESIAN_POINT('Origin',(-2.37044333190376,-1.36927158015968,8.75721825406948));
#399879=CARTESIAN_POINT('Origin',(-2.37044333190376,-1.36927158015968,9.));
#399880=CARTESIAN_POINT('Origin',(-2.37044333190376,-1.36927158015968,7.51860402984325));
#399881=CARTESIAN_POINT('Ctrl Pts',(-2.36854787837649,-1.39009122804435,
7.50366195182966));
#399882=CARTESIAN_POINT('Ctrl Pts',(-2.37170608696157,-1.39194476796656,
7.50000065167735));
#399883=CARTESIAN_POINT('Ctrl Pts',(-2.37170608696163,-1.39194476796646,
7.49482233047108));
#399884=CARTESIAN_POINT('Ctrl Pts',(-2.3735332551357,-1.38456856399741,
7.50215800491337));
#399885=CARTESIAN_POINT('Ctrl Pts',(-2.37653148948253,-1.38372281700463,
7.49877273257266));
#399886=CARTESIAN_POINT('Ctrl Pts',(-2.37827884268994,-1.38074558454502,
7.49481816995647));
#399887=CARTESIAN_POINT('Ctrl Pts',(-2.37267722747953,-1.38188952816452,
7.51043025814041));
#399888=CARTESIAN_POINT('Ctrl Pts',(-2.37836144152799,-1.38055443729186,
7.51006209594514));
#399889=CARTESIAN_POINT('Ctrl Pts',(-2.38126854047388,-1.37552176942273,
7.50731281821699));
#399890=CARTESIAN_POINT('Ctrl Pts',(-2.36986020095858,-1.38175797108343,
7.51860402984325));
#399891=CARTESIAN_POINT('Ctrl Pts',(-2.37746118835,-1.38211294723218,7.51860402984324));
#399892=CARTESIAN_POINT('Ctrl Pts',(-2.38126727405858,-1.37552396180424,
7.51860402984325));
#399893=CARTESIAN_POINT('Origin',(0.,0.,7.5));
#399894=CARTESIAN_POINT('Origin',(-2.19147106502123,-1.52131278661257,7.5));
#399895=CARTESIAN_POINT('',(-2.19147106502123,-1.52131278661257,7.59394543036555));
#399896=CARTESIAN_POINT('',(-2.19147106502123,-1.52131278661257,8.85049129520029));
#399897=CARTESIAN_POINT('',(-2.19147106502123,-1.52131278661257,7.5));
#399898=CARTESIAN_POINT('',(-2.26252622397767,-1.52920804991441,8.78727029226991));
#399899=CARTESIAN_POINT('Ctrl Pts',(-2.19147106502123,-1.52131278661257,
8.85049129520029));
#399900=CARTESIAN_POINT('Ctrl Pts',(-2.215190546525,-1.52394836655645,8.82945686509571));
#399901=CARTESIAN_POINT('Ctrl Pts',(-2.23887476615139,-1.52658002839207,
8.80838212259895));
#399902=CARTESIAN_POINT('Ctrl Pts',(-2.26252622397767,-1.52920804991441,
8.78727029226991));
#399903=CARTESIAN_POINT('',(-2.27646303399419,-1.5307566325407,8.75721825406948));
#399904=CARTESIAN_POINT('Origin',(-2.23452231565444,-1.52609661077909,8.7593767971309));
#399905=CARTESIAN_POINT('',(-2.27646303399419,-1.5307566325407,7.51860402984325));
#399906=CARTESIAN_POINT('',(-2.27646303399419,-1.5307566325407,7.5));
#399907=CARTESIAN_POINT('Ctrl Pts',(-2.27646303399419,-1.5307566325407,
7.51860402984325));
#399908=CARTESIAN_POINT('Ctrl Pts',(-2.26551783731017,-1.5295404617379,
7.52834476460825));
#399909=CARTESIAN_POINT('Ctrl Pts',(-2.25456553516241,-1.52832350141458,
7.53807742314407));
#399910=CARTESIAN_POINT('Ctrl Pts',(-2.24360588897549,-1.52710572506151,
7.54780169004674));
#399911=CARTESIAN_POINT('Ctrl Pts',(-2.22624640173375,-1.52517683313345,
7.5632044032688));
#399912=CARTESIAN_POINT('Ctrl Pts',(-2.20886846717179,-1.52324589143935,
7.57858609112102));
#399913=CARTESIAN_POINT('Ctrl Pts',(-2.19147106502123,-1.52131278661257,
7.59394543036555));
#399914=CARTESIAN_POINT('Origin',(-2.30745690681615,-1.77722975964336,7.5));
#399915=CARTESIAN_POINT('',(-2.22277754110615,-1.60771882366397,8.75721825406948));
#399916=CARTESIAN_POINT('',(-2.21651095806263,-1.59517439388236,8.78727029226991));
#399917=CARTESIAN_POINT('Origin',(-2.20060403297877,-1.5633319522567,8.75658640621004));
#399918=CARTESIAN_POINT('',(-2.18456153393018,-1.53121811901793,8.85049129520029));
#399919=CARTESIAN_POINT('Ctrl Pts',(-2.21651095806263,-1.59517439388236,
8.78727029226991));
#399920=CARTESIAN_POINT('Ctrl Pts',(-2.20587625583213,-1.57388587437304,
8.80838212259896));
#399921=CARTESIAN_POINT('Ctrl Pts',(-2.1952268225017,-1.55256786618585,
8.82945686509571));
#399922=CARTESIAN_POINT('Ctrl Pts',(-2.18456153393018,-1.53121811901793,
8.85049129520029));
#399923=CARTESIAN_POINT('',(-2.18456153393018,-1.53121811901793,7.59394543036555));
#399924=CARTESIAN_POINT('',(-2.18456153393018,-1.53121811901793,7.5));
#399925=CARTESIAN_POINT('',(-2.22277754110615,-1.60771882366397,7.51860402984325));
#399926=CARTESIAN_POINT('Ctrl Pts',(-2.18456153393018,-1.53121811901793,
7.59394543036555));
#399927=CARTESIAN_POINT('Ctrl Pts',(-2.19238414650715,-1.54687740470822,
7.57858609112103));
#399928=CARTESIAN_POINT('Ctrl Pts',(-2.20019800562751,-1.56251916775161,
7.56320440326857));
#399929=CARTESIAN_POINT('Ctrl Pts',(-2.20800357004751,-1.57814432648525,
7.54780169004651));
#399930=CARTESIAN_POINT('Ctrl Pts',(-2.21293149350176,-1.58800903095206,
7.53807742314383));
#399931=CARTESIAN_POINT('Ctrl Pts',(-2.21785611476348,-1.59786712509838,
7.52834476460825));
#399932=CARTESIAN_POINT('Ctrl Pts',(-2.22277754110615,-1.60771882366397,
7.51860402984325));
#399933=CARTESIAN_POINT('',(-2.22277754110615,-1.60771882366397,7.5));
#399934=CARTESIAN_POINT('Origin',(-2.19071182494582,-1.52814573469578,7.5));
#399935=CARTESIAN_POINT('Ctrl Pts',(-2.18456153393018,-1.53121811901793,
8.85049129520029));
#399936=CARTESIAN_POINT('Ctrl Pts',(-2.18447498810115,-1.53104487180049,
8.85097269580138));
#399937=CARTESIAN_POINT('Ctrl Pts',(-2.18439705895477,-1.53087005142215,
8.85143669361005));
#399938=CARTESIAN_POINT('Ctrl Pts',(-2.18432495664555,-1.53068525200685,
8.8519052845931));
#399939=CARTESIAN_POINT('Ctrl Pts',(-2.18418392910126,-1.53032379607007,
8.85282181883899));
#399940=CARTESIAN_POINT('Ctrl Pts',(-2.18406900446172,-1.52993339018136,
8.85372622499636));
#399941=CARTESIAN_POINT('Ctrl Pts',(-2.18399317054837,-1.52950355408831,
8.85462257735071));
#399942=CARTESIAN_POINT('Ctrl Pts',(-2.18393021592687,-1.52914671943019,
8.85536669723986));
#399943=CARTESIAN_POINT('Ctrl Pts',(-2.18389415610197,-1.5287626346629,
8.85610498449051));
#399944=CARTESIAN_POINT('Ctrl Pts',(-2.18390038630544,-1.52834452303797,
8.85681338218371));
#399945=CARTESIAN_POINT('Ctrl Pts',(-2.18390604022488,-1.5279650860817,
8.85745625420284));
#399946=CARTESIAN_POINT('Ctrl Pts',(-2.18394599498023,-1.52755285743402,
8.85808743050665));
#399947=CARTESIAN_POINT('Ctrl Pts',(-2.18404711722399,-1.5270980376494,
8.85866804508409));
#399948=CARTESIAN_POINT('Ctrl Pts',(-2.18409377283519,-1.52688819366006,
8.85893592806395));
#399949=CARTESIAN_POINT('Ctrl Pts',(-2.18415368514345,-1.52666922800997,
8.85919241173848));
#399950=CARTESIAN_POINT('Ctrl Pts',(-2.18423108248651,-1.52644003474419,
8.85943017985534));
#399951=CARTESIAN_POINT('Ctrl Pts',(-2.1843355918117,-1.52613055598692,
8.8597512372));
#399952=CARTESIAN_POINT('Ctrl Pts',(-2.18447524850651,-1.52579475712461,
8.86004599534706));
#399953=CARTESIAN_POINT('Ctrl Pts',(-2.18465799121656,-1.52544067212629,
8.86026130871721));
#399954=CARTESIAN_POINT('Ctrl Pts',(-2.18472489847477,-1.52531103162569,
8.86034014101235));
#399955=CARTESIAN_POINT('Ctrl Pts',(-2.18479857547465,-1.52517698687705,
8.86040910639693));
#399956=CARTESIAN_POINT('Ctrl Pts',(-2.18487730971225,-1.5250423518811,
8.86046313645507));
#399957=CARTESIAN_POINT('Ctrl Pts',(-2.18500017383063,-1.52483225509748,
8.8605474499083));
#399958=CARTESIAN_POINT('Ctrl Pts',(-2.18513883375115,-1.52461506020084,
8.86059655985669));
#399959=CARTESIAN_POINT('Ctrl Pts',(-2.18528414986347,-1.52440453891958,
8.86059725258816));
#399960=CARTESIAN_POINT('Ctrl Pts',(-2.18542980171407,-1.52419353125005,
8.86059794692011));
#399961=CARTESIAN_POINT('Ctrl Pts',(-2.18558594230478,-1.52398839721477,
8.86056369958366));
#399962=CARTESIAN_POINT('Ctrl Pts',(-2.18574106129468,-1.5237980457274,
8.86048590497774));
#399963=CARTESIAN_POINT('Ctrl Pts',(-2.1857815427326,-1.52374836965664,
8.86046560290182));
#399964=CARTESIAN_POINT('Ctrl Pts',(-2.18582255145109,-1.52369911132095,
8.86044257503091));
#399965=CARTESIAN_POINT('Ctrl Pts',(-2.18586279501899,-1.52365177184095,
8.86041778462584));
#399966=CARTESIAN_POINT('Ctrl Pts',(-2.18613358429285,-1.52333323588389,
8.86025097596201));
#399967=CARTESIAN_POINT('Ctrl Pts',(-2.18640631964952,-1.52305905007566,
8.8599848982295));
#399968=CARTESIAN_POINT('Ctrl Pts',(-2.18666703383916,-1.52283124213451,
8.85968173251462));
#399969=CARTESIAN_POINT('Ctrl Pts',(-2.18680493670834,-1.52271074478549,
8.85952137522077));
#399970=CARTESIAN_POINT('Ctrl Pts',(-2.18694200881965,-1.52260075658167,
8.85934740853961));
#399971=CARTESIAN_POINT('Ctrl Pts',(-2.18707534425059,-1.52250161612591,
8.8591675900182));
#399972=CARTESIAN_POINT('Ctrl Pts',(-2.18761075531217,-1.52210351566385,
8.85844552518696));
#399973=CARTESIAN_POINT('Ctrl Pts',(-2.18811436935619,-1.52185540067336,
8.85759444184127));
#399974=CARTESIAN_POINT('Ctrl Pts',(-2.18854315989625,-1.52168998323699,
8.85683498915142));
#399975=CARTESIAN_POINT('Ctrl Pts',(-2.18858803168432,-1.52167267274281,
8.85675551445));
#399976=CARTESIAN_POINT('Ctrl Pts',(-2.18863208747596,-1.52165628755188,
8.85667699793652));
#399977=CARTESIAN_POINT('Ctrl Pts',(-2.1886752795288,-1.52164076359268,
8.85659965593547));
#399978=CARTESIAN_POINT('Ctrl Pts',(-2.18925828806187,-1.52143122039921,
8.85555568965886));
#399979=CARTESIAN_POINT('Ctrl Pts',(-2.18984885756596,-1.52131403437626,
8.85434650606346));
#399980=CARTESIAN_POINT('Ctrl Pts',(-2.19044869788364,-1.52128253033578,
8.85297329937117));
#399981=CARTESIAN_POINT('Ctrl Pts',(-2.19078607151352,-1.52126481123258,
8.85220095427747));
#399982=CARTESIAN_POINT('Ctrl Pts',(-2.19112653220933,-1.52127450399796,
8.85137579139183));
#399983=CARTESIAN_POINT('Ctrl Pts',(-2.19147106502123,-1.52131278661257,
8.85049129520029));
#399984=CARTESIAN_POINT('Origin',(-2.19071182494582,-1.52814573469578,7.59394543036555));
#399985=CARTESIAN_POINT('Ctrl Pts',(-2.18431026219255,-1.5307151239013,
7.59443877723642));
#399986=CARTESIAN_POINT('Ctrl Pts',(-2.1817224050621,-1.52553475816893,
7.58783886950016));
#399987=CARTESIAN_POINT('Ctrl Pts',(-2.18823340177431,-1.52008626265638,
7.58559994247159));
#399988=CARTESIAN_POINT('Ctrl Pts',(-2.19843729834314,-1.55899458844882,
7.56670252222135));
#399989=CARTESIAN_POINT('Ctrl Pts',(-2.19585318140097,-1.55382170981567,
7.56004874999027));
#399990=CARTESIAN_POINT('Ctrl Pts',(-2.20238904649611,-1.54832454466309,
7.55786368756704));
#399991=CARTESIAN_POINT('Ctrl Pts',(-2.2125379536652,-1.58722124392178,
7.53888913333558));
#399992=CARTESIAN_POINT('Ctrl Pts',(-2.20993847918949,-1.58201762261763,
7.53222002137276));
#399993=CARTESIAN_POINT('Ctrl Pts',(-2.21651771578449,-1.57651161766423,
7.53005029815327));
#399994=CARTESIAN_POINT('Ctrl Pts',(-2.22661159009451,-1.61539381304489,
7.51101258149734));
#399995=CARTESIAN_POINT('Ctrl Pts',(-2.22398060526481,-1.61012711439532,
7.5043616886572));
#399996=CARTESIAN_POINT('Ctrl Pts',(-2.2306187854571,-1.60464605197282,
7.50217374673251));
#399997=CARTESIAN_POINT('',(-2.22986633334693,-1.60314476287808,7.50366116523517));
#399998=CARTESIAN_POINT('Ctrl Pts',(-2.22277754110615,-1.60771882366397,
7.51860402984325));
#399999=CARTESIAN_POINT('Ctrl Pts',(-2.22297489374258,-1.6081138836628,
7.51734760759494));
#400000=CARTESIAN_POINT('Ctrl Pts',(-2.22320645518636,-1.60844428819929,
7.51608817408573));
#400001=CARTESIAN_POINT('Ctrl Pts',(-2.22348262824042,-1.6087016133381,
7.5148100591312));
#400002=CARTESIAN_POINT('Ctrl Pts',(-2.22373279239217,-1.60893470459781,
7.51365231206384));
#400003=CARTESIAN_POINT('Ctrl Pts',(-2.22401974321264,-1.60910834456724,
7.51247773061042));
#400004=CARTESIAN_POINT('Ctrl Pts',(-2.22435763202006,-1.60918793729049,
7.51129758471022));
#400005=CARTESIAN_POINT('Ctrl Pts',(-2.22477758921932,-1.60928686195565,
7.50983079813402));
#400006=CARTESIAN_POINT('Ctrl Pts',(-2.22526581718584,-1.60922467093318,
7.50839324291155));
#400007=CARTESIAN_POINT('Ctrl Pts',(-2.22581546211117,-1.60891913153019,
7.50715379678855));
#400008=CARTESIAN_POINT('Ctrl Pts',(-2.22606938222904,-1.60877798112991,
7.50658120839351));
#400009=CARTESIAN_POINT('Ctrl Pts',(-2.22636789030147,-1.60855652531023,
7.50598221009429));
#400010=CARTESIAN_POINT('Ctrl Pts',(-2.22669032953811,-1.60824176621978,
7.50545747549611));
#400011=CARTESIAN_POINT('Ctrl Pts',(-2.22686239309521,-1.60807380102642,
7.50517746087247));
#400012=CARTESIAN_POINT('Ctrl Pts',(-2.22704327857473,-1.60787759016943,
7.50491486231392));
#400013=CARTESIAN_POINT('Ctrl Pts',(-2.22722696943707,-1.60765719904463,
7.50468370960992));
#400014=CARTESIAN_POINT('Ctrl Pts',(-2.22750164521828,-1.60732764479462,
7.50433806340447));
#400015=CARTESIAN_POINT('Ctrl Pts',(-2.22779040260933,-1.60693378573885,
7.50405484070984));
#400016=CARTESIAN_POINT('Ctrl Pts',(-2.22807321658152,-1.60650172397162,
7.50385766036131));
#400017=CARTESIAN_POINT('Ctrl Pts',(-2.22810345913992,-1.60645552168138,
7.50383657498791));
#400018=CARTESIAN_POINT('Ctrl Pts',(-2.22813363242865,-1.60640891087603,
7.50381643264937));
#400019=CARTESIAN_POINT('Ctrl Pts',(-2.22816371133269,-1.60636194407087,
7.50379723213559));
#400020=CARTESIAN_POINT('Ctrl Pts',(-2.22836449785661,-1.60604842528247,
7.50366906242519));
#400021=CARTESIAN_POINT('Ctrl Pts',(-2.22856484065419,-1.60571183559279,
7.50358235568538));
#400022=CARTESIAN_POINT('Ctrl Pts',(-2.22875014780004,-1.60538276269125,
7.5035341175365));
#400023=CARTESIAN_POINT('Ctrl Pts',(-2.22902799489253,-1.60488935511924,
7.50346178989176));
#400024=CARTESIAN_POINT('Ctrl Pts',(-2.22930591601758,-1.60434674711438,
7.50346967198527));
#400025=CARTESIAN_POINT('Ctrl Pts',(-2.22956235809399,-1.60380567910415,
7.50354272648692));
#400026=CARTESIAN_POINT('Ctrl Pts',(-2.22966783802805,-1.6035831266321,
7.50357277531559));
#400027=CARTESIAN_POINT('Ctrl Pts',(-2.22976967202096,-1.60336119113259,
7.50361331098761));
#400028=CARTESIAN_POINT('Ctrl Pts',(-2.22986633334808,-1.6031447628789,
7.50366116523658));
#400029=CARTESIAN_POINT('',(-2.19311322794424,-1.52982084947218,7.57603338622103));
#400030=CARTESIAN_POINT('Origin',(-2.20036267203955,-1.53487426909768,7.58486873427629));
#400031=CARTESIAN_POINT('Ctrl Pts',(-2.22986633336772,-1.60314476293152,
7.50366116529969));
#400032=CARTESIAN_POINT('Ctrl Pts',(-2.21763603662393,-1.5787429670886,
7.5278357307971));
#400033=CARTESIAN_POINT('Ctrl Pts',(-2.20538559594532,-1.55430280858916,
7.55196141284068));
#400034=CARTESIAN_POINT('Ctrl Pts',(-2.1931132281663,-1.52982085070438,
7.57603338728831));
#400035=CARTESIAN_POINT('Ctrl Pts',(-2.18517840491731,-1.53205954976697,
7.59639677331371));
#400036=CARTESIAN_POINT('Ctrl Pts',(-2.17402775867868,-1.51650765230946,
7.59974925422225));
#400037=CARTESIAN_POINT('Ctrl Pts',(-2.19247376689057,-1.52160109977802,
7.59639677331372));
#400038=CARTESIAN_POINT('Ctrl Pts',(-2.18242551594711,-1.52929609063005,
7.58707626057422));
#400039=CARTESIAN_POINT('Ctrl Pts',(-2.1824791983704,-1.52240301078146,
7.58811717123964));
#400040=CARTESIAN_POINT('Ctrl Pts',(-2.18892959610593,-1.51997200262531,
7.58707626057424));
#400041=CARTESIAN_POINT('Ctrl Pts',(-2.18850179951101,-1.52922968044567,
7.58015376756929));
#400042=CARTESIAN_POINT('Ctrl Pts',(-2.18814772189234,-1.52635712740384,
7.58208760766041));
#400043=CARTESIAN_POINT('Ctrl Pts',(-2.19096580824873,-1.52569733863038,
7.5801537675693));
#400044=CARTESIAN_POINT('Ctrl Pts',(-2.19311322726537,-1.52982084899888,
7.57603338509286));
#400045=CARTESIAN_POINT('Ctrl Pts',(-2.19311322726537,-1.52982084899888,
7.57603338509286));
#400046=CARTESIAN_POINT('Ctrl Pts',(-2.19311322726537,-1.52982084899888,
7.57603338509286));
#400047=CARTESIAN_POINT('Origin',(-2.20035940734054,-1.53487894928956,7.58486873427621));
#400048=CARTESIAN_POINT('Ctrl Pts',(-2.28501686554784,-1.53170708783975,
7.51098857897448));
#400049=CARTESIAN_POINT('Ctrl Pts',(-2.27916555827345,-1.53105692235888,
7.50433767179957));
#400050=CARTESIAN_POINT('Ctrl Pts',(-2.27631435376175,-1.53917964874323,
7.50214974420965));
#400051=CARTESIAN_POINT('Ctrl Pts',(-2.25370825427415,-1.52822824501889,
7.5388732158917));
#400052=CARTESIAN_POINT('Ctrl Pts',(-2.24792705604509,-1.52758586967431,
7.53220407452063));
#400053=CARTESIAN_POINT('Ctrl Pts',(-2.24503206325589,-1.53566187962183,
7.53003438070911));
#400054=CARTESIAN_POINT('Ctrl Pts',(-2.22233951891752,-1.52474272153652,
7.56669465659234));
#400055=CARTESIAN_POINT('Ctrl Pts',(-2.21659248649516,-1.52410414251082,
7.56004085833299));
#400056=CARTESIAN_POINT('Ctrl Pts',(-2.21369080731583,-1.53213638429416,
7.55785582193789));
#400057=CARTESIAN_POINT('Ctrl Pts',(-2.19091207816031,-1.52125067502892,
7.59443891967696));
#400058=CARTESIAN_POINT('Ctrl Pts',(-2.18515671325649,-1.52061117014312,
7.58783901202978));
#400059=CARTESIAN_POINT('Ctrl Pts',(-2.1822921429825,-1.52860325467306,
7.58560008491213));
#400060=CARTESIAN_POINT('',(-2.27461864350411,-1.53898896096138,7.50366116523517));
#400061=CARTESIAN_POINT('Ctrl Pts',(-2.27461864350442,-1.53898896096159,
7.50366116523554));
#400062=CARTESIAN_POINT('Ctrl Pts',(-2.27516108906423,-1.5384599143366,
7.50350835821027));
#400063=CARTESIAN_POINT('Ctrl Pts',(-2.27564251620971,-1.53795594418397,
7.50345484956));
#400064=CARTESIAN_POINT('Ctrl Pts',(-2.27607767238034,-1.53746248185761,
7.50349758195598));
#400065=CARTESIAN_POINT('Ctrl Pts',(-2.2763009397679,-1.53720929908806,
7.50351950684424));
#400066=CARTESIAN_POINT('Ctrl Pts',(-2.27653412976726,-1.53693401335552,
7.50357029184312));
#400067=CARTESIAN_POINT('Ctrl Pts',(-2.27675169537738,-1.53666237746654,
7.50365515313923));
#400068=CARTESIAN_POINT('Ctrl Pts',(-2.27708639938674,-1.53624449147305,
7.50378570417639));
#400069=CARTESIAN_POINT('Ctrl Pts',(-2.27739422114995,-1.53582319390498,
7.50400001621911));
#400070=CARTESIAN_POINT('Ctrl Pts',(-2.27764989774498,-1.53542921218322,
7.50428903009635));
#400071=CARTESIAN_POINT('Ctrl Pts',(-2.27767827587996,-1.53538548324322,
7.50432110841318));
#400072=CARTESIAN_POINT('Ctrl Pts',(-2.27770603964485,-1.53534207924711,
7.50435406373354));
#400073=CARTESIAN_POINT('Ctrl Pts',(-2.27773317506315,-1.53529903339034,
7.50438785222352));
#400074=CARTESIAN_POINT('Ctrl Pts',(-2.27789884983483,-1.53503621774426,
7.50459414719561));
#400075=CARTESIAN_POINT('Ctrl Pts',(-2.27804330321256,-1.53478229309382,
7.50483629897752));
#400076=CARTESIAN_POINT('Ctrl Pts',(-2.27816214511761,-1.53454763795562,
7.5050991045531));
#400077=CARTESIAN_POINT('Ctrl Pts',(-2.27842432229669,-1.53402996515188,
7.50567888004914));
#400078=CARTESIAN_POINT('Ctrl Pts',(-2.2785726469613,-1.53358591053842,
7.50637912803144));
#400079=CARTESIAN_POINT('Ctrl Pts',(-2.27863797653866,-1.53321727343212,
7.50710440483569));
#400080=CARTESIAN_POINT('Ctrl Pts',(-2.278653996648,-1.53312687629518,7.50728225710685));
#400081=CARTESIAN_POINT('Ctrl Pts',(-2.27866548865364,-1.53303924015845,
7.50746498566954));
#400082=CARTESIAN_POINT('Ctrl Pts',(-2.27867259735185,-1.53295646489845,
7.50764697238949));
#400083=CARTESIAN_POINT('Ctrl Pts',(-2.27871081175708,-1.53251148788104,
7.50862528291182));
#400084=CARTESIAN_POINT('Ctrl Pts',(-2.27862994836162,-1.53216694270042,
7.50965856837423));
#400085=CARTESIAN_POINT('Ctrl Pts',(-2.27848810672668,-1.5318908944724,
7.51067959873204));
#400086=CARTESIAN_POINT('Ctrl Pts',(-2.27841005109607,-1.53173898478433,
7.5112414730258));
#400087=CARTESIAN_POINT('Ctrl Pts',(-2.27831312390072,-1.53160797959289,
7.51180065547253));
#400088=CARTESIAN_POINT('Ctrl Pts',(-2.27820463850915,-1.53149388563419,
7.51235175716501));
#400089=CARTESIAN_POINT('Ctrl Pts',(-2.27782977826581,-1.53109964555724,
7.51425603304536));
#400090=CARTESIAN_POINT('Ctrl Pts',(-2.27726782574237,-1.53086449499047,
7.5162690050518));
#400091=CARTESIAN_POINT('Ctrl Pts',(-2.27657644598839,-1.5307706179452,
7.51827788969243));
#400092=CARTESIAN_POINT('Ctrl Pts',(-2.27653902720958,-1.53076553714211,
7.51838661432545));
#400093=CARTESIAN_POINT('Ctrl Pts',(-2.27650122102355,-1.53076087567597,
7.51849533314856));
#400094=CARTESIAN_POINT('Ctrl Pts',(-2.27646303399419,-1.53075663254069,
7.51860402984325));
#400095=CARTESIAN_POINT('Ctrl Pts',(-2.19311322917843,-1.5298208492555,
7.57603338728985));
#400096=CARTESIAN_POINT('Ctrl Pts',(-2.22032722053524,-1.53288286616341,
7.55196141284922));
#400097=CARTESIAN_POINT('Ctrl Pts',(-2.24749441165089,-1.53593874122896,
7.52783573083105));
#400098=CARTESIAN_POINT('Ctrl Pts',(-2.27461864356328,-1.53898896096256,
7.50366116530176));
#400099=CARTESIAN_POINT('Origin',(-7.57821998246247E-16,-5.28623820391016E-16,
7.49482233047033));
#400100=CARTESIAN_POINT('Origin',(-2.2226897170392,-1.59798519134822,7.49482233047033));
#400101=CARTESIAN_POINT('Origin',(0.,0.,7.50366116523517));
#400102=CARTESIAN_POINT('Origin',(-2.26729799607036,-1.53403586888161,7.49482233047033));
#400103=CARTESIAN_POINT('Ctrl Pts',(-2.22277706837911,-1.60771787746033,
7.51860402984325));
#400104=CARTESIAN_POINT('Ctrl Pts',(-2.22617803012197,-1.61452447317726,
7.51860402984325));
#400105=CARTESIAN_POINT('Ctrl Pts',(-2.22169380199589,-1.62067166636955,
7.51860402984325));
#400106=CARTESIAN_POINT('Ctrl Pts',(-2.22403986754687,-1.61024521346863,
7.51041458714366));
#400107=CARTESIAN_POINT('Ctrl Pts',(-2.22511565711965,-1.61598080781928,
7.51004642900442));
#400108=CARTESIAN_POINT('Ctrl Pts',(-2.22169256529901,-1.62067336169245,
7.5072913648301));
#400109=CARTESIAN_POINT('Ctrl Pts',(-2.22683740462711,-1.60993292596653,
7.50215815450137));
#400110=CARTESIAN_POINT('Ctrl Pts',(-2.22727886798614,-1.61301564791053,
7.4987716367153));
#400111=CARTESIAN_POINT('Ctrl Pts',(-2.22526486157011,-1.61581702288554,
7.4948158853317));
#400112=CARTESIAN_POINT('Ctrl Pts',(-2.2298658863588,-1.60314444151892,
7.50366171572174));
#400113=CARTESIAN_POINT('Ctrl Pts',(-2.23283898515376,-1.60528192738146,
7.50000045605858));
#400114=CARTESIAN_POINT('Ctrl Pts',(-2.23283898515369,-1.60528192738156,
7.49482233047317));
#400115=CARTESIAN_POINT('Origin',(-2.211595193805,-1.61330497697696,7.51860402984325));
#400116=CARTESIAN_POINT('Origin',(-2.211595193805,-1.61330497697696,9.));
#400117=CARTESIAN_POINT('Origin',(-2.211595193805,-1.61330497697696,8.75721825406948));
#400118=CARTESIAN_POINT('Ctrl Pts',(-2.21531434125615,-1.59277907704497,
8.78942910404912));
#400119=CARTESIAN_POINT('Ctrl Pts',(-2.21782269718833,-1.59775507736844,
8.79672699501691));
#400120=CARTESIAN_POINT('Ctrl Pts',(-2.21072551350639,-1.60316834530628,
8.79893251111267));
#400121=CARTESIAN_POINT('Ctrl Pts',(-2.22022762891699,-1.60261447348346,
8.78111911759583));
#400122=CARTESIAN_POINT('Ctrl Pts',(-2.22319466688172,-1.60851693024666,
8.78644465894813));
#400123=CARTESIAN_POINT('Ctrl Pts',(-2.21795342948707,-1.61470117978466,
8.78817647674132));
#400124=CARTESIAN_POINT('Ctrl Pts',(-2.22328970695173,-1.6087441271545,
8.76780923932029));
#400125=CARTESIAN_POINT('Ctrl Pts',(-2.22678761706441,-1.61571401679595,
8.76988516158374));
#400126=CARTESIAN_POINT('Ctrl Pts',(-2.22245839467586,-1.62191032326892,
8.77093053738833));
#400127=CARTESIAN_POINT('Ctrl Pts',(-2.22269264364088,-1.60754892857963,
8.75371302330492));
#400128=CARTESIAN_POINT('Ctrl Pts',(-2.22610538539148,-1.61434741334548,
8.75300828287559));
#400129=CARTESIAN_POINT('Ctrl Pts',(-2.22157935547678,-1.62050448996881,
8.75267964240738));
#400130=CARTESIAN_POINT('Origin',(-2.20532861076148,-1.60076054719536,8.78727029226991));
#400131=CARTESIAN_POINT('Ctrl Pts',(-2.18456153393018,-1.53121811901793,
8.85049129520029));
#400132=CARTESIAN_POINT('Ctrl Pts',(-2.18717121304408,-1.53644216794051,
8.85711686593484));
#400133=CARTESIAN_POINT('Ctrl Pts',(-2.18059607577691,-1.54190736071221,
8.85933012996512));
#400134=CARTESIAN_POINT('Ctrl Pts',(-2.19522683681492,-1.55256789483801,
8.82945683644723));
#400135=CARTESIAN_POINT('Ctrl Pts',(-2.19785817784331,-1.55783530652517,
8.8360746990239));
#400136=CARTESIAN_POINT('Ctrl Pts',(-2.19123976416883,-1.56328770443169,
8.83829567148519));
#400137=CARTESIAN_POINT('Ctrl Pts',(-2.20587624220565,-1.57388584709558,
8.80838214965003));
#400138=CARTESIAN_POINT('Ctrl Pts',(-2.20851796773429,-1.57917404644855,
8.81501364461988));
#400139=CARTESIAN_POINT('Ctrl Pts',(-2.20186790511426,-1.58463531733958,
8.81722098428721));
#400140=CARTESIAN_POINT('Ctrl Pts',(-2.21651095806263,-1.59517439388236,
8.78727029226991));
#400141=CARTESIAN_POINT('Ctrl Pts',(-2.21915312239055,-1.60046347162264,
8.79393457792714));
#400142=CARTESIAN_POINT('Ctrl Pts',(-2.21248169808584,-1.60595268950177,
8.79610912703474));
#400143=CARTESIAN_POINT('Origin',(-2.17337918662903,-1.53680427233093,8.85049129520029));
#400144=CARTESIAN_POINT('Ctrl Pts',(-2.19147106502123,-1.52131278661257,
8.85049129520029));
#400145=CARTESIAN_POINT('Ctrl Pts',(-2.19727496193952,-1.52195768411219,
8.85711686593484));
#400146=CARTESIAN_POINT('Ctrl Pts',(-2.20013305013606,-1.51389963881729,
8.85933012996512));
#400147=CARTESIAN_POINT('Ctrl Pts',(-2.18633644119776,-1.52074225510384,
8.86332496987231));
#400148=CARTESIAN_POINT('Ctrl Pts',(-2.18920666304214,-1.51712096790993,
8.86648636486737));
#400149=CARTESIAN_POINT('Ctrl Pts',(-2.18576683858332,-1.51232058151034,
8.87206031107457));
#400150=CARTESIAN_POINT('Ctrl Pts',(-2.18223709983611,-1.52656507284068,
8.86341338519877));
#400151=CARTESIAN_POINT('Ctrl Pts',(-2.17979784447351,-1.53050506064653,
8.86654584966059));
#400152=CARTESIAN_POINT('Ctrl Pts',(-2.17410071658646,-1.52887200013751,
8.87215952290715));
#400153=CARTESIAN_POINT('Ctrl Pts',(-2.18456153393018,-1.53121811901793,
8.85049129520029));
#400154=CARTESIAN_POINT('Ctrl Pts',(-2.18717121304408,-1.53644216794051,
8.85711686593484));
#400155=CARTESIAN_POINT('Ctrl Pts',(-2.18059607577691,-1.54190736071221,
8.85933012996512));
#400156=CARTESIAN_POINT('Origin',(-2.19285150152199,-1.50888924464309,8.85049129520029));
#400157=CARTESIAN_POINT('Ctrl Pts',(-2.26252622397767,-1.52920804991441,
8.78727029226991));
#400158=CARTESIAN_POINT('Ctrl Pts',(-2.26840236764559,-1.52986097508042,
8.79393457792714));
#400159=CARTESIAN_POINT('Ctrl Pts',(-2.27124974846884,-1.52170427000879,
8.79610912703474));
#400160=CARTESIAN_POINT('Ctrl Pts',(-2.23887473584625,-1.52658002502472,
8.80838214965001));
#400161=CARTESIAN_POINT('Ctrl Pts',(-2.24474990362948,-1.52723284175572,
8.81501364461986));
#400162=CARTESIAN_POINT('Ctrl Pts',(-2.24757843466631,-1.5191058358637,
8.81722098428721));
#400163=CARTESIAN_POINT('Ctrl Pts',(-2.21519057835742,-1.5239483700935,
8.82945683644723));
#400164=CARTESIAN_POINT('Ctrl Pts',(-2.22104265112923,-1.52459862063229,
8.83607469902389));
#400165=CARTESIAN_POINT('Ctrl Pts',(-2.22387378559008,-1.51650438069502,
8.8382956714852));
#400166=CARTESIAN_POINT('Ctrl Pts',(-2.19147106502123,-1.52131278661257,
8.85049129520029));
#400167=CARTESIAN_POINT('Ctrl Pts',(-2.19727496193952,-1.52195768411219,
8.85711686593484));
#400168=CARTESIAN_POINT('Ctrl Pts',(-2.20013305013606,-1.51389963881729,
8.85933012996512));
#400169=CARTESIAN_POINT('Origin',(-2.26390666047843,-1.51678450794493,8.78727029226991));
#400170=CARTESIAN_POINT('Ctrl Pts',(-2.2762790074659,-1.53073616595188,
8.75374538247848));
#400171=CARTESIAN_POINT('Ctrl Pts',(-2.28383003900887,-1.53158839891579,
8.75304829418601));
#400172=CARTESIAN_POINT('Ctrl Pts',(-2.28804536797155,-1.5252243086473,
8.75272238421917));
#400173=CARTESIAN_POINT('Ctrl Pts',(-2.27759091723009,-1.53088193866796,
8.76769408445021));
#400174=CARTESIAN_POINT('Ctrl Pts',(-2.28533204362691,-1.53175493184132,
8.7697431809397));
#400175=CARTESIAN_POINT('Ctrl Pts',(-2.28965015289765,-1.52556039476369,
8.77077869880429));
#400176=CARTESIAN_POINT('Ctrl Pts',(-2.27086681512297,-1.53013479078126,
8.78108014887988));
#400177=CARTESIAN_POINT('Ctrl Pts',(-2.27742671510839,-1.53087839651124,
8.78639403366323));
#400178=CARTESIAN_POINT('Ctrl Pts',(-2.2814316297261,-1.52384399997465,
8.78812224174741));
#400179=CARTESIAN_POINT('Ctrl Pts',(-2.25984749613409,-1.5289103802946,
8.78944554828685));
#400180=CARTESIAN_POINT('Ctrl Pts',(-2.2653753061266,-1.52954262574045,
8.79673892988686));
#400181=CARTESIAN_POINT('Ctrl Pts',(-2.26800404459053,-1.52102245623481,
8.79894799272499));
#400182=CARTESIAN_POINT('Origin',(-2.27784347049495,-1.51833309057122,8.75721825406948));
#400183=CARTESIAN_POINT('Origin',(-2.27784347049495,-1.51833309057122,9.));
#400184=CARTESIAN_POINT('Origin',(-2.27784347049495,-1.51833309057122,7.51860402984325));
#400185=CARTESIAN_POINT('Ctrl Pts',(-2.27461799196034,-1.53898852013195,
7.50366195182966));
#400186=CARTESIAN_POINT('Ctrl Pts',(-2.2776509549566,-1.54104059887638,
7.50000065167735));
#400187=CARTESIAN_POINT('Ctrl Pts',(-2.27765095495667,-1.54104059887629,
7.49482233047108));
#400188=CARTESIAN_POINT('Ctrl Pts',(-2.27994696402869,-1.53379661717625,
7.50215800491337));
#400189=CARTESIAN_POINT('Ctrl Pts',(-2.28299322537738,-1.53314470539552,
7.49877273257265));
#400190=CARTESIAN_POINT('Ctrl Pts',(-2.28492774039884,-1.53028554328369,
7.49481816995647));
#400191=CARTESIAN_POINT('Ctrl Pts',(-2.2792643415883,-1.53106823982956,
7.51043025814043));
#400192=CARTESIAN_POINT('Ctrl Pts',(-2.28502241637527,-1.53010008088879,
7.51006209594515));
#400193=CARTESIAN_POINT('Ctrl Pts',(-2.28824598651205,-1.52526401164451,
7.50731281821701));
#400194=CARTESIAN_POINT('Ctrl Pts',(-2.27646153184158,-1.53075646553772,
7.51860402984326));
#400195=CARTESIAN_POINT('Ctrl Pts',(-2.28402415878926,-1.53159770928414,
7.51860402984326));
#400196=CARTESIAN_POINT('Ctrl Pts',(-2.28824458223237,-1.52526611838204,
7.51860402984327));
#400197=CARTESIAN_POINT('Origin',(0.,0.,7.5));
#400198=CARTESIAN_POINT('Origin',(-2.08949760778587,-1.65859511954946,7.5));
#400199=CARTESIAN_POINT('',(-2.08949760778587,-1.65859511954946,7.59394543036555));
#400200=CARTESIAN_POINT('',(-2.08949760778587,-1.65859511954946,8.85049129520029));
#400201=CARTESIAN_POINT('',(-2.08949760778587,-1.65859511954946,7.5));
#400202=CARTESIAN_POINT('',(-2.15990092504104,-1.67102668085119,8.78727029226991));
#400203=CARTESIAN_POINT('Ctrl Pts',(-2.08949760778587,-1.65859511954946,
8.85049129520029));
#400204=CARTESIAN_POINT('Ctrl Pts',(-2.1129994928842,-1.66274499680947,
8.82945686509571));
#400205=CARTESIAN_POINT('Ctrl Pts',(-2.13646643958853,-1.66688870477513,
8.80838212259895));
#400206=CARTESIAN_POINT('Ctrl Pts',(-2.15990092504104,-1.67102668085119,
8.78727029226991));
#400207=CARTESIAN_POINT('',(-2.17370988235714,-1.67346501623198,8.75721825406948));
#400208=CARTESIAN_POINT('Origin',(-2.13215390434231,-1.66612741793497,8.75937679713138));
#400209=CARTESIAN_POINT('',(-2.17370988235714,-1.67346501623198,7.51860402984325));
#400210=CARTESIAN_POINT('',(-2.17370988235714,-1.67346501623198,7.5));
#400211=CARTESIAN_POINT('Ctrl Pts',(-2.17370988235714,-1.67346501623198,
7.51860402984325));
#400212=CARTESIAN_POINT('Ctrl Pts',(-2.16286509408444,-1.67155008302325,
7.52834476460825));
#400213=CARTESIAN_POINT('Ctrl Pts',(-2.15201326553169,-1.66963390666753,
7.53807742314407));
#400214=CARTESIAN_POINT('Ctrl Pts',(-2.14115416031211,-1.66771644542448,
7.54780169004674));
#400215=CARTESIAN_POINT('Ctrl Pts',(-2.12395392452886,-1.66467929044543,
7.5632044032688));
#400216=CARTESIAN_POINT('Ctrl Pts',(-2.10673541065635,-1.66163890798794,
7.57858609112103));
#400217=CARTESIAN_POINT('Ctrl Pts',(-2.08949760778587,-1.65859511954946,
7.59394543036555));
#400218=CARTESIAN_POINT('Origin',(-2.1888484874705,-1.92141752211061,7.5));
#400219=CARTESIAN_POINT('',(-2.11520370755652,-1.74682943894031,8.75721825406948));
#400220=CARTESIAN_POINT('',(-2.10975372425559,-1.73390928168094,8.78727029226991));
#400221=CARTESIAN_POINT('Origin',(-2.09591963389519,-1.70111310357778,8.75658640621024));
#400222=CARTESIAN_POINT('',(-2.0819676362413,-1.66803740521009,8.85049129520029));
#400223=CARTESIAN_POINT('Ctrl Pts',(-2.10975372425559,-1.73390928168094,
8.78727029226991));
#400224=CARTESIAN_POINT('Ctrl Pts',(-2.10050483228942,-1.71198313400681,
8.80838212259896));
#400225=CARTESIAN_POINT('Ctrl Pts',(-2.09124312883602,-1.69002661441764,
8.82945686509571));
#400226=CARTESIAN_POINT('Ctrl Pts',(-2.0819676362413,-1.66803740521009,
8.85049129520029));
#400227=CARTESIAN_POINT('',(-2.0819676362413,-1.66803740521009,7.59394543036555));
#400228=CARTESIAN_POINT('',(-2.0819676362413,-1.66803740521009,7.5));
#400229=CARTESIAN_POINT('',(-2.11520370755652,-1.7468294389403,7.51860402984325));
#400230=CARTESIAN_POINT('Ctrl Pts',(-2.0819676362413,-1.66803740521009,
7.59394543036555));
#400231=CARTESIAN_POINT('Ctrl Pts',(-2.08877088254284,-1.68416571372711,
7.57858609112103));
#400232=CARTESIAN_POINT('Ctrl Pts',(-2.09556651605252,-1.70027597476349,
7.56320440326857));
#400233=CARTESIAN_POINT('Ctrl Pts',(-2.10235493574598,-1.71636913416218,
7.54780169004651));
#400234=CARTESIAN_POINT('Ctrl Pts',(-2.10664070046775,-1.72652930367544,
7.53807742314383));
#400235=CARTESIAN_POINT('Ctrl Pts',(-2.11092359330638,-1.73668266487762,
7.52834476460825));
#400236=CARTESIAN_POINT('Ctrl Pts',(-2.11520370755652,-1.7468294389403,
7.51860402984325));
#400237=CARTESIAN_POINT('',(-2.11520370755652,-1.74682943894031,7.5));
#400238=CARTESIAN_POINT('Origin',(-2.08830213916381,-1.66536538392936,7.5));
#400239=CARTESIAN_POINT('Ctrl Pts',(-2.0819676362413,-1.66803740521009,
8.85049129520029));
#400240=CARTESIAN_POINT('Ctrl Pts',(-2.08189236821729,-1.66785896893733,
8.85097269580138));
#400241=CARTESIAN_POINT('Ctrl Pts',(-2.0818257999648,-1.66767951480866,
8.85143669361005));
#400242=CARTESIAN_POINT('Ctrl Pts',(-2.08176568593669,-1.66749047547276,
8.8519052845931));
#400243=CARTESIAN_POINT('Ctrl Pts',(-2.08164810671,-1.66712072652019,8.85282181883899));
#400244=CARTESIAN_POINT('Ctrl Pts',(-2.08155843158663,-1.66672375951531,
8.85372622499635));
#400245=CARTESIAN_POINT('Ctrl Pts',(-2.08151029317523,-1.6662899478711,
8.85462257735071));
#400246=CARTESIAN_POINT('Ctrl Pts',(-2.08147033037579,-1.66592981285161,
8.85536669723986));
#400247=CARTESIAN_POINT('Ctrl Pts',(-2.08145895303519,-1.66554420686675,
8.85610498449051));
#400248=CARTESIAN_POINT('Ctrl Pts',(-2.08149195894183,-1.66512735346751,
8.85681338218371));
#400249=CARTESIAN_POINT('Ctrl Pts',(-2.08152191185394,-1.66474905835301,
8.85745625420285));
#400250=CARTESIAN_POINT('Ctrl Pts',(-2.08158819609811,-1.66434023658327,
8.85808743050666));
#400251=CARTESIAN_POINT('Ctrl Pts',(-2.08171825097903,-1.66389283019907,
8.85866804508411));
#400252=CARTESIAN_POINT('Ctrl Pts',(-2.08177825548183,-1.66368640659199,
8.85893592806396));
#400253=CARTESIAN_POINT('Ctrl Pts',(-2.08185207387119,-1.66347172942508,
8.85919241173848));
#400254=CARTESIAN_POINT('Ctrl Pts',(-2.08194399665606,-1.66324796592625,
8.85943017985534));
#400255=CARTESIAN_POINT('Ctrl Pts',(-2.0820681196277,-1.66294581896174,
8.8597512372));
#400256=CARTESIAN_POINT('Ctrl Pts',(-2.08222900408983,-1.66261965786936,
8.86004599534706));
#400257=CARTESIAN_POINT('Ctrl Pts',(-2.08243405763912,-1.66227800874228,
8.86026130871721));
#400258=CARTESIAN_POINT('Ctrl Pts',(-2.08250913352459,-1.66215292136474,
8.86034014101235));
#400259=CARTESIAN_POINT('Ctrl Pts',(-2.08259124742369,-1.662023872527,8.86040910639692));
#400260=CARTESIAN_POINT('Ctrl Pts',(-2.08267844598716,-1.66189455867301,
8.86046313645506));
#400261=CARTESIAN_POINT('Ctrl Pts',(-2.08281451861518,-1.66169276548686,
8.86054744990829));
#400262=CARTESIAN_POINT('Ctrl Pts',(-2.08296680936883,-1.66148490081205,
8.86059655985668));
#400263=CARTESIAN_POINT('Ctrl Pts',(-2.08312531505842,-1.66128412250461,
8.86059725258816));
#400264=CARTESIAN_POINT('Ctrl Pts',(-2.08328418695947,-1.66108288031908,
8.86059794692011));
#400265=CARTESIAN_POINT('Ctrl Pts',(-2.08345314972536,-1.66088817171568,
8.86056369958366));
#400266=CARTESIAN_POINT('Ctrl Pts',(-2.08362014586833,-1.66070814983365,
8.86048590497774));
#400267=CARTESIAN_POINT('Ctrl Pts',(-2.08366372688957,-1.66066116948234,
8.86046560290182));
#400268=CARTESIAN_POINT('Ctrl Pts',(-2.08370780734365,-1.6606146397908,
8.86044257503091));
#400269=CARTESIAN_POINT('Ctrl Pts',(-2.08375100127772,-1.66056997598908,
8.86041778462583));
#400270=CARTESIAN_POINT('Ctrl Pts',(-2.08404164285482,-1.66026944402666,
8.86025097596201));
#400271=CARTESIAN_POINT('Ctrl Pts',(-2.08433138499249,-1.66001329577687,
8.8599848982295));
#400272=CARTESIAN_POINT('Ctrl Pts',(-2.08460615922178,-1.65980265990706,
8.85968173251461));
#400273=CARTESIAN_POINT('Ctrl Pts',(-2.08475149904638,-1.65969124559992,
8.85952137522076));
#400274=CARTESIAN_POINT('Ctrl Pts',(-2.08489533649675,-1.65959026561899,
8.85934740853961));
#400275=CARTESIAN_POINT('Ctrl Pts',(-2.08503474992656,-1.65949987168832,
8.8591675900182));
#400276=CARTESIAN_POINT('Ctrl Pts',(-2.08559456731288,-1.65913689307085,
8.85844552518694));
#400277=CARTESIAN_POINT('Ctrl Pts',(-2.08611304340986,-1.6589215545218,
8.85759444184122));
#400278=CARTESIAN_POINT('Ctrl Pts',(-2.08655155128532,-1.65878394965752,
8.85683498915135));
#400279=CARTESIAN_POINT('Ctrl Pts',(-2.08659743996664,-1.65876954967494,
8.85675551444996));
#400280=CARTESIAN_POINT('Ctrl Pts',(-2.08664245504371,-1.65875602081341,
8.8566769979365));
#400281=CARTESIAN_POINT('Ctrl Pts',(-2.08668655297731,-1.65874329607418,
8.85659965593547));
#400282=CARTESIAN_POINT('Ctrl Pts',(-2.08728178913533,-1.65857153689463,
8.85555568965886));
#400283=CARTESIAN_POINT('Ctrl Pts',(-2.0878786533853,-1.65849242956098,
8.85434650606346));
#400284=CARTESIAN_POINT('Ctrl Pts',(-2.08847927973752,-1.65849942215004,
8.85297329937117));
#400285=CARTESIAN_POINT('Ctrl Pts',(-2.08881709546394,-1.65850335505532,
8.85220095427747));
#400286=CARTESIAN_POINT('Ctrl Pts',(-2.08915623562913,-1.65853484129755,
8.85137579139183));
#400287=CARTESIAN_POINT('Ctrl Pts',(-2.08949760778587,-1.65859511954946,
8.85049129520029));
#400288=CARTESIAN_POINT('Origin',(-2.08830213916381,-1.66536538392936,7.59394543036555));
#400289=CARTESIAN_POINT('Ctrl Pts',(-2.08174910777617,-1.66751934451537,
7.59443877723642));
#400290=CARTESIAN_POINT('Ctrl Pts',(-2.0794984748478,-1.66218381782436,
7.58783886950016));
#400291=CARTESIAN_POINT('Ctrl Pts',(-2.08634518032501,-1.65716367782183,
7.58559994247159));
#400292=CARTESIAN_POINT('Ctrl Pts',(-2.0940352469014,-1.69664582818389,
7.56670252222139));
#400293=CARTESIAN_POINT('Ctrl Pts',(-2.09178786677668,-1.69131801284369,
7.5600487499903));
#400294=CARTESIAN_POINT('Ctrl Pts',(-2.09866250781647,-1.68625089652093,
7.55786368756705));
#400295=CARTESIAN_POINT('Ctrl Pts',(-2.10629844288932,-1.72571792105421,
7.53888913333559));
#400296=CARTESIAN_POINT('Ctrl Pts',(-2.10403770647443,-1.72035844224663,
7.53222002137282));
#400297=CARTESIAN_POINT('Ctrl Pts',(-2.11095619627074,-1.71528528310685,
7.53005029815326));
#400298=CARTESIAN_POINT('Ctrl Pts',(-2.11853814082205,-1.7547343075945,
7.51101258149734));
#400299=CARTESIAN_POINT('Ctrl Pts',(-2.1162500001739,-1.74930986216536,
7.5043616886572));
#400300=CARTESIAN_POINT('Ctrl Pts',(-2.12322571438818,-1.74426537083864,
7.50217374673251));
#400301=CARTESIAN_POINT('',(-2.12257099619412,-1.74271895653113,7.50366116523517));
#400302=CARTESIAN_POINT('Ctrl Pts',(-2.11520370755652,-1.74682943894031,
7.51860402984325));
#400303=CARTESIAN_POINT('Ctrl Pts',(-2.11537534312976,-1.74723633167283,
7.51734760759493));
#400304=CARTESIAN_POINT('Ctrl Pts',(-2.11558525971438,-1.74758089355041,
7.51608817408572));
#400305=CARTESIAN_POINT('Ctrl Pts',(-2.11584437846304,-1.74785538445544,
7.51481005913119));
#400306=CARTESIAN_POINT('Ctrl Pts',(-2.11607909441742,-1.7481040248764,
7.51365231206383));
#400307=CARTESIAN_POINT('Ctrl Pts',(-2.11635433051562,-1.74829569308608,
7.51247773061042));
#400308=CARTESIAN_POINT('Ctrl Pts',(-2.11668642557096,-1.74839677088776,
7.51129758471022));
#400309=CARTESIAN_POINT('Ctrl Pts',(-2.11709918179806,-1.74852239905173,
7.50983079813402));
#400310=CARTESIAN_POINT('Ctrl Pts',(-2.11759039124035,-1.74849161668061,
7.50839324291155));
#400311=CARTESIAN_POINT('Ctrl Pts',(-2.118158482838,-1.74822192091236,7.50715379678855));
#400312=CARTESIAN_POINT('Ctrl Pts',(-2.11842092478694,-1.74809732923853,
7.50658120839351));
#400313=CARTESIAN_POINT('Ctrl Pts',(-2.1187330082656,-1.74789545390144,
7.50598221009429));
#400314=CARTESIAN_POINT('Ctrl Pts',(-2.11907495170042,-1.74760200027013,
7.50545747549612));
#400315=CARTESIAN_POINT('Ctrl Pts',(-2.11925742330137,-1.74744540432923,
7.50517746087247));
#400316=CARTESIAN_POINT('Ctrl Pts',(-2.11945050840504,-1.74726118598095,
7.50491486231392));
#400317=CARTESIAN_POINT('Ctrl Pts',(-2.11964794236266,-1.74705301678731,
7.50468370960993));
#400318=CARTESIAN_POINT('Ctrl Pts',(-2.11994316840631,-1.74674173817957,
7.50433806340446));
#400319=CARTESIAN_POINT('Ctrl Pts',(-2.12025656715067,-1.74636718909903,
7.50405484070983));
#400320=CARTESIAN_POINT('Ctrl Pts',(-2.12056648234371,-1.74595413500245,
7.5038576603613));
#400321=CARTESIAN_POINT('Ctrl Pts',(-2.12059962295642,-1.74590996528715,
7.50383657498791));
#400322=CARTESIAN_POINT('Ctrl Pts',(-2.12063272061545,-1.74586538345795,
7.50381643264937));
#400323=CARTESIAN_POINT('Ctrl Pts',(-2.12066574689268,-1.74582044031312,
7.50379723213559));
#400324=CARTESIAN_POINT('Ctrl Pts',(-2.1208862080969,-1.74552043011945,
7.50366906242519));
#400325=CARTESIAN_POINT('Ctrl Pts',(-2.12110770464417,-1.74519736799651,
7.50358235568538));
#400326=CARTESIAN_POINT('Ctrl Pts',(-2.12131371482981,-1.74488084388013,
7.5035341175365));
#400327=CARTESIAN_POINT('Ctrl Pts',(-2.12162260378732,-1.74440625179124,
7.50346178989176));
#400328=CARTESIAN_POINT('Ctrl Pts',(-2.12193471890785,-1.74388256510034,
7.50346967198527));
#400329=CARTESIAN_POINT('Ctrl Pts',(-2.12222530044295,-1.74335903907261,
7.50354272648692));
#400330=CARTESIAN_POINT('Ctrl Pts',(-2.12234482264302,-1.74314370198106,
7.50357277531559));
#400331=CARTESIAN_POINT('Ctrl Pts',(-2.12246066686334,-1.74292874699817,
7.50361331098761));
#400332=CARTESIAN_POINT('Ctrl Pts',(-2.12257099619522,-1.74271895653203,
7.50366116523658));
#400333=CARTESIAN_POINT('',(-2.09059128325,-1.66719091542116,7.57603338622103));
#400334=CARTESIAN_POINT('Origin',(-2.09750205887796,-1.67269842573203,7.58486873427627));
#400335=CARTESIAN_POINT('Ctrl Pts',(-2.12257099621145,-1.7427189565858,
7.50366116529969));
#400336=CARTESIAN_POINT('Ctrl Pts',(-2.11192925635161,-1.71758369904671,
7.52783573079709));
#400337=CARTESIAN_POINT('Ctrl Pts',(-2.10126987184862,-1.69240886704498,
7.55196141284069));
#400338=CARTESIAN_POINT('Ctrl Pts',(-2.09059128339266,-1.66719091666507,
7.57603338728831));
#400339=CARTESIAN_POINT('Ctrl Pts',(-2.0824357048269,-1.66876158506199,
7.59642833564546));
#400340=CARTESIAN_POINT('Ctrl Pts',(-2.07320936503718,-1.65296337419292,
7.59959882295454));
#400341=CARTESIAN_POINT('Ctrl Pts',(-2.09047977720865,-1.65894708367391,
7.59639677331373));
#400342=CARTESIAN_POINT('Ctrl Pts',(-2.07997313262292,-1.66580784542594,
7.58710240504251));
#400343=CARTESIAN_POINT('Ctrl Pts',(-2.08056667580051,-1.65907270568811,
7.58809943920597));
#400344=CARTESIAN_POINT('Ctrl Pts',(-2.08704726491593,-1.65709425787427,
7.58707626057426));
#400345=CARTESIAN_POINT('Ctrl Pts',(-2.08602293135984,-1.66622189099849,
7.58020924244131));
#400346=CARTESIAN_POINT('Ctrl Pts',(-2.08590041445982,-1.66340905174837,
7.58205880659759));
#400347=CARTESIAN_POINT('Ctrl Pts',(-2.08871246990533,-1.66293829112231,
7.58015376756931));
#400348=CARTESIAN_POINT('Ctrl Pts',(-2.09059128260286,-1.66719091490534,
7.57603338509286));
#400349=CARTESIAN_POINT('Ctrl Pts',(-2.09059128260286,-1.66719091490534,
7.57603338509286));
#400350=CARTESIAN_POINT('Ctrl Pts',(-2.09059128260286,-1.66719091490534,
7.57603338509286));
#400351=CARTESIAN_POINT('Origin',(-2.09749850102522,-1.67270288713742,7.58486873427623));
#400352=CARTESIAN_POINT('Ctrl Pts',(-2.18218524326637,-1.67496156458801,
7.51098857897448));
#400353=CARTESIAN_POINT('Ctrl Pts',(-2.17638761437571,-1.6739378403976,
7.50433767179956));
#400354=CARTESIAN_POINT('Ctrl Pts',(-2.17302184310319,-1.68186120046916,
7.50214974420965));
#400355=CARTESIAN_POINT('Ctrl Pts',(-2.15116384911717,-1.66948391981123,
7.53887321589168));
#400356=CARTESIAN_POINT('Ctrl Pts',(-2.14543568610955,-1.6684724616534,
7.53220407452062));
#400357=CARTESIAN_POINT('Ctrl Pts',(-2.14202920965963,-1.67634639574748,
7.53003438070912));
#400358=CARTESIAN_POINT('Ctrl Pts',(-2.1200828824479,-1.66399575593586,
7.56669465659233));
#400359=CARTESIAN_POINT('Ctrl Pts',(-2.11438857181869,-1.66299027530768,
7.560040858333));
#400360=CARTESIAN_POINT('Ctrl Pts',(-2.11097822695242,-1.67082010276551,
7.55785582193789));
#400361=CARTESIAN_POINT('Ctrl Pts',(-2.08894374892624,-1.65849732116958,
7.59443891967696));
#400362=CARTESIAN_POINT('Ctrl Pts',(-2.08324118225558,-1.6574903827197,
7.58783901202978));
#400363=CARTESIAN_POINT('Ctrl Pts',(-2.07987044293451,-1.66528251300722,
7.58560008491213));
#400364=CARTESIAN_POINT('',(-2.17134183427226,-1.68156225994657,7.50366116523517));
#400365=CARTESIAN_POINT('Ctrl Pts',(-2.17134183427256,-1.6815622599468,
7.50366116523554));
#400366=CARTESIAN_POINT('Ctrl Pts',(-2.17191706145343,-1.68106905491119,
7.50350835821027));
#400367=CARTESIAN_POINT('Ctrl Pts',(-2.17242978893375,-1.6805969653624,
7.50345484956));
#400368=CARTESIAN_POINT('Ctrl Pts',(-2.17289566726916,-1.68013239745889,
7.50349758195598));
#400369=CARTESIAN_POINT('Ctrl Pts',(-2.17313469740567,-1.67989403967114,
7.50351950684424));
#400370=CARTESIAN_POINT('Ctrl Pts',(-2.17338504590861,-1.67963426007722,
7.50357029184312));
#400371=CARTESIAN_POINT('Ctrl Pts',(-2.173619568278,-1.6793771217698,7.50365515313924));
#400372=CARTESIAN_POINT('Ctrl Pts',(-2.17398035864961,-1.67898153892741,
7.50378570417639));
#400373=CARTESIAN_POINT('Ctrl Pts',(-2.17431454058786,-1.67858082916846,
7.50400001621911));
#400374=CARTESIAN_POINT('Ctrl Pts',(-2.17459493436348,-1.6782040381801,
7.50428903009635));
#400375=CARTESIAN_POINT('Ctrl Pts',(-2.17462605591535,-1.67816221727924,
7.50432110841318));
#400376=CARTESIAN_POINT('Ctrl Pts',(-2.17465654354018,-1.67812068129182,
7.50435406373354));
#400377=CARTESIAN_POINT('Ctrl Pts',(-2.17468638116337,-1.67807946244959,
7.50438785222352));
#400378=CARTESIAN_POINT('Ctrl Pts',(-2.17486855419472,-1.67782780160552,
7.50459414719561));
#400379=CARTESIAN_POINT('Ctrl Pts',(-2.1750289797857,-1.67758365383019,
7.50483629897752));
#400380=CARTESIAN_POINT('Ctrl Pts',(-2.17516261192364,-1.67735709504314,
7.5050991045531));
#400381=CARTESIAN_POINT('Ctrl Pts',(-2.175457417842,-1.67685728360323,7.50567888004914));
#400382=CARTESIAN_POINT('Ctrl Pts',(-2.17563388843445,-1.67642364454149,
7.50637912803145));
#400383=CARTESIAN_POINT('Ctrl Pts',(-2.17572270244567,-1.67605995052005,
7.50710440483569));
#400384=CARTESIAN_POINT('Ctrl Pts',(-2.17574448140443,-1.67597076552566,
7.50728225710685));
#400385=CARTESIAN_POINT('Ctrl Pts',(-2.17576156466507,-1.6758840457421,
7.50746498566954));
#400386=CARTESIAN_POINT('Ctrl Pts',(-2.17577396218682,-1.6758018960086,
7.50764697238949));
#400387=CARTESIAN_POINT('Ctrl Pts',(-2.17584060785185,-1.67536028164955,
7.50862528291182));
#400388=CARTESIAN_POINT('Ctrl Pts',(-2.17578198568442,-1.67501126343843,
7.50965856837422));
#400389=CARTESIAN_POINT('Ctrl Pts',(-2.17565812194903,-1.67472669455634,
7.51067959873202));
#400390=CARTESIAN_POINT('Ctrl Pts',(-2.17558995957922,-1.67457009594159,
7.51124147302579));
#400391=CARTESIAN_POINT('Ctrl Pts',(-2.17550162506262,-1.67443314976764,
7.51180065547253));
#400392=CARTESIAN_POINT('Ctrl Pts',(-2.17540067259095,-1.67431233954431,
7.512351757165));
#400393=CARTESIAN_POINT('Ctrl Pts',(-2.17505184158664,-1.67389489209763,
7.51425603304536));
#400394=CARTESIAN_POINT('Ctrl Pts',(-2.17450610980346,-1.67362422025112,
7.5162690050518));
#400395=CARTESIAN_POINT('Ctrl Pts',(-2.17382216528628,-1.67348623923338,
7.51827788969244));
#400396=CARTESIAN_POINT('Ctrl Pts',(-2.17378514891654,-1.67347877143995,
7.51838661432545));
#400397=CARTESIAN_POINT('Ctrl Pts',(-2.17374771906854,-1.67347169730064,
7.51849533314856));
#400398=CARTESIAN_POINT('Ctrl Pts',(-2.17370988235714,-1.67346501623197,
7.51860402984325));
#400399=CARTESIAN_POINT('Ctrl Pts',(-2.09059128449555,-1.667190915284,7.57603338728985));
#400400=CARTESIAN_POINT('Ctrl Pts',(-2.11755317769155,-1.67199024736255,
7.55196141284922));
#400401=CARTESIAN_POINT('Ctrl Pts',(-2.1444687603117,-1.67678045171609,
7.52783573083105));
#400402=CARTESIAN_POINT('Ctrl Pts',(-2.17134183433124,-1.68156225995155,
7.50366116530176));
#400403=CARTESIAN_POINT('Origin',(-7.22395927215198E-16,-5.76091528191156E-16,
7.49482233047033));
#400404=CARTESIAN_POINT('Origin',(-2.11573969989722,-1.73711017850879,7.49482233047033));
#400405=CARTESIAN_POINT('Origin',(0.,0.,7.50366116523517));
#400406=CARTESIAN_POINT('Origin',(-2.16435357359294,-1.67615030903422,7.49482233047033));
#400407=CARTESIAN_POINT('Ctrl Pts',(-2.11520329642423,-1.74682846439302,
7.51860402984325));
#400408=CARTESIAN_POINT('Ctrl Pts',(-2.11816117044153,-1.75383897559606,
7.51860402984325));
#400409=CARTESIAN_POINT('Ctrl Pts',(-2.11329230362297,-1.75968623323817,
7.51860402984325));
#400410=CARTESIAN_POINT('Ctrl Pts',(-2.11630157406165,-1.74943151553891,
7.51041458714367));
#400411=CARTESIAN_POINT('Ctrl Pts',(-2.11700767251761,-1.7552242515704,
7.51004642900444));
#400412=CARTESIAN_POINT('Ctrl Pts',(-2.11329096084731,-1.7596878458424,
7.50729136483011));
#400413=CARTESIAN_POINT('Ctrl Pts',(-2.11911337163088,-1.7492991084811,
7.50215815450137));
#400414=CARTESIAN_POINT('Ctrl Pts',(-2.11935641728299,-1.75240378129678,
7.49877163671527));
#400415=CARTESIAN_POINT('Ctrl Pts',(-2.11716706414825,-1.75507036271234,
7.49481588533168));
#400416=CARTESIAN_POINT('Ctrl Pts',(-2.12257057071394,-1.74271860719361,
7.50366171572174));
#400417=CARTESIAN_POINT('Ctrl Pts',(-2.12540061176914,-1.74504218845602,
7.50000045605858));
#400418=CARTESIAN_POINT('Ctrl Pts',(-2.12540061176906,-1.74504218845612,
7.49482233047317));
#400419=CARTESIAN_POINT('Origin',(-2.10368642951559,-1.75168765945072,7.51860402984325));
#400420=CARTESIAN_POINT('Origin',(-2.10368642951559,-1.75168765945072,9.));
#400421=CARTESIAN_POINT('Origin',(-2.10368642951559,-1.75168765945072,8.75721825406948));
#400422=CARTESIAN_POINT('Ctrl Pts',(-2.10871303450337,-1.73144221877687,
8.78942910404913));
#400423=CARTESIAN_POINT('Ctrl Pts',(-2.11089742331394,-1.73656870629036,
8.79672699501692));
#400424=CARTESIAN_POINT('Ctrl Pts',(-2.10346799228943,-1.74151613396892,
8.79893251111267));
#400425=CARTESIAN_POINT('Ctrl Pts',(-2.11298607127434,-1.74157220275977,
8.78111911759577));
#400426=CARTESIAN_POINT('Ctrl Pts',(-2.11556884143811,-1.74765263106761,
8.78644465894808));
#400427=CARTESIAN_POINT('Ctrl Pts',(-2.10994214649951,-1.75348836716885,
8.78817647674131));
#400428=CARTESIAN_POINT('Ctrl Pts',(-2.11564912968225,-1.74788545041324,
8.76780923932033));
#400429=CARTESIAN_POINT('Ctrl Pts',(-2.1186932906009,-1.7550651315393,8.76988516158378));
#400430=CARTESIAN_POINT('Ctrl Pts',(-2.11397596434525,-1.76097133280529,
8.77093053738833));
#400431=CARTESIAN_POINT('Ctrl Pts',(-2.11512986973763,-1.74665445352436,
8.75371302330491));
#400432=CARTESIAN_POINT('Ctrl Pts',(-2.1181000192298,-1.75365762518883,
8.75300828287558));
#400433=CARTESIAN_POINT('Ctrl Pts',(-2.11318880327528,-1.75951206770562,
8.75267964240738));
#400434=CARTESIAN_POINT('Origin',(-2.09823644621466,-1.73876750219136,8.78727029226991));
#400435=CARTESIAN_POINT('Ctrl Pts',(-2.0819676362413,-1.66803740521009,
8.85049129520029));
#400436=CARTESIAN_POINT('Ctrl Pts',(-2.08423724752591,-1.67341792347879,
8.85711686593484));
#400437=CARTESIAN_POINT('Ctrl Pts',(-2.07732546348032,-1.67845061693468,
8.85933012996512));
#400438=CARTESIAN_POINT('Ctrl Pts',(-2.09124314128408,-1.69002664392798,
8.82945683644723));
#400439=CARTESIAN_POINT('Ctrl Pts',(-2.09353159171458,-1.69545182375142,
8.83607469902389));
#400440=CARTESIAN_POINT('Ctrl Pts',(-2.08657743994754,-1.70046897590164,
8.83829567148519));
#400441=CARTESIAN_POINT('Ctrl Pts',(-2.10050482043861,-1.71198310591234,
8.80838214965002));
#400442=CARTESIAN_POINT('Ctrl Pts',(-2.10280230216299,-1.71742969602838,
8.81501364461993));
#400443=CARTESIAN_POINT('Ctrl Pts',(-2.09581599798245,-1.72245367517764,
8.81722098428721));
#400444=CARTESIAN_POINT('Ctrl Pts',(-2.10975372425559,-1.73390928168094,
8.78727029226991));
#400445=CARTESIAN_POINT('Ctrl Pts',(-2.11205158759922,-1.73935677649347,
8.79393457792714));
#400446=CARTESIAN_POINT('Ctrl Pts',(-2.1050421750542,-1.74440727656297,
8.79610912703474));
#400447=CARTESIAN_POINT('Origin',(-2.07045035820037,-1.67289562572051,8.85049129520029));
#400448=CARTESIAN_POINT('Ctrl Pts',(-2.08949760778587,-1.65859511954946,
8.85049129520029));
#400449=CARTESIAN_POINT('Ctrl Pts',(-2.09524826125081,-1.65961054899031,
8.85711686593484));
#400450=CARTESIAN_POINT('Ctrl Pts',(-2.09861675793328,-1.65175217815317,
8.85933012996512));
#400451=CARTESIAN_POINT('Ctrl Pts',(-2.08441008767702,-1.65769678378102,
8.86332496987232));
#400452=CARTESIAN_POINT('Ctrl Pts',(-2.08750642900991,-1.65426683265499,
8.86648636486738));
#400453=CARTESIAN_POINT('Ctrl Pts',(-2.08438123385197,-1.64925591885433,
8.87206031107457));
#400454=CARTESIAN_POINT('Ctrl Pts',(-2.07994609963853,-1.66324499221152,
8.86341338519876));
#400455=CARTESIAN_POINT('Ctrl Pts',(-2.07725942010221,-1.66702060126219,
8.86654584966059));
#400456=CARTESIAN_POINT('Ctrl Pts',(-2.0716786281215,-1.66502587981416,
8.87215952290713));
#400457=CARTESIAN_POINT('Ctrl Pts',(-2.0819676362413,-1.66803740521009,
8.85049129520029));
#400458=CARTESIAN_POINT('Ctrl Pts',(-2.08423724752591,-1.67341792347879,
8.85711686593484));
#400459=CARTESIAN_POINT('Ctrl Pts',(-2.07732546348032,-1.67845061693468,
8.85933012996512));
#400460=CARTESIAN_POINT('Origin',(-2.09167118709871,-1.64628554794966,8.85049129520029));
#400461=CARTESIAN_POINT('Ctrl Pts',(-2.15990092504104,-1.67102668085119,
8.78727029226991));
#400462=CARTESIAN_POINT('Ctrl Pts',(-2.16572316248256,-1.67205475032986,
8.79393457792714));
#400463=CARTESIAN_POINT('Ctrl Pts',(-2.16908729494479,-1.66409723639932,
8.79610912703474));
#400464=CARTESIAN_POINT('Ctrl Pts',(-2.13646640956138,-1.66688869947304,
8.80838214965003));
#400465=CARTESIAN_POINT('Ctrl Pts',(-2.14228768007073,-1.66791659821436,
8.81501364461985));
#400466=CARTESIAN_POINT('Ctrl Pts',(-2.14563109864247,-1.65998751473331,
8.81722098428721));
#400467=CARTESIAN_POINT('Ctrl Pts',(-2.11299952442461,-1.66274500237876,
8.82945683644721));
#400468=CARTESIAN_POINT('Ctrl Pts',(-2.1187979117902,-1.6637688604979,8.83607469902389));
#400469=CARTESIAN_POINT('Ctrl Pts',(-2.12214182911503,-1.65587264245239,
8.8382956714852));
#400470=CARTESIAN_POINT('Ctrl Pts',(-2.08949760778587,-1.65859511954946,
8.85049129520029));
#400471=CARTESIAN_POINT('Ctrl Pts',(-2.09524826125081,-1.65961054899031,
8.85711686593484));
#400472=CARTESIAN_POINT('Ctrl Pts',(-2.09861675793328,-1.65175217815317,
8.85933012996512));
#400473=CARTESIAN_POINT('Origin',(-2.16207450435388,-1.65871710925138,8.78727029226991));
#400474=CARTESIAN_POINT('Ctrl Pts',(-2.17352754522994,-1.67343280107381,
8.75374538247848));
#400475=CARTESIAN_POINT('Ctrl Pts',(-2.18100845961528,-1.67476707928573,
8.75304829418602));
#400476=CARTESIAN_POINT('Ctrl Pts',(-2.18562287639599,-1.66868614177718,
8.75272238421917));
#400477=CARTESIAN_POINT('Ctrl Pts',(-2.17482741984483,-1.6736623286314,
8.76769408445018));
#400478=CARTESIAN_POINT('Ctrl Pts',(-2.18249670840255,-1.67502950381778,
8.76974318093967));
#400479=CARTESIAN_POINT('Ctrl Pts',(-2.18720283100794,-1.66912435629184,
8.7707786988043));
#400480=CARTESIAN_POINT('Ctrl Pts',(-2.16816500305613,-1.67248590113899,
8.78108014887993));
#400481=CARTESIAN_POINT('Ctrl Pts',(-2.17466378204077,-1.67364827328635,
8.78639403366326));
#400482=CARTESIAN_POINT('Ctrl Pts',(-2.17911116346539,-1.66688492543245,
8.78812224174741));
#400483=CARTESIAN_POINT('Ctrl Pts',(-2.15724677268913,-1.67055799614333,
8.78944554828685));
#400484=CARTESIAN_POINT('Ctrl Pts',(-2.16272271709835,-1.67154311057534,
8.79673892988686));
#400485=CARTESIAN_POINT('Ctrl Pts',(-2.16589194367168,-1.6632088705234,
8.79894799272499));
#400486=CARTESIAN_POINT('Origin',(-2.17588346166998,-1.66115544463217,8.75721825406948));
#400487=CARTESIAN_POINT('Origin',(-2.17588346166998,-1.66115544463217,9.));
#400488=CARTESIAN_POINT('Origin',(-2.17588346166998,-1.66115544463217,7.51860402984325));
#400489=CARTESIAN_POINT('Ctrl Pts',(-2.1713412123112,-1.68156177827833,
7.50366195182966));
#400490=CARTESIAN_POINT('Ctrl Pts',(-2.17423646662313,-1.68380396341326,
7.50000065167735));
#400491=CARTESIAN_POINT('Ctrl Pts',(-2.1742364666232,-1.68380396341317,
7.49482233047108));
#400492=CARTESIAN_POINT('Ctrl Pts',(-2.1769918817994,-1.67672197105677,
7.50215800491337));
#400493=CARTESIAN_POINT('Ctrl Pts',(-2.18007365240864,-1.67626657333344,
7.49877273257265));
#400494=CARTESIAN_POINT('Ctrl Pts',(-2.18218737990697,-1.67353723047978,
7.49481816995649));
#400495=CARTESIAN_POINT('Ctrl Pts',(-2.17648546961679,-1.67395546368403,
7.51043025814043));
#400496=CARTESIAN_POINT('Ctrl Pts',(-2.18229374397787,-1.67335821504791,
7.51006209594516));
#400497=CARTESIAN_POINT('Ctrl Pts',(-2.18582053896442,-1.66873861687435,
7.50731281821699));
#400498=CARTESIAN_POINT('Ctrl Pts',(-2.17370839399078,-1.67346475332887,
7.51860402984326));
#400499=CARTESIAN_POINT('Ctrl Pts',(-2.18120158403841,-1.67478880782197,
7.51860402984326));
#400500=CARTESIAN_POINT('Ctrl Pts',(-2.18581900259085,-1.66874062931085,
7.51860402984327));
#400501=CARTESIAN_POINT('Origin',(0.,0.,7.5));
#400502=CARTESIAN_POINT('Origin',(-1.97893795668429,-1.78906192937259,7.5));
#400503=CARTESIAN_POINT('',(-1.97893795668429,-1.78906192937259,7.59394543036555));
#400504=CARTESIAN_POINT('',(-1.97893795668429,-1.78906192937259,8.85049129520029));
#400505=CARTESIAN_POINT('',(-1.97893795668429,-1.78906192937259,7.5));
#400506=CARTESIAN_POINT('',(-2.04840012990612,-1.80597870472226,8.78727029226991));
#400507=CARTESIAN_POINT('Ctrl Pts',(-1.97893795668429,-1.7890619293726,
8.85049129520029));
#400508=CARTESIAN_POINT('Ctrl Pts',(-2.00212567109017,-1.79470905121291,
8.82945686509571));
#400509=CARTESIAN_POINT('Ctrl Pts',(-2.02527891415478,-1.80034777792376,
8.80838212259896));
#400510=CARTESIAN_POINT('Ctrl Pts',(-2.04840012990612,-1.80597870472226,
8.78727029226991));
#400511=CARTESIAN_POINT('',(-2.06202449055417,-1.80929677321444,8.75721825406948));
#400512=CARTESIAN_POINT('Origin',(-2.02102401529018,-1.7993117501472,8.75937679713149));
#400513=CARTESIAN_POINT('',(-2.06202449055417,-1.80929677321444,7.51860402984325));
#400514=CARTESIAN_POINT('',(-2.06202449055417,-1.80929677321444,7.5));
#400515=CARTESIAN_POINT('Ctrl Pts',(-2.06202449055417,-1.80929677321444,
7.51860402984325));
#400516=CARTESIAN_POINT('Ctrl Pts',(-2.05132467425402,-1.80669094647109,
7.52834476460825));
#400517=CARTESIAN_POINT('Ctrl Pts',(-2.04061791178752,-1.80408342806264,
7.53807742314407));
#400518=CARTESIAN_POINT('Ctrl Pts',(-2.02990396992789,-1.80147416118915,
7.54780169004674));
#400519=CARTESIAN_POINT('Ctrl Pts',(-2.0129336650614,-1.79734122348038,
7.5632044032688));
#400520=CARTESIAN_POINT('Ctrl Pts',(-1.9959453264452,-1.79320389384317,
7.57858609112103));
#400521=CARTESIAN_POINT('Ctrl Pts',(-1.97893795668429,-1.7890619293726,
7.59394543036555));
#400522=CARTESIAN_POINT('Origin',(-2.0612456201833,-2.05770976783674,7.5));
#400523=CARTESIAN_POINT('',(-1.99893804826277,-1.8787619573583,8.75721825406948));
#400524=CARTESIAN_POINT('',(-1.99432705985483,-1.86551916431873,8.78727029226991));
#400525=CARTESIAN_POINT('Origin',(-1.98262265146148,-1.83190401626567,8.75658640620927));
#400526=CARTESIAN_POINT('',(-1.97081848695445,-1.79800236791134,8.85049129520029));
#400527=CARTESIAN_POINT('Ctrl Pts',(-1.99432705985483,-1.86551916431873,
8.78727029226991));
#400528=CARTESIAN_POINT('Ctrl Pts',(-1.98650198383396,-1.84304548772371,
8.80838212259896));
#400529=CARTESIAN_POINT('Ctrl Pts',(-1.97866606858371,-1.82054068078121,
8.82945686509571));
#400530=CARTESIAN_POINT('Ctrl Pts',(-1.97081848695445,-1.79800236791134,
8.85049129520029));
#400531=CARTESIAN_POINT('',(-1.97081848695445,-1.79800236791134,7.59394543036555));
#400532=CARTESIAN_POINT('',(-1.97081848695445,-1.79800236791134,7.5));
#400533=CARTESIAN_POINT('',(-1.99893804826277,-1.8787619573583,7.51860402984325));
#400534=CARTESIAN_POINT('Ctrl Pts',(-1.97081848695445,-1.79800236791134,
7.59394543036555));
#400535=CARTESIAN_POINT('Ctrl Pts',(-1.97657441098221,-1.81453342457588,
7.57858609112103));
#400536=CARTESIAN_POINT('Ctrl Pts',(-1.98232389416547,-1.83104598308701,
7.56320440326857));
#400537=CARTESIAN_POINT('Ctrl Pts',(-1.98806727405975,-1.84754101290681,
7.54780169004651));
#400538=CARTESIAN_POINT('Ctrl Pts',(-1.9916932689225,-1.85795489715064,
7.53807742314383));
#400539=CARTESIAN_POINT('Ctrl Pts',(-1.99531683401268,-1.86836180306961,
7.52834476460825));
#400540=CARTESIAN_POINT('Ctrl Pts',(-1.99893804826277,-1.8787619573583,
7.51860402984324));
#400541=CARTESIAN_POINT('',(-1.99893804826277,-1.8787619573583,7.5));
#400542=CARTESIAN_POINT('Origin',(-1.97731117195258,-1.79574168958062,7.5));
#400543=CARTESIAN_POINT('Ctrl Pts',(-1.97081848695445,-1.79800236791134,
8.85049129520029));
#400544=CARTESIAN_POINT('Ctrl Pts',(-1.97075480602791,-1.79781947581619,
8.85097269580138));
#400545=CARTESIAN_POINT('Ctrl Pts',(-1.97069987221253,-1.79763612535269,
8.85143669361005));
#400546=CARTESIAN_POINT('Ctrl Pts',(-1.97065199348698,-1.79744362289938,
8.8519052845931));
#400547=CARTESIAN_POINT('Ctrl Pts',(-1.97055834573615,-1.79706710030876,
8.85282181883899));
#400548=CARTESIAN_POINT('Ctrl Pts',(-1.97049428862327,-1.79666520341029,
8.85372622499636));
#400549=CARTESIAN_POINT('Ctrl Pts',(-1.97047404352487,-1.79622919884002,
8.85462257735071));
#400550=CARTESIAN_POINT('Ctrl Pts',(-1.97045723676321,-1.7958672433312,
8.85536669723986));
#400551=CARTESIAN_POINT('Ctrl Pts',(-1.97047058865886,-1.79548170066648,
8.85610498449051));
#400552=CARTESIAN_POINT('Ctrl Pts',(-1.97053023464031,-1.79506781843295,
8.8568133821837));
#400553=CARTESIAN_POINT('Ctrl Pts',(-1.97058436346215,-1.79469221965601,
8.85745625420284));
#400554=CARTESIAN_POINT('Ctrl Pts',(-1.97067670481895,-1.79428848470054,
8.85808743050666));
#400555=CARTESIAN_POINT('Ctrl Pts',(-1.97083515791362,-1.79385033020558,
8.8586680450841));
#400556=CARTESIAN_POINT('Ctrl Pts',(-1.97090826473665,-1.79364817521963,
8.85893592806395));
#400557=CARTESIAN_POINT('Ctrl Pts',(-1.97099568587152,-1.79343866869043,
8.85919241173848));
#400558=CARTESIAN_POINT('Ctrl Pts',(-1.97110175636777,-1.79322125445075,
8.85943017985534));
#400559=CARTESIAN_POINT('Ctrl Pts',(-1.97124498293793,-1.79292768086568,
8.8597512372));
#400560=CARTESIAN_POINT('Ctrl Pts',(-1.97142643405862,-1.79261249780912,
8.86004599534706));
#400561=CARTESIAN_POINT('Ctrl Pts',(-1.97165295583813,-1.79228468846282,
8.86026130871721));
#400562=CARTESIAN_POINT('Ctrl Pts',(-1.97173589184793,-1.79216466821922,
8.86034014101236));
#400563=CARTESIAN_POINT('Ctrl Pts',(-1.97182610522264,-1.79204114558174,
8.86040910639693));
#400564=CARTESIAN_POINT('Ctrl Pts',(-1.97192140979439,-1.79191768424807,
8.86046313645507));
#400565=CARTESIAN_POINT('Ctrl Pts',(-1.97207013178043,-1.79172502387087,
8.8605474499083));
#400566=CARTESIAN_POINT('Ctrl Pts',(-1.97223542757183,-1.79152734357841,
8.86059655985668));
#400567=CARTESIAN_POINT('Ctrl Pts',(-1.9724064715048,-1.79133713328595,
8.86059725258816));
#400568=CARTESIAN_POINT('Ctrl Pts',(-1.97257791061759,-1.79114648353172,
8.86059794692011));
#400569=CARTESIAN_POINT('Ctrl Pts',(-1.97275900125441,-1.7909630004596,
8.86056369958366));
#400570=CARTESIAN_POINT('Ctrl Pts',(-1.97293718832747,-1.79079404793146,
8.86048590497774));
#400571=CARTESIAN_POINT('Ctrl Pts',(-1.97298368984828,-1.79074995635193,
8.86046560290182));
#400572=CARTESIAN_POINT('Ctrl Pts',(-1.97303066090191,-1.79070634650503,
8.86044257503091));
#400573=CARTESIAN_POINT('Ctrl Pts',(-1.97307662770901,-1.79066454191473,
8.86041778462583));
#400574=CARTESIAN_POINT('Ctrl Pts',(-1.97338592728076,-1.79038324889724,
8.860250975962));
#400575=CARTESIAN_POINT('Ctrl Pts',(-1.97369148558685,-1.790146190774,8.8599848982295));
#400576=CARTESIAN_POINT('Ctrl Pts',(-1.97397919074953,-1.78995359252349,
8.85968173251461));
#400577=CARTESIAN_POINT('Ctrl Pts',(-1.97413137029704,-1.78985171908353,
8.85952137522076));
#400578=CARTESIAN_POINT('Ctrl Pts',(-1.97428138202754,-1.78976016227389,
8.85934740853961));
#400579=CARTESIAN_POINT('Ctrl Pts',(-1.97442630057652,-1.78967888631636,
8.8591675900182));
#400580=CARTESIAN_POINT('Ctrl Pts',(-1.97500822387785,-1.78935252110047,
8.85844552518694));
#400581=CARTESIAN_POINT('Ctrl Pts',(-1.97553943149829,-1.78917084386516,
8.85759444184123));
#400582=CARTESIAN_POINT('Ctrl Pts',(-1.97598585478622,-1.78906161702088,
8.85683498915137));
#400583=CARTESIAN_POINT('Ctrl Pts',(-1.97603257179437,-1.78905018672252,
8.85675551444997));
#400584=CARTESIAN_POINT('Ctrl Pts',(-1.97607836118027,-1.78903956978337,
8.85667699793651));
#400585=CARTESIAN_POINT('Ctrl Pts',(-1.97612318378679,-1.78902969655278,
8.85659965593547));
#400586=CARTESIAN_POINT('Ctrl Pts',(-1.9767282016167,-1.78889642718248,
8.85555568965886));
#400587=CARTESIAN_POINT('Ctrl Pts',(-1.97732890796932,-1.78885572360712,
8.85434650606346));
#400588=CARTESIAN_POINT('Ctrl Pts',(-1.97792785225356,-1.78890118409167,
8.85297329937117));
#400589=CARTESIAN_POINT('Ctrl Pts',(-1.97826472191923,-1.78892675284428,
8.85220095427747));
#400590=CARTESIAN_POINT('Ctrl Pts',(-1.97860114795411,-1.78897990317963,
8.85137579139183));
#400591=CARTESIAN_POINT('Ctrl Pts',(-1.97893795668429,-1.7890619293726,
8.85049129520029));
#400592=CARTESIAN_POINT('Origin',(-1.97731117195258,-1.79574168958062,7.59394543036555));
#400593=CARTESIAN_POINT('Ctrl Pts',(-1.97063359974216,-1.79747137046104,
7.59443877723642));
#400594=CARTESIAN_POINT('Ctrl Pts',(-1.96872943934933,-1.79200260763504,
7.58783886950016));
#400595=CARTESIAN_POINT('Ctrl Pts',(-1.97588371901012,-1.78743145197463,
7.58559994247159));
#400596=CARTESIAN_POINT('Ctrl Pts',(-1.98102835546094,-1.82732518628148,
7.56670252222134));
#400597=CARTESIAN_POINT('Ctrl Pts',(-1.97912694712048,-1.82186432737039,
7.56004874999026));
#400598=CARTESIAN_POINT('Ctrl Pts',(-1.98631211473056,-1.81724808174524,
7.55786368756704));
#400599=CARTESIAN_POINT('Ctrl Pts',(-1.99140370001201,-1.8571232530837,
7.5388891333356));
#400600=CARTESIAN_POINT('Ctrl Pts',(-1.98949099150868,-1.85162994002071,
7.53222002137281));
#400601=CARTESIAN_POINT('Ctrl Pts',(-1.99672030494783,-1.84701047339366,
7.53005029815326));
#400602=CARTESIAN_POINT('Ctrl Pts',(-2.00175916390394,-1.88686422248488,
7.51101258149734));
#400603=CARTESIAN_POINT('Ctrl Pts',(-1.99982326989808,-1.88130432048597,
7.5043616886572));
#400604=CARTESIAN_POINT('Ctrl Pts',(-2.00710785342835,-1.87671712915194,
7.50217374673251));
#400605=CARTESIAN_POINT('',(-2.00655355952791,-1.87513194417975,7.50366116523517));
#400606=CARTESIAN_POINT('Ctrl Pts',(-1.99893804826277,-1.8787619573583,
7.51860402984325));
#400607=CARTESIAN_POINT('Ctrl Pts',(-1.99908326148543,-1.879179010815,7.51734760759493));
#400608=CARTESIAN_POINT('Ctrl Pts',(-1.99927067061862,-1.879536314155,7.51608817408573));
#400609=CARTESIAN_POINT('Ctrl Pts',(-1.99951167028735,-1.87982684288426,
7.5148100591312));
#400610=CARTESIAN_POINT('Ctrl Pts',(-1.99972997354617,-1.88009001074963,
7.51365231206384));
#400611=CARTESIAN_POINT('Ctrl Pts',(-1.99999236391793,-1.88029891959378,
7.51247773061043));
#400612=CARTESIAN_POINT('Ctrl Pts',(-2.00031730057137,-1.88042106712353,
7.51129758471022));
#400613=CARTESIAN_POINT('Ctrl Pts',(-2.00072115972243,-1.88057288255323,
7.50983079813402));
#400614=CARTESIAN_POINT('Ctrl Pts',(-2.00121333215552,-1.88057363532481,
7.50839324291155));
#400615=CARTESIAN_POINT('Ctrl Pts',(-2.00179753601526,-1.88034089142908,
7.50715379678855));
#400616=CARTESIAN_POINT('Ctrl Pts',(-2.00206742136502,-1.8802333704556,
7.50658120839351));
#400617=CARTESIAN_POINT('Ctrl Pts',(-2.00239179783196,-1.88005190515018,
7.50598221009429));
#400618=CARTESIAN_POINT('Ctrl Pts',(-2.00275184034603,-1.87978096284191,
7.50545747549611));
#400619=CARTESIAN_POINT('Ctrl Pts',(-2.00294397017589,-1.87963637963978,
7.50517746087247));
#400620=CARTESIAN_POINT('Ctrl Pts',(-2.0031484614756,-1.87946491079292,
7.50491486231392));
#400621=CARTESIAN_POINT('Ctrl Pts',(-2.00335882723001,-1.87926981894231,
7.50468370960992));
#400622=CARTESIAN_POINT('Ctrl Pts',(-2.00367339038896,-1.87897809508742,
7.50433806340446));
#400623=CARTESIAN_POINT('Ctrl Pts',(-2.00401014266398,-1.87862439508463,
7.50405484070983));
#400624=CARTESIAN_POINT('Ctrl Pts',(-2.00434588556985,-1.87823204598658,
7.5038576603613));
#400625=CARTESIAN_POINT('Ctrl Pts',(-2.004381788055,-1.87819009034904,7.50383657498791));
#400626=CARTESIAN_POINT('Ctrl Pts',(-2.00441767407893,-1.87814772069229,
7.50381643264937));
#400627=CARTESIAN_POINT('Ctrl Pts',(-2.00445351201731,-1.87810498588882,
7.50379723213559));
#400628=CARTESIAN_POINT('Ctrl Pts',(-2.00469274197945,-1.87781971709612,
7.50366906242519));
#400629=CARTESIAN_POINT('Ctrl Pts',(-2.0049344820996,-1.87751151007147,
7.50358235568538));
#400630=CARTESIAN_POINT('Ctrl Pts',(-2.00516034878498,-1.87720883540575,
7.5035341175365));
#400631=CARTESIAN_POINT('Ctrl Pts',(-2.00549901031654,-1.87675500900065,
7.50346178989176));
#400632=CARTESIAN_POINT('Ctrl Pts',(-2.00584403688456,-1.87625239556466,
7.50346967198527));
#400633=CARTESIAN_POINT('Ctrl Pts',(-2.0061675638165,-1.87574856280017,
7.50354272648692));
#400634=CARTESIAN_POINT('Ctrl Pts',(-2.00630063714021,-1.87554132595542,
7.50357277531559));
#400635=CARTESIAN_POINT('Ctrl Pts',(-2.0064300155592,-1.87533423478528,
7.50361331098761));
#400636=CARTESIAN_POINT('Ctrl Pts',(-2.00655355952895,-1.87513194418072,
7.50366116523659));
#400637=CARTESIAN_POINT('',(-1.97947865054248,-1.79771013628735,7.57603338622103));
#400638=CARTESIAN_POINT('Origin',(-1.98602235984329,-1.80364910574218,7.58486873427627));
#400639=CARTESIAN_POINT('Ctrl Pts',(-2.0065535595417,-1.87513194423542,
7.50366116529968));
#400640=CARTESIAN_POINT('Ctrl Pts',(-1.99754410575752,-1.8493665111649,
7.52783573079709));
#400641=CARTESIAN_POINT('Ctrl Pts',(-1.98851957912756,-1.82356045444553,
7.55196141284068));
#400642=CARTESIAN_POINT('Ctrl Pts',(-1.97947865060515,-1.79771013753784,
7.57603338728831));
#400643=CARTESIAN_POINT('Ctrl Pts',(-1.97132269366337,-1.79891577423654,
7.59639677331371));
#400644=CARTESIAN_POINT('Ctrl Pts',(-1.96265932869603,-1.78282173735349,
7.59959882295466));
#400645=CARTESIAN_POINT('Ctrl Pts',(-1.97972755753913,-1.78940841912533,
7.59642833564546));
#400646=CARTESIAN_POINT('Ctrl Pts',(-1.9689457891844,-1.79582297143299,
7.58707626057422));
#400647=CARTESIAN_POINT('Ctrl Pts',(-1.96986457548299,-1.78910969184893,
7.58809943920599));
#400648=CARTESIAN_POINT('Ctrl Pts',(-1.97641865331219,-1.78744882924111,
7.58710240504253));
#400649=CARTESIAN_POINT('Ctrl Pts',(-1.97498067889014,-1.79653412437102,
7.58015376756929));
#400650=CARTESIAN_POINT('Ctrl Pts',(-1.97499660145064,-1.79368298111467,
7.5820588065976));
#400651=CARTESIAN_POINT('Ctrl Pts',(-1.97779293880242,-1.79335499871752,
7.58020924244127));
#400652=CARTESIAN_POINT('Ctrl Pts',(-1.97947864992971,-1.79771013573113,
7.57603338509286));
#400653=CARTESIAN_POINT('Ctrl Pts',(-1.97947864992971,-1.79771013573113,
7.57603338509286));
#400654=CARTESIAN_POINT('Ctrl Pts',(-1.97947864992971,-1.79771013573113,
7.57603338509286));
#400655=CARTESIAN_POINT('Origin',(-1.98601852345799,-1.80365333002949,7.58486873427621));
#400656=CARTESIAN_POINT('Ctrl Pts',(-2.07038655374306,-1.81133326498924,
7.51098857897448));
#400657=CARTESIAN_POINT('Ctrl Pts',(-2.06466642693682,-1.80994018879159,
7.50433767179956));
#400658=CARTESIAN_POINT('Ctrl Pts',(-2.06079991957958,-1.81763162376426,
7.50214974420965));
#400659=CARTESIAN_POINT('Ctrl Pts',(-2.03977985028097,-1.80387932707387,
7.53887321589165));
#400660=CARTESIAN_POINT('Ctrl Pts',(-2.03412826074525,-1.80250294240135,
7.53220407452058));
#400661=CARTESIAN_POINT('Ctrl Pts',(-2.03022429857704,-1.81014244495788,
7.5300343807091));
#400662=CARTESIAN_POINT('Ctrl Pts',(-2.00911437065794,-1.79641107484808,
7.56669465659233));
#400663=CARTESIAN_POINT('Ctrl Pts',(-2.00349618096568,-1.79504282435305,
7.560040858333));
#400664=CARTESIAN_POINT('Ctrl Pts',(-1.99959118425106,-1.80263806304482,
7.5578558219379));
#400665=CARTESIAN_POINT('Ctrl Pts',(-1.97839150175079,-1.78892884607099,
7.59443891967696));
#400666=CARTESIAN_POINT('Ctrl Pts',(-1.97276516638296,-1.78755861178311,
7.58783901202978));
#400667=CARTESIAN_POINT('Ctrl Pts',(-1.96890210910569,-1.79511876829345,
7.58560008491213));
#400668=CARTESIAN_POINT('',(-2.05914251569203,-1.81722565891167,7.50366116523517));
#400669=CARTESIAN_POINT('Ctrl Pts',(-2.05914251569231,-1.81722565891192,
7.50366116523554));
#400670=CARTESIAN_POINT('Ctrl Pts',(-2.05974816076237,-1.81677032215097,
7.50350835821027));
#400671=CARTESIAN_POINT('Ctrl Pts',(-2.06029008167033,-1.81633205312325,
7.50345484955999));
#400672=CARTESIAN_POINT('Ctrl Pts',(-2.06078476777651,-1.81589828865175,
7.50349758195598));
#400673=CARTESIAN_POINT('Ctrl Pts',(-2.06103857843586,-1.81567573530907,
7.50351950684424));
#400674=CARTESIAN_POINT('Ctrl Pts',(-2.06130505670668,-1.81543252934383,
7.50357029184312));
#400675=CARTESIAN_POINT('Ctrl Pts',(-2.06155557213264,-1.81519094525445,
7.50365515313923));
#400676=CARTESIAN_POINT('Ctrl Pts',(-2.06194096630147,-1.81481929109791,
7.50378570417639));
#400677=CARTESIAN_POINT('Ctrl Pts',(-2.06230013518949,-1.81444081575043,
7.50400001621911));
#400678=CARTESIAN_POINT('Ctrl Pts',(-2.06260409394753,-1.81408276381045,
7.50428903009634));
#400679=CARTESIAN_POINT('Ctrl Pts',(-2.06263783103116,-1.8140430227998,
7.50432110841318));
#400680=CARTESIAN_POINT('Ctrl Pts',(-2.06267091723574,-1.81400352550134,
7.50435406373354));
#400681=CARTESIAN_POINT('Ctrl Pts',(-2.06270333445462,-1.81396430305073,
7.50438785222351));
#400682=CARTESIAN_POINT('Ctrl Pts',(-2.06290125715758,-1.81372483113704,
7.50459414719561));
#400683=CARTESIAN_POINT('Ctrl Pts',(-2.06307699573866,-1.81349146349241,
7.50483629897752));
#400684=CARTESIAN_POINT('Ctrl Pts',(-2.06322486898636,-1.81327393203516,
7.5050991045531));
#400685=CARTESIAN_POINT('Ctrl Pts',(-2.06355109222325,-1.8127940357915,
7.50567888004914));
#400686=CARTESIAN_POINT('Ctrl Pts',(-2.06375498358801,-1.81237259419739,
7.50637912803144));
#400687=CARTESIAN_POINT('Ctrl Pts',(-2.06386691707729,-1.81201533775757,
7.50710440483569));
#400688=CARTESIAN_POINT('Ctrl Pts',(-2.06389436539105,-1.81192773138599,
7.50728225710685));
#400689=CARTESIAN_POINT('Ctrl Pts',(-2.06391696970791,-1.81184228430579,
7.50746498566954));
#400690=CARTESIAN_POINT('Ctrl Pts',(-2.06393460510911,-1.81176109766968,
7.50764697238949));
#400691=CARTESIAN_POINT('Ctrl Pts',(-2.0640294081726,-1.81132466065711,
7.50862528291182));
#400692=CARTESIAN_POINT('Ctrl Pts',(-2.06399326812427,-1.81097260360617,
7.50965856837421));
#400693=CARTESIAN_POINT('Ctrl Pts',(-2.06388789127109,-1.8106806834246,
7.51067959873202));
#400694=CARTESIAN_POINT('Ctrl Pts',(-2.06382990225587,-1.81052003938047,
7.51124147302578));
#400695=CARTESIAN_POINT('Ctrl Pts',(-2.0637505234035,-1.81037771496521,
7.51180065547253));
#400696=CARTESIAN_POINT('Ctrl Pts',(-2.0636575186871,-1.81025068491237,
7.51235175716501));
#400697=CARTESIAN_POINT('Ctrl Pts',(-2.06333615034324,-1.80981174547706,
7.51425603304536));
#400698=CARTESIAN_POINT('Ctrl Pts',(-2.06280888182929,-1.80950666459949,
7.5162690050518));
#400699=CARTESIAN_POINT('Ctrl Pts',(-2.06213518302363,-1.80932514660288,
7.51827788969243));
#400700=CARTESIAN_POINT('Ctrl Pts',(-2.06209872117116,-1.80931532250589,
7.51838661432545));
#400701=CARTESIAN_POINT('Ctrl Pts',(-2.06206182146845,-1.80930586476256,
7.51849533314856));
#400702=CARTESIAN_POINT('Ctrl Pts',(-2.06202449055417,-1.80929677321444,
7.51860402984325));
#400703=CARTESIAN_POINT('Ctrl Pts',(-1.97947865179425,-1.79771013623028,
7.57603338728985));
#400704=CARTESIAN_POINT('Ctrl Pts',(-2.00607765462698,-1.80422706199452,
7.55196141284922));
#400705=CARTESIAN_POINT('Ctrl Pts',(-2.03263102684926,-1.81073191165887,
7.52783573083104));
#400706=CARTESIAN_POINT('Ctrl Pts',(-2.05914251575056,-1.81722565892042,
7.50366116530176));
#400707=CARTESIAN_POINT('Origin',(-6.84001376365782E-16,-6.21191952330714E-16,
7.49482233047033));
#400708=CARTESIAN_POINT('Origin',(-2.00009565450361,-1.86909700733691,7.49482233047033));
#400709=CARTESIAN_POINT('Origin',(0.,0.,7.50366116523517));
#400710=CARTESIAN_POINT('Origin',(-2.05251535802923,-1.81137708803389,7.49482233047033));
#400711=CARTESIAN_POINT('Ctrl Pts',(-1.99893770041465,-1.87876095847199,
7.51860402984325));
#400712=CARTESIAN_POINT('Ctrl Pts',(-2.00144033216759,-1.88594657746685,
7.51860402984325));
#400713=CARTESIAN_POINT('Ctrl Pts',(-1.99620683387468,-1.8914698719229,
7.51860402984325));
#400714=CARTESIAN_POINT('Ctrl Pts',(-1.99986694346334,-1.88142902825996,
7.51041458714366));
#400715=CARTESIAN_POINT('Ctrl Pts',(-2.00020044929248,-1.88725510237742,
7.51004642900442));
#400716=CARTESIAN_POINT('Ctrl Pts',(-1.99620539053799,-1.89147139518193,
7.5072913648301));
#400717=CARTESIAN_POINT('Ctrl Pts',(-2.00268144724221,-1.88147704573545,
7.50215815450137));
#400718=CARTESIAN_POINT('Ctrl Pts',(-2.0027250764607,-1.88459091165625,
7.49877163671529));
#400719=CARTESIAN_POINT('Ctrl Pts',(-2.00036937312889,-1.88711174195734,
7.49481588533171));
#400720=CARTESIAN_POINT('Ctrl Pts',(-2.00655315730405,-1.87513156829938,
7.50366171572174));
#400721=CARTESIAN_POINT('Ctrl Pts',(-2.00922851137376,-1.87763169686784,
7.50000045605858));
#400722=CARTESIAN_POINT('Ctrl Pts',(-2.00922851137367,-1.87763169686793,
7.49482233047317));
#400723=CARTESIAN_POINT('Origin',(-1.98713316644798,-1.88287228159597,7.51860402984325));
#400724=CARTESIAN_POINT('Origin',(-1.98713316644798,-1.88287228159597,9.));
#400725=CARTESIAN_POINT('Origin',(-1.98713316644798,-1.88287228159597,8.75721825406948));
#400726=CARTESIAN_POINT('Ctrl Pts',(-1.99344657357429,-1.86299049303862,
8.78942910404913));
#400727=CARTESIAN_POINT('Ctrl Pts',(-1.99529801914105,-1.86824640190532,
8.79672699501692));
#400728=CARTESIAN_POINT('Ctrl Pts',(-1.98756686989969,-1.87270765928303,
8.79893251111267));
#400729=CARTESIAN_POINT('Ctrl Pts',(-1.99706180063075,-1.8733734382889,
8.78111911759577));
#400730=CARTESIAN_POINT('Ctrl Pts',(-1.99924968983697,-1.87960685235721,
8.78644465894809));
#400731=CARTESIAN_POINT('Ctrl Pts',(-1.99326065865081,-1.88507009473026,
8.78817647674131));
#400732=CARTESIAN_POINT('Ctrl Pts',(-1.9993148963336,-1.87984433743598,
8.76780923932034));
#400733=CARTESIAN_POINT('Ctrl Pts',(-2.001892798948,-1.88720430719687,8.76988516158377));
#400734=CARTESIAN_POINT('Ctrl Pts',(-1.99680675333073,-1.892796133408,8.77093053738833));
#400735=CARTESIAN_POINT('Ctrl Pts',(-1.99887557350569,-1.87858260066336,
8.75371302330491));
#400736=CARTESIAN_POINT('Ctrl Pts',(-2.00139092575808,-1.88576168169189,
8.75300828287558));
#400737=CARTESIAN_POINT('Ctrl Pts',(-1.99611470500354,-1.89128943294206,
8.75267964240738));
#400738=CARTESIAN_POINT('Origin',(-1.98252217804004,-1.8696294885564,8.78727029226991));
#400739=CARTESIAN_POINT('Ctrl Pts',(-1.97081848695445,-1.79800236791134,
8.85049129520029));
#400740=CARTESIAN_POINT('Ctrl Pts',(-1.97273870409017,-1.80351724582248,
8.85711686593484));
#400741=CARTESIAN_POINT('Ctrl Pts',(-1.96551867526937,-1.80809675954565,
8.85933012996512));
#400742=CARTESIAN_POINT('Ctrl Pts',(-1.97866607911545,-1.82054071102847,
8.82945683644723));
#400743=CARTESIAN_POINT('Ctrl Pts',(-1.98060223521441,-1.82610136576062,
8.83607469902389));
#400744=CARTESIAN_POINT('Ctrl Pts',(-1.97334092145605,-1.83066265560015,
8.83829567148519));
#400745=CARTESIAN_POINT('Ctrl Pts',(-1.98650197380751,-1.84304545892768,
8.80838214965003));
#400746=CARTESIAN_POINT('Ctrl Pts',(-1.98844577088239,-1.84862805859967,
8.81501364461995));
#400747=CARTESIAN_POINT('Ctrl Pts',(-1.98115193336382,-1.85319410139924,
8.81722098428721));
#400748=CARTESIAN_POINT('Ctrl Pts',(-1.99432705985483,-1.86551916431873,
8.78727029226991));
#400749=CARTESIAN_POINT('Ctrl Pts',(-1.99627117980079,-1.87110269127883,
8.79393457792714));
#400750=CARTESIAN_POINT('Ctrl Pts',(-1.98895258219515,-1.87569371995058,
8.79610912703474));
#400751=CARTESIAN_POINT('Origin',(-1.95901360513965,-1.80211269214901,8.85049129520029));
#400752=CARTESIAN_POINT('Ctrl Pts',(-1.97893795668429,-1.7890619293726,
8.85049129520029));
#400753=CARTESIAN_POINT('Ctrl Pts',(-1.98461173602728,-1.79044371813728,
8.85711686593484));
#400754=CARTESIAN_POINT('Ctrl Pts',(-1.98847679932027,-1.78281731348928,
8.85933012996512));
#400755=CARTESIAN_POINT('Ctrl Pts',(-1.97391844600142,-1.78783948079881,
8.86332496987231));
#400756=CARTESIAN_POINT('Ctrl Pts',(-1.97722818329212,-1.78461496014556,
8.86648636486737));
#400757=CARTESIAN_POINT('Ctrl Pts',(-1.97443045953234,-1.77941410986347,
8.87206031107458));
#400758=CARTESIAN_POINT('Ctrl Pts',(-1.96910815477049,-1.79309028114442,
8.86341338519877));
#400759=CARTESIAN_POINT('Ctrl Pts',(-1.96618509120301,-1.79668599665246,
8.86654584966059));
#400760=CARTESIAN_POINT('Ctrl Pts',(-1.96074356779992,-1.7943378110037,
8.87215952290714));
#400761=CARTESIAN_POINT('Ctrl Pts',(-1.97081848695445,-1.79800236791134,
8.85049129520029));
#400762=CARTESIAN_POINT('Ctrl Pts',(-1.97273870409017,-1.80351724582248,
8.85711686593484));
#400763=CARTESIAN_POINT('Ctrl Pts',(-1.96551867526937,-1.80809675954565,
8.85933012996512));
#400764=CARTESIAN_POINT('Origin',(-1.98189574710558,-1.77691691081256,8.85049129520029));
#400765=CARTESIAN_POINT('Ctrl Pts',(-2.04840012990612,-1.80597870472226,
8.78727029226991));
#400766=CARTESIAN_POINT('Ctrl Pts',(-2.05414453629873,-1.80737769395559,
8.79393457792714));
#400767=CARTESIAN_POINT('Ctrl Pts',(-2.05801159645804,-1.79965207029775,
8.79610912703474));
#400768=CARTESIAN_POINT('Ctrl Pts',(-2.02527888452904,-1.80034777070873,
8.80838214965003));
#400769=CARTESIAN_POINT('Ctrl Pts',(-2.03102233691532,-1.80174652760395,
8.81501364461987));
#400770=CARTESIAN_POINT('Ctrl Pts',(-2.0348669041979,-1.79404794883867,
8.81722098428721));
#400771=CARTESIAN_POINT('Ctrl Pts',(-2.00212570220896,-1.79470905879156,
8.82945683644722));
#400772=CARTESIAN_POINT('Ctrl Pts',(-2.00784657735091,-1.79610231723843,
8.83607469902389));
#400773=CARTESIAN_POINT('Ctrl Pts',(-2.01168953666615,-1.78843656833836,
8.8382956714852));
#400774=CARTESIAN_POINT('Ctrl Pts',(-1.97893795668429,-1.7890619293726,
8.85049129520029));
#400775=CARTESIAN_POINT('Ctrl Pts',(-1.98461173602728,-1.79044371813728,
8.85711686593484));
#400776=CARTESIAN_POINT('Ctrl Pts',(-1.98847679932027,-1.78281731348928,
8.85933012996512));
#400777=CARTESIAN_POINT('Origin',(-2.05135792032741,-1.79383368616222,8.78727029226991));
#400778=CARTESIAN_POINT('Ctrl Pts',(-2.06184459209043,-1.80925294186592,
8.75374538247848));
#400779=CARTESIAN_POINT('Ctrl Pts',(-2.06922464863629,-1.81106378249048,
8.75304829418601));
#400780=CARTESIAN_POINT('Ctrl Pts',(-2.07421919160669,-1.80529098561844,
8.75272238421917));
#400781=CARTESIAN_POINT('Ctrl Pts',(-2.06312709009239,-1.80956528108705,
8.76769408445021));
#400782=CARTESIAN_POINT('Ctrl Pts',(-2.07069302605931,-1.81142102027037,
8.76974318093969));
#400783=CARTESIAN_POINT('Ctrl Pts',(-2.07576782353208,-1.80582952781393,
8.7707786988043));
#400784=CARTESIAN_POINT('Ctrl Pts',(-2.05655373592175,-1.80796440818184,
8.78108014887988));
#400785=CARTESIAN_POINT('Ctrl Pts',(-2.06296468902881,-1.80954077031012,
8.78639403366325));
#400786=CARTESIAN_POINT('Ctrl Pts',(-2.06783626201611,-1.80307626318597,
8.78812224174741));
#400787=CARTESIAN_POINT('Ctrl Pts',(-2.0457814595272,-1.80534093085235,
8.78944554828685));
#400788=CARTESIAN_POINT('Ctrl Pts',(-2.05118303652298,-1.806674866224,8.79673892988686));
#400789=CARTESIAN_POINT('Ctrl Pts',(-2.05487972817392,-1.79856080280581,
8.79894799272499));
#400790=CARTESIAN_POINT('Origin',(-2.06498228097546,-1.7971517546544,8.75721825406948));
#400791=CARTESIAN_POINT('Origin',(-2.06498228097546,-1.7971517546544,9.));
#400792=CARTESIAN_POINT('Origin',(-2.06498228097546,-1.7971517546544,7.51860402984325));
#400793=CARTESIAN_POINT('Ctrl Pts',(-2.05914192586944,-1.81722513838389,
7.50366195182966));
#400794=CARTESIAN_POINT('Ctrl Pts',(-2.06188757427604,-1.81964821628965,
7.50000065167735));
#400795=CARTESIAN_POINT('Ctrl Pts',(-2.06188757427611,-1.81964821628956,
7.49482233047108));
#400796=CARTESIAN_POINT('Ctrl Pts',(-2.06509107296448,-1.81275731470247,
7.50215800491337));
#400797=CARTESIAN_POINT('Ctrl Pts',(-2.06819568917779,-1.81250030236346,
7.49877273257265));
#400798=CARTESIAN_POINT('Ctrl Pts',(-2.07047994339333,-1.80991199422324,
7.49481816995649));
#400799=CARTESIAN_POINT('Ctrl Pts',(-2.06476295199598,-1.8099640454759,
7.51043025814041));
#400800=CARTESIAN_POINT('Ctrl Pts',(-2.07059755848594,-1.80974016136719,
7.51006209594514));
#400801=CARTESIAN_POINT('Ctrl Pts',(-2.07441308596515,-1.80535601718414,
7.50731281821698));
#400802=CARTESIAN_POINT('Ctrl Pts',(-2.06202302209009,-1.80929641549154,
7.51860402984325));
#400803=CARTESIAN_POINT('Ctrl Pts',(-2.06941598411249,-1.81109783990738,
7.51860402984325));
#400804=CARTESIAN_POINT('Ctrl Pts',(-2.07441142381097,-1.80535792705008,
7.51860402984325));
#400805=CARTESIAN_POINT('Origin',(0.,0.,7.5));
#400806=CARTESIAN_POINT('Origin',(-1.86024642503783,-1.91217709997535,7.5));
#400807=CARTESIAN_POINT('',(-1.86024642503783,-1.91217709997535,7.59394543036555));
#400808=CARTESIAN_POINT('',(-1.86024642503783,-1.91217709997535,8.85049129520029));
#400809=CARTESIAN_POINT('',(-1.86024642503783,-1.91217709997535,7.5));
#400810=CARTESIAN_POINT('',(-1.92848201925696,-1.9335095747144,8.78727029226991));
#400811=CARTESIAN_POINT('Ctrl Pts',(-1.86024642503783,-1.91217709997535,
8.85049129520029));
#400812=CARTESIAN_POINT('Ctrl Pts',(-1.88302468545903,-1.91929826116103,
8.82945686509571));
#400813=CARTESIAN_POINT('Ctrl Pts',(-1.9057690832418,-1.92640883587952,
8.80838212259896));
#400814=CARTESIAN_POINT('Ctrl Pts',(-1.92848201925696,-1.9335095747144,
8.78727029226991));
#400815=CARTESIAN_POINT('',(-1.94186579781665,-1.93769374166282,8.75721825406948));
#400816=CARTESIAN_POINT('Origin',(-1.90158930505031,-1.92510232442672,8.7593767971313));
#400817=CARTESIAN_POINT('',(-1.94186579781665,-1.93769374166282,7.51860402984325));
#400818=CARTESIAN_POINT('',(-1.94186579781665,-1.93769374166282,7.5));
#400819=CARTESIAN_POINT('Ctrl Pts',(-1.94186579781665,-1.93769374166282,
7.51860402984325));
#400820=CARTESIAN_POINT('Ctrl Pts',(-1.93135492132931,-1.93440772928589,
7.52834476460825));
#400821=CARTESIAN_POINT('Ctrl Pts',(-1.92083722133263,-1.93111958367715,
7.53807742314407));
#400822=CARTESIAN_POINT('Ctrl Pts',(-1.9103124687182,-1.92782923321049,
7.54780169004674));
#400823=CARTESIAN_POINT('Ctrl Pts',(-1.89364182939128,-1.92261749589956,
7.5632044032688));
#400824=CARTESIAN_POINT('Ctrl Pts',(-1.87695347475875,-1.91740022025758,
7.57858609112103));
#400825=CARTESIAN_POINT('Ctrl Pts',(-1.86024642503783,-1.91217709997535,
7.59394543036555));
#400826=CARTESIAN_POINT('Origin',(-1.92517265250698,-2.18554644274946,7.5));
#400827=CARTESIAN_POINT('',(-1.87445832375784,-2.00297423990033,8.75721825406948));
#400828=CARTESIAN_POINT('',(-1.87070527778332,-1.98946322855772,8.78727029226991));
#400829=CARTESIAN_POINT('Origin',(-1.86117864728312,-1.95516724241237,8.75658640620986));
#400830=CARTESIAN_POINT('',(-1.85157082176546,-1.92057895321254,8.85049129520029));
#400831=CARTESIAN_POINT('Ctrl Pts',(-1.87070527778332,-1.98946322855772,
8.78727029226991));
#400832=CARTESIAN_POINT('Ctrl Pts',(-1.86433617262359,-1.96653437219954,
8.80838212259896));
#400833=CARTESIAN_POINT('Ctrl Pts',(-1.85795824503304,-1.9435737549827,
8.82945686509571));
#400834=CARTESIAN_POINT('Ctrl Pts',(-1.85157082176546,-1.92057895321254,
8.85049129520029));
#400835=CARTESIAN_POINT('',(-1.85157082176546,-1.92057895321254,7.59394543036555));
#400836=CARTESIAN_POINT('',(-1.85157082176546,-1.92057895321254,7.5));
#400837=CARTESIAN_POINT('',(-1.87445832375784,-2.00297423990033,7.51860402984325));
#400838=CARTESIAN_POINT('Ctrl Pts',(-1.85157082176546,-1.92057895321254,
7.59394543036555));
#400839=CARTESIAN_POINT('Ctrl Pts',(-1.85625577119297,-1.93744482836686,
7.57858609112103));
#400840=CARTESIAN_POINT('Ctrl Pts',(-1.86093547819015,-1.9542918307079,
7.56320440326857));
#400841=CARTESIAN_POINT('Ctrl Pts',(-1.86561021750532,-1.97112094933311,
7.54780169004651));
#400842=CARTESIAN_POINT('Ctrl Pts',(-1.86856154251838,-1.98174575542338,
7.53807742314383));
#400843=CARTESIAN_POINT('Ctrl Pts',(-1.87151088985391,-1.99236344185045,
7.52834476460825));
#400844=CARTESIAN_POINT('Ctrl Pts',(-1.87445832375784,-2.00297423990033,
7.51860402984325));
#400845=CARTESIAN_POINT('',(-1.87445832375784,-2.00297423990033,7.5));
#400846=CARTESIAN_POINT('Origin',(-1.85819500900388,-1.918738907444,7.5));
#400847=CARTESIAN_POINT('Ctrl Pts',(-1.85157082176546,-1.92057895321254,
8.85049129520029));
#400848=CARTESIAN_POINT('Ctrl Pts',(-1.85151898961498,-1.92039235683784,
8.85097269580138));
#400849=CARTESIAN_POINT('Ctrl Pts',(-1.85147591597155,-1.9202058634659,
8.85143669361005));
#400850=CARTESIAN_POINT('Ctrl Pts',(-1.8514404692925,-1.92001068892905,
8.8519052845931));
#400851=CARTESIAN_POINT('Ctrl Pts',(-1.85137113783624,-1.91962893991248,
8.85282181883899));
#400852=CARTESIAN_POINT('Ctrl Pts',(-1.85133296195825,-1.91922376460098,
8.85372622499635));
#400853=CARTESIAN_POINT('Ctrl Pts',(-1.85134069336431,-1.91878735874095,
8.85462257735071));
#400854=CARTESIAN_POINT('Ctrl Pts',(-1.85134711170302,-1.91842507009562,
8.85536669723986));
#400855=CARTESIAN_POINT('Ctrl Pts',(-1.8513851379691,-1.91804117502855,
8.85610498449051));
#400856=CARTESIAN_POINT('Ctrl Pts',(-1.85147117892724,-1.91763196469161,
8.85681338218371));
#400857=CARTESIAN_POINT('Ctrl Pts',(-1.85154926123187,-1.91726060566816,
8.85745625420284));
#400858=CARTESIAN_POINT('Ctrl Pts',(-1.85166728025086,-1.91686361656051,
8.85808743050666));
#400859=CARTESIAN_POINT('Ctrl Pts',(-1.85185348044153,-1.91643651442558,
8.8586680450841));
#400860=CARTESIAN_POINT('Ctrl Pts',(-1.85193938917318,-1.91623945875896,
8.85893592806395));
#400861=CARTESIAN_POINT('Ctrl Pts',(-1.85204005382136,-1.91603598377474,
8.85919241173848));
#400862=CARTESIAN_POINT('Ctrl Pts',(-1.85215983616256,-1.91582581219596,
8.85943017985534));
#400863=CARTESIAN_POINT('Ctrl Pts',(-1.85232157778255,-1.91554201834716,
8.8597512372));
#400864=CARTESIAN_POINT('Ctrl Pts',(-1.85252284994022,-1.91523910848121,
8.86004599534706));
#400865=CARTESIAN_POINT('Ctrl Pts',(-1.85276990912336,-1.91492648595462,
8.86026130871721));
#400866=CARTESIAN_POINT('Ctrl Pts',(-1.85286036445565,-1.91481202603387,
8.86034014101235));
#400867=CARTESIAN_POINT('Ctrl Pts',(-1.85295830659987,-1.91469453717766,
8.86040910639692));
#400868=CARTESIAN_POINT('Ctrl Pts',(-1.85306132555295,-1.91457743569342,
8.86046313645506));
#400869=CARTESIAN_POINT('Ctrl Pts',(-1.85322208576647,-1.91439469980799,
8.86054744990829));
#400870=CARTESIAN_POINT('Ctrl Pts',(-1.85339970735976,-1.91420801620861,
8.86059655985668));
#400871=CARTESIAN_POINT('Ctrl Pts',(-1.85358258667991,-1.914029155546,8.86059725258816));
#400872=CARTESIAN_POINT('Ctrl Pts',(-1.85376588852435,-1.91384988164381,
8.86059794692011));
#400873=CARTESIAN_POINT('Ctrl Pts',(-1.85395836289182,-1.91367837807428,
8.86056369958366));
#400874=CARTESIAN_POINT('Ctrl Pts',(-1.85414700868609,-1.91352118916219,
8.86048590497774));
#400875=CARTESIAN_POINT('Ctrl Pts',(-1.85419623962173,-1.91348016753622,
8.86046560290182));
#400876=CARTESIAN_POINT('Ctrl Pts',(-1.85424590826078,-1.91343965673616,
8.86044257503091));
#400877=CARTESIAN_POINT('Ctrl Pts',(-1.85429445905344,-1.91340088314132,
8.86041778462583));
#400878=CARTESIAN_POINT('Ctrl Pts',(-1.85462114564156,-1.9131399849621,
8.860250975962));
#400879=CARTESIAN_POINT('Ctrl Pts',(-1.85494126451144,-1.91292299108809,
8.8599848982295));
#400880=CARTESIAN_POINT('Ctrl Pts',(-1.85524071836528,-1.9127492218844,
8.85968173251462));
#400881=CARTESIAN_POINT('Ctrl Pts',(-1.8553991122973,-1.91265730793144,
8.85952137522077));
#400882=CARTESIAN_POINT('Ctrl Pts',(-1.85555468187754,-1.91257555051965,
8.85934740853961));
#400883=CARTESIAN_POINT('Ctrl Pts',(-1.8557045100443,-1.9125037265156,8.8591675900182));
#400884=CARTESIAN_POINT('Ctrl Pts',(-1.85630614801297,-1.91221531580599,
8.85844552518695));
#400885=CARTESIAN_POINT('Ctrl Pts',(-1.85684790431081,-1.91206804643514,
8.85759444184124));
#400886=CARTESIAN_POINT('Ctrl Pts',(-1.85730040856215,-1.91198764644738,
8.85683498915138));
#400887=CARTESIAN_POINT('Ctrl Pts',(-1.85734776192694,-1.91197923280278,
8.85675551444998));
#400888=CARTESIAN_POINT('Ctrl Pts',(-1.85739413746327,-1.91197157141331,
8.85667699793651));
#400889=CARTESIAN_POINT('Ctrl Pts',(-1.85743950055698,-1.91196459026259,
8.85659965593547));
#400890=CARTESIAN_POINT('Ctrl Pts',(-1.85805181391075,-1.91187035833396,
8.85555568965886));
#400891=CARTESIAN_POINT('Ctrl Pts',(-1.85865389393477,-1.91186822577661,
8.85434650606346));
#400892=CARTESIAN_POINT('Ctrl Pts',(-1.85924869496049,-1.91195196734977,
8.85297329937117));
#400893=CARTESIAN_POINT('Ctrl Pts',(-1.85958323429571,-1.91199906688222,
8.85220095427747));
#400894=CARTESIAN_POINT('Ctrl Pts',(-1.85991556375354,-1.91207366290457,
8.85137579139184));
#400895=CARTESIAN_POINT('Ctrl Pts',(-1.86024642503783,-1.91217709997535,
8.85049129520029));
#400896=CARTESIAN_POINT('Origin',(-1.85819500900388,-1.918738907444,7.59394543036555));
#400897=CARTESIAN_POINT('Ctrl Pts',(-1.85142033554723,-1.9200372009891,
7.59443877723642));
#400898=CARTESIAN_POINT('Ctrl Pts',(-1.84987047229342,-1.9144576743476,
7.58783886950016));
#400899=CARTESIAN_POINT('Ctrl Pts',(-1.85730292766809,-1.91035428688841,
7.58559994247159));
#400900=CARTESIAN_POINT('Ctrl Pts',(-1.85988099357869,-1.95049567322872,
7.56670252222139));
#400901=CARTESIAN_POINT('Ctrl Pts',(-1.85833337031734,-1.94492421058725,
7.5600487499903));
#400902=CARTESIAN_POINT('Ctrl Pts',(-1.86579953910258,-1.94077780480321,
7.55786368756704));
#400903=CARTESIAN_POINT('Ctrl Pts',(-1.86832585217658,-1.98089726731457,
7.53888913333561));
#400904=CARTESIAN_POINT('Ctrl Pts',(-1.86676903131439,-1.97529269319784,
7.53222002137278));
#400905=CARTESIAN_POINT('Ctrl Pts',(-1.87427946159672,-1.97114590146277,
7.53005029815327));
#400906=CARTESIAN_POINT('Ctrl Pts',(-1.87675452920536,-2.01124060755397,
7.51101258149734));
#400907=CARTESIAN_POINT('Ctrl Pts',(-1.87517883684549,-2.0055680958152,
7.5043616886572));
#400908=CARTESIAN_POINT('Ctrl Pts',(-1.88274235577551,-2.00145705422698,
7.50217374673251));
#400909=CARTESIAN_POINT('',(-1.88229076388121,-1.9998396124552,7.50366116523517));
#400910=CARTESIAN_POINT('Ctrl Pts',(-1.87445832375784,-2.00297423990033,
7.51860402984325));
#400911=CARTESIAN_POINT('Ctrl Pts',(-1.87457651791765,-2.0033997403191,
7.51734760759493));
#400912=CARTESIAN_POINT('Ctrl Pts',(-1.87474064949508,-2.00376831688545,
7.51608817408573));
#400913=CARTESIAN_POINT('Ctrl Pts',(-1.87496253976455,-2.00407368959407,
7.51481005913119));
#400914=CARTESIAN_POINT('Ctrl Pts',(-1.87516353327288,-2.00435030349066,
7.51365231206383));
#400915=CARTESIAN_POINT('Ctrl Pts',(-1.87541199969988,-2.00457559451801,
7.51247773061042));
#400916=CARTESIAN_POINT('Ctrl Pts',(-1.87572844271701,-2.00471830984543,
7.51129758471022));
#400917=CARTESIAN_POINT('Ctrl Pts',(-1.87612174524816,-2.0048956886987,
7.50983079813402));
#400918=CARTESIAN_POINT('Ctrl Pts',(-1.87661285822996,-2.00492797351969,
7.50839324291155));
#400919=CARTESIAN_POINT('Ctrl Pts',(-1.87721077373281,-2.00473313789105,
7.50715379678855));
#400920=CARTESIAN_POINT('Ctrl Pts',(-1.8774869934666,-2.00464312944468,
7.50658120839351));
#400921=CARTESIAN_POINT('Ctrl Pts',(-1.87782232998934,-2.00448281985078,
7.50598221009429));
#400922=CARTESIAN_POINT('Ctrl Pts',(-1.87819899209074,-2.00423550222563,
7.50545747549612));
#400923=CARTESIAN_POINT('Ctrl Pts',(-1.87839999064682,-2.00410352588565,
7.50517746087247));
#400924=CARTESIAN_POINT('Ctrl Pts',(-1.87861504784397,-2.00394551114248,
7.50491486231392));
#400925=CARTESIAN_POINT('Ctrl Pts',(-1.87883748095715,-2.00376429830917,
7.50468370960993));
#400926=CARTESIAN_POINT('Ctrl Pts',(-1.87917008862392,-2.00349332796302,
7.50433806340447));
#400927=CARTESIAN_POINT('Ctrl Pts',(-1.87952881064225,-2.00316193046716,
7.50405484070984));
#400928=CARTESIAN_POINT('Ctrl Pts',(-1.87988900162133,-2.00279189861426,
7.50385766036131));
#400929=CARTESIAN_POINT('Ctrl Pts',(-1.8799275184479,-2.00275232945919,
7.50383657498791));
#400930=CARTESIAN_POINT('Ctrl Pts',(-1.87996604537338,-2.00271234608088,
7.50381643264937));
#400931=CARTESIAN_POINT('Ctrl Pts',(-1.88000454770714,-2.00267199522525,
7.50379723213559));
#400932=CARTESIAN_POINT('Ctrl Pts',(-1.88026156337996,-2.00240264006418,
7.50366906242519));
#400933=CARTESIAN_POINT('Ctrl Pts',(-1.88052255371097,-2.00211055462659,
7.50358235568538));
#400934=CARTESIAN_POINT('Ctrl Pts',(-1.88076734876144,-2.00182297316665,
7.5035341175365));
#400935=CARTESIAN_POINT('Ctrl Pts',(-1.88113439123417,-2.0013917773154,
7.50346178989176));
#400936=CARTESIAN_POINT('Ctrl Pts',(-1.88151091146151,-2.00091230248073,
7.50346967198527));
#400937=CARTESIAN_POINT('Ctrl Pts',(-1.88186605434872,-2.0004302333364,
7.50354272648692));
#400938=CARTESIAN_POINT('Ctrl Pts',(-1.88201213196926,-2.00023194831909,
7.50357277531559));
#400939=CARTESIAN_POINT('Ctrl Pts',(-1.88215451294323,-2.00003357194373,
7.50361331098761));
#400940=CARTESIAN_POINT('Ctrl Pts',(-1.88229076388218,-1.99983961245623,
7.50366116523659));
#400941=CARTESIAN_POINT('',(-1.86023191546303,-1.92084218059593,7.57603338622103));
#400942=CARTESIAN_POINT('Origin',(-1.866381668932,-1.92718820469555,7.58486873427629));
#400943=CARTESIAN_POINT('Ctrl Pts',(-1.8822907638914,-1.99983961251163,
7.50366116529968));
#400944=CARTESIAN_POINT('Ctrl Pts',(-1.87495061796101,-1.97354987960083,
7.52783573079709));
#400945=CARTESIAN_POINT('Ctrl Pts',(-1.86759803291972,-1.94721864078629,
7.55196141284068));
#400946=CARTESIAN_POINT('Ctrl Pts',(-1.86023191544545,-1.92084218184786,
7.57603338728831));
#400947=CARTESIAN_POINT('Ctrl Pts',(-1.85201547038342,-1.92152278748123,
7.59639677331371));
#400948=CARTESIAN_POINT('Ctrl Pts',(-1.8444010537121,-1.90490675382385,
7.59959882295465));
#400949=CARTESIAN_POINT('Ctrl Pts',(-1.86101220389835,-1.9125734677282,
7.59642833564546));
#400950=CARTESIAN_POINT('Ctrl Pts',(-1.84984160606563,-1.9182840503799,
7.58707626057422));
#400951=CARTESIAN_POINT('Ctrl Pts',(-1.85118862591897,-1.91164343078902,
7.58809943920599));
#400952=CARTESIAN_POINT('Ctrl Pts',(-1.85783564952498,-1.91040590180985,
7.58710240504253));
#400953=CARTESIAN_POINT('Ctrl Pts',(-1.85581853271803,-1.91938039888897,
7.5801537675693));
#400954=CARTESIAN_POINT('Ctrl Pts',(-1.85601709593955,-1.91653613377419,
7.5820588065976));
#400955=CARTESIAN_POINT('Ctrl Pts',(-1.85882870182067,-1.91638798720131,
7.58020924244128));
#400956=CARTESIAN_POINT('Ctrl Pts',(-1.86023191488716,-1.92084218000158,
7.57603338509286));
#400957=CARTESIAN_POINT('Ctrl Pts',(-1.86023191488716,-1.92084218000158,
7.57603338509286));
#400958=CARTESIAN_POINT('Ctrl Pts',(-1.86023191488716,-1.92084218000158,
7.57603338509286));
#400959=CARTESIAN_POINT('Origin',(-1.86637756977769,-1.92719217450528,7.58486873427621));
#400960=CARTESIAN_POINT('Ctrl Pts',(-1.95008020177389,-1.94026180847486,
7.51098857897448));
#400961=CARTESIAN_POINT('Ctrl Pts',(-1.94446108228009,-1.93850510471887,
7.50433767179956));
#400962=CARTESIAN_POINT('Ctrl Pts',(-1.94010972714623,-1.94593300883656,
7.50214974420965));
#400963=CARTESIAN_POINT('Ctrl Pts',(-1.92001395850861,-1.93086220725069,
7.53887321589168));
#400964=CARTESIAN_POINT('Ctrl Pts',(-1.91446216603847,-1.92912655192329,
7.53220407452062));
#400965=CARTESIAN_POINT('Ctrl Pts',(-1.91007676036987,-1.93650023058753,
7.53003438070911));
#400966=CARTESIAN_POINT('Ctrl Pts',(-1.88988997696527,-1.92144455532479,
7.56669465659231));
#400967=CARTESIAN_POINT('Ctrl Pts',(-1.88437099455649,-1.91971915739764,
7.56004085833299));
#400968=CARTESIAN_POINT('Ctrl Pts',(-1.87998739246263,-1.92704859685846,
7.55785582193789));
#400969=CARTESIAN_POINT('Ctrl Pts',(-1.85970961953101,-1.91200927861987,
7.59443891967696));
#400970=CARTESIAN_POINT('Ctrl Pts',(-1.85418263528486,-1.91028137908059,
7.58783901202978));
#400971=CARTESIAN_POINT('Ctrl Pts',(-1.84984313418238,-1.917578495509,7.58560008491213));
#400972=CARTESIAN_POINT('',(-1.93848173883013,-1.94542168785063,7.50366116523517));
#400973=CARTESIAN_POINT('Ctrl Pts',(-1.93848173883039,-1.94542168785089,
7.50366116523554));
#400974=CARTESIAN_POINT('Ctrl Pts',(-1.93911531306414,-1.94500609044102,
7.50350835821027));
#400975=CARTESIAN_POINT('Ctrl Pts',(-1.93968420053049,-1.9446034428758,
7.50345484956));
#400976=CARTESIAN_POINT('Ctrl Pts',(-1.94020566163612,-1.94420226426758,
7.50349758195598));
#400977=CARTESIAN_POINT('Ctrl Pts',(-1.94047320985588,-1.94399642988938,
7.50351950684424));
#400978=CARTESIAN_POINT('Ctrl Pts',(-1.9407547228782,-1.94377079693832,
7.50357029184312));
#400979=CARTESIAN_POINT('Ctrl Pts',(-1.9410202019391,-1.94354575978781,
7.50365515313923));
#400980=CARTESIAN_POINT('Ctrl Pts',(-1.94142861623784,-1.94319956152377,
7.50378570417639));
#400981=CARTESIAN_POINT('Ctrl Pts',(-1.94181129617362,-1.94284487582416,
7.50400001621911));
#400982=CARTESIAN_POINT('Ctrl Pts',(-1.94213757088236,-1.94250703424478,
7.50428903009634));
#400983=CARTESIAN_POINT('Ctrl Pts',(-1.94217378486482,-1.94246953642866,
7.50432110841318));
#400984=CARTESIAN_POINT('Ctrl Pts',(-1.94220933369086,-1.94243224012205,
7.50435406373354));
#400985=CARTESIAN_POINT('Ctrl Pts',(-1.94224419729613,-1.94239517523651,
7.50438785222352));
#400986=CARTESIAN_POINT('Ctrl Pts',(-1.94245705636385,-1.94216887629467,
7.50459414719561));
#400987=CARTESIAN_POINT('Ctrl Pts',(-1.9426473857875,-1.94194724773844,
7.50483629897752));
#400988=CARTESIAN_POINT('Ctrl Pts',(-1.94280889250207,-1.94173963749441,
7.5050991045531));
#400989=CARTESIAN_POINT('Ctrl Pts',(-1.94316519253623,-1.9412816284436,
7.50567888004914));
#400990=CARTESIAN_POINT('Ctrl Pts',(-1.94339566683996,-1.94087411611104,
7.50637912803145));
#400991=CARTESIAN_POINT('Ctrl Pts',(-1.94353025984857,-1.94052476529617,
7.50710440483569));
#400992=CARTESIAN_POINT('Ctrl Pts',(-1.94356326472632,-1.94043909754077,
7.50728225710685));
#400993=CARTESIAN_POINT('Ctrl Pts',(-1.94359129721341,-1.94035527428432,
7.50746498566954));
#400994=CARTESIAN_POINT('Ctrl Pts',(-1.94361409802643,-1.9402753843589,
7.50764697238949));
#400995=CARTESIAN_POINT('Ctrl Pts',(-1.94373666892226,-1.93984591810612,
7.50862528291181));
#400996=CARTESIAN_POINT('Ctrl Pts',(-1.94372315950023,-1.93949226889329,
7.50965856837421));
#400997=CARTESIAN_POINT('Ctrl Pts',(-1.94363670254535,-1.93919419697488,
7.51067959873201));
#400998=CARTESIAN_POINT('Ctrl Pts',(-1.94358912517403,-1.93903016762221,
7.51124147302578));
#400999=CARTESIAN_POINT('Ctrl Pts',(-1.94351902817062,-1.93888304980718,
7.51180065547252));
#401000=CARTESIAN_POINT('Ctrl Pts',(-1.94343435338581,-1.93875032191858,
7.512351757165));
#401001=CARTESIAN_POINT('Ctrl Pts',(-1.94314176827386,-1.93829169419093,
7.51425603304535));
#401002=CARTESIAN_POINT('Ctrl Pts',(-1.94263512968855,-1.93795345792506,
7.5162690050518));
#401003=CARTESIAN_POINT('Ctrl Pts',(-1.94197444496732,-1.93772914884597,
7.51827788969243));
#401004=CARTESIAN_POINT('Ctrl Pts',(-1.94193868746169,-1.93771700881472,
7.51838661432545));
#401005=CARTESIAN_POINT('Ctrl Pts',(-1.94190246953308,-1.93770520633127,
7.51849533314856));
#401006=CARTESIAN_POINT('Ctrl Pts',(-1.94186579781665,-1.93769374166282,
7.51860402984325));
#401007=CARTESIAN_POINT('Ctrl Pts',(-1.86023191671588,-1.92084218061917,
7.57603338728984));
#401008=CARTESIAN_POINT('Ctrl Pts',(-1.88635872817725,-1.92904992062326,
7.55196141284921));
#401009=CARTESIAN_POINT('Ctrl Pts',(-1.91244077649953,-1.93724268577581,
7.52783573083105));
#401010=CARTESIAN_POINT('Ctrl Pts',(-1.93848173888798,-1.9454216878631,
7.50366116530176));
#401011=CARTESIAN_POINT('Origin',(-6.42796117143043E-16,-6.63739765492889E-16,
7.49482233047033));
#401012=CARTESIAN_POINT('Origin',(-1.87623278704648,-1.99340331564182,7.49482233047033));
#401013=CARTESIAN_POINT('Origin',(0.,0.,7.50366116523517));
#401014=CARTESIAN_POINT('Origin',(-1.93224291659623,-1.93916053003967,7.49482233047033));
#401015=CARTESIAN_POINT('Ctrl Pts',(-1.87445804062327,-2.00297322077964,
7.51860402984325));
#401016=CARTESIAN_POINT('Ctrl Pts',(-1.87649514626118,-2.01030442031656,
7.51860402984325));
#401017=CARTESIAN_POINT('Ctrl Pts',(-1.87091852206099,-2.01548105518488,
7.51860402984325));
#401018=CARTESIAN_POINT('Ctrl Pts',(-1.87521443062422,-2.00569534553861,
7.51041458714366));
#401019=CARTESIAN_POINT('Ctrl Pts',(-1.87517397337955,-2.01153081715378,
7.51004642900442));
#401020=CARTESIAN_POINT('Ctrl Pts',(-1.87091698409425,-2.0154824828393,
7.5072913648301));
#401021=CARTESIAN_POINT('Ctrl Pts',(-1.87802007521301,-2.0059235902333,
7.50215815450138));
#401022=CARTESIAN_POINT('Ctrl Pts',(-1.87786410871604,-2.00903385371624,
7.4987716367153));
#401023=CARTESIAN_POINT('Ctrl Pts',(-1.87535173527746,-2.01139857427044,
7.4948158853317));
#401024=CARTESIAN_POINT('Ctrl Pts',(-1.8822903865665,-1.99983921157654,
7.50366171572174));
#401025=CARTESIAN_POINT('Ctrl Pts',(-1.88480006004697,-2.0025056138865,
7.50000045605858));
#401026=CARTESIAN_POINT('Ctrl Pts',(-1.88480006004688,-2.00250561388658,
7.49482233047317));
#401027=CARTESIAN_POINT('Origin',(-1.86241434696071,-2.00631977766131,7.51860402984325));
#401028=CARTESIAN_POINT('Origin',(-1.86241434696071,-2.00631977766131,9.));
#401029=CARTESIAN_POINT('Origin',(-1.86241434696071,-2.00631977766131,8.75721825406948));
#401030=CARTESIAN_POINT('Ctrl Pts',(-1.86998861308145,-1.98688333975427,
8.78942910404913));
#401031=CARTESIAN_POINT('Ctrl Pts',(-1.87149950741743,-1.99224707231726,
8.7967269950169));
#401032=CARTESIAN_POINT('Ctrl Pts',(-1.86349840890978,-1.99620382713061,
8.79893251111267));
#401033=CARTESIAN_POINT('Ctrl Pts',(-1.87293117467996,-1.99747658052279,
8.78111911759583));
#401034=CARTESIAN_POINT('Ctrl Pts',(-1.87471519242254,-2.00383736591608,
8.78644465894814));
#401035=CARTESIAN_POINT('Ctrl Pts',(-1.86838843520263,-2.00890566492617,
8.78817647674132));
#401036=CARTESIAN_POINT('Ctrl Pts',(-1.87476504922421,-2.00407854085086,
8.76780923932029));
#401037=CARTESIAN_POINT('Ctrl Pts',(-1.87686610037958,-2.01158855555212,
8.76988516158373));
#401038=CARTESIAN_POINT('Ctrl Pts',(-1.87143223505307,-2.01684302869503,
8.77093053738833));
#401039=CARTESIAN_POINT('Ctrl Pts',(-1.87440746878475,-2.00279124894153,
8.75371302330492));
#401040=CARTESIAN_POINT('Ctrl Pts',(-1.8764576876754,-2.01011673895027,
8.75300828287559));
#401041=CARTESIAN_POINT('Ctrl Pts',(-1.87083814324369,-2.01529508421824,
8.75267964240738));
#401042=CARTESIAN_POINT('Origin',(-1.85866130098619,-1.9928087663187,8.78727029226991));
#401043=CARTESIAN_POINT('Ctrl Pts',(-1.85157082176546,-1.92057895321254,
8.85049129520029));
#401044=CARTESIAN_POINT('Ctrl Pts',(-1.8531337541682,-1.92620552894984,
8.85711686593484));
#401045=CARTESIAN_POINT('Ctrl Pts',(-1.84563514921931,-1.9303130447361,
8.85933012996512));
#401046=CARTESIAN_POINT('Ctrl Pts',(-1.8579582536052,-1.94357378584259,
8.82945683644724));
#401047=CARTESIAN_POINT('Ctrl Pts',(-1.85953415929186,-1.94924706556039,
8.8360746990239));
#401048=CARTESIAN_POINT('Ctrl Pts',(-1.85199552183797,-1.9533337497709,
8.8382956714852));
#401049=CARTESIAN_POINT('Ctrl Pts',(-1.86433616446271,-1.96653434282028,
8.80838214965003));
#401050=CARTESIAN_POINT('Ctrl Pts',(-1.86591828940898,-1.97223001194863,
8.81501364461986));
#401051=CARTESIAN_POINT('Ctrl Pts',(-1.85834689049523,-1.97631935554932,
8.81722098428721));
#401052=CARTESIAN_POINT('Ctrl Pts',(-1.87070527778332,-1.98946322855772,
8.78727029226991));
#401053=CARTESIAN_POINT('Ctrl Pts',(-1.87228766552574,-1.99515984375545,
8.79393457792714));
#401054=CARTESIAN_POINT('Ctrl Pts',(-1.86468995654685,-1.99927253550787,
8.79610912703474));
#401055=CARTESIAN_POINT('Origin',(-1.83952684496832,-1.92392449097352,8.85049129520029));
#401056=CARTESIAN_POINT('Ctrl Pts',(-1.86024642503783,-1.91217709997535,
8.85049129520029));
#401057=CARTESIAN_POINT('Ctrl Pts',(-1.86582001548252,-1.91391956999746,
8.85711686593484));
#401058=CARTESIAN_POINT('Ctrl Pts',(-1.87016576301192,-1.90655647007116,
8.85933012996512));
#401059=CARTESIAN_POINT('Ctrl Pts',(-1.85531555002704,-1.91063556189962,
8.86332496987232));
#401060=CARTESIAN_POINT('Ctrl Pts',(-1.85882508285509,-1.90762972196618,
8.86648636486738));
#401061=CARTESIAN_POINT('Ctrl Pts',(-1.8563663269405,-1.90226030661205,
8.87206031107457));
#401062=CARTESIAN_POINT('Ctrl Pts',(-1.85017872212212,-1.91556737749544,
8.86341338519876));
#401063=CARTESIAN_POINT('Ctrl Pts',(-1.84703128601865,-1.91896842389454,
8.86654584966058));
#401064=CARTESIAN_POINT('Ctrl Pts',(-1.84175139158006,-1.91627642324357,
8.87215952290715));
#401065=CARTESIAN_POINT('Ctrl Pts',(-1.85157082176546,-1.92057895321254,
8.85049129520029));
#401066=CARTESIAN_POINT('Ctrl Pts',(-1.8531337541682,-1.92620552894984,
8.85711686593484));
#401067=CARTESIAN_POINT('Ctrl Pts',(-1.84563514921931,-1.9303130447361,
8.85933012996512));
#401068=CARTESIAN_POINT('Origin',(-1.86397627237229,-1.90024654094144,8.85049129520029));
#401069=CARTESIAN_POINT('Ctrl Pts',(-1.92848201925696,-1.9335095747144,
8.78727029226991));
#401070=CARTESIAN_POINT('Ctrl Pts',(-1.93412498960262,-1.93527373495554,
8.79393457792714));
#401071=CARTESIAN_POINT('Ctrl Pts',(-1.93847908687934,-1.92781174781517,
8.79610912703474));
#401072=CARTESIAN_POINT('Ctrl Pts',(-1.90576905413921,-1.92640882678118,
8.80838214965002));
#401073=CARTESIAN_POINT('Ctrl Pts',(-1.91141108732466,-1.92817269403819,
8.81501364461993));
#401074=CARTESIAN_POINT('Ctrl Pts',(-1.91574100516639,-1.92073625510017,
8.81722098428721));
#401075=CARTESIAN_POINT('Ctrl Pts',(-1.88302471602829,-1.91929827071789,
8.82945683644722));
#401076=CARTESIAN_POINT('Ctrl Pts',(-1.88864457064352,-1.92105520429472,
8.83607469902389));
#401077=CARTESIAN_POINT('Ctrl Pts',(-1.89297078040505,-1.91365142474659,
8.83829567148519));
#401078=CARTESIAN_POINT('Ctrl Pts',(-1.86024642503783,-1.91217709997535,
8.85049129520029));
#401079=CARTESIAN_POINT('Ctrl Pts',(-1.86582001548252,-1.91391956999746,
8.85711686593484));
#401080=CARTESIAN_POINT('Ctrl Pts',(-1.87016576301192,-1.90655647007116,
8.85933012996512));
#401081=CARTESIAN_POINT('Origin',(-1.93221186659142,-1.92157901568049,8.78727029226991));
#401082=CARTESIAN_POINT('Ctrl Pts',(-1.94168907725774,-1.93763847423637,
8.75374538247848));
#401083=CARTESIAN_POINT('Ctrl Pts',(-1.94893794972875,-1.93991843614102,
8.75304829418601));
#401084=CARTESIAN_POINT('Ctrl Pts',(-1.95429209524045,-1.93447750156609,
8.75272238421917));
#401085=CARTESIAN_POINT('Ctrl Pts',(-1.9429489285874,-1.93803234165217,
8.76769408445021));
#401086=CARTESIAN_POINT('Ctrl Pts',(-1.95038042190973,-1.94036901920208,
8.76974318093969));
#401087=CARTESIAN_POINT('Ctrl Pts',(-1.95580304081854,-1.93511415845701,
8.7707786988043));
#401088=CARTESIAN_POINT('Ctrl Pts',(-1.9364916483571,-1.93601360166431,
8.78108014887988));
#401089=CARTESIAN_POINT('Ctrl Pts',(-1.9427884316051,-1.9379974761634,8.78639403366325));
#401090=CARTESIAN_POINT('Ctrl Pts',(-1.94806417781673,-1.9318583738154,
8.78812224174741));
#401091=CARTESIAN_POINT('Ctrl Pts',(-1.92590959152934,-1.93270533243208,
8.78944554828685));
#401092=CARTESIAN_POINT('Ctrl Pts',(-1.93121460487315,-1.93438260731681,
8.79673892988686));
#401093=CARTESIAN_POINT('Ctrl Pts',(-1.93542357110277,-1.92652206295941,
8.79894799272499));
#401094=CARTESIAN_POINT('Origin',(-1.94559564515111,-1.92576318262891,8.75721825406948));
#401095=CARTESIAN_POINT('Origin',(-1.94559564515111,-1.92576318262891,9.));
#401096=CARTESIAN_POINT('Origin',(-1.94559564515111,-1.92576318262891,7.51860402984325));
#401097=CARTESIAN_POINT('Ctrl Pts',(-1.93848118356972,-1.94542113060226,
7.50366195182966));
#401098=CARTESIAN_POINT('Ctrl Pts',(-1.94106594361275,-1.94801514433199,
7.50000065167735));
#401099=CARTESIAN_POINT('Ctrl Pts',(-1.94106594361283,-1.9480151443319,
7.49482233047108));
#401100=CARTESIAN_POINT('Ctrl Pts',(-1.94470436195012,-1.94134364970685,
7.50215800491337));
#401101=CARTESIAN_POINT('Ctrl Pts',(-1.94781906623355,-1.941286078871,7.49877273257268));
#401102=CARTESIAN_POINT('Ctrl Pts',(-1.95026446067573,-1.93884944135752,
7.49481816995647));
#401103=CARTESIAN_POINT('Ctrl Pts',(-1.94455588051516,-1.93853509676885,
7.51043025814041));
#401104=CARTESIAN_POINT('Ctrl Pts',(-1.95039284348443,-1.93868549717535,
7.51006209594513));
#401105=CARTESIAN_POINT('Ctrl Pts',(-1.95448142463543,-1.93455482237167,
7.50731281821699));
#401106=CARTESIAN_POINT('Ctrl Pts',(-1.94186435528907,-1.93769329059009,
7.51860402984325));
#401107=CARTESIAN_POINT('Ctrl Pts',(-1.9491267100195,-1.93996468248934,
7.51860402984324));
#401108=CARTESIAN_POINT('Ctrl Pts',(-1.9544796435308,-1.934556621819,7.51860402984325));
#401109=CARTESIAN_POINT('Origin',(0.,0.,7.5));
#401110=CARTESIAN_POINT('Origin',(-1.73391074180929,-2.02743472471361,7.5));
#401111=CARTESIAN_POINT('',(-1.73391074180929,-2.02743472471361,7.59394543036555));
#401112=CARTESIAN_POINT('',(-1.73391074180929,-2.02743472471361,8.85049129520029));
#401113=CARTESIAN_POINT('',(-1.73391074180929,-2.02743472471361,7.5));
#401114=CARTESIAN_POINT('',(-1.80063936233258,-2.05309523912754,8.78727029226991));
#401115=CARTESIAN_POINT('Ctrl Pts',(-1.73391074180929,-2.02743472471361,
8.85049129520029));
#401116=CARTESIAN_POINT('Ctrl Pts',(-1.7561859474878,-2.03600066286585,
8.82945686509571));
#401117=CARTESIAN_POINT('Ctrl Pts',(-1.7784280383796,-2.04455386671525,
8.80838212259896));
#401118=CARTESIAN_POINT('Ctrl Pts',(-1.80063936233259,-2.05309523912754,
8.78727029226991));
#401119=CARTESIAN_POINT('',(-1.813727561987,-2.05812831089271,8.75721825406948));
#401120=CARTESIAN_POINT('Origin',(-1.77434055646776,-2.0429822403225,8.75937679713164));
#401121=CARTESIAN_POINT('',(-1.813727561987,-2.05812831089271,7.51860402984325));
#401122=CARTESIAN_POINT('',(-1.813727561987,-2.05812831089271,7.5));
#401123=CARTESIAN_POINT('Ctrl Pts',(-1.813727561987,-2.05812831089271,7.51860402984325));
#401124=CARTESIAN_POINT('Ctrl Pts',(-1.80344881675854,-2.0541756158119,
7.52834476460825));
#401125=CARTESIAN_POINT('Ctrl Pts',(-1.793163398717,-2.05022035469848,7.53807742314407));
#401126=CARTESIAN_POINT('Ctrl Pts',(-1.7828710838138,-2.04626244139449,
7.54780169004674));
#401127=CARTESIAN_POINT('Ctrl Pts',(-1.76656861325929,-2.03999332062794,
7.5632044032688));
#401128=CARTESIAN_POINT('Ctrl Pts',(-1.75024881863925,-2.03371753788588,
7.57858609112103));
#401129=CARTESIAN_POINT('Ctrl Pts',(-1.73391074180929,-2.02743472471361,
7.59394543036555));
#401130=CARTESIAN_POINT('Origin',(-1.78118873745326,-2.30440223853068,7.5));
#401131=CARTESIAN_POINT('',(-1.74227604793054,-2.11895587165399,8.75721825406948));
#401132=CARTESIAN_POINT('',(-1.73939636646037,-2.10523216165204,8.78727029226991));
#401133=CARTESIAN_POINT('Origin',(-1.73208666082126,-2.07039626697765,8.75658640621007));
#401134=CARTESIAN_POINT('',(-1.72471465490914,-2.0352634676321,8.85049129520029));
#401135=CARTESIAN_POINT('Ctrl Pts',(-1.73939636646037,-2.10523216165204,
8.78727029226991));
#401136=CARTESIAN_POINT('Ctrl Pts',(-1.73450940418104,-2.08194234511969,
8.80838212259896));
#401137=CARTESIAN_POINT('Ctrl Pts',(-1.72961567252274,-2.0586202677297,
8.82945686509571));
#401138=CARTESIAN_POINT('Ctrl Pts',(-1.72471465490914,-2.0352634676321,
8.85049129520029));
#401139=CARTESIAN_POINT('',(-1.72471465490914,-2.0352634676321,7.59394543036555));
#401140=CARTESIAN_POINT('',(-1.72471465490914,-2.0352634676321,7.5));
#401141=CARTESIAN_POINT('',(-1.74227604793054,-2.11895587165399,7.51860402984325));
#401142=CARTESIAN_POINT('Ctrl Pts',(-1.72471465490914,-2.0352634676321,
7.59394543036555));
#401143=CARTESIAN_POINT('Ctrl Pts',(-1.72830937827429,-2.05239485577748,
7.57858609112103));
#401144=CARTESIAN_POINT('Ctrl Pts',(-1.73190007916554,-2.06950707400212,
7.56320440326857));
#401145=CARTESIAN_POINT('Ctrl Pts',(-1.73548696839503,-2.08660112697448,
7.54780169004651));
#401146=CARTESIAN_POINT('Ctrl Pts',(-1.73775149593086,-2.09739319530395,
7.53807742314383));
#401147=CARTESIAN_POINT('Ctrl Pts',(-1.74001450601091,-2.10817803188809,
7.52834476460825));
#401148=CARTESIAN_POINT('Ctrl Pts',(-1.74227604793054,-2.11895587165399,
7.51860402984325));
#401149=CARTESIAN_POINT('',(-1.74227604793054,-2.11895587165399,7.5));
#401150=CARTESIAN_POINT('Origin',(-1.7314431241816,-2.0338516155685,7.5));
#401151=CARTESIAN_POINT('Ctrl Pts',(-1.72471465490914,-2.0352634676321,
8.85049129520029));
#401152=CARTESIAN_POINT('Ctrl Pts',(-1.72467488452415,-2.03507393374238,
8.85097269580138));
#401153=CARTESIAN_POINT('Ctrl Pts',(-1.7246438480515,-2.03488506380326,
8.85143669361005));
#401154=CARTESIAN_POINT('Ctrl Pts',(-1.72462097907697,-2.03468801919691,
8.8519052845931));
#401155=CARTESIAN_POINT('Ctrl Pts',(-1.72457624881308,-2.03430261244298,
8.85282181883899));
#401156=CARTESIAN_POINT('Ctrl Pts',(-1.72456411104288,-2.03389582367071,
8.85372622499635));
#401157=CARTESIAN_POINT('Ctrl Pts',(-1.72459978718338,-2.03346080980621,
8.8546225773507));
#401158=CARTESIAN_POINT('Ctrl Pts',(-1.72462940424813,-2.03309967674613,
8.85536669723986));
#401159=CARTESIAN_POINT('Ctrl Pts',(-1.72469194862657,-2.03271900678389,
8.85610498449051));
#401160=CARTESIAN_POINT('Ctrl Pts',(-1.72480403100063,-2.03231614987659,
8.85681338218371));
#401161=CARTESIAN_POINT('Ctrl Pts',(-1.72490574593113,-2.03195055660051,
8.85745625420284));
#401162=CARTESIAN_POINT('Ctrl Pts',(-1.72504895764684,-2.03156194465407,
8.85808743050666));
#401163=CARTESIAN_POINT('Ctrl Pts',(-1.72526213979698,-2.03114764993346,
8.8586680450841));
#401164=CARTESIAN_POINT('Ctrl Pts',(-1.72536049741984,-2.03095650333018,
8.85893592806395));
#401165=CARTESIAN_POINT('Ctrl Pts',(-1.72547399192871,-2.03075989601328,
8.85919241173848));
#401166=CARTESIAN_POINT('Ctrl Pts',(-1.72560699390353,-2.0305578307355,
8.85943017985534));
#401167=CARTESIAN_POINT('Ctrl Pts',(-1.72578658594233,-2.03028498279278,
8.8597512372));
#401168=CARTESIAN_POINT('Ctrl Pts',(-1.72600685206651,-2.02999559083906,
8.86004599534706));
#401169=CARTESIAN_POINT('Ctrl Pts',(-1.72627343343412,-2.02969943976519,
8.86026130871721));
#401170=CARTESIAN_POINT('Ctrl Pts',(-1.72637103638852,-2.02959101050766,
8.86034014101235));
#401171=CARTESIAN_POINT('Ctrl Pts',(-1.72647630483696,-2.02948003821962,
8.86040910639692));
#401172=CARTESIAN_POINT('Ctrl Pts',(-1.72658661484442,-2.02936977777993,
8.86046313645506));
#401173=CARTESIAN_POINT('Ctrl Pts',(-1.72675875268721,-2.02919771728722,
8.86054744990829));
#401174=CARTESIAN_POINT('Ctrl Pts',(-1.72694797019717,-2.02902279750387,
8.86059655985668));
#401175=CARTESIAN_POINT('Ctrl Pts',(-1.72714193341414,-2.02885602144795,
8.86059725258816));
#401176=CARTESIAN_POINT('Ctrl Pts',(-1.72733634476364,-2.02868886007271,
8.86059794692011));
#401177=CARTESIAN_POINT('Ctrl Pts',(-1.7275394119433,-2.02853004075073,
8.86056369958366));
#401178=CARTESIAN_POINT('Ctrl Pts',(-1.72773774127272,-2.02838526137766,
8.86048590497774));
#401179=CARTESIAN_POINT('Ctrl Pts',(-1.72778949932273,-2.02834747827189,
8.86046560290182));
#401180=CARTESIAN_POINT('Ctrl Pts',(-1.7278416614481,-2.02831023298624,
8.86044257503091));
#401181=CARTESIAN_POINT('Ctrl Pts',(-1.72789259672071,-2.02827464971588,
8.86041778462583));
#401182=CARTESIAN_POINT('Ctrl Pts',(-1.72823532789993,-2.02803521846152,
8.86025097596201));
#401183=CARTESIAN_POINT('Ctrl Pts',(-1.7285686918965,-2.0278391805111,8.8599848982295));
#401184=CARTESIAN_POINT('Ctrl Pts',(-1.72887866392139,-2.02768495440917,
8.85968173251461));
#401185=CARTESIAN_POINT('Ctrl Pts',(-1.72904262136327,-2.02760337763735,
8.85952137522076));
#401186=CARTESIAN_POINT('Ctrl Pts',(-1.72920310952448,-2.02753175558216,
8.85934740853961));
#401187=CARTESIAN_POINT('Ctrl Pts',(-1.72935723163294,-2.02746967867184,
8.8591675900182));
#401188=CARTESIAN_POINT('Ctrl Pts',(-1.72997611200949,-2.02722040760996,
8.85844552518695));
#401189=CARTESIAN_POINT('Ctrl Pts',(-1.7305261907919,-2.02710815126501,
8.85759444184125));
#401190=CARTESIAN_POINT('Ctrl Pts',(-1.73098291656963,-2.02705690851457,
8.85683498915139));
#401191=CARTESIAN_POINT('Ctrl Pts',(-1.73103071170591,-2.02705154609721,
8.85675551444998));
#401192=CARTESIAN_POINT('Ctrl Pts',(-1.73107748282563,-2.02704687173969,
8.85667699793651));
#401193=CARTESIAN_POINT('Ctrl Pts',(-1.73112319999987,-2.02704281135589,
8.85659965593547));
#401194=CARTESIAN_POINT('Ctrl Pts',(-1.73174029275058,-2.02698800408813,
8.85555568965886));
#401195=CARTESIAN_POINT('Ctrl Pts',(-1.73234127237003,-2.02702445131194,
8.85434650606346));
#401196=CARTESIAN_POINT('Ctrl Pts',(-1.73292948597224,-2.02714612986161,
8.85297329937118));
#401197=CARTESIAN_POINT('Ctrl Pts',(-1.73326032028311,-2.02721456663182,
8.85220095427748));
#401198=CARTESIAN_POINT('Ctrl Pts',(-1.73358718755086,-2.02731030181011,
8.85137579139184));
#401199=CARTESIAN_POINT('Ctrl Pts',(-1.73391074180929,-2.02743472471361,
8.85049129520029));
#401200=CARTESIAN_POINT('Origin',(-1.7314431241816,-2.0338516155685,7.59394543036555));
#401201=CARTESIAN_POINT('Ctrl Pts',(-1.72459918806511,-2.0347131868116,
7.59443877723642));
#401202=CARTESIAN_POINT('Ctrl Pts',(-1.7234099906709,-2.02904582382637,
7.58783886950016));
#401203=CARTESIAN_POINT('Ctrl Pts',(-1.73109008020605,-2.02542706626766,
7.58559994247159));
#401204=CARTESIAN_POINT('Ctrl Pts',(-1.73109098175056,-2.06565115507454,
7.56670252222133));
#401205=CARTESIAN_POINT('Ctrl Pts',(-1.72990350308425,-2.05999198303778,
7.5600487499902));
#401206=CARTESIAN_POINT('Ctrl Pts',(-1.73761999295569,-2.05633245556569,
7.55786368756705));
#401207=CARTESIAN_POINT('Ctrl Pts',(-1.73757065265992,-2.09653134977288,
7.53888913333557));
#401208=CARTESIAN_POINT('Ctrl Pts',(-1.7363761167497,-2.09083854499964,
7.53222002137274));
#401209=CARTESIAN_POINT('Ctrl Pts',(-1.74413680190624,-2.08718146821332,
7.53005029815327));
#401210=CARTESIAN_POINT('Ctrl Pts',(-1.74403790758369,-2.12735237355686,
7.51101258149734));
#401211=CARTESIAN_POINT('Ctrl Pts',(-1.74282889172772,-2.12159056164571,
7.5043616886572));
#401212=CARTESIAN_POINT('Ctrl Pts',(-1.75064026593581,-2.11797256295502,
7.50217374673251));
#401213=CARTESIAN_POINT('',(-1.75029323173561,-2.11632951079882,7.50366116523517));
#401214=CARTESIAN_POINT('Ctrl Pts',(-1.74227604793054,-2.11895587165399,
7.51860402984325));
#401215=CARTESIAN_POINT('Ctrl Pts',(-1.74236673734234,-2.11938807056232,
7.51734760759494));
#401216=CARTESIAN_POINT('Ctrl Pts',(-1.74250691691215,-2.11976640579486,
7.51608817408573));
#401217=CARTESIAN_POINT('Ctrl Pts',(-1.74270878598765,-2.12008536764088,
7.5148100591312));
#401218=CARTESIAN_POINT('Ctrl Pts',(-1.74289164382005,-2.12037429090284,
7.51365231206384));
#401219=CARTESIAN_POINT('Ctrl Pts',(-1.74312516530045,-2.12061503834426,
7.51247773061043));
#401220=CARTESIAN_POINT('Ctrl Pts',(-1.74343181434905,-2.12077773502144,
7.51129758471022));
#401221=CARTESIAN_POINT('Ctrl Pts',(-1.74381294409581,-2.12097994841053,
7.50983079813402));
#401222=CARTESIAN_POINT('Ctrl Pts',(-1.74430097953774,-2.12104363261567,
7.50839324291155));
#401223=CARTESIAN_POINT('Ctrl Pts',(-1.74491014972064,-2.12088750587553,
7.50715379678855));
#401224=CARTESIAN_POINT('Ctrl Pts',(-1.74519156879233,-2.12081537982027,
7.50658120839351));
#401225=CARTESIAN_POINT('Ctrl Pts',(-1.74553648740116,-2.1206768846844,
7.50598221009429));
#401226=CARTESIAN_POINT('Ctrl Pts',(-1.74592822130452,-2.12045420802353,
7.50545747549611));
#401227=CARTESIAN_POINT('Ctrl Pts',(-1.74613726264066,-2.1203353808648,
7.50517746087247));
#401228=CARTESIAN_POINT('Ctrl Pts',(-1.74636200201908,-2.1201914695418,
7.50491486231392));
#401229=CARTESIAN_POINT('Ctrl Pts',(-1.74659558846567,-2.12002488036818,
7.50468370960992));
#401230=CARTESIAN_POINT('Ctrl Pts',(-1.74694487388399,-2.11977577700604,
7.50433806340446));
#401231=CARTESIAN_POINT('Ctrl Pts',(-1.74732409157993,-2.11946804380051,
7.50405484070984));
#401232=CARTESIAN_POINT('Ctrl Pts',(-1.74770725053022,-2.119121849733,7.50385766036131));
#401233=CARTESIAN_POINT('Ctrl Pts',(-1.74774822342432,-2.11908482965855,
7.50383657498791));
#401234=CARTESIAN_POINT('Ctrl Pts',(-1.74778923293594,-2.11904739685898,
7.50381643264937));
#401235=CARTESIAN_POINT('Ctrl Pts',(-1.74783024145072,-2.11900959576149,
7.50379723213559));
#401236=CARTESIAN_POINT('Ctrl Pts',(-1.7481039867017,-2.11875726107019,
7.50366906242519));
#401237=CARTESIAN_POINT('Ctrl Pts',(-1.74838315477833,-2.11848249746138,
7.50358235568538));
#401238=CARTESIAN_POINT('Ctrl Pts',(-1.74864587227851,-2.11821119094112,
7.5035341175365));
#401239=CARTESIAN_POINT('Ctrl Pts',(-1.74903978743616,-2.11780439751997,
7.50346178989176));
#401240=CARTESIAN_POINT('Ctrl Pts',(-1.74944625412045,-2.11735003155156,
7.50346967198527));
#401241=CARTESIAN_POINT('Ctrl Pts',(-1.74983155360463,-2.1168917069529,
7.50354272648692));
#401242=CARTESIAN_POINT('Ctrl Pts',(-1.7499900352577,-2.11670318855871,
7.50357277531559));
#401243=CARTESIAN_POINT('Ctrl Pts',(-1.7501448337127,-2.11651434214921,
7.50361331098761));
#401244=CARTESIAN_POINT('Ctrl Pts',(-1.75029323173652,-2.11632951079991,
7.50366116523659));
#401245=CARTESIAN_POINT('',(-1.73334108842445,-2.03608107236507,7.57603338622103));
#401246=CARTESIAN_POINT('Origin',(-1.73907161540567,-2.04280807393543,7.58486873427627));
#401247=CARTESIAN_POINT('Ctrl Pts',(-1.75029323174217,-2.11632951085579,
7.50366116529969));
#401248=CARTESIAN_POINT('Ctrl Pts',(-1.74465255589966,-2.08962350825637,
7.52783573079709));
#401249=CARTESIAN_POINT('Ctrl Pts',(-1.7390021257961,-2.06287528805497,
7.55196141284069));
#401250=CARTESIAN_POINT('Ctrl Pts',(-1.73334108832669,-2.03608107361331,
7.57603338728831));
#401251=CARTESIAN_POINT('Ctrl Pts',(-1.72509791827961,-2.03623385142682,
7.59639677331372));
#401252=CARTESIAN_POINT('Ctrl Pts',(-1.71825676553203,-2.01836216837368,
7.59974925422225));
#401253=CARTESIAN_POINT('Ctrl Pts',(-1.73480751822064,-2.02796794848296,
7.59639677331372));
#401254=CARTESIAN_POINT('Ctrl Pts',(-1.72313602699774,-2.03286248869316,
7.58707626057422));
#401255=CARTESIAN_POINT('Ctrl Pts',(-1.72493641503088,-2.02620846475785,
7.58811717123965));
#401256=CARTESIAN_POINT('Ctrl Pts',(-1.73179248798735,-2.02549313601007,
7.58707626057424));
#401257=CARTESIAN_POINT('Ctrl Pts',(-1.72903043012316,-2.03433952764208,
7.5801537675693));
#401258=CARTESIAN_POINT('Ctrl Pts',(-1.72941656890807,-2.03147110842989,
7.58208760766041));
#401259=CARTESIAN_POINT('Ctrl Pts',(-1.73230984781102,-2.03154771866078,
7.5801537675693));
#401260=CARTESIAN_POINT('Ctrl Pts',(-1.73334108788784,-2.03608107173505,
7.57603338509286));
#401261=CARTESIAN_POINT('Ctrl Pts',(-1.73334108788784,-2.03608107173505,
7.57603338509286));
#401262=CARTESIAN_POINT('Ctrl Pts',(-1.73334108788784,-2.03608107173505,
7.57603338509286));
#401263=CARTESIAN_POINT('Origin',(-1.73906727032637,-2.0428117729544,7.58486873427621));
#401264=CARTESIAN_POINT('Ctrl Pts',(-1.82176055196474,-2.06121740000461,
7.51098857897448));
#401265=CARTESIAN_POINT('Ctrl Pts',(-1.81626552995068,-2.05910428736283,
7.50433767179956));
#401266=CARTESIAN_POINT('Ctrl Pts',(-1.81144720769181,-2.06623813777422,
7.50214974420965));
#401267=CARTESIAN_POINT('Ctrl Pts',(-1.79235831753897,-2.04991076044924,
7.53887321589164));
#401268=CARTESIAN_POINT('Ctrl Pts',(-1.78692913564055,-2.04782296664701,
7.53220407452058));
#401269=CARTESIAN_POINT('Ctrl Pts',(-1.78208030704416,-2.05490052139174,
7.53003438070911));
#401270=CARTESIAN_POINT('Ctrl Pts',(-1.76289961997713,-2.0385824079751,
7.56669465659231));
#401271=CARTESIAN_POINT('Ctrl Pts',(-1.75750252353432,-2.03650695264607,
7.56004085833295));
#401272=CARTESIAN_POINT('Ctrl Pts',(-1.75265832922258,-2.04354047463692,
7.55785582193789));
#401273=CARTESIAN_POINT('Ctrl Pts',(-1.73338579157812,-2.02723285491819,
7.59443891967696));
#401274=CARTESIAN_POINT('Ctrl Pts',(-1.72798087001745,-2.02515439043735,
7.58783901202978));
#401275=CARTESIAN_POINT('Ctrl Pts',(-1.7231827570306,-2.0321584813672,7.58560008491213));
#401276=CARTESIAN_POINT('',(-1.80985532470035,-2.06562356178256,7.50366116523517));
#401277=CARTESIAN_POINT('Ctrl Pts',(-1.8098553247006,-2.06562356178284,
7.50366116523554));
#401278=CARTESIAN_POINT('Ctrl Pts',(-1.81051422460561,-2.06524941150295,
7.50350835821027));
#401279=CARTESIAN_POINT('Ctrl Pts',(-1.81110774094972,-2.06488403996545,
7.50345484956));
#401280=CARTESIAN_POINT('Ctrl Pts',(-1.81165383425926,-2.06451709574946,
7.50349758195598));
#401281=CARTESIAN_POINT('Ctrl Pts',(-1.8119340206264,-2.06432882615336,
7.50351950684424));
#401282=CARTESIAN_POINT('Ctrl Pts',(-1.81222941160284,-2.06412169339066,
7.50357029184312));
#401283=CARTESIAN_POINT('Ctrl Pts',(-1.81250876338827,-2.06391412790494,
7.50365515313924));
#401284=CARTESIAN_POINT('Ctrl Pts',(-1.81293851955496,-2.06359480813633,
7.50378570417639));
#401285=CARTESIAN_POINT('Ctrl Pts',(-1.81334313802457,-2.0632653695642,
7.50400001621911));
#401286=CARTESIAN_POINT('Ctrl Pts',(-1.81369038795123,-2.06294912660894,
7.50428903009634));
#401287=CARTESIAN_POINT('Ctrl Pts',(-1.81372893002152,-2.06291402607393,
7.50432110841318));
#401288=CARTESIAN_POINT('Ctrl Pts',(-1.81376679539125,-2.06287908401768,
7.50435406373354));
#401289=CARTESIAN_POINT('Ctrl Pts',(-1.81380396212087,-2.06284432900478,
7.50438785222352));
#401290=CARTESIAN_POINT('Ctrl Pts',(-1.8140308828698,-2.06263213294569,
7.50459414719561));
#401291=CARTESIAN_POINT('Ctrl Pts',(-1.81423502103158,-2.06242315419714,
7.50483629897752));
#401292=CARTESIAN_POINT('Ctrl Pts',(-1.81440949754729,-2.06222631828135,
7.5050991045531));
#401293=CARTESIAN_POINT('Ctrl Pts',(-1.81479441026545,-2.06179207848082,
7.50567888004914));
#401294=CARTESIAN_POINT('Ctrl Pts',(-1.8150505204398,-2.0614001699654,7.50637912803144));
#401295=CARTESIAN_POINT('Ctrl Pts',(-1.8152072198962,-2.06106016033291,
7.50710440483569));
#401296=CARTESIAN_POINT('Ctrl Pts',(-1.81524564571382,-2.06097678322089,
7.50728225710685));
#401297=CARTESIAN_POINT('Ctrl Pts',(-1.81527899117964,-2.06089492823592,
7.50746498566954));
#401298=CARTESIAN_POINT('Ctrl Pts',(-1.81530686371104,-2.06081666330602,
7.50764697238949));
#401299=CARTESIAN_POINT('Ctrl Pts',(-1.81545669876911,-2.06039593258197,
7.50862528291182));
#401300=CARTESIAN_POINT('Ctrl Pts',(-1.8154658754865,-2.06004214442774,
7.50965856837422));
#401301=CARTESIAN_POINT('Ctrl Pts',(-1.81539869370008,-2.05973914561394,
7.51067959873203));
#401302=CARTESIAN_POINT('Ctrl Pts',(-1.81536172347828,-2.05957240498452,
7.51124147302579));
#401303=CARTESIAN_POINT('Ctrl Pts',(-1.81530119636746,-2.05942109830839,
7.51180065547253));
#401304=CARTESIAN_POINT('Ctrl Pts',(-1.81522519946109,-2.05928321799138,
7.51235175716501));
#401305=CARTESIAN_POINT('Ctrl Pts',(-1.81496259987603,-2.0588067865711,
7.51425603304536));
#401306=CARTESIAN_POINT('Ctrl Pts',(-1.814478673106,-2.0584367848023,7.51626900505181));
#401307=CARTESIAN_POINT('Ctrl Pts',(-1.81383371736442,-2.05817060637484,
7.51827788969245));
#401308=CARTESIAN_POINT('Ctrl Pts',(-1.81379881114089,-2.05815620029534,
7.51838661432546));
#401309=CARTESIAN_POINT('Ctrl Pts',(-1.81376342381362,-2.0581421015707,
7.51849533314857));
#401310=CARTESIAN_POINT('Ctrl Pts',(-1.813727561987,-2.05812831089271,7.51860402984325));
#401311=CARTESIAN_POINT('Ctrl Pts',(-1.73334108967324,-2.03608107246854,
7.57603338728985));
#401312=CARTESIAN_POINT('Ctrl Pts',(-1.75888834909077,-2.04594589934822,
7.55196141284922));
#401313=CARTESIAN_POINT('Ctrl Pts',(-1.7843918967819,-2.05579291415967,
7.52783573083105));
#401314=CARTESIAN_POINT('Ctrl Pts',(-1.80985532475728,-2.06562356179871,
7.50366116530176));
#401315=CARTESIAN_POINT('Origin',(-5.98949470795629E-16,-7.0356012958692E-16,
7.49482233047033));
#401316=CARTESIAN_POINT('Origin',(-1.7446600766167,-2.1095183021391,7.49482233047033));
#401317=CARTESIAN_POINT('Origin',(0.,0.,7.50366116523517));
#401318=CARTESIAN_POINT('Origin',(-1.80403047455412,-2.05897554547888,7.49482233047033));
#401319=CARTESIAN_POINT('Ctrl Pts',(-1.74227583067299,-2.11895483648669,
7.51860402984325));
#401320=CARTESIAN_POINT('Ctrl Pts',(-1.74383903929183,-2.12640149109424,
7.51860402984325));
#401321=CARTESIAN_POINT('Ctrl Pts',(-1.73794220472938,-2.13121019447177,
7.51860402984325));
#401322=CARTESIAN_POINT('Ctrl Pts',(-1.74285625945743,-2.12171983042215,
7.51041458714365));
#401323=CARTESIAN_POINT('Ctrl Pts',(-1.74244200538642,-2.12754072033047,
7.51004642900441));
#401324=CARTESIAN_POINT('Ctrl Pts',(-1.73794057845242,-2.13121152065507,
7.50729136483009));
#401325=CARTESIAN_POINT('Ctrl Pts',(-1.74564151586071,-2.12212736442963,
7.50215815450138));
#401326=CARTESIAN_POINT('Ctrl Pts',(-1.74528659454811,-2.12522124473491,
7.49877163671531));
#401327=CARTESIAN_POINT('Ctrl Pts',(-1.74262787488409,-2.12742013839822,
7.49481588533172));
#401328=CARTESIAN_POINT('Ctrl Pts',(-1.75029288088052,-2.11632908656917,
7.50366171572174));
#401329=CARTESIAN_POINT('Ctrl Pts',(-1.75262656098511,-2.11915080580159,
7.50000045605858));
#401330=CARTESIAN_POINT('Ctrl Pts',(-1.75262656098502,-2.11915080580166,
7.49482233047317));
#401331=CARTESIAN_POINT('Origin',(-1.73004246743515,-2.12152287540599,7.51860402984325));
#401332=CARTESIAN_POINT('Origin',(-1.73004246743515,-2.12152287540599,9.));
#401333=CARTESIAN_POINT('Origin',(-1.73004246743515,-2.12152287540599,8.75721825406948));
#401334=CARTESIAN_POINT('Ctrl Pts',(-1.73884646826615,-2.10261165664174,
8.78942910404912));
#401335=CARTESIAN_POINT('Ctrl Pts',(-1.74001060278245,-2.10806117217338,
8.79672699501689));
#401336=CARTESIAN_POINT('Ctrl Pts',(-1.73177243323851,-2.11149716526814,
8.79893251111266));
#401337=CARTESIAN_POINT('Ctrl Pts',(-1.74110427278992,-2.11337166302987,
8.78111911759584));
#401338=CARTESIAN_POINT('Ctrl Pts',(-1.74247708815732,-2.11983368191661,
8.78644465894819));
#401339=CARTESIAN_POINT('Ctrl Pts',(-1.73583860290615,-2.12448621083597,
8.78817647674132));
#401340=CARTESIAN_POINT('Ctrl Pts',(-1.74251139039172,-2.1200775556679,
8.76780923932029));
#401341=CARTESIAN_POINT('Ctrl Pts',(-1.74412695641818,-2.12770675504822,
8.76988516158369));
#401342=CARTESIAN_POINT('Ctrl Pts',(-1.73836760030061,-2.13260228336569,
8.77093053738832));
#401343=CARTESIAN_POINT('Ctrl Pts',(-1.74223702171543,-2.11876999838042,
8.75371302330492));
#401344=CARTESIAN_POINT('Ctrl Pts',(-1.74381368245516,-2.1262117953596,
8.7530082828756));
#401345=CARTESIAN_POINT('Ctrl Pts',(-1.73787390625973,-2.13101945571392,
8.75267964240738));
#401346=CARTESIAN_POINT('Origin',(-1.72716278596498,-2.10779916540405,8.78727029226991));
#401347=CARTESIAN_POINT('Ctrl Pts',(-1.72471465490914,-2.0352634676321,
8.85049129520029));
#401348=CARTESIAN_POINT('Ctrl Pts',(-1.72591388015441,-2.04097862038896,
8.85711686593484));
#401349=CARTESIAN_POINT('Ctrl Pts',(-1.71816751245361,-2.04459725957488,
8.85933012996512));
#401350=CARTESIAN_POINT('Ctrl Pts',(-1.72961567910009,-2.05862029907538,
8.82945683644723));
#401351=CARTESIAN_POINT('Ctrl Pts',(-1.73082485863996,-2.06438289105558,
8.83607469902389));
#401352=CARTESIAN_POINT('Ctrl Pts',(-1.72303987536888,-2.06797817657507,
8.8382956714852));
#401353=CARTESIAN_POINT('Ctrl Pts',(-1.73450939791927,-2.08194231527794,
8.80838214965001));
#401354=CARTESIAN_POINT('Ctrl Pts',(-1.73572334944616,-2.08772764913656,
8.81501364461988));
#401355=CARTESIAN_POINT('Ctrl Pts',(-1.72790550163945,-2.09132348954826,
8.81722098428721));
#401356=CARTESIAN_POINT('Ctrl Pts',(-1.73939636646037,-2.10523216165204,
8.78727029226991));
#401357=CARTESIAN_POINT('Ctrl Pts',(-1.7406105196286,-2.11101845647365,
8.79393457792714));
#401358=CARTESIAN_POINT('Ctrl Pts',(-1.73276491989237,-2.11463591137414,
8.79610912703474));
#401359=CARTESIAN_POINT('Origin',(-1.71248107441375,-2.03783047138411,8.85049129520029));
#401360=CARTESIAN_POINT('Ctrl Pts',(-1.73391074180929,-2.02743472471361,
8.85049129520029));
#401361=CARTESIAN_POINT('Ctrl Pts',(-1.73936124027702,-2.02953071581005,
8.85711686593484));
#401362=CARTESIAN_POINT('Ctrl Pts',(-1.74416981443405,-2.02246117716243,
8.85933012996512));
#401363=CARTESIAN_POINT('Ctrl Pts',(-1.72908876449367,-2.02558043164655,
8.86332496987232));
#401364=CARTESIAN_POINT('Ctrl Pts',(-1.73278367143589,-2.02280562407395,
8.86648636486738));
#401365=CARTESIAN_POINT('Ctrl Pts',(-1.73067398692192,-2.0172897077272,
8.87206031107457));
#401366=CARTESIAN_POINT('Ctrl Pts',(-1.72364650824247,-2.03017299660442,
8.86341338519876));
#401367=CARTESIAN_POINT('Ctrl Pts',(-1.72028763309307,-2.03336539826539,
8.86654584966058));
#401368=CARTESIAN_POINT('Ctrl Pts',(-1.71519106383778,-2.03034064462033,
8.87215952290714));
#401369=CARTESIAN_POINT('Ctrl Pts',(-1.72471465490914,-2.0352634676321,
8.85049129520029));
#401370=CARTESIAN_POINT('Ctrl Pts',(-1.72591388015441,-2.04097862038896,
8.85711686593484));
#401371=CARTESIAN_POINT('Ctrl Pts',(-1.71816751245361,-2.04459725957488,
8.85933012996512));
#401372=CARTESIAN_POINT('Origin',(-1.73839731931417,-2.015767650432,8.85049129520029));
#401373=CARTESIAN_POINT('Ctrl Pts',(-1.80063936233259,-2.05309523912754,
8.78727029226991));
#401374=CARTESIAN_POINT('Ctrl Pts',(-1.80615770845573,-2.05521732106365,
8.79393457792714));
#401375=CARTESIAN_POINT('Ctrl Pts',(-1.8109809509302,-2.0480496333465,8.79610912703474));
#401376=CARTESIAN_POINT('Ctrl Pts',(-1.77842800991973,-2.044553855771,8.80838214965002));
#401377=CARTESIAN_POINT('Ctrl Pts',(-1.78394543957973,-2.04667558528088,
8.81501364461995));
#401378=CARTESIAN_POINT('Ctrl Pts',(-1.7887429154195,-2.03953184409284,
8.8172209842872));
#401379=CARTESIAN_POINT('Ctrl Pts',(-1.75618597738195,-2.03600067436165,
8.82945683644722));
#401380=CARTESIAN_POINT('Ctrl Pts',(-1.7616817182824,-2.03811406345147,
8.83607469902389));
#401381=CARTESIAN_POINT('Ctrl Pts',(-1.76647340116631,-2.03100267697358,
8.8382956714852));
#401382=CARTESIAN_POINT('Ctrl Pts',(-1.73391074180929,-2.02743472471361,
8.85049129520029));
#401383=CARTESIAN_POINT('Ctrl Pts',(-1.73936124027702,-2.02953071581005,
8.85711686593484));
#401384=CARTESIAN_POINT('Ctrl Pts',(-1.74416981443405,-2.02246117716243,
8.85933012996512));
#401385=CARTESIAN_POINT('Origin',(-1.80512593983747,-2.04142816484593,8.78727029226991));
#401386=CARTESIAN_POINT('Ctrl Pts',(-1.81355474551559,-2.05806183449402,
8.75374538247848));
#401387=CARTESIAN_POINT('Ctrl Pts',(-1.82064264673989,-2.06080154882625,
8.75304829418601));
#401388=CARTESIAN_POINT('Ctrl Pts',(-1.82633439346053,-2.05571483451569,
8.75272238421917));
#401389=CARTESIAN_POINT('Ctrl Pts',(-1.81478677317361,-2.05853561161882,
8.76769408445021));
#401390=CARTESIAN_POINT('Ctrl Pts',(-1.82205328625124,-2.06134362562603,
8.76974318093972));
#401391=CARTESIAN_POINT('Ctrl Pts',(-1.82780144389182,-2.0564469899423,
8.7707786988043));
#401392=CARTESIAN_POINT('Ctrl Pts',(-1.80847210123318,-2.05610729998394,
8.78108014887987));
#401393=CARTESIAN_POINT('Ctrl Pts',(-1.81462883978909,-2.05849053468797,
8.78639403366321));
#401394=CARTESIAN_POINT('Ctrl Pts',(-1.82028708005224,-2.05270206400449,
8.78812224174741));
#401395=CARTESIAN_POINT('Ctrl Pts',(-1.79812374791357,-2.05212783323685,
8.78944554828685));
#401396=CARTESIAN_POINT('Ctrl Pts',(-1.80331039816767,-2.05414155535238,
8.79673892988687));
#401397=CARTESIAN_POINT('Ctrl Pts',(-1.8080143434309,-2.04656683071863,
8.79894799272499));
#401398=CARTESIAN_POINT('Origin',(-1.81821413949188,-2.0464612366111,8.75721825406948));
#401399=CARTESIAN_POINT('Origin',(-1.81821413949188,-2.0464612366111,9.));
#401400=CARTESIAN_POINT('Origin',(-1.81821413949188,-2.0464612366111,7.51860402984325));
#401401=CARTESIAN_POINT('Ctrl Pts',(-1.80985480628381,-2.06562297010346,
7.50366195182966));
#401402=CARTESIAN_POINT('Ctrl Pts',(-1.81226805662981,-2.06837726029833,
7.50000065167735));
#401403=CARTESIAN_POINT('Ctrl Pts',(-1.8122680566299,-2.06837726029825,
7.49482233047108));
#401404=CARTESIAN_POINT('Ctrl Pts',(-1.81632644357473,-2.06195258723768,
7.50215800491337));
#401405=CARTESIAN_POINT('Ctrl Pts',(-1.81943843694026,-2.06209469447589,
7.49877273257264));
#401406=CARTESIAN_POINT('Ctrl Pts',(-1.82203492295881,-2.05981974025537,
7.49481816995649));
#401407=CARTESIAN_POINT('Ctrl Pts',(-1.81635821181536,-2.0591402915347,
7.51043025814042));
#401408=CARTESIAN_POINT('Ctrl Pts',(-1.82217354593106,-2.05966435842889,
7.51006209594515));
#401409=CARTESIAN_POINT('Ctrl Pts',(-1.82651837989694,-2.05580412683336,
7.50731281821698));
#401410=CARTESIAN_POINT('Ctrl Pts',(-1.81372615132356,-2.05812776832369,
7.51860402984325));
#401411=CARTESIAN_POINT('Ctrl Pts',(-1.82082805618867,-2.06085979406984,
7.51860402984325));
#401412=CARTESIAN_POINT('Ctrl Pts',(-1.8265164871608,-2.05580580846777,
7.51860402984325));
#401413=CARTESIAN_POINT('Origin',(0.,0.,7.5));
#401414=CARTESIAN_POINT('Origin',(-1.60045004741996,-2.13436118528464,7.5));
#401415=CARTESIAN_POINT('',(-1.60045004741996,-2.13436118528464,7.59394543036555));
#401416=CARTESIAN_POINT('',(-1.60045004741996,-2.13436118528464,8.85049129520029));
#401417=CARTESIAN_POINT('',(-1.60045004741996,-2.13436118528464,7.5));
#401418=CARTESIAN_POINT('',(-1.66539749203245,-2.16424429481556,8.78727029226991));
#401419=CARTESIAN_POINT('Ctrl Pts',(-1.60045004741996,-2.13436118528464,
8.85049129520029));
#401420=CARTESIAN_POINT('Ctrl Pts',(-1.62213066475764,-2.14433670112619,
8.82945686509571));
#401421=CARTESIAN_POINT('Ctrl Pts',(-1.64377905123609,-2.15429738715722,
8.80838212259897));
#401422=CARTESIAN_POINT('Ctrl Pts',(-1.66539749203245,-2.16424429481556,
8.78727029226991));
#401423=CARTESIAN_POINT('',(-1.67813633056179,-2.170105589426,8.75721825406948));
#401424=CARTESIAN_POINT('Origin',(-1.63980066194096,-2.15246710397329,8.75937679713085));
#401425=CARTESIAN_POINT('',(-1.67813633056179,-2.170105589426,7.51860402984325));
#401426=CARTESIAN_POINT('',(-1.67813633056179,-2.170105589426,7.5));
#401427=CARTESIAN_POINT('Ctrl Pts',(-1.67813633056179,-2.170105589426,7.51860402984325));
#401428=CARTESIAN_POINT('Ctrl Pts',(-1.66813195416114,-2.16550245411324,
7.52834476460825));
#401429=CARTESIAN_POINT('Ctrl Pts',(-1.6581210830637,-2.16089633051147,
7.53807742314407));
#401430=CARTESIAN_POINT('Ctrl Pts',(-1.64810349920137,-2.15628711828489,
7.54780169004674));
#401431=CARTESIAN_POINT('Ctrl Pts',(-1.63223618776764,-2.14898637522465,
7.5632044032688));
#401432=CARTESIAN_POINT('Ctrl Pts',(-1.61635201469678,-2.14167787391998,
7.57858609112103));
#401433=CARTESIAN_POINT('Ctrl Pts',(-1.60045004741996,-2.13436118528464,
7.59394543036555));
#401434=CARTESIAN_POINT('Origin',(-1.62988553581356,-2.41378875122106,7.5));
#401435=CARTESIAN_POINT('',(-1.60293438610525,-2.2262302592164,8.75721825406948));
#401436=CARTESIAN_POINT('',(-1.60093990236828,-2.21235024422326,8.78727029226991));
#401437=CARTESIAN_POINT('Origin',(-1.59587715873825,-2.17711758918138,8.75658640620972));
#401438=CARTESIAN_POINT('',(-1.59077126558566,-2.14158464790052,8.85049129520029));
#401439=CARTESIAN_POINT('Ctrl Pts',(-1.60093990236828,-2.21235024422326,
8.78727029226991));
#401440=CARTESIAN_POINT('Ctrl Pts',(-1.59755516454562,-2.18879517036853,
8.80838212259896));
#401441=CARTESIAN_POINT('Ctrl Pts',(-1.59416573821265,-2.16520746822394,
8.82945686509571));
#401442=CARTESIAN_POINT('Ctrl Pts',(-1.59077126558566,-2.14158464790052,
8.85049129520029));
#401443=CARTESIAN_POINT('',(-1.59077126558566,-2.14158464790052,7.59394543036555));
#401444=CARTESIAN_POINT('',(-1.59077126558566,-2.14158464790052,7.5));
#401445=CARTESIAN_POINT('',(-1.60293438610525,-2.2262302592164,7.51860402984325));
#401446=CARTESIAN_POINT('Ctrl Pts',(-1.59077126558566,-2.14158464790052,
7.59394543036555));
#401447=CARTESIAN_POINT('Ctrl Pts',(-1.59326099139908,-2.15891115248839,
7.57858609112103));
#401448=CARTESIAN_POINT('Ctrl Pts',(-1.59574793122424,-2.1762182688214,
7.56320440326857));
#401449=CARTESIAN_POINT('Ctrl Pts',(-1.59823223107081,-2.19350701301057,
7.54780169004651));
#401450=CARTESIAN_POINT('Ctrl Pts',(-1.59980065570003,-2.20442199665558,
7.53807742314383));
#401451=CARTESIAN_POINT('Ctrl Pts',(-1.60136802933076,-2.21532966618995,
7.52834476460825));
#401452=CARTESIAN_POINT('Ctrl Pts',(-1.60293438610525,-2.2262302592164,
7.51860402984325));
#401453=CARTESIAN_POINT('',(-1.60293438610525,-2.2262302592164,7.5));
#401454=CARTESIAN_POINT('Origin',(-1.59757636816867,-2.14060679114482,7.5));
#401455=CARTESIAN_POINT('Ctrl Pts',(-1.59077126558566,-2.14158464790052,
8.85049129520029));
#401456=CARTESIAN_POINT('Ctrl Pts',(-1.59074372039121,-2.14139295533119,
8.85097269580138));
#401457=CARTESIAN_POINT('Ctrl Pts',(-1.59072484862487,-2.14120248493199,
8.85143669361005));
#401458=CARTESIAN_POINT('Ctrl Pts',(-1.59071465132837,-2.14100437995467,
8.8519052845931));
#401459=CARTESIAN_POINT('Ctrl Pts',(-1.59069470606311,-2.14061689918241,
8.85282181883899));
#401460=CARTESIAN_POINT('Ctrl Pts',(-1.59070865627738,-2.1402101685317,
8.85372622499635));
#401461=CARTESIAN_POINT('Ctrl Pts',(-1.59077213055142,-2.13977833422801,
8.85462257735071));
#401462=CARTESIAN_POINT('Ctrl Pts',(-1.59082482463934,-2.13941984072639,
8.85536669723986));
#401463=CARTESIAN_POINT('Ctrl Pts',(-1.59091163012186,-2.13904396012349,
8.85610498449051));
#401464=CARTESIAN_POINT('Ctrl Pts',(-1.59104929334134,-2.13864911207127,
8.85681338218371));
#401465=CARTESIAN_POINT('Ctrl Pts',(-1.59117422292922,-2.13829078684376,
8.85745625420285));
#401466=CARTESIAN_POINT('Ctrl Pts',(-1.591342038854,-2.13791214894837,8.85808743050666));
#401467=CARTESIAN_POINT('Ctrl Pts',(-1.59158132695244,-2.13751236406794,
8.85866804508411));
#401468=CARTESIAN_POINT('Ctrl Pts',(-1.59169172929393,-2.1373279119904,
8.85893592806396));
#401469=CARTESIAN_POINT('Ctrl Pts',(-1.5918175872902,-2.13713898024247,
8.85919241173849));
#401470=CARTESIAN_POINT('Ctrl Pts',(-1.591963262365,-2.13694585159527,8.85943017985534));
#401471=CARTESIAN_POINT('Ctrl Pts',(-1.59215996684041,-2.13668507074933,
8.8597512372));
#401472=CARTESIAN_POINT('Ctrl Pts',(-1.59239832181035,-2.13641038588145,
8.86004599534706));
#401473=CARTESIAN_POINT('Ctrl Pts',(-1.59268332992239,-2.13613192320859,
8.86026130871721));
#401474=CARTESIAN_POINT('Ctrl Pts',(-1.59278767942744,-2.13602997017336,
8.86034014101235));
#401475=CARTESIAN_POINT('Ctrl Pts',(-1.59289984160947,-2.13592597046244,
8.86040910639692));
#401476=CARTESIAN_POINT('Ctrl Pts',(-1.59301698938381,-2.13582300415109,
8.86046313645506));
#401477=CARTESIAN_POINT('Ctrl Pts',(-1.59319979750456,-2.13566232608457,
8.86054744990829));
#401478=CARTESIAN_POINT('Ctrl Pts',(-1.59339983339585,-2.13549988890017,
8.86059655985669));
#401479=CARTESIAN_POINT('Ctrl Pts',(-1.59360408347319,-2.13534588276952,
8.86059725258816));
#401480=CARTESIAN_POINT('Ctrl Pts',(-1.59380880544979,-2.13519152082318,
8.86059794692011));
#401481=CARTESIAN_POINT('Ctrl Pts',(-1.59402163099506,-2.13504603837139,
8.86056369958366));
#401482=CARTESIAN_POINT('Ctrl Pts',(-1.59422882888188,-2.13491426346684,
8.86048590497774));
#401483=CARTESIAN_POINT('Ctrl Pts',(-1.59428290136132,-2.13487987414016,
8.86046560290182));
#401484=CARTESIAN_POINT('Ctrl Pts',(-1.59433734262766,-2.1348460474178,
8.86044257503091));
#401485=CARTESIAN_POINT('Ctrl Pts',(-1.59439045307624,-2.1348138006912,
8.86041778462583));
#401486=CARTESIAN_POINT('Ctrl Pts',(-1.59474782049063,-2.13459682023608,
8.86025097596201));
#401487=CARTESIAN_POINT('Ctrl Pts',(-1.59509305974973,-2.13442254377125,
8.8599848982295));
#401488=CARTESIAN_POINT('Ctrl Pts',(-1.59541227620413,-2.13428849451921,
8.85968173251462));
#401489=CARTESIAN_POINT('Ctrl Pts',(-1.59558112341958,-2.13421759014499,
8.85952137522077));
#401490=CARTESIAN_POINT('Ctrl Pts',(-1.59574587068148,-2.13415639775678,
8.85934740853961));
#401491=CARTESIAN_POINT('Ctrl Pts',(-1.59590365341084,-2.13410432302752,
8.8591675900182));
#401492=CARTESIAN_POINT('Ctrl Pts',(-1.59653723308305,-2.13389521592164,
8.85844552518695));
#401493=CARTESIAN_POINT('Ctrl Pts',(-1.59709337395832,-2.13381843388799,
8.85759444184124));
#401494=CARTESIAN_POINT('Ctrl Pts',(-1.59755244447825,-2.13379655894233,
8.85683498915138));
#401495=CARTESIAN_POINT('Ctrl Pts',(-1.59760048498555,-2.13379426978752,
8.85675551444998));
#401496=CARTESIAN_POINT('Ctrl Pts',(-1.59764745949611,-2.1337926016699,
8.85667699793651));
#401497=CARTESIAN_POINT('Ctrl Pts',(-1.59769334288919,-2.133791478738,8.85659965593547));
#401498=CARTESIAN_POINT('Ctrl Pts',(-1.59831267927036,-2.13377632134594,
8.85555568965886));
#401499=CARTESIAN_POINT('Ctrl Pts',(-1.59891008893109,-2.13385119858145,
8.85434650606346));
#401500=CARTESIAN_POINT('Ctrl Pts',(-1.59948929801393,-2.13401031410438,
8.85297329937117));
#401501=CARTESIAN_POINT('Ctrl Pts',(-1.59981506783129,-2.13409980689098,
8.85220095427747));
#401502=CARTESIAN_POINT('Ctrl Pts',(-1.60013512974126,-2.13421628782883,
8.85137579139183));
#401503=CARTESIAN_POINT('Ctrl Pts',(-1.60045004741996,-2.13436118528464,
8.85049129520029));
#401504=CARTESIAN_POINT('Origin',(-1.59757636816867,-2.14060679114482,7.59394543036555));
#401505=CARTESIAN_POINT('Ctrl Pts',(-1.59069129259387,-2.14102809970488,
7.59443877723642));
#401506=CARTESIAN_POINT('Ctrl Pts',(-1.58986764772642,-2.13529618878608,
7.58783886950016));
#401507=CARTESIAN_POINT('Ctrl Pts',(-1.59776381228678,-2.13217693137887,
7.58559994247159));
#401508=CARTESIAN_POINT('Ctrl Pts',(-1.5951875457606,-2.17231843324347,
7.56670252222137));
#401509=CARTESIAN_POINT('Ctrl Pts',(-1.59436509129382,-2.16659480656329,
7.56004874999029));
#401510=CARTESIAN_POINT('Ctrl Pts',(-1.60230019353943,-2.16343719518632,
7.55786368756705));
#401511=CARTESIAN_POINT('Ctrl Pts',(-1.59967540262376,-2.20355033521046,
7.53888913333558));
#401512=CARTESIAN_POINT('Ctrl Pts',(-1.59884806026982,-2.19779269273666,
7.53222002137279));
#401513=CARTESIAN_POINT('Ctrl Pts',(-1.60682710998053,-2.19464035861195,
7.53005029815326));
#401514=CARTESIAN_POINT('Ctrl Pts',(-1.6041546601048,-2.23472239234115,
7.51101258149734));
#401515=CARTESIAN_POINT('Ctrl Pts',(-1.6033172888582,-2.22889495677867,
7.5043616886572));
#401516=CARTESIAN_POINT('Ctrl Pts',(-1.61134441973222,-2.22578486811819,
7.50217374673251));
#401517=CARTESIAN_POINT('',(-1.6111033692641,-2.22412295723131,7.50366116523517));
#401518=CARTESIAN_POINT('Ctrl Pts',(-1.60293438610525,-2.2262302592164,
7.51860402984325));
#401519=CARTESIAN_POINT('Ctrl Pts',(-1.6029971981068,-2.22666738061629,
7.51734760759494));
#401520=CARTESIAN_POINT('Ctrl Pts',(-1.60311284964108,-2.2270539198544,
7.51608817408573));
#401521=CARTESIAN_POINT('Ctrl Pts',(-1.60329386799927,-2.22738516015517,
7.51481005913121));
#401522=CARTESIAN_POINT('Ctrl Pts',(-1.60345783875369,-2.22768520553485,
7.51365231206384));
#401523=CARTESIAN_POINT('Ctrl Pts',(-1.60367545569763,-2.22794042010745,
7.51247773061043));
#401524=CARTESIAN_POINT('Ctrl Pts',(-1.60397105069097,-2.22812242957886,
7.51129758471022));
#401525=CARTESIAN_POINT('Ctrl Pts',(-1.60433844150947,-2.22834864656557,
7.50983079813401));
#401526=CARTESIAN_POINT('Ctrl Pts',(-1.60482139396921,-2.2284434684628,
7.50839324291155));
#401527=CARTESIAN_POINT('Ctrl Pts',(-1.60543931562123,-2.22832669216941,
7.50715379678855));
#401528=CARTESIAN_POINT('Ctrl Pts',(-1.60572477761947,-2.2282727448867,
7.50658120839351));
#401529=CARTESIAN_POINT('Ctrl Pts',(-1.60607786096985,-2.22815663331509,
7.50598221009429));
#401530=CARTESIAN_POINT('Ctrl Pts',(-1.60648305695654,-2.22795951264466,
7.50545747549611));
#401531=CARTESIAN_POINT('Ctrl Pts',(-1.60669928207703,-2.22785432295346,
7.50517746087247));
#401532=CARTESIAN_POINT('Ctrl Pts',(-1.60693278013442,-2.22772510641312,
7.50491486231392));
#401533=CARTESIAN_POINT('Ctrl Pts',(-1.60717656005761,-2.22757382544985,
7.50468370960992));
#401534=CARTESIAN_POINT('Ctrl Pts',(-1.60754108793879,-2.22734761269087,
7.50433806340446));
#401535=CARTESIAN_POINT('Ctrl Pts',(-1.60793924302547,-2.22706480831741,
7.50405484070983));
#401536=CARTESIAN_POINT('Ctrl Pts',(-1.60834379546466,-2.22674387462097,
7.50385766036131));
#401537=CARTESIAN_POINT('Ctrl Pts',(-1.60838705605987,-2.22670955575058,
7.50383657498791));
#401538=CARTESIAN_POINT('Ctrl Pts',(-1.60843037964076,-2.22667482734914,
7.50381643264937));
#401539=CARTESIAN_POINT('Ctrl Pts',(-1.60847372582378,-2.22663973134263,
7.50379723213559));
#401540=CARTESIAN_POINT('Ctrl Pts',(-1.60876307577496,-2.22640545401846,
7.50366906242519));
#401541=CARTESIAN_POINT('Ctrl Pts',(-1.60905927443569,-2.22614914130103,
7.50358235568538));
#401542=CARTESIAN_POINT('Ctrl Pts',(-1.60933883482303,-2.22589522457715,
7.5035341175365));
#401543=CARTESIAN_POINT('Ctrl Pts',(-1.60975800398372,-2.22551450518751,
7.50346178989176));
#401544=CARTESIAN_POINT('Ctrl Pts',(-1.61019274686616,-2.22508711517259,
7.50346967198527));
#401545=CARTESIAN_POINT('Ctrl Pts',(-1.61060661966909,-2.22465441847368,
7.50354272648692));
#401546=CARTESIAN_POINT('Ctrl Pts',(-1.61077685411959,-2.22447644136512,
7.50357277531559));
#401547=CARTESIAN_POINT('Ctrl Pts',(-1.61094343395556,-2.22429790093189,
7.50361331098761));
#401548=CARTESIAN_POINT('Ctrl Pts',(-1.61110336926493,-2.22412295723246,
7.50366116523659));
#401549=CARTESIAN_POINT('',(-1.59932759105303,-2.14295327026985,7.57603338622103));
#401550=CARTESIAN_POINT('Origin',(-1.60461534358153,-2.15003360661828,7.58486873427627));
#401551=CARTESIAN_POINT('Ctrl Pts',(-1.61110336926699,-2.22412295728858,
7.50366116529968));
#401552=CARTESIAN_POINT('Ctrl Pts',(-1.6071853422593,-2.19711042569364,
7.52783573079709));
#401553=CARTESIAN_POINT('Ctrl Pts',(-1.6032602859228,-2.17005513827966,
7.55196141284069));
#401554=CARTESIAN_POINT('Ctrl Pts',(-1.5993275908755,-2.14295327150926,
7.57603338728831));
#401555=CARTESIAN_POINT('Ctrl Pts',(-1.59109156879725,-2.14257759370614,
7.59639677331371));
#401556=CARTESIAN_POINT('Ctrl Pts',(-1.58540951459622,-2.12430431578109,
7.59974925422226));
#401557=CARTESIAN_POINT('Ctrl Pts',(-1.60131081754378,-2.1349507701505,
7.59639677331372));
#401558=CARTESIAN_POINT('Ctrl Pts',(-1.58934971238339,-2.1390874589928,
7.58707626057422));
#401559=CARTESIAN_POINT('Ctrl Pts',(-1.5915727261035,-2.13256245772062,
7.58811717123965));
#401560=CARTESIAN_POINT('Ctrl Pts',(-1.598460543793,-2.13228786879498,7.58707626057424));
#401561=CARTESIAN_POINT('Ctrl Pts',(-1.59513737061506,-2.14093911891165,
7.58015376756929));
#401562=CARTESIAN_POINT('Ctrl Pts',(-1.59570649628635,-2.13810133317125,
7.58208760766041));
#401563=CARTESIAN_POINT('Ctrl Pts',(-1.59858892220314,-2.13836315901398,
7.5801537675693));
#401564=CARTESIAN_POINT('Ctrl Pts',(-1.59932759055789,-2.14295326960675,
7.57603338509286));
#401565=CARTESIAN_POINT('Ctrl Pts',(-1.59932759055789,-2.14295326960675,
7.57603338509286));
#401566=CARTESIAN_POINT('Ctrl Pts',(-1.59932759055789,-2.14295326960675,
7.57603338509286));
#401567=CARTESIAN_POINT('Origin',(-1.60461077043282,-2.15003701964728,7.58486873427622));
#401568=CARTESIAN_POINT('Ctrl Pts',(-1.68595489728115,-2.173703007108,7.51098857897448));
#401569=CARTESIAN_POINT('Ctrl Pts',(-1.68060655297096,-2.17124216881352,
7.50433767179956));
#401570=CARTESIAN_POINT('Ctrl Pts',(-1.67534106310677,-2.17805265099708,
7.50214974420965));
#401571=CARTESIAN_POINT('Ctrl Pts',(-1.65733749178295,-2.16053579062864,
7.53887321589163));
#401572=CARTESIAN_POINT('Ctrl Pts',(-1.65205323012919,-2.15810443754416,
7.5322040745206));
#401573=CARTESIAN_POINT('Ctrl Pts',(-1.64676090348176,-2.16485678517878,
7.53003438070911));
#401574=CARTESIAN_POINT('Ctrl Pts',(-1.62866513030972,-2.14734328823649,
7.56669465659233));
#401575=CARTESIAN_POINT('Ctrl Pts',(-1.6234120976599,-2.14492630399672,
7.56004085833299));
#401576=CARTESIAN_POINT('Ctrl Pts',(-1.61812721696367,-2.15163500626709,
7.55785582193789));
#401577=CARTESIAN_POINT('Ctrl Pts',(-1.59993910959754,-2.13412609657558,
7.59443891967696));
#401578=CARTESIAN_POINT('Ctrl Pts',(-1.5946784607044,-2.13170560800955,
7.58783901202978));
#401579=CARTESIAN_POINT('Ctrl Pts',(-1.58944145230864,-2.13838789212884,
7.58560008491213));
#401580=CARTESIAN_POINT('',(-1.67379182682863,-2.17733734542426,7.50366116523517));
#401581=CARTESIAN_POINT('Ctrl Pts',(-1.67379182682885,-2.17733734542456,
7.50366116523554));
#401582=CARTESIAN_POINT('Ctrl Pts',(-1.67447334484408,-2.1770061797384,
7.50350835821027));
#401583=CARTESIAN_POINT('Ctrl Pts',(-1.67508905117999,-2.17667958561864,
7.50345484956));
#401584=CARTESIAN_POINT('Ctrl Pts',(-1.6756575326789,-2.17634838364737,
7.50349758195598));
#401585=CARTESIAN_POINT('Ctrl Pts',(-1.67594920584753,-2.17617845247352,
7.50351950684424));
#401586=CARTESIAN_POINT('Ctrl Pts',(-1.6762572609532,-2.17599067105215,
7.50357029184312));
#401587=CARTESIAN_POINT('Ctrl Pts',(-1.67654933754676,-2.17580143016232,
7.50365515313923));
#401588=CARTESIAN_POINT('Ctrl Pts',(-1.67699866962114,-2.17551030104256,
7.50378570417639));
#401589=CARTESIAN_POINT('Ctrl Pts',(-1.6774235639605,-2.17520746333165,
7.50400001621911));
#401590=CARTESIAN_POINT('Ctrl Pts',(-1.67779036218066,-2.17491411851065,
7.50428903009635));
#401591=CARTESIAN_POINT('Ctrl Pts',(-1.67783107396112,-2.17488155949238,
7.50432110841318));
#401592=CARTESIAN_POINT('Ctrl Pts',(-1.67787110027762,-2.17484911527091,
7.50435406373354));
#401593=CARTESIAN_POINT('Ctrl Pts',(-1.67791041740552,-2.17481681294646,
7.50438785222352));
#401594=CARTESIAN_POINT('Ctrl Pts',(-1.67815046736962,-2.17461959172922,
7.50459414719561));
#401595=CARTESIAN_POINT('Ctrl Pts',(-1.67836757542204,-2.17442412152686,
7.50483629897752));
#401596=CARTESIAN_POINT('Ctrl Pts',(-1.67855430477747,-2.17423886878031,
7.5050991045531));
#401597=CARTESIAN_POINT('Ctrl Pts',(-1.67896624849071,-2.17383018261455,
7.50567888004914));
#401598=CARTESIAN_POINT('Ctrl Pts',(-1.67924694212404,-2.17345548835241,
7.50637912803144));
#401599=CARTESIAN_POINT('Ctrl Pts',(-1.67942510411654,-2.17312621707482,
7.50710440483569));
#401600=CARTESIAN_POINT('Ctrl Pts',(-1.67946879297412,-2.17304547322061,
7.50728225710685));
#401601=CARTESIAN_POINT('Ctrl Pts',(-1.67950731439499,-2.17296592286682,
7.50746498566954));
#401602=CARTESIAN_POINT('Ctrl Pts',(-1.67954014411056,-2.17288960453983,
7.50764697238949));
#401603=CARTESIAN_POINT('Ctrl Pts',(-1.67971662762648,-2.1724793382173,
7.50862528291182));
#401604=CARTESIAN_POINT('Ctrl Pts',(-1.67974845277418,-2.17212686491309,
7.50965856837423));
#401605=CARTESIAN_POINT('Ctrl Pts',(-1.67970082222061,-2.171820184291,7.51067959873204));
#401606=CARTESIAN_POINT('Ctrl Pts',(-1.6796746110669,-2.17165141755785,
7.5112414730258));
#401607=CARTESIAN_POINT('Ctrl Pts',(-1.67962390256754,-2.17149654377221,
7.51180065547253));
#401608=CARTESIAN_POINT('Ctrl Pts',(-1.67955689582721,-2.17135407760659,
7.51235175716501));
#401609=CARTESIAN_POINT('Ctrl Pts',(-1.67932536084707,-2.17086180025258,
7.51425603304536));
#401610=CARTESIAN_POINT('Ctrl Pts',(-1.6788661344512,-2.17046155339749,
7.5162690050518));
#401611=CARTESIAN_POINT('Ctrl Pts',(-1.67823955795078,-2.17015459940591,
7.51827788969243));
#401612=CARTESIAN_POINT('Ctrl Pts',(-1.67820564644651,-2.17013798647583,
7.51838661432545));
#401613=CARTESIAN_POINT('Ctrl Pts',(-1.67817123513467,-2.17012164944469,
7.51849533314856));
#401614=CARTESIAN_POINT('Ctrl Pts',(-1.67813633056179,-2.170105589426,7.51860402984325));
#401615=CARTESIAN_POINT('Ctrl Pts',(-1.59932759229263,-2.14295327045312,
7.57603338728985));
#401616=CARTESIAN_POINT('Ctrl Pts',(-1.62419032049749,-2.15443464751878,
7.55196141284921));
#401617=CARTESIAN_POINT('Ctrl Pts',(-1.64901056800952,-2.16589544849306,
7.52783573083104));
#401618=CARTESIAN_POINT('Ctrl Pts',(-1.67379182688441,-2.17733734544403,
7.50366116530176));
#401619=CARTESIAN_POINT('Origin',(-5.52641612598457E-16,-7.40489414195304E-16,
7.49482233047033));
#401620=CARTESIAN_POINT('Origin',(-1.6059181837037,-2.21696482544262,7.49482233047033));
#401621=CARTESIAN_POINT('Origin',(0.,0.,7.50366116523517));
#401622=CARTESIAN_POINT('Origin',(-1.66840488432875,-2.17032978875285,7.49482233047033));
#401623=CARTESIAN_POINT('Ctrl Pts',(-1.60293423561748,-2.22622921225624,
7.51860402984325));
#401624=CARTESIAN_POINT('Ctrl Pts',(-1.60401712365773,-2.23376072203332,
7.51860402984325));
#401625=CARTESIAN_POINT('Ctrl Pts',(-1.5978243100911,-2.23818173392643,
7.51860402984325));
#401626=CARTESIAN_POINT('Ctrl Pts',(-1.60333631807904,-2.22902571341501,
7.51041458714365));
#401627=CARTESIAN_POINT('Ctrl Pts',(-1.60254996944053,-2.23480810233128,
7.5100464290044));
#401628=CARTESIAN_POINT('Ctrl Pts',(-1.59782260218664,-2.23818295318902,
7.50729136483009));
#401629=CARTESIAN_POINT('Ctrl Pts',(-1.60608974108081,-2.22961086209062,
7.50215815450138));
#401630=CARTESIAN_POINT('Ctrl Pts',(-1.60553732340035,-2.2326756458004,
7.49877163671532));
#401631=CARTESIAN_POINT('Ctrl Pts',(-1.60274318276032,-2.23469967684713,
7.49481588533172));
#401632=CARTESIAN_POINT('Ctrl Pts',(-1.61110304631036,-2.22412251139392,
7.50366171572174));
#401633=CARTESIAN_POINT('Ctrl Pts',(-1.61325114344695,-2.22708795249921,
7.50000045605858));
#401634=CARTESIAN_POINT('Ctrl Pts',(-1.61325114344685,-2.22708795249928,
7.49482233047317));
#401635=CARTESIAN_POINT('Origin',(-1.59056147231796,-2.2280081805904,7.51860402984325));
#401636=CARTESIAN_POINT('Origin',(-1.59056147231796,-2.2280081805904,9.));
#401637=CARTESIAN_POINT('Origin',(-1.59056147231796,-2.2280081805904,8.75721825406948));
#401638=CARTESIAN_POINT('Ctrl Pts',(-1.60055903033135,-2.20969989122327,
8.78942910404913));
#401639=CARTESIAN_POINT('Ctrl Pts',(-1.60137162134954,-2.21521279649535,
8.79672699501692));
#401640=CARTESIAN_POINT('Ctrl Pts',(-1.59293023317501,-2.21811390863887,
8.79893251111267));
#401641=CARTESIAN_POINT('Ctrl Pts',(-1.6021227999773,-2.22058244805677,
8.78111911759578));
#401642=CARTESIAN_POINT('Ctrl Pts',(-1.60307877177671,-2.22711914661524,
8.7864446589481));
#401643=CARTESIAN_POINT('Ctrl Pts',(-1.59615583745414,-2.23133678720458,
8.78817647674132));
#401644=CARTESIAN_POINT('Ctrl Pts',(-1.60309737848858,-2.22736471705345,
8.76780923932033));
#401645=CARTESIAN_POINT('Ctrl Pts',(-1.60422082067881,-2.23508175109612,
8.76988516158376));
#401646=CARTESIAN_POINT('Ctrl Pts',(-1.59815964019984,-2.23959821781224,
8.77093053738833));
#401647=CARTESIAN_POINT('Ctrl Pts',(-1.60290734901521,-2.22604226742122,
8.75371302330491));
#401648=CARTESIAN_POINT('Ctrl Pts',(-1.60400397276686,-2.23356979143083,
8.75300828287559));
#401649=CARTESIAN_POINT('Ctrl Pts',(-1.59776837262215,-2.23798701116384,
8.75267964240738));
#401650=CARTESIAN_POINT('Origin',(-1.58856698858099,-2.21412816559725,8.78727029226991));
#401651=CARTESIAN_POINT('Ctrl Pts',(-1.59077126558566,-2.14158464790052,
8.85049129520029));
#401652=CARTESIAN_POINT('Ctrl Pts',(-1.59160185579969,-2.14736489288836,
8.85711686593484));
#401653=CARTESIAN_POINT('Ctrl Pts',(-1.58363955683346,-2.15047978570934,
8.85933012996512));
#401654=CARTESIAN_POINT('Ctrl Pts',(-1.59416574276816,-2.16520749992665,
8.82945683644722));
#401655=CARTESIAN_POINT('Ctrl Pts',(-1.59500322738315,-2.17103572444268,
8.83607469902388));
#401656=CARTESIAN_POINT('Ctrl Pts',(-1.58700388846102,-2.17412483747175,
8.8382956714852));
#401657=CARTESIAN_POINT('Ctrl Pts',(-1.59755516020868,-2.18879514018687,
8.80838214965003));
#401658=CARTESIAN_POINT('Ctrl Pts',(-1.59839594992901,-2.19464636559806,
8.81501364461995));
#401659=CARTESIAN_POINT('Ctrl Pts',(-1.59036377844286,-2.19773392674116,
8.81722098428721));
#401660=CARTESIAN_POINT('Ctrl Pts',(-1.60093990236828,-2.21235024422326,
8.78727029226991));
#401661=CARTESIAN_POINT('Ctrl Pts',(-1.60178083174652,-2.21820244154215,
8.79393457792714));
#401662=CARTESIAN_POINT('Ctrl Pts',(-1.59371958050514,-2.2213097946926,
8.79610912703474));
#401663=CARTESIAN_POINT('Origin',(-1.57839835179836,-2.14336256927451,8.85049129520029));
#401664=CARTESIAN_POINT('Ctrl Pts',(-1.60045004741996,-2.13436118528464,
8.85049129520029));
#401665=CARTESIAN_POINT('Ctrl Pts',(-1.6057550566434,-2.1368020845784,8.85711686593484));
#401666=CARTESIAN_POINT('Ctrl Pts',(-1.61100669796542,-2.13005515746017,
8.85933012996512));
#401667=CARTESIAN_POINT('Ctrl Pts',(-1.5957567823386,-2.1322017569142,8.86332496987232));
#401668=CARTESIAN_POINT('Ctrl Pts',(-1.59962188022982,-2.12966938398194,
8.86648636486737));
#401669=CARTESIAN_POINT('Ctrl Pts',(-1.59786993626268,-2.12402963272601,
8.87206031107457));
#401670=CARTESIAN_POINT('Ctrl Pts',(-1.59003146113943,-2.1364361993996,
8.86341338519876));
#401671=CARTESIAN_POINT('Ctrl Pts',(-1.58647494928258,-2.13940683805928,
8.86654584966058));
#401672=CARTESIAN_POINT('Ctrl Pts',(-1.58158264810685,-2.13606176078165,
8.87215952290714));
#401673=CARTESIAN_POINT('Ctrl Pts',(-1.59077126558566,-2.14158464790052,
8.85049129520029));
#401674=CARTESIAN_POINT('Ctrl Pts',(-1.59160185579969,-2.14736489288836,
8.85711686593484));
#401675=CARTESIAN_POINT('Ctrl Pts',(-1.58363955683346,-2.15047978570933,
8.85933012996512));
#401676=CARTESIAN_POINT('Origin',(-1.60567491878593,-2.12300553826612,8.85049129520029));
#401677=CARTESIAN_POINT('Ctrl Pts',(-1.66539749203245,-2.16424429481556,
8.78727029226991));
#401678=CARTESIAN_POINT('Ctrl Pts',(-1.67076853786518,-2.16671557835678,
8.79393457792714));
#401679=CARTESIAN_POINT('Ctrl Pts',(-1.67604110579949,-2.15987164362913,
8.79610912703474));
#401680=CARTESIAN_POINT('Ctrl Pts',(-1.64377902353589,-2.15429737441203,
8.80838214965003));
#401681=CARTESIAN_POINT('Ctrl Pts',(-1.64914917736846,-2.15676824753314,
8.81501364461995));
#401682=CARTESIAN_POINT('Ctrl Pts',(-1.65439449734899,-2.14994655925992,
8.81722098428721));
#401683=CARTESIAN_POINT('Ctrl Pts',(-1.62213069385384,-2.1443367145137,
8.82945683644723));
#401684=CARTESIAN_POINT('Ctrl Pts',(-1.62747973786129,-2.1467978747474,
8.83607469902389));
#401685=CARTESIAN_POINT('Ctrl Pts',(-1.63271720381481,-2.14000810355221,
8.83829567148519));
#401686=CARTESIAN_POINT('Ctrl Pts',(-1.60045004741996,-2.13436118528464,
8.85049129520029));
#401687=CARTESIAN_POINT('Ctrl Pts',(-1.6057550566434,-2.1368020845784,8.85711686593484));
#401688=CARTESIAN_POINT('Ctrl Pts',(-1.61100669796542,-2.13005515746017,
8.85933012996512));
#401689=CARTESIAN_POINT('Origin',(-1.67062236339842,-2.15288864779705,8.78727029226991));
#401690=CARTESIAN_POINT('Ctrl Pts',(-1.67796812831785,-2.17002817722086,
8.75374538247848));
#401691=CARTESIAN_POINT('Ctrl Pts',(-1.68486593258896,-2.1732163859068,
8.75304829418601));
#401692=CARTESIAN_POINT('Ctrl Pts',(-1.69087189191038,-2.16850479426081,
8.75272238421917));
#401693=CARTESIAN_POINT('Ctrl Pts',(-1.6791672696383,-2.17057991720282,
8.7676940844502));
#401694=CARTESIAN_POINT('Ctrl Pts',(-1.68623894281032,-2.17384772893549,
8.7697431809397));
#401695=CARTESIAN_POINT('Ctrl Pts',(-1.69228901876997,-2.16932943963944,
8.7707786988043));
#401696=CARTESIAN_POINT('Ctrl Pts',(-1.67302115432925,-2.1677520123743,
8.78108014887988));
#401697=CARTESIAN_POINT('Ctrl Pts',(-1.67901254883375,-2.17052481406068,
8.78639403366324));
#401698=CARTESIAN_POINT('Ctrl Pts',(-1.68503003222547,-2.16511076110939,
8.78812224174741));
#401699=CARTESIAN_POINT('Ctrl Pts',(-1.66294902812128,-2.16311770059481,
8.78944554828685));
#401700=CARTESIAN_POINT('Ctrl Pts',(-1.66799600222725,-2.16545959512503,
8.79673892988686));
#401701=CARTESIAN_POINT('Ctrl Pts',(-1.67317559700402,-2.15820181638322,
8.79894799272499));
#401702=CARTESIAN_POINT('Origin',(-1.68336120192776,-2.15874994240749,8.75721825406948));
#401703=CARTESIAN_POINT('Origin',(-1.68336120192776,-2.15874994240749,9.));
#401704=CARTESIAN_POINT('Origin',(-1.68336120192776,-2.15874994240749,7.51860402984325));
#401705=CARTESIAN_POINT('Ctrl Pts',(-1.67379134738624,-2.17733672174576,
7.50366195182966));
#401706=CARTESIAN_POINT('Ctrl Pts',(-1.67602317147191,-2.18023997043657,
7.50000065167735));
#401707=CARTESIAN_POINT('Ctrl Pts',(-1.676023171472,-2.1802399704365,7.49482233047108));
#401708=CARTESIAN_POINT('Ctrl Pts',(-1.68048485024188,-2.17408851930009,
7.50215800491337));
#401709=CARTESIAN_POINT('Ctrl Pts',(-1.6835813448413,-2.17442972066326,
7.49877273257265));
#401710=CARTESIAN_POINT('Ctrl Pts',(-1.68631825291818,-2.17232579801055,
7.49481816995647));
#401711=CARTESIAN_POINT('Ctrl Pts',(-1.6806967376156,-2.17128403715842,
7.51043025814042));
#401712=CARTESIAN_POINT('Ctrl Pts',(-1.68646654642247,-2.17217961703705,
7.51006209594514));
#401713=CARTESIAN_POINT('Ctrl Pts',(-1.69104977934849,-2.1686056911693,
7.50731281821699));
#401714=CARTESIAN_POINT('Ctrl Pts',(-1.67813495755924,-2.17010495759023,
7.51860402984325));
#401715=CARTESIAN_POINT('Ctrl Pts',(-1.68504722930857,-2.17328639070347,
7.51860402984324));
#401716=CARTESIAN_POINT('Ctrl Pts',(-1.69104778275849,-2.16860724808058,
7.51860402984325));
#401717=CARTESIAN_POINT('Origin',(0.,0.,7.5));
#401718=CARTESIAN_POINT('Origin',(-1.46041276049032,-2.23251709792629,7.5));
#401719=CARTESIAN_POINT('',(-1.46041276049032,-2.23251709792629,7.59394543036555));
#401720=CARTESIAN_POINT('',(-1.46041276049032,-2.23251709792629,8.85049129520029));
#401721=CARTESIAN_POINT('',(-1.46041276049032,-2.23251709792629,7.5));
#401722=CARTESIAN_POINT('',(-1.52331214621091,-2.26650000646724,8.78727029226991));
#401723=CARTESIAN_POINT('Ctrl Pts',(-1.46041276049032,-2.23251709792629,
8.85049129520029));
#401724=CARTESIAN_POINT('Ctrl Pts',(-1.48140969918006,-2.24386119992282,
8.82945686509571));
#401725=CARTESIAN_POINT('Ctrl Pts',(-1.50237542338152,-2.25518843754002,
8.80838212259896));
#401726=CARTESIAN_POINT('Ctrl Pts',(-1.52331214621091,-2.26650000646724,
8.78727029226991));
#401727=CARTESIAN_POINT('',(-1.5356492769952,-2.27316543860615,8.75721825406948));
#401728=CARTESIAN_POINT('Origin',(-1.49852247476105,-2.25310701859239,8.75937679713122));
#401729=CARTESIAN_POINT('',(-1.5356492769952,-2.27316543860615,7.51860402984325));
#401730=CARTESIAN_POINT('',(-1.5356492769952,-2.27316543860615,7.5));
#401731=CARTESIAN_POINT('Ctrl Pts',(-1.5356492769952,-2.27316543860615,
7.51860402984325));
#401732=CARTESIAN_POINT('Ctrl Pts',(-1.52596037955092,-2.26793077833182,
7.52834476460825));
#401733=CARTESIAN_POINT('Ctrl Pts',(-1.51626519221423,-2.26269271979158,
7.53807742314407));
#401734=CARTESIAN_POINT('Ctrl Pts',(-1.50656350379362,-2.25745114888412,
7.54780169004674));
#401735=CARTESIAN_POINT('Ctrl Pts',(-1.49119655366689,-2.24914878384944,
7.5632044032688));
#401736=CARTESIAN_POINT('Ctrl Pts',(-1.4758132736195,-2.24083759618167,
7.57858609112103));
#401737=CARTESIAN_POINT('Ctrl Pts',(-1.46041276049032,-2.23251709792629,
7.59394543036555));
#401738=CARTESIAN_POINT('Origin',(-1.47188478489785,-2.5132564881766,7.5));
#401739=CARTESIAN_POINT('',(-1.45700592305911,-2.32435658911881,8.75721825406948));
#401740=CARTESIAN_POINT('',(-1.45590483281683,-2.31037730509332,8.78727029226991));
#401741=CARTESIAN_POINT('Origin',(-1.45310985509581,-2.27489266822439,8.75658640621072));
#401742=CARTESIAN_POINT('',(-1.45029105591253,-2.23910559748224,8.85049129520029));
#401743=CARTESIAN_POINT('Ctrl Pts',(-1.45590483281683,-2.31037730509332,
8.78727029226991));
#401744=CARTESIAN_POINT('Ctrl Pts',(-1.45403622806458,-2.28665376676723,
8.80838212259897));
#401745=CARTESIAN_POINT('Ctrl Pts',(-1.45216503493676,-2.2628973667957,
8.82945686509571));
#401746=CARTESIAN_POINT('Ctrl Pts',(-1.45029105591253,-2.23910559748224,
8.85049129520029));
#401747=CARTESIAN_POINT('',(-1.45029105591253,-2.23910559748224,7.59394543036555));
#401748=CARTESIAN_POINT('',(-1.45029105591253,-2.23910559748224,7.5));
#401749=CARTESIAN_POINT('',(-1.45700592305911,-2.32435658911881,7.51860402984325));
#401750=CARTESIAN_POINT('Ctrl Pts',(-1.45029105591253,-2.23910559748224,
7.59394543036555));
#401751=CARTESIAN_POINT('Ctrl Pts',(-1.4516655533568,-2.25655602018874,
7.57858609112103));
#401752=CARTESIAN_POINT('Ctrl Pts',(-1.45303851274667,-2.27398691597673,
7.56320440326857));
#401753=CARTESIAN_POINT('Ctrl Pts',(-1.45441001468938,-2.29139930822442,
7.54780169004651));
#401754=CARTESIAN_POINT('Ctrl Pts',(-1.45527589141876,-2.30239235517593,
7.53807742314383));
#401755=CARTESIAN_POINT('Ctrl Pts',(-1.45614118792573,-2.3133780357067,
7.52834476460825));
#401756=CARTESIAN_POINT('Ctrl Pts',(-1.45700592305911,-2.32435658911881,
7.51860402984325));
#401757=CARTESIAN_POINT('',(-1.45700592305911,-2.32435658911881,7.5));
#401758=CARTESIAN_POINT('Origin',(-1.45714482817989,-2.23856575425761,7.5));
#401759=CARTESIAN_POINT('Ctrl Pts',(-1.45029105591253,-2.23910559748224,
8.85049129520029));
#401760=CARTESIAN_POINT('Ctrl Pts',(-1.45027584909771,-2.23891253393919,
8.85097269580139));
#401761=CARTESIAN_POINT('Ctrl Pts',(-1.45026921958582,-2.23872124576363,
8.85143669361005));
#401762=CARTESIAN_POINT('Ctrl Pts',(-1.45027173587024,-2.23852289447121,
8.8519052845931));
#401763=CARTESIAN_POINT('Ctrl Pts',(-1.45027665756298,-2.23813493192222,
8.852821818839));
#401764=CARTESIAN_POINT('Ctrl Pts',(-1.45031663843731,-2.23772993073654,
8.85372622499636));
#401765=CARTESIAN_POINT('Ctrl Pts',(-1.45040765001548,-2.23730305049344,
8.85462257735071));
#401766=CARTESIAN_POINT('Ctrl Pts',(-1.45048320459525,-2.23694866967697,
8.85536669723987));
#401767=CARTESIAN_POINT('Ctrl Pts',(-1.45059391447951,-2.23657912300745,
8.85610498449051));
#401768=CARTESIAN_POINT('Ctrl Pts',(-1.4507565928567,-2.23619390632566,
8.85681338218371));
#401769=CARTESIAN_POINT('Ctrl Pts',(-1.4509042237395,-2.23584432158194,
8.85745625420285));
#401770=CARTESIAN_POINT('Ctrl Pts',(-1.45109595428171,-2.23547721364192,
8.85808743050666));
#401771=CARTESIAN_POINT('Ctrl Pts',(-1.45136036504233,-2.23509358140352,
8.85866804508411));
#401772=CARTESIAN_POINT('Ctrl Pts',(-1.45148235843555,-2.23491658180486,
8.85893592806396));
#401773=CARTESIAN_POINT('Ctrl Pts',(-1.45162006274172,-2.23473610198698,
8.85919241173849));
#401774=CARTESIAN_POINT('Ctrl Pts',(-1.45177781230636,-2.23455270357738,
8.85943017985534));
#401775=CARTESIAN_POINT('Ctrl Pts',(-1.4519908209175,-2.23430506143267,
8.8597512372));
#401776=CARTESIAN_POINT('Ctrl Pts',(-1.4522462852815,-2.23404621238967,
8.86004599534706));
#401777=CARTESIAN_POINT('Ctrl Pts',(-1.45254854897852,-2.23378658238067,
8.86026130871721));
#401778=CARTESIAN_POINT('Ctrl Pts',(-1.45265921623971,-2.23369152451463,
8.86034014101236));
#401779=CARTESIAN_POINT('Ctrl Pts',(-1.45277781125687,-2.23359492473794,
8.86040910639692));
#401780=CARTESIAN_POINT('Ctrl Pts',(-1.45290131541276,-2.2334996756656,
8.86046313645506));
#401781=CARTESIAN_POINT('Ctrl Pts',(-1.45309404261369,-2.23335104028591,
8.86054744990829));
#401782=CARTESIAN_POINT('Ctrl Pts',(-1.45330407489592,-2.23320175318968,
8.86059655985668));
#401783=CARTESIAN_POINT('Ctrl Pts',(-1.45351777252623,-2.23306114982853,
8.86059725258816));
#401784=CARTESIAN_POINT('Ctrl Pts',(-1.45373196388344,-2.23292022161744,
8.86059794692011));
#401785=CARTESIAN_POINT('Ctrl Pts',(-1.45395367324849,-2.23278867385446,
8.86056369958366));
#401786=CARTESIAN_POINT('Ctrl Pts',(-1.45416888827215,-2.23267044490976,
8.86048590497774));
#401787=CARTESIAN_POINT('Ctrl Pts',(-1.45422505298561,-2.2326395906753,
8.86046560290182));
#401788=CARTESIAN_POINT('Ctrl Pts',(-1.45428154968207,-2.23260932151747,
8.86044257503091));
#401789=CARTESIAN_POINT('Ctrl Pts',(-1.45433661706441,-2.23258054384336,
8.86041778462583));
#401790=CARTESIAN_POINT('Ctrl Pts',(-1.45470715221461,-2.23238690580671,
8.86025097596201));
#401791=CARTESIAN_POINT('Ctrl Pts',(-1.45506284807406,-2.23223510696685,
8.8599848982295));
#401792=CARTESIAN_POINT('Ctrl Pts',(-1.45538999722908,-2.23212178540182,
8.85968173251461));
#401793=CARTESIAN_POINT('Ctrl Pts',(-1.45556304038868,-2.23206184478648,
8.85952137522076));
#401794=CARTESIAN_POINT('Ctrl Pts',(-1.45573136976944,-2.23201133351791,
8.85934740853961));
#401795=CARTESIAN_POINT('Ctrl Pts',(-1.45589216475661,-2.23196947495595,
8.8591675900182));
#401796=CARTESIAN_POINT('Ctrl Pts',(-1.4565378402097,-2.23180139107202,
8.85844552518696));
#401797=CARTESIAN_POINT('Ctrl Pts',(-1.45709775787568,-2.2317603988635,
8.85759444184126));
#401798=CARTESIAN_POINT('Ctrl Pts',(-1.45755728671856,-2.23176798161146,
8.85683498915141));
#401799=CARTESIAN_POINT('Ctrl Pts',(-1.45760537518815,-2.23176877512584,
8.85675551445));
#401800=CARTESIAN_POINT('Ctrl Pts',(-1.45765236006121,-2.23177012010277,
8.85667699793652));
#401801=CARTESIAN_POINT('Ctrl Pts',(-1.45769822112844,-2.23177193923715,
8.85659965593547));
#401802=CARTESIAN_POINT('Ctrl Pts',(-1.45831725615403,-2.23179649400576,
8.85555568965886));
#401803=CARTESIAN_POINT('Ctrl Pts',(-1.45890864097159,-2.23190949356633,
8.85434650606346));
#401804=CARTESIAN_POINT('Ctrl Pts',(-1.45947646544069,-2.23210539222271,
8.85297329937117));
#401805=CARTESIAN_POINT('Ctrl Pts',(-1.4597958321065,-2.23221557328064,
8.85220095427747));
#401806=CARTESIAN_POINT('Ctrl Pts',(-1.46010777345564,-2.23235232133289,
8.85137579139183));
#401807=CARTESIAN_POINT('Ctrl Pts',(-1.46041276049032,-2.23251709792629,
8.85049129520029));
#401808=CARTESIAN_POINT('Origin',(-1.45714482817989,-2.23856575425761,7.59394543036555));
#401809=CARTESIAN_POINT('Ctrl Pts',(-1.45024690539915,-2.23854506888738,
7.59443877723642));
#401810=CARTESIAN_POINT('Ctrl Pts',(-1.44979219759189,-2.23277216368647,
7.58783886950015));
#401811=CARTESIAN_POINT('Ctrl Pts',(-1.45787199014355,-2.23016522412853,
7.58559994247159));
#401812=CARTESIAN_POINT('Ctrl Pts',(-1.45272914197844,-2.27005918900933,
7.56670252222136));
#401813=CARTESIAN_POINT('Ctrl Pts',(-1.45227509135304,-2.26429462729539,
7.56004874999029));
#401814=CARTESIAN_POINT('Ctrl Pts',(-1.46039619893562,-2.26165190731611,
7.55786368756704));
#401815=CARTESIAN_POINT('Ctrl Pts',(-1.45520674322891,-2.30151445966057,
7.53888913333559));
#401816=CARTESIAN_POINT('Ctrl Pts',(-1.45474999415843,-2.29571563887414,
7.53222002137278));
#401817=CARTESIAN_POINT('Ctrl Pts',(-1.4629146207966,-2.29308100102817,
7.53005029815327));
#401818=CARTESIAN_POINT('Ctrl Pts',(-1.45767959703745,-2.33290945746886,
7.51101258149734));
#401819=CARTESIAN_POINT('Ctrl Pts',(-1.45721731133829,-2.32704034443776,
7.5043616886572));
#401820=CARTESIAN_POINT('Ctrl Pts',(-1.46542721367566,-2.3244509458289,
7.50217374673251));
#401821=CARTESIAN_POINT('',(-1.46529313746768,-2.32277700535966,7.50366116523517));
#401822=CARTESIAN_POINT('Ctrl Pts',(-1.45700592305911,-2.32435658911881,
7.51860402984325));
#401823=CARTESIAN_POINT('Ctrl Pts',(-1.45704059954241,-2.32479683678466,
7.51734760759493));
#401824=CARTESIAN_POINT('Ctrl Pts',(-1.45713124780419,-2.32518999165569,
7.51608817408572));
#401825=CARTESIAN_POINT('Ctrl Pts',(-1.45729067160182,-2.32553214927377,
7.51481005913119));
#401826=CARTESIAN_POINT('Ctrl Pts',(-1.45743508148726,-2.32584208382034,
7.51365231206383));
#401827=CARTESIAN_POINT('Ctrl Pts',(-1.45763589966004,-2.32611071679269,
7.51247773061042));
#401828=CARTESIAN_POINT('Ctrl Pts',(-1.45791922593489,-2.32631129114238,
7.51129758471022));
#401829=CARTESIAN_POINT('Ctrl Pts',(-1.45827136813745,-2.32656058215258,
7.50983079813402));
#401830=CARTESIAN_POINT('Ctrl Pts',(-1.45874725305975,-2.32668615209839,
7.50839324291155));
#401831=CARTESIAN_POINT('Ctrl Pts',(-1.45937138700827,-2.3266092061106,
7.50715379678855));
#401832=CARTESIAN_POINT('Ctrl Pts',(-1.4596597189085,-2.32657365928139,
7.50658120839351));
#401833=CARTESIAN_POINT('Ctrl Pts',(-1.4600195161052,-2.32648040840138,
7.50598221009429));
#401834=CARTESIAN_POINT('Ctrl Pts',(-1.46043650913799,-2.32630965373252,
7.50545747549611));
#401835=CARTESIAN_POINT('Ctrl Pts',(-1.46065902952744,-2.32621853375586,
7.50517746087247));
#401836=CARTESIAN_POINT('Ctrl Pts',(-1.46090032677019,-2.32610454297666,
7.50491486231392));
#401837=CARTESIAN_POINT('Ctrl Pts',(-1.46115329842597,-2.32596919186965,
7.50468370960992));
#401838=CARTESIAN_POINT('Ctrl Pts',(-1.46153157084676,-2.32576679927059,
7.50433806340446));
#401839=CARTESIAN_POINT('Ctrl Pts',(-1.46194702721954,-2.32551008583303,
7.50405484070983));
#401840=CARTESIAN_POINT('Ctrl Pts',(-1.46237131075489,-2.32521573129307,
7.5038576603613));
#401841=CARTESIAN_POINT('Ctrl Pts',(-1.46241668128413,-2.32518425465033,
7.50383657498791));
#401842=CARTESIAN_POINT('Ctrl Pts',(-1.46246214090839,-2.32515237335347,
7.50381643264937));
#401843=CARTESIAN_POINT('Ctrl Pts',(-1.46250764664089,-2.32512012665495,
7.50379723213559));
#401844=CARTESIAN_POINT('Ctrl Pts',(-1.46281141229126,-2.32490486939369,
7.50366906242519));
#401845=CARTESIAN_POINT('Ctrl Pts',(-1.46312342439227,-2.32466806081158,
7.50358235568538));
#401846=CARTESIAN_POINT('Ctrl Pts',(-1.46341867889316,-2.32443257728236,
7.5035341175365));
#401847=CARTESIAN_POINT('Ctrl Pts',(-1.4638613796009,-2.32407949638187,
7.50346178989176));
#401848=CARTESIAN_POINT('Ctrl Pts',(-1.46432261222973,-2.32368083855769,
7.50346967198527));
#401849=CARTESIAN_POINT('Ctrl Pts',(-1.46476335765928,-2.32327554780208,
7.50354272648692));
#401850=CARTESIAN_POINT('Ctrl Pts',(-1.46494464537735,-2.32310884332527,
7.50357277531559));
#401851=CARTESIAN_POINT('Ctrl Pts',(-1.46512232208201,-2.32294134252925,
7.50361331098761));
#401852=CARTESIAN_POINT('Ctrl Pts',(-1.46529313746844,-2.32277700536086,
7.50366116523658));
#401853=CARTESIAN_POINT('',(-1.45874211355529,-2.24101961352506,7.57603338622103));
#401854=CARTESIAN_POINT('Origin',(-1.46356536312152,-2.24842419003061,7.58486873427627));
#401855=CARTESIAN_POINT('Ctrl Pts',(-1.4652931374669,-2.322777005417,7.50366116529969));
#401856=CARTESIAN_POINT('Ctrl Pts',(-1.46311385930744,-2.29556894511303,
7.52783573079709));
#401857=CARTESIAN_POINT('Ctrl Pts',(-1.4609303056364,-2.26831776646579,
7.55196141284068));
#401858=CARTESIAN_POINT('Ctrl Pts',(-1.45874211329872,-2.24101961475054,
7.57603338728831));
#401859=CARTESIAN_POINT('Ctrl Pts',(-1.45054708277062,-2.24011702507145,
7.59639677331371));
#401860=CARTESIAN_POINT('Ctrl Pts',(-1.44624938057004,-2.22235184363283,
7.59959882295467));
#401861=CARTESIAN_POINT('Ctrl Pts',(-1.461088648627,-2.2330525415605,7.59642833564546));
#401862=CARTESIAN_POINT('Ctrl Pts',(-1.44903241888642,-2.23652246009058,
7.58707626057422));
#401863=CARTESIAN_POINT('Ctrl Pts',(-1.45162401029285,-2.23026179359102,
7.58809943920599));
#401864=CARTESIAN_POINT('Ctrl Pts',(-1.4583850215227,-2.23031772160695,
7.58710240504252));
#401865=CARTESIAN_POINT('Ctrl Pts',(-1.4546895494952,-2.2387411321116,7.58015376756929));
#401866=CARTESIAN_POINT('Ctrl Pts',(-1.45542815686251,-2.23598727471642,
7.5820588065976));
#401867=CARTESIAN_POINT('Ctrl Pts',(-1.45821623385673,-2.2363793228159,
7.58020924244127));
#401868=CARTESIAN_POINT('Ctrl Pts',(-1.45874211310365,-2.24101961283159,
7.57603338509286));
#401869=CARTESIAN_POINT('Ctrl Pts',(-1.45874211310365,-2.24101961283159,
7.57603338509286));
#401870=CARTESIAN_POINT('Ctrl Pts',(-1.45874211310365,-2.24101961283159,
7.57603338509286));
#401871=CARTESIAN_POINT('Origin',(-1.46356058069554,-2.24842730304479,7.58486873427621));
#401872=CARTESIAN_POINT('Ctrl Pts',(-1.54322129228844,-2.27725640229734,
7.51098857897448));
#401873=CARTESIAN_POINT('Ctrl Pts',(-1.53804160317611,-2.27445795046258,
7.50433767179956));
#401874=CARTESIAN_POINT('Ctrl Pts',(-1.53235058273389,-2.28091707868616,
7.50214974420965));
#401875=CARTESIAN_POINT('Ctrl Pts',(-1.51550631077548,-2.26228271581091,
7.53887321589173));
#401876=CARTESIAN_POINT('Ctrl Pts',(-1.51038868353099,-2.25951779439551,
7.53220407452067));
#401877=CARTESIAN_POINT('Ctrl Pts',(-1.50467460613786,-2.26591718807517,
7.53003438070911));
#401878=CARTESIAN_POINT('Ctrl Pts',(-1.48773810627429,-2.24728027432282,
7.56669465659231));
#401879=CARTESIAN_POINT('Ctrl Pts',(-1.48265072325536,-2.24453169307891,
7.56004085833298));
#401880=CARTESIAN_POINT('Ctrl Pts',(-1.4769468728831,-2.25088800813222,
7.55785582193789));
#401881=CARTESIAN_POINT('Ctrl Pts',(-1.45991793462976,-2.23224975633352,
7.59443891967696));
#401882=CARTESIAN_POINT('Ctrl Pts',(-1.45482317553887,-2.22949718998902,
7.58783901202978));
#401883=CARTESIAN_POINT('Ctrl Pts',(-1.44916879172502,-2.23583020835896,
7.58560008491213));
#401884=CARTESIAN_POINT('',(-1.53085035931324,-2.28010398287622,7.50366116523517));
#401885=CARTESIAN_POINT('Ctrl Pts',(-1.53085035931345,-2.28010398287653,
7.50366116523554));
#401886=CARTESIAN_POINT('Ctrl Pts',(-1.53155169493518,-2.27981716261495,
7.50350835821027));
#401887=CARTESIAN_POINT('Ctrl Pts',(-1.53218706119349,-2.27953068795822,
7.50345484955999));
#401888=CARTESIAN_POINT('Ctrl Pts',(-1.53277559486935,-2.27923658921161,
7.50349758195598));
#401889=CARTESIAN_POINT('Ctrl Pts',(-1.53307755629186,-2.27908569474366,
7.50351950684424));
#401890=CARTESIAN_POINT('Ctrl Pts',(-1.53339700966226,-2.27891803629774,
7.50357029184312));
#401891=CARTESIAN_POINT('Ctrl Pts',(-1.53370061085857,-2.27874789763522,
7.50365515313924));
#401892=CARTESIAN_POINT('Ctrl Pts',(-1.53416767243875,-2.27848615547631,
7.50378570417639));
#401893=CARTESIAN_POINT('Ctrl Pts',(-1.53461109666587,-2.27821116305176,
7.50400001621911));
#401894=CARTESIAN_POINT('Ctrl Pts',(-1.53499593592696,-2.27794192178181,
7.50428903009634));
#401895=CARTESIAN_POINT('Ctrl Pts',(-1.53503865012417,-2.27791203807226,
7.50432110841317));
#401896=CARTESIAN_POINT('Ctrl Pts',(-1.53508067291071,-2.27788222500581,
7.50435406373354));
#401897=CARTESIAN_POINT('Ctrl Pts',(-1.5351219788744,-2.27785250810699,
7.50438785222352));
#401898=CARTESIAN_POINT('Ctrl Pts',(-1.53537417163688,-2.2776710721559,
7.50459414719561));
#401899=CARTESIAN_POINT('Ctrl Pts',(-1.53560335743639,-2.27748991372871,
7.50483629897752));
#401900=CARTESIAN_POINT('Ctrl Pts',(-1.53580157232054,-2.27731700539468,
7.5050991045531));
#401901=CARTESIAN_POINT('Ctrl Pts',(-1.5362388542638,-2.27693555224281,
7.50567888004914));
#401902=CARTESIAN_POINT('Ctrl Pts',(-1.53654297792575,-2.27657961193305,
7.50637912803145));
#401903=CARTESIAN_POINT('Ctrl Pts',(-1.53674187034852,-2.27626243205666,
7.50710440483569));
#401904=CARTESIAN_POINT('Ctrl Pts',(-1.53679064271915,-2.27618465325407,
7.50728225710685));
#401905=CARTESIAN_POINT('Ctrl Pts',(-1.5368341818023,-2.27610773442093,
7.50746498566955));
#401906=CARTESIAN_POINT('Ctrl Pts',(-1.5368718337977,-2.27603367630522,
7.50764697238949));
#401907=CARTESIAN_POINT('Ctrl Pts',(-1.53707424056284,-2.27563556025655,
7.50862528291181));
#401908=CARTESIAN_POINT('Ctrl Pts',(-1.5371285833645,-2.27528585019075,
7.50965856837421));
#401909=CARTESIAN_POINT('Ctrl Pts',(-1.53710069976793,-2.27497674797686,
7.51067959873201));
#401910=CARTESIAN_POINT('Ctrl Pts',(-1.53708535538957,-2.27480664863867,
7.51124147302578));
#401911=CARTESIAN_POINT('Ctrl Pts',(-1.53704467387377,-2.27464884415312,
7.51180065547252));
#401912=CARTESIAN_POINT('Ctrl Pts',(-1.53698693264455,-2.27450237756292,
7.51235175716501));
#401913=CARTESIAN_POINT('Ctrl Pts',(-1.53678741369622,-2.27399627714842,
7.51425603304535));
#401914=CARTESIAN_POINT('Ctrl Pts',(-1.53635477473429,-2.27356742990722,
7.51626900505179));
#401915=CARTESIAN_POINT('Ctrl Pts',(-1.53574915221225,-2.27322096169132,
7.51827788969243));
#401916=CARTESIAN_POINT('Ctrl Pts',(-1.53571637477688,-2.27320221017675,
7.51838661432545));
#401917=CARTESIAN_POINT('Ctrl Pts',(-1.53568308088396,-2.27318370197147,
7.51849533314856));
#401918=CARTESIAN_POINT('Ctrl Pts',(-1.5356492769952,-2.27316543860615,
7.51860402984325));
#401919=CARTESIAN_POINT('Ctrl Pts',(-1.4587421147806,-2.24101961378737,
7.57603338728985));
#401920=CARTESIAN_POINT('Ctrl Pts',(-1.48281814548957,-2.25407036159787,
7.55196141284922));
#401921=CARTESIAN_POINT('Ctrl Pts',(-1.50685310110155,-2.26709785384546,
7.52783573083104));
#401922=CARTESIAN_POINT('Ctrl Pts',(-1.53085035936764,-2.28010398289952,
7.50366116530176));
#401923=CARTESIAN_POINT('Origin',(-5.04062831473864E-16,-7.74375868966278E-16,
7.49482233047033));
#401924=CARTESIAN_POINT('Origin',(-1.46057722850548,-2.31530136474094,7.49482233047033));
#401925=CARTESIAN_POINT('Origin',(0.,0.,7.50366116523517));
#401926=CARTESIAN_POINT('Origin',(-1.52592346056194,-2.27276568139056,7.49482233047033));
#401927=CARTESIAN_POINT('Ctrl Pts',(-1.4570058399595,-2.32435553466795,
7.51860402984325));
#401928=CARTESIAN_POINT('Ctrl Pts',(-1.45760395760193,-2.3319409510254,
7.51860402984325));
#401929=CARTESIAN_POINT('Ctrl Pts',(-1.45114061263041,-2.33595610454791,
7.51860402984325));
#401930=CARTESIAN_POINT('Ctrl Pts',(-1.4572279238551,-2.32717205162693,
7.51041458714366));
#401931=CARTESIAN_POINT('Ctrl Pts',(-1.45607271192434,-2.33289217847475,
7.51004642900444));
#401932=CARTESIAN_POINT('Ctrl Pts',(-1.45113883011662,-2.33595721187957,
7.50729136483011));
#401933=CARTESIAN_POINT('Ctrl Pts',(-1.45993819904965,-2.32793241046926,
7.50215815450137));
#401934=CARTESIAN_POINT('Ctrl Pts',(-1.45919055500407,-2.3309555037299,
7.49877163671527));
#401935=CARTESIAN_POINT('Ctrl Pts',(-1.45627247511124,-2.3327963549823,
7.49481588533168));
#401936=CARTESIAN_POINT('Ctrl Pts',(-1.46529284374239,-2.32277653974657,
7.50366171572174));
#401937=CARTESIAN_POINT('Ctrl Pts',(-1.46724653091907,-2.32587351709115,
7.50000045605858));
#401938=CARTESIAN_POINT('Ctrl Pts',(-1.46724653091897,-2.32587351709122,
7.49482233047317));
#401939=CARTESIAN_POINT('Origin',(-1.44454451893664,-2.32533812225451,7.51860402984325));
#401940=CARTESIAN_POINT('Origin',(-1.44454451893664,-2.32533812225451,9.));
#401941=CARTESIAN_POINT('Origin',(-1.44454451893664,-2.32533812225451,8.75721825406948));
#401942=CARTESIAN_POINT('Ctrl Pts',(-1.45569455202209,-2.30770799497263,
8.78942910404913));
#401943=CARTESIAN_POINT('Ctrl Pts',(-1.45615226043136,-2.31326163627486,
8.79672699501693));
#401944=CARTESIAN_POINT('Ctrl Pts',(-1.44754234110095,-2.31561594617505,
8.79893251111267));
#401945=CARTESIAN_POINT('Ctrl Pts',(-1.45655786092531,-2.31866838349119,
8.78111911759578));
#401946=CARTESIAN_POINT('Ctrl Pts',(-1.45709306086354,-2.32525290102489,
8.78644465894808));
#401947=CARTESIAN_POINT('Ctrl Pts',(-1.44991412529166,-2.32901832209435,
8.78817647674131));
#401948=CARTESIAN_POINT('Ctrl Pts',(-1.45709589559393,-2.32549915904842,
8.76780923932034));
#401949=CARTESIAN_POINT('Ctrl Pts',(-1.45772259748297,-2.33327231680526,
8.76988516158378));
#401950=CARTESIAN_POINT('Ctrl Pts',(-1.45138449933333,-2.33739116278949,
8.77093053738834));
#401951=CARTESIAN_POINT('Ctrl Pts',(-1.45699098619534,-2.32416725130063,
8.75371302330491));
#401952=CARTESIAN_POINT('Ctrl Pts',(-1.45760306669667,-2.33174957012983,
8.75300828287558));
#401953=CARTESIAN_POINT('Ctrl Pts',(-1.45109726602123,-2.33575819793818,
8.75267964240738));
#401954=CARTESIAN_POINT('Origin',(-1.44344342869436,-2.31135883822902,8.78727029226991));
#401955=CARTESIAN_POINT('Ctrl Pts',(-1.45029105591253,-2.23910559748224,
8.85049129520029));
#401956=CARTESIAN_POINT('Ctrl Pts',(-1.45074959802197,-2.24492718243455,
8.85711686593484));
#401957=CARTESIAN_POINT('Ctrl Pts',(-1.44260408658466,-2.24752552912784,
8.85933012996512));
#401958=CARTESIAN_POINT('Ctrl Pts',(-1.45216503745171,-2.26289739872513,
8.82945683644722));
#401959=CARTESIAN_POINT('Ctrl Pts',(-1.4526273857379,-2.26876730635234,
8.83607469902388));
#401960=CARTESIAN_POINT('Ctrl Pts',(-1.44444656216418,-2.27133755306296,
8.83829567148519));
#401961=CARTESIAN_POINT('Ctrl Pts',(-1.45403622567029,-2.28665373636973,
8.80838214965003));
#401962=CARTESIAN_POINT('Ctrl Pts',(-1.4545003985987,-2.29254680939303,
8.81501364461989));
#401963=CARTESIAN_POINT('Ctrl Pts',(-1.44628690934868,-2.29511340381663,
8.81722098428722));
#401964=CARTESIAN_POINT('Ctrl Pts',(-1.45590483281683,-2.31037730509332,
8.78727029226991));
#401965=CARTESIAN_POINT('Ctrl Pts',(-1.45636908284588,-2.31627135697542,
8.79393457792714));
#401966=CARTESIAN_POINT('Ctrl Pts',(-1.44812530550984,-2.31885583959521,
8.79610912703474));
#401967=CARTESIAN_POINT('Origin',(-1.43782965179006,-2.24008713061794,8.85049129520029));
#401968=CARTESIAN_POINT('Ctrl Pts',(-1.46041276049032,-2.23251709792629,
8.85049129520029));
#401969=CARTESIAN_POINT('Ctrl Pts',(-1.46555048104865,-2.23529287523862,
8.85711686593484));
#401970=CARTESIAN_POINT('Ctrl Pts',(-1.471223609415,-2.22889628422052,8.85933012996512));
#401971=CARTESIAN_POINT('Ctrl Pts',(-1.45586749327615,-2.23006140780684,
8.86332496987233));
#401972=CARTESIAN_POINT('Ctrl Pts',(-1.45988689960007,-2.22778187557852,
8.86648636486738));
#401973=CARTESIAN_POINT('Ctrl Pts',(-1.4584998952933,-2.22204146436104,
8.87206031107457));
#401974=CARTESIAN_POINT('Ctrl Pts',(-1.44988263370189,-2.23392032758733,
8.86341338519875));
#401975=CARTESIAN_POINT('Ctrl Pts',(-1.44614309960767,-2.23665699625423,
8.86654584966056));
#401976=CARTESIAN_POINT('Ctrl Pts',(-1.44147517002644,-2.2330053409841,
8.87215952290714));
#401977=CARTESIAN_POINT('Ctrl Pts',(-1.45029105591253,-2.23910559748224,
8.85049129520029));
#401978=CARTESIAN_POINT('Ctrl Pts',(-1.45074959802197,-2.24492718243455,
8.85711686593484));
#401979=CARTESIAN_POINT('Ctrl Pts',(-1.44260408658466,-2.24752552912784,
8.85933012996512));
#401980=CARTESIAN_POINT('Origin',(-1.4663544556002,-2.22151954096026,8.85049129520029));
#401981=CARTESIAN_POINT('Ctrl Pts',(-1.52331214621091,-2.26650000646724,
8.78727029226991));
#401982=CARTESIAN_POINT('Ctrl Pts',(-1.52851382097382,-2.26931033657941,
8.79393457792714));
#401983=CARTESIAN_POINT('Ctrl Pts',(-1.53421404825535,-2.26281827803708,
8.79610912703474));
#401984=CARTESIAN_POINT('Ctrl Pts',(-1.50237539655483,-2.25518842304625,
8.80838214965001));
#401985=CARTESIAN_POINT('Ctrl Pts',(-1.50757620744601,-2.25799828643088,
8.81501364461993));
#401986=CARTESIAN_POINT('Ctrl Pts',(-1.51324781742239,-2.25152668285288,
8.81722098428721));
#401987=CARTESIAN_POINT('Ctrl Pts',(-1.48140972735873,-2.24386121514702,
8.82945683644724));
#401988=CARTESIAN_POINT('Ctrl Pts',(-1.48659009410403,-2.24666003308931,
8.8360746990239));
#401989=CARTESIAN_POINT('Ctrl Pts',(-1.49225182125611,-2.24021977780301,
8.8382956714852));
#401990=CARTESIAN_POINT('Ctrl Pts',(-1.46041276049032,-2.23251709792629,
8.85049129520029));
#401991=CARTESIAN_POINT('Ctrl Pts',(-1.46555048104865,-2.23529287523862,
8.85711686593484));
#401992=CARTESIAN_POINT('Ctrl Pts',(-1.471223609415,-2.22889628422052,8.85933012996512));
#401993=CARTESIAN_POINT('Origin',(-1.52925384132079,-2.2555024495012,8.78727029226991));
#401994=CARTESIAN_POINT('Ctrl Pts',(-1.53548638015782,-2.27307740869792,
8.75374538247847));
#401995=CARTESIAN_POINT('Ctrl Pts',(-1.54216574291842,-2.27670101070421,
8.75304829418601));
#401996=CARTESIAN_POINT('Ctrl Pts',(-1.54846123506549,-2.27238390266349,
8.75272238421917));
#401997=CARTESIAN_POINT('Ctrl Pts',(-1.53664770761178,-2.27370484431909,
8.76769408445023));
#401998=CARTESIAN_POINT('Ctrl Pts',(-1.54349548185628,-2.27741902563785,
8.76974318093971));
#401999=CARTESIAN_POINT('Ctrl Pts',(-1.54982261507514,-2.27329764934939,
8.7707786988043));
#402000=CARTESIAN_POINT('Ctrl Pts',(-1.53069540464028,-2.27048896676447,
8.78108014887986));
#402001=CARTESIAN_POINT('Ctrl Pts',(-1.53649683516817,-2.27363994139627,
8.78639403366322));
#402002=CARTESIAN_POINT('Ctrl Pts',(-1.54284883455847,-2.26862255368208,
8.78812224174741));
#402003=CARTESIAN_POINT('Ctrl Pts',(-1.52094089407099,-2.26521885333373,
8.78944554828685));
#402004=CARTESIAN_POINT('Ctrl Pts',(-1.52582745292966,-2.26787929693168,
8.79673892988687));
#402005=CARTESIAN_POINT('Ctrl Pts',(-1.53146141315401,-2.26096828785145,
8.79894799272499));
#402006=CARTESIAN_POINT('Origin',(-1.54159097210508,-2.26216788164012,8.75721825406948));
#402007=CARTESIAN_POINT('Origin',(-1.54159097210508,-2.26216788164012,9.));
#402008=CARTESIAN_POINT('Origin',(-1.54159097210508,-2.26216788164012,7.51860402984325));
#402009=CARTESIAN_POINT('Ctrl Pts',(-1.53084992081514,-2.28010332976116,
7.50366195182966));
#402010=CARTESIAN_POINT('Ctrl Pts',(-1.53289114759659,-2.28314360687628,
7.50000065167735));
#402011=CARTESIAN_POINT('Ctrl Pts',(-1.53289114759668,-2.28314360687622,
7.49482233047108));
#402012=CARTESIAN_POINT('Ctrl Pts',(-1.53773778419653,-2.27729065529617,
7.50215800491337));
#402013=CARTESIAN_POINT('Ctrl Pts',(-1.54080605586929,-2.27782954871471,
7.49877273257264));
#402014=CARTESIAN_POINT('Ctrl Pts',(-1.54367213946218,-2.27590530309928,
7.49481816995647));
#402015=CARTESIAN_POINT('Ctrl Pts',(-1.53812892001266,-2.27450551093449,
7.51043025814041));
#402016=CARTESIAN_POINT('Ctrl Pts',(-1.54382949412869,-2.2757689236677,
7.51006209594514));
#402017=CARTESIAN_POINT('Ctrl Pts',(-1.54863229252765,-2.27249598955575,
7.50731281821699));
#402018=CARTESIAN_POINT('Ctrl Pts',(-1.53564794729548,-2.27316472009998,
7.51860402984325));
#402019=CARTESIAN_POINT('Ctrl Pts',(-1.54234218192175,-2.27678248738922,
7.51860402984324));
#402020=CARTESIAN_POINT('Ctrl Pts',(-1.54863020028821,-2.27249741534623,
7.51860402984325));
#402021=CARTESIAN_POINT('Origin',(0.,0.,7.5));
#402022=CARTESIAN_POINT('Origin',(-1.31437432427028,-2.32149911893915,7.5));
#402023=CARTESIAN_POINT('',(-1.31437432427028,-2.32149911893915,7.59394543036555));
#402024=CARTESIAN_POINT('',(-1.31437432427028,-2.32149911893915,8.85049129520029));
#402025=CARTESIAN_POINT('',(-1.31437432427028,-2.32149911893915,7.5));
#402026=CARTESIAN_POINT('',(-1.37496718403116,-2.35944218342961,8.78727029226991));
#402027=CARTESIAN_POINT('Ctrl Pts',(-1.31437432427028,-2.32149911893915,
8.85049129520029));
#402028=CARTESIAN_POINT('Ctrl Pts',(-1.33460130338716,-2.33416519174224,
8.82945686509571));
#402029=CARTESIAN_POINT('Ctrl Pts',(-1.35479821265378,-2.34681243489656,
8.80838212259897));
#402030=CARTESIAN_POINT('Ctrl Pts',(-1.37496718403116,-2.35944218342961,
8.78727029226991));
#402031=CARTESIAN_POINT('',(-1.38685191115369,-2.36688436340661,8.75721825406948));
#402032=CARTESIAN_POINT('Origin',(-1.35108653730004,-2.34448843318215,8.75937679713147));
#402033=CARTESIAN_POINT('',(-1.38685191115369,-2.36688436340661,7.51860402984325));
#402034=CARTESIAN_POINT('',(-1.38685191115369,-2.36688436340661,7.5));
#402035=CARTESIAN_POINT('Ctrl Pts',(-1.38685191115369,-2.36688436340661,
7.51860402984325));
#402036=CARTESIAN_POINT('Ctrl Pts',(-1.37751830642364,-2.3610396885126,
7.52834476460825));
#402037=CARTESIAN_POINT('Ctrl Pts',(-1.36817864245209,-2.35519121934,7.53807742314407));
#402038=CARTESIAN_POINT('Ctrl Pts',(-1.35883271579193,-2.34933882849083,
7.54780169004674));
#402039=CARTESIAN_POINT('Ctrl Pts',(-1.34402927306647,-2.34006895768049,
7.5632044032688));
#402040=CARTESIAN_POINT('Ctrl Pts',(-1.32921009923996,-2.33078923610249,
7.57858609112103));
#402041=CARTESIAN_POINT('Ctrl Pts',(-1.31437432427028,-2.32149911893915,
7.59394543036555));
#402042=CARTESIAN_POINT('Origin',(-1.3078357436827,-2.6023967151304,7.5));
#402043=CARTESIAN_POINT('',(-1.30509031014833,-2.4129316392236,8.75721825406948));
#402044=CARTESIAN_POINT('',(-1.30488713801673,-2.39891053004237,8.78727029226991));
#402045=CARTESIAN_POINT('Origin',(-1.30437141136731,-2.36331972532774,8.75658640621058));
#402046=CARTESIAN_POINT('',(-1.30385128920419,-2.32742558187727,8.85049129520029));
#402047=CARTESIAN_POINT('Ctrl Pts',(-1.30488713801673,-2.39891053004237,
8.78727029226991));
#402048=CARTESIAN_POINT('Ctrl Pts',(-1.30454234483262,-2.37511601235258,
8.80838212259897));
#402049=CARTESIAN_POINT('Ctrl Pts',(-1.30419707404389,-2.35128853469734,
8.82945686509571));
#402050=CARTESIAN_POINT('Ctrl Pts',(-1.30385128920419,-2.32742558187727,
8.85049129520029));
#402051=CARTESIAN_POINT('',(-1.30385128920419,-2.32742558187727,7.59394543036555));
#402052=CARTESIAN_POINT('',(-1.30385128920419,-2.32742558187727,7.5));
#402053=CARTESIAN_POINT('',(-1.30509031014833,-2.4129316392236,7.51860402984325));
#402054=CARTESIAN_POINT('Ctrl Pts',(-1.30385128920419,-2.32742558187727,
7.59394543036555));
#402055=CARTESIAN_POINT('Ctrl Pts',(-1.30410491017449,-2.34492821517238,
7.57858609112103));
#402056=CARTESIAN_POINT('Ctrl Pts',(-1.30435824734445,-2.36241126312565,
7.56320440326857));
#402057=CARTESIAN_POINT('Ctrl Pts',(-1.30461131558762,-2.37987575217717,
7.54780169004651));
#402058=CARTESIAN_POINT('Ctrl Pts',(-1.30477108634396,-2.39090168964724,
7.53807742314383));
#402059=CARTESIAN_POINT('Ctrl Pts',(-1.3049307500382,-2.4019202386567,7.52834476460825));
#402060=CARTESIAN_POINT('Ctrl Pts',(-1.30509031014833,-2.4129316392236,
7.51860402984325));
#402061=CARTESIAN_POINT('',(-1.30509031014833,-2.4129316392236,7.5));
#402062=CARTESIAN_POINT('Origin',(-1.31072556753552,-2.32732597051531,7.5));
#402063=CARTESIAN_POINT('Ctrl Pts',(-1.30385128920419,-2.32742558187727,
8.85049129520029));
#402064=CARTESIAN_POINT('Ctrl Pts',(-1.30384848325709,-2.3272319407,8.85097269580138));
#402065=CARTESIAN_POINT('Ctrl Pts',(-1.30385412324172,-2.32704062079223,
8.85143669361005));
#402066=CARTESIAN_POINT('Ctrl Pts',(-1.3038693427671,-2.32684283825271,
8.8519052845931));
#402067=CARTESIAN_POINT('Ctrl Pts',(-1.30389911119356,-2.32645598814832,
8.85282181883899));
#402068=CARTESIAN_POINT('Ctrl Pts',(-1.30396495843795,-2.32605438066443,
8.85372622499636));
#402069=CARTESIAN_POINT('Ctrl Pts',(-1.30408313333415,-2.32563420862441,
8.85462257735071));
#402070=CARTESIAN_POINT('Ctrl Pts',(-1.3041812379358,-2.32528539671988,
8.85536669723986));
#402071=CARTESIAN_POINT('Ctrl Pts',(-1.30431539729114,-2.32492370253026,
8.85610498449051));
#402072=CARTESIAN_POINT('Ctrl Pts',(-1.30450242234571,-2.32454970015687,
8.85681338218371));
#402073=CARTESIAN_POINT('Ctrl Pts',(-1.30467214787645,-2.32421029241564,
8.85745625420284));
#402074=CARTESIAN_POINT('Ctrl Pts',(-1.30488700517417,-2.32385622295628,
8.85808743050665));
#402075=CARTESIAN_POINT('Ctrl Pts',(-1.30517545207643,-2.32349031978706,
8.8586680450841));
#402076=CARTESIAN_POINT('Ctrl Pts',(-1.30530853522436,-2.32332149999658,
8.85893592806395));
#402077=CARTESIAN_POINT('Ctrl Pts',(-1.3054575199839,-2.32315021373903,
8.85919241173848));
#402078=CARTESIAN_POINT('Ctrl Pts',(-1.30562669581159,-2.32297729919044,
8.85943017985534));
#402079=CARTESIAN_POINT('Ctrl Pts',(-1.30585513326038,-2.32274381336165,
8.8597512372));
#402080=CARTESIAN_POINT('Ctrl Pts',(-1.30612665726057,-2.32250186380976,
8.86004599534705));
#402081=CARTESIAN_POINT('Ctrl Pts',(-1.3064449344762,-2.32226213334002,
8.86026130871721));
#402082=CARTESIAN_POINT('Ctrl Pts',(-1.30656146473803,-2.32217436125633,
8.86034014101235));
#402083=CARTESIAN_POINT('Ctrl Pts',(-1.30668600525794,-2.32208555836309,
8.86040910639692));
#402084=CARTESIAN_POINT('Ctrl Pts',(-1.30681535829032,-2.32199841792861,
8.86046313645506));
#402085=CARTESIAN_POINT('Ctrl Pts',(-1.30701721261402,-2.32186243601041,
8.86054744990829));
#402086=CARTESIAN_POINT('Ctrl Pts',(-1.3072363782195,-2.32172691245506,
8.86059655985669));
#402087=CARTESIAN_POINT('Ctrl Pts',(-1.30745864527339,-2.32160028963278,
8.86059725258816));
#402088=CARTESIAN_POINT('Ctrl Pts',(-1.30768142585297,-2.32147337426119,
8.86059794692011));
#402089=CARTESIAN_POINT('Ctrl Pts',(-1.30791110798646,-2.32135630174498,
8.86056369958366));
#402090=CARTESIAN_POINT('Ctrl Pts',(-1.30813345578227,-2.32125210458825,
8.86048590497774));
#402091=CARTESIAN_POINT('Ctrl Pts',(-1.30819148193688,-2.32122491223266,
8.86046560290182));
#402092=CARTESIAN_POINT('Ctrl Pts',(-1.30824980190643,-2.32119832502184,
8.86044257503091));
#402093=CARTESIAN_POINT('Ctrl Pts',(-1.30830659993883,-2.32117313465384,
8.86041778462583));
#402094=CARTESIAN_POINT('Ctrl Pts',(-1.30868878021643,-2.32100363473589,
8.86025097596201));
#402095=CARTESIAN_POINT('Ctrl Pts',(-1.30905347104566,-2.32087493729499,
8.8599848982295));
#402096=CARTESIAN_POINT('Ctrl Pts',(-1.30938720857525,-2.3207828090796,
8.85968173251461));
#402097=CARTESIAN_POINT('Ctrl Pts',(-1.30956373660753,-2.32073407853198,
8.85952137522076));
#402098=CARTESIAN_POINT('Ctrl Pts',(-1.30973495640561,-2.32069445594468,
8.85934740853961));
#402099=CARTESIAN_POINT('Ctrl Pts',(-1.30989810290951,-2.32066298555583,
8.8591675900182));
#402100=CARTESIAN_POINT('Ctrl Pts',(-1.31055322092456,-2.32053661558658,
8.85844552518695));
#402101=CARTESIAN_POINT('Ctrl Pts',(-1.31111461455946,-2.32053158164898,
8.85759444184125));
#402102=CARTESIAN_POINT('Ctrl Pts',(-1.31157271342272,-2.32056859093142,
8.85683498915139));
#402103=CARTESIAN_POINT('Ctrl Pts',(-1.31162065224875,-2.32057246385427,
8.85675551444998));
#402104=CARTESIAN_POINT('Ctrl Pts',(-1.31166745441337,-2.32057681639896,
8.85667699793651));
#402105=CARTESIAN_POINT('Ctrl Pts',(-1.31171310470178,-2.32058157012439,
8.85659965593547));
#402106=CARTESIAN_POINT('Ctrl Pts',(-1.3123292946241,-2.32064573615286,
8.85555568965886));
#402107=CARTESIAN_POINT('Ctrl Pts',(-1.31291222447142,-2.32079639369907,
8.85434650606346));
#402108=CARTESIAN_POINT('Ctrl Pts',(-1.31346633101424,-2.3210282704993,
8.85297329937117));
#402109=CARTESIAN_POINT('Ctrl Pts',(-1.31377798218236,-2.32115868707096,
8.85220095427747));
#402110=CARTESIAN_POINT('Ctrl Pts',(-1.31408052113675,-2.32131514031053,
8.85137579139183));
#402111=CARTESIAN_POINT('Ctrl Pts',(-1.31437432427028,-2.32149911893915,
8.85049129520029));
#402112=CARTESIAN_POINT('Origin',(-1.31072556753552,-2.32732597051531,7.59394543036555));
#402113=CARTESIAN_POINT('Ctrl Pts',(-1.30384314259316,-2.32686337621542,
7.59443877723642));
#402114=CARTESIAN_POINT('Ctrl Pts',(-1.30375924033801,-2.32107319883815,
7.58783886950016));
#402115=CARTESIAN_POINT('Ctrl Pts',(-1.31198945928027,-2.31898928960331,
7.58559994247159));
#402116=CARTESIAN_POINT('Ctrl Pts',(-1.30430116254246,-2.35847178464137,
7.56670252222136));
#402117=CARTESIAN_POINT('Ctrl Pts',(-1.30421738154994,-2.35268997571428,
7.56004874999027));
#402118=CARTESIAN_POINT('Ctrl Pts',(-1.31249112309637,-2.35057300663592,
7.55786368756704));
#402119=CARTESIAN_POINT('Ctrl Pts',(-1.30475832718527,-2.39002116752266,
7.53888913333561));
#402120=CARTESIAN_POINT('Ctrl Pts',(-1.30467404827816,-2.384204997022,7.53222002137279));
#402121=CARTESIAN_POINT('Ctrl Pts',(-1.3129907016416,-2.38209888174683,
7.53005029815327));
#402122=CARTESIAN_POINT('Ctrl Pts',(-1.30521461583457,-2.42151009722832,
7.51101258149734));
#402123=CARTESIAN_POINT('Ctrl Pts',(-1.30512931531396,-2.41562342417297,
7.5043616886572));
#402124=CARTESIAN_POINT('Ctrl Pts',(-1.31348825286495,-2.41356535601003,
7.50217374673251));
#402125=CARTESIAN_POINT('',(-1.31346170186502,-2.41188626453888,7.50366116523517));
#402126=CARTESIAN_POINT('Ctrl Pts',(-1.30509031014833,-2.4129316392236,
7.51860402984325));
#402127=CARTESIAN_POINT('Ctrl Pts',(-1.30509670862028,-2.41337320408332,
7.51734760759493));
#402128=CARTESIAN_POINT('Ctrl Pts',(-1.30516198111641,-2.41377135902957,
7.51608817408573));
#402129=CARTESIAN_POINT('Ctrl Pts',(-1.30529915524689,-2.41412302796591,
7.5148100591312));
#402130=CARTESIAN_POINT('Ctrl Pts',(-1.30542341085215,-2.41444157809184,
7.51365231206383));
#402131=CARTESIAN_POINT('Ctrl Pts',(-1.30560660504883,-2.41472252559345,
7.51247773061043));
#402132=CARTESIAN_POINT('Ctrl Pts',(-1.30587649835675,-2.41494084061838,
7.51129758471022));
#402133=CARTESIAN_POINT('Ctrl Pts',(-1.30621194491553,-2.41521218126185,
7.50983079813402));
#402134=CARTESIAN_POINT('Ctrl Pts',(-1.30667880678716,-2.4153679832624,
7.50839324291155));
#402135=CARTESIAN_POINT('Ctrl Pts',(-1.30730658833191,-2.41533118376777,
7.50715379678855));
#402136=CARTESIAN_POINT('Ctrl Pts',(-1.30759660531649,-2.41531418346161,
7.50658120839351));
#402137=CARTESIAN_POINT('Ctrl Pts',(-1.30796163787566,-2.41524417646108,
7.50598221009429));
#402138=CARTESIAN_POINT('Ctrl Pts',(-1.30838871444075,-2.41510048946133,
7.50545747549611));
#402139=CARTESIAN_POINT('Ctrl Pts',(-1.30861661571513,-2.41502381363074,
7.50517746087247));
#402140=CARTESIAN_POINT('Ctrl Pts',(-1.30886472060112,-2.41492551702525,
7.50491486231392));
#402141=CARTESIAN_POINT('Ctrl Pts',(-1.30912584447471,-2.41480665196124,
7.50468370960992));
#402142=CARTESIAN_POINT('Ctrl Pts',(-1.30951630703258,-2.41462891119669,
7.50433806340446));
#402143=CARTESIAN_POINT('Ctrl Pts',(-1.30994735749209,-2.41439934358562,
7.50405484070983));
#402144=CARTESIAN_POINT('Ctrl Pts',(-1.31038962865154,-2.41413277776807,
7.50385766036131));
#402145=CARTESIAN_POINT('Ctrl Pts',(-1.31043692267759,-2.41410427269726,
7.50383657498791));
#402146=CARTESIAN_POINT('Ctrl Pts',(-1.31048433154189,-2.41407536951207,
7.50381643264937));
#402147=CARTESIAN_POINT('Ctrl Pts',(-1.31053180983105,-2.41404610463014,
7.50379723213559));
#402148=CARTESIAN_POINT('Ctrl Pts',(-1.31084874294239,-2.41385075197005,
7.50366906242519));
#402149=CARTESIAN_POINT('Ctrl Pts',(-1.31117528635902,-2.41363442062052,
7.50358235568538));
#402150=CARTESIAN_POINT('Ctrl Pts',(-1.3114850217094,-2.41341833793829,
7.5035341175365));
#402151=CARTESIAN_POINT('Ctrl Pts',(-1.31194943481202,-2.41309434641211,
7.50346178989176));
#402152=CARTESIAN_POINT('Ctrl Pts',(-1.31243526188344,-2.41272605894918,
7.50346967198527));
#402153=CARTESIAN_POINT('Ctrl Pts',(-1.3129010688221,-2.41234983956352,
7.50354272648692));
#402154=CARTESIAN_POINT('Ctrl Pts',(-1.31309266485761,-2.41219509274291,
7.50357277531559));
#402155=CARTESIAN_POINT('Ctrl Pts',(-1.31328070831928,-2.41203931988079,
7.50361331098761));
#402156=CARTESIAN_POINT('Ctrl Pts',(-1.3134617018657,-2.41188626454012,
7.50366116523659));
#402157=CARTESIAN_POINT('',(-1.31216235181375,-2.32987712649109,7.57603338622103));
#402158=CARTESIAN_POINT('Origin',(-1.31650127865063,-2.33757551616054,7.58486873427627));
#402159=CARTESIAN_POINT('Ctrl Pts',(-1.31346170186057,-2.41188626459605,
7.50366116529969));
#402160=CARTESIAN_POINT('Ctrl Pts',(-1.31303012767074,-2.38459447933895,
7.52783573079709));
#402161=CARTESIAN_POINT('Ctrl Pts',(-1.31259704935557,-2.35725939039689,
7.55196141284068));
#402162=CARTESIAN_POINT('Ctrl Pts',(-1.31216235147919,-2.32987712769762,
7.57603338728831));
#402163=CARTESIAN_POINT('Ctrl Pts',(-1.30401338901575,-2.32827248701352,
7.59642833564546));
#402164=CARTESIAN_POINT('Ctrl Pts',(-1.30138988733093,-2.31016651972364,
7.5995988229546));
#402165=CARTESIAN_POINT('Ctrl Pts',(-1.31515263304405,-2.32219393616171,
7.59639677331372));
#402166=CARTESIAN_POINT('Ctrl Pts',(-1.30283923060014,-2.32461049415274,
7.58710240504252));
#402167=CARTESIAN_POINT('Ctrl Pts',(-1.30591687143453,-2.31859031743716,
7.58809943920598));
#402168=CARTESIAN_POINT('Ctrl Pts',(-1.31266628426856,-2.31918841227223,
7.58707626057424));
#402169=CARTESIAN_POINT('Ctrl Pts',(-1.308291512786,-2.32726456978442,7.58020924244129));
#402170=CARTESIAN_POINT('Ctrl Pts',(-1.30923351557898,-2.32461132539759,
7.5820588065976));
#402171=CARTESIAN_POINT('Ctrl Pts',(-1.31201671782412,-2.32523024110922,
7.5801537675693));
#402172=CARTESIAN_POINT('Ctrl Pts',(-1.31216235140747,-2.32987712577011,
7.57603338509286));
#402173=CARTESIAN_POINT('Ctrl Pts',(-1.31216235140747,-2.32987712577011,
7.57603338509286));
#402174=CARTESIAN_POINT('Ctrl Pts',(-1.31216235140747,-2.32987712577011,
7.57603338509286));
#402175=CARTESIAN_POINT('Origin',(-1.31649630659947,-2.33757831636809,7.58486873427622));
#402176=CARTESIAN_POINT('Ctrl Pts',(-1.39414625998579,-2.37145206245968,
7.51098857897448));
#402177=CARTESIAN_POINT('Ctrl Pts',(-1.38915651052492,-2.36832749652349,
7.50433767179956));
#402178=CARTESIAN_POINT('Ctrl Pts',(-1.38306334512839,-2.37440872884375,
7.50214974420965));
#402179=CARTESIAN_POINT('Ctrl Pts',(-1.36744758926186,-2.35473343605575,
7.5388732158917));
#402180=CARTESIAN_POINT('Ctrl Pts',(-1.36251762585473,-2.35164630796459,
7.53220407452064));
#402181=CARTESIAN_POINT('Ctrl Pts',(-1.35640527808569,-2.35766645120803,
7.53003438070912));
#402182=CARTESIAN_POINT('Ctrl Pts',(-1.34069764724134,-2.33798270372184,
7.5666946565923));
#402183=CARTESIAN_POINT('Ctrl Pts',(-1.33579681900136,-2.33491381998372,
7.56004085833294));
#402184=CARTESIAN_POINT('Ctrl Pts',(-1.32969743729772,-2.34089162835798,
7.55785582193789));
#402185=CARTESIAN_POINT('Ctrl Pts',(-1.31389764371717,-2.32120062302661,
7.59443891967696));
#402186=CARTESIAN_POINT('Ctrl Pts',(-1.30898970988645,-2.31812728978918,
7.58783901202978));
#402187=CARTESIAN_POINT('Ctrl Pts',(-1.30294118573047,-2.32408501867886,
7.58560008491213));
#402188=CARTESIAN_POINT('',(-1.38161829930507,-2.37350118398177,7.50366116523517));
#402189=CARTESIAN_POINT('Ctrl Pts',(-1.38161829930525,-2.37350118398209,
7.50366116523554));
#402190=CARTESIAN_POINT('Ctrl Pts',(-1.38233657059499,-2.37325988775106,
7.50350835821027));
#402191=CARTESIAN_POINT('Ctrl Pts',(-1.38298898591945,-2.37301470974318,
7.50345484956));
#402192=CARTESIAN_POINT('Ctrl Pts',(-1.38359515336115,-2.37275892273606,
7.50349758195598));
#402193=CARTESIAN_POINT('Ctrl Pts',(-1.38390616221329,-2.37262768503175,
7.50351950684424));
#402194=CARTESIAN_POINT('Ctrl Pts',(-1.38423570114598,-2.3724808385058,
7.50357029184312));
#402195=CARTESIAN_POINT('Ctrl Pts',(-1.38454957938261,-2.37233050120684,
7.50365515313924));
#402196=CARTESIAN_POINT('Ctrl Pts',(-1.38503245121239,-2.37209922156346,
7.50378570417639));
#402197=CARTESIAN_POINT('Ctrl Pts',(-1.38549258320202,-2.3718532044281,
7.50400001621911));
#402198=CARTESIAN_POINT('Ctrl Pts',(-1.38589388211697,-2.37160917307933,
7.50428903009635));
#402199=CARTESIAN_POINT('Ctrl Pts',(-1.38593842320912,-2.37158208747708,
7.50432110841318));
#402200=CARTESIAN_POINT('Ctrl Pts',(-1.38598226978506,-2.37155502807397,
7.50435406373354));
#402201=CARTESIAN_POINT('Ctrl Pts',(-1.38602539484945,-2.37152801871388,
7.50438785222351));
#402202=CARTESIAN_POINT('Ctrl Pts',(-1.38628869409615,-2.37136311358818,
7.50459414719561));
#402203=CARTESIAN_POINT('Ctrl Pts',(-1.38652901586914,-2.371197011355,7.50483629897752));
#402204=CARTESIAN_POINT('Ctrl Pts',(-1.38673790177455,-2.37103715795091,
7.5050991045531));
#402205=CARTESIAN_POINT('Ctrl Pts',(-1.38719872506251,-2.37068450528575,
7.50567888004914));
#402206=CARTESIAN_POINT('Ctrl Pts',(-1.38752502904372,-2.37034878156346,
7.50637912803144));
#402207=CARTESIAN_POINT('Ctrl Pts',(-1.38774383460514,-2.37004499644843,
7.50710440483569));
#402208=CARTESIAN_POINT('Ctrl Pts',(-1.38779749007269,-2.36997050230724,
7.50728225710685));
#402209=CARTESIAN_POINT('Ctrl Pts',(-1.38784586790669,-2.36989653107072,
7.50746498566954));
#402210=CARTESIAN_POINT('Ctrl Pts',(-1.38788818746179,-2.36982503748699,
7.50764697238949));
#402211=CARTESIAN_POINT('Ctrl Pts',(-1.38811568574333,-2.3694407076564,
7.50862528291182));
#402212=CARTESIAN_POINT('Ctrl Pts',(-1.38819232289273,-2.3690951978627,
7.50965856837421));
#402213=CARTESIAN_POINT('Ctrl Pts',(-1.38818430083284,-2.36878494422429,
7.51067959873202));
#402214=CARTESIAN_POINT('Ctrl Pts',(-1.38817988628316,-2.36861421125573,
7.51124147302578));
#402215=CARTESIAN_POINT('Ctrl Pts',(-1.38814939892001,-2.36845412452276,
7.51180065547253));
#402216=CARTESIAN_POINT('Ctrl Pts',(-1.38810116047299,-2.36830425937062,
7.51235175716501));
#402217=CARTESIAN_POINT('Ctrl Pts',(-1.38793447742262,-2.36778641557079,
7.51425603304536));
#402218=CARTESIAN_POINT('Ctrl Pts',(-1.38753020370092,-2.36733073016878,
7.51626900505179));
#402219=CARTESIAN_POINT('Ctrl Pts',(-1.38694802379011,-2.36694617144078,
7.51827788969243));
#402220=CARTESIAN_POINT('Ctrl Pts',(-1.38691651511317,-2.3669253583957,
7.51838661432545));
#402221=CARTESIAN_POINT('Ctrl Pts',(-1.38688447545091,-2.36690475507048,
7.51849533314856));
#402222=CARTESIAN_POINT('Ctrl Pts',(-1.38685191115369,-2.36688436340661,
7.51860402984325));
#402223=CARTESIAN_POINT('Ctrl Pts',(-1.31216235301973,-2.32987712683137,
7.57603338728985));
#402224=CARTESIAN_POINT('Ctrl Pts',(-1.33535275265834,-2.34444361706459,
7.55196141284922));
#402225=CARTESIAN_POINT('Ctrl Pts',(-1.3585036515822,-2.35898426782541,
7.52783573083106));
#402226=CARTESIAN_POINT('Ctrl Pts',(-1.38161829935786,-2.3735011840085,
7.50366116530176));
#402227=CARTESIAN_POINT('Origin',(-4.53412748053607E-16,-8.05080247188567E-16,
7.49482233047033));
#402228=CARTESIAN_POINT('Origin',(-1.3092344481825,-2.40412383410095,7.49482233047033));
#402229=CARTESIAN_POINT('Origin',(0.,0.,7.50366116523517));
#402230=CARTESIAN_POINT('Origin',(-1.37717168998613,-2.36586229233672,7.49482233047033));
#402231=CARTESIAN_POINT('Ctrl Pts',(-1.30509029477835,-2.41293058161501,
7.51860402984325));
#402232=CARTESIAN_POINT('Ctrl Pts',(-1.30520118422927,-2.42053873444995,
7.51860402984325));
#402233=CARTESIAN_POINT('Ctrl Pts',(-1.29849386712375,-2.42413153047479,
7.51860402984325));
#402234=CARTESIAN_POINT('Ctrl Pts',(-1.30513146751763,-2.41575554070188,
7.51041458714366));
#402235=CARTESIAN_POINT('Ctrl Pts',(-1.30361213930822,-2.42138990025308,
7.51004642900443));
#402236=CARTESIAN_POINT('Ctrl Pts',(-1.29849201732533,-2.42413252132527,
7.5072913648301));
#402237=CARTESIAN_POINT('Ctrl Pts',(-1.30778745780282,-2.41668798523334,
7.50215815450138));
#402238=CARTESIAN_POINT('Ctrl Pts',(-1.30684765962189,-2.41965696550619,
7.49877163671529));
#402239=CARTESIAN_POINT('Ctrl Pts',(-1.30381763149247,-2.4213070725116,
7.4948158853317));
#402240=CARTESIAN_POINT('Ctrl Pts',(-1.31346143857516,-2.4118857810634,
7.50366171572174));
#402241=CARTESIAN_POINT('Ctrl Pts',(-1.31521268767226,-2.41510156850306,
7.50000045605858));
#402242=CARTESIAN_POINT('Ctrl Pts',(-1.31521268767215,-2.41510156850312,
7.49482233047317));
#402243=CARTESIAN_POINT('Origin',(-1.29259162227319,-2.41311275079081,7.51860402984325));
#402244=CARTESIAN_POINT('Origin',(-1.29259162227319,-2.41311275079081,9.));
#402245=CARTESIAN_POINT('Origin',(-1.29259162227319,-2.41311275079081,8.75721825406948));
#402246=CARTESIAN_POINT('Ctrl Pts',(-1.30484831255306,-2.39623323156884,
8.78942910404912));
#402247=CARTESIAN_POINT('Ctrl Pts',(-1.30494925753138,-2.40180478779784,
8.7967269950169));
#402248=CARTESIAN_POINT('Ctrl Pts',(-1.29620618705045,-2.40360262109034,
8.79893251111266));
#402249=CARTESIAN_POINT('Ctrl Pts',(-1.30500761319209,-2.40722641318503,
8.78111911759583));
#402250=CARTESIAN_POINT('Ctrl Pts',(-1.30511984201779,-2.41383169249906,
8.78644465894817));
#402251=CARTESIAN_POINT('Ctrl Pts',(-1.29771440498274,-2.41712942112574,
8.78817647674132));
#402252=CARTESIAN_POINT('Ctrl Pts',(-1.30510689311819,-2.41407762618086,
8.76780923932028));
#402253=CARTESIAN_POINT('Ctrl Pts',(-1.30523427945356,-2.4218749660793,
8.76988516158371));
#402254=CARTESIAN_POINT('Ctrl Pts',(-1.29864530823805,-2.42557926611001,
8.77093053738833));
#402255=CARTESIAN_POINT('Ctrl Pts',(-1.30508753488961,-2.41274173341213,
8.75371302330492));
#402256=CARTESIAN_POINT('Ctrl Pts',(-1.30521255697054,-2.42034768968646,
8.7530082828756));
#402257=CARTESIAN_POINT('Ctrl Pts',(-1.29846328949484,-2.42393125325862,
8.75267964240738));
#402258=CARTESIAN_POINT('Origin',(-1.29238845014159,-2.39909164160958,8.78727029226991));
#402259=CARTESIAN_POINT('Ctrl Pts',(-1.30385128920419,-2.32742558187727,
8.85049129520029));
#402260=CARTESIAN_POINT('Ctrl Pts',(-1.30393589896117,-2.33326458465275,
8.85711686593484));
#402261=CARTESIAN_POINT('Ctrl Pts',(-1.29564064670648,-2.33533570805444,
8.85933012996512));
#402262=CARTESIAN_POINT('Ctrl Pts',(-1.30419707450795,-2.3512885667223,
8.82945683644722));
#402263=CARTESIAN_POINT('Ctrl Pts',(-1.30428238657706,-2.35717603675116,
8.83607469902389));
#402264=CARTESIAN_POINT('Ctrl Pts',(-1.29595369511063,-2.35921685544824,
8.8382956714852));
#402265=CARTESIAN_POINT('Ctrl Pts',(-1.30454234439083,-2.37511598186413,
8.80838214965003));
#402266=CARTESIAN_POINT('Ctrl Pts',(-1.30462799314121,-2.38102668659851,
8.8150136446199));
#402267=CARTESIAN_POINT('Ctrl Pts',(-1.29626693711643,-2.38306176761555,
8.81722098428721));
#402268=CARTESIAN_POINT('Ctrl Pts',(-1.30488713801673,-2.39891053004237,
8.78727029226991));
#402269=CARTESIAN_POINT('Ctrl Pts',(-1.30497280099364,-2.40482221656424,
8.79393457792714));
#402270=CARTESIAN_POINT('Ctrl Pts',(-1.29658037301229,-2.4068732084599,
8.79610912703474));
#402271=CARTESIAN_POINT('Origin',(-1.29135260132905,-2.32760669344448,8.85049129520029));
#402272=CARTESIAN_POINT('Ctrl Pts',(-1.31437432427028,-2.32149911893915,
8.85049129520029));
#402273=CARTESIAN_POINT('Ctrl Pts',(-1.31932364416768,-2.32459836800566,
8.85711686593484));
#402274=CARTESIAN_POINT('Ctrl Pts',(-1.32539494747702,-2.31857839805225,
8.85933012996512));
#402275=CARTESIAN_POINT('Ctrl Pts',(-1.30999573240122,-2.31875725802814,
8.86332496987232));
#402276=CARTESIAN_POINT('Ctrl Pts',(-1.3141529305551,-2.31673993359062,
8.86648636486737));
#402277=CARTESIAN_POINT('Ctrl Pts',(-1.31313656540692,-2.31092245099259,
8.87206031107457));
#402278=CARTESIAN_POINT('Ctrl Pts',(-1.30377592752361,-2.32222479797459,
8.86341338519876));
#402279=CARTESIAN_POINT('Ctrl Pts',(-1.29986873773977,-2.32471625109019,
8.86654584966059));
#402280=CARTESIAN_POINT('Ctrl Pts',(-1.29544436127693,-2.32077302326231,
8.87215952290714));
#402281=CARTESIAN_POINT('Ctrl Pts',(-1.30385128920419,-2.32742558187727,
8.85049129520029));
#402282=CARTESIAN_POINT('Ctrl Pts',(-1.30393589896117,-2.33326458465275,
8.85711686593484));
#402283=CARTESIAN_POINT('Ctrl Pts',(-1.29564064670648,-2.33533570805444,
8.85933012996512));
#402284=CARTESIAN_POINT('Origin',(-1.32100842742437,-2.31090484334613,8.85049129520029));
#402285=CARTESIAN_POINT('Ctrl Pts',(-1.37496718403116,-2.35944218342961,
8.78727029226991));
#402286=CARTESIAN_POINT('Ctrl Pts',(-1.37997811292689,-2.36258001186349,
8.79393457792714));
#402287=CARTESIAN_POINT('Ctrl Pts',(-1.38608257609906,-2.35646650676757,
8.79610912703474));
#402288=CARTESIAN_POINT('Ctrl Pts',(-1.35479818681082,-2.34681241871378,
8.80838214965003));
#402289=CARTESIAN_POINT('Ctrl Pts',(-1.35980828351301,-2.34994972603062,
8.81501364461989));
#402290=CARTESIAN_POINT('Ctrl Pts',(-1.36588287762334,-2.34385480035508,
8.81722098428721));
#402291=CARTESIAN_POINT('Ctrl Pts',(-1.33460133053251,-2.33416520874058,
8.8294568364472));
#402292=CARTESIAN_POINT('Ctrl Pts',(-1.33959173277746,-2.3372901834482,
8.83607469902387));
#402293=CARTESIAN_POINT('Ctrl Pts',(-1.34565445587685,-2.3312259084612,
8.8382956714852));
#402294=CARTESIAN_POINT('Ctrl Pts',(-1.31437432427028,-2.32149911893915,
8.85049129520029));
#402295=CARTESIAN_POINT('Ctrl Pts',(-1.31932364416768,-2.32459836800566,
8.85711686593484));
#402296=CARTESIAN_POINT('Ctrl Pts',(-1.32539494747702,-2.31857839805225,
8.85933012996512));
#402297=CARTESIAN_POINT('Origin',(-1.38160128718526,-2.3488479078366,8.78727029226991));
#402298=CARTESIAN_POINT('Ctrl Pts',(-1.38669498910092,-2.36678607752907,
8.75374538247848));
#402299=CARTESIAN_POINT('Ctrl Pts',(-1.3931284634167,-2.3708301826978,8.75304829418602));
#402300=CARTESIAN_POINT('Ctrl Pts',(-1.39968761886182,-2.36692529818531,
8.75272238421917));
#402301=CARTESIAN_POINT('Ctrl Pts',(-1.38781373054482,-2.36748663052191,
8.7676940844502));
#402302=CARTESIAN_POINT('Ctrl Pts',(-1.39440946688856,-2.37163191905902,
8.76974318093968));
#402303=CARTESIAN_POINT('Ctrl Pts',(-1.40098765781906,-2.36792439139734,
8.7707786988043));
#402304=CARTESIAN_POINT('Ctrl Pts',(-1.38207969920049,-2.36389599497184,
8.78108014887989));
#402305=CARTESIAN_POINT('Ctrl Pts',(-1.38766732642936,-2.36741219451847,
8.78639403366325));
#402306=CARTESIAN_POINT('Ctrl Pts',(-1.39432774009023,-2.36281208956369,
8.78812224174741));
#402307=CARTESIAN_POINT('Ctrl Pts',(-1.37268288764618,-2.35801173591639,
8.78944554828685));
#402308=CARTESIAN_POINT('Ctrl Pts',(-1.37738895133901,-2.36097979624865,
8.79673892988686));
#402309=CARTESIAN_POINT('Ctrl Pts',(-1.3834541258599,-2.35444395564872,
8.79894799272499));
#402310=CARTESIAN_POINT('Origin',(-1.39348601430779,-2.3562900878136,8.75721825406948));
#402311=CARTESIAN_POINT('Origin',(-1.39348601430779,-2.3562900878136,9.));
#402312=CARTESIAN_POINT('Origin',(-1.39348601430779,-2.3562900878136,7.51860402984325));
#402313=CARTESIAN_POINT('Ctrl Pts',(-1.38161790355313,-2.37350050411393,
7.50366195182966));
#402314=CARTESIAN_POINT('Ctrl Pts',(-1.38346014519167,-2.37666531650257,
7.50000065167735));
#402315=CARTESIAN_POINT('Ctrl Pts',(-1.38346014519177,-2.37666531650251,
7.49482233047108));
#402316=CARTESIAN_POINT('Ctrl Pts',(-1.38867182375219,-2.37113491551234,
7.50215800491337));
#402317=CARTESIAN_POINT('Ctrl Pts',(-1.39169926431185,-2.37186928655758,
7.49877273257265));
#402318=CARTESIAN_POINT('Ctrl Pts',(-1.39468274606848,-2.37013262511743,
7.49481816995649));
#402319=CARTESIAN_POINT('Ctrl Pts',(-1.38924060074977,-2.36838055368623,
7.51043025814041));
#402320=CARTESIAN_POINT('Ctrl Pts',(-1.39484851529315,-2.3700066076401,
7.51006209594514));
#402321=CARTESIAN_POINT('Ctrl Pts',(-1.39985114343625,-2.36704811447225,
7.50731281821697));
#402322=CARTESIAN_POINT('Ctrl Pts',(-1.38685063022083,-2.36688356118254,
7.51860402984325));
#402323=CARTESIAN_POINT('Ctrl Pts',(-1.39329931967805,-2.37092279646599,
7.51860402984324));
#402324=CARTESIAN_POINT('Ctrl Pts',(-1.39984896414482,-2.36704940328306,
7.51860402984325));
#402325=CARTESIAN_POINT('Origin',(0.,0.,7.5));
#402326=CARTESIAN_POINT('Origin',(-1.1629348420194,-2.40094160211229,7.5));
#402327=CARTESIAN_POINT('',(-1.1629348420194,-2.40094160211229,7.59394543036555));
#402328=CARTESIAN_POINT('',(-1.1629348420194,-2.40094160211229,8.85049129520029));
#402329=CARTESIAN_POINT('',(-1.1629348420194,-2.40094160211229,7.5));
#402330=CARTESIAN_POINT('',(-1.22097218676269,-2.44268890636151,8.78727029226991));
#402331=CARTESIAN_POINT('Ctrl Pts',(-1.1629348420194,-2.40094160211229,
8.85049129520029));
#402332=CARTESIAN_POINT('Ctrl Pts',(-1.18230874456756,-2.41487759811194,
8.82945686509571));
#402333=CARTESIAN_POINT('Ctrl Pts',(-1.20165384546694,-2.42879287656843,
8.80838212259897));
#402334=CARTESIAN_POINT('Ctrl Pts',(-1.22097218676269,-2.44268890636151,
8.78727029226991));
#402335=CARTESIAN_POINT('',(-1.23235567333045,-2.45087725266273,8.75721825406948));
#402336=CARTESIAN_POINT('Origin',(-1.19809869544859,-2.42623584190782,8.75937679713118));
#402337=CARTESIAN_POINT('',(-1.23235567333045,-2.45087725266273,7.51860402984325));
#402338=CARTESIAN_POINT('',(-1.23235567333045,-2.45087725266273,7.5));
#402339=CARTESIAN_POINT('Ctrl Pts',(-1.23235567333045,-2.45087725266273,
7.51860402984325));
#402340=CARTESIAN_POINT('Ctrl Pts',(-1.22341571509852,-2.44444658017186,
7.52834476460825));
#402341=CARTESIAN_POINT('Ctrl Pts',(-1.21446995317471,-2.43801173298122,
7.53807742314407));
#402342=CARTESIAN_POINT('Ctrl Pts',(-1.20551819269234,-2.43157257091968,
7.54780169004674));
#402343=CARTESIAN_POINT('Ctrl Pts',(-1.19133908788964,-2.42137328622121,
7.5632044032688));
#402344=CARTESIAN_POINT('Ctrl Pts',(-1.17714491544797,-2.41116316309945,
7.57858609112103));
#402345=CARTESIAN_POINT('Ctrl Pts',(-1.1629348420194,-2.40094160211229,
7.59394543036555));
#402346=CARTESIAN_POINT('Origin',(-1.13841252486687,-2.68084313576938,7.5));
#402347=CARTESIAN_POINT('',(-1.14781180121215,-2.49159143565061,8.75721825406948));
#402348=CARTESIAN_POINT('',(-1.14850738206911,-2.47758611705879,8.78727029226991));
#402349=CARTESIAN_POINT('Origin',(-1.15027302572279,-2.44203539474894,8.75658640621031));
#402350=CARTESIAN_POINT('',(-1.1520537178733,-2.40618167532514,8.85049129520029));
#402351=CARTESIAN_POINT('Ctrl Pts',(-1.14850738206911,-2.47758611705879,
8.78727029226991));
#402352=CARTESIAN_POINT('Ctrl Pts',(-1.14968781728229,-2.45381839678239,
8.80838212259896));
#402353=CARTESIAN_POINT('Ctrl Pts',(-1.15086988762439,-2.43001775366009,
8.82945686509571));
#402354=CARTESIAN_POINT('Ctrl Pts',(-1.1520537178733,-2.40618167532514,
8.85049129520029));
#402355=CARTESIAN_POINT('',(-1.1520537178733,-2.40618167532514,7.59394543036555));
#402356=CARTESIAN_POINT('',(-1.1520537178733,-2.40618167532514,7.5));
#402357=CARTESIAN_POINT('',(-1.14781180121215,-2.49159143565061,7.51860402984325));
#402358=CARTESIAN_POINT('Ctrl Pts',(-1.1520537178733,-2.40618167532514,
7.59394543036555));
#402359=CARTESIAN_POINT('Ctrl Pts',(-1.15118542018665,-2.42366459713435,
7.57858609112103));
#402360=CARTESIAN_POINT('Ctrl Pts',(-1.15031809411992,-2.44112795565877,
7.56320440326857));
#402361=CARTESIAN_POINT('Ctrl Pts',(-1.14945168875186,-2.45857277618247,
7.54780169004651));
#402362=CARTESIAN_POINT('Ctrl Pts',(-1.14890469700285,-2.46958629622899,
7.53807742314383));
#402363=CARTESIAN_POINT('Ctrl Pts',(-1.148358071792,-2.48059243613579,7.52834476460825));
#402364=CARTESIAN_POINT('Ctrl Pts',(-1.14781180121215,-2.49159143565061,
7.51860402984325));
#402365=CARTESIAN_POINT('',(-1.14781180121215,-2.49159143565061,7.5));
#402366=CARTESIAN_POINT('Origin',(-1.1589202543844,-2.4065227051503,7.5));
#402367=CARTESIAN_POINT('Ctrl Pts',(-1.1520537178733,-2.40618167532514,
8.85049129520029));
#402368=CARTESIAN_POINT('Ctrl Pts',(-1.15206332432413,-2.40598825222679,
8.85097269580138));
#402369=CARTESIAN_POINT('Ctrl Pts',(-1.15208121062939,-2.40579768676134,
8.85143669361005));
#402370=CARTESIAN_POINT('Ctrl Pts',(-1.15210907085544,-2.4056012857056,
8.8519052845931));
#402371=CARTESIAN_POINT('Ctrl Pts',(-1.15216356369076,-2.40521713769588,
8.85282181883899));
#402372=CARTESIAN_POINT('Ctrl Pts',(-1.15225500672476,-2.40482057420506,
8.85372622499636));
#402373=CARTESIAN_POINT('Ctrl Pts',(-1.152399859333,-2.40440883694516,8.85462257735071));
#402374=CARTESIAN_POINT('Ctrl Pts',(-1.15252011082368,-2.40406702729551,
8.85536669723987));
#402375=CARTESIAN_POINT('Ctrl Pts',(-1.15267716836054,-2.4037146718648,
8.85610498449051));
#402376=CARTESIAN_POINT('Ctrl Pts',(-1.1528877715664,-2.40335342065579,
8.85681338218371));
#402377=CARTESIAN_POINT('Ctrl Pts',(-1.15307889430648,-2.40302558461625,
8.85745625420285));
#402378=CARTESIAN_POINT('Ctrl Pts',(-1.153315995465,-2.4026860085849,8.85808743050666));
#402379=CARTESIAN_POINT('Ctrl Pts',(-1.1536272932187,-2.40233933805946,
8.8586680450841));
#402380=CARTESIAN_POINT('Ctrl Pts',(-1.15377091925415,-2.40217939179392,
8.85893592806395));
#402381=CARTESIAN_POINT('Ctrl Pts',(-1.15393057225672,-2.40201800294867,
8.85919241173848));
#402382=CARTESIAN_POINT('Ctrl Pts',(-1.15411047916769,-2.40185628280406,
8.85943017985535));
#402383=CARTESIAN_POINT('Ctrl Pts',(-1.15435340675565,-2.40163791273454,
8.85975123720001));
#402384=CARTESIAN_POINT('Ctrl Pts',(-1.15463987464168,-2.40141385689638,
8.86004599534706));
#402385=CARTESIAN_POINT('Ctrl Pts',(-1.15497285750656,-2.40119501106982,
8.86026130871721));
#402386=CARTESIAN_POINT('Ctrl Pts',(-1.15509477192118,-2.4011148854428,
8.86034014101236));
#402387=CARTESIAN_POINT('Ctrl Pts',(-1.15522474618014,-2.40103424434313,
8.86040910639693));
#402388=CARTESIAN_POINT('Ctrl Pts',(-1.15535941654965,-2.40095557062527,
8.86046313645507));
#402389=CARTESIAN_POINT('Ctrl Pts',(-1.1555695685334,-2.40083280094742,
8.8605474499083));
#402390=CARTESIAN_POINT('Ctrl Pts',(-1.15579696686364,-2.4007115978283,
8.86059655985669));
#402391=CARTESIAN_POINT('Ctrl Pts',(-1.15602688999811,-2.40059947586523,
8.86059725258816));
#402392=CARTESIAN_POINT('Ctrl Pts',(-1.15625734434688,-2.40048709485562,
8.86059794692011));
#402393=CARTESIAN_POINT('Ctrl Pts',(-1.15649405543566,-2.40038497866228,
8.86056369958366));
#402394=CARTESIAN_POINT('Ctrl Pts',(-1.15672262232883,-2.40029524146196,
8.86048590497774));
#402395=CARTESIAN_POINT('Ctrl Pts',(-1.15678227148269,-2.40027182272448,
8.86046560290182));
#402396=CARTESIAN_POINT('Ctrl Pts',(-1.15684217507605,-2.40024902671321,
8.86044257503091));
#402397=CARTESIAN_POINT('Ctrl Pts',(-1.15690047036322,-2.40022752716396,
8.86041778462584));
#402398=CARTESIAN_POINT('Ctrl Pts',(-1.15729272530748,-2.40008286187622,
8.86025097596201));
#402399=CARTESIAN_POINT('Ctrl Pts',(-1.15766491251364,-2.39997779467967,
8.8599848982295));
#402400=CARTESIAN_POINT('Ctrl Pts',(-1.15800386701871,-2.39990723838852,
8.85968173251461));
#402401=CARTESIAN_POINT('Ctrl Pts',(-1.15818315453212,-2.39986991815289,
8.85952137522076));
#402402=CARTESIAN_POINT('Ctrl Pts',(-1.15835656116864,-2.39984134706458,
8.85934740853961));
#402403=CARTESIAN_POINT('Ctrl Pts',(-1.15852138878529,-2.39982039416741,
8.8591675900182));
#402404=CARTESIAN_POINT('Ctrl Pts',(-1.15918325734184,-2.39973625739415,
8.85844552518696));
#402405=CARTESIAN_POINT('Ctrl Pts',(-1.1597438200588,-2.39976720241301,
8.85759444184126));
#402406=CARTESIAN_POINT('Ctrl Pts',(-1.16019860651595,-2.39983348615085,
8.85683498915141));
#402407=CARTESIAN_POINT('Ctrl Pts',(-1.1602461987075,-2.39984042256749,
8.85675551445));
#402408=CARTESIAN_POINT('Ctrl Pts',(-1.16029262584356,-2.39984776479439,
8.85667699793652));
#402409=CARTESIAN_POINT('Ctrl Pts',(-1.16033787776632,-2.3998554335768,
8.85659965593547));
#402410=CARTESIAN_POINT('Ctrl Pts',(-1.1609486905288,-2.39995894719316,
8.85555568965886));
#402411=CARTESIAN_POINT('Ctrl Pts',(-1.1615207700221,-2.40014664364083,
8.85434650606346));
#402412=CARTESIAN_POINT('Ctrl Pts',(-1.162058881696,-2.4004135457534,8.85297329937117));
#402413=CARTESIAN_POINT('Ctrl Pts',(-1.16236153672494,-2.40056366192913,
8.85220095427747));
#402414=CARTESIAN_POINT('Ctrl Pts',(-1.16265343008713,-2.4007391774561,
8.85137579139184));
#402415=CARTESIAN_POINT('Ctrl Pts',(-1.1629348420194,-2.40094160211229,
8.85049129520029));
#402416=CARTESIAN_POINT('Origin',(-1.1589202543844,-2.4065227051503,7.59394543036555));
#402417=CARTESIAN_POINT('Ctrl Pts',(-1.15208160864078,-2.40562010281996,
7.59443877723642));
#402418=CARTESIAN_POINT('Ctrl Pts',(-1.1523688567101,-2.39983644634716,
7.58783886950016));
#402419=CARTESIAN_POINT('Ctrl Pts',(-1.16071568230795,-2.39828413066546,
7.58559994247159));
#402420=CARTESIAN_POINT('Ctrl Pts',(-1.15051352985788,-2.43719291381971,
7.56670252222137));
#402421=CARTESIAN_POINT('Ctrl Pts',(-1.15080036277219,-2.43141761637255,
7.5600487499903));
#402422=CARTESIAN_POINT('Ctrl Pts',(-1.15919273970383,-2.42983509727514,
7.55786368756705));
#402423=CARTESIAN_POINT('Ctrl Pts',(-1.14894837930544,-2.46870676574944,
7.5388891333356));
#402424=CARTESIAN_POINT('Ctrl Pts',(-1.1492369168818,-2.46289714542674,
7.53222002137277));
#402425=CARTESIAN_POINT('Ctrl Pts',(-1.15767142205792,-2.46132820720179,
7.53005029815326));
#402426=CARTESIAN_POINT('Ctrl Pts',(-1.14738622780757,-2.50016023258599,
7.51101258149734));
#402427=CARTESIAN_POINT('Ctrl Pts',(-1.14767826298364,-2.49428018910865,
7.5043616886572));
#402428=CARTESIAN_POINT('Ctrl Pts',(-1.15615188708088,-2.49276190843518,
7.50217374673251));
#402429=CARTESIAN_POINT('',(-1.15623297039275,-2.49108456570912,7.50366116523517));
#402430=CARTESIAN_POINT('Ctrl Pts',(-1.14781180121215,-2.49159143565061,
7.51860402984325));
#402431=CARTESIAN_POINT('Ctrl Pts',(-1.14778989538006,-2.49203250321947,
7.51734760759494));
#402432=CARTESIAN_POINT('Ctrl Pts',(-1.14782952389185,-2.49243402213687,
7.51608817408573));
#402433=CARTESIAN_POINT('Ctrl Pts',(-1.14794388467726,-2.49279375730838,
7.5148100591312));
#402434=CARTESIAN_POINT('Ctrl Pts',(-1.14804747540941,-2.49311961402288,
7.51365231206384));
#402435=CARTESIAN_POINT('Ctrl Pts',(-1.14821229284573,-2.49341172158019,
7.51247773061043));
#402436=CARTESIAN_POINT('Ctrl Pts',(-1.14846764413724,-2.4936468801771,
7.51129758471022));
#402437=CARTESIAN_POINT('Ctrl Pts',(-1.14878501663036,-2.49393915545693,
7.50983079813401));
#402438=CARTESIAN_POINT('Ctrl Pts',(-1.14924093701577,-2.49412454928837,
7.50839324291155));
#402439=CARTESIAN_POINT('Ctrl Pts',(-1.14986978646771,-2.49412804750393,
7.50715379678855));
#402440=CARTESIAN_POINT('Ctrl Pts',(-1.15016029679465,-2.49412966357871,
7.50658120839351));
#402441=CARTESIAN_POINT('Ctrl Pts',(-1.1505290647192,-2.49408318813144,
7.50598221009429));
#402442=CARTESIAN_POINT('Ctrl Pts',(-1.15096446986736,-2.49396715924152,
7.50545747549611));
#402443=CARTESIAN_POINT('Ctrl Pts',(-1.15119681553147,-2.49390524263443,
7.50517746087247));
#402444=CARTESIAN_POINT('Ctrl Pts',(-1.1514507085445,-2.49382304412448,
7.50491486231392));
#402445=CARTESIAN_POINT('Ctrl Pts',(-1.15171891162188,-2.49372115354552,
7.50468370960992));
#402446=CARTESIAN_POINT('Ctrl Pts',(-1.15211995982243,-2.49356879499041,
7.50433806340447));
#402447=CARTESIAN_POINT('Ctrl Pts',(-1.15256483308989,-2.49336731654838,
7.50405484070984));
#402448=CARTESIAN_POINT('Ctrl Pts',(-1.15302327448637,-2.49312963482937,
7.50385766036131));
#402449=CARTESIAN_POINT('Ctrl Pts',(-1.15307229766794,-2.49310421846394,
7.50383657498791));
#402450=CARTESIAN_POINT('Ctrl Pts',(-1.15312146095907,-2.4930784121598,
7.50381643264937));
#402451=CARTESIAN_POINT('Ctrl Pts',(-1.15317071670641,-2.49305224935014,
7.50379723213559));
#402452=CARTESIAN_POINT('Ctrl Pts',(-1.1534995149326,-2.49287760403721,
7.50366906242519));
#402453=CARTESIAN_POINT('Ctrl Pts',(-1.15383924782791,-2.49268263887218,
7.50358235568538));
#402454=CARTESIAN_POINT('Ctrl Pts',(-1.15416219125878,-2.49248684496702,
7.5035341175365));
#402455=CARTESIAN_POINT('Ctrl Pts',(-1.15464640838322,-2.49219327416583,
7.50346178989176));
#402456=CARTESIAN_POINT('Ctrl Pts',(-1.15515483352959,-2.49185687043632,
7.50346967198527));
#402457=CARTESIAN_POINT('Ctrl Pts',(-1.15564378787674,-2.49151126838677,
7.50354272648693));
#402458=CARTESIAN_POINT('Ctrl Pts',(-1.15584490492048,-2.49136911511025,
7.50357277531559));
#402459=CARTESIAN_POINT('Ctrl Pts',(-1.15604254242823,-2.49122571028613,
7.50361331098761));
#402460=CARTESIAN_POINT('Ctrl Pts',(-1.15623297039335,-2.49108456571041,
7.50366116523658));
#402461=CARTESIAN_POINT('',(-1.16019063351066,-2.40916067458729,7.57603338622103));
#402462=CARTESIAN_POINT('Origin',(-1.16402740803746,-2.41712124308652,7.58486873427627));
#402463=CARTESIAN_POINT('Ctrl Pts',(-1.15623297038464,-2.49108456576589,
7.50366116529969));
#402464=CARTESIAN_POINT('Ctrl Pts',(-1.15755087359535,-2.46382120335537,
7.52783573079709));
#402465=CARTESIAN_POINT('Ctrl Pts',(-1.15887005024774,-2.43651452986229,
7.55196141284068));
#402466=CARTESIAN_POINT('Ctrl Pts',(-1.16019063309948,-2.4091606757699,
7.57603338728831));
#402467=CARTESIAN_POINT('Ctrl Pts',(-1.15217830426507,-2.40721753909579,
7.5963967733137));
#402468=CARTESIAN_POINT('Ctrl Pts',(-1.1501876471192,-2.38904863159187,
7.59959882295471));
#402469=CARTESIAN_POINT('Ctrl Pts',(-1.16353671011163,-2.40155908041819,
7.59642833564546));
#402470=CARTESIAN_POINT('Ctrl Pts',(-1.15113573851764,-2.4034587945253,
7.5870762605742));
#402471=CARTESIAN_POINT('Ctrl Pts',(-1.15450664925665,-2.39758093336444,
7.58809943920598));
#402472=CARTESIAN_POINT('Ctrl Pts',(-1.16120500076186,-2.39850098113831,
7.58710240504253));
#402473=CARTESIAN_POINT('Ctrl Pts',(-1.15646270668161,-2.40638266908519,
7.58015376756929));
#402474=CARTESIAN_POINT('Ctrl Pts',(-1.15754740556005,-2.40374587183485,
7.58205880659762));
#402475=CARTESIAN_POINT('Ctrl Pts',(-1.16026245848246,-2.40449123259747,
7.58020924244126));
#402476=CARTESIAN_POINT('Ctrl Pts',(-1.16019063315141,-2.40916067384176,
7.57603338509286));
#402477=CARTESIAN_POINT('Ctrl Pts',(-1.16019063315141,-2.40916067384176,
7.57603338509286));
#402478=CARTESIAN_POINT('Ctrl Pts',(-1.16019063315141,-2.40916067384176,
7.57603338509286));
#402479=CARTESIAN_POINT('Origin',(-1.16402226679189,-2.41712371898008,7.58486873427622));
#402480=CARTESIAN_POINT('Ctrl Pts',(-1.23934238165743,-2.4559029174225,
7.51098857897448));
#402481=CARTESIAN_POINT('Ctrl Pts',(-1.23456307579885,-2.45246507689652,
7.50433767179957));
#402482=CARTESIAN_POINT('Ctrl Pts',(-1.2280928035716,-2.45814342422544,
7.50214974420965));
#402483=CARTESIAN_POINT('Ctrl Pts',(-1.21376973228739,-2.4375080515231,
7.53887321589169));
#402484=CARTESIAN_POINT('Ctrl Pts',(-1.20904769099473,-2.43411140242769,
7.53220407452063));
#402485=CARTESIAN_POINT('Ctrl Pts',(-1.2025621897978,-2.43972755717505,
7.53003438070912));
#402486=CARTESIAN_POINT('Ctrl Pts',(-1.18814797399718,-2.41907786069558,
7.56669465659233));
#402487=CARTESIAN_POINT('Ctrl Pts',(-1.18345383909065,-2.41570128516483,
7.56004085833299));
#402488=CARTESIAN_POINT('Ctrl Pts',(-1.17698398972327,-2.42127602276314,
7.55785582193789));
#402489=CARTESIAN_POINT('Ctrl Pts',(-1.16247826555639,-2.40061317846372,
7.59443891967696));
#402490=CARTESIAN_POINT('Ctrl Pts',(-1.15777732473869,-2.39723170731885,
7.58783901202978));
#402491=CARTESIAN_POINT('Ctrl Pts',(-1.15135951492375,-2.40278966514233,
7.58560008491213));
#402492=CARTESIAN_POINT('',(-1.22670887334885,-2.45714515960792,7.50366116523517));
#402493=CARTESIAN_POINT('Ctrl Pts',(-1.22670887334902,-2.45714515960826,
7.50366116523554));
#402494=CARTESIAN_POINT('Ctrl Pts',(-1.22744112877596,-2.45695037894576,
7.50350835821027));
#402495=CARTESIAN_POINT('Ctrl Pts',(-1.22810791225206,-2.45674750507575,
7.50345484956));
#402496=CARTESIAN_POINT('Ctrl Pts',(-1.22872922258755,-2.4565310808918,
7.50349758195598));
#402497=CARTESIAN_POINT('Ctrl Pts',(-1.22904800086723,-2.456420039235,7.50351950684424));
#402498=CARTESIAN_POINT('Ctrl Pts',(-1.22938627121607,-2.4562946080529,
7.50357029184313));
#402499=CARTESIAN_POINT('Ctrl Pts',(-1.22970913670001,-2.45616468988571,
7.50365515313924));
#402500=CARTESIAN_POINT('Ctrl Pts',(-1.23020583455546,-2.45596482313552,
7.50378570417639));
#402501=CARTESIAN_POINT('Ctrl Pts',(-1.23068078352655,-2.45574879222655,
7.50400001621911));
#402502=CARTESIAN_POINT('Ctrl Pts',(-1.23109689307203,-2.45553097357611,
7.50428903009635));
#402503=CARTESIAN_POINT('Ctrl Pts',(-1.23114307803023,-2.45550679738171,
7.50432110841318));
#402504=CARTESIAN_POINT('Ctrl Pts',(-1.23118856822059,-2.45548260283481,
7.50435406373354));
#402505=CARTESIAN_POINT('Ctrl Pts',(-1.23123333517556,-2.45545841200071,
7.50438785222352));
#402506=CARTESIAN_POINT('Ctrl Pts',(-1.23150665895339,-2.45531071533093,
7.50459414719561));
#402507=CARTESIAN_POINT('Ctrl Pts',(-1.23175712916614,-2.45516035184146,
7.50483629897752));
#402508=CARTESIAN_POINT('Ctrl Pts',(-1.23197582773583,-2.45501421023925,
7.5050991045531));
#402509=CARTESIAN_POINT('Ctrl Pts',(-1.23245829874675,-2.45469180718625,
7.50567888004914));
#402510=CARTESIAN_POINT('Ctrl Pts',(-1.23280544219417,-2.4543776796122,
7.50637912803145));
#402511=CARTESIAN_POINT('Ctrl Pts',(-1.23304326177524,-2.45408853757672,
7.50710440483569));
#402512=CARTESIAN_POINT('Ctrl Pts',(-1.2331015798579,-2.45401763420935,
7.50728225710685));
#402513=CARTESIAN_POINT('Ctrl Pts',(-1.23315459764784,-2.45394691453314,
7.50746498566954));
#402514=CARTESIAN_POINT('Ctrl Pts',(-1.23320141086251,-2.45387827926384,
7.50764697238949));
#402515=CARTESIAN_POINT('Ctrl Pts',(-1.23345306582123,-2.45350931494506,
7.50862528291181));
#402516=CARTESIAN_POINT('Ctrl Pts',(-1.23355168239988,-2.4531694251973,
7.50965856837421));
#402517=CARTESIAN_POINT('Ctrl Pts',(-1.23356355484103,-2.45285929503312,
7.51067959873201));
#402518=CARTESIAN_POINT('Ctrl Pts',(-1.23357008826037,-2.45268863001259,
7.51124147302578));
#402519=CARTESIAN_POINT('Ctrl Pts',(-1.23354992032897,-2.45252691886292,
7.51180065547252));
#402520=CARTESIAN_POINT('Ctrl Pts',(-1.23351138288628,-2.4523742709769,
7.512351757165));
#402521=CARTESIAN_POINT('Ctrl Pts',(-1.23337822067029,-2.45184681172299,
7.51425603304535));
#402522=CARTESIAN_POINT('Ctrl Pts',(-1.23300397343626,-2.45136616066922,
7.51626900505179));
#402523=CARTESIAN_POINT('Ctrl Pts',(-1.23244762843881,-2.45094509166342,
7.51827788969243));
#402524=CARTESIAN_POINT('Ctrl Pts',(-1.2324175179962,-2.45092230261311,
7.51838661432545));
#402525=CARTESIAN_POINT('Ctrl Pts',(-1.23238686422244,-2.45089968883142,
7.51849533314856));
#402526=CARTESIAN_POINT('Ctrl Pts',(-1.23235567333046,-2.45087725266273,
7.51860402984325));
#402527=CARTESIAN_POINT('Ctrl Pts',(-1.16019063469236,-2.40916067500414,
7.57603338728984));
#402528=CARTESIAN_POINT('Ctrl Pts',(-1.18240010893415,-2.42518305082722,
7.55196141284921));
#402529=CARTESIAN_POINT('Ctrl Pts',(-1.20457181916034,-2.44117710944838,
7.52783573083105));
#402530=CARTESIAN_POINT('Ctrl Pts',(-1.22670887339983,-2.45714515963799,
7.50366116530176));
#402531=CARTESIAN_POINT('Origin',(-4.00899494394867E-16,-8.32476377985987E-16,
7.49482233047033));
#402532=CARTESIAN_POINT('Origin',(-1.15251174268203,-2.4830672429437,7.49482233047033));
#402533=CARTESIAN_POINT('Origin',(0.,0.,7.50366116523517));
#402534=CARTESIAN_POINT('Origin',(-1.22276082553376,-2.4492370676478,7.49482233047033));
#402535=CARTESIAN_POINT('Ctrl Pts',(-1.14781185363497,-2.49159037923024,
7.51860402984325));
#402536=CARTESIAN_POINT('Ctrl Pts',(-1.14743505922584,-2.49919000501071,
7.51860402984325));
#402537=CARTESIAN_POINT('Ctrl Pts',(-1.14051133179101,-2.50234567996836,
7.51860402984325));
#402538=CARTESIAN_POINT('Ctrl Pts',(-1.14767194603031,-2.49441217208215,
7.51041458714365));
#402539=CARTESIAN_POINT('Ctrl Pts',(-1.14579474478775,-2.49993761154477,
7.51004642900441));
#402540=CARTESIAN_POINT('Ctrl Pts',(-1.14050942230919,-2.50234655026605,
7.50729136483009));
#402541=CARTESIAN_POINT('Ctrl Pts',(-1.15026273737235,-2.49551287068815,
7.50215815450138));
#402542=CARTESIAN_POINT('Ctrl Pts',(-1.14913464688838,-2.49841553779643,
7.49877163671531));
#402543=CARTESIAN_POINT('Ctrl Pts',(-1.1460051215579,-2.49986811991121,
7.49481588533171));
#402544=CARTESIAN_POINT('Ctrl Pts',(-1.15623273862022,-2.49108406635796,
7.50366171572174));
#402545=CARTESIAN_POINT('Ctrl Pts',(-1.15777435337956,-2.49440544953232,
7.50000045605858));
#402546=CARTESIAN_POINT('Ctrl Pts',(-1.15777435337945,-2.49440544953238,
7.49482233047317));
#402547=CARTESIAN_POINT('Origin',(-1.13532718937378,-2.49097138142305,7.51860402984325));
#402548=CARTESIAN_POINT('Origin',(-1.13532718937378,-2.49097138142305,9.));
#402549=CARTESIAN_POINT('Origin',(-1.13532718937378,-2.49097138142305,8.75721825406948));
#402550=CARTESIAN_POINT('Ctrl Pts',(-1.14864017147867,-2.4749118318261,
8.78942910404913));
#402551=CARTESIAN_POINT('Ctrl Pts',(-1.14838393822148,-2.48047840826226,
8.79672699501689));
#402552=CARTESIAN_POINT('Ctrl Pts',(-1.13954364374201,-2.48171237726442,
8.79893251111267));
#402553=CARTESIAN_POINT('Ctrl Pts',(-1.14809480925301,-2.48589263319865,
8.78111911759581));
#402554=CARTESIAN_POINT('Ctrl Pts',(-1.14778360579387,-2.49249153178346,
8.78644465894816));
#402555=CARTESIAN_POINT('Ctrl Pts',(-1.14018209782489,-2.49530801689311,
8.78817647674132));
#402556=CARTESIAN_POINT('Ctrl Pts',(-1.14775492647408,-2.49273613052926,
8.7678092393203));
#402557=CARTESIAN_POINT('Ctrl Pts',(-1.14738247379801,-2.50052561162717,
8.76988516158372));
#402558=CARTESIAN_POINT('Ctrl Pts',(-1.14056970501268,-2.50380014394096,
8.77093053738833));
#402559=CARTESIAN_POINT('Ctrl Pts',(-1.14782119896262,-2.49140174220956,
8.75371302330492));
#402560=CARTESIAN_POINT('Ctrl Pts',(-1.14745864888062,-2.49900008142322,
8.7530082828756));
#402561=CARTESIAN_POINT('Ctrl Pts',(-1.14049364879242,-2.50214385512781,
8.75267964240737));
#402562=CARTESIAN_POINT('Origin',(-1.13602277023073,-2.47696606283122,8.78727029226991));
#402563=CARTESIAN_POINT('Ctrl Pts',(-1.1520537178733,-2.40618167532514,
8.85049129520029));
#402564=CARTESIAN_POINT('Ctrl Pts',(-1.15176404759815,-2.41201410220894,
8.85711686593484));
#402565=CARTESIAN_POINT('Ctrl Pts',(-1.14335314149693,-2.41354949162872,
8.85933012996512));
#402566=CARTESIAN_POINT('Ctrl Pts',(-1.15086988603564,-2.430017785649,8.82945683644723));
#402567=CARTESIAN_POINT('Ctrl Pts',(-1.15057781132208,-2.43589862520228,
8.8360746990239));
#402568=CARTESIAN_POINT('Ctrl Pts',(-1.14213547634264,-2.43740162972406,
8.8382956714852));
#402569=CARTESIAN_POINT('Ctrl Pts',(-1.14968781879481,-2.45381836632827,
8.80838214965003));
#402570=CARTESIAN_POINT('Ctrl Pts',(-1.14939459141806,-2.45972241442018,
8.81501364461993));
#402571=CARTESIAN_POINT('Ctrl Pts',(-1.14092032599118,-2.46121761944619,
8.81722098428721));
#402572=CARTESIAN_POINT('Ctrl Pts',(-1.14850738206911,-2.47758611705879,
8.78727029226991));
#402573=CARTESIAN_POINT('Ctrl Pts',(-1.14821410598632,-2.48349114583244,
8.79393457792714));
#402574=CARTESIAN_POINT('Ctrl Pts',(-1.13970751364641,-2.48500021903835,
8.79610912703474));
#402575=CARTESIAN_POINT('Origin',(-1.13956910603492,-2.40556162109758,8.85049129520029));
#402576=CARTESIAN_POINT('Ctrl Pts',(-1.1629348420194,-2.40094160211229,
8.85049129520029));
#402577=CARTESIAN_POINT('Ctrl Pts',(-1.16767542343879,-2.40435158745378,
8.85711686593484));
#402578=CARTESIAN_POINT('Ctrl Pts',(-1.17411995340352,-2.39873297591288,
8.85933012996512));
#402579=CARTESIAN_POINT('Ctrl Pts',(-1.15874091806867,-2.39792483730433,
8.86332496987231));
#402580=CARTESIAN_POINT('Ctrl Pts',(-1.16301882523356,-2.39617801027643,
8.86648636486737));
#402581=CARTESIAN_POINT('Ctrl Pts',(-1.16237727570637,-2.39030736158171,
8.87206031107457));
#402582=CARTESIAN_POINT('Ctrl Pts',(-1.15231172640009,-2.40098674855131,
8.86341338519876));
#402583=CARTESIAN_POINT('Ctrl Pts',(-1.1482529364075,-2.40322274820032,
8.86654584966058));
#402584=CARTESIAN_POINT('Ctrl Pts',(-1.144090293775,-2.39900415138368,8.87215952290714));
#402585=CARTESIAN_POINT('Ctrl Pts',(-1.1520537178733,-2.40618167532514,
8.85049129520029));
#402586=CARTESIAN_POINT('Ctrl Pts',(-1.15176404759815,-2.41201410220893,
8.85711686593484));
#402587=CARTESIAN_POINT('Ctrl Pts',(-1.14335314149693,-2.41354949162871,
8.85933012996512));
#402588=CARTESIAN_POINT('Origin',(-1.17023409226484,-2.39079414204317,8.85049129520029));
#402589=CARTESIAN_POINT('Ctrl Pts',(-1.22097218676269,-2.44268890636151,
8.78727029226991));
#402590=CARTESIAN_POINT('Ctrl Pts',(-1.22577177880956,-2.446141339107,8.79393457792714));
#402591=CARTESIAN_POINT('Ctrl Pts',(-1.23225539332379,-2.44043150916128,
8.79610912703474));
#402592=CARTESIAN_POINT('Ctrl Pts',(-1.20165382071392,-2.42879285876314,
8.80838214965003));
#402593=CARTESIAN_POINT('Ctrl Pts',(-1.20645261566517,-2.43224471814342,
8.81501364461989));
#402594=CARTESIAN_POINT('Ctrl Pts',(-1.2129052320992,-2.42655151572731,
8.81722098428722));
#402595=CARTESIAN_POINT('Ctrl Pts',(-1.18230877056806,-2.41487761681456,
8.82945683644724));
#402596=CARTESIAN_POINT('Ctrl Pts',(-1.18708870167944,-2.41831590709611,
8.8360746990239));
#402597=CARTESIAN_POINT('Ctrl Pts',(-1.19352750769642,-2.41265253181512,
8.8382956714852));
#402598=CARTESIAN_POINT('Ctrl Pts',(-1.1629348420194,-2.40094160211229,
8.85049129520029));
#402599=CARTESIAN_POINT('Ctrl Pts',(-1.16767542343879,-2.40435158745378,
8.85711686593484));
#402600=CARTESIAN_POINT('Ctrl Pts',(-1.17411995340352,-2.39873297591288,
8.85933012996512));
#402601=CARTESIAN_POINT('Origin',(-1.22827143700814,-2.43254144629239,8.78727029226991));
#402602=CARTESIAN_POINT('Ctrl Pts',(-1.23220537088867,-2.45076911469362,
8.75374538247848));
#402603=CARTESIAN_POINT('Ctrl Pts',(-1.2383665202337,-2.45521710492921,
8.75304829418601));
#402604=CARTESIAN_POINT('Ctrl Pts',(-1.24516238600019,-2.45174048995301,
8.75272238421917));
#402605=CARTESIAN_POINT('Ctrl Pts',(-1.23327692917392,-2.45153990633562,
8.76769408445022));
#402606=CARTESIAN_POINT('Ctrl Pts',(-1.2395935243215,-2.45609926821132,
8.76974318093971));
#402607=CARTESIAN_POINT('Ctrl Pts',(-1.2463957417661,-2.45282082420285,
8.7707786988043));
#402608=CARTESIAN_POINT('Ctrl Pts',(-1.22778473182153,-2.44758926748178,
8.78108014887988));
#402609=CARTESIAN_POINT('Ctrl Pts',(-1.23313559499255,-2.45145624312503,
8.78639403366323));
#402610=CARTESIAN_POINT('Ctrl Pts',(-1.2400770538556,-2.44729232374767,
8.78812224174741));
#402611=CARTESIAN_POINT('Ctrl Pts',(-1.21878423279646,-2.44111504248424,
8.78944554828686));
#402612=CARTESIAN_POINT('Ctrl Pts',(-1.22329046309831,-2.44437852315427,
8.79673892988686));
#402613=CARTESIAN_POINT('Ctrl Pts',(-1.22976192881266,-2.43824470820559,
8.79894799272499));
#402614=CARTESIAN_POINT('Origin',(-1.2396549235759,-2.44072979259361,8.75721825406948));
#402615=CARTESIAN_POINT('Origin',(-1.2396549235759,-2.44072979259361,9.));
#402616=CARTESIAN_POINT('Origin',(-1.2396549235759,-2.44072979259361,7.51860402984325));
#402617=CARTESIAN_POINT('Ctrl Pts',(-1.22670852196932,-2.45714445578104,
7.50366195182966));
#402618=CARTESIAN_POINT('Ctrl Pts',(-1.22834420829888,-2.46042079855024,
7.50000065167735));
#402619=CARTESIAN_POINT('Ctrl Pts',(-1.22834420829899,-2.46042079855019,
7.49482233047108));
#402620=CARTESIAN_POINT('Ctrl Pts',(-1.23389951291487,-2.45523567375381,
7.50215800491337));
#402621=CARTESIAN_POINT('Ctrl Pts',(-1.2368736819588,-2.45616250473761,
7.49877273257265));
#402622=CARTESIAN_POINT('Ctrl Pts',(-1.2399623021127,-2.45462056378711,
7.49481816995647));
#402623=CARTESIAN_POINT('Ctrl Pts',(-1.23464359386723,-2.45252341272685,
7.51043025814041));
#402624=CARTESIAN_POINT('Ctrl Pts',(-1.24013580471421,-2.45450542609691,
7.51006209594514));
#402625=CARTESIAN_POINT('Ctrl Pts',(-1.24531770572932,-2.45187353095617,
7.50731281821699));
#402626=CARTESIAN_POINT('Ctrl Pts',(-1.23235444642809,-2.45087637001726,
7.51860402984325));
#402627=CARTESIAN_POINT('Ctrl Pts',(-1.23853109166802,-2.45532047521073,
7.51860402984325));
#402628=CARTESIAN_POINT('Ctrl Pts',(-1.24531544834109,-2.4518746774913,
7.51860402984325));
#402629=CARTESIAN_POINT('Origin',(0.,0.,7.5));
#402630=CARTESIAN_POINT('Origin',(-1.00671661105392,-2.47051810124199,7.5));
#402631=CARTESIAN_POINT('',(-1.00671661105392,-2.47051810124199,7.59394543036555));
#402632=CARTESIAN_POINT('',(-1.00671661105392,-2.47051810124199,8.85049129520029));
#402633=CARTESIAN_POINT('',(-1.00671661105392,-2.47051810124199,7.5));
#402634=CARTESIAN_POINT('',(-1.0619599528811,-2.51589809662205,8.78727029226991));
#402635=CARTESIAN_POINT('Ctrl Pts',(-1.00671661105392,-2.47051810124199,
8.85049129520029));
#402636=CARTESIAN_POINT('Ctrl Pts',(-1.0251578255121,-2.48566675444137,
8.82945686509571));
#402637=CARTESIAN_POINT('Ctrl Pts',(-1.04357162487512,-2.50079288733603,
8.80838212259896));
#402638=CARTESIAN_POINT('Ctrl Pts',(-1.0619599528811,-2.51589809662205,
8.78727029226991));
#402639=CARTESIAN_POINT('',(-1.07279542170604,-2.52479896157614,8.75721825406948));
#402640=CARTESIAN_POINT('Origin',(-1.04018760906769,-2.49801332713423,8.75937679713151));
#402641=CARTESIAN_POINT('',(-1.07279542170604,-2.52479896157614,7.51860402984325));
#402642=CARTESIAN_POINT('',(-1.07279542170604,-2.52479896157614,7.5));
#402643=CARTESIAN_POINT('Ctrl Pts',(-1.07279542170604,-2.52479896157614,
7.51860402984325));
#402644=CARTESIAN_POINT('Ctrl Pts',(-1.06428584617822,-2.51780871650105,
7.52834476460825));
#402645=CARTESIAN_POINT('Ctrl Pts',(-1.05577074635675,-2.51081393345974,
7.53807742314407));
#402646=CARTESIAN_POINT('Ctrl Pts',(-1.04724993675614,-2.50381446008393,
7.54780169004674));
#402647=CARTESIAN_POINT('Ctrl Pts',(-1.03375343485924,-2.49272767254591,
7.5632044032688));
#402648=CARTESIAN_POINT('Ctrl Pts',(-1.02024259070161,-2.48162910346635,
7.57858609112102));
#402649=CARTESIAN_POINT('Ctrl Pts',(-1.00671661105392,-2.47051810124199,
7.59394543036555));
#402650=CARTESIAN_POINT('Origin',(-0.964311324797644,-2.74827339692444,
7.5));
#402651=CARTESIAN_POINT('',(-0.985816687379938,-2.56001274842385,8.75721825406948));
#402652=CARTESIAN_POINT('',(-0.987408162934497,-2.54608077127965,8.78727029226991));
#402653=CARTESIAN_POINT('Origin',(-0.991447921482891,-2.51071621691815,
8.75658640621013));
#402654=CARTESIAN_POINT('',(-0.995522110700908,-2.47505025214475,8.85049129520029));
#402655=CARTESIAN_POINT('Ctrl Pts',(-0.987408162934496,-2.54608077127965,
8.78727029226991));
#402656=CARTESIAN_POINT('Ctrl Pts',(-0.990108975883482,-2.52243751507743,
8.80838212259897));
#402657=CARTESIAN_POINT('Ctrl Pts',(-0.992813529975814,-2.49876150843588,
8.82945686509571));
#402658=CARTESIAN_POINT('Ctrl Pts',(-0.995522110700908,-2.47505025214475,
8.85049129520029));
#402659=CARTESIAN_POINT('',(-0.995522110700908,-2.47505025214475,7.59394543036555));
#402660=CARTESIAN_POINT('',(-0.995522110700908,-2.47505025214475,7.5));
#402661=CARTESIAN_POINT('',(-0.985816687379938,-2.56001274842385,7.51860402984325));
#402662=CARTESIAN_POINT('Ctrl Pts',(-0.995522110700909,-2.47505025214475,
7.59394543036555));
#402663=CARTESIAN_POINT('Ctrl Pts',(-0.993535462378759,-2.49244162139227,
7.57858609112103));
#402664=CARTESIAN_POINT('Ctrl Pts',(-0.991551037104199,-2.50981352980177,
7.56320440326857));
#402665=CARTESIAN_POINT('Ctrl Pts',(-0.989568718370413,-2.52716699728824,
7.54780169004651));
#402666=CARTESIAN_POINT('Ctrl Pts',(-0.988317211822469,-2.53812284299494,
7.53807742314383));
#402667=CARTESIAN_POINT('Ctrl Pts',(-0.987066543906777,-2.54907134720939,
7.52834476460825));
#402668=CARTESIAN_POINT('Ctrl Pts',(-0.985816687379938,-2.56001274842385,
7.51860402984325));
#402669=CARTESIAN_POINT('',(-0.985816687379938,-2.56001274842385,7.5));
#402670=CARTESIAN_POINT('Origin',(-1.0023526893204,-2.47583052179233,7.5));
#402671=CARTESIAN_POINT('Ctrl Pts',(-0.995522110700909,-2.47505025214475,
8.85049129520029));
#402672=CARTESIAN_POINT('Ctrl Pts',(-0.995544090074723,-2.47485784194232,
8.85097269580139));
#402673=CARTESIAN_POINT('Ctrl Pts',(-0.995574149201944,-2.47466881399357,
8.85143669361005));
#402674=CARTESIAN_POINT('Ctrl Pts',(-0.995614535645016,-2.47447460147567,
8.8519052845931));
#402675=CARTESIAN_POINT('Ctrl Pts',(-0.995693528966451,-2.47409473410718,
8.85282181883899));
#402676=CARTESIAN_POINT('Ctrl Pts',(-0.995810192031023,-2.4737048441739,
8.85372622499635));
#402677=CARTESIAN_POINT('Ctrl Pts',(-0.995981127120858,-2.47330323361082,
8.8546225773507));
#402678=CARTESIAN_POINT('Ctrl Pts',(-0.996123031361399,-2.47296983078522,
8.85536669723986));
#402679=CARTESIAN_POINT('Ctrl Pts',(-0.996302341696657,-2.47262826201747,
8.85610498449051));
#402680=CARTESIAN_POINT('Ctrl Pts',(-0.996535657640079,-2.47228124643154,
8.8568133821837));
#402681=CARTESIAN_POINT('Ctrl Pts',(-0.996747392225165,-2.47196632924231,
8.85745625420284));
#402682=CARTESIAN_POINT('Ctrl Pts',(-0.997005762944949,-2.47164264202971,
8.85808743050666));
#402683=CARTESIAN_POINT('Ctrl Pts',(-0.997338632360855,-2.47131662869161,
8.8586680450841));
#402684=CARTESIAN_POINT('Ctrl Pts',(-0.997492211093629,-2.47116621320451,
8.85893592806395));
#402685=CARTESIAN_POINT('Ctrl Pts',(-0.997661876290801,-2.47101538495295,
8.85919241173848));
#402686=CARTESIAN_POINT('Ctrl Pts',(-0.997851775008971,-2.47086552375508,
8.85943017985534));
#402687=CARTESIAN_POINT('Ctrl Pts',(-0.998108194494538,-2.4706631667743,
8.8597512372));
#402688=CARTESIAN_POINT('Ctrl Pts',(-0.998408429108412,-2.47045792534336,
8.86004599534705));
#402689=CARTESIAN_POINT('Ctrl Pts',(-0.998754749324536,-2.47026086344443,
8.86026130871721));
#402690=CARTESIAN_POINT('Ctrl Pts',(-0.99888154691946,-2.47018871352746,
8.86034014101235));
#402691=CARTESIAN_POINT('Ctrl Pts',(-0.999016420825366,-2.47011656559295,
8.86040910639692));
#402692=CARTESIAN_POINT('Ctrl Pts',(-0.999155855142562,-2.47004668187887,
8.86046313645506));
#402693=CARTESIAN_POINT('Ctrl Pts',(-0.999373441226795,-2.46993762892833,
8.86054744990829));
#402694=CARTESIAN_POINT('Ctrl Pts',(-0.999608137853282,-2.46983124429506,
8.86059655985668));
#402695=CARTESIAN_POINT('Ctrl Pts',(-0.99984477226485,-2.46973408392438,
8.86059725258816));
#402696=CARTESIAN_POINT('Ctrl Pts',(-1.00008195339645,-2.46963669907444,
8.86059794692011));
#402697=CARTESIAN_POINT('Ctrl Pts',(-1.00032472074388,-2.46954995882129,
8.86056369958366));
#402698=CARTESIAN_POINT('Ctrl Pts',(-1.00055856750402,-2.46947505032681,
8.86048590497774));
#402699=CARTESIAN_POINT('Ctrl Pts',(-1.00061959454596,-2.46945550144004,
8.86046560290182));
#402700=CARTESIAN_POINT('Ctrl Pts',(-1.00068083560641,-2.46943659030202,
8.86044257503091));
#402701=CARTESIAN_POINT('Ctrl Pts',(-1.00074038860052,-2.46941886991778,
8.86041778462583));
#402702=CARTESIAN_POINT('Ctrl Pts',(-1.00114110635174,-2.46929963372096,
8.86025097596201));
#402703=CARTESIAN_POINT('Ctrl Pts',(-1.00151926053775,-2.4692186285124,
8.8599848982295));
#402704=CARTESIAN_POINT('Ctrl Pts',(-1.00186203918154,-2.46916993407642,
8.85968173251461));
#402705=CARTESIAN_POINT('Ctrl Pts',(-1.00204334944522,-2.46914417750964,
8.85952137522076));
#402706=CARTESIAN_POINT('Ctrl Pts',(-1.00221823035513,-2.46912677532505,
8.85934740853961));
#402707=CARTESIAN_POINT('Ctrl Pts',(-1.0023840617725,-2.4691164260195,8.8591675900182));
#402708=CARTESIAN_POINT('Ctrl Pts',(-1.00304996111069,-2.46907486817829,
8.85844552518695));
#402709=CARTESIAN_POINT('Ctrl Pts',(-1.00360738943727,-2.46914166499387,
8.85759444184123));
#402710=CARTESIAN_POINT('Ctrl Pts',(-1.00405699467321,-2.46923695081302,
8.85683498915137));
#402711=CARTESIAN_POINT('Ctrl Pts',(-1.00410404466375,-2.46924692222023,
8.85675551444997));
#402712=CARTESIAN_POINT('Ctrl Pts',(-1.00414990599218,-2.46925722395855,
8.85667699793651));
#402713=CARTESIAN_POINT('Ctrl Pts',(-1.00419457359943,-2.46926777628528,
8.85659965593547));
#402714=CARTESIAN_POINT('Ctrl Pts',(-1.0047974992414,-2.46941021212986,
8.85555568965886));
#402715=CARTESIAN_POINT('Ctrl Pts',(-1.00535637758334,-2.46963417619404,
8.85434650606346));
#402716=CARTESIAN_POINT('Ctrl Pts',(-1.00587628317203,-2.4699350068609,
8.85297329937117));
#402717=CARTESIAN_POINT('Ctrl Pts',(-1.00616869838735,-2.47010420578113,
8.85220095427747));
#402718=CARTESIAN_POINT('Ctrl Pts',(-1.00644874670489,-2.47029806236456,
8.85137579139183));
#402719=CARTESIAN_POINT('Ctrl Pts',(-1.00671661105392,-2.47051810124199,
8.85049129520029));
#402720=CARTESIAN_POINT('Origin',(-1.0023526893204,-2.47583052179233,7.59394543036555));
#402721=CARTESIAN_POINT('Ctrl Pts',(-0.995585924237762,-2.47449162041812,
7.59443877723642));
#402722=CARTESIAN_POINT('Ctrl Pts',(-0.996243142267619,-2.46873825113483,
7.58783886950016));
#402723=CARTESIAN_POINT('Ctrl Pts',(-1.00467227562429,-2.46772390780438,
7.58559994247159));
#402724=CARTESIAN_POINT('Ctrl Pts',(-0.991998190294734,-2.50589909453893,
7.56670252222135));
#402725=CARTESIAN_POINT('Ctrl Pts',(-0.992654458457976,-2.50015404050765,
7.56004874999025));
#402726=CARTESIAN_POINT('Ctrl Pts',(-1.00113098469781,-2.49911247430166,
7.55786368756704));
#402727=CARTESIAN_POINT('Ctrl Pts',(-0.988417156086389,-2.53724791833978,
7.53888913333556));
#402728=CARTESIAN_POINT('Ctrl Pts',(-0.989077324483434,-2.53146872117112,
7.53222002137274));
#402729=CARTESIAN_POINT('Ctrl Pts',(-0.997595022281296,-2.5304434071001,
7.53005029815327));
#402730=CARTESIAN_POINT('Ctrl Pts',(-0.98484298365694,-2.56853667326526,
7.51101258149734));
#402731=CARTESIAN_POINT('Ctrl Pts',(-0.985511154494509,-2.56268742172586,
7.5043616886572));
#402732=CARTESIAN_POINT('Ctrl Pts',(-0.994064645198984,-2.56171516748281,
7.50217374673251));
#402733=CARTESIAN_POINT('',(-0.99425302963394,-2.56004646606291,7.50366116523517));
#402734=CARTESIAN_POINT('Ctrl Pts',(-0.985816687379937,-2.56001274842385,
7.51860402984325));
#402735=CARTESIAN_POINT('Ctrl Pts',(-0.985766567259559,-2.5604515062606,
7.51734760759493));
#402736=CARTESIAN_POINT('Ctrl Pts',(-0.985780388944966,-2.56085473922179,
7.51608817408572));
#402737=CARTESIAN_POINT('Ctrl Pts',(-0.985871466452295,-2.56122106239948,
7.51481005913119));
#402738=CARTESIAN_POINT('Ctrl Pts',(-0.985953966634802,-2.56155288668741,
7.51365231206383));
#402739=CARTESIAN_POINT('Ctrl Pts',(-0.986099730040565,-2.56185495396782,
7.51247773061042));
#402740=CARTESIAN_POINT('Ctrl Pts',(-0.986339490022423,-2.56210598981959,
7.51129758471022));
#402741=CARTESIAN_POINT('Ctrl Pts',(-0.98663748429825,-2.56241799871396,
7.50983079813402));
#402742=CARTESIAN_POINT('Ctrl Pts',(-0.987080589722761,-2.56263222255328,
7.50839324291155));
#402743=CARTESIAN_POINT('Ctrl Pts',(-0.987707923004627,-2.5626760041041,
7.50715379678855));
#402744=CARTESIAN_POINT('Ctrl Pts',(-0.987997732904675,-2.56269622991904,
7.50658120839351));
#402745=CARTESIAN_POINT('Ctrl Pts',(-0.988368720848104,-2.5626734770026,
7.50598221009429));
#402746=CARTESIAN_POINT('Ctrl Pts',(-0.988810665406192,-2.5625855830101,
7.50545747549611));
#402747=CARTESIAN_POINT('Ctrl Pts',(-0.989046500701851,-2.56253868005513,
7.50517746087247));
#402748=CARTESIAN_POINT('Ctrl Pts',(-0.989305138541066,-2.56247291741204,
7.50491486231392));
#402749=CARTESIAN_POINT('Ctrl Pts',(-0.989579318718269,-2.56238842000836,
7.50468370960993));
#402750=CARTESIAN_POINT('Ctrl Pts',(-0.989989304568424,-2.56226206973668,
7.50433806340447));
#402751=CARTESIAN_POINT('Ctrl Pts',(-0.990446172564147,-2.56208950838183,
7.50405484070984));
#402752=CARTESIAN_POINT('Ctrl Pts',(-0.990918900363643,-2.56188168744652,
7.50385766036131));
#402753=CARTESIAN_POINT('Ctrl Pts',(-0.990969451253942,-2.56185946422776,
7.50383657498791));
#402754=CARTESIAN_POINT('Ctrl Pts',(-0.9910201669494,-2.56183686084833,
7.50381643264937));
#402755=CARTESIAN_POINT('Ctrl Pts',(-0.991070997752494,-2.56181390761953,
7.50379723213559));
#402756=CARTESIAN_POINT('Ctrl Pts',(-0.991410309991077,-2.56166068730881,
7.50366906242519));
#402757=CARTESIAN_POINT('Ctrl Pts',(-0.991761836329731,-2.56148788948195,
7.50358235568538));
#402758=CARTESIAN_POINT('Ctrl Pts',(-0.992096660797257,-2.56131318891303,
7.5035341175365));
#402759=CARTESIAN_POINT('Ctrl Pts',(-0.992598692191497,-2.56105124518222,
7.50346178989176));
#402760=CARTESIAN_POINT('Ctrl Pts',(-0.993127626184824,-2.56074810754123,
7.50346967198527));
#402761=CARTESIAN_POINT('Ctrl Pts',(-0.99363771872217,-2.56043454298073,
7.50354272648692));
#402762=CARTESIAN_POINT('Ctrl Pts',(-0.993847530341072,-2.5603055673866,
7.50357277531559));
#402763=CARTESIAN_POINT('Ctrl Pts',(-0.994053949759997,-2.56017511988167,
7.50361331098761));
#402764=CARTESIAN_POINT('Ctrl Pts',(-0.994253029634453,-2.56004646606423,
7.50366116523659));
#402765=CARTESIAN_POINT('',(-1.00345144303437,-2.47854446470827,7.57603338622103));
#402766=CARTESIAN_POINT('Origin',(-1.00677029912175,-2.48673450035405,7.58486873427628));
#402767=CARTESIAN_POINT('Ctrl Pts',(-0.994253029622211,-2.56004646611904,
7.50366116529969));
#402768=CARTESIAN_POINT('Ctrl Pts',(-0.997314994686491,-2.5329235575592,
7.52783573079709));
#402769=CARTESIAN_POINT('Ctrl Pts',(-1.00038100552661,-2.50575750849375,
7.55196141284068));
#402770=CARTESIAN_POINT('Ctrl Pts',(-1.00345144254827,-2.47854446586211,
7.57603338728831));
#402771=CARTESIAN_POINT('Ctrl Pts',(-0.995580073096921,-2.47609196989964,
7.59639677331372));
#402772=CARTESIAN_POINT('Ctrl Pts',(-0.994718951965595,-2.45697504293775,
7.59974925422226));
#402773=CARTESIAN_POINT('Ctrl Pts',(-1.00739967866913,-2.47130674194168,
7.59639677331372));
#402774=CARTESIAN_POINT('Ctrl Pts',(-0.994780473004169,-2.47227415065623,
7.58707626057422));
#402775=CARTESIAN_POINT('Ctrl Pts',(-0.998585879238811,-2.46652642806453,
7.58811717123965));
#402776=CARTESIAN_POINT('Ctrl Pts',(-1.00531808064709,-2.4680079461374,
7.58707626057422));
#402777=CARTESIAN_POINT('Ctrl Pts',(-0.999909163054398,-2.47553331782441,
7.5801537675693));
#402778=CARTESIAN_POINT('Ctrl Pts',(-1.00117949275385,-2.47293270359068,
7.58208760766041));
#402779=CARTESIAN_POINT('Ctrl Pts',(-1.00390123521108,-2.47391710692992,
7.58015376756931));
#402780=CARTESIAN_POINT('Ctrl Pts',(-1.00345144272362,-2.47854446394126,
7.57603338509286));
#402781=CARTESIAN_POINT('Ctrl Pts',(-1.00345144272362,-2.47854446394126,
7.57603338509286));
#402782=CARTESIAN_POINT('Ctrl Pts',(-1.00345144272362,-2.47854446394126,
7.57603338509286));
#402783=CARTESIAN_POINT('Origin',(-1.00676500980816,-2.48673664175991,7.58486873427621));
#402784=CARTESIAN_POINT('Ctrl Pts',(-1.07944577964472,-2.5302619405081,
7.51098857897448));
#402785=CARTESIAN_POINT('Ctrl Pts',(-1.07489655658137,-2.52652495221648,
7.50433767179956));
#402786=CARTESIAN_POINT('Ctrl Pts',(-1.06807576525986,-2.53177708100687,
7.50214974420965));
#402787=CARTESIAN_POINT('Ctrl Pts',(-1.05510423513016,-2.51026642356291,
7.53887321589169));
#402788=CARTESIAN_POINT('Ctrl Pts',(-1.0506095198325,-2.50657421102301,
7.53220407452063));
#402789=CARTESIAN_POINT('Ctrl Pts',(-1.04377751552323,-2.51176329928973,
7.53003438070911));
#402790=CARTESIAN_POINT('Ctrl Pts',(-1.03071594587089,-2.49023250784913,
7.56669465659233));
#402791=CARTESIAN_POINT('Ctrl Pts',(-1.02624779350501,-2.48656211559887,
7.56004085833301));
#402792=CARTESIAN_POINT('Ctrl Pts',(-1.0194340624728,-2.49171087462867,
7.55785582193789));
#402793=CARTESIAN_POINT('Ctrl Pts',(-1.00628201485164,-2.4701610994206,
7.59443891967696));
#402794=CARTESIAN_POINT('Ctrl Pts',(-1.00180738422113,-2.46648538555856,
7.58783901202978));
#402795=CARTESIAN_POINT('Ctrl Pts',(-0.995046660904368,-2.47162073347496,
7.58560008491213));
#402796=CARTESIAN_POINT('',(-1.06675863750382,-2.53069219871727,7.50366116523517));
#402797=CARTESIAN_POINT('Ctrl Pts',(-1.06675863750396,-2.53069219871762,
7.50366116523554));
#402798=CARTESIAN_POINT('Ctrl Pts',(-1.06750186807349,-2.53054473401916,
7.50350835821027));
#402799=CARTESIAN_POINT('Ctrl Pts',(-1.06818027974491,-2.53038499793927,
7.50345484956));
#402800=CARTESIAN_POINT('Ctrl Pts',(-1.06881417987675,-2.53020882591189,
7.50349758195598));
#402801=CARTESIAN_POINT('Ctrl Pts',(-1.06913941765565,-2.53011843659659,
7.50351950684424));
#402802=CARTESIAN_POINT('Ctrl Pts',(-1.0694850293952,-2.53001493618197,
7.50357029184312));
#402803=CARTESIAN_POINT('Ctrl Pts',(-1.06981555540293,-2.52990597100817,
7.50365515313924));
#402804=CARTESIAN_POINT('Ctrl Pts',(-1.07032403824601,-2.52973833844651,
7.50378570417639));
#402805=CARTESIAN_POINT('Ctrl Pts',(-1.07081185253136,-2.52955318148127,
7.50400001621911));
#402806=CARTESIAN_POINT('Ctrl Pts',(-1.071241062824,-2.52936247059273,7.50428903009634));
#402807=CARTESIAN_POINT('Ctrl Pts',(-1.07128870186434,-2.52934130315135,
7.50432110841318));
#402808=CARTESIAN_POINT('Ctrl Pts',(-1.07133564874018,-2.52932007288123,
7.50435406373354));
#402809=CARTESIAN_POINT('Ctrl Pts',(-1.0713818736287,-2.52929879997845,
7.50438785222352));
#402810=CARTESIAN_POINT('Ctrl Pts',(-1.07166409879164,-2.52916891868189,
7.50459414719561));
#402811=CARTESIAN_POINT('Ctrl Pts',(-1.07192368820832,-2.52903491181197,
7.50483629897752));
#402812=CARTESIAN_POINT('Ctrl Pts',(-1.07215130076294,-2.52890308253883,
7.5050991045531));
#402813=CARTESIAN_POINT('Ctrl Pts',(-1.07265343691995,-2.52861225392127,
7.50567888004914));
#402814=CARTESIAN_POINT('Ctrl Pts',(-1.07301999334671,-2.52832101331306,
7.50637912803145));
#402815=CARTESIAN_POINT('Ctrl Pts',(-1.07327584969576,-2.52804770250378,
7.50710440483569));
#402816=CARTESIAN_POINT('Ctrl Pts',(-1.07333859075201,-2.52798068126736,
7.50728225710685));
#402817=CARTESIAN_POINT('Ctrl Pts',(-1.07339603063643,-2.52791350375377,
7.50746498566954));
#402818=CARTESIAN_POINT('Ctrl Pts',(-1.07344714514513,-2.52784800883596,
7.50764697238949));
#402819=CARTESIAN_POINT('Ctrl Pts',(-1.07372192267682,-2.52749592618251,
7.50862528291182));
#402820=CARTESIAN_POINT('Ctrl Pts',(-1.07384211344803,-2.52716305316058,
7.50965856837423));
#402821=CARTESIAN_POINT('Ctrl Pts',(-1.07387383160382,-2.52685432086199,
7.51067959873204));
#402822=CARTESIAN_POINT('Ctrl Pts',(-1.07389128614496,-2.52668442508867,
7.5112414730258));
#402823=CARTESIAN_POINT('Ctrl Pts',(-1.07388152051967,-2.5265217540281,
7.51180065547253));
#402824=CARTESIAN_POINT('Ctrl Pts',(-1.07385284243993,-2.5263669506711,
7.51235175716501));
#402825=CARTESIAN_POINT('Ctrl Pts',(-1.07375374825042,-2.52583204340632,
7.51425603304536));
#402826=CARTESIAN_POINT('Ctrl Pts',(-1.07341106536622,-2.52532840179909,
7.5162690050518));
#402827=CARTESIAN_POINT('Ctrl Pts',(-1.07288284142306,-2.52487255277834,
7.51827788969243));
#402828=CARTESIAN_POINT('Ctrl Pts',(-1.07285425294505,-2.5248478813679,
7.51838661432545));
#402829=CARTESIAN_POINT('Ctrl Pts',(-1.07282511102272,-2.52482335005462,
7.51849533314856));
#402830=CARTESIAN_POINT('Ctrl Pts',(-1.07279542170604,-2.52479896157613,
7.51860402984325));
#402831=CARTESIAN_POINT('Ctrl Pts',(-1.00345144418694,-2.47854446519997,
7.57603338728985));
#402832=CARTESIAN_POINT('Ctrl Pts',(-1.02458872953834,-2.49595688723385,
7.55196141284922));
#402833=CARTESIAN_POINT('Ctrl Pts',(-1.04569014275369,-2.51333863069778,
7.52783573083105));
#402834=CARTESIAN_POINT('Ctrl Pts',(-1.06675863755276,-2.53069219875054,
7.50366116530176));
#402835=CARTESIAN_POINT('Origin',(-3.46738858720988E-16,-8.56451684780639E-16,
7.49482233047033));
#402836=CARTESIAN_POINT('Origin',(-0.991053119217889,-2.55180719586894,
7.49482233047033));
#402837=CARTESIAN_POINT('Origin',(0.,0.,7.50366116523517));
#402838=CARTESIAN_POINT('Origin',(-1.06332537456791,-2.52254740248821,7.49482233047033));
#402839=CARTESIAN_POINT('Ctrl Pts',(-0.985816807380133,-2.56001169753273,
7.51860402984325));
#402840=CARTESIAN_POINT('Ctrl Pts',(-0.98495387744,-2.56757156776631,7.51860402984325));
#402841=CARTESIAN_POINT('Ctrl Pts',(-0.977842190757029,-2.57027715431148,
7.51860402984325));
#402842=CARTESIAN_POINT('Ctrl Pts',(-0.985496394341891,-2.56281872879758,
7.51041458714367));
#402843=CARTESIAN_POINT('Ctrl Pts',(-0.983269033888756,-2.56821254295568,
7.51004642900442));
#402844=CARTESIAN_POINT('Ctrl Pts',(-0.977840229438281,-2.57027790048012,
7.50729136483011));
#402845=CARTESIAN_POINT('Ctrl Pts',(-0.988011340623444,-2.56408315847147,
7.50215815450137));
#402846=CARTESIAN_POINT('Ctrl Pts',(-0.986699593402196,-2.56690758473339,
7.4987716367153));
#402847=CARTESIAN_POINT('Ctrl Pts',(-0.983483430761509,-2.56815667298608,
7.49481588533169));
#402848=CARTESIAN_POINT('Ctrl Pts',(-0.994252830331148,-2.560045952888,
7.50366171572174));
#402849=CARTESIAN_POINT('Ctrl Pts',(-0.995578475927007,-2.56345928352117,
7.50000045605858));
#402850=CARTESIAN_POINT('Ctrl Pts',(-0.995578475926891,-2.56345928352122,
7.49482233047317));
#402851=CARTESIAN_POINT('Origin',(-0.973397453526316,-2.55859407633733,
7.51860402984325));
#402852=CARTESIAN_POINT('Origin',(-0.973397453526316,-2.55859407633733,
9.));
#402853=CARTESIAN_POINT('Origin',(-0.973397453526316,-2.55859407633733,
8.75721825406948));
#402854=CARTESIAN_POINT('Ctrl Pts',(-0.987712021557121,-2.54342048849949,
8.78942910404912));
#402855=CARTESIAN_POINT('Ctrl Pts',(-0.987099662981832,-2.54895921088619,
8.7967269950169));
#402856=CARTESIAN_POINT('Ctrl Pts',(-0.978198471170077,-2.54962424495468,
8.79893251111267));
#402857=CARTESIAN_POINT('Ctrl Pts',(-0.986464237477146,-2.55434378716014,
8.78111911759585));
#402858=CARTESIAN_POINT('Ctrl Pts',(-0.985730880534933,-2.56090918872596,
8.78644465894816));
#402859=CARTESIAN_POINT('Ctrl Pts',(-0.97796453785879,-2.56323285677716,
8.78817647674132));
#402860=CARTESIAN_POINT('Ctrl Pts',(-0.985686588644423,-2.56115144742717,
8.76780923932029));
#402861=CARTESIAN_POINT('Ctrl Pts',(-0.984815827444824,-2.56890106107585,
8.76988516158371));
#402862=CARTESIAN_POINT('Ctrl Pts',(-0.977807256217964,-2.57173236991701,
8.77093053738832));
#402863=CARTESIAN_POINT('Ctrl Pts',(-0.985838219522211,-2.55982404684425,
8.75371302330492));
#402864=CARTESIAN_POINT('Ctrl Pts',(-0.984989587073333,-2.56738354579156,
8.7530082828756));
#402865=CARTESIAN_POINT('Ctrl Pts',(-0.977837475051993,-2.57007461118809,
8.75267964240738));
#402866=CARTESIAN_POINT('Origin',(-0.974988929080874,-2.54466209919314,
8.78727029226991));
#402867=CARTESIAN_POINT('Ctrl Pts',(-0.995522110700908,-2.47505025214475,
8.85049129520029));
#402868=CARTESIAN_POINT('Ctrl Pts',(-0.994859350710948,-2.48085213644374,
8.85711686593484));
#402869=CARTESIAN_POINT('Ctrl Pts',(-0.986367352980499,-2.48184548263714,
8.85933012996512));
#402870=CARTESIAN_POINT('Ctrl Pts',(-0.9928135263408,-2.49876154025725,
8.8294568364472));
#402871=CARTESIAN_POINT('Ctrl Pts',(-0.992145265042209,-2.5046115837038,
8.83607469902387));
#402872=CARTESIAN_POINT('Ctrl Pts',(-0.983623977915089,-2.50557059788234,
8.83829567148519));
#402873=CARTESIAN_POINT('Ctrl Pts',(-0.990108979344094,-2.52243748478279,
8.80838214965003));
#402874=CARTESIAN_POINT('Ctrl Pts',(-0.989438080774434,-2.52831061523216,
8.81501364461996));
#402875=CARTESIAN_POINT('Ctrl Pts',(-0.980885428519782,-2.52925980014899,
8.81722098428721));
#402876=CARTESIAN_POINT('Ctrl Pts',(-0.987408162934496,-2.54608077127965,
8.78727029226991));
#402877=CARTESIAN_POINT('Ctrl Pts',(-0.986737152926361,-2.55195487727524,
8.79393457792714));
#402878=CARTESIAN_POINT('Ctrl Pts',(-0.978151351640473,-2.5529158306859,
8.79610912703474));
#402879=CARTESIAN_POINT('Origin',(-0.983102876847287,-2.47363158005824,
8.85049129520029));
#402880=CARTESIAN_POINT('Ctrl Pts',(-1.00671661105392,-2.47051810124199,
8.85049129520029));
#402881=CARTESIAN_POINT('Ctrl Pts',(-1.0112289739294,-2.47422481049725,
8.85711686593484));
#402882=CARTESIAN_POINT('Ctrl Pts',(-1.01802024859356,-2.46903064544887,
8.85933012996512));
#402883=CARTESIAN_POINT('Ctrl Pts',(-1.00272458875463,-2.46723882907077,
8.86332496987232));
#402884=CARTESIAN_POINT('Ctrl Pts',(-1.00710562609237,-2.46576967753948,
8.86648636486737));
#402885=CARTESIAN_POINT('Ctrl Pts',(-1.0068415284508,-2.45986998650278,
8.87206031107456));
#402886=CARTESIAN_POINT('Ctrl Pts',(-0.996112429222693,-2.46988252956822,
8.86341338519877));
#402887=CARTESIAN_POINT('Ctrl Pts',(-0.991918717460054,-2.47185388754845,
8.8665458496606));
#402888=CARTESIAN_POINT('Ctrl Pts',(-0.988034913849338,-2.46737725686223,
8.87215952290715));
#402889=CARTESIAN_POINT('Ctrl Pts',(-0.995522110700908,-2.47505025214475,
8.85049129520029));
#402890=CARTESIAN_POINT('Ctrl Pts',(-0.994859350710948,-2.48085213644373,
8.85711686593484));
#402891=CARTESIAN_POINT('Ctrl Pts',(-0.986367352980499,-2.48184548263714,
8.85933012996512));
#402892=CARTESIAN_POINT('Origin',(-1.01465101420576,-2.46085915478681,8.85049129520029));
#402893=CARTESIAN_POINT('Ctrl Pts',(-1.0619599528811,-2.51589809662205,
8.78727029226991));
#402894=CARTESIAN_POINT('Ctrl Pts',(-1.06652848552588,-2.51965094689244,
8.79393457792714));
#402895=CARTESIAN_POINT('Ctrl Pts',(-1.07336460881941,-2.51436825501292,
8.79610912703474));
#402896=CARTESIAN_POINT('Ctrl Pts',(-1.04357160131374,-2.50079286798139,
8.80838214965003));
#402897=CARTESIAN_POINT('Ctrl Pts',(-1.0481393752363,-2.50454509499456,
8.81501364461993));
#402898=CARTESIAN_POINT('Ctrl Pts',(-1.05494349880899,-2.49927701042777,
8.81722098428722));
#402899=CARTESIAN_POINT('Ctrl Pts',(-1.02515785026093,-2.48566677477146,
8.82945683644728));
#402900=CARTESIAN_POINT('Ctrl Pts',(-1.02970766847652,-2.48940425195465,
8.83607469902396));
#402901=CARTESIAN_POINT('Ctrl Pts',(-1.03649609897604,-2.48416504840346,
8.8382956714852));
#402902=CARTESIAN_POINT('Ctrl Pts',(-1.00671661105392,-2.47051810124199,
8.85049129520029));
#402903=CARTESIAN_POINT('Ctrl Pts',(-1.0112289739294,-2.47422481049725,
8.85711686593484));
#402904=CARTESIAN_POINT('Ctrl Pts',(-1.01802024859356,-2.46903064544887,
8.85933012996512));
#402905=CARTESIAN_POINT('Origin',(-1.06989435603295,-2.50623915016687,8.78727029226991));
#402906=CARTESIAN_POINT('Ctrl Pts',(-1.07265235650021,-2.52468141587758,
8.75374538247848));
#402907=CARTESIAN_POINT('Ctrl Pts',(-1.07851586339026,-2.52951501343405,
8.75304829418602));
#402908=CARTESIAN_POINT('Ctrl Pts',(-1.08552051380799,-2.5264809541508,
8.75272238421917));
#402909=CARTESIAN_POINT('Ctrl Pts',(-1.07367232836399,-2.52551927882054,
8.76769408445019));
#402910=CARTESIAN_POINT('Ctrl Pts',(-1.07968382607105,-2.53047397863889,
8.76974318093968));
#402911=CARTESIAN_POINT('Ctrl Pts',(-1.08668211825917,-2.52763809011329,
8.7707786988043));
#402912=CARTESIAN_POINT('Ctrl Pts',(-1.06844453362053,-2.52122487068539,
8.78108014887992));
#402913=CARTESIAN_POINT('Ctrl Pts',(-1.07353664488914,-2.5254267321929,
8.78639403366326));
#402914=CARTESIAN_POINT('Ctrl Pts',(-1.08073062501099,-2.5217161088308,
8.78812224174741));
#402915=CARTESIAN_POINT('Ctrl Pts',(-1.05987733210579,-2.51418728372498,
8.78944554828685));
#402916=CARTESIAN_POINT('Ctrl Pts',(-1.06416521194977,-2.51773277439068,
8.79673892988685));
#402917=CARTESIAN_POINT('Ctrl Pts',(-1.07101637621682,-2.51202619025459,
8.79894799272499));
#402918=CARTESIAN_POINT('Origin',(-1.08072982485788,-2.51514001512096,8.75721825406948));
#402919=CARTESIAN_POINT('Origin',(-1.08072982485788,-2.51514001512096,9.));
#402920=CARTESIAN_POINT('Origin',(-1.08072982485788,-2.51514001512096,7.51860402984325));
#402921=CARTESIAN_POINT('Ctrl Pts',(-1.06675833194057,-2.53069147382351,
7.50366195182966));
#402922=CARTESIAN_POINT('Ctrl Pts',(-1.06818074157519,-2.53406588377806,
7.50000065167735));
#402923=CARTESIAN_POINT('Ctrl Pts',(-1.0681807415753,-2.53406588377801,
7.49482233047108));
#402924=CARTESIAN_POINT('Ctrl Pts',(-1.07405684430838,-2.52924734196545,
7.50215800491337));
#402925=CARTESIAN_POINT('Ctrl Pts',(-1.07696552033801,-2.5303628243405,
7.49877273257269));
#402926=CARTESIAN_POINT('Ctrl Pts',(-1.08014658708644,-2.52902194004573,
7.49481816995647));
#402927=CARTESIAN_POINT('Ctrl Pts',(-1.07497317162725,-2.52658832699994,
7.51043025814042));
#402928=CARTESIAN_POINT('Ctrl Pts',(-1.0803271101054,-2.52891815526811,
7.51006209594511));
#402929=CARTESIAN_POINT('Ctrl Pts',(-1.08566699044975,-2.52662367317616,
7.50731281821699));
#402930=CARTESIAN_POINT('Ctrl Pts',(-1.07279425387576,-2.52479800213625,
7.51860402984325));
#402931=CARTESIAN_POINT('Ctrl Pts',(-1.07867347373825,-2.52962871545823,
7.51860402984325));
#402932=CARTESIAN_POINT('Ctrl Pts',(-1.0856646642408,-2.52662467272425,
7.51860402984325));
#402933=CARTESIAN_POINT('Origin',(0.,0.,7.5));
#402934=CARTESIAN_POINT('Origin',(-0.84636156559358,-2.52994271156921,7.5));
#402935=CARTESIAN_POINT('',(-0.84636156559358,-2.52994271156921,7.59394543036555));
#402936=CARTESIAN_POINT('',(-0.84636156559358,-2.52994271156921,8.85049129520029));
#402937=CARTESIAN_POINT('',(-0.84636156559358,-2.52994271156921,7.5));
#402938=CARTESIAN_POINT('',(-0.89858389776343,-2.57876892194511,8.78727029226991));
#402939=CARTESIAN_POINT('Ctrl Pts',(-0.846361565593581,-2.52994271156921,
8.85049129520029));
#402940=CARTESIAN_POINT('Ctrl Pts',(-0.863794313055953,-2.54624177290296,
8.82945686509571));
#402941=CARTESIAN_POINT('Ctrl Pts',(-0.881201144631286,-2.56251660371118,
8.80838212259896));
#402942=CARTESIAN_POINT('Ctrl Pts',(-0.89858389776343,-2.57876892194511,
8.78727029226991));
#402943=CARTESIAN_POINT('',(-0.908826823579936,-2.58834572998875,8.75721825406948));
#402944=CARTESIAN_POINT('Origin',(-0.878002168679522,-2.55952593977548,
8.75937679713084));
#402945=CARTESIAN_POINT('',(-0.908826823579936,-2.58834572998875,7.51860402984325));
#402946=CARTESIAN_POINT('',(-0.908826823579936,-2.58834572998875,7.5));
#402947=CARTESIAN_POINT('Ctrl Pts',(-0.908826823579935,-2.58834572998875,
7.51860402984325));
#402948=CARTESIAN_POINT('Ctrl Pts',(-0.900782598427366,-2.58082463674586,
7.52834476460825));
#402949=CARTESIAN_POINT('Ctrl Pts',(-0.892733151079904,-2.57329866091778,
7.53807742314407));
#402950=CARTESIAN_POINT('Ctrl Pts',(-0.884678306195408,-2.56576763856519,
7.54780169004674));
#402951=CARTESIAN_POINT('Ctrl Pts',(-0.871919867225587,-2.55383890617572,
7.5632044032688));
#402952=CARTESIAN_POINT('Ctrl Pts',(-0.85914787030871,-2.54189749753934,
7.57858609112103));
#402953=CARTESIAN_POINT('Ctrl Pts',(-0.84636156559358,-2.52994271156921,
7.59394543036555));
#402954=CARTESIAN_POINT('Origin',(-0.786247562650692,-2.80441041318874,
7.5));
#402955=CARTESIAN_POINT('',(-0.819770641322262,-2.61791441969279,8.75721825406948));
#402956=CARTESIAN_POINT('',(-0.822251471860003,-2.60411303347872,8.78727029226991));
#402957=CARTESIAN_POINT('Origin',(-0.828548745068065,-2.56907996760912,
8.75658640621115));
#402958=CARTESIAN_POINT('',(-0.834899689636828,-2.53374831658168,8.85049129520029));
#402959=CARTESIAN_POINT('Ctrl Pts',(-0.822251471860003,-2.60411303347872,
8.78727029226991));
#402960=CARTESIAN_POINT('Ctrl Pts',(-0.826461564325062,-2.58069139656185,
8.80838212259896));
#402961=CARTESIAN_POINT('Ctrl Pts',(-0.830677488574736,-2.55723731619085,
8.82945686509571));
#402962=CARTESIAN_POINT('Ctrl Pts',(-0.834899689636828,-2.53374831658168,
8.85049129520029));
#402963=CARTESIAN_POINT('',(-0.834899689636828,-2.53374831658168,7.59394543036555));
#402964=CARTESIAN_POINT('',(-0.834899689636828,-2.53374831658168,7.5));
#402965=CARTESIAN_POINT('',(-0.819770641322262,-2.61791441969279,7.51860402984325));
#402966=CARTESIAN_POINT('Ctrl Pts',(-0.834899689636828,-2.53374831658168,
7.59394543036555));
#402967=CARTESIAN_POINT('Ctrl Pts',(-0.831802854243269,-2.55097666840084,
7.57858609112103));
#402968=CARTESIAN_POINT('Ctrl Pts',(-0.828709484189984,-2.56818574179751,
7.56320440326857));
#402969=CARTESIAN_POINT('Ctrl Pts',(-0.825619397863354,-2.58537654712652,
7.54780169004651));
#402970=CARTESIAN_POINT('Ctrl Pts',(-0.823668519225333,-2.59622969857337,
7.53807742314383));
#402971=CARTESIAN_POINT('Ctrl Pts',(-0.821718947867528,-2.60707557734321,
7.52834476460825));
#402972=CARTESIAN_POINT('Ctrl Pts',(-0.819770641322262,-2.61791441969279,
7.51860402984324));
#402973=CARTESIAN_POINT('',(-0.819770641322262,-2.61791441969279,7.5));
#402974=CARTESIAN_POINT('Origin',(-0.841666242052004,-2.53496461975634,
7.5));
#402975=CARTESIAN_POINT('Ctrl Pts',(-0.834899689636828,-2.53374831658168,
8.85049129520029));
#402976=CARTESIAN_POINT('Ctrl Pts',(-0.834933951615658,-2.53355770992996,
8.85097269580138));
#402977=CARTESIAN_POINT('Ctrl Pts',(-0.834976060045437,-2.5333709962543,
8.85143669361005));
#402978=CARTESIAN_POINT('Ctrl Pts',(-0.835028806748976,-2.53317977033515,
8.8519052845931));
#402979=CARTESIAN_POINT('Ctrl Pts',(-0.835131975956022,-2.53280574456438,
8.85282181883899));
#402980=CARTESIAN_POINT('Ctrl Pts',(-0.835273379657609,-2.53242413032999,
8.85372622499635));
#402981=CARTESIAN_POINT('Ctrl Pts',(-0.835469694820092,-2.5320342967677,
8.8546225773507));
#402982=CARTESIAN_POINT('Ctrl Pts',(-0.83563266869553,-2.53171067078987,
8.85536669723986));
#402983=CARTESIAN_POINT('Ctrl Pts',(-0.835833495004561,-2.53138129226441,
8.85610498449051));
#402984=CARTESIAN_POINT('Ctrl Pts',(-0.836088564940283,-2.53104993826304,
8.85681338218371));
#402985=CARTESIAN_POINT('Ctrl Pts',(-0.836320041307544,-2.53074923398639,
8.85745625420284));
#402986=CARTESIAN_POINT('Ctrl Pts',(-0.836598619887889,-2.53044276569274,
8.85808743050665));
#402987=CARTESIAN_POINT('Ctrl Pts',(-0.836951693134167,-2.53013874920071,
8.8586680450841));
#402988=CARTESIAN_POINT('Ctrl Pts',(-0.837114593476311,-2.52999848258155,
8.85893592806395));
#402989=CARTESIAN_POINT('Ctrl Pts',(-0.837293573677397,-2.52985883470932,
8.85919241173848));
#402990=CARTESIAN_POINT('Ctrl Pts',(-0.837492683868199,-2.52972144827,8.85943017985534));
#402991=CARTESIAN_POINT('Ctrl Pts',(-0.837761541568706,-2.52953593590618,
8.8597512372));
#402992=CARTESIAN_POINT('Ctrl Pts',(-0.838074309181994,-2.52935035226354,
8.86004599534706));
#402993=CARTESIAN_POINT('Ctrl Pts',(-0.838432543645307,-2.52917588406184,
8.86026130871721));
#402994=CARTESIAN_POINT('Ctrl Pts',(-0.838563703382024,-2.52911200633442,
8.86034014101235));
#402995=CARTESIAN_POINT('Ctrl Pts',(-0.838702922709061,-2.52904864803639,
8.86040910639693));
#402996=CARTESIAN_POINT('Ctrl Pts',(-0.838846548008433,-2.52898784149327,
8.86046313645507));
#402997=CARTESIAN_POINT('Ctrl Pts',(-0.83907067408525,-2.52889295339199,
8.8605474499083));
#402998=CARTESIAN_POINT('Ctrl Pts',(-0.839311704589203,-2.52880182440185,
8.86059655985668));
#402999=CARTESIAN_POINT('Ctrl Pts',(-0.839554077896316,-2.52872002487638,
8.86059725258815));
#403000=CARTESIAN_POINT('Ctrl Pts',(-0.839797011182598,-2.52863803636133,
8.86059794692011));
#403001=CARTESIAN_POINT('Ctrl Pts',(-0.840044837205576,-2.52856702848269,
8.86056369958366));
#403002=CARTESIAN_POINT('Ctrl Pts',(-0.84028300290619,-2.52850725650911,
8.86048590497774));
#403003=CARTESIAN_POINT('Ctrl Pts',(-0.840345157063002,-2.52849165780363,
8.86046560290182));
#403004=CARTESIAN_POINT('Ctrl Pts',(-0.840407483937903,-2.52847670924879,
8.86044257503091));
#403005=CARTESIAN_POINT('Ctrl Pts',(-0.840468049922912,-2.52846284084641,
8.86041778462583));
#403006=CARTESIAN_POINT('Ctrl Pts',(-0.840875583845895,-2.52836952370761,
8.86025097596201));
#403007=CARTESIAN_POINT('Ctrl Pts',(-0.841258151095109,-2.52831291335483,
8.8599848982295));
#403008=CARTESIAN_POINT('Ctrl Pts',(-0.841603345326632,-2.5282862808699,
8.85968173251461));
#403009=CARTESIAN_POINT('Ctrl Pts',(-0.841785933297837,-2.52827219381123,
8.85952137522076));
#403010=CARTESIAN_POINT('Ctrl Pts',(-0.841961569857954,-2.52826603203966,
8.85934740853961));
#403011=CARTESIAN_POINT('Ctrl Pts',(-0.842127723639171,-2.52826632885326,
8.8591675900182));
#403012=CARTESIAN_POINT('Ctrl Pts',(-0.842794917435792,-2.52826752071417,
8.85844552518694));
#403013=CARTESIAN_POINT('Ctrl Pts',(-0.843346920779428,-2.52836989484404,
8.8575944418412));
#403014=CARTESIAN_POINT('Ctrl Pts',(-0.843789497269798,-2.52849379119463,
8.85683498915134));
#403015=CARTESIAN_POINT('Ctrl Pts',(-0.843835811720827,-2.52850675661776,
8.85675551444995));
#403016=CARTESIAN_POINT('Ctrl Pts',(-0.843880918787595,-2.52851997553546,
8.8566769979365));
#403017=CARTESIAN_POINT('Ctrl Pts',(-0.843924818530555,-2.52853336804471,
8.85659965593547));
#403018=CARTESIAN_POINT('Ctrl Pts',(-0.844517379501239,-2.5287141408181,
8.85555568965886));
#403019=CARTESIAN_POINT('Ctrl Pts',(-0.845060760140823,-2.52897345218239,
8.85434650606346));
#403020=CARTESIAN_POINT('Ctrl Pts',(-0.845560323240718,-2.52930697522583,
8.85297329937117));
#403021=CARTESIAN_POINT('Ctrl Pts',(-0.845841297045581,-2.5294945616159,
8.85220095427747));
#403022=CARTESIAN_POINT('Ctrl Pts',(-0.846108349539873,-2.52970596265749,
8.85137579139183));
#403023=CARTESIAN_POINT('Ctrl Pts',(-0.84636156559358,-2.52994271156921,
8.85049129520029));
#403024=CARTESIAN_POINT('Origin',(-0.841666242052004,-2.53496461975634,
7.59394543036555));
#403025=CARTESIAN_POINT('Ctrl Pts',(-0.83499916371954,-2.53319492117119,
7.59443877723642));
#403026=CARTESIAN_POINT('Ctrl Pts',(-0.836023651060078,-2.52749548090589,
7.58783886950016));
#403027=CARTESIAN_POINT('Ctrl Pts',(-0.844500455058569,-2.52702327808101,
7.58559994247159));
#403028=CARTESIAN_POINT('Ctrl Pts',(-0.829406517384719,-2.56430799836504,
7.56670252222137));
#403029=CARTESIAN_POINT('Ctrl Pts',(-0.830429524050224,-2.55861679540901,
7.56004874999028));
#403030=CARTESIAN_POINT('Ctrl Pts',(-0.838955367733715,-2.55812046211334,
7.55786368756704));
#403031=CARTESIAN_POINT('Ctrl Pts',(-0.823824314758165,-2.59536297499574,
7.53888913333558));
#403032=CARTESIAN_POINT('Ctrl Pts',(-0.824853401202346,-2.5896379489419,
7.53222002137275));
#403033=CARTESIAN_POINT('Ctrl Pts',(-0.833419290574643,-2.58916047226024,
7.53005029815327));
#403034=CARTESIAN_POINT('Ctrl Pts',(-0.818252808438304,-2.62635844580471,
7.51101258149734));
#403035=CARTESIAN_POINT('Ctrl Pts',(-0.819294369280078,-2.62056402203247,
7.5043616886572));
#403036=CARTESIAN_POINT('Ctrl Pts',(-0.827892578463771,-2.62014178942107,
7.50217374673251));
#403037=CARTESIAN_POINT('',(-0.828187489909756,-2.6184885863594,7.50366116523517));
#403038=CARTESIAN_POINT('Ctrl Pts',(-0.819770641322261,-2.61791441969279,
7.51860402984325));
#403039=CARTESIAN_POINT('Ctrl Pts',(-0.819692512867927,-2.61834906484738,
7.51734760759493));
#403040=CARTESIAN_POINT('Ctrl Pts',(-0.819680470930672,-2.61875235488163,
7.51608817408572));
#403041=CARTESIAN_POINT('Ctrl Pts',(-0.819747890902916,-2.619123760765,
7.51481005913118));
#403042=CARTESIAN_POINT('Ctrl Pts',(-0.819808961524827,-2.61946018908918,
7.51365231206383));
#403043=CARTESIAN_POINT('Ctrl Pts',(-0.819935071926935,-2.61977097483344,
7.51247773061042));
#403044=CARTESIAN_POINT('Ctrl Pts',(-0.820158255373951,-2.6200368563799,
7.51129758471022));
#403045=CARTESIAN_POINT('Ctrl Pts',(-0.82043564691008,-2.62036731677734,
7.50983079813402));
#403046=CARTESIAN_POINT('Ctrl Pts',(-0.820864116558463,-2.62060949033283,
7.50839324291155));
#403047=CARTESIAN_POINT('Ctrl Pts',(-0.821487355823228,-2.62069337531113,
7.50715379678855));
#403048=CARTESIAN_POINT('Ctrl Pts',(-0.821775274405341,-2.62073212775401,
7.50658120839351));
#403049=CARTESIAN_POINT('Ctrl Pts',(-0.822146957898613,-2.62073319086503,
7.50598221009429));
#403050=CARTESIAN_POINT('Ctrl Pts',(-0.822593625821642,-2.62067379294522,
7.50545747549611));
#403051=CARTESIAN_POINT('Ctrl Pts',(-0.822831981651036,-2.62064209637667,
7.50517746087247));
#403052=CARTESIAN_POINT('Ctrl Pts',(-0.823094301518081,-2.62059303983323,
7.50491486231392));
#403053=CARTESIAN_POINT('Ctrl Pts',(-0.823373332129946,-2.62052628282281,
7.50468370960992));
#403054=CARTESIAN_POINT('Ctrl Pts',(-0.8237905709099,-2.62042646003491,
7.50433806340447));
#403055=CARTESIAN_POINT('Ctrl Pts',(-0.82425755626529,-2.62028352485886,
7.50405484070984));
#403056=CARTESIAN_POINT('Ctrl Pts',(-0.82474262792786,-2.62010641868806,
7.50385766036131));
#403057=CARTESIAN_POINT('Ctrl Pts',(-0.824794498802451,-2.62008747993595,
7.50383657498791));
#403058=CARTESIAN_POINT('Ctrl Pts',(-0.824846558500569,-2.62006817236335,
7.50381643264937));
#403059=CARTESIAN_POINT('Ctrl Pts',(-0.824898755484747,-2.62004852303516,
7.50379723213559));
#403060=CARTESIAN_POINT('Ctrl Pts',(-0.825247187428958,-2.61991735734176,
7.50366906242519));
#403061=CARTESIAN_POINT('Ctrl Pts',(-0.825609062713827,-2.61976743691642,
7.50358235568538));
#403062=CARTESIAN_POINT('Ctrl Pts',(-0.825954392352455,-2.61961454756584,
7.5035341175365));
#403063=CARTESIAN_POINT('Ctrl Pts',(-0.82647217506181,-2.61938530728838,
7.50346178989176));
#403064=CARTESIAN_POINT('Ctrl Pts',(-0.827019444398862,-2.61911668139349,
7.50346967198527));
#403065=CARTESIAN_POINT('Ctrl Pts',(-0.827548579046752,-2.6188364428261,
7.50354272648692));
#403066=CARTESIAN_POINT('Ctrl Pts',(-0.827766223079868,-2.61872117490273,
7.50357277531559));
#403067=CARTESIAN_POINT('Ctrl Pts',(-0.827980576188296,-2.61860422075377,
7.50361331098761));
#403068=CARTESIAN_POINT('Ctrl Pts',(-0.828187489910183,-2.61848858636075,
7.50366116523658));
#403069=CARTESIAN_POINT('',(-0.842588855338984,-2.53774338397764,7.57603338622103));
#403070=CARTESIAN_POINT('Origin',(-0.84537615509485,-2.546129232156,7.58486873427627));
#403071=CARTESIAN_POINT('Ctrl Pts',(-0.828187489894455,-2.61848858641467,
7.50366116529969));
#403072=CARTESIAN_POINT('Ctrl Pts',(-0.832980934541063,-2.59161758555462,
7.52783573079709));
#403073=CARTESIAN_POINT('Ctrl Pts',(-0.837781180672694,-2.56470379203952,
7.55196141284069));
#403074=CARTESIAN_POINT('Ctrl Pts',(-0.842588854779952,-2.53774338509797,
7.57603338728831));
#403075=CARTESIAN_POINT('Ctrl Pts',(-0.834890789857168,-2.53479160767929,
7.5963967733137));
#403076=CARTESIAN_POINT('Ctrl Pts',(-0.835239864301339,-2.51651730706895,
7.59959882295473));
#403077=CARTESIAN_POINT('Ctrl Pts',(-0.84687953098394,-2.53063208557011,
7.59642833564546));
#403078=CARTESIAN_POINT('Ctrl Pts',(-0.834337441147255,-2.53093040200112,
7.5870762605742));
#403079=CARTESIAN_POINT('Ctrl Pts',(-0.838432320957715,-2.52553186049669,
7.58809943920599));
#403080=CARTESIAN_POINT('Ctrl Pts',(-0.844958025991749,-2.52730092086952,
7.58710240504253));
#403081=CARTESIAN_POINT('Ctrl Pts',(-0.839246778196438,-2.53451146916045,
7.58015376756929));
#403082=CARTESIAN_POINT('Ctrl Pts',(-0.840659757860373,-2.53203502819294,
7.58205880659762));
#403083=CARTESIAN_POINT('Ctrl Pts',(-0.843257205617099,-2.53312146281555,
7.58020924244125));
#403084=CARTESIAN_POINT('Ctrl Pts',(-0.842588855078019,-2.5377433831923,
7.57603338509286));
#403085=CARTESIAN_POINT('Ctrl Pts',(-0.842588855078019,-2.5377433831923,
7.57603338509286));
#403086=CARTESIAN_POINT('Ctrl Pts',(-0.842588855078019,-2.5377433831923,
7.57603338509286));
#403087=CARTESIAN_POINT('Origin',(-0.84537073944863,-2.54613103027482,7.58486873427621));
#403088=CARTESIAN_POINT('Ctrl Pts',(-0.915113503383067,-2.59422357454067,
7.51098857897448));
#403089=CARTESIAN_POINT('Ctrl Pts',(-0.910813056848305,-2.59020279456988,
7.50433767179956));
#403090=CARTESIAN_POINT('Ctrl Pts',(-0.903669774527125,-2.59500712269797,
7.50214974420965));
#403091=CARTESIAN_POINT('Ctrl Pts',(-0.89210308835163,-2.57270957241784,
7.53887321589168));
#403092=CARTESIAN_POINT('Ctrl Pts',(-0.887854168798268,-2.56873696852669,
7.53220407452062));
#403093=CARTESIAN_POINT('Ctrl Pts',(-0.880703735547826,-2.57347766723606,
7.53003438070911));
#403094=CARTESIAN_POINT('Ctrl Pts',(-0.869048484835137,-2.55115425547473,
7.56669465659232));
#403095=CARTESIAN_POINT('Ctrl Pts',(-0.864824675606418,-2.54720512893398,
7.56004085833299));
#403096=CARTESIAN_POINT('Ctrl Pts',(-0.857695061991683,-2.55190675204006,
7.55785582193789));
#403097=CARTESIAN_POINT('Ctrl Pts',(-0.845950735501038,-2.52955859857208,
7.59443891967696));
#403098=CARTESIAN_POINT('Ctrl Pts',(-0.841720802274792,-2.52560374628955,
7.58783901202978));
#403099=CARTESIAN_POINT('Ctrl Pts',(-0.834644946718488,-2.53029538205276,
7.58560008491213));
#403100=CARTESIAN_POINT('',(-0.902424861598272,-2.59384008075032,7.50366116523517));
#403101=CARTESIAN_POINT('Ctrl Pts',(-0.902424861598394,-2.59384008075067,
7.50366116523554));
#403102=CARTESIAN_POINT('Ctrl Pts',(-0.903176013216671,-2.59374053798034,
7.50350835821027));
#403103=CARTESIAN_POINT('Ctrl Pts',(-0.903863265344334,-2.59362459608038,
7.50345484956));
#403104=CARTESIAN_POINT('Ctrl Pts',(-0.904507150440919,-2.59348940013822,
7.50349758195598));
#403105=CARTESIAN_POINT('Ctrl Pts',(-0.90483751124723,-2.5934200345935,
7.50351950684424));
#403106=CARTESIAN_POINT('Ctrl Pts',(-0.905189044184732,-2.59333889025176,
7.50357029184312));
#403107=CARTESIAN_POINT('Ctrl Pts',(-0.905525872513984,-2.59325132583262,
7.50365515313924));
#403108=CARTESIAN_POINT('Ctrl Pts',(-0.906044050879637,-2.59311661629765,
7.50378570417639));
#403109=CARTESIAN_POINT('Ctrl Pts',(-0.906542725945715,-2.59296309412583,
7.50400001621911));
#403110=CARTESIAN_POINT('Ctrl Pts',(-0.906983273268363,-2.59280027467113,
7.50428903009635));
#403111=CARTESIAN_POINT('Ctrl Pts',(-0.907032170631807,-2.59278220296432,
7.50432110841318));
#403112=CARTESIAN_POINT('Ctrl Pts',(-0.90708038127832,-2.59276402421073,
7.50435406373354));
#403113=CARTESIAN_POINT('Ctrl Pts',(-0.907127874152411,-2.59274575665419,
7.50438785222352));
#403114=CARTESIAN_POINT('Ctrl Pts',(-0.907417840976726,-2.59263422444096,
7.50459414719561));
#403115=CARTESIAN_POINT('Ctrl Pts',(-0.907685482888746,-2.59251712485355,
7.50483629897752));
#403116=CARTESIAN_POINT('Ctrl Pts',(-0.907921074119493,-2.59240014962423,
7.5050991045531));
#403117=CARTESIAN_POINT('Ctrl Pts',(-0.908440812037419,-2.59214209051931,
7.50567888004914));
#403118=CARTESIAN_POINT('Ctrl Pts',(-0.908825275184519,-2.59187493364706,
7.50637912803144));
#403119=CARTESIAN_POINT('Ctrl Pts',(-0.909098116932933,-2.59161857715671,
7.50710440483569));
#403120=CARTESIAN_POINT('Ctrl Pts',(-0.909165023146312,-2.59155571345589,
7.50728225710685));
#403121=CARTESIAN_POINT('Ctrl Pts',(-0.909226649092401,-2.59149235415174,
7.50746498566954));
#403122=CARTESIAN_POINT('Ctrl Pts',(-0.909281854854655,-2.59143026871808,
7.50764697238949));
#403123=CARTESIAN_POINT('Ctrl Pts',(-0.909578625839493,-2.59109651451309,
7.50862528291181));
#403124=CARTESIAN_POINT('Ctrl Pts',(-0.909719896913618,-2.59077202606364,
7.50965856837421));
#403125=CARTESIAN_POINT('Ctrl Pts',(-0.909771330447341,-2.5904659602779,
7.51067959873202));
#403126=CARTESIAN_POINT('Ctrl Pts',(-0.909799634385823,-2.59029753188995,
7.51124147302578));
#403127=CARTESIAN_POINT('Ctrl Pts',(-0.909800311195693,-2.59013456936876,
7.51180065547253));
#403128=CARTESIAN_POINT('Ctrl Pts',(-0.909781610323276,-2.58997824666098,
7.512351757165));
#403129=CARTESIAN_POINT('Ctrl Pts',(-0.909716991359532,-2.58943808943403,
7.51425603304535));
#403130=CARTESIAN_POINT('Ctrl Pts',(-0.909407280982637,-2.58891352684471,
7.51626900505179));
#403131=CARTESIAN_POINT('Ctrl Pts',(-0.908909348679264,-2.58842477099044,
7.51827788969243));
#403132=CARTESIAN_POINT('Ctrl Pts',(-0.908882399642043,-2.58839831859998,
7.51838661432545));
#403133=CARTESIAN_POINT('Ctrl Pts',(-0.908854889321556,-2.58837197055954,
7.51849533314856));
#403134=CARTESIAN_POINT('Ctrl Pts',(-0.908826823579939,-2.58834572998874,
7.51860402984325));
#403135=CARTESIAN_POINT('Ctrl Pts',(-0.84258885645768,-2.53774338454218,
7.57603338728984));
#403136=CARTESIAN_POINT('Ctrl Pts',(-0.862567095279249,-2.55647430140978,
7.55196141284921));
#403137=CARTESIAN_POINT('Ctrl Pts',(-0.882511501250651,-2.57517230440418,
7.52783573083105));
#403138=CARTESIAN_POINT('Ctrl Pts',(-0.902424861644981,-2.59384008078666,
7.50366116530176));
#403139=CARTESIAN_POINT('Origin',(-2.91153398701372E-16,-8.76907647894217E-16,
7.49482233047033));
#403140=CARTESIAN_POINT('Origin',(-0.825522045906653,-2.61006122566543,
7.49482233047033));
#403141=CARTESIAN_POINT('Origin',(0.,0.,7.50366116523517));
#403142=CARTESIAN_POINT('Origin',(-0.899520491555372,-2.58549204896708,
7.49482233047033));
#403143=CARTESIAN_POINT('Ctrl Pts',(-0.819770828406729,-2.61791337864929,
7.51860402984325));
#403144=CARTESIAN_POINT('Ctrl Pts',(-0.818425308899815,-2.62540242820759,
7.51860402984325));
#403145=CARTESIAN_POINT('Ctrl Pts',(-0.811154886414735,-2.62764680850481,
7.51860402984325));
#403146=CARTESIAN_POINT('Ctrl Pts',(-0.819271226580806,-2.62069411363351,
7.51041458714367));
#403147=CARTESIAN_POINT('Ctrl Pts',(-0.816702859618967,-2.62593413814771,
7.51004642900443));
#403148=CARTESIAN_POINT('Ctrl Pts',(-0.811152881318541,-2.62764742747825,
7.50729136483011));
#403149=CARTESIAN_POINT('Ctrl Pts',(-0.821699993348142,-2.62211707856253,
7.50215815450137));
#403150=CARTESIAN_POINT('Ctrl Pts',(-0.820209979640322,-2.62485165780475,
7.49877163671529));
#403151=CARTESIAN_POINT('Ctrl Pts',(-0.816920395591586,-2.62589211942377,
7.49481588533168));
#403152=CARTESIAN_POINT('Ctrl Pts',(-0.828187323895682,-2.61848806146948,
7.50366171572174));
#403153=CARTESIAN_POINT('Ctrl Pts',(-0.829291552965956,-2.62197931345374,
7.50000045605858));
#403154=CARTESIAN_POINT('Ctrl Pts',(-0.829291552965837,-2.62197931345377,
7.49482233047317));
#403155=CARTESIAN_POINT('Origin',(-0.807467818749214,-2.61570295937524,
7.51860402984325));
#403156=CARTESIAN_POINT('Origin',(-0.807467818749214,-2.61570295937524,
9.));
#403157=CARTESIAN_POINT('Origin',(-0.807467818749214,-2.61570295937524,
8.75721825406948));
#403158=CARTESIAN_POINT('Ctrl Pts',(-0.822725151075437,-2.60147768482362,
8.78942910404913));
#403159=CARTESIAN_POINT('Ctrl Pts',(-0.82175918349479,-2.60696579336252,
8.79672699501689));
#403160=CARTESIAN_POINT('Ctrl Pts',(-0.812833671257198,-2.60705915972975,
8.79893251111267));
#403161=CARTESIAN_POINT('Ctrl Pts',(-0.82078007255357,-2.6122985945952,
8.78111911759583));
#403162=CARTESIAN_POINT('Ctrl Pts',(-0.819627575649261,-2.61880352049878,
8.78644465894818));
#403163=CARTESIAN_POINT('Ctrl Pts',(-0.811728311833873,-2.620624823041,
8.78817647674133));
#403164=CARTESIAN_POINT('Ctrl Pts',(-0.819567853192924,-2.61904244366225,
8.7678092393203));
#403165=CARTESIAN_POINT('Ctrl Pts',(-0.818202361614366,-2.62672034503694,
8.7698851615837));
#403166=CARTESIAN_POINT('Ctrl Pts',(-0.811026787668476,-2.62909679595021,
8.77093053738833));
#403167=CARTESIAN_POINT('Ctrl Pts',(-0.819804219376154,-2.61772748538993,
8.75371302330492));
#403168=CARTESIAN_POINT('Ctrl Pts',(-0.81847299177316,-2.62521708046822,
8.7530082828756));
#403169=CARTESIAN_POINT('Ctrl Pts',(-0.811163157381088,-2.62744437939174,
8.75267964240738));
#403170=CARTESIAN_POINT('Origin',(-0.809948649286955,-2.60190157316117,
8.78727029226991));
#403171=CARTESIAN_POINT('Ctrl Pts',(-0.834899689636828,-2.53374831658168,
8.85049129520029));
#403172=CARTESIAN_POINT('Ctrl Pts',(-0.83386656335501,-2.53949581710878,
8.85711686593484));
#403173=CARTESIAN_POINT('Ctrl Pts',(-0.825328369435533,-2.53994303820322,
8.85933012996512));
#403174=CARTESIAN_POINT('Ctrl Pts',(-0.830677482908384,-2.55723734771397,
8.82945683644724));
#403175=CARTESIAN_POINT('Ctrl Pts',(-0.829635781053786,-2.56303255597043,
8.8360746990239));
#403176=CARTESIAN_POINT('Ctrl Pts',(-0.821070557575579,-2.56344363901071,
8.8382956714852));
#403177=CARTESIAN_POINT('Ctrl Pts',(-0.826461569719549,-2.58069136655118,
8.80838214965003));
#403178=CARTESIAN_POINT('Ctrl Pts',(-0.82541575682307,-2.58650944540522,
8.81501364461996));
#403179=CARTESIAN_POINT('Ctrl Pts',(-0.816819862423326,-2.58690870980847,
8.81722098428721));
#403180=CARTESIAN_POINT('Ctrl Pts',(-0.822251471860003,-2.60411303347872,
8.78727029226991));
#403181=CARTESIAN_POINT('Ctrl Pts',(-0.821205485250568,-2.60993207873471,
8.79393457792714));
#403182=CARTESIAN_POINT('Ctrl Pts',(-0.812575755917834,-2.61034096358643,
8.79610912703474));
#403183=CARTESIAN_POINT('Origin',(-0.822596867063781,-2.53153685626413,
8.85049129520029));
#403184=CARTESIAN_POINT('Ctrl Pts',(-0.84636156559358,-2.52994271156921,
8.85049129520029));
#403185=CARTESIAN_POINT('Ctrl Pts',(-0.850627167658196,-2.53393091307483,
8.85711686593484));
#403186=CARTESIAN_POINT('Ctrl Pts',(-0.857737280217463,-2.5291825384573,
8.85933012996512));
#403187=CARTESIAN_POINT('Ctrl Pts',(-0.842587849021636,-2.52641440726749,
8.8633249698723));
#403188=CARTESIAN_POINT('Ctrl Pts',(-0.847054013910112,-2.52522896829153,
8.86648636486736));
#403189=CARTESIAN_POINT('Ctrl Pts',(-0.847168453388,-2.51932447800883,8.87206031107457));
#403190=CARTESIAN_POINT('Ctrl Pts',(-0.835819892408176,-2.52862903348297,
8.86341338519878));
#403191=CARTESIAN_POINT('Ctrl Pts',(-0.831508491736669,-2.53032764906163,
8.86654584966058));
#403192=CARTESIAN_POINT('Ctrl Pts',(-0.827919486529851,-2.52561137994159,
8.87215952290714));
#403193=CARTESIAN_POINT('Ctrl Pts',(-0.834899689636828,-2.53374831658168,
8.85049129520029));
#403194=CARTESIAN_POINT('Ctrl Pts',(-0.83386656335501,-2.53949581710877,
8.85711686593484));
#403195=CARTESIAN_POINT('Ctrl Pts',(-0.825328369435533,-2.53994303820322,
8.85933012996512));
#403196=CARTESIAN_POINT('Origin',(-0.854898517487354,-2.5208119694108,8.85049129520029));
#403197=CARTESIAN_POINT('Ctrl Pts',(-0.89858389776343,-2.57876892194511,
8.78727029226991));
#403198=CARTESIAN_POINT('Ctrl Pts',(-0.902902597925538,-2.58280676847368,
8.79393457792714));
#403199=CARTESIAN_POINT('Ctrl Pts',(-0.910063138901394,-2.57797292237442,
8.79610912703474));
#403200=CARTESIAN_POINT('Ctrl Pts',(-0.881201122358369,-2.56251658288672,
8.80838214965003));
#403201=CARTESIAN_POINT('Ctrl Pts',(-0.885519105289315,-2.5665537588271,
8.81501364461988));
#403202=CARTESIAN_POINT('Ctrl Pts',(-0.892646776397478,-2.56173243979916,
8.81722098428721));
#403203=CARTESIAN_POINT('Ctrl Pts',(-0.863794336451352,-2.54624179477691,
8.82945683644723));
#403204=CARTESIAN_POINT('Ctrl Pts',(-0.86809534559213,-2.55026310076634,
8.83607469902389));
#403205=CARTESIAN_POINT('Ctrl Pts',(-0.875205505457217,-2.54546959795621,
8.83829567148519));
#403206=CARTESIAN_POINT('Ctrl Pts',(-0.846361565593581,-2.52994271156921,
8.85049129520029));
#403207=CARTESIAN_POINT('Ctrl Pts',(-0.850627167658196,-2.53393091307483,
8.85711686593484));
#403208=CARTESIAN_POINT('Ctrl Pts',(-0.857737280217463,-2.5291825384573,
8.85933012996512));
#403209=CARTESIAN_POINT('Origin',(-0.907120849657204,-2.5696381797867,8.78727029226991));
#403210=CARTESIAN_POINT('Ctrl Pts',(-0.908691583495682,-2.58821925958122,
8.75374538247848));
#403211=CARTESIAN_POINT('Ctrl Pts',(-0.914233353523221,-2.59341860216942,
8.75304829418602));
#403212=CARTESIAN_POINT('Ctrl Pts',(-0.921418004981141,-2.59083956617952,
8.75272238421917));
#403213=CARTESIAN_POINT('Ctrl Pts',(-0.909655777654809,-2.5891207508666,
8.76769408445019));
#403214=CARTESIAN_POINT('Ctrl Pts',(-0.915337475387793,-2.5944504287033,
8.76974318093968));
#403215=CARTESIAN_POINT('Ctrl Pts',(-0.922503084835728,-2.59206874893479,
8.7707786988043));
#403216=CARTESIAN_POINT('Ctrl Pts',(-0.904713867650227,-2.58450022009429,
8.78108014887992));
#403217=CARTESIAN_POINT('Ctrl Pts',(-0.909526302439,-2.58901970111583,8.78639403366326));
#403218=CARTESIAN_POINT('Ctrl Pts',(-0.916943242212213,-2.58577762151636,
8.78812224174741));
#403219=CARTESIAN_POINT('Ctrl Pts',(-0.896615168114524,-2.57692819012542,
8.78944554828685));
#403220=CARTESIAN_POINT('Ctrl Pts',(-0.900667077682591,-2.58074112160516,
8.79673892988686));
#403221=CARTESIAN_POINT('Ctrl Pts',(-0.907869787598809,-2.5754852178599,
8.79894799272499));
#403222=CARTESIAN_POINT('Origin',(-0.91736377547371,-2.57921498783034,8.75721825406948));
#403223=CARTESIAN_POINT('Origin',(-0.91736377547371,-2.57921498783034,9.));
#403224=CARTESIAN_POINT('Origin',(-0.91736377547371,-2.57921498783034,7.51860402984325));
#403225=CARTESIAN_POINT('Ctrl Pts',(-0.902424603106939,-2.59383933776842,
7.50366195182966));
#403226=CARTESIAN_POINT('Ctrl Pts',(-0.903627891060323,-2.59729794873401,
7.50000065167735));
#403227=CARTESIAN_POINT('Ctrl Pts',(-0.903627891060433,-2.59729794873397,
7.49482233047108));
#403228=CARTESIAN_POINT('Ctrl Pts',(-0.909800645744154,-2.59286579032708,
7.50215800491337));
#403229=CARTESIAN_POINT('Ctrl Pts',(-0.912631876385771,-2.59416534033701,
7.49877273257265));
#403230=CARTESIAN_POINT('Ctrl Pts',(-0.915892318043139,-2.5930310226792,
7.49481816995649));
#403231=CARTESIAN_POINT('Ctrl Pts',(-0.910885454044046,-2.59027094788589,
7.51043025814041));
#403232=CARTESIAN_POINT('Ctrl Pts',(-0.916079119671714,-2.59293901728808,
7.51006209594514));
#403233=CARTESIAN_POINT('Ctrl Pts',(-0.921555036631571,-2.590991376764,
7.50731281821697));
#403234=CARTESIAN_POINT('Ctrl Pts',(-0.908825719620616,-2.58834469769699,
7.51860402984325));
#403235=CARTESIAN_POINT('Ctrl Pts',(-0.914383355130147,-2.59354216871026,
7.51860402984324));
#403236=CARTESIAN_POINT('Ctrl Pts',(-0.92155265116081,-2.59099222521769,
7.51860402984325));
#403237=CARTESIAN_POINT('Origin',(0.,0.,7.5));
#403238=CARTESIAN_POINT('Origin',(-0.682528638916234,-2.57897124462359,
7.5));
#403239=CARTESIAN_POINT('',(-0.682528638916234,-2.57897124462359,7.59394543036555));
#403240=CARTESIAN_POINT('',(-0.682528638916234,-2.57897124462359,8.85049129520029));
#403241=CARTESIAN_POINT('',(-0.682528638916234,-2.57897124462359,7.5));
#403242=CARTESIAN_POINT('',(-0.731515368664204,-2.63104303262371,8.78727029226991));
#403243=CARTESIAN_POINT('Ctrl Pts',(-0.682528638916234,-2.57897124462359,
8.85049129520029));
#403244=CARTESIAN_POINT('Ctrl Pts',(-0.698881284484156,-2.59635373775254,
8.82945686509571));
#403245=CARTESIAN_POINT('Ctrl Pts',(-0.715209619867108,-2.61371038970359,
8.80838212259895));
#403246=CARTESIAN_POINT('Ctrl Pts',(-0.731515368664204,-2.63104303262371,
8.78727029226991));
#403247=CARTESIAN_POINT('',(-0.741123661093001,-2.64125643059841,8.75721825406948));
#403248=CARTESIAN_POINT('Origin',(-0.712208829051481,-2.6105209113155,8.75937679713132));
#403249=CARTESIAN_POINT('',(-0.741123661093001,-2.64125643059841,7.51860402984325));
#403250=CARTESIAN_POINT('',(-0.741123661093001,-2.64125643059841,7.5));
#403251=CARTESIAN_POINT('Ctrl Pts',(-0.741123661093001,-2.64125643059841,
7.51860402984325));
#403252=CARTESIAN_POINT('Ctrl Pts',(-0.733577841762315,-2.63323539497313,
7.52834476460825));
#403253=CARTESIAN_POINT('Ctrl Pts',(-0.726027123794601,-2.62520915220727,
7.53807742314407));
#403254=CARTESIAN_POINT('Ctrl Pts',(-0.71847134271161,-2.61717752746414,
7.54780169004674));
#403255=CARTESIAN_POINT('Ctrl Pts',(-0.706503393831275,-2.60445586794331,
7.5632044032688));
#403256=CARTESIAN_POINT('Ctrl Pts',(-0.694522727030071,-2.59172068955963,
7.57858609112103));
#403257=CARTESIAN_POINT('Ctrl Pts',(-0.682528638916234,-2.57897124462359,
7.59394543036555));
#403258=CARTESIAN_POINT('Origin',(-0.604952940619234,-2.8490235055211,7.5));
#403259=CARTESIAN_POINT('',(-0.650355981859141,-2.66505851907034,8.75721825406948));
#403260=CARTESIAN_POINT('',(-0.653715973115249,-2.65144443664273,8.78727029226991));
#403261=CARTESIAN_POINT('Origin',(-0.662244884137802,-2.61688681764065,
8.75658640621008));
#403262=CARTESIAN_POINT('',(-0.670846486662608,-2.58203466569847,8.85049129520029));
#403263=CARTESIAN_POINT('Ctrl Pts',(-0.653715973115249,-2.65144443664273,
8.78727029226991));
#403264=CARTESIAN_POINT('Ctrl Pts',(-0.659418044923381,-2.62834066354124,
8.80838212259896));
#403265=CARTESIAN_POINT('Ctrl Pts',(-0.665128015193342,-2.6052048872879,
8.82945686509571));
#403266=CARTESIAN_POINT('Ctrl Pts',(-0.670846486662608,-2.58203466569847,
8.85049129520029));
#403267=CARTESIAN_POINT('',(-0.670846486662608,-2.58203466569847,7.59394543036555));
#403268=CARTESIAN_POINT('',(-0.670846486662608,-2.58203466569847,7.5));
#403269=CARTESIAN_POINT('',(-0.650355981859141,-2.66505851907034,7.51860402984325));
#403270=CARTESIAN_POINT('Ctrl Pts',(-0.670846486662608,-2.58203466569847,
7.59394543036555));
#403271=CARTESIAN_POINT('Ctrl Pts',(-0.666652189758541,-2.59902920509618,
7.57858609112103));
#403272=CARTESIAN_POINT('Ctrl Pts',(-0.662462586247605,-2.61600472770608,
7.56320440326857));
#403273=CARTESIAN_POINT('Ctrl Pts',(-0.658277430155668,-2.63296223017113,
7.54780169004651));
#403274=CARTESIAN_POINT('Ctrl Pts',(-0.655635196006356,-2.64366808943085,
7.53807742314383));
#403275=CARTESIAN_POINT('Ctrl Pts',(-0.652994732413329,-2.65436677471377,
7.52834476460825));
#403276=CARTESIAN_POINT('Ctrl Pts',(-0.650355981859142,-2.66505851907034,
7.51860402984325));
#403277=CARTESIAN_POINT('',(-0.650355981859141,-2.66505851907034,7.5));
#403278=CARTESIAN_POINT('Origin',(-0.677521207658174,-2.58368200434956,
7.5));
#403279=CARTESIAN_POINT('Ctrl Pts',(-0.670846486662608,-2.58203466569847,
8.85049129520029));
#403280=CARTESIAN_POINT('Ctrl Pts',(-0.670892890456633,-2.58184664584108,
8.85097269580138));
#403281=CARTESIAN_POINT('Ctrl Pts',(-0.670946875156401,-2.58166301368505,
8.85143669361005));
#403282=CARTESIAN_POINT('Ctrl Pts',(-0.671011765372886,-2.58147556015295,
8.8519052845931));
#403283=CARTESIAN_POINT('Ctrl Pts',(-0.671138686521143,-2.58110891293204,
8.85282181883899));
#403284=CARTESIAN_POINT('Ctrl Pts',(-0.671304249801605,-2.58073714253129,
8.85372622499636));
#403285=CARTESIAN_POINT('Ctrl Pts',(-0.671525138335623,-2.58036068787951,
8.85462257735071));
#403286=CARTESIAN_POINT('Ctrl Pts',(-0.671708512151346,-2.58004816859801,
8.85536669723987));
#403287=CARTESIAN_POINT('Ctrl Pts',(-0.67193002919577,-2.57973233380185,
8.85610498449051));
#403288=CARTESIAN_POINT('Ctrl Pts',(-0.672205804986711,-2.5794180029897,
8.85681338218371));
#403289=CARTESIAN_POINT('Ctrl Pts',(-0.672456071950103,-2.57913274728401,
8.85745625420284));
#403290=CARTESIAN_POINT('Ctrl Pts',(-0.672753713651867,-2.57884475725327,
8.85808743050666));
#403291=CARTESIAN_POINT('Ctrl Pts',(-0.673125539874815,-2.57856398687628,
8.8586680450841));
#403292=CARTESIAN_POINT('Ctrl Pts',(-0.673297092433881,-2.57843444551069,
8.85893592806395));
#403293=CARTESIAN_POINT('Ctrl Pts',(-0.673484652170842,-2.57830655186085,
8.85919241173848));
#403294=CARTESIAN_POINT('Ctrl Pts',(-0.673692155647793,-2.57818220473043,
8.85943017985534));
#403295=CARTESIAN_POINT('Ctrl Pts',(-0.673972346769279,-2.57801429929367,
8.8597512372));
#403296=CARTESIAN_POINT('Ctrl Pts',(-0.67429636215277,-2.57784913604231,
8.86004599534706));
#403297=CARTESIAN_POINT('Ctrl Pts',(-0.67466503880102,-2.57769797846511,
8.86026130871721));
#403298=CARTESIAN_POINT('Ctrl Pts',(-0.674800021716039,-2.57764263541451,
8.86034014101235));
#403299=CARTESIAN_POINT('Ctrl Pts',(-0.674943014382129,-2.57758832710581,
8.86040910639692));
#403300=CARTESIAN_POINT('Ctrl Pts',(-0.675090240476513,-2.57753684760079,
8.86046313645506));
#403301=CARTESIAN_POINT('Ctrl Pts',(-0.675319985563791,-2.57745651426433,
8.86054744990829));
#403302=CARTESIAN_POINT('Ctrl Pts',(-0.675566359499169,-2.57738101538588,
8.86059655985668));
#403303=CARTESIAN_POINT('Ctrl Pts',(-0.67581347573792,-2.57731491283742,
8.86059725258816));
#403304=CARTESIAN_POINT('Ctrl Pts',(-0.676061162913906,-2.57724865756566,
8.86059794692011));
#403305=CARTESIAN_POINT('Ctrl Pts',(-0.676313029242146,-2.57719367384813,
8.86056369958366));
#403306=CARTESIAN_POINT('Ctrl Pts',(-0.67655453520928,-2.57714928401131,
8.86048590497774));
#403307=CARTESIAN_POINT('Ctrl Pts',(-0.676617561076204,-2.57713769958554,
8.86046560290182));
#403308=CARTESIAN_POINT('Ctrl Pts',(-0.676680717651053,-2.5771267750407,
8.86044257503091));
#403309=CARTESIAN_POINT('Ctrl Pts',(-0.676742047748341,-2.57711681560841,
8.86041778462584));
#403310=CARTESIAN_POINT('Ctrl Pts',(-0.677154723198782,-2.57704980098778,
8.86025097596201));
#403311=CARTESIAN_POINT('Ctrl Pts',(-0.677540131460308,-2.57701781811485,
8.8599848982295));
#403312=CARTESIAN_POINT('Ctrl Pts',(-0.677886322802429,-2.57701335701957,
8.85968173251461));
#403313=CARTESIAN_POINT('Ctrl Pts',(-0.678069438188012,-2.57701099735576,
8.85952137522076));
#403314=CARTESIAN_POINT('Ctrl Pts',(-0.67824510867004,-2.57701610131725,
8.85934740853961));
#403315=CARTESIAN_POINT('Ctrl Pts',(-0.678410902053581,-2.57702704303034,
8.8591675900182));
#403316=CARTESIAN_POINT('Ctrl Pts',(-0.679076648666189,-2.57707097969576,
8.85844552518695));
#403317=CARTESIAN_POINT('Ctrl Pts',(-0.679620958726725,-2.57720851046265,
8.85759444184123));
#403318=CARTESIAN_POINT('Ctrl Pts',(-0.680054687829788,-2.577360508228,
8.85683498915138));
#403319=CARTESIAN_POINT('Ctrl Pts',(-0.680100076425306,-2.57737641438933,
8.85675551444997));
#403320=CARTESIAN_POINT('Ctrl Pts',(-0.680144243875811,-2.57739249616704,
8.85667699793651));
#403321=CARTESIAN_POINT('Ctrl Pts',(-0.680187195361034,-2.57740867382615,
8.85659965593547));
#403322=CARTESIAN_POINT('Ctrl Pts',(-0.680766956700293,-2.57762704069422,
8.85555568965886));
#403323=CARTESIAN_POINT('Ctrl Pts',(-0.681292606769922,-2.57792063379262,
8.85434650606346));
#403324=CARTESIAN_POINT('Ctrl Pts',(-0.681769774569088,-2.5782854786949,
8.85297329937117));
#403325=CARTESIAN_POINT('Ctrl Pts',(-0.682038152381857,-2.5784906817221,
8.85220095427747));
#403326=CARTESIAN_POINT('Ctrl Pts',(-0.68229111167692,-2.57871875852963,
8.85137579139183));
#403327=CARTESIAN_POINT('Ctrl Pts',(-0.682528638916234,-2.57897124462359,
8.85049129520029));
#403328=CARTESIAN_POINT('Origin',(-0.677521207658174,-2.58368200434956,
7.59394543036555));
#403329=CARTESIAN_POINT('Ctrl Pts',(-0.670981212530835,-2.58148878062456,
7.59443877723642));
#403330=CARTESIAN_POINT('Ctrl Pts',(-0.672368759343822,-2.57586668959982,
7.58783886950016));
#403331=CARTESIAN_POINT('Ctrl Pts',(-0.680858400978228,-2.57593856766321,
7.58559994247159));
#403332=CARTESIAN_POINT('Ctrl Pts',(-0.663406635187641,-2.61217961058346,
7.56670252222133));
#403333=CARTESIAN_POINT('Ctrl Pts',(-0.664792176601553,-2.60656564507641,
7.56004874999027));
#403334=CARTESIAN_POINT('Ctrl Pts',(-0.67333230320828,-2.60661658423106,
7.55786368756704));
#403335=CARTESIAN_POINT('Ctrl Pts',(-0.655846202610834,-2.64281312848384,
7.53888913333559));
#403336=CARTESIAN_POINT('Ctrl Pts',(-0.657239978365184,-2.6371657989049,
7.53222002137279));
#403337=CARTESIAN_POINT('Ctrl Pts',(-0.665818860235125,-2.63723812166668,
7.53005029815327));
#403338=CARTESIAN_POINT('Ctrl Pts',(-0.648300256915117,-2.67338794813822,
7.51101258149734));
#403339=CARTESIAN_POINT('Ctrl Pts',(-0.649710927764185,-2.66767216266333,
7.5043616886572));
#403340=CARTESIAN_POINT('Ctrl Pts',(-0.658318523541249,-2.66780168672796,
7.50217374673251));
#403341=CARTESIAN_POINT('',(-0.658718750143873,-2.6661707753905,7.50366116523517));
#403342=CARTESIAN_POINT('Ctrl Pts',(-0.650355981859141,-2.66505851907034,
7.51860402984325));
#403343=CARTESIAN_POINT('Ctrl Pts',(-0.650250166117427,-2.66548726549259,
7.51734760759493));
#403344=CARTESIAN_POINT('Ctrl Pts',(-0.650212310040413,-2.66588895539464,
7.51608817408572));
#403345=CARTESIAN_POINT('Ctrl Pts',(-0.650255795434444,-2.66626391779723,
7.51481005913119));
#403346=CARTESIAN_POINT('Ctrl Pts',(-0.650295185543474,-2.66660356770152,
7.51365231206383));
#403347=CARTESIAN_POINT('Ctrl Pts',(-0.650401124727235,-2.66692179482434,
7.51247773061042));
#403348=CARTESIAN_POINT('Ctrl Pts',(-0.650606814530752,-2.6672014295012,
7.51129758471022));
#403349=CARTESIAN_POINT('Ctrl Pts',(-0.650862463465862,-2.66754898346906,
7.50983079813402));
#403350=CARTESIAN_POINT('Ctrl Pts',(-0.651274536664425,-2.66781811159763,
7.50839324291155));
#403351=CARTESIAN_POINT('Ctrl Pts',(-0.651891120888266,-2.66794175530204,
7.50715379678855));
#403352=CARTESIAN_POINT('Ctrl Pts',(-0.652175965033233,-2.66799887513076,
7.50658120839351));
#403353=CARTESIAN_POINT('Ctrl Pts',(-0.652546816749148,-2.66802374990068,
7.50598221009429));
#403354=CARTESIAN_POINT('Ctrl Pts',(-0.652996372582813,-2.66799309213236,
7.50545747549611));
#403355=CARTESIAN_POINT('Ctrl Pts',(-0.653236269490711,-2.66797673219823,
7.50517746087247));
#403356=CARTESIAN_POINT('Ctrl Pts',(-0.653501193456985,-2.66794458333831,
7.50491486231392));
#403357=CARTESIAN_POINT('Ctrl Pts',(-0.653783927906875,-2.66789584104,7.50468370960993));
#403358=CARTESIAN_POINT('Ctrl Pts',(-0.654206705092984,-2.66782295592915,
7.50433806340447));
#403359=CARTESIAN_POINT('Ctrl Pts',(-0.654681888865048,-2.6677102342832,
7.50405484070984));
#403360=CARTESIAN_POINT('Ctrl Pts',(-0.655177311127184,-2.66756457064415,
7.50385766036131));
#403361=CARTESIAN_POINT('Ctrl Pts',(-0.655230288837517,-2.66754899418207,
7.50383657498791));
#403362=CARTESIAN_POINT('Ctrl Pts',(-0.655283478613827,-2.66753306175526,
7.50381643264938));
#403363=CARTESIAN_POINT('Ctrl Pts',(-0.655336827290485,-2.66751679707098,
7.50379723213559));
#403364=CARTESIAN_POINT('Ctrl Pts',(-0.655692947158727,-2.66740822498289,
7.50366906242519));
#403365=CARTESIAN_POINT('Ctrl Pts',(-0.656063684366644,-2.66728179801424,
7.50358235568538));
#403366=CARTESIAN_POINT('Ctrl Pts',(-0.656418100142817,-2.66715134813715,
7.5035341175365));
#403367=CARTESIAN_POINT('Ctrl Pts',(-0.656949506487069,-2.66695575331051,
7.50346178989176));
#403368=CARTESIAN_POINT('Ctrl Pts',(-0.657512862320752,-2.66672274300315,
7.50346967198527));
#403369=CARTESIAN_POINT('Ctrl Pts',(-0.658058864751418,-2.66647698198924,
7.50354272648693));
#403370=CARTESIAN_POINT('Ctrl Pts',(-0.658283446852733,-2.66637589539726,
7.50357277531559));
#403371=CARTESIAN_POINT('Ctrl Pts',(-0.658504852827761,-2.66627291519395,
7.50361331098762));
#403372=CARTESIAN_POINT('Ctrl Pts',(-0.658718750144213,-2.66617077539187,
7.50366116523659));
#403373=CARTESIAN_POINT('',(-0.678263889302273,-2.586514171338,7.57603338622103));
#403374=CARTESIAN_POINT('Origin',(-0.680508179114217,-2.5950613728002,7.58486873427629));
#403375=CARTESIAN_POINT('Ctrl Pts',(-0.658718750125062,-2.66617077544467,
7.50366116529969));
#403376=CARTESIAN_POINT('Ctrl Pts',(-0.665223977061745,-2.63966210099077,
7.52783573079709));
#403377=CARTESIAN_POINT('Ctrl Pts',(-0.671738733243923,-2.61311115757656,
7.55196141284068));
#403378=CARTESIAN_POINT('Ctrl Pts',(-0.678263888672613,-2.58651417242021,
7.57603338728831));
#403379=CARTESIAN_POINT('Ctrl Pts',(-0.670770761278379,-2.58307524303168,
7.59639677331371));
#403380=CARTESIAN_POINT('Ctrl Pts',(-0.672361328299651,-2.56400514804977,
7.59974925422224));
#403381=CARTESIAN_POINT('Ctrl Pts',(-0.683105249421501,-2.57984075934191,
7.59639677331372));
#403382=CARTESIAN_POINT('Ctrl Pts',(-0.670465937780008,-2.57918651744113,
7.58707626057423));
#403383=CARTESIAN_POINT('Ctrl Pts',(-0.674975104133252,-2.5739726081208,
7.58811717123965));
#403384=CARTESIAN_POINT('Ctrl Pts',(-0.681462581934873,-2.57630285775876,
7.58707626057423));
#403385=CARTESIAN_POINT('Ctrl Pts',(-0.675135748308901,-2.58307476921871,
7.58015376756929));
#403386=CARTESIAN_POINT('Ctrl Pts',(-0.676728207785887,-2.58065795214827,
7.5820876076604));
#403387=CARTESIAN_POINT('Ctrl Pts',(-0.679301722070223,-2.58198232224996,
7.5801537675693));
#403388=CARTESIAN_POINT('Ctrl Pts',(-0.678263889092161,-2.58651417053755,
7.57603338509286));
#403389=CARTESIAN_POINT('Ctrl Pts',(-0.678263889092161,-2.58651417053755,
7.57603338509286));
#403390=CARTESIAN_POINT('Ctrl Pts',(-0.678263889092161,-2.58651417053755,
7.57603338509286));
#403391=CARTESIAN_POINT('Origin',(-0.680502659389277,-2.59506282024289,
7.58486873427622));
#403392=CARTESIAN_POINT('Ctrl Pts',(-0.747020829444778,-2.64752498744625,
7.51098857897448));
#403393=CARTESIAN_POINT('Ctrl Pts',(-0.742986830895866,-2.64323693804364,
7.50433767179957));
#403394=CARTESIAN_POINT('Ctrl Pts',(-0.735550410854303,-2.64757372349462,
7.50214974420965));
#403395=CARTESIAN_POINT('Ctrl Pts',(-0.725436098627555,-2.62458090579523,
7.53887321589168));
#403396=CARTESIAN_POINT('Ctrl Pts',(-0.721450434540312,-2.62034423483435,
7.5322040745206));
#403397=CARTESIAN_POINT('Ctrl Pts',(-0.714010955012724,-2.62461706343848,
7.53003438070912));
#403398=CARTESIAN_POINT('Ctrl Pts',(-0.70380991716486,-2.60159276304368,
7.56669465659227));
#403399=CARTESIAN_POINT('Ctrl Pts',(-0.699847807611344,-2.59738113002054,
7.56004085833293));
#403400=CARTESIAN_POINT('Ctrl Pts',(-0.69243160852584,-2.60161629722503,
7.55785582193789));
#403401=CARTESIAN_POINT('Ctrl Pts',(-0.682143263122402,-2.5785615988534,
7.59443891967696));
#403402=CARTESIAN_POINT('Ctrl Pts',(-0.678175409003361,-2.57434385948673,
7.58783901202978));
#403403=CARTESIAN_POINT('Ctrl Pts',(-0.670813497415762,-2.57857250415905,
7.58560008491213));
#403404=CARTESIAN_POINT('',(-0.734382828366891,-2.6463293175146,7.50366116523517));
#403405=CARTESIAN_POINT('Ctrl Pts',(-0.734382828366991,-2.64632931751496,
7.50366116523554));
#403406=CARTESIAN_POINT('Ctrl Pts',(-0.7351388143909,-2.64627810571535,
7.50350835821027));
#403407=CARTESIAN_POINT('Ctrl Pts',(-0.735832082908394,-2.64620643442547,
7.50345484956));
#403408=CARTESIAN_POINT('Ctrl Pts',(-0.736483307107746,-2.64611277011765,
7.50349758195598));
#403409=CARTESIAN_POINT('Ctrl Pts',(-0.73681743341806,-2.64606471338141,
7.50351950684424));
#403410=CARTESIAN_POINT('Ctrl Pts',(-0.737173443029265,-2.64600625855206,
7.50357029184312));
#403411=CARTESIAN_POINT('Ctrl Pts',(-0.737515189580187,-2.64594045470856,
7.50365515313923));
#403412=CARTESIAN_POINT('Ctrl Pts',(-0.738040934162347,-2.64583922175066,
7.50378570417639));
#403413=CARTESIAN_POINT('Ctrl Pts',(-0.738548420846335,-2.64571796522779,
7.50400001621911));
#403414=CARTESIAN_POINT('Ctrl Pts',(-0.738998494895536,-2.64558370626699,
7.50428903009634));
#403415=CARTESIAN_POINT('Ctrl Pts',(-0.739048449652339,-2.64556880455527,
7.50432110841318));
#403416=CARTESIAN_POINT('Ctrl Pts',(-0.739097725961653,-2.64555375201861,
7.50435406373354));
#403417=CARTESIAN_POINT('Ctrl Pts',(-0.739146291662912,-2.64553856487361,
7.50438785222352));
#403418=CARTESIAN_POINT('Ctrl Pts',(-0.739442808612724,-2.6454458400535,
7.50459414719561));
#403419=CARTESIAN_POINT('Ctrl Pts',(-0.739717403222056,-2.64534612893593,
7.50483629897752));
#403420=CARTESIAN_POINT('Ctrl Pts',(-0.739960005034027,-2.64524448842675,
7.5050991045531));
#403421=CARTESIAN_POINT('Ctrl Pts',(-0.740495208998279,-2.64502025925466,
7.50567888004914));
#403422=CARTESIAN_POINT('Ctrl Pts',(-0.740895999024185,-2.64477828392327,
7.50637912803144));
#403423=CARTESIAN_POINT('Ctrl Pts',(-0.741184705006695,-2.64453993517567,
7.50710440483569));
#403424=CARTESIAN_POINT('Ctrl Pts',(-0.741255501445223,-2.64448148733087,
7.50728225710685));
#403425=CARTESIAN_POINT('Ctrl Pts',(-0.741321060218752,-2.64442220659312,
7.50746498566954));
#403426=CARTESIAN_POINT('Ctrl Pts',(-0.741380130382238,-2.64436378576598,
7.50764697238949));
#403427=CARTESIAN_POINT('Ctrl Pts',(-0.741697675324592,-2.64404973147709,
7.50862528291181));
#403428=CARTESIAN_POINT('Ctrl Pts',(-0.741859446188481,-2.64373496099275,
7.50965856837421));
#403429=CARTESIAN_POINT('Ctrl Pts',(-0.741930383748714,-2.64343281940981,
7.51067959873201));
#403430=CARTESIAN_POINT('Ctrl Pts',(-0.741969420777586,-2.64326655051562,
7.51124147302578));
#403431=CARTESIAN_POINT('Ctrl Pts',(-0.741980537241458,-2.64310396618176,
7.51180065547252));
#403432=CARTESIAN_POINT('Ctrl Pts',(-0.741971890422264,-2.64294676648674,
7.51235175716501));
#403433=CARTESIAN_POINT('Ctrl Pts',(-0.741942012217466,-2.64240357891952,
7.51425603304535));
#403434=CARTESIAN_POINT('Ctrl Pts',(-0.741666547014249,-2.64186025088833,
7.51626900505179));
#403435=CARTESIAN_POINT('Ctrl Pts',(-0.741200952461297,-2.64134059660316,
7.51827788969242));
#403436=CARTESIAN_POINT('Ctrl Pts',(-0.741175753604239,-2.64131247193123,
7.51838661432544));
#403437=CARTESIAN_POINT('Ctrl Pts',(-0.741149987931403,-2.64128441543338,
7.51849533314856));
#403438=CARTESIAN_POINT('Ctrl Pts',(-0.741123661093005,-2.64125643059841,
7.51860402984325));
#403439=CARTESIAN_POINT('Ctrl Pts',(-0.678263890382501,-2.58651417197306,
7.57603338728985));
#403440=CARTESIAN_POINT('Ctrl Pts',(-0.697000987805607,-2.60648661431919,
7.55196141284922));
#403441=CARTESIAN_POINT('Ctrl Pts',(-0.715706430690877,-2.62642404273905,
7.52783573083105));
#403442=CARTESIAN_POINT('Ctrl Pts',(-0.734382828411178,-2.64632931755386,
7.50366116530176));
#403443=CARTESIAN_POINT('Origin',(-2.34371526914283E-16,-8.93760209386497E-16,
7.49482233047033));
#403444=CARTESIAN_POINT('Origin',(-0.656598725434862,-2.65758995402928,
7.49482233047033));
#403445=CARTESIAN_POINT('Origin',(0.,0.,7.50366116523517));
#403446=CARTESIAN_POINT('Origin',(-0.732019285896496,-2.63781235403044,
7.49482233047033));
#403447=CARTESIAN_POINT('Ctrl Pts',(-0.65035623525911,-2.66505749215231,
7.51860402984325));
#403448=CARTESIAN_POINT('Ctrl Pts',(-0.648533655213682,-2.6724449469243,
7.51860402984325));
#403449=CARTESIAN_POINT('Ctrl Pts',(-0.641134372651985,-2.67421889833352,
7.51860402984325));
#403450=CARTESIAN_POINT('Ctrl Pts',(-0.64967949761657,-2.66780050421939,
7.51041458714367));
#403451=CARTESIAN_POINT('Ctrl Pts',(-0.646780678116779,-2.67286520670501,
7.51004642900444));
#403452=CARTESIAN_POINT('Ctrl Pts',(-0.641132332017705,-2.67421938756826,
7.50729136483011));
#403453=CARTESIAN_POINT('Ctrl Pts',(-0.652012104546077,-2.66937615713541,
7.50215815450137));
#403454=CARTESIAN_POINT('Ctrl Pts',(-0.650349947137616,-2.67200965238524,
7.49877163671527));
#403455=CARTESIAN_POINT('Ctrl Pts',(-0.647000459287308,-2.67283721189065,
7.49481588533168));
#403456=CARTESIAN_POINT('Ctrl Pts',(-0.658718618100706,-2.66617024094247,
7.50366171572174));
#403457=CARTESIAN_POINT('Ctrl Pts',(-0.659596893131287,-2.66972506797452,
7.50000045605858));
#403458=CARTESIAN_POINT('Ctrl Pts',(-0.659596893131166,-2.66972506797455,
7.49482233047317));
#403459=CARTESIAN_POINT('Origin',(-0.638220125503567,-2.66206335788655,
7.51860402984325));
#403460=CARTESIAN_POINT('Origin',(-0.638220125503567,-2.66206335788655,
9.));
#403461=CARTESIAN_POINT('Origin',(-0.638220125503568,-2.66206335788655,
8.75721825406948));
#403462=CARTESIAN_POINT('Ctrl Pts',(-0.654357526473991,-2.64884485132562,
8.78942910404913));
#403463=CARTESIAN_POINT('Ctrl Pts',(-0.653041919255973,-2.65425979420155,
8.79672699501691));
#403464=CARTESIAN_POINT('Ctrl Pts',(-0.644128763436838,-2.65378110920504,
8.79893251111267));
#403465=CARTESIAN_POINT('Ctrl Pts',(-0.6517231462551,-2.65951890676874,
8.78111911759582));
#403466=CARTESIAN_POINT('Ctrl Pts',(-0.650156245245687,-2.66593662687421,
8.78644465894813));
#403467=CARTESIAN_POINT('Ctrl Pts',(-0.642156520060473,-2.66724807978471,
8.78817647674132));
#403468=CARTESIAN_POINT('Ctrl Pts',(-0.650081337635898,-2.66617123271351,
8.76780923932031));
#403469=CARTESIAN_POINT('Ctrl Pts',(-0.648226726776183,-2.67374587167056,
8.76988516158375));
#403470=CARTESIAN_POINT('Ctrl Pts',(-0.640913636083743,-2.67565769930935,
8.77093053738834));
#403471=CARTESIAN_POINT('Ctrl Pts',(-0.650401467845226,-2.66487412019735,
8.75371302330492));
#403472=CARTESIAN_POINT('Ctrl Pts',(-0.648593115387881,-2.67226303505393,
8.75300828287559));
#403473=CARTESIAN_POINT('Ctrl Pts',(-0.641155596302552,-2.67401741505541,
8.75267964240737));
#403474=CARTESIAN_POINT('Origin',(-0.641580116759675,-2.64844927545894,
8.78727029226991));
#403475=CARTESIAN_POINT('Ctrl Pts',(-0.670846486662608,-2.58203466569847,
8.85049129520029));
#403476=CARTESIAN_POINT('Ctrl Pts',(-0.669447239426428,-2.58770416474117,
8.85711686593484));
#403477=CARTESIAN_POINT('Ctrl Pts',(-0.660897934588176,-2.58760342300926,
8.85933012996512));
#403478=CARTESIAN_POINT('Ctrl Pts',(-0.665128007518938,-2.60520491838321,
8.82945683644723));
#403479=CARTESIAN_POINT('Ctrl Pts',(-0.663717145684703,-2.6109214776958,
8.83607469902391));
#403480=CARTESIAN_POINT('Ctrl Pts',(-0.655143182195925,-2.61078294036945,
8.8382956714852));
#403481=CARTESIAN_POINT('Ctrl Pts',(-0.659418052229574,-2.62834063393785,
8.80838214965003));
#403482=CARTESIAN_POINT('Ctrl Pts',(-0.658001622475826,-2.63407975346252,
8.81501364461989));
#403483=CARTESIAN_POINT('Ctrl Pts',(-0.649397808304884,-2.63392745668915,
8.81722098428721));
#403484=CARTESIAN_POINT('Ctrl Pts',(-0.653715973115249,-2.65144443664273,
8.78727029226991));
#403485=CARTESIAN_POINT('Ctrl Pts',(-0.652299308087855,-2.65718450945399,
8.79393457792714));
#403486=CARTESIAN_POINT('Ctrl Pts',(-0.643661112117175,-2.6570396455512,
8.79610912703474));
#403487=CARTESIAN_POINT('Origin',(-0.658710630307035,-2.57903950451468,
8.85049129520029));
#403488=CARTESIAN_POINT('Ctrl Pts',(-0.682528638916234,-2.57897124462359,
8.85049129520029));
#403489=CARTESIAN_POINT('Ctrl Pts',(-0.686529951896131,-2.58322455000411,
8.85711686593484));
#403490=CARTESIAN_POINT('Ctrl Pts',(-0.693929685372884,-2.57894147790725,
8.85933012996512));
#403491=CARTESIAN_POINT('Ctrl Pts',(-0.67898873508248,-2.57520840675055,
8.86332496987231));
#403492=CARTESIAN_POINT('Ctrl Pts',(-0.683521675092156,-2.57431155155301,
8.86648636486739));
#403493=CARTESIAN_POINT('Ctrl Pts',(-0.684014181433158,-2.56842652484136,
8.87206031107457));
#403494=CARTESIAN_POINT('Ctrl Pts',(-0.672092792372952,-2.5769848583099,
8.86341338519876));
#403495=CARTESIAN_POINT('Ctrl Pts',(-0.667681419262742,-2.57840375151124,
8.86654584966056));
#403496=CARTESIAN_POINT('Ctrl Pts',(-0.66440196045204,-2.5734672241188,
8.87215952290715));
#403497=CARTESIAN_POINT('Ctrl Pts',(-0.670846486662608,-2.58203466569847,
8.85049129520029));
#403498=CARTESIAN_POINT('Ctrl Pts',(-0.669447239426428,-2.58770416474117,
8.85711686593484));
#403499=CARTESIAN_POINT('Ctrl Pts',(-0.660897934588176,-2.58760342300926,
8.85933012996512));
#403500=CARTESIAN_POINT('Origin',(-0.691633059385434,-2.57040622694001,
8.85049129520029));
#403501=CARTESIAN_POINT('Ctrl Pts',(-0.731515368664204,-2.63104303262371,
8.78727029226991));
#403502=CARTESIAN_POINT('Ctrl Pts',(-0.735566489878316,-2.63534928303294,
8.79393457792714));
#403503=CARTESIAN_POINT('Ctrl Pts',(-0.743022024337704,-2.63098414602442,
8.79610912703474));
#403504=CARTESIAN_POINT('Ctrl Pts',(-0.715209598974184,-2.61371036749489,
8.80838214965002));
#403505=CARTESIAN_POINT('Ctrl Pts',(-0.719260047395506,-2.61801590274056,
8.81501364461988));
#403506=CARTESIAN_POINT('Ctrl Pts',(-0.726681976909647,-2.61366116108551,
8.81722098428721));
#403507=CARTESIAN_POINT('Ctrl Pts',(-0.698881306430013,-2.59635376108049,
8.82945683644723));
#403508=CARTESIAN_POINT('Ctrl Pts',(-0.702915832726872,-2.60064237146729,
8.83607469902389));
#403509=CARTESIAN_POINT('Ctrl Pts',(-0.710318504785465,-2.59631426692943,
8.83829567148519));
#403510=CARTESIAN_POINT('Ctrl Pts',(-0.682528638916234,-2.57897124462359,
8.85049129520029));
#403511=CARTESIAN_POINT('Ctrl Pts',(-0.686529951896131,-2.58322455000411,
8.85711686593484));
#403512=CARTESIAN_POINT('Ctrl Pts',(-0.693929685372884,-2.57894147790725,
8.85933012996512));
#403513=CARTESIAN_POINT('Origin',(-0.740619789133404,-2.62247801494013,
8.78727029226991));
#403514=CARTESIAN_POINT('Ctrl Pts',(-0.740996801860829,-2.64112155517595,
8.75374538247848));
#403515=CARTESIAN_POINT('Ctrl Pts',(-0.746194062704114,-2.64666527758192,
8.75304829418601));
#403516=CARTESIAN_POINT('Ctrl Pts',(-0.75352919192828,-2.64455186269746,
8.75272238421917));
#403517=CARTESIAN_POINT('Ctrl Pts',(-0.741901256234692,-2.64208297038268,
8.7676940844502));
#403518=CARTESIAN_POINT('Ctrl Pts',(-0.747229806678894,-2.64776572544829,
8.76974318093971));
#403519=CARTESIAN_POINT('Ctrl Pts',(-0.754533288360401,-2.64584804126991,
8.7707786988043));
#403520=CARTESIAN_POINT('Ctrl Pts',(-0.737265538337216,-2.63715530372526,
8.78108014887989));
#403521=CARTESIAN_POINT('Ctrl Pts',(-0.741778521319334,-2.6419738327439,
8.78639403366323));
#403522=CARTESIAN_POINT('Ctrl Pts',(-0.749387942947467,-2.63921361930754,
8.78812224174741));
#403523=CARTESIAN_POINT('Ctrl Pts',(-0.729668620074122,-2.62907994584327,
8.78944554828685));
#403524=CARTESIAN_POINT('Ctrl Pts',(-0.733467909200736,-2.63314464998371,
8.79673892988686));
#403525=CARTESIAN_POINT('Ctrl Pts',(-0.740992567286101,-2.62836102426519,
8.79894799272499));
#403526=CARTESIAN_POINT('Origin',(-0.750228081562201,-2.63269141291484,
8.75721825406948));
#403527=CARTESIAN_POINT('Origin',(-0.750228081562201,-2.63269141291484,
9.));
#403528=CARTESIAN_POINT('Origin',(-0.750228081562201,-2.63269141291484,
7.51860402984325));
#403529=CARTESIAN_POINT('Ctrl Pts',(-0.734382618009671,-2.64632855949765,
7.50366195182966));
#403530=CARTESIAN_POINT('Ctrl Pts',(-0.735361839713509,-2.64985715929995,
7.50000065167735));
#403531=CARTESIAN_POINT('Ctrl Pts',(-0.735361839713621,-2.64985715929991,
7.49482233047108));
#403532=CARTESIAN_POINT('Ctrl Pts',(-0.741805881174942,-2.64582959698829,
7.50215800491337));
#403533=CARTESIAN_POINT('Ctrl Pts',(-0.744548032294539,-2.64730787450337,
7.49877273257268));
#403534=CARTESIAN_POINT('Ctrl Pts',(-0.747874451006705,-2.64638478463707,
7.49481816995647));
#403535=CARTESIAN_POINT('Ctrl Pts',(-0.743054712745854,-2.64330958983561,
7.51043025814041));
#403536=CARTESIAN_POINT('Ctrl Pts',(-0.748066763636952,-2.64630493670231,
7.51006209594513));
#403537=CARTESIAN_POINT('Ctrl Pts',(-0.753656215494947,-2.6447121410188,
7.50731281821699));
#403538=CARTESIAN_POINT('Ctrl Pts',(-0.741122625541046,-2.6412553296967,
7.51860402984325));
#403539=CARTESIAN_POINT('Ctrl Pts',(-0.746335839181204,-2.64679820087801,
7.51860402984325));
#403540=CARTESIAN_POINT('Ctrl Pts',(-0.753653780564773,-2.64471283489161,
7.51860402984325));
#403541=CARTESIAN_POINT('Origin',(0.,0.,7.5));
#403542=CARTESIAN_POINT('Origin',(-0.515891055659646,-2.61740223164621,
7.5));
#403543=CARTESIAN_POINT('',(-0.515891055659646,-2.61740223164621,7.59394543036555));
#403544=CARTESIAN_POINT('',(-0.515891055659646,-2.61740223164621,8.85049129520029));
#403545=CARTESIAN_POINT('',(-0.515891055659646,-2.61740223164621,7.5));
#403546=CARTESIAN_POINT('',(-0.561440886005583,-2.67250562312429,8.78727029226991));
#403547=CARTESIAN_POINT('Ctrl Pts',(-0.515891055659647,-2.61740223164621,
8.85049129520029));
#403548=CARTESIAN_POINT('Ctrl Pts',(-0.531096402804849,-2.63579672817757,
8.82945686509571));
#403549=CARTESIAN_POINT('Ctrl Pts',(-0.546279145362919,-2.6541638790656,
8.80838212259896));
#403550=CARTESIAN_POINT('Ctrl Pts',(-0.561440886005583,-2.67250562312429,
8.78727029226991));
#403551=CARTESIAN_POINT('',(-0.570375062512109,-2.68331364198703,8.75721825406948));
#403552=CARTESIAN_POINT('Origin',(-0.543488870576429,-2.65078869247601,
8.75937679713158));
#403553=CARTESIAN_POINT('',(-0.570375062512109,-2.68331364198703,7.51860402984325));
#403554=CARTESIAN_POINT('',(-0.570375062512109,-2.68331364198703,7.5));
#403555=CARTESIAN_POINT('Ctrl Pts',(-0.570375062512109,-2.68331364198703,
7.51860402984325));
#403556=CARTESIAN_POINT('Ctrl Pts',(-0.563358656393509,-2.67482562413524,
7.52834476460825));
#403557=CARTESIAN_POINT('Ctrl Pts',(-0.556337695325301,-2.66633209598475,
7.53807742314407));
#403558=CARTESIAN_POINT('Ctrl Pts',(-0.549312026368994,-2.65783287251993,
7.54780169004674));
#403559=CARTESIAN_POINT('Ctrl Pts',(-0.538183746447212,-2.6443705618955,
7.5632044032688));
#403560=CARTESIAN_POINT('Ctrl Pts',(-0.527043640891408,-2.63089394534418,
7.57858609112103));
#403561=CARTESIAN_POINT('Ctrl Pts',(-0.515891055659647,-2.61740223164621,
7.59394543036555));
#403562=CARTESIAN_POINT('Origin',(-0.421172437192773,-2.88192934915564,
7.5));
#403563=CARTESIAN_POINT('',(-0.478268870165641,-2.70125132133977,8.75721825406948));
#403564=CARTESIAN_POINT('',(-0.482494215215328,-2.68788048588352,8.78727029226991));
#403565=CARTESIAN_POINT('Origin',(-0.493219716927205,-2.65394031842054,
8.75658640620967));
#403566=CARTESIAN_POINT('',(-0.504036631578572,-2.61971088052921,8.85049129520029));
#403567=CARTESIAN_POINT('Ctrl Pts',(-0.482494215215328,-2.68788048588352,
8.78727029226991));
#403568=CARTESIAN_POINT('Ctrl Pts',(-0.489664835330383,-2.66518951495683,
8.80838212259895));
#403569=CARTESIAN_POINT('Ctrl Pts',(-0.496845388128006,-2.64246711268839,
8.82945686509571));
#403570=CARTESIAN_POINT('Ctrl Pts',(-0.504036631578572,-2.61971088052921,
8.85049129520029));
#403571=CARTESIAN_POINT('',(-0.504036631578572,-2.61971088052921,7.59394543036555));
#403572=CARTESIAN_POINT('',(-0.504036631578572,-2.61971088052921,7.5));
#403573=CARTESIAN_POINT('',(-0.478268870165641,-2.70125132133977,7.51860402984325));
#403574=CARTESIAN_POINT('Ctrl Pts',(-0.504036631578572,-2.61971088052921,
7.59394543036555));
#403575=CARTESIAN_POINT('Ctrl Pts',(-0.49876210842965,-2.63640177329775,
7.57858609112103));
#403576=CARTESIAN_POINT('Ctrl Pts',(-0.493493487440555,-2.65307398905726,
7.56320440326857));
#403577=CARTESIAN_POINT('Ctrl Pts',(-0.488230459287406,-2.66972850664335,
7.54780169004651));
#403578=CARTESIAN_POINT('Ctrl Pts',(-0.484907727133681,-2.68024308104382,
7.53807742314383));
#403579=CARTESIAN_POINT('Ctrl Pts',(-0.481587221536713,-2.69075060964715,
7.52834476460825));
#403580=CARTESIAN_POINT('Ctrl Pts',(-0.478268870165641,-2.70125132133977,
7.51860402984325));
#403581=CARTESIAN_POINT('',(-0.478268870165641,-2.70125132133977,7.5));
#403582=CARTESIAN_POINT('Origin',(-0.510592093294233,-2.62178248538885,
7.5));
#403583=CARTESIAN_POINT('Ctrl Pts',(-0.504036631578572,-2.61971088052921,
8.85049129520029));
#403584=CARTESIAN_POINT('Ctrl Pts',(-0.504094986504649,-2.61952622008007,
8.85097269580138));
#403585=CARTESIAN_POINT('Ctrl Pts',(-0.504160625639693,-2.61934642402759,
8.85143669361005));
#403586=CARTESIAN_POINT('Ctrl Pts',(-0.504237392721307,-2.61916351316932,
8.8519052845931));
#403587=CARTESIAN_POINT('Ctrl Pts',(-0.504387544264551,-2.61880575113034,
8.85282181883899));
#403588=CARTESIAN_POINT('Ctrl Pts',(-0.504576586788855,-2.61844535224755,
8.85372622499635));
#403589=CARTESIAN_POINT('Ctrl Pts',(-0.504821141016042,-2.61808382343919,
8.8546225773507));
#403590=CARTESIAN_POINT('Ctrl Pts',(-0.505024161249708,-2.61778369506278,
8.85536669723986));
#403591=CARTESIAN_POINT('Ctrl Pts',(-0.505265458768475,-2.61748270182885,
8.85610498449051));
#403592=CARTESIAN_POINT('Ctrl Pts',(-0.505560807192758,-2.61718668585866,
8.85681338218371));
#403593=CARTESIAN_POINT('Ctrl Pts',(-0.50582883635165,-2.61691805090081,
8.85745625420284));
#403594=CARTESIAN_POINT('Ctrl Pts',(-0.506144318101241,-2.61664972254577,
8.85808743050666));
#403595=CARTESIAN_POINT('Ctrl Pts',(-0.506533369387157,-2.61639335202953,
8.85866804508411));
#403596=CARTESIAN_POINT('Ctrl Pts',(-0.506712869216879,-2.61627506823078,
8.85893592806396));
#403597=CARTESIAN_POINT('Ctrl Pts',(-0.506908237766522,-2.61615945434576,
8.85919241173848));
#403598=CARTESIAN_POINT('Ctrl Pts',(-0.507123281853322,-2.61604865749327,
8.85943017985534));
#403599=CARTESIAN_POINT('Ctrl Pts',(-0.507413655030366,-2.61589904894303,
8.8597512372));
#403600=CARTESIAN_POINT('Ctrl Pts',(-0.507747586735349,-2.61575498477418,
8.86004599534705));
#403601=CARTESIAN_POINT('Ctrl Pts',(-0.508125190597107,-2.61562775896039,
8.86026130871721));
#403602=CARTESIAN_POINT('Ctrl Pts',(-0.508263442016677,-2.61558117800309,
8.86034014101235));
#403603=CARTESIAN_POINT('Ctrl Pts',(-0.508409620434284,-2.61553614284821,
8.86040910639693));
#403604=CARTESIAN_POINT('Ctrl Pts',(-0.508559842340078,-2.6154942019216,
8.86046313645507));
#403605=CARTESIAN_POINT('Ctrl Pts',(-0.508794262365973,-2.61542875345688,
8.8605474499083));
#403606=CARTESIAN_POINT('Ctrl Pts',(-0.509044967329427,-2.61536919493121,
8.86059655985668));
#403607=CARTESIAN_POINT('Ctrl Pts',(-0.509295811046183,-2.6153190609893,
8.86059725258816));
#403608=CARTESIAN_POINT('Ctrl Pts',(-0.509547234312138,-2.61526881121795,
8.86059794692011));
#403609=CARTESIAN_POINT('Ctrl Pts',(-0.509802105972871,-2.61523007760143,
8.86056369958366));
#403610=CARTESIAN_POINT('Ctrl Pts',(-0.510045959806705,-2.61520125230872,
8.86048590497774));
#403611=CARTESIAN_POINT('Ctrl Pts',(-0.510109598396932,-2.61519372976556,
8.86046560290182));
#403612=CARTESIAN_POINT('Ctrl Pts',(-0.510173325147816,-2.61518687412201,
8.86044257503091));
#403613=CARTESIAN_POINT('Ctrl Pts',(-0.510235167338859,-2.61518086458527,
8.86041778462583));
#403614=CARTESIAN_POINT('Ctrl Pts',(-0.510651288544813,-2.61514042786026,
8.86025097596201));
#403615=CARTESIAN_POINT('Ctrl Pts',(-0.511037954093436,-2.61513320389167,
8.8599848982295));
#403616=CARTESIAN_POINT('Ctrl Pts',(-0.511383719971671,-2.61515093251763,
8.85968173251461));
#403617=CARTESIAN_POINT('Ctrl Pts',(-0.511566610311235,-2.61516030994504,
8.85952137522076));
#403618=CARTESIAN_POINT('Ctrl Pts',(-0.511741592847482,-2.61517665866632,
8.85934740853961));
#403619=CARTESIAN_POINT('Ctrl Pts',(-0.511906344552771,-2.61519820031704,
8.8591675900182));
#403620=CARTESIAN_POINT('Ctrl Pts',(-0.51256790828575,-2.61528470124179,
8.85844552518694));
#403621=CARTESIAN_POINT('Ctrl Pts',(-0.513102288376403,-2.61545682350229,
8.85759444184122));
#403622=CARTESIAN_POINT('Ctrl Pts',(-0.513525387806247,-2.61563629809097,
8.85683498915135));
#403623=CARTESIAN_POINT('Ctrl Pts',(-0.513569664034767,-2.61565507962869,
8.85675551444996));
#403624=CARTESIAN_POINT('Ctrl Pts',(-0.513612710375468,-2.61567395818293,
8.8566769979365));
#403625=CARTESIAN_POINT('Ctrl Pts',(-0.513654537106076,-2.6156928545144,
8.85659965593547));
#403626=CARTESIAN_POINT('Ctrl Pts',(-0.514219116450211,-2.61594791816087,
8.85555568965886));
#403627=CARTESIAN_POINT('Ctrl Pts',(-0.514724875940997,-2.61627458655635,
8.85434650606346));
#403628=CARTESIAN_POINT('Ctrl Pts',(-0.515177687654596,-2.61666925409151,
8.85297329937117));
#403629=CARTESIAN_POINT('Ctrl Pts',(-0.515432366653272,-2.61689123053259,
8.85220095427747));
#403630=CARTESIAN_POINT('Ctrl Pts',(-0.515670193285102,-2.61713504588954,
8.85137579139183));
#403631=CARTESIAN_POINT('Ctrl Pts',(-0.515891055659646,-2.61740223164621,
8.85049129520029));
#403632=CARTESIAN_POINT('Origin',(-0.510592093294233,-2.62178248538885,
7.59394543036555));
#403633=CARTESIAN_POINT('Ctrl Pts',(-0.504206055614823,-2.61917474895074,
7.59443877723642));
#403634=CARTESIAN_POINT('Ctrl Pts',(-0.505950960172775,-2.61365310954452,
7.58783886950016));
#403635=CARTESIAN_POINT('Ctrl Pts',(-0.514418553684599,-2.61426877313379,
7.58559994247159));
#403636=CARTESIAN_POINT('Ctrl Pts',(-0.494680672826292,-2.64931721647128,
7.56670252222134));
#403637=CARTESIAN_POINT('Ctrl Pts',(-0.496423055501789,-2.64380355740164,
7.56004874999026));
#403638=CARTESIAN_POINT('Ctrl Pts',(-0.504942371819622,-2.64440155968668,
7.55786368756704));
#403639=CARTESIAN_POINT('Ctrl Pts',(-0.485173077738411,-2.67940339594534,
7.53888913333558));
#403640=CARTESIAN_POINT('Ctrl Pts',(-0.486925815479463,-2.67385696892985,
7.53222002137275));
#403641=CARTESIAN_POINT('Ctrl Pts',(-0.495482437381228,-2.67447879394538,
7.53005029815327));
#403642=CARTESIAN_POINT('Ctrl Pts',(-0.475683700576297,-2.70943192595292,
7.51101258149734));
#403643=CARTESIAN_POINT('Ctrl Pts',(-0.47745768468355,-2.70381826616392,
7.5043616886572));
#403644=CARTESIAN_POINT('Ctrl Pts',(-0.486039296596616,-2.70449901466241,
7.50217374673251));
#403645=CARTESIAN_POINT('',(-0.486543193738921,-2.70289709681368,7.50366116523517));
#403646=CARTESIAN_POINT('Ctrl Pts',(-0.47826887016564,-2.70125132133977,
7.51860402984325));
#403647=CARTESIAN_POINT('Ctrl Pts',(-0.478135801956128,-2.70167240721866,
7.51734760759493));
#403648=CARTESIAN_POINT('Ctrl Pts',(-0.478072287298096,-2.70207084635854,
7.51608817408573));
#403649=CARTESIAN_POINT('Ctrl Pts',(-0.478091659423101,-2.70244782447943,
7.5148100591312));
#403650=CARTESIAN_POINT('Ctrl Pts',(-0.478109207156843,-2.70278930026951,
7.51365231206383));
#403651=CARTESIAN_POINT('Ctrl Pts',(-0.478194539795425,-2.70311366110739,
7.51247773061043));
#403652=CARTESIAN_POINT('Ctrl Pts',(-0.47838189073192,-2.70340589983577,
7.51129758471022));
#403653=CARTESIAN_POINT('Ctrl Pts',(-0.478614746549699,-2.70376911920023,
7.50983079813402));
#403654=CARTESIAN_POINT('Ctrl Pts',(-0.47900873000128,-2.70406409599668,
7.50839324291155));
#403655=CARTESIAN_POINT('Ctrl Pts',(-0.479616125507365,-2.70422699034869,
7.50715379678855));
#403656=CARTESIAN_POINT('Ctrl Pts',(-0.479896724729495,-2.70430224284564,
7.50658120839351));
#403657=CARTESIAN_POINT('Ctrl Pts',(-0.480265220758804,-2.70435082705869,
7.50598221009429));
#403658=CARTESIAN_POINT('Ctrl Pts',(-0.480715817181755,-2.7043490354212,
7.50545747549612));
#403659=CARTESIAN_POINT('Ctrl Pts',(-0.480956269380306,-2.70434807934797,
7.50517746087247));
#403660=CARTESIAN_POINT('Ctrl Pts',(-0.481222708816406,-2.70433297027813,
7.50491486231392));
#403661=CARTESIAN_POINT('Ctrl Pts',(-0.481507985287821,-2.7043024429845,
7.50468370960993));
#403662=CARTESIAN_POINT('Ctrl Pts',(-0.481934563597949,-2.70425679505124,
7.50433806340447));
#403663=CARTESIAN_POINT('Ctrl Pts',(-0.482415993154648,-2.70417475013281,
7.50405484070984));
#403664=CARTESIAN_POINT('Ctrl Pts',(-0.482919730220015,-2.70406112758864,
7.50385766036131));
#403665=CARTESIAN_POINT('Ctrl Pts',(-0.482973597069306,-2.70404897742364,
7.50383657498791));
#403666=CARTESIAN_POINT('Ctrl Pts',(-0.483027698355602,-2.70403648561238,
7.50381643264937));
#403667=CARTESIAN_POINT('Ctrl Pts',(-0.483081979503577,-2.70402367240709,
7.50379723213559));
#403668=CARTESIAN_POINT('Ctrl Pts',(-0.483444323922925,-2.70393814007029,
7.50366906242519));
#403669=CARTESIAN_POINT('Ctrl Pts',(-0.483822399615178,-2.70383572607388,
7.50358235568538));
#403670=CARTESIAN_POINT('Ctrl Pts',(-0.484184445158451,-2.70372825171679,
7.5035341175365));
#403671=CARTESIAN_POINT('Ctrl Pts',(-0.484727291474945,-2.70356710608208,
7.50346178989176));
#403672=CARTESIAN_POINT('Ctrl Pts',(-0.485304418855301,-2.70337066885157,
7.50346967198527));
#403673=CARTESIAN_POINT('Ctrl Pts',(-0.485865045427639,-2.70316039527586,
7.50354272648693));
#403674=CARTESIAN_POINT('Ctrl Pts',(-0.486095642741125,-2.70307390540177,
7.5035727753156));
#403675=CARTESIAN_POINT('Ctrl Pts',(-0.48632319177811,-2.70298532231186,
7.50361331098761));
#403676=CARTESIAN_POINT('Ctrl Pts',(-0.486543193739172,-2.70289709681507,
7.50366116523659));
#403677=CARTESIAN_POINT('',(-0.511151791457271,-2.62465641716278,7.57603338622103));
#403678=CARTESIAN_POINT('Origin',(-0.512843849057443,-2.63332984962537,
7.58486873427628));
#403679=CARTESIAN_POINT('Ctrl Pts',(-0.486543193716677,-2.70289709686653,
7.50366116529969));
#403680=CARTESIAN_POINT('Ctrl Pts',(-0.494733471570603,-2.6768596786482,
7.52783573079709));
#403681=CARTESIAN_POINT('Ctrl Pts',(-0.502935967272741,-2.65078068885653,
7.55196141284068));
#403682=CARTESIAN_POINT('Ctrl Pts',(-0.511151790759568,-2.62465641820242,
7.57603338728831));
#403683=CARTESIAN_POINT('Ctrl Pts',(-0.503894391761617,-2.62074446814268,
7.59639677331371));
#403684=CARTESIAN_POINT('Ctrl Pts',(-0.506703515972818,-2.60181546269509,
7.59974925422225));
#403685=CARTESIAN_POINT('Ctrl Pts',(-0.516410771457498,-2.61830690341518,
7.59639677331372));
#403686=CARTESIAN_POINT('Ctrl Pts',(-0.503839346059824,-2.61684420224733,
7.58707626057422));
#403687=CARTESIAN_POINT('Ctrl Pts',(-0.508673304164277,-2.61192990874306,
7.58811717123965));
#403688=CARTESIAN_POINT('Ctrl Pts',(-0.514998153140088,-2.61467102476307,
7.58707626057425));
#403689=CARTESIAN_POINT('Ctrl Pts',(-0.508250440815455,-2.62102366098244,
7.5801537675693));
#403690=CARTESIAN_POINT('Ctrl Pts',(-0.509994474415078,-2.61871383875086,
7.5820876076604));
#403691=CARTESIAN_POINT('Ctrl Pts',(-0.512477848454491,-2.62020037341847,
7.5801537675693));
#403692=CARTESIAN_POINT('Ctrl Pts',(-0.511151791298875,-2.62465641635051,
7.57603338509286));
#403693=CARTESIAN_POINT('Ctrl Pts',(-0.511151791298874,-2.62465641635051,
7.57603338509286));
#403694=CARTESIAN_POINT('Ctrl Pts',(-0.511151791298874,-2.62465641635051,
7.57603338509286));
#403695=CARTESIAN_POINT('Origin',(-0.512838247935145,-2.63333094044376,
7.58486873427623));
#403696=CARTESIAN_POINT('Ctrl Pts',(-0.575858486682835,-2.68994715228608,
7.51098857897448));
#403697=CARTESIAN_POINT('Ctrl Pts',(-0.572107512685101,-2.68540945396642,
7.50433767179956));
#403698=CARTESIAN_POINT('Ctrl Pts',(-0.564408512768212,-2.68926087595865,
7.50214974420965));
#403699=CARTESIAN_POINT('Ctrl Pts',(-0.55578813636867,-2.66566727325987,
7.53887321589168));
#403700=CARTESIAN_POINT('Ctrl Pts',(-0.552082105696198,-2.66118394461909,
7.53220407452066));
#403701=CARTESIAN_POINT('Ctrl Pts',(-0.544384150308563,-2.66497134514865,
7.53003438070912));
#403702=CARTESIAN_POINT('Ctrl Pts',(-0.535679243578268,-2.64134076790947,
7.56669465659234));
#403703=CARTESIAN_POINT('Ctrl Pts',(-0.531995114858089,-2.63688393490737,
7.56004085833301));
#403704=CARTESIAN_POINT('Ctrl Pts',(-0.524322805054464,-2.64063524299976,
7.55785582193788));
#403705=CARTESIAN_POINT('Ctrl Pts',(-0.515532717756325,-2.6169687364253,
7.59443891967696));
#403706=CARTESIAN_POINT('Ctrl Pts',(-0.511843247508166,-2.61250544157026,
7.58783901202978));
#403707=CARTESIAN_POINT('Ctrl Pts',(-0.504225531563111,-2.61625371874368,
7.58560008491213));
#403708=CARTESIAN_POINT('',(-0.563323058569129,-2.68794421947737,7.50366116523517));
#403709=CARTESIAN_POINT('Ctrl Pts',(-0.563323058569206,-2.68794421947773,
7.50366116523554));
#403710=CARTESIAN_POINT('Ctrl Pts',(-0.564080772490016,-2.68794154908911,
7.50350835821027));
#403711=CARTESIAN_POINT('Ctrl Pts',(-0.564777208608298,-2.687914442922,
7.50345484956));
#403712=CARTESIAN_POINT('Ctrl Pts',(-0.565433095890495,-2.68786269513525,
7.50349758195598));
#403713=CARTESIAN_POINT('Ctrl Pts',(-0.565769614708131,-2.68783614468294,
7.50351950684424));
#403714=CARTESIAN_POINT('Ctrl Pts',(-0.566128638073183,-2.68780061956941,
7.50357029184312));
#403715=CARTESIAN_POINT('Ctrl Pts',(-0.566473898535893,-2.68775684670366,
7.50365515313924));
#403716=CARTESIAN_POINT('Ctrl Pts',(-0.567005048937309,-2.68768950631076,
7.50378570417639));
#403717=CARTESIAN_POINT('Ctrl Pts',(-0.567519261867576,-2.6876010137059,
7.50400001621911));
#403718=CARTESIAN_POINT('Ctrl Pts',(-0.567977013192528,-2.68749586693788,
7.50428903009635));
#403719=CARTESIAN_POINT('Ctrl Pts',(-0.568027820067869,-2.68748419645558,
7.50432110841318));
#403720=CARTESIAN_POINT('Ctrl Pts',(-0.568077959553052,-2.68747233198995,
7.50435406373354));
#403721=CARTESIAN_POINT('Ctrl Pts',(-0.568127398514586,-2.68746028766373,
7.50438785222352));
#403722=CARTESIAN_POINT('Ctrl Pts',(-0.568429247138146,-2.68738675126291,
7.50459414719561));
#403723=CARTESIAN_POINT('Ctrl Pts',(-0.56870966607664,-2.68730483834955,
7.50483629897752));
#403724=CARTESIAN_POINT('Ctrl Pts',(-0.568958281566951,-2.68721895022315,
7.5050991045531));
#403725=CARTESIAN_POINT('Ctrl Pts',(-0.56950675230964,-2.68702947238968,
7.50567888004914));
#403726=CARTESIAN_POINT('Ctrl Pts',(-0.569922222282166,-2.68681367292768,
7.50637912803144));
#403727=CARTESIAN_POINT('Ctrl Pts',(-0.570225606143961,-2.68659431134895,
7.50710440483569));
#403728=CARTESIAN_POINT('Ctrl Pts',(-0.570300001889887,-2.68654051953491,
7.50728225710685));
#403729=CARTESIAN_POINT('Ctrl Pts',(-0.570369224095793,-2.68648556096084,
7.50746498566954));
#403730=CARTESIAN_POINT('Ctrl Pts',(-0.570431915928539,-2.68643104480392,
7.50764697238949));
#403731=CARTESIAN_POINT('Ctrl Pts',(-0.570768929968127,-2.68613798094756,
7.50862528291181));
#403732=CARTESIAN_POINT('Ctrl Pts',(-0.570950535870602,-2.68583422188777,
7.50965856837421));
#403733=CARTESIAN_POINT('Ctrl Pts',(-0.571040685959693,-2.68553724607221,
7.51067959873201));
#403734=CARTESIAN_POINT('Ctrl Pts',(-0.57109029566743,-2.68537381990632,
7.51124147302578));
#403735=CARTESIAN_POINT('Ctrl Pts',(-0.571111806105371,-2.6852122818537,
7.51180065547252));
#403736=CARTESIAN_POINT('Ctrl Pts',(-0.571113248871035,-2.6850548511387,
7.512351757165));
#403737=CARTESIAN_POINT('Ctrl Pts',(-0.571118234201136,-2.68451086530544,
7.51425603304536));
#403738=CARTESIAN_POINT('Ctrl Pts',(-0.570878146117201,-2.68395100448379,
7.51626900505181));
#403739=CARTESIAN_POINT('Ctrl Pts',(-0.570446802542556,-2.68340258713865,
7.51827788969244));
#403740=CARTESIAN_POINT('Ctrl Pts',(-0.57042345741317,-2.68337290575557,
7.51838661432546));
#403741=CARTESIAN_POINT('Ctrl Pts',(-0.570399542264663,-2.68334325609048,
7.51849533314857));
#403742=CARTESIAN_POINT('Ctrl Pts',(-0.570375062512112,-2.68331364198702,
7.51860402984325));
#403743=CARTESIAN_POINT('Ctrl Pts',(-0.511151792494592,-2.62465641786574,
7.57603338728984));
#403744=CARTESIAN_POINT('Ctrl Pts',(-0.528570753766828,-2.64578831464073,
7.55196141284922));
#403745=CARTESIAN_POINT('Ctrl Pts',(-0.545960368888816,-2.66688324131612,
7.52783573083105));
#403746=CARTESIAN_POINT('Ctrl Pts',(-0.56332305861081,-2.68794421951938,
7.50366116530176));
#403747=CARTESIAN_POINT('Origin',(-1.76626572250569E-16,-9.06940118467444E-16,
7.49482233047033));
#403748=CARTESIAN_POINT('Origin',(-0.484977299960275,-2.69419807522076,
7.49482233047033));
#403749=CARTESIAN_POINT('Origin',(0.,0.,7.50366116523517));
#403750=CARTESIAN_POINT('Origin',(-0.561510055974226,-2.67929332232211,
7.49482233047033));
#403751=CARTESIAN_POINT('Ctrl Pts',(-0.478269188839834,-2.70125031276705,
7.51860402984325));
#403752=CARTESIAN_POINT('Ctrl Pts',(-0.475977037628241,-2.70850581611646,
7.51860402984325));
#403753=CARTESIAN_POINT('Ctrl Pts',(-0.468479300229117,-2.70980204909083,
7.51860402984325));
#403754=CARTESIAN_POINT('Ctrl Pts',(-0.477418096240812,-2.70394433029203,
7.51041458714366));
#403755=CARTESIAN_POINT('Ctrl Pts',(-0.47420073607419,-2.70881289880017,
7.51004642900442));
#403756=CARTESIAN_POINT('Ctrl Pts',(-0.468477232442164,-2.70980240657649,
7.5072913648301));
#403757=CARTESIAN_POINT('Ctrl Pts',(-0.479644958150266,-2.70566619649922,
7.50215815450138));
#403758=CARTESIAN_POINT('Ctrl Pts',(-0.4778174872025,-2.70818778615984,
7.4987716367153));
#403759=CARTESIAN_POINT('Ctrl Pts',(-0.47442185931465,-2.70879904293209,
7.49481588533171));
#403760=CARTESIAN_POINT('Ctrl Pts',(-0.486543096209253,-2.7028965550037,
7.50366171572174));
#403761=CARTESIAN_POINT('Ctrl Pts',(-0.487191808179652,-2.70650034953677,
7.50000045605858));
#403762=CARTESIAN_POINT('Ctrl Pts',(-0.487191808179529,-2.70650034953679,
7.49482233047317));
#403763=CARTESIAN_POINT('Origin',(-0.466349848864439,-2.69748476704951,
7.51860402984325));
#403764=CARTESIAN_POINT('Origin',(-0.466349848864439,-2.69748476704951,
9.));
#403765=CARTESIAN_POINT('Origin',(-0.46634984886444,-2.69748476704951,8.75721825406948));
#403766=CARTESIAN_POINT('Ctrl Pts',(-0.483301006437013,-2.68532734615808,
8.78942910404913));
#403767=CARTESIAN_POINT('Ctrl Pts',(-0.481641165693878,-2.69064687220925,
8.7967269950169));
#403768=CARTESIAN_POINT('Ctrl Pts',(-0.472776992362339,-2.68959810286835,
8.79893251111267));
#403769=CARTESIAN_POINT('Ctrl Pts',(-0.479988149754494,-2.69581068528936,
8.78111911759583));
#403770=CARTESIAN_POINT('Ctrl Pts',(-0.478013283372321,-2.70211482780821,
8.78644465894815));
#403771=CARTESIAN_POINT('Ctrl Pts',(-0.469945969403999,-2.70291104204565,
8.78817647674132));
#403772=CARTESIAN_POINT('Ctrl Pts',(-0.477923498420511,-2.70234415227764,
8.7678092393203));
#403773=CARTESIAN_POINT('Ctrl Pts',(-0.47558738927346,-2.7097844030008,
8.76988516158372));
#403774=CARTESIAN_POINT('Ctrl Pts',(-0.468166832892793,-2.71122375125525,
8.77093053738833));
#403775=CARTESIAN_POINT('Ctrl Pts',(-0.478326077172247,-2.70107021563117,
8.75371302330492));
#403776=CARTESIAN_POINT('Ctrl Pts',(-0.476048030768691,-2.70832808762997,
8.75300828287559));
#403777=CARTESIAN_POINT('Ctrl Pts',(-0.468513389351372,-2.70960233958568,
8.75267964240738));
#403778=CARTESIAN_POINT('Origin',(-0.470575193914126,-2.68411393159326,
8.78727029226991));
#403779=CARTESIAN_POINT('Ctrl Pts',(-0.504036631578572,-2.61971088052921,
8.85049129520029));
#403780=CARTESIAN_POINT('Ctrl Pts',(-0.502277013195061,-2.62527908089984,
8.85711686593484));
#403781=CARTESIAN_POINT('Ctrl Pts',(-0.493751728365434,-2.62463079031095,
8.85933012996512));
#403782=CARTESIAN_POINT('Ctrl Pts',(-0.49684537847709,-2.6424671432281,
8.82945683644722));
#403783=CARTESIAN_POINT('Ctrl Pts',(-0.495071154197114,-2.64808156302841,
8.83607469902389));
#403784=CARTESIAN_POINT('Ctrl Pts',(-0.486523682952861,-2.64739397461503,
8.83829567148519));
#403785=CARTESIAN_POINT('Ctrl Pts',(-0.48966484451826,-2.66518948588238,
8.80838214965002));
#403786=CARTESIAN_POINT('Ctrl Pts',(-0.487883618320902,-2.67082606280457,
8.81501364461992));
#403787=CARTESIAN_POINT('Ctrl Pts',(-0.479307239296707,-2.67012283067464,
8.81722098428721));
#403788=CARTESIAN_POINT('Ctrl Pts',(-0.482494215215328,-2.68788048588352,
8.78727029226991));
#403789=CARTESIAN_POINT('Ctrl Pts',(-0.480712693150447,-2.69351799905962,
8.79393457792714));
#403790=CARTESIAN_POINT('Ctrl Pts',(-0.472101526741951,-2.69281998167918,
8.79610912703474));
#403791=CARTESIAN_POINT('Origin',(-0.49211761027737,-2.61594432623894,8.85049129520029));
#403792=CARTESIAN_POINT('Ctrl Pts',(-0.515891055659646,-2.61740223164621,
8.85049129520029));
#403793=CARTESIAN_POINT('Ctrl Pts',(-0.519611637301511,-2.6219031631575,
8.85711686593484));
#403794=CARTESIAN_POINT('Ctrl Pts',(-0.527270584603657,-2.61810299364327,
8.85933012996512));
#403795=CARTESIAN_POINT('Ctrl Pts',(-0.512599510788254,-2.61342032250981,
8.86332496987231));
#403796=CARTESIAN_POINT('Ctrl Pts',(-0.517180599096329,-2.61281573646103,
8.86648636486738));
#403797=CARTESIAN_POINT('Ctrl Pts',(-0.51804914848623,-2.60697435615754,
8.87206031107457));
#403798=CARTESIAN_POINT('Ctrl Pts',(-0.505603918890411,-2.61475129959254,
8.86341338519877));
#403799=CARTESIAN_POINT('Ctrl Pts',(-0.501110700619822,-2.61588463988002,
8.86654584966058));
#403800=CARTESIAN_POINT('Ctrl Pts',(-0.498154264204961,-2.61074813946514,
8.87215952290714));
#403801=CARTESIAN_POINT('Ctrl Pts',(-0.504036631578572,-2.61971088052921,
8.85049129520029));
#403802=CARTESIAN_POINT('Ctrl Pts',(-0.502277013195061,-2.62527908089984,
8.85711686593484));
#403803=CARTESIAN_POINT('Ctrl Pts',(-0.493751728365435,-2.62463079031095,
8.85933012996512));
#403804=CARTESIAN_POINT('Origin',(-0.525525532687672,-2.60943813393232,
8.85049129520029));
#403805=CARTESIAN_POINT('Ctrl Pts',(-0.561440886005583,-2.67250562312429,
8.78727029226991));
#403806=CARTESIAN_POINT('Ctrl Pts',(-0.565207781345668,-2.67706258210757,
8.79393457792714));
#403807=CARTESIAN_POINT('Ctrl Pts',(-0.572927672898287,-2.67318409147408,
8.79610912703474));
#403808=CARTESIAN_POINT('Ctrl Pts',(-0.546279125935841,-2.65416385556391,
8.80838214965003));
#403809=CARTESIAN_POINT('Ctrl Pts',(-0.550045395686168,-2.65872005774707,
8.81501364461994));
#403810=CARTESIAN_POINT('Ctrl Pts',(-0.557731085305896,-2.65484978803239,
8.81722098428722));
#403811=CARTESIAN_POINT('Ctrl Pts',(-0.531096423210991,-2.63579675286367,
8.82945683644724));
#403812=CARTESIAN_POINT('Ctrl Pts',(-0.534847887929972,-2.64033504482783,
8.8360746990239));
#403813=CARTESIAN_POINT('Ctrl Pts',(-0.542512653014741,-2.63649012367217,
8.83829567148519));
#403814=CARTESIAN_POINT('Ctrl Pts',(-0.515891055659647,-2.61740223164621,
8.85049129520029));
#403815=CARTESIAN_POINT('Ctrl Pts',(-0.519611637301512,-2.6219031631575,
8.85711686593484));
#403816=CARTESIAN_POINT('Ctrl Pts',(-0.527270584603657,-2.61810299364327,
8.85933012996512));
#403817=CARTESIAN_POINT('Origin',(-0.571075363033608,-2.6645415254104,8.78727029226991));
#403818=CARTESIAN_POINT('Ctrl Pts',(-0.570257105423824,-2.68317091578167,
8.75374538247847));
#403819=CARTESIAN_POINT('Ctrl Pts',(-0.57508850042324,-2.68903623766093,
8.75304829418601));
#403820=CARTESIAN_POINT('Ctrl Pts',(-0.582543965794282,-2.68739712835698,
8.75272238421917));
#403821=CARTESIAN_POINT('Ctrl Pts',(-0.571098103415368,-2.68418830424843,
8.76769408445022));
#403822=CARTESIAN_POINT('Ctrl Pts',(-0.576051610414045,-2.69020078488342,
8.76974318093972));
#403823=CARTESIAN_POINT('Ctrl Pts',(-0.583462952756313,-2.68875497647084,
8.7707786988043));
#403824=CARTESIAN_POINT('Ctrl Pts',(-0.566787626784249,-2.67897375054521,
8.78108014887986));
#403825=CARTESIAN_POINT('Ctrl Pts',(-0.5709826131446,-2.68407152719164,
8.78639403366322));
#403826=CARTESIAN_POINT('Ctrl Pts',(-0.578753247881951,-2.68180452222744,
8.78812224174741));
#403827=CARTESIAN_POINT('Ctrl Pts',(-0.559723707160403,-2.67042824812776,
8.78944554828686));
#403828=CARTESIAN_POINT('Ctrl Pts',(-0.5632547637516,-2.67472802218773,
8.79673892988686));
#403829=CARTESIAN_POINT('Ctrl Pts',(-0.571070449572005,-2.67043633144009,
8.79894799272499));
#403830=CARTESIAN_POINT('Origin',(-0.580009539540134,-2.67534954427313,
8.75721825406948));
#403831=CARTESIAN_POINT('Origin',(-0.580009539540134,-2.67534954427313,
9.));
#403832=CARTESIAN_POINT('Origin',(-0.580009539540134,-2.67534954427313,
7.51860402984325));
#403833=CARTESIAN_POINT('Ctrl Pts',(-0.563322897210423,-2.6879434495402,
7.50366195182966));
#403834=CARTESIAN_POINT('Ctrl Pts',(-0.564074028832693,-2.69152753840574,
7.50000065167735));
#403835=CARTESIAN_POINT('Ctrl Pts',(-0.564074028832807,-2.69152753840572,
7.49482233047108));
#403836=CARTESIAN_POINT('Ctrl Pts',(-0.57076287712312,-2.68792112230681,
7.50215800491337));
#403837=CARTESIAN_POINT('Ctrl Pts',(-0.573404680633563,-2.68957205276764,
7.49877273257264));
#403838=CARTESIAN_POINT('Ctrl Pts',(-0.576783407432534,-2.68886398386711,
7.49481816995649));
#403839=CARTESIAN_POINT('Ctrl Pts',(-0.572170600248251,-2.68548630569255,
7.51043025814043));
#403840=CARTESIAN_POINT('Ctrl Pts',(-0.576980440810586,-2.68879662150103,
7.51006209594516));
#403841=CARTESIAN_POINT('Ctrl Pts',(-0.582660459310099,-2.68756521579719,
7.50731281821699));
#403842=CARTESIAN_POINT('Ctrl Pts',(-0.570374099622813,-2.68331247699918,
7.51860402984326));
#403843=CARTESIAN_POINT('Ctrl Pts',(-0.57522146918052,-2.68917797150193,
7.51860402984326));
#403844=CARTESIAN_POINT('Ctrl Pts',(-0.582657984926167,-2.68756575223785,
7.51860402984327));
#403845=CARTESIAN_POINT('Origin',(0.,0.,7.5));
#403846=CARTESIAN_POINT('Origin',(-0.34713356539707,-2.64507775146798,7.5));
#403847=CARTESIAN_POINT('',(-0.34713356539707,-2.64507775146798,7.59394543036555));
#403848=CARTESIAN_POINT('',(-0.34713356539707,-2.64507775146798,8.85049129520029));
#403849=CARTESIAN_POINT('',(-0.34713356539707,-2.64507775146798,7.5));
#403850=CARTESIAN_POINT('',(-0.389059322317672,-2.7029863147688,8.78727029226991));
#403851=CARTESIAN_POINT('Ctrl Pts',(-0.34713356539707,-2.64507775146798,
8.85049129520029));
#403852=CARTESIAN_POINT('Ctrl Pts',(-0.361129132086595,-2.66440866446988,
8.82945686509571));
#403853=CARTESIAN_POINT('Ctrl Pts',(-0.37510389267392,-2.68371083973216,
8.80838212259896));
#403854=CARTESIAN_POINT('Ctrl Pts',(-0.389059322317672,-2.7029863147688,
8.78727029226991));
#403855=CARTESIAN_POINT('',(-0.397282670454287,-2.71434454205174,8.75721825406948));
#403856=CARTESIAN_POINT('Origin',(-0.372535599752971,-2.68016381430528,
8.75937679713133));
#403857=CARTESIAN_POINT('',(-0.397282670454287,-2.71434454205174,7.51860402984325));
#403858=CARTESIAN_POINT('',(-0.397282670454287,-2.71434454205174,7.5));
#403859=CARTESIAN_POINT('Ctrl Pts',(-0.397282670454287,-2.71434454205174,
7.51860402984325));
#403860=CARTESIAN_POINT('Ctrl Pts',(-0.39082450946553,-2.70542442105947,
7.52834476460825));
#403861=CARTESIAN_POINT('Ctrl Pts',(-0.384362155931846,-2.69649850925338,
7.53807742314407));
#403862=CARTESIAN_POINT('Ctrl Pts',(-0.377895469082967,-2.68756661219917,
7.54780169004674));
#403863=CARTESIAN_POINT('Ctrl Pts',(-0.367652586608945,-2.67341896999315,
7.5632044032688));
#403864=CARTESIAN_POINT('Ctrl Pts',(-0.357398819381816,-2.65925629358233,
7.57858609112103));
#403865=CARTESIAN_POINT('Ctrl Pts',(-0.34713356539707,-2.64507775146798,
7.59394543036555));
#403866=CARTESIAN_POINT('Origin',(-0.235661245880683,-2.9029927269226,7.5));
#403867=CARTESIAN_POINT('',(-0.304216449096279,-2.72634410251322,8.75721825406948));
#403868=CARTESIAN_POINT('',(-0.309289785090403,-2.71327145765926,8.78727029226991));
#403869=CARTESIAN_POINT('Origin',(-0.322167804103753,-2.68008820916575,
8.7565864062101));
#403870=CARTESIAN_POINT('',(-0.33515558185986,-2.64662214142563,8.85049129520029));
#403871=CARTESIAN_POINT('Ctrl Pts',(-0.309289785090403,-2.71327145765926,
8.78727029226991));
#403872=CARTESIAN_POINT('Ctrl Pts',(-0.317899487896232,-2.69108653097411,
8.80838212259896));
#403873=CARTESIAN_POINT('Ctrl Pts',(-0.326521116789851,-2.66887087391543,
8.82945686509571));
#403874=CARTESIAN_POINT('Ctrl Pts',(-0.33515558185986,-2.64662214142563,
8.85049129520029));
#403875=CARTESIAN_POINT('',(-0.33515558185986,-2.64662214142563,7.59394543036555));
#403876=CARTESIAN_POINT('',(-0.33515558185986,-2.64662214142563,7.5));
#403877=CARTESIAN_POINT('',(-0.304216449096279,-2.72634410251322,7.51860402984325));
#403878=CARTESIAN_POINT('Ctrl Pts',(-0.335155581859861,-2.64662214142562,
7.59394543036555));
#403879=CARTESIAN_POINT('Ctrl Pts',(-0.328822506613084,-2.66294080110644,
7.57858609112103));
#403880=CARTESIAN_POINT('Ctrl Pts',(-0.322496518039592,-2.67924120030481,
7.56320440326857));
#403881=CARTESIAN_POINT('Ctrl Pts',(-0.316177244736828,-2.69552429602679,
7.54780169004651));
#403882=CARTESIAN_POINT('Ctrl Pts',(-0.312187668397832,-2.70580437892645,
7.53807742314383));
#403883=CARTESIAN_POINT('Ctrl Pts',(-0.308200765466668,-2.71607757316128,
7.52834476460825));
#403884=CARTESIAN_POINT('Ctrl Pts',(-0.30421644909628,-2.72634410251322,
7.51860402984325));
#403885=CARTESIAN_POINT('',(-0.304216449096279,-2.72634410251322,7.5));
#403886=CARTESIAN_POINT('Origin',(-0.341564846497285,-2.64910949982511,
7.5));
#403887=CARTESIAN_POINT('Ctrl Pts',(-0.335155581859861,-2.64662214142563,
8.85049129520029));
#403888=CARTESIAN_POINT('Ctrl Pts',(-0.335225648125082,-2.64644159919414,
8.85097269580138));
#403889=CARTESIAN_POINT('Ctrl Pts',(-0.335302671970118,-2.64626637806575,
8.85143669361005));
#403890=CARTESIAN_POINT('Ctrl Pts',(-0.335391000464455,-2.64608876150126,
8.8519052845931));
#403891=CARTESIAN_POINT('Ctrl Pts',(-0.335563765397788,-2.64574135476517,
8.85282181883899));
#403892=CARTESIAN_POINT('Ctrl Pts',(-0.335775510349653,-2.64539380835665,
8.85372622499635));
#403893=CARTESIAN_POINT('Ctrl Pts',(-0.336042725344232,-2.64504869099114,
8.8546225773507));
#403894=CARTESIAN_POINT('Ctrl Pts',(-0.336264557742153,-2.64476218681169,
8.85536669723986));
#403895=CARTESIAN_POINT('Ctrl Pts',(-0.336524644191998,-2.64447727198575,
8.8561049844905));
#403896=CARTESIAN_POINT('Ctrl Pts',(-0.336838351599596,-2.64420078725064,
8.8568133821837));
#403897=CARTESIAN_POINT('Ctrl Pts',(-0.337123041564678,-2.64394987691929,
8.85745625420284));
#403898=CARTESIAN_POINT('Ctrl Pts',(-0.337455066979912,-2.64370231285873,
8.85808743050666));
#403899=CARTESIAN_POINT('Ctrl Pts',(-0.337859744633607,-2.64347139568469,
8.85866804508411));
#403900=CARTESIAN_POINT('Ctrl Pts',(-0.338046454130684,-2.64336485550626,
8.85893592806396));
#403901=CARTESIAN_POINT('Ctrl Pts',(-0.338248828681736,-2.64326199646832,
8.85919241173848));
#403902=CARTESIAN_POINT('Ctrl Pts',(-0.338470529716108,-2.64316520518179,
8.85943017985534));
#403903=CARTESIAN_POINT('Ctrl Pts',(-0.338769891743043,-2.6430345082917,
8.8597512372));
#403904=CARTESIAN_POINT('Ctrl Pts',(-0.339112367572514,-2.64291213519593,
8.86004599534706));
#403905=CARTESIAN_POINT('Ctrl Pts',(-0.339497346992517,-2.64280936394371,
8.86026130871721));
#403906=CARTESIAN_POINT('Ctrl Pts',(-0.339638298811899,-2.64277173649084,
8.86034014101236));
#403907=CARTESIAN_POINT('Ctrl Pts',(-0.339787062302549,-2.64273615954889,
8.86040910639693));
#403908=CARTESIAN_POINT('Ctrl Pts',(-0.339939662725721,-2.64270392954496,
8.86046313645507));
#403909=CARTESIAN_POINT('Ctrl Pts',(-0.340177794408063,-2.64265363489376,
8.8605474499083));
#403910=CARTESIAN_POINT('Ctrl Pts',(-0.340431800199123,-2.64261026145963,
8.86059655985668));
#403911=CARTESIAN_POINT('Ctrl Pts',(-0.340685340623247,-2.64257630213539,
8.86059725258816));
#403912=CARTESIAN_POINT('Ctrl Pts',(-0.340939466827042,-2.64254226435154,
8.86059794692011));
#403913=CARTESIAN_POINT('Ctrl Pts',(-0.341196296497944,-2.64251994000076,
8.86056369958366));
#403914=CARTESIAN_POINT('Ctrl Pts',(-0.341441496150768,-2.64250679770149,
8.86048590497774));
#403915=CARTESIAN_POINT('Ctrl Pts',(-0.341505485959682,-2.64250336795267,
8.86046560290182));
#403916=CARTESIAN_POINT('Ctrl Pts',(-0.341569521019712,-2.64250060938172,
8.86044257503091));
#403917=CARTESIAN_POINT('Ctrl Pts',(-0.341631621181681,-2.64249857443501,
8.86041778462583));
#403918=CARTESIAN_POINT('Ctrl Pts',(-0.342049478211856,-2.64248488176879,
8.86025097596201));
#403919=CARTESIAN_POINT('Ctrl Pts',(-0.342435812155897,-2.64250244638938,
8.8599848982295));
#403920=CARTESIAN_POINT('Ctrl Pts',(-0.342779731744087,-2.64254229188586,
8.85968173251461));
#403921=CARTESIAN_POINT('Ctrl Pts',(-0.342961645501996,-2.64256336787062,
8.85952137522076));
#403922=CARTESIAN_POINT('Ctrl Pts',(-0.343135221051685,-2.64259089417129,
8.85934740853961));
#403923=CARTESIAN_POINT('Ctrl Pts',(-0.343298254078627,-2.64262294724037,
8.8591675900182));
#403924=CARTESIAN_POINT('Ctrl Pts',(-0.343952916424673,-2.6427516569736,
8.85844552518696));
#403925=CARTESIAN_POINT('Ctrl Pts',(-0.344475170663018,-2.64295766344041,
8.85759444184125));
#403926=CARTESIAN_POINT('Ctrl Pts',(-0.344885901813324,-2.64316387735284,
8.8568349891514));
#403927=CARTESIAN_POINT('Ctrl Pts',(-0.34492888373434,-2.64318545708959,
8.85675551444999));
#403928=CARTESIAN_POINT('Ctrl Pts',(-0.344970632078601,-2.64320705484434,
8.85667699793652));
#403929=CARTESIAN_POINT('Ctrl Pts',(-0.345011162179599,-2.6432285921991,
8.85659965593547));
#403930=CARTESIAN_POINT('Ctrl Pts',(-0.345558239550983,-2.64351930451273,
8.85555568965886));
#403931=CARTESIAN_POINT('Ctrl Pts',(-0.346042030188692,-2.64387770585479,
8.85434650606346));
#403932=CARTESIAN_POINT('Ctrl Pts',(-0.346468625116265,-2.64430057424927,
8.85297329937117));
#403933=CARTESIAN_POINT('Ctrl Pts',(-0.346708558770214,-2.64453841195541,
8.85220095427747));
#403934=CARTESIAN_POINT('Ctrl Pts',(-0.346930275458167,-2.64479696397218,
8.85137579139183));
#403935=CARTESIAN_POINT('Ctrl Pts',(-0.347133565397069,-2.64507775146798,
8.85049129520029));
#403936=CARTESIAN_POINT('Origin',(-0.341564846497285,-2.64910949982511,
7.59394543036555));
#403937=CARTESIAN_POINT('Ctrl Pts',(-0.335359007864429,-2.64609796642226,
7.59443877723642));
#403938=CARTESIAN_POINT('Ctrl Pts',(-0.337454099980237,-2.64069946823527,
7.58783886950016));
#403939=CARTESIAN_POINT('Ctrl Pts',(-0.345864850211447,-2.64185638745667,
7.58559994247159));
#403940=CARTESIAN_POINT('Ctrl Pts',(-0.323921961471631,-2.67556820963984,
7.56670252222133));
#403941=CARTESIAN_POINT('Ctrl Pts',(-0.326014025584513,-2.67017751381542,
7.56004874999029));
#403942=CARTESIAN_POINT('Ctrl Pts',(-0.334477523915351,-2.6713201219112,
7.55786368756704));
#403943=CARTESIAN_POINT('Ctrl Pts',(-0.312506272620259,-2.70498342012268,
7.53888913333559));
#403944=CARTESIAN_POINT('Ctrl Pts',(-0.31461076997261,-2.699560687129,7.53222002137277));
#403945=CARTESIAN_POINT('Ctrl Pts',(-0.323109970911466,-2.70072945918586,
7.53005029815327));
#403946=CARTESIAN_POINT('Ctrl Pts',(-0.301112457877976,-2.73434226681255,
7.51101258149734));
#403947=CARTESIAN_POINT('Ctrl Pts',(-0.303242465562199,-2.72885380044164,
7.5043616886572));
#403948=CARTESIAN_POINT('Ctrl Pts',(-0.311762829927165,-2.73008297603239,
7.50217374673251));
#403949=CARTESIAN_POINT('',(-0.312368326987707,-2.72851663429644,7.50366116523517));
#403950=CARTESIAN_POINT('Ctrl Pts',(-0.304216449096279,-2.72634410251322,
7.51860402984325));
#403951=CARTESIAN_POINT('Ctrl Pts',(-0.304056675224784,-2.72675579751655,
7.51734760759494));
#403952=CARTESIAN_POINT('Ctrl Pts',(-0.303967762981087,-2.72714934862238,
7.51608817408573));
#403953=CARTESIAN_POINT('Ctrl Pts',(-0.30396294223285,-2.72752679337759,
7.5148100591312));
#403954=CARTESIAN_POINT('Ctrl Pts',(-0.303958575483901,-2.72786869185621,
7.51365231206384));
#403955=CARTESIAN_POINT('Ctrl Pts',(-0.304022950927189,-2.72819785354088,
7.51247773061043));
#403956=CARTESIAN_POINT('Ctrl Pts',(-0.304191193131477,-2.72850149544917,
7.51129758471022));
#403957=CARTESIAN_POINT('Ctrl Pts',(-0.304400298977422,-2.72887888766396,
7.50983079813402));
#403958=CARTESIAN_POINT('Ctrl Pts',(-0.30477457371951,-2.72919850100535,
7.50839324291155));
#403959=CARTESIAN_POINT('Ctrl Pts',(-0.305370284589417,-2.72939997663714,
7.50715379678855));
#403960=CARTESIAN_POINT('Ctrl Pts',(-0.305645485846318,-2.72949305257364,
7.50658120839351));
#403961=CARTESIAN_POINT('Ctrl Pts',(-0.306010111959797,-2.72956514658688,
7.50598221009429));
#403962=CARTESIAN_POINT('Ctrl Pts',(-0.306459897374679,-2.72959222844244,
7.50545747549611));
#403963=CARTESIAN_POINT('Ctrl Pts',(-0.306699916794221,-2.72960668015883,
7.50517746087247));
#403964=CARTESIAN_POINT('Ctrl Pts',(-0.306966776843353,-2.72960867296547,
7.50491486231392));
#403965=CARTESIAN_POINT('Ctrl Pts',(-0.307253423074079,-2.72959648611972,
7.50468370960992));
#403966=CARTESIAN_POINT('Ctrl Pts',(-0.30768204960644,-2.72957826294121,
7.50433806340447));
#403967=CARTESIAN_POINT('Ctrl Pts',(-0.30816774665045,-2.72952723189046,
7.50405484070984));
#403968=CARTESIAN_POINT('Ctrl Pts',(-0.308677728555385,-2.72944611734059,
7.50385766036131));
#403969=CARTESIAN_POINT('Ctrl Pts',(-0.308732263193207,-2.72943744340028,
7.50383657498791));
#403970=CARTESIAN_POINT('Ctrl Pts',(-0.308787053675708,-2.7294284435361,
7.50381643264937));
#403971=CARTESIAN_POINT('Ctrl Pts',(-0.308842044242128,-2.72941913446201,
7.50379723213559));
#403972=CARTESIAN_POINT('Ctrl Pts',(-0.30920912426164,-2.72935699334722,
7.50366906242519));
#403973=CARTESIAN_POINT('Ctrl Pts',(-0.309592984844114,-2.72927901316412,
7.50358235568538));
#403974=CARTESIAN_POINT('Ctrl Pts',(-0.30996117243169,-2.72919495596223,
7.5035341175365));
#403975=CARTESIAN_POINT('Ctrl Pts',(-0.310513228048472,-2.72906892170142,
7.50346178989176));
#403976=CARTESIAN_POINT('Ctrl Pts',(-0.311101755435299,-2.72890986475049,
7.50346967198527));
#403977=CARTESIAN_POINT('Ctrl Pts',(-0.31167470241447,-2.72873594267221,
7.50354272648692));
#403978=CARTESIAN_POINT('Ctrl Pts',(-0.311910367366302,-2.72866440492144,
7.50357277531559));
#403979=CARTESIAN_POINT('Ctrl Pts',(-0.312143124417443,-2.72859058295185,
7.50361331098761));
#403980=CARTESIAN_POINT('Ctrl Pts',(-0.312368326987868,-2.72851663429785,
7.50366116523658));
#403981=CARTESIAN_POINT('',(-0.341939261259455,-2.65201338678241,7.57603338622103));
#403982=CARTESIAN_POINT('Origin',(-0.343072133619649,-2.66077740924966,
7.58486873427626));
#403983=CARTESIAN_POINT('Ctrl Pts',(-0.312368326962123,-2.72851663434776,
7.50366116529969));
#403984=CARTESIAN_POINT('Ctrl Pts',(-0.322210000124767,-2.70305746570147,
7.52783573079709));
#403985=CARTESIAN_POINT('Ctrl Pts',(-0.3320665295326,-2.67755759369531,
7.55196141284068));
#403986=CARTESIAN_POINT('Ctrl Pts',(-0.341939260496575,-2.65201338777521,
7.57603338728831));
#403987=CARTESIAN_POINT('Ctrl Pts',(-0.334947412104101,-2.64764449208613,
7.59639677331371));
#403988=CARTESIAN_POINT('Ctrl Pts',(-0.338963550211403,-2.62893435951653,
7.59974925422225));
#403989=CARTESIAN_POINT('Ctrl Pts',(-0.347594250863831,-2.64601386279728,
7.59639677331372));
#403990=CARTESIAN_POINT('Ctrl Pts',(-0.335142370393516,-2.64374871291513,
7.58707626057422));
#403991=CARTESIAN_POINT('Ctrl Pts',(-0.34028125647849,-2.63915422911306,
7.58811717123965));
#403992=CARTESIAN_POINT('Ctrl Pts',(-0.346417486467326,-2.64229494768145,
7.58707626057424));
#403993=CARTESIAN_POINT('Ctrl Pts',(-0.339276623241309,-2.64820220431539,
7.58015376756929));
#403994=CARTESIAN_POINT('Ctrl Pts',(-0.341165064355278,-2.6460088684777,
7.5820876076604));
#403995=CARTESIAN_POINT('Ctrl Pts',(-0.343548093433292,-2.6476514592214,
7.5801537675693));
#403996=CARTESIAN_POINT('Ctrl Pts',(-0.341939261153426,-2.65201338596166,
7.57603338509286));
#403997=CARTESIAN_POINT('Ctrl Pts',(-0.341939261153426,-2.65201338596166,
7.57603338509286));
#403998=CARTESIAN_POINT('Ctrl Pts',(-0.341939261153426,-2.65201338596166,
7.57603338509286));
#403999=CARTESIAN_POINT('Origin',(-0.343066474116721,-2.66077813896297,
7.58486873427621));
#404000=CARTESIAN_POINT('Ctrl Pts',(-0.402329817877854,-2.72131574728531,
7.51098857897448));
#404001=CARTESIAN_POINT('Ctrl Pts',(-0.398877281988035,-2.71654704642434,
7.50433767179956));
#404002=CARTESIAN_POINT('Ctrl Pts',(-0.390947339037911,-2.71989727863872,
7.50214974420965));
#404003=CARTESIAN_POINT('Ctrl Pts',(-0.383856321441283,-2.69579984211488,
7.53887321589172));
#404004=CARTESIAN_POINT('Ctrl Pts',(-0.380445153058564,-2.69108827875315,
7.53220407452066));
#404005=CARTESIAN_POINT('Ctrl Pts',(-0.372520354360768,-2.69437468796705,
7.53003438070912));
#404006=CARTESIAN_POINT('Ctrl Pts',(-0.365347349076916,-2.67023493699403,
7.56669465659231));
#404007=CARTESIAN_POINT('Ctrl Pts',(-0.36195634006512,-2.66555121809578,
7.56004085833295));
#404008=CARTESIAN_POINT('Ctrl Pts',(-0.35405944671022,-2.66880325214652,
7.55785582193789));
#404009=CARTESIAN_POINT('Ctrl Pts',(-0.346803737871566,-2.6446221881212,
7.59443891967696));
#404010=CARTESIAN_POINT('Ctrl Pts',(-0.343407812318927,-2.63993167841372,
7.58783901202978));
#404011=CARTESIAN_POINT('Ctrl Pts',(-0.33556559484523,-2.64318418561333,
7.58560008491213));
#404012=CARTESIAN_POINT('',(-0.38994847349129,-2.71851378208007,7.50366116523517));
#404013=CARTESIAN_POINT('Ctrl Pts',(-0.389948473491343,-2.71851378208044,
7.50366116523554));
#404014=CARTESIAN_POINT('Ctrl Pts',(-0.390704801700024,-2.71855966407601,
7.50350835821027));
#404015=CARTESIAN_POINT('Ctrl Pts',(-0.391401543613698,-2.71857723441672,
7.50345484956));
#404016=CARTESIAN_POINT('Ctrl Pts',(-0.39205939879721,-2.71856761579381,
7.50349758195598));
#404017=CARTESIAN_POINT('Ctrl Pts',(-0.392396927294164,-2.71856268072692,
7.50351950684424));
#404018=CARTESIAN_POINT('Ctrl Pts',(-0.392757489109047,-2.71855023130952,
7.50357029184312));
#404019=CARTESIAN_POINT('Ctrl Pts',(-0.393104844734244,-2.71852866929362,
7.50365515313924));
#404020=CARTESIAN_POINT('Ctrl Pts',(-0.39363921834398,-2.71849549818184,
7.50378570417639));
#404021=CARTESIAN_POINT('Ctrl Pts',(-0.394158044509289,-2.71844013313008,
7.50400001621911));
#404022=CARTESIAN_POINT('Ctrl Pts',(-0.394621592111607,-2.71836453062546,
7.50428903009635));
#404023=CARTESIAN_POINT('Ctrl Pts',(-0.394673042329143,-2.7183561393291,
7.50432110841318));
#404024=CARTESIAN_POINT('Ctrl Pts',(-0.394723838956302,-2.71834751168813,
7.50435406373354));
#404025=CARTESIAN_POINT('Ctrl Pts',(-0.39477394802282,-2.71833865967341,
7.50438785222352));
#404026=CARTESIAN_POINT('Ctrl Pts',(-0.395079887959387,-2.71828461386872,
7.50459414719561));
#404027=CARTESIAN_POINT('Ctrl Pts',(-0.395364978925474,-2.71822083575731,
7.50483629897752));
#404028=CARTESIAN_POINT('Ctrl Pts',(-0.395618586479749,-2.71815105294643,
7.5050991045531));
#404029=CARTESIAN_POINT('Ctrl Pts',(-0.396178070216947,-2.71799710505662,
7.50567888004914));
#404030=CARTESIAN_POINT('Ctrl Pts',(-0.396606512880857,-2.7178083682303,
7.50637912803145));
#404031=CARTESIAN_POINT('Ctrl Pts',(-0.396923327952575,-2.71760889522423,
7.50710440483569));
#404032=CARTESIAN_POINT('Ctrl Pts',(-0.397001017297821,-2.71755998048304,
7.50728225710686));
#404033=CARTESIAN_POINT('Ctrl Pts',(-0.397073618487211,-2.71750956990922,
7.50746498566955));
#404034=CARTESIAN_POINT('Ctrl Pts',(-0.39713967437503,-2.7174591824411,
7.50764697238949));
#404035=CARTESIAN_POINT('Ctrl Pts',(-0.397494772648874,-2.71718831327952,
7.50862528291182));
#404036=CARTESIAN_POINT('Ctrl Pts',(-0.397695467332326,-2.71689681385543,
7.50965856837421));
#404037=CARTESIAN_POINT('Ctrl Pts',(-0.397804459504223,-2.71660622414456,
7.51067959873201));
#404038=CARTESIAN_POINT('Ctrl Pts',(-0.397864438033894,-2.71644631226014,
7.51124147302578));
#404039=CARTESIAN_POINT('Ctrl Pts',(-0.3978962540549,-2.71628648428327,
7.51180065547253));
#404040=CARTESIAN_POINT('Ctrl Pts',(-0.397907780476789,-2.71612946946487,
7.51235175716501));
#404041=CARTESIAN_POINT('Ctrl Pts',(-0.397947608855998,-2.71558692072005,
7.51425603304536));
#404042=CARTESIAN_POINT('Ctrl Pts',(-0.397743884464782,-2.71501282769615,
7.51626900505181));
#404043=CARTESIAN_POINT('Ctrl Pts',(-0.397348564351717,-2.71443790085555,
7.51827788969244));
#404044=CARTESIAN_POINT('Ctrl Pts',(-0.397327168880147,-2.71440678472847,
7.51838661432546));
#404045=CARTESIAN_POINT('Ctrl Pts',(-0.397305202528441,-2.71437566373297,
7.51849533314857));
#404046=CARTESIAN_POINT('Ctrl Pts',(-0.39728267045429,-2.71434454205174,
7.51860402984325));
#404047=CARTESIAN_POINT('Ctrl Pts',(-0.341939262249606,-2.65201338755038,
7.57603338728985));
#404048=CARTESIAN_POINT('Ctrl Pts',(-0.357968509122751,-2.67421790325761,
7.55196141284922));
#404049=CARTESIAN_POINT('Ctrl Pts',(-0.373970838822866,-2.69638364460996,
7.52783573083105));
#404050=CARTESIAN_POINT('Ctrl Pts',(-0.389948473530192,-2.71851378212467,
7.50366116530176));
#404051=CARTESIAN_POINT('Origin',(-1.18155821115197E-16,-9.16393216063564E-16,
7.49482233047033));
#404052=CARTESIAN_POINT('Origin',(-0.311362998732846,-2.71973515861749,
7.49482233047033));
#404053=CARTESIAN_POINT('Origin',(0.,0.,7.50366116523517));
#404054=CARTESIAN_POINT('Origin',(-0.388693460788429,-2.70976449964574,
7.49482233047033));
#404055=CARTESIAN_POINT('Ctrl Pts',(-0.304216831735198,-2.72634311643025,
7.51860402984325));
#404056=CARTESIAN_POINT('Ctrl Pts',(-0.301464528298434,-2.73343685393752,
7.51860402984325));
#404057=CARTESIAN_POINT('Ctrl Pts',(-0.293899145873112,-2.7342500419777,
7.51860402984325));
#404058=CARTESIAN_POINT('Ctrl Pts',(-0.303194881501745,-2.72897706911724,
7.51041458714365));
#404059=CARTESIAN_POINT('Ctrl Pts',(-0.299672201491327,-2.73362949765558,
7.51004642900442));
#404060=CARTESIAN_POINT('Ctrl Pts',(-0.293897059430465,-2.73425026624531,
7.50729136483009));
#404061=CARTESIAN_POINT('Ctrl Pts',(-0.305306847737899,-2.73083807309805,
7.50215815450138));
#404062=CARTESIAN_POINT('Ctrl Pts',(-0.303321572720941,-2.73323739541664,
7.4987716367153));
#404063=CARTESIAN_POINT('Ctrl Pts',(-0.299893758158899,-2.73362983767054,
7.49481588533172));
#404064=CARTESIAN_POINT('Ctrl Pts',(-0.312368264372309,-2.72851608735092,
7.50366171572174));
#404065=CARTESIAN_POINT('Ctrl Pts',(-0.312784747585891,-2.73215404062027,
7.50000045605858));
#404066=CARTESIAN_POINT('Ctrl Pts',(-0.312784747585768,-2.73215404062028,
7.49482233047317));
#404067=CARTESIAN_POINT('Origin',(-0.292563240664598,-2.72182163269599,
7.51860402984325));
#404068=CARTESIAN_POINT('Origin',(-0.292563240664598,-2.72182163269599,
9.));
#404069=CARTESIAN_POINT('Origin',(-0.292563240664598,-2.72182163269599,
8.75721825406948));
#404070=CARTESIAN_POINT('Ctrl Pts',(-0.310258498896846,-2.71077525492425,
8.78942910404912));
#404071=CARTESIAN_POINT('Ctrl Pts',(-0.308261245270244,-2.71597750507709,
8.7967269950169));
#404072=CARTESIAN_POINT('Ctrl Pts',(-0.299482479215875,-2.71436296100999,
8.79893251111267));
#404073=CARTESIAN_POINT('Ctrl Pts',(-0.306280778989409,-2.72102479945455,
8.78111911759584));
#404074=CARTESIAN_POINT('Ctrl Pts',(-0.303906062384054,-2.72718945931296,
8.78644465894814));
#404075=CARTESIAN_POINT('Ctrl Pts',(-0.295804309956148,-2.72746716306224,
8.78817647674132));
#404076=CARTESIAN_POINT('Ctrl Pts',(-0.303801769035854,-2.72741256006903,
8.76780923932029));
#404077=CARTESIAN_POINT('Ctrl Pts',(-0.300993761175047,-2.73468784897214,
8.76988516158373));
#404078=CARTESIAN_POINT('Ctrl Pts',(-0.293496231764021,-2.73564880325158,
8.77093053738833));
#404079=CARTESIAN_POINT('Ctrl Pts',(-0.304285142047544,-2.72616703417122,
8.75371302330492));
#404080=CARTESIAN_POINT('Ctrl Pts',(-0.30154676267909,-2.7332640391594,
8.75300828287559));
#404081=CARTESIAN_POINT('Ctrl Pts',(-0.293945960387538,-2.73405292689471,
8.75267964240738));
#404082=CARTESIAN_POINT('Origin',(-0.297636576658722,-2.70874898784203,
8.78727029226991));
#404083=CARTESIAN_POINT('Ctrl Pts',(-0.33515558185986,-2.64662214142563,
8.85049129520029));
#404084=CARTESIAN_POINT('Ctrl Pts',(-0.333042822978394,-2.6520661621945,
8.85711686593484));
#404085=CARTESIAN_POINT('Ctrl Pts',(-0.324576590381425,-2.65087298671372,
8.85933012996512));
#404086=CARTESIAN_POINT('Ctrl Pts',(-0.326521105202078,-2.66887090377406,
8.82945683644724));
#404087=CARTESIAN_POINT('Ctrl Pts',(-0.324390809144484,-2.67436011320682,
8.8360746990239));
#404088=CARTESIAN_POINT('Ctrl Pts',(-0.315904953537523,-2.67312629915468,
8.8382956714852));
#404089=CARTESIAN_POINT('Ctrl Pts',(-0.317899498928037,-2.69108650254807,
8.80838214965002));
#404090=CARTESIAN_POINT('Ctrl Pts',(-0.315760795727605,-2.69659737496413,
8.81501364461989));
#404091=CARTESIAN_POINT('Ctrl Pts',(-0.307247094031181,-2.69534609720933,
8.81722098428721));
#404092=CARTESIAN_POINT('Ctrl Pts',(-0.309289785090403,-2.71327145765926,
8.78727029226991));
#404093=CARTESIAN_POINT('Ctrl Pts',(-0.307150726644335,-2.71878324544933,
8.79393457792714));
#404094=CARTESIAN_POINT('Ctrl Pts',(-0.298601974927885,-2.71753494289437,
8.79610912703474));
#404095=CARTESIAN_POINT('Origin',(-0.32350237342818,-2.64209967160839,8.85049129520029));
#404096=CARTESIAN_POINT('Ctrl Pts',(-0.347133565397069,-2.64507775146798,
8.85049129520029));
#404097=CARTESIAN_POINT('Ctrl Pts',(-0.350558127032874,-2.64980781381701,
8.85711686593484));
#404098=CARTESIAN_POINT('Ctrl Pts',(-0.358444815903108,-2.64650616259708,
8.85933012996512));
#404099=CARTESIAN_POINT('Ctrl Pts',(-0.34410390515194,-2.64089313358697,
8.86332496987232));
#404100=CARTESIAN_POINT('Ctrl Pts',(-0.348714317083905,-2.64058330106072,
8.86648636486736));
#404101=CARTESIAN_POINT('Ctrl Pts',(-0.349955340466984,-2.63480957065002,
8.87206031107457));
#404102=CARTESIAN_POINT('Ctrl Pts',(-0.337037410453453,-2.64177316692274,
8.86341338519876));
#404103=CARTESIAN_POINT('Ctrl Pts',(-0.332480810620164,-2.64261629715804,
8.86654584966059));
#404104=CARTESIAN_POINT('Ctrl Pts',(-0.329859545232499,-2.63730093070269,
8.87215952290714));
#404105=CARTESIAN_POINT('Ctrl Pts',(-0.335155581859861,-2.64662214142563,
8.85049129520029));
#404106=CARTESIAN_POINT('Ctrl Pts',(-0.333042822978394,-2.65206616219449,
8.85711686593484));
#404107=CARTESIAN_POINT('Ctrl Pts',(-0.324576590381426,-2.65087298671372,
8.85933012996512));
#404108=CARTESIAN_POINT('Origin',(-0.357258508851223,-2.63774729990957,
8.85049129520029));
#404109=CARTESIAN_POINT('Ctrl Pts',(-0.389059322317672,-2.7029863147688,
8.78727029226991));
#404110=CARTESIAN_POINT('Ctrl Pts',(-0.392526512802782,-2.70777525680419,
8.79393457792714));
#404111=CARTESIAN_POINT('Ctrl Pts',(-0.40047903875833,-2.70439935009569,
8.79610912703474));
#404112=CARTESIAN_POINT('Ctrl Pts',(-0.375103874792512,-2.68371081503405,
8.80838214965003));
#404113=CARTESIAN_POINT('Ctrl Pts',(-0.378570489461523,-2.68849896174254,
8.81501364461988));
#404114=CARTESIAN_POINT('Ctrl Pts',(-0.386488357039691,-2.68512906773677,
8.81722098428721));
#404115=CARTESIAN_POINT('Ctrl Pts',(-0.361129150869165,-2.66440869041269,
8.82945683644722));
#404116=CARTESIAN_POINT('Ctrl Pts',(-0.364582138437075,-2.66917801513904,
8.83607469902387));
#404117=CARTESIAN_POINT('Ctrl Pts',(-0.372477500384171,-2.66583207697137,
8.8382956714852));
#404118=CARTESIAN_POINT('Ctrl Pts',(-0.34713356539707,-2.64507775146798,
8.85049129520029));
#404119=CARTESIAN_POINT('Ctrl Pts',(-0.350558127032874,-2.64980781381701,
8.85711686593484));
#404120=CARTESIAN_POINT('Ctrl Pts',(-0.358444815903108,-2.64650616259708,
8.85933012996512));
#404121=CARTESIAN_POINT('Origin',(-0.399184265771826,-2.69565586321039,
8.78727029226991));
#404122=CARTESIAN_POINT('Ctrl Pts',(-0.397174100220863,-2.71419455155609,
8.75374538247848));
#404123=CARTESIAN_POINT('Ctrl Pts',(-0.401619776138025,-2.72035737104291,
8.75304829418601));
#404124=CARTESIAN_POINT('Ctrl Pts',(-0.409164941549541,-2.71919930277121,
8.75272238421917));
#404125=CARTESIAN_POINT('Ctrl Pts',(-0.397948185988983,-2.71526373261547,
8.76769408445021));
#404126=CARTESIAN_POINT('Ctrl Pts',(-0.402506294519359,-2.72158123224724,
8.76974318093972));
#404127=CARTESIAN_POINT('Ctrl Pts',(-0.409995042726961,-2.7206132407373,
8.7707786988043));
#404128=CARTESIAN_POINT('Ctrl Pts',(-0.393980663297242,-2.70978371958609,
8.78108014887987));
#404129=CARTESIAN_POINT('Ctrl Pts',(-0.397840414937065,-2.71513979600257,
8.78639403366322));
#404130=CARTESIAN_POINT('Ctrl Pts',(-0.405740331578698,-2.71337531512024,
8.78812224174741));
#404131=CARTESIAN_POINT('Ctrl Pts',(-0.387478769473611,-2.70080318793564,
8.78944554828686));
#404132=CARTESIAN_POINT('Ctrl Pts',(-0.390727083660446,-2.70532036322122,
8.79673892988687));
#404133=CARTESIAN_POINT('Ctrl Pts',(-0.398801680886392,-2.70153824292231,
8.79894799272499));
#404134=CARTESIAN_POINT('Origin',(-0.407407613908441,-2.70701409049333,
8.75721825406948));
#404135=CARTESIAN_POINT('Origin',(-0.407407613908441,-2.70701409049333,
9.));
#404136=CARTESIAN_POINT('Origin',(-0.407407613908441,-2.70701409049333,
7.51860402984325));
#404137=CARTESIAN_POINT('Ctrl Pts',(-0.389948361794155,-2.71851300338654,
7.50366195182966));
#404138=CARTESIAN_POINT('Ctrl Pts',(-0.390468316773903,-2.72213785352538,
7.50000065167735));
#404139=CARTESIAN_POINT('Ctrl Pts',(-0.390468316774018,-2.72213785352537,
7.49482233047108));
#404140=CARTESIAN_POINT('Ctrl Pts',(-0.397374485980942,-2.7189674031765,
7.50215800491337));
#404141=CARTESIAN_POINT('Ctrl Pts',(-0.399905086144938,-2.72078420255571,
7.49877273257269));
#404142=CARTESIAN_POINT('Ctrl Pts',(-0.403322237117555,-2.72029406422792,
7.49481816995647));
#404143=CARTESIAN_POINT('Ctrl Pts',(-0.398935316024023,-2.7166277822844,
7.51043025814043));
#404144=CARTESIAN_POINT('Ctrl Pts',(-0.403523181591025,-2.72023946423692,
7.51006209594513));
#404145=CARTESIAN_POINT('Ctrl Pts',(-0.409270426317671,-2.71937450862293,
7.50731281821701));
#404146=CARTESIAN_POINT('Ctrl Pts',(-0.397281784184379,-2.71434331776496,
7.51860402984326));
#404147=CARTESIAN_POINT('Ctrl Pts',(-0.401743390778365,-2.72050733301407,
7.51860402984326));
#404148=CARTESIAN_POINT('Ctrl Pts',(-0.409267922647754,-2.71937488542709,
7.51860402984327));
#404149=CARTESIAN_POINT('Origin',(0.,0.,7.5));
#404150=CARTESIAN_POINT('Origin',(-0.17694962885436,-2.66188407944157,7.5));
#404151=CARTESIAN_POINT('',(-0.17694962885436,-2.66188407944157,7.59394543036555));
#404152=CARTESIAN_POINT('',(-0.17694962885436,-2.66188407944157,8.85049129520029));
#404153=CARTESIAN_POINT('',(-0.17694962885436,-2.66188407944157,7.5));
#404154=CARTESIAN_POINT('',(-0.215079030421395,-2.72235985585717,8.78727029226991));
#404155=CARTESIAN_POINT('Ctrl Pts',(-0.17694962885436,-2.66188407944157,
8.85049129520029));
#404156=CARTESIAN_POINT('Ctrl Pts',(-0.189677904302642,-2.68207197404603,
8.82945686509571));
#404157=CARTESIAN_POINT('Ctrl Pts',(-0.202387257630392,-2.70222985690408,
8.80838212259896));
#404158=CARTESIAN_POINT('Ctrl Pts',(-0.215079030421396,-2.72235985585717,
8.78727029226991));
#404159=CARTESIAN_POINT('',(-0.222557758686703,-2.73422161816809,8.75721825406948));
#404160=CARTESIAN_POINT('Origin',(-0.200051500241768,-2.69852556812846,
8.75937679713109));
#404161=CARTESIAN_POINT('',(-0.222557758686703,-2.73422161816809,7.51860402984325));
#404162=CARTESIAN_POINT('',(-0.222557758686703,-2.73422161816809,7.5));
#404163=CARTESIAN_POINT('Ctrl Pts',(-0.222557758686702,-2.73422161816809,
7.51860402984325));
#404164=CARTESIAN_POINT('Ctrl Pts',(-0.216684380796561,-2.72490604872586,
7.52834476460825));
#404165=CARTESIAN_POINT('Ctrl Pts',(-0.210807189994241,-2.71558443175037,
7.53807742314407));
#404166=CARTESIAN_POINT('Ctrl Pts',(-0.204926058256151,-2.70625656418765,
7.54780169004674));
#404167=CARTESIAN_POINT('Ctrl Pts',(-0.195610663431066,-2.69148172609652,
7.5632044032688));
#404168=CARTESIAN_POINT('Ctrl Pts',(-0.186285369461577,-2.67669118730146,
7.57858609112103));
#404169=CARTESIAN_POINT('Ctrl Pts',(-0.176949628854359,-2.66188407944157,
7.59394543036555));
#404170=CARTESIAN_POINT('Origin',(-0.0491816719600905,-2.91212708488465,
7.5));
#404171=CARTESIAN_POINT('',(-0.128913937383357,-2.74023375097047,8.75721825406948));
#404172=CARTESIAN_POINT('',(-0.13481441689609,-2.72751301502058,8.78727029226991));
#404173=CARTESIAN_POINT('Origin',(-0.149792034667995,-2.69522304258297,
8.7565864062109));
#404174=CARTESIAN_POINT('',(-0.16489730596464,-2.66265786424426,8.85049129520029));
#404175=CARTESIAN_POINT('Ctrl Pts',(-0.13481441689609,-2.72751301502058,
8.78727029226991));
#404176=CARTESIAN_POINT('Ctrl Pts',(-0.144827823277088,-2.70592529519938,
8.80838212259897));
#404177=CARTESIAN_POINT('Ctrl Pts',(-0.154855100144247,-2.68430767225054,
8.82945686509571));
#404178=CARTESIAN_POINT('Ctrl Pts',(-0.16489730596464,-2.66265786424426,
8.85049129520029));
#404179=CARTESIAN_POINT('',(-0.16489730596464,-2.66265786424426,7.59394543036555));
#404180=CARTESIAN_POINT('',(-0.16489730596464,-2.66265786424426,7.5));
#404181=CARTESIAN_POINT('',(-0.128913937383357,-2.74023375097047,7.51860402984325));
#404182=CARTESIAN_POINT('Ctrl Pts',(-0.16489730596464,-2.66265786424426,
7.59394543036555));
#404183=CARTESIAN_POINT('Ctrl Pts',(-0.157531702584637,-2.67853723396437,
7.57858609112103));
#404184=CARTESIAN_POINT('Ctrl Pts',(-0.150174341270717,-2.69439883476488,
7.56320440326857));
#404185=CARTESIAN_POINT('Ctrl Pts',(-0.142824790067819,-2.71024359788972,
7.54780169004651));
#404186=CARTESIAN_POINT('Ctrl Pts',(-0.138184763568491,-2.72024694622285,
7.53807742314383));
#404187=CARTESIAN_POINT('Ctrl Pts',(-0.133547846342464,-2.73024359133049,
7.52834476460825));
#404188=CARTESIAN_POINT('Ctrl Pts',(-0.128913937383358,-2.74023375097047,
7.51860402984324));
#404189=CARTESIAN_POINT('',(-0.128913937383357,-2.74023375097047,7.5));
#404190=CARTESIAN_POINT('Origin',(-0.17113403648065,-2.66555075509437,7.5));
#404191=CARTESIAN_POINT('Ctrl Pts',(-0.16489730596464,-2.66265786424426,
8.85049129520029));
#404192=CARTESIAN_POINT('Ctrl Pts',(-0.164978795651692,-2.66248218211717,
8.85097269580138));
#404193=CARTESIAN_POINT('Ctrl Pts',(-0.165066887699218,-2.66231225593408,
8.85143669361005));
#404194=CARTESIAN_POINT('Ctrl Pts',(-0.16516641464555,-2.66214066352794,
8.8519052845931));
#404195=CARTESIAN_POINT('Ctrl Pts',(-0.165361083040803,-2.66180503966352,
8.85282181883899));
#404196=CARTESIAN_POINT('Ctrl Pts',(-0.165594660314802,-2.66147177387202,
8.85372622499635));
#404197=CARTESIAN_POINT('Ctrl Pts',(-0.165883438033044,-2.66114448611064,
8.8546225773507));
#404198=CARTESIAN_POINT('Ctrl Pts',(-0.166123171038314,-2.66087278343529,
8.85536669723986));
#404199=CARTESIAN_POINT('Ctrl Pts',(-0.166400977668228,-2.66060511779347,
8.85610498449051));
#404200=CARTESIAN_POINT('Ctrl Pts',(-0.166731754968112,-2.66034930042851,
8.85681338218371));
#404201=CARTESIAN_POINT('Ctrl Pts',(-0.167031935887252,-2.66011714576804,
8.85745625420284));
#404202=CARTESIAN_POINT('Ctrl Pts',(-0.167379140604479,-2.65989136329579,
8.85808743050666));
#404203=CARTESIAN_POINT('Ctrl Pts',(-0.167797781718671,-2.65968684835214,
8.8586680450841));
#404204=CARTESIAN_POINT('Ctrl Pts',(-0.167990933653731,-2.65959248959048,
8.85893592806396));
#404205=CARTESIAN_POINT('Ctrl Pts',(-0.168199482605751,-2.65950280806947,
8.85919241173848));
#404206=CARTESIAN_POINT('Ctrl Pts',(-0.168426929570591,-2.65942042008507,
8.85943017985534));
#404207=CARTESIAN_POINT('Ctrl Pts',(-0.168734050304635,-2.65930917191667,
8.8597512372));
#404208=CARTESIAN_POINT('Ctrl Pts',(-0.16908366295195,-2.65920899275128,
8.86004599534705));
#404209=CARTESIAN_POINT('Ctrl Pts',(-0.169474435967183,-2.65913109836975,
8.86026130871721));
#404210=CARTESIAN_POINT('Ctrl Pts',(-0.169617508985118,-2.65910257904059,
8.86034014101235));
#404211=CARTESIAN_POINT('Ctrl Pts',(-0.169768246247719,-2.65907660650485,
8.86040910639692));
#404212=CARTESIAN_POINT('Ctrl Pts',(-0.169922598120396,-2.65905421986361,
8.86046313645506));
#404213=CARTESIAN_POINT('Ctrl Pts',(-0.170163462925023,-2.65901928569743,
8.86054744990829));
#404214=CARTESIAN_POINT('Ctrl Pts',(-0.17041972577941,-2.65899227558559,
8.86059655985669));
#404215=CARTESIAN_POINT('Ctrl Pts',(-0.170674921058915,-2.65897463042517,
8.86059725258816));
#404216=CARTESIAN_POINT('Ctrl Pts',(-0.170930705941467,-2.65895694449738,
8.86059794692011));
#404217=CARTESIAN_POINT('Ctrl Pts',(-0.171188438254332,-2.65895112114788,
8.86056369958366));
#404218=CARTESIAN_POINT('Ctrl Pts',(-0.171433976148177,-2.65895371584657,
8.86048590497774));
#404219=CARTESIAN_POINT('Ctrl Pts',(-0.171498054227927,-2.65895439298567,
8.86046560290182));
#404220=CARTESIAN_POINT('Ctrl Pts',(-0.171562134463306,-2.65895574282289,
8.86044257503091));
#404221=CARTESIAN_POINT('Ctrl Pts',(-0.171624237413315,-2.65895769082823,
8.86041778462584));
#404222=CARTESIAN_POINT('Ctrl Pts',(-0.172042113203544,-2.6589707984869,
8.86025097596201));
#404223=CARTESIAN_POINT('Ctrl Pts',(-0.172426528013957,-2.65901307951987,
8.8599848982295));
#404224=CARTESIAN_POINT('Ctrl Pts',(-0.172767188072743,-2.65907487815318,
8.85968173251462));
#404225=CARTESIAN_POINT('Ctrl Pts',(-0.172947377726346,-2.65910756608956,
8.85952137522077));
#404226=CARTESIAN_POINT('Ctrl Pts',(-0.173118833030314,-2.65914615685814,
8.85934740853961));
#404227=CARTESIAN_POINT('Ctrl Pts',(-0.173279477441229,-2.65918858963266,
8.8591675900182));
#404228=CARTESIAN_POINT('Ctrl Pts',(-0.17392454825235,-2.65935897927846,
8.85844552518696));
#404229=CARTESIAN_POINT('Ctrl Pts',(-0.174432530583701,-2.65959802342683,
8.85759444184126));
#404230=CARTESIAN_POINT('Ctrl Pts',(-0.174829205672076,-2.65983012928581,
8.85683498915141));
#404231=CARTESIAN_POINT('Ctrl Pts',(-0.174870716663646,-2.6598544185458,
8.85675551445));
#404232=CARTESIAN_POINT('Ctrl Pts',(-0.17491099545856,-2.65987864675125,
8.85667699793652));
#404233=CARTESIAN_POINT('Ctrl Pts',(-0.174950062383063,-2.6599027366277,
8.85659965593547));
#404234=CARTESIAN_POINT('Ctrl Pts',(-0.175477389723428,-2.66022790300923,
8.85555568965886));
#404235=CARTESIAN_POINT('Ctrl Pts',(-0.175937223508559,-2.66061656454988,
8.85434650606346));
#404236=CARTESIAN_POINT('Ctrl Pts',(-0.176335848680044,-2.66106589614674,
8.85297329937117));
#404237=CARTESIAN_POINT('Ctrl Pts',(-0.176560051050416,-2.6613186177918,
8.85220095427747));
#404238=CARTESIAN_POINT('Ctrl Pts',(-0.176764746713064,-2.66159084402269,
8.85137579139183));
#404239=CARTESIAN_POINT('Ctrl Pts',(-0.17694962885436,-2.66188407944157,
8.85049129520029));
#404240=CARTESIAN_POINT('Origin',(-0.17113403648065,-2.66555075509437,7.59394543036555));
#404241=CARTESIAN_POINT('Ctrl Pts',(-0.165133898016439,-2.66214779976352,
7.59443877723642));
#404242=CARTESIAN_POINT('Ctrl Pts',(-0.167570568507203,-2.65689462638278,
7.58783886950016));
#404243=CARTESIAN_POINT('Ctrl Pts',(-0.175889913880998,-2.65858804720708,
7.58559994247159));
#404244=CARTESIAN_POINT('Ctrl Pts',(-0.151832185296232,-2.69082471912743,
7.56670252222135));
#404245=CARTESIAN_POINT('Ctrl Pts',(-0.154265334106355,-2.68557913807363,
7.56004874999027));
#404246=CARTESIAN_POINT('Ctrl Pts',(-0.162638236120098,-2.6872616567584,
7.55786368756704));
#404247=CARTESIAN_POINT('Ctrl Pts',(-0.138555312195516,-2.71944808720963,
7.53888913333562));
#404248=CARTESIAN_POINT('Ctrl Pts',(-0.14100292132816,-2.71417133141079,
7.53222002137279));
#404249=CARTESIAN_POINT('Ctrl Pts',(-0.149409776264355,-2.7158822477739,
7.53005029815327));
#404250=CARTESIAN_POINT('Ctrl Pts',(-0.125303879501814,-2.74801660878327,
7.51101258149734));
#404251=CARTESIAN_POINT('Ctrl Pts',(-0.127781158104548,-2.74267588911605,
7.5043616886572));
#404252=CARTESIAN_POINT('Ctrl Pts',(-0.136205262916626,-2.74444844085289,
7.50217374673251));
#404253=CARTESIAN_POINT('',(-0.136909871778105,-2.7429241116639,7.50366116523517));
#404254=CARTESIAN_POINT('Ctrl Pts',(-0.128913937383357,-2.74023375097047,
7.51860402984325));
#404255=CARTESIAN_POINT('Ctrl Pts',(-0.128728114394988,-2.74063436335517,
7.51734760759494));
#404256=CARTESIAN_POINT('Ctrl Pts',(-0.128614169925107,-2.74102140924103,
7.51608817408573));
#404257=CARTESIAN_POINT('Ctrl Pts',(-0.128585176113117,-2.74139776962911,
7.5148100591312));
#404258=CARTESIAN_POINT('Ctrl Pts',(-0.128558912825387,-2.74173868586207,
7.51365231206384));
#404259=CARTESIAN_POINT('Ctrl Pts',(-0.128602066540877,-2.74207129579757,
7.51247773061043));
#404260=CARTESIAN_POINT('Ctrl Pts',(-0.128750508669652,-2.74238509315603,
7.51129758471022));
#404261=CARTESIAN_POINT('Ctrl Pts',(-0.128935005282989,-2.74277510743559,
7.50983079813402));
#404262=CARTESIAN_POINT('Ctrl Pts',(-0.129288033340387,-2.74311804396215,
7.50839324291155));
#404263=CARTESIAN_POINT('Ctrl Pts',(-0.129869611670373,-2.74335727296713,
7.50715379678855));
#404264=CARTESIAN_POINT('Ctrl Pts',(-0.130138284101049,-2.7434677898742,
7.50658120839351));
#404265=CARTESIAN_POINT('Ctrl Pts',(-0.130497541971785,-2.74356309743786,
7.50598221009429));
#404266=CARTESIAN_POINT('Ctrl Pts',(-0.13094466811385,-2.74361894150132,
7.50545747549611));
#404267=CARTESIAN_POINT('Ctrl Pts',(-0.131183268463104,-2.74364874162211,
7.50517746087247));
#404268=CARTESIAN_POINT('Ctrl Pts',(-0.131449452540084,-2.74366782811637,
7.50491486231392));
#404269=CARTESIAN_POINT('Ctrl Pts',(-0.131736290639274,-2.74367403179687,
7.50468370960992));
#404270=CARTESIAN_POINT('Ctrl Pts',(-0.132165204075514,-2.74368330825604,
7.50433806340446));
#404271=CARTESIAN_POINT('Ctrl Pts',(-0.132653172773507,-2.74366350077051,
7.50405484070983));
#404272=CARTESIAN_POINT('Ctrl Pts',(-0.133167303892982,-2.74361522753202,
7.50385766036131));
#404273=CARTESIAN_POINT('Ctrl Pts',(-0.133222282224801,-2.7436100654595,
7.50383657498791));
#404274=CARTESIAN_POINT('Ctrl Pts',(-0.133277536757653,-2.74360459452477,
7.50381643264937));
#404275=CARTESIAN_POINT('Ctrl Pts',(-0.133333010774479,-2.74359882783486,
7.50379723213559));
#404276=CARTESIAN_POINT('Ctrl Pts',(-0.133703317983615,-2.74356033329326,
7.50366906242519));
#404277=CARTESIAN_POINT('Ctrl Pts',(-0.134091386090839,-2.74350710736077,
7.50358235568538));
#404278=CARTESIAN_POINT('Ctrl Pts',(-0.134464202760945,-2.74344681272314,
7.5035341175365));
#404279=CARTESIAN_POINT('Ctrl Pts',(-0.13502319916307,-2.74335640773805,
7.50346178989176));
#404280=CARTESIAN_POINT('Ctrl Pts',(-0.135620708171097,-2.74323538466582,
7.50346967198527));
#404281=CARTESIAN_POINT('Ctrl Pts',(-0.136203621195066,-2.74309852876809,
7.50354272648692));
#404282=CARTESIAN_POINT('Ctrl Pts',(-0.136443385387408,-2.74304223710461,
7.50357277531559));
#404283=CARTESIAN_POINT('Ctrl Pts',(-0.136680394004056,-2.74298347960564,
7.50361331098761));
#404284=CARTESIAN_POINT('Ctrl Pts',(-0.136909871778176,-2.74292411166531,
7.50366116523658));
#404285=CARTESIAN_POINT('',(-0.171321629291381,-2.66847266454066,7.57603338622103));
#404286=CARTESIAN_POINT('Origin',(-0.171890661196624,-2.67729126376579,
7.58486873427628));
#404287=CARTESIAN_POINT('Ctrl Pts',(-0.136909871749285,-2.74292411171347,
7.50366116529968));
#404288=CARTESIAN_POINT('Ctrl Pts',(-0.148362498674589,-2.71814780982416,
7.52783573079709));
#404289=CARTESIAN_POINT('Ctrl Pts',(-0.159832559194555,-2.6933318400473,
7.55196141284068));
#404290=CARTESIAN_POINT('Ctrl Pts',(-0.171321628466457,-2.66847266548254,
7.57603338728831));
#404291=CARTESIAN_POINT('Ctrl Pts',(-0.164624061684239,-2.6636647768937,
7.5963967733137));
#404292=CARTESIAN_POINT('Ctrl Pts',(-0.169830710514483,-2.64525040115009,
7.59974925422226));
#404293=CARTESIAN_POINT('Ctrl Pts',(-0.177349390934601,-2.66284778364888,
7.59639677331373));
#404294=CARTESIAN_POINT('Ctrl Pts',(-0.165068222839374,-2.6597894930393,
7.5870762605742));
#404295=CARTESIAN_POINT('Ctrl Pts',(-0.170490920119603,-2.65553369865884,
7.58811717123965));
#404296=CARTESIAN_POINT('Ctrl Pts',(-0.176413316036275,-2.65906111388928,
7.58707626057426));
#404297=CARTESIAN_POINT('Ctrl Pts',(-0.168908645247684,-2.66449871675321,
7.58015376756929));
#404298=CARTESIAN_POINT('Ctrl Pts',(-0.170933733866522,-2.66243088019682,
7.58208760766041));
#404299=CARTESIAN_POINT('Ctrl Pts',(-0.173206625605373,-2.66422277725892,
7.5801537675693));
#404300=CARTESIAN_POINT('Ctrl Pts',(-0.171321629238156,-2.6684726637148,
7.57603338509286));
#404301=CARTESIAN_POINT('Ctrl Pts',(-0.171321629238156,-2.6684726637148,
7.57603338509286));
#404302=CARTESIAN_POINT('Ctrl Pts',(-0.171321629238156,-2.6684726637148,
7.57603338509286));
#404303=CARTESIAN_POINT('Origin',(-0.171884966568706,-2.6772916293733,7.58486873427622));
#404304=CARTESIAN_POINT('Ctrl Pts',(-0.227147889551738,-2.74150187215855,
7.51098857897448));
#404305=CARTESIAN_POINT('Ctrl Pts',(-0.224007978980372,-2.73652176437099,
7.50433767179956));
#404306=CARTESIAN_POINT('Ctrl Pts',(-0.215879678833561,-2.73935703998472,
7.50214974420965));
#404307=CARTESIAN_POINT('Ctrl Pts',(-0.210347158552128,-2.71485479117133,
7.53887321589167));
#404308=CARTESIAN_POINT('Ctrl Pts',(-0.207244869681734,-2.70993435391318,
7.53220407452062));
#404309=CARTESIAN_POINT('Ctrl Pts',(-0.199125792371522,-2.71270626725104,
7.53003438070911));
#404310=CARTESIAN_POINT('Ctrl Pts',(-0.193514163951469,-2.68815653795892,
7.56669465659233));
#404311=CARTESIAN_POINT('Ctrl Pts',(-0.190430209031565,-2.68326517957015,
7.56004085833302));
#404312=CARTESIAN_POINT('Ctrl Pts',(-0.182341182153933,-2.6860045762737,
7.55785582193789));
#404313=CARTESIAN_POINT('Ctrl Pts',(-0.176649667038724,-2.66140831997643,
7.59443891967696));
#404314=CARTESIAN_POINT('Ctrl Pts',(-0.173561240768126,-2.656509869727,
7.58783901202978));
#404315=CARTESIAN_POINT('Ctrl Pts',(-0.165526747119535,-2.65925324170307,
7.58560008491213));
#404316=CARTESIAN_POINT('',(-0.214971506492189,-2.73791238843283,7.50366116523517));
#404317=CARTESIAN_POINT('Ctrl Pts',(-0.214971506492218,-2.7379123884332,
7.50366116523554));
#404318=CARTESIAN_POINT('Ctrl Pts',(-0.21572334107393,-2.73800663427399,
7.50350835821027));
#404319=CARTESIAN_POINT('Ctrl Pts',(-0.216417525721022,-2.73806880892224,
7.50345484955999));
#404320=CARTESIAN_POINT('Ctrl Pts',(-0.217074645537791,-2.73810135898814,
7.50349758195598));
#404321=CARTESIAN_POINT('Ctrl Pts',(-0.217411796737069,-2.73811805958593,
7.50351950684424));
#404322=CARTESIAN_POINT('Ctrl Pts',(-0.217772415375944,-2.73812873702199,
7.50357029184312));
#404323=CARTESIAN_POINT('Ctrl Pts',(-0.218120438804858,-2.73812947445888,
7.50365515313923));
#404324=CARTESIAN_POINT('Ctrl Pts',(-0.218655839767129,-2.73813060893543,
7.50378570417639));
#404325=CARTESIAN_POINT('Ctrl Pts',(-0.219177147199483,-2.73810859894365,
7.50400001621911));
#404326=CARTESIAN_POINT('Ctrl Pts',(-0.219644586262637,-2.73806285136934,
7.50428903009634));
#404327=CARTESIAN_POINT('Ctrl Pts',(-0.219696468402389,-2.73805777374055,
7.50432110841318));
#404328=CARTESIAN_POINT('Ctrl Pts',(-0.219747713437285,-2.73805241837707,
7.50435406373354));
#404329=CARTESIAN_POINT('Ctrl Pts',(-0.219798286699883,-2.73804679504868,
7.50438785222352));
#404330=CARTESIAN_POINT('Ctrl Pts',(-0.220107060776633,-2.73801246192593,
7.50459414719561));
#404331=CARTESIAN_POINT('Ctrl Pts',(-0.220395652270383,-2.7379670806944,
7.50483629897752));
#404332=CARTESIAN_POINT('Ctrl Pts',(-0.220653209760782,-2.73791368995159,
7.50509910455309));
#404333=CARTESIAN_POINT('Ctrl Pts',(-0.221221407453803,-2.73779590461034,
7.50567888004914));
#404334=CARTESIAN_POINT('Ctrl Pts',(-0.221661062246291,-2.73763500597979,
7.50637912803144));
#404335=CARTESIAN_POINT('Ctrl Pts',(-0.221990006666845,-2.73745624122375,
7.50710440483569));
#404336=CARTESIAN_POINT('Ctrl Pts',(-0.222070670369226,-2.73741240455658,
7.50728225710685));
#404337=CARTESIAN_POINT('Ctrl Pts',(-0.22214635220824,-2.73736674913086,
7.50746498566954));
#404338=CARTESIAN_POINT('Ctrl Pts',(-0.22221550071332,-2.73732069740447,
7.50764697238949));
#404339=CARTESIAN_POINT('Ctrl Pts',(-0.222587224046446,-2.73707313599715,
7.50862528291181));
#404340=CARTESIAN_POINT('Ctrl Pts',(-0.222806182813372,-2.7367950940424,
7.50965856837421));
#404341=CARTESIAN_POINT('Ctrl Pts',(-0.222933569195861,-2.7365120845317,
7.51067959873201));
#404342=CARTESIAN_POINT('Ctrl Pts',(-0.223003670082823,-2.73635634404098,
7.51124147302578));
#404343=CARTESIAN_POINT('Ctrl Pts',(-0.223045660948038,-2.73619888290729,
7.51180065547252));
#404344=CARTESIAN_POINT('Ctrl Pts',(-0.223067223661612,-2.73604292919307,
7.512351757165));
#404345=CARTESIAN_POINT('Ctrl Pts',(-0.223141731426575,-2.73550404698584,
7.51425603304536));
#404346=CARTESIAN_POINT('Ctrl Pts',(-0.2229752078753,-2.73491808083107,
7.51626900505181));
#404347=CARTESIAN_POINT('Ctrl Pts',(-0.222617535678955,-2.73431900699272,
7.51827788969245));
#404348=CARTESIAN_POINT('Ctrl Pts',(-0.222598177783783,-2.7342865839845,
7.51838661432546));
#404349=CARTESIAN_POINT('Ctrl Pts',(-0.222578250493331,-2.73425411954143,
7.51849533314857));
#404350=CARTESIAN_POINT('Ctrl Pts',(-0.222557758686706,-2.73422161816809,
7.51860402984325));
#404351=CARTESIAN_POINT('Ctrl Pts',(-0.171321630230296,-2.66847266537049,
7.57603338728985));
#404352=CARTESIAN_POINT('Ctrl Pts',(-0.185895295090683,-2.69165855689206,
7.55196141284922));
#404353=CARTESIAN_POINT('Ctrl Pts',(-0.200444582363687,-2.71480402913563,
7.52783573083105));
#404354=CARTESIAN_POINT('Ctrl Pts',(-0.214971506528153,-2.73791238847983,
7.50366116530176));
#404355=CARTESIAN_POINT('Origin',(-5.91995423665181E-17,-9.22080657369149E-16,
7.49482233047033));
#404356=CARTESIAN_POINT('Origin',(-0.13646924015647,-2.7340962668661,7.49482233047033));
#404357=CARTESIAN_POINT('Origin',(0.,0.,7.50366116523517));
#404358=CARTESIAN_POINT('Origin',(-0.214279640797767,-2.72910067339767,
7.49482233047033));
#404359=CARTESIAN_POINT('Ctrl Pts',(-0.128914382414656,-2.74023279142927,
7.51860402984325));
#404360=CARTESIAN_POINT('Ctrl Pts',(-0.12571323655791,-2.74713561340538,
7.51860402984325));
#404361=CARTESIAN_POINT('Ctrl Pts',(-0.118111296885546,-2.7474624149473,
7.51860402984325));
#404362=CARTESIAN_POINT('Ctrl Pts',(-0.12772577395949,-2.7427958558017,
7.51041458714365));
#404363=CARTESIAN_POINT('Ctrl Pts',(-0.123912249553073,-2.74721302654344,
7.51004642900443));
#404364=CARTESIAN_POINT('Ctrl Pts',(-0.11810920036085,-2.74746250507528,
7.50729136483009));
#404365=CARTESIAN_POINT('Ctrl Pts',(-0.129714166000064,-2.74478835029159,
7.50215815450138));
#404366=CARTESIAN_POINT('Ctrl Pts',(-0.127579244834786,-2.74705554593811,
7.49877163671529));
#404367=CARTESIAN_POINT('Ctrl Pts',(-0.12413332922386,-2.74722756104425,
7.49481588533172));
#404368=CARTESIAN_POINT('Ctrl Pts',(-0.136909844334277,-2.74292356183035,
7.50366171572174));
#404369=CARTESIAN_POINT('Ctrl Pts',(-0.137092387372183,-2.74658072470565,
7.50000045605858));
#404370=CARTESIAN_POINT('Ctrl Pts',(-0.137092387372058,-2.74658072470566,
7.49482233047317));
#404371=CARTESIAN_POINT('Origin',(-0.117574427354248,-2.73497394942481,
7.51860402984325));
#404372=CARTESIAN_POINT('Origin',(-0.117574427354248,-2.73497394942481,
9.));
#404373=CARTESIAN_POINT('Origin',(-0.117574427354248,-2.73497394942481,
8.75721825406948));
#404374=CARTESIAN_POINT('Ctrl Pts',(-0.135941072634473,-2.72508400670848,
8.78942910404912));
#404375=CARTESIAN_POINT('Ctrl Pts',(-0.133614613267969,-2.73014760380123,
8.79672699501691));
#404376=CARTESIAN_POINT('Ctrl Pts',(-0.124957328323518,-2.72797391951581,
8.79893251111267));
#404377=CARTESIAN_POINT('Ctrl Pts',(-0.131314834806437,-2.73505763906079,
8.78111911759582));
#404378=CARTESIAN_POINT('Ctrl Pts',(-0.128550026197797,-2.74105748434906,
8.78644465894813));
#404379=CARTESIAN_POINT('Ctrl Pts',(-0.120447127148859,-2.74081553646593,
8.78817647674131));
#404380=CARTESIAN_POINT('Ctrl Pts',(-0.128431653016956,-2.74127344462293,
8.76780923932029));
#404381=CARTESIAN_POINT('Ctrl Pts',(-0.125163285149012,-2.74835387598339,
8.76988516158374));
#404382=CARTESIAN_POINT('Ctrl Pts',(-0.117619591664189,-2.74883248752051,
8.77093053738833));
#404383=CARTESIAN_POINT('Ctrl Pts',(-0.12899383400521,-2.74006144760687,
8.75371302330492));
#404384=CARTESIAN_POINT('Ctrl Pts',(-0.125806374260063,-2.74696842246862,
8.75300828287559));
#404385=CARTESIAN_POINT('Ctrl Pts',(-0.118170644421256,-2.74726870427462,
8.75267964240738));
#404386=CARTESIAN_POINT('Origin',(-0.123474906866981,-2.72225321347492,
8.78727029226991));
#404387=CARTESIAN_POINT('Ctrl Pts',(-0.16489730596464,-2.66265786424426,
8.85049129520029));
#404388=CARTESIAN_POINT('Ctrl Pts',(-0.162440088364647,-2.66795533476229,
8.85711686593484));
#404389=CARTESIAN_POINT('Ctrl Pts',(-0.154067697566079,-2.66622217740361,
8.85933012996512));
#404390=CARTESIAN_POINT('Ctrl Pts',(-0.154855086667233,-2.68430770130539,
8.82945683644723));
#404391=CARTESIAN_POINT('Ctrl Pts',(-0.152377472675502,-2.68964914403162,
8.83607469902388));
#404392=CARTESIAN_POINT('Ctrl Pts',(-0.14398810290671,-2.68787417434732,
8.8382956714852));
#404393=CARTESIAN_POINT('Ctrl Pts',(-0.14482783610749,-2.70592526753855,
8.80838214965003));
#404394=CARTESIAN_POINT('Ctrl Pts',(-0.142340444294174,-2.71128779009164,
8.81501364461989));
#404395=CARTESIAN_POINT('Ctrl Pts',(-0.133924404551986,-2.70949360848066,
8.81722098428721));
#404396=CARTESIAN_POINT('Ctrl Pts',(-0.13481441689609,-2.72751301502058,
8.78727029226991));
#404397=CARTESIAN_POINT('Ctrl Pts',(-0.132326611918816,-2.7328764283063,
8.79393457792714));
#404398=CARTESIAN_POINT('Ctrl Pts',(-0.123875403548917,-2.73108297011979,
8.79610912703474));
#404399=CARTESIAN_POINT('Origin',(-0.153557795935531,-2.6573980626986,8.85049129520029));
#404400=CARTESIAN_POINT('Ctrl Pts',(-0.17694962885436,-2.66188407944157,
8.85049129520029));
#404401=CARTESIAN_POINT('Ctrl Pts',(-0.180064098225775,-2.66682383578755,
8.85711686593484));
#404402=CARTESIAN_POINT('Ctrl Pts',(-0.188146120567841,-2.66403427005499,
8.85933012996512));
#404403=CARTESIAN_POINT('Ctrl Pts',(-0.174194302759305,-2.65751394830842,
8.8633249698723));
#404404=CARTESIAN_POINT('Ctrl Pts',(-0.178815093143622,-2.657500142473,
8.86648636486737));
#404405=CARTESIAN_POINT('Ctrl Pts',(-0.180423490888559,-2.65181778745183,
8.87206031107456));
#404406=CARTESIAN_POINT('Ctrl Pts',(-0.167085943002642,-2.6579394216515,
8.86341338519877));
#404407=CARTESIAN_POINT('Ctrl Pts',(-0.162484685652769,-2.65848887723162,
8.86654584966057));
#404408=CARTESIAN_POINT('Ctrl Pts',(-0.160209362634038,-2.65301648671671,
8.87215952290715));
#404409=CARTESIAN_POINT('Ctrl Pts',(-0.16489730596464,-2.66265786424426,
8.85049129520029));
#404410=CARTESIAN_POINT('Ctrl Pts',(-0.162440088364647,-2.66795533476229,
8.85711686593484));
#404411=CARTESIAN_POINT('Ctrl Pts',(-0.154067697566079,-2.66622217740361,
8.85933012996512));
#404412=CARTESIAN_POINT('Origin',(-0.187523433170195,-2.65521739643648,
8.85049129520029));
#404413=CARTESIAN_POINT('Ctrl Pts',(-0.215079030421396,-2.72235985585717,
8.78727029226991));
#404414=CARTESIAN_POINT('Ctrl Pts',(-0.218232268622115,-2.72736110215464,
8.79393457792714));
#404415=CARTESIAN_POINT('Ctrl Pts',(-0.22638475034563,-2.72450165169591,
8.79610912703474));
#404416=CARTESIAN_POINT('Ctrl Pts',(-0.202387241368133,-2.70222983111105,
8.80838214965003));
#404417=CARTESIAN_POINT('Ctrl Pts',(-0.205539955892626,-2.70723024682309,
8.81501364461993));
#404418=CARTESIAN_POINT('Ctrl Pts',(-0.213657465212903,-2.70437457614343,
8.81722098428721));
#404419=CARTESIAN_POINT('Ctrl Pts',(-0.189677921384463,-2.68207200113894,
8.82945683644722));
#404420=CARTESIAN_POINT('Ctrl Pts',(-0.192818242734711,-2.68705276044921,
8.83607469902389));
#404421=CARTESIAN_POINT('Ctrl Pts',(-0.200911757808346,-2.68421955444713,
8.8382956714852));
#404422=CARTESIAN_POINT('Ctrl Pts',(-0.17694962885436,-2.66188407944157,
8.85049129520029));
#404423=CARTESIAN_POINT('Ctrl Pts',(-0.180064098225775,-2.66682383578755,
8.85711686593484));
#404424=CARTESIAN_POINT('Ctrl Pts',(-0.188146120567841,-2.66403427005499,
8.85933012996512));
#404425=CARTESIAN_POINT('Origin',(-0.225652834737231,-2.71569317285208,
8.78727029226991));
#404426=CARTESIAN_POINT('Ctrl Pts',(-0.222459021446524,-2.73406497972526,
8.75374538247848));
#404427=CARTESIAN_POINT('Ctrl Pts',(-0.226500710045497,-2.74049997247247,
8.75304829418602));
#404428=CARTESIAN_POINT('Ctrl Pts',(-0.234104570794377,-2.73982770398393,
8.75272238421917));
#404429=CARTESIAN_POINT('Ctrl Pts',(-0.223163014106709,-2.73518155988289,
8.76769408445022));
#404430=CARTESIAN_POINT('Ctrl Pts',(-0.22730699392311,-2.74177811855035,
8.76974318093967));
#404431=CARTESIAN_POINT('Ctrl Pts',(-0.234842375123349,-2.74129192162787,
8.77077869880429));
#404432=CARTESIAN_POINT('Ctrl Pts',(-0.219554748756185,-2.72945860607643,
8.78108014887986));
#404433=CARTESIAN_POINT('Ctrl Pts',(-0.223063405128077,-2.73505097299613,
8.78639403366327));
#404434=CARTESIAN_POINT('Ctrl Pts',(-0.231060141221982,-2.73379626682602,
8.78812224174741));
#404435=CARTESIAN_POINT('Ctrl Pts',(-0.213641598409107,-2.72007994812382,
8.78944554828685));
#404436=CARTESIAN_POINT('Ctrl Pts',(-0.216593822171823,-2.72479596259281,
8.79673892988685));
#404437=CARTESIAN_POINT('Ctrl Pts',(-0.224894150551318,-2.72153895428623,
8.79894799272499));
#404438=CARTESIAN_POINT('Origin',(-0.233131563002538,-2.72755493516299,
8.75721825406948));
#404439=CARTESIAN_POINT('Origin',(-0.233131563002538,-2.72755493516299,
9.));
#404440=CARTESIAN_POINT('Origin',(-0.233131563002538,-2.72755493516299,
7.51860402984325));
#404441=CARTESIAN_POINT('Ctrl Pts',(-0.214971444915614,-2.73791160418274,
7.50366195182966));
#404442=CARTESIAN_POINT('Ctrl Pts',(-0.215258086646298,-2.74156232030815,
7.50000065167735));
#404443=CARTESIAN_POINT('Ctrl Pts',(-0.215258086646414,-2.74156232030814,
7.49482233047108));
#404444=CARTESIAN_POINT('Ctrl Pts',(-0.222353197839311,-2.73884086376986,
7.50215800491336));
#404445=CARTESIAN_POINT('Ctrl Pts',(-0.224762195877981,-2.74081606644907,
7.49877273257263));
#404446=CARTESIAN_POINT('Ctrl Pts',(-0.228203729217914,-2.74054587277758,
7.49481816995647));
#404447=CARTESIAN_POINT('Ctrl Pts',(-0.224060721014886,-2.73660605260401,
7.51043025814043));
#404448=CARTESIAN_POINT('Ctrl Pts',(-0.228407759062826,-2.74050425952473,
7.51006209594517));
#404449=CARTESIAN_POINT('Ctrl Pts',(-0.234198613355267,-2.74000930828873,
7.50731281821702));
#404450=CARTESIAN_POINT('Ctrl Pts',(-0.222556952678053,-2.73422033961323,
7.51860402984326));
#404451=CARTESIAN_POINT('Ctrl Pts',(-0.226614462609811,-2.74065754634786,
7.51860402984327));
#404452=CARTESIAN_POINT('Ctrl Pts',(-0.234196090687486,-2.74000952390803,
7.51860402984327));
#404453=CARTESIAN_POINT('Origin',(0.,0.,7.5));
#404454=CARTESIAN_POINT('Origin',(-0.00603856833113048,-2.66775215476039,
7.5));
#404455=CARTESIAN_POINT('',(-0.00603856833113048,-2.66775215476039,7.59394543036555));
#404456=CARTESIAN_POINT('',(-0.00603856833113048,-2.66775215476039,8.85049129520029));
#404457=CARTESIAN_POINT('',(-0.00603856833113048,-2.66775215476039,7.5));
#404458=CARTESIAN_POINT('',(-0.0402149326548299,-2.73054663635347,8.78727029226991));
#404459=CARTESIAN_POINT('Ctrl Pts',(-0.00603856833113057,-2.66775215476039,
8.85049129520029));
#404460=CARTESIAN_POINT('Ctrl Pts',(-0.0174472493241456,-2.68871407457819,
8.82945686509571));
#404461=CARTESIAN_POINT('Ctrl Pts',(-0.0288389699333437,-2.70964483196749,
8.80838212259895));
#404462=CARTESIAN_POINT('Ctrl Pts',(-0.0402149326548299,-2.73054663635347,
8.78727029226991));
#404463=CARTESIAN_POINT('',(-0.0469183093502055,-2.74286319116668,8.75721825406948));
#404464=CARTESIAN_POINT('Origin',(-0.0267453462054665,-2.70579850156065,
8.75937679713102));
#404465=CARTESIAN_POINT('',(-0.0469183093502055,-2.74286319116668,7.51860402984325));
#404466=CARTESIAN_POINT('',(-0.0469183093502055,-2.74286319116668,7.5));
#404467=CARTESIAN_POINT('Ctrl Pts',(-0.0469183093502053,-2.74286319116668,
7.51860402984325));
#404468=CARTESIAN_POINT('Ctrl Pts',(-0.041653849528267,-2.73319045294751,
7.52834476460825));
#404469=CARTESIAN_POINT('Ctrl Pts',(-0.0363859720949718,-2.72351143532627,
7.53807742314407));
#404470=CARTESIAN_POINT('Ctrl Pts',(-0.0311145622994817,-2.71382592746367,
7.54780169004674));
#404471=CARTESIAN_POINT('Ctrl Pts',(-0.0227649340788154,-2.69848460646635,
7.5632044032688));
#404472=CARTESIAN_POINT('Ctrl Pts',(-0.0144064330001542,-2.68312698278351,
7.57858609112103));
#404473=CARTESIAN_POINT('Ctrl Pts',(-0.00603856833113041,-2.66775215476039,
7.59394543036555));
#404474=CARTESIAN_POINT('Origin',(0.1375,-2.90929488800561,7.5));
#404475=CARTESIAN_POINT('',(0.0469183093502055,-2.74286319116668,8.75721825406948));
#404476=CARTESIAN_POINT('',(0.0402149326548299,-2.73054663635347,8.78727029226991));
#404477=CARTESIAN_POINT('Origin',(0.0231992623667671,-2.69928262639098,
8.75658640621021));
#404478=CARTESIAN_POINT('',(0.00603856833113048,-2.66775215476039,8.85049129520029));
#404479=CARTESIAN_POINT('Ctrl Pts',(0.04021493265483,-2.73054663635347,
8.78727029226991));
#404480=CARTESIAN_POINT('Ctrl Pts',(0.0288389699333486,-2.7096448319675,
8.80838212259896));
#404481=CARTESIAN_POINT('Ctrl Pts',(0.017447249324145,-2.68871407457819,
8.82945686509571));
#404482=CARTESIAN_POINT('Ctrl Pts',(0.00603856833113064,-2.66775215476039,
8.85049129520029));
#404483=CARTESIAN_POINT('',(0.00603856833113048,-2.66775215476039,7.59394543036555));
#404484=CARTESIAN_POINT('',(0.00603856833113048,-2.66775215476039,7.5));
#404485=CARTESIAN_POINT('',(0.0469183093502055,-2.74286319116668,7.51860402984325));
#404486=CARTESIAN_POINT('Ctrl Pts',(0.00603856833112958,-2.66775215476039,
7.59394543036555));
#404487=CARTESIAN_POINT('Ctrl Pts',(0.0144064330001523,-2.68312698278351,
7.57858609112103));
#404488=CARTESIAN_POINT('Ctrl Pts',(0.022764934078714,-2.69848460646616,
7.56320440326857));
#404489=CARTESIAN_POINT('Ctrl Pts',(0.031114562299379,-2.71382592746348,
7.54780169004651));
#404490=CARTESIAN_POINT('Ctrl Pts',(0.0363859720948704,-2.72351143532608,
7.53807742314383));
#404491=CARTESIAN_POINT('Ctrl Pts',(0.0416538495282657,-2.73319045294751,
7.52834476460825));
#404492=CARTESIAN_POINT('Ctrl Pts',(0.0469183093502052,-2.74286319116668,
7.51860402984325));
#404493=CARTESIAN_POINT('',(0.0469183093502055,-2.74286319116668,7.5));
#404494=CARTESIAN_POINT('Origin',(0.,-2.67103869055211,7.5));
#404495=CARTESIAN_POINT('Ctrl Pts',(0.0060385683311304,-2.66775215476039,
8.85049129520029));
#404496=CARTESIAN_POINT('Ctrl Pts',(0.0059459900808512,-2.66758205465325,
8.85097269580139));
#404497=CARTESIAN_POINT('Ctrl Pts',(0.00584719181995321,-2.66741812167859,
8.85143669361005));
#404498=CARTESIAN_POINT('Ctrl Pts',(0.00573687539919907,-2.6672532585408,
8.8519052845931));
#404499=CARTESIAN_POINT('Ctrl Pts',(0.00552110347621796,-2.66693079669851,
8.85282181883899));
#404500=CARTESIAN_POINT('Ctrl Pts',(0.00526665369920735,-2.66661318098465,
8.85372622499635));
#404501=CARTESIAN_POINT('Ctrl Pts',(0.00495749990689061,-2.66630506772301,
8.8546225773507));
#404502=CARTESIAN_POINT('Ctrl Pts',(0.00470085140861172,-2.66604928303633,
8.85536669723986));
#404503=CARTESIAN_POINT('Ctrl Pts',(0.00440646616566121,-2.66579996647417,
8.85610498449051));
#404504=CARTESIAN_POINT('Ctrl Pts',(0.00405997820836668,-2.66556586768779,
8.85681338218371));
#404505=CARTESIAN_POINT('Ctrl Pts',(0.00374553984295258,-2.66535342267149,
8.85745625420284));
#404506=CARTESIAN_POINT('Ctrl Pts',(0.00338458256238873,-2.66515034957616,
8.85808743050666));
#404507=CARTESIAN_POINT('Ctrl Pts',(0.00295369827383558,-2.66497307725867,
8.85866804508411));
#404508=CARTESIAN_POINT('Ctrl Pts',(0.00275489760352519,-2.66489128765418,
8.85893592806396));
#404509=CARTESIAN_POINT('Ctrl Pts',(0.00254103122291519,-2.6648151521707,
8.85919241173849));
#404510=CARTESIAN_POINT('Ctrl Pts',(0.00230877295597377,-2.66474750603832,
8.85943017985535));
#404511=CARTESIAN_POINT('Ctrl Pts',(0.00199515553979517,-2.66465616373421,
8.85975123720001));
#404512=CARTESIAN_POINT('Ctrl Pts',(0.00163984270799643,-2.66457859015688,
8.86004599534706));
#404513=CARTESIAN_POINT('Ctrl Pts',(0.00124488186767327,-2.66452589273075,
8.86026130871721));
#404514=CARTESIAN_POINT('Ctrl Pts',(0.00110027556890578,-2.66450659871735,
8.86034014101236));
#404515=CARTESIAN_POINT('Ctrl Pts',(0.000948183946098822,-2.66449033731455,
8.86040910639693));
#404516=CARTESIAN_POINT('Ctrl Pts',(0.000792714888868764,-2.6644778860275,
8.86046313645507));
#404517=CARTESIAN_POINT('Ctrl Pts',(0.000550106727103745,-2.66445845589833,
8.8605474499083));
#404518=CARTESIAN_POINT('Ctrl Pts',(0.000292639848427733,-2.66444792009911,
8.86059655985668));
#404519=CARTESIAN_POINT('Ctrl Pts',(3.68383656842663E-5,-2.66444666161026,
8.86059725258816));
#404520=CARTESIAN_POINT('Ctrl Pts',(-0.000219554120677806,-2.6644454002138,
8.86059794692011));
#404521=CARTESIAN_POINT('Ctrl Pts',(-0.000477129998147651,-2.66445610179498,
8.86056369958366));
#404522=CARTESIAN_POINT('Ctrl Pts',(-0.000721997165140026,-2.66447442282945,
8.86048590497774));
#404523=CARTESIAN_POINT('Ctrl Pts',(-0.000785900205151045,-2.66447920407396,
8.86046560290182));
#404524=CARTESIAN_POINT('Ctrl Pts',(-0.000849762296446932,-2.66448465677257,
8.86044257503091));
#404525=CARTESIAN_POINT('Ctrl Pts',(-0.000911612840154663,-2.66449057972519,
8.86041778462583));
#404526=CARTESIAN_POINT('Ctrl Pts',(-0.00132779024918037,-2.66453043384658,
8.860250975962));
#404527=CARTESIAN_POINT('Ctrl Pts',(-0.0017087062830535,-2.6645972575501,
8.8599848982295));
#404528=CARTESIAN_POINT('Ctrl Pts',(-0.00204470696718254,-2.6646807553764,
8.85968173251462));
#404529=CARTESIAN_POINT('Ctrl Pts',(-0.00222243207854282,-2.66472492094265,
8.85952137522077));
#404530=CARTESIAN_POINT('Ctrl Pts',(-0.00239106259016765,-2.6647744176014,
8.85934740853961));
#404531=CARTESIAN_POINT('Ctrl Pts',(-0.00254865826271333,-2.66482705571598,
8.8591675900182));
#404532=CARTESIAN_POINT('Ctrl Pts',(-0.00318148680458622,-2.66503842510675,
8.85844552518695));
#404533=CARTESIAN_POINT('Ctrl Pts',(-0.00367310982058979,-2.665309524653,
8.85759444184124));
#404534=CARTESIAN_POINT('Ctrl Pts',(-0.0040540988240094,-2.66556656868577,
8.85683498915139));
#404535=CARTESIAN_POINT('Ctrl Pts',(-0.00409396830856038,-2.66559346765924,
8.85675551444998));
#404536=CARTESIAN_POINT('Ctrl Pts',(-0.00413261203991475,-2.66562022675649,
8.85667699793651));
#404537=CARTESIAN_POINT('Ctrl Pts',(-0.00417005525354386,-2.66564677016415,
8.85659965593547));
#404538=CARTESIAN_POINT('Ctrl Pts',(-0.00467546566173685,-2.66600505443517,
8.85555568965886));
#404539=CARTESIAN_POINT('Ctrl Pts',(-0.00510945303863149,-2.66642237908077,
8.85434650606346));
#404540=CARTESIAN_POINT('Ctrl Pts',(-0.00547847041769397,-2.6668963274801,
8.85297329937117));
#404541=CARTESIAN_POINT('Ctrl Pts',(-0.00568602020885762,-2.66716289457662,
8.85220095427747));
#404542=CARTESIAN_POINT('Ctrl Pts',(-0.00587285370781608,-2.66744767638566,
8.85137579139183));
#404543=CARTESIAN_POINT('Ctrl Pts',(-0.00603856833113047,-2.66775215476039,
8.85049129520029));
#404544=CARTESIAN_POINT('Origin',(-2.28698895758661E-17,-2.67103869055211,
7.59394543036555));
#404545=CARTESIAN_POINT('Ctrl Pts',(0.00576978243959104,-2.66725829676663,
7.59443877723642));
#404546=CARTESIAN_POINT('Ctrl Pts',(0.00300154637558126,-2.66217203460837,
7.58783886950016));
#404547=CARTESIAN_POINT('Ctrl Pts',(-0.00519220816616302,-2.66439499840616,
7.58559994247159));
#404548=CARTESIAN_POINT('Ctrl Pts',(0.02088150189643,-2.69502405266403,
7.56670252222137));
#404549=CARTESIAN_POINT('Ctrl Pts',(0.0181172667194093,-2.68994514159859,
7.56004874999026));
#404550=CARTESIAN_POINT('Ctrl Pts',(0.00986936707313795,-2.69216065704217,
7.55786368756704));
#404551=CARTESIAN_POINT('Ctrl Pts',(0.0359650017270119,-2.72273795878639,
7.53888913333556));
#404552=CARTESIAN_POINT('Ctrl Pts',(0.0331843385650257,-2.71762886350384,
7.53222002137276));
#404553=CARTESIAN_POINT('Ctrl Pts',(0.0249043752016816,-2.71987489365092,
7.53005029815326));
#404554=CARTESIAN_POINT('Ctrl Pts',(0.0510195993927981,-2.75039876106078,
7.51101258149734));
#404555=CARTESIAN_POINT('Ctrl Pts',(0.0482052295407062,-2.74522773425994,
7.5043616886572));
#404556=CARTESIAN_POINT('Ctrl Pts',(0.0399120007351545,-2.74753637834759,
7.50217374673251));
#404557=CARTESIAN_POINT('',(0.0391111754616882,-2.74606032550115,7.50366116523517));
#404558=CARTESIAN_POINT('Ctrl Pts',(0.0469183093502058,-2.74286319116668,
7.51860402984325));
#404559=CARTESIAN_POINT('Ctrl Pts',(0.0471294178689308,-2.74325107473053,
7.51734760759493));
#404560=CARTESIAN_POINT('Ctrl Pts',(0.0472679263427267,-2.74363002494186,
7.51608817408573));
#404561=CARTESIAN_POINT('Ctrl Pts',(0.0473209740766766,-2.74400375441725,
7.5148100591312));
#404562=CARTESIAN_POINT('Ctrl Pts',(0.0473690259817052,-2.74434228750662,
7.51365231206384));
#404563=CARTESIAN_POINT('Ctrl Pts',(0.0473472713218873,-2.74467697892738,
7.51247773061042));
#404564=CARTESIAN_POINT('Ctrl Pts',(0.0472192392491715,-2.74499964227536,
7.51129758471022));
#404565=CARTESIAN_POINT('Ctrl Pts',(0.0470601100046003,-2.74540067596735,
7.50983079813402));
#404566=CARTESIAN_POINT('Ctrl Pts',(0.046729779299906,-2.74576552647934,
7.50839324291155));
#404567=CARTESIAN_POINT('Ctrl Pts',(0.0461647233399476,-2.7460415258142,
7.50715379678855));
#404568=CARTESIAN_POINT('Ctrl Pts',(0.0459036837681432,-2.74616902955418,
7.50658120839351));
#404569=CARTESIAN_POINT('Ctrl Pts',(0.0455512704078028,-2.74628715902903,
7.50598221009429));
#404570=CARTESIAN_POINT('Ctrl Pts',(0.0451086408757811,-2.74637153582515,
7.50545747549612));
#404571=CARTESIAN_POINT('Ctrl Pts',(0.0448724400568288,-2.74641656189527,
7.50517746087247));
#404572=CARTESIAN_POINT('Ctrl Pts',(0.0446080257594691,-2.74645266364665,
7.50491486231392));
#404573=CARTESIAN_POINT('Ctrl Pts',(0.0443221744710907,-2.74647723236113,
7.50468370960992));
#404574=CARTESIAN_POINT('Ctrl Pts',(0.0438947366282894,-2.74651397033903,
7.50433806340447));
#404575=CARTESIAN_POINT('Ctrl Pts',(0.0434065014443691,-2.74652546781193,
7.50405484070984));
#404576=CARTESIAN_POINT('Ctrl Pts',(0.0428903337854138,-2.74651023424991,
7.50385766036131));
#404577=CARTESIAN_POINT('Ctrl Pts',(0.0428351376773493,-2.74650860525724,
7.50383657498791));
#404578=CARTESIAN_POINT('Ctrl Pts',(0.0427796461468655,-2.7465066857332,
7.50381643264937));
#404579=CARTESIAN_POINT('Ctrl Pts',(0.0427239166342627,-2.74650448512403,
7.50379723213559));
#404580=CARTESIAN_POINT('Ctrl Pts',(0.0423519039072551,-2.74648979533795,
7.50366906242519));
#404581=CARTESIAN_POINT('Ctrl Pts',(0.041961222930374,-2.74646154237284,
7.50358235568538));
#404582=CARTESIAN_POINT('Ctrl Pts',(0.041585309161405,-2.74642525806308,
7.5035341175365));
#404583=CARTESIAN_POINT('Ctrl Pts',(0.0410216690100585,-2.74637085384718,
7.50346178989176));
#404584=CARTESIAN_POINT('Ctrl Pts',(0.0404176336735106,-2.74628836196342,
7.50346967198527));
#404585=CARTESIAN_POINT('Ctrl Pts',(0.0398271499193935,-2.74618913461648,
7.50354272648692));
#404586=CARTESIAN_POINT('Ctrl Pts',(0.0395842717290363,-2.74614832035481,
7.50357277531559));
#404587=CARTESIAN_POINT('Ctrl Pts',(0.0393439854661266,-2.74610486877363,
7.50361331098761));
#404588=CARTESIAN_POINT('Ctrl Pts',(0.0391111754617084,-2.74606032550256,
7.50366116523659));
#404589=CARTESIAN_POINT('',(-1.95335088339909E-13,-2.67396661573471,7.57603338622103));
#404590=CARTESIAN_POINT('Origin',(-2.85317610332501E-6,-2.68280355420138,
7.58486873427628));
#404591=CARTESIAN_POINT('Ctrl Pts',(0.039111175493625,-2.74606032554878,
7.50366116529969));
#404592=CARTESIAN_POINT('Ctrl Pts',(0.0260946561062611,-2.72206870155541,
7.52783573079709));
#404593=CARTESIAN_POINT('Ctrl Pts',(0.0130581974131689,-2.69803860815066,
7.55196141284069));
#404594=CARTESIAN_POINT('Ctrl Pts',(8.83381775932182E-10,-2.67396661662181,
7.57603338728831));
#404595=CARTESIAN_POINT('Ctrl Pts',(0.00637576431677354,-2.66873949177856,
7.59639677331371));
#404596=CARTESIAN_POINT('Ctrl Pts',(0.000286090908296224,-2.6515061579884,
7.59959882295465));
#404597=CARTESIAN_POINT('Ctrl Pts',(-0.00631291894862653,-2.66856962426893,
7.59642833564546));
#404598=CARTESIAN_POINT('Ctrl Pts',(0.00568422544926916,-2.66490062761342,
7.58707626057423));
#404599=CARTESIAN_POINT('Ctrl Pts',(9.68314384630046E-5,-2.66106744105337,
7.58809943920598));
#404600=CARTESIAN_POINT('Ctrl Pts',(-0.0055389809656482,-2.66480268125159,
7.58710240504252));
#404601=CARTESIAN_POINT('Ctrl Pts',(0.00215341460009478,-2.66984623243071,
7.58015376756929));
#404602=CARTESIAN_POINT('Ctrl Pts',(3.20712293815052E-5,-2.66794119340239,
7.58205880659761));
#404603=CARTESIAN_POINT('Ctrl Pts',(-0.00209070701379044,-2.66979075755872,
7.58020924244128));
#404604=CARTESIAN_POINT('Ctrl Pts',(7.55734230502141E-15,-2.67396661490714,
7.57603338509286));
#404605=CARTESIAN_POINT('Ctrl Pts',(7.55734230502141E-15,-2.67396661490714,
7.57603338509286));
#404606=CARTESIAN_POINT('Ctrl Pts',(7.55734230502141E-15,-2.67396661490714,
7.57603338509286));
#404607=CARTESIAN_POINT('Origin',(2.85317624624927E-6,-2.68280355420188,
7.58486873427622));
#404608=CARTESIAN_POINT('Ctrl Pts',(-0.0510325618244046,-2.75042257778878,
7.51098857897448));
#404609=CARTESIAN_POINT('Ctrl Pts',(-0.0482181791375388,-2.74525152740576,
7.50433767179956));
#404610=CARTESIAN_POINT('Ctrl Pts',(-0.0399249227228591,-2.74756019566318,
7.50214974420965));
#404611=CARTESIAN_POINT('Ctrl Pts',(-0.0359736340692041,-2.72275381955636,
7.53887321589169));
#404612=CARTESIAN_POINT('Ctrl Pts',(-0.0331929726815447,-2.71764472753391,
7.53220407452065));
#404613=CARTESIAN_POINT('Ctrl Pts',(-0.0249129797891101,-2.71989075460921,
7.53003438070911));
#404614=CARTESIAN_POINT('Ctrl Pts',(-0.0208857876177118,-2.69503192710157,
7.56669465659234));
#404615=CARTESIAN_POINT('Ctrl Pts',(-0.0181215594219111,-2.68995302886307,
7.56004085833303));
#404616=CARTESIAN_POINT('Ctrl Pts',(-0.00987363856813336,-2.6921685314508,
7.55785582193789));
#404617=CARTESIAN_POINT('Ctrl Pts',(-0.00576970483280572,-2.66725815417458,
7.59443891967696));
#404618=CARTESIAN_POINT('Ctrl Pts',(-0.00300146885025822,-2.66217189216599,
7.58783901202978));
#404619=CARTESIAN_POINT('Ctrl Pts',(0.00519228551543038,-2.66439485581461,
7.58560008491213));
#404620=CARTESIAN_POINT('',(-0.0391111754616882,-2.74606032550115,7.50366116523517));
#404621=CARTESIAN_POINT('Ctrl Pts',(-0.0391111754616935,-2.74606032550152,
7.50366116523554));
#404622=CARTESIAN_POINT('Ctrl Pts',(-0.0398554269668709,-2.74620254791117,
7.50350835821027));
#404623=CARTESIAN_POINT('Ctrl Pts',(-0.0405442017937647,-2.74630907137797,
7.50345484956));
#404624=CARTESIAN_POINT('Ctrl Pts',(-0.041197885997511,-2.74638365637749,
7.50349758195598));
#404625=CARTESIAN_POINT('Ctrl Pts',(-0.0415332744725173,-2.74642192401361,
7.50351950684424));
#404626=CARTESIAN_POINT('Ctrl Pts',(-0.0418924680760451,-2.74645568442726,
7.50357029184312));
#404627=CARTESIAN_POINT('Ctrl Pts',(-0.0422397292057554,-2.74647871828665,
7.50365515313923));
#404628=CARTESIAN_POINT('Ctrl Pts',(-0.0427739574431678,-2.74651415368973,
7.50378570417639));
#404629=CARTESIAN_POINT('Ctrl Pts',(-0.043295603978508,-2.74652558920171,
7.50400001621911));
#404630=CARTESIAN_POINT('Ctrl Pts',(-0.0437650136951257,-2.7465098845443,
7.50428903009635));
#404631=CARTESIAN_POINT('Ctrl Pts',(-0.0438171145622485,-2.74650814144815,
7.50432110841318));
#404632=CARTESIAN_POINT('Ctrl Pts',(-0.0438685974280384,-2.7465060803685,
7.50435406373354));
#404633=CARTESIAN_POINT('Ctrl Pts',(-0.0439194270703296,-2.7465037088339,
7.50438785222352));
#404634=CARTESIAN_POINT('Ctrl Pts',(-0.0442297664683503,-2.74648922947526,
7.50459414719561));
#404635=CARTESIAN_POINT('Ctrl Pts',(-0.0445206726054126,-2.74646243160482,
7.50483629897752));
#404636=CARTESIAN_POINT('Ctrl Pts',(-0.0447811216729617,-2.74642565232408,
7.5050991045531));
#404637=CARTESIAN_POINT('Ctrl Pts',(-0.0453556984756071,-2.74634451353664,
7.50567888004914));
#404638=CARTESIAN_POINT('Ctrl Pts',(-0.0458047587608244,-2.74621211426885,
7.50637912803145));
#404639=CARTESIAN_POINT('Ctrl Pts',(-0.0461444808270324,-2.74605479234555,
7.50710440483569));
#404640=CARTESIAN_POINT('Ctrl Pts',(-0.0462277874220943,-2.74601621388668,
7.50728225710685));
#404641=CARTESIAN_POINT('Ctrl Pts',(-0.0463062389178226,-2.74597550121701,
7.50746498566954));
#404642=CARTESIAN_POINT('Ctrl Pts',(-0.046378195894123,-2.74593397446876,
7.50764697238949));
#404643=CARTESIAN_POINT('Ctrl Pts',(-0.046765016795621,-2.74571073809862,
7.50862528291182));
#404644=CARTESIAN_POINT('Ctrl Pts',(-0.0470013398974825,-2.74544729614725,
7.50965856837422));
#404645=CARTESIAN_POINT('Ctrl Pts',(-0.0471465970325942,-2.74517302978349,
7.51067959873203));
#404646=CARTESIAN_POINT('Ctrl Pts',(-0.047226532217264,-2.74502210065757,
7.51124147302579));
#404647=CARTESIAN_POINT('Ctrl Pts',(-0.0472785253772167,-2.74486765340863,
7.51180065547253));
#404648=CARTESIAN_POINT('Ctrl Pts',(-0.0473100357766602,-2.74471340164584,
7.512351757165));
#404649=CARTESIAN_POINT('Ctrl Pts',(-0.0474189167589901,-2.7441804003588,
7.51425603304535));
#404650=CARTESIAN_POINT('Ctrl Pts',(-0.0472902783286503,-2.74358496893378,
7.51626900505179));
#404651=CARTESIAN_POINT('Ctrl Pts',(-0.0469717238008019,-2.74296420982058,
7.51827788969243));
#404652=CARTESIAN_POINT('Ctrl Pts',(-0.0469544830277697,-2.7429306131643,
7.51838661432545));
#404653=CARTESIAN_POINT('Ctrl Pts',(-0.046936676684081,-2.74289693867703,
7.51849533314856));
#404654=CARTESIAN_POINT('Ctrl Pts',(-0.0469183093502091,-2.74286319116668,
7.51860402984325));
#404655=CARTESIAN_POINT('Ctrl Pts',(-8.84014432836477E-10,-2.673966616623,
7.57603338728985));
#404656=CARTESIAN_POINT('Ctrl Pts',(-0.0130581974166911,-2.69803860815728,
7.55196141284922));
#404657=CARTESIAN_POINT('Ctrl Pts',(-0.0260946561203838,-2.72206870158194,
7.52783573083105));
#404658=CARTESIAN_POINT('Ctrl Pts',(-0.0391111754945677,-2.74606032555036,
7.50366116530176));
#404659=CARTESIAN_POINT('Origin',(0.,-9.23979071467924E-16,7.49482233047033));
#404660=CARTESIAN_POINT('Origin',(0.0389852998002483,-2.73722238709234,
7.49482233047033));
#404661=CARTESIAN_POINT('Origin',(0.,0.,7.50366116523517));
#404662=CARTESIAN_POINT('Origin',(-0.0389852998002483,-2.73722238709234,
7.49482233047033));
#404663=CARTESIAN_POINT('Ctrl Pts',(0.0469178037552554,-2.74286226211022,
7.51860402984325));
#404664=CARTESIAN_POINT('Ctrl Pts',(0.0505546378370144,-2.74954580337903,
7.51860402984325));
#404665=CARTESIAN_POINT('Ctrl Pts',(0.0581618967556967,-2.74938487552503,
7.51860402984325));
#404666=CARTESIAN_POINT('Ctrl Pts',(0.0482681861850447,-2.74534390598683,
7.51041458714366));
#404667=CARTESIAN_POINT('Ctrl Pts',(0.0523568843976852,-2.74950766782993,
7.51004642900441));
#404668=CARTESIAN_POINT('Ctrl Pts',(0.0581639947473825,-2.74938483114304,
7.50729136483008));
#404669=CARTESIAN_POINT('Ctrl Pts',(0.046411539069441,-2.74745970339853,
7.50215815450138));
#404670=CARTESIAN_POINT('Ctrl Pts',(0.0486873335340281,-2.74958545597972,
7.49877163671531));
#404671=CARTESIAN_POINT('Ctrl Pts',(0.0521371901874483,-2.74953633709117,
7.49481588533172));
#404672=CARTESIAN_POINT('Ctrl Pts',(0.0391111676211739,-2.74605977503896,
7.50366171572174));
#404673=CARTESIAN_POINT('Ctrl Pts',(0.0391633148674429,-2.7497211194535,
7.50000045605858));
#404674=CARTESIAN_POINT('Ctrl Pts',(0.0391633148675675,-2.7497211194535,
7.49482233047317));
#404675=CARTESIAN_POINT('Origin',(0.0578975244977156,-2.73688767154537,
7.51860402984325));
#404676=CARTESIAN_POINT('Origin',(0.0578975244977156,-2.73688767154537,
9.));
#404677=CARTESIAN_POINT('Origin',(0.0578975244977155,-2.73688767154537,
8.75721825406948));
#404678=CARTESIAN_POINT('Ctrl Pts',(0.0389349646546054,-2.72819480378046,
8.78942910404912));
#404679=CARTESIAN_POINT('Ctrl Pts',(0.0415810698404544,-2.73309894040653,
8.79672699501691));
#404680=CARTESIAN_POINT('Ctrl Pts',(0.0500812990341605,-2.73037504803777,
8.79893251111266));
#404681=CARTESIAN_POINT('Ctrl Pts',(0.0441907101996742,-2.7378515401601,
8.78111911759583));
#404682=CARTESIAN_POINT('Ctrl Pts',(0.0473342496199764,-2.74366191622698,
8.78644465894812));
#404683=CARTESIAN_POINT('Ctrl Pts',(0.0554049987396859,-2.74290131092718,
8.78817647674132));
#404684=CARTESIAN_POINT('Ctrl Pts',(0.0474662162126847,-2.74386984859159,
8.76780923932029));
#404685=CARTESIAN_POINT('Ctrl Pts',(0.0511815136631335,-2.75072632739817,
8.76988516158375));
#404686=CARTESIAN_POINT('Ctrl Pts',(0.0587403725670997,-2.75072062947551,
8.77093053738833));
#404687=CARTESIAN_POINT('Ctrl Pts',(0.0468275373701203,-2.74269636081296,
8.75371302330492));
#404688=CARTESIAN_POINT('Ctrl Pts',(0.0504509795361609,-2.74938492330704,
8.75300828287559));
#404689=CARTESIAN_POINT('Ctrl Pts',(0.058090260070451,-2.74919536526138,
8.75267964240738));
#404690=CARTESIAN_POINT('Origin',(0.0511941478023398,-2.72457111673216,
8.78727029226991));
#404691=CARTESIAN_POINT('Ctrl Pts',(0.00603856833113048,-2.66775215476039,
8.85049129520029));
#404692=CARTESIAN_POINT('Ctrl Pts',(0.00883014741545966,-2.67288130658491,
8.85711686593484));
#404693=CARTESIAN_POINT('Ctrl Pts',(0.0170742924659647,-2.67061528926368,
8.85933012996512));
#404694=CARTESIAN_POINT('Ctrl Pts',(0.0174472646350165,-2.68871410270986,
8.82945683644723));
#404695=CARTESIAN_POINT('Ctrl Pts',(0.0202620155135629,-2.69388582959568,
8.8360746990239));
#404696=CARTESIAN_POINT('Ctrl Pts',(0.0285204257242725,-2.69157699801036,
8.8382956714852));
#404697=CARTESIAN_POINT('Ctrl Pts',(0.0288389553570734,-2.70964480518555,
8.80838214965002));
#404698=CARTESIAN_POINT('Ctrl Pts',(0.0316648145567818,-2.71483694212032,
8.81501364461994));
#404699=CARTESIAN_POINT('Ctrl Pts',(0.0399486090321783,-2.71250722933019,
8.81722098428721));
#404700=CARTESIAN_POINT('Ctrl Pts',(0.04021493265483,-2.73054663635347,
8.78727029226991));
#404701=CARTESIAN_POINT('Ctrl Pts',(0.0430412612390256,-2.73573963571921,
8.79393457792714));
#404702=CARTESIAN_POINT('Ctrl Pts',(0.0513601984344042,-2.73340839160553,
8.79610912703474));
#404703=CARTESIAN_POINT('Origin',(0.0170177834786405,-2.66177663513908,
8.85049129520029));
#404704=CARTESIAN_POINT('Ctrl Pts',(-0.00603856833113047,-2.66775215476039,
8.85049129520029));
#404705=CARTESIAN_POINT('Ctrl Pts',(-0.00883014741545964,-2.67288130658491,
8.85711686593484));
#404706=CARTESIAN_POINT('Ctrl Pts',(-0.0170742924659647,-2.67061528926368,
8.85933012996512));
#404707=CARTESIAN_POINT('Ctrl Pts',(-0.0035688986120927,-2.66321446818132,
8.86332496987232));
#404708=CARTESIAN_POINT('Ctrl Pts',(-0.00818107962988514,-2.66349674576787,
8.86648636486738));
#404709=CARTESIAN_POINT('Ctrl Pts',(-0.0101502424853851,-2.65792911615186,
8.87206031107457));
#404710=CARTESIAN_POINT('Ctrl Pts',(0.00355211642776816,-2.66318363317047,
8.86341338519876));
#404711=CARTESIAN_POINT('Ctrl Pts',(0.0081791237408215,-2.6634371562646,
8.86654584966058));
#404712=CARTESIAN_POINT('Ctrl Pts',(0.0100991546002723,-2.65783022891655,
8.87215952290714));
#404713=CARTESIAN_POINT('Ctrl Pts',(0.0060385683311304,-2.66775215476039,
8.85049129520029));
#404714=CARTESIAN_POINT('Ctrl Pts',(0.00883014741545944,-2.67288130658491,
8.85711686593484));
#404715=CARTESIAN_POINT('Ctrl Pts',(0.0170742924659645,-2.67061528926368,
8.85933012996512));
#404716=CARTESIAN_POINT('Origin',(-0.0170177834786405,-2.66177663513908,
8.85049129520029));
#404717=CARTESIAN_POINT('Ctrl Pts',(-0.0402149326548301,-2.73054663635347,
8.78727029226991));
#404718=CARTESIAN_POINT('Ctrl Pts',(-0.0430412612390258,-2.73573963571921,
8.79393457792714));
#404719=CARTESIAN_POINT('Ctrl Pts',(-0.0513601984344043,-2.73340839160553,
8.79610912703474));
#404720=CARTESIAN_POINT('Ctrl Pts',(-0.0288389553570644,-2.70964480518553,
8.80838214965001));
#404721=CARTESIAN_POINT('Ctrl Pts',(-0.0316648145567926,-2.71483694212031,
8.81501364461994));
#404722=CARTESIAN_POINT('Ctrl Pts',(-0.0399486090321813,-2.71250722933019,
8.81722098428722));
#404723=CARTESIAN_POINT('Ctrl Pts',(-0.0174472646350206,-2.68871410270986,
8.82945683644722));
#404724=CARTESIAN_POINT('Ctrl Pts',(-0.0202620155135602,-2.69388582959568,
8.8360746990239));
#404725=CARTESIAN_POINT('Ctrl Pts',(-0.0285204257242735,-2.69157699801037,
8.83829567148519));
#404726=CARTESIAN_POINT('Ctrl Pts',(-0.00603856833113056,-2.66775215476039,
8.85049129520029));
#404727=CARTESIAN_POINT('Ctrl Pts',(-0.00883014741545973,-2.67288130658491,
8.85711686593484));
#404728=CARTESIAN_POINT('Ctrl Pts',(-0.0170742924659648,-2.67061528926368,
8.85933012996512));
#404729=CARTESIAN_POINT('Origin',(-0.05119414780234,-2.72457111673216,8.78727029226991));
#404730=CARTESIAN_POINT('Ctrl Pts',(-0.046829810835768,-2.74270054843765,
8.75374538247848));
#404731=CARTESIAN_POINT('Ctrl Pts',(-0.0504509039511556,-2.74938127167972,
8.75304829418601));
#404732=CARTESIAN_POINT('Ctrl Pts',(-0.0580822141425596,-2.74919756546978,
8.75272238421917));
#404733=CARTESIAN_POINT('Ctrl Pts',(-0.0474608175312104,-2.7438599394262,
8.7676940844502));
#404734=CARTESIAN_POINT('Ctrl Pts',(-0.0511736401317078,-2.75070845045484,
8.76974318093969));
#404735=CARTESIAN_POINT('Ctrl Pts',(-0.0587246898268686,-2.7507060460072,
8.77077869880429));
#404736=CARTESIAN_POINT('Ctrl Pts',(-0.0442266366581528,-2.73791756168736,
8.78108014887991));
#404737=CARTESIAN_POINT('Ctrl Pts',(-0.0473697799404577,-2.74372323887499,
8.78639403366324));
#404738=CARTESIAN_POINT('Ctrl Pts',(-0.0554304751827418,-2.74298346327396,
8.78812224174742));
#404739=CARTESIAN_POINT('Ctrl Pts',(-0.0389265281907873,-2.72817931634984,
8.78944554828685));
#404740=CARTESIAN_POINT('Ctrl Pts',(-0.041570530208704,-2.73307479088723,
8.79673892988686));
#404741=CARTESIAN_POINT('Ctrl Pts',(-0.0500624819120103,-2.73035627831871,
8.79894799272499));
#404742=CARTESIAN_POINT('Origin',(-0.0578975244977156,-2.73688767154537,
8.75721825406948));
#404743=CARTESIAN_POINT('Origin',(-0.0578975244977156,-2.73688767154537,
9.));
#404744=CARTESIAN_POINT('Origin',(-0.0578975244977155,-2.73688767154537,
7.51860402984325));
#404745=CARTESIAN_POINT('Ctrl Pts',(-0.0391111642587046,-2.74605953891717,
7.50366195182966));
#404746=CARTESIAN_POINT('Ctrl Pts',(-0.0391633148679688,-2.74972111945349,
7.50000065167735));
#404747=CARTESIAN_POINT('Ctrl Pts',(-0.0391633148680856,-2.74972111945349,
7.49482233047108));
#404748=CARTESIAN_POINT('Ctrl Pts',(-0.0464182127131561,-2.74745983977445,
7.50215800491338));
#404749=CARTESIAN_POINT('Ctrl Pts',(-0.0486957095368232,-2.74958532922222,
7.49877273257267));
#404750=CARTESIAN_POINT('Ctrl Pts',(-0.0521474832453746,-2.74953619049074,
7.49481816995647));
#404751=CARTESIAN_POINT('Ctrl Pts',(-0.0482654124422661,-2.74533902165334,
7.51043025814041));
#404752=CARTESIAN_POINT('Ctrl Pts',(-0.05235376005938,-2.74950773497384,
7.51006209594513));
#404753=CARTESIAN_POINT('Ctrl Pts',(-0.0581644280551635,-2.74938482197663,
7.50731281821699));
#404754=CARTESIAN_POINT('Ctrl Pts',(-0.0469175869148848,-2.74286186359761,
7.51860402984325));
#404755=CARTESIAN_POINT('Ctrl Pts',(-0.0505543270057747,-2.74954580995451,
7.51860402984325));
#404756=CARTESIAN_POINT('Ctrl Pts',(-0.0581618967557014,-2.74938487552503,
7.51860402984325));
#404757=CARTESIAN_POINT('Origin',(0.,0.,7.5));
#404758=CARTESIAN_POINT('Origin',(0.164897305964678,-2.66265786424426,7.5));
#404759=CARTESIAN_POINT('',(0.164897305964678,-2.66265786424426,7.59394543036555));
#404760=CARTESIAN_POINT('',(0.164897305964678,-2.66265786424426,8.85049129520029));
#404761=CARTESIAN_POINT('',(0.164897305964678,-2.66265786424426,7.5));
#404762=CARTESIAN_POINT('',(0.13481441689613,-2.72751301502058,8.78727029226991));
#404763=CARTESIAN_POINT('Ctrl Pts',(0.164897305964678,-2.66265786424426,
8.85049129520029));
#404764=CARTESIAN_POINT('Ctrl Pts',(0.154855100144285,-2.68430767225054,
8.82945686509571));
#404765=CARTESIAN_POINT('Ctrl Pts',(0.144827823277126,-2.70592529519937,
8.80838212259897));
#404766=CARTESIAN_POINT('Ctrl Pts',(0.13481441689613,-2.72751301502058,
8.78727029226991));
#404767=CARTESIAN_POINT('',(0.128913937383397,-2.74023375097047,8.75721825406948));
#404768=CARTESIAN_POINT('Origin',(0.146670710195346,-2.70195272855781,8.7593767971309));
#404769=CARTESIAN_POINT('',(0.128913937383397,-2.74023375097047,7.51860402984325));
#404770=CARTESIAN_POINT('',(0.128913937383397,-2.74023375097047,7.5));
#404771=CARTESIAN_POINT('Ctrl Pts',(0.128913937383397,-2.74023375097047,
7.51860402984325));
#404772=CARTESIAN_POINT('Ctrl Pts',(0.133547846342501,-2.73024359133049,
7.52834476460825));
#404773=CARTESIAN_POINT('Ctrl Pts',(0.138184763568441,-2.72024694622305,
7.53807742314407));
#404774=CARTESIAN_POINT('Ctrl Pts',(0.142824790067768,-2.71024359788991,
7.54780169004674));
#404775=CARTESIAN_POINT('Ctrl Pts',(0.150174341270667,-2.69439883476507,
7.5632044032688));
#404776=CARTESIAN_POINT('Ctrl Pts',(0.157531702584675,-2.67853723396437,
7.57858609112103));
#404777=CARTESIAN_POINT('Ctrl Pts',(0.164897305964679,-2.66265786424426,
7.59394543036555));
#404778=CARTESIAN_POINT('Origin',(0.323616654966475,-2.89450777438995,7.5));
#404779=CARTESIAN_POINT('',(0.222557758686742,-2.73422161816808,8.75721825406948));
#404780=CARTESIAN_POINT('',(0.215079030421435,-2.72235985585717,8.78727029226991));
#404781=CARTESIAN_POINT('Origin',(0.19609522865786,-2.69225027889583,8.75658640621063));
#404782=CARTESIAN_POINT('',(0.176949628854398,-2.66188407944157,8.85049129520029));
#404783=CARTESIAN_POINT('Ctrl Pts',(0.215079030421435,-2.72235985585717,
8.78727029226991));
#404784=CARTESIAN_POINT('Ctrl Pts',(0.202387257630427,-2.70222985690407,
8.80838212259895));
#404785=CARTESIAN_POINT('Ctrl Pts',(0.18967790430268,-2.68207197404603,
8.82945686509571));
#404786=CARTESIAN_POINT('Ctrl Pts',(0.176949628854398,-2.66188407944157,
8.85049129520029));
#404787=CARTESIAN_POINT('',(0.176949628854398,-2.66188407944157,7.59394543036555));
#404788=CARTESIAN_POINT('',(0.176949628854398,-2.66188407944157,7.5));
#404789=CARTESIAN_POINT('',(0.222557758686742,-2.73422161816808,7.51860402984325));
#404790=CARTESIAN_POINT('Ctrl Pts',(0.176949628854397,-2.66188407944157,
7.59394543036555));
#404791=CARTESIAN_POINT('Ctrl Pts',(0.186285369461614,-2.67669118730145,
7.57858609112103));
#404792=CARTESIAN_POINT('Ctrl Pts',(0.195610663430991,-2.69148172609634,
7.56320440326857));
#404793=CARTESIAN_POINT('Ctrl Pts',(0.204926058256075,-2.70625656418746,
7.54780169004651));
#404794=CARTESIAN_POINT('Ctrl Pts',(0.210807189994167,-2.71558443175019,
7.53807742314383));
#404795=CARTESIAN_POINT('Ctrl Pts',(0.2166843807966,-2.72490604872585,7.52834476460825));
#404796=CARTESIAN_POINT('Ctrl Pts',(0.222557758686742,-2.73422161816808,
7.51860402984325));
#404797=CARTESIAN_POINT('',(0.222557758686742,-2.73422161816808,7.5));
#404798=CARTESIAN_POINT('Origin',(0.171134036480688,-2.66555075509437,7.5));
#404799=CARTESIAN_POINT('Ctrl Pts',(0.176949628854398,-2.66188407944157,
8.85049129520029));
#404800=CARTESIAN_POINT('Ctrl Pts',(0.176846342464779,-2.6617202603322,
8.85097269580138));
#404801=CARTESIAN_POINT('Ctrl Pts',(0.176737243973756,-2.66156299420173,
8.85143669361005));
#404802=CARTESIAN_POINT('Ctrl Pts',(0.176616591392414,-2.66140553779028,
8.8519052845931));
#404803=CARTESIAN_POINT('Ctrl Pts',(0.176380602594819,-2.661097563035,8.85282181883899));
#404804=CARTESIAN_POINT('Ctrl Pts',(0.176106325903508,-2.66079690254988,
8.85372622499635));
#404805=CARTESIAN_POINT('Ctrl Pts',(0.175778066416361,-2.66050922989145,
8.8546225773507));
#404806=CARTESIAN_POINT('Ctrl Pts',(0.175505557048805,-2.6602704142676,
8.85536669723986));
#404807=CARTESIAN_POINT('Ctrl Pts',(0.175195802884927,-2.66004047128033,
8.85610498449051));
#404808=CARTESIAN_POINT('Ctrl Pts',(0.174835028063561,-2.65982905303466,
8.85681338218371));
#404809=CARTESIAN_POINT('Ctrl Pts',(0.174507624346565,-2.65963719064467,
8.85745625420285));
#404810=CARTESIAN_POINT('Ctrl Pts',(0.174134397753556,-2.65945766139716,
8.85808743050666));
#404811=CARTESIAN_POINT('Ctrl Pts',(0.173693040886609,-2.65930836015582,
8.85866804508411));
#404812=CARTESIAN_POINT('Ctrl Pts',(0.173489408395645,-2.65923947579952,
8.85893592806396));
#404813=CARTESIAN_POINT('Ctrl Pts',(0.173271103409276,-2.65917719921061,
8.85919241173848));
#404814=CARTESIAN_POINT('Ctrl Pts',(0.173034988239271,-2.65912457290272,
8.85943017985534));
#404815=CARTESIAN_POINT('Ctrl Pts',(0.172716162862191,-2.65905351180801,
8.8597512372));
#404816=CARTESIAN_POINT('Ctrl Pts',(0.172356609902548,-2.65899886258521,
8.86004599534705));
#404817=CARTESIAN_POINT('Ctrl Pts',(0.171959084215947,-2.65897157865952,
8.86026130871721));
#404818=CARTESIAN_POINT('Ctrl Pts',(0.171813538854646,-2.65896158924511,
8.86034014101235));
#404819=CARTESIAN_POINT('Ctrl Pts',(0.171660717848735,-2.65895510579683,
8.86040910639692));
#404820=CARTESIAN_POINT('Ctrl Pts',(0.171504770462657,-2.65895264102898,
8.86046313645506));
#404821=CARTESIAN_POINT('Ctrl Pts',(0.17126141587273,-2.6589487947794,8.86054744990829));
#404822=CARTESIAN_POINT('Ctrl Pts',(0.171003802956396,-2.65895477658666,
8.86059655985668));
#404823=CARTESIAN_POINT('Ctrl Pts',(0.170748446413576,-2.65896990994078,
8.86059725258816));
#404824=CARTESIAN_POINT('Ctrl Pts',(0.170492499895126,-2.658985078259,8.86059794692011));
#404825=CARTESIAN_POINT('Ctrl Pts',(0.170236138887582,-2.65901226079576,
8.86056369958366));
#404826=CARTESIAN_POINT('Ctrl Pts',(0.169992948659155,-2.65904623288096,
8.86048590497774));
#404827=CARTESIAN_POINT('Ctrl Pts',(0.169929483250181,-2.65905509858372,
8.86046560290182));
#404828=CARTESIAN_POINT('Ctrl Pts',(0.169866101726,-2.65906463173741,8.86044257503091));
#404829=CARTESIAN_POINT('Ctrl Pts',(0.169804757745746,-2.65907450529864,
8.86041778462583));
#404830=CARTESIAN_POINT('Ctrl Pts',(0.169391988880166,-2.6591409421136,
8.86025097596201));
#404831=CARTESIAN_POINT('Ctrl Pts',(0.169016136888523,-2.65923203389475,
8.8599848982295));
#404832=CARTESIAN_POINT('Ctrl Pts',(0.168686176277933,-2.65933688780354,
8.85968173251461));
#404833=CARTESIAN_POINT('Ctrl Pts',(0.168511646019421,-2.65939234951388,
8.85952137522076));
#404834=CARTESIAN_POINT('Ctrl Pts',(0.168346533239082,-2.65945254867042,
8.85934740853961));
#404835=CARTESIAN_POINT('Ctrl Pts',(0.168192633899328,-2.65951517582375,
8.8591675900182));
#404836=CARTESIAN_POINT('Ctrl Pts',(0.167574648054925,-2.65976665639733,
8.85844552518695));
#404837=CARTESIAN_POINT('Ctrl Pts',(0.167101404538696,-2.66006869733527,
8.85759444184123));
#404838=CARTESIAN_POINT('Ctrl Pts',(0.166737667185769,-2.66034962329277,
8.85683498915137));
#404839=CARTESIAN_POINT('Ctrl Pts',(0.1666996030405,-2.66037902144606,8.85675551444997));
#404840=CARTESIAN_POINT('Ctrl Pts',(0.166662753168086,-2.66040820147624,
8.85667699793651));
#404841=CARTESIAN_POINT('Ctrl Pts',(0.166627087527525,-2.66043708934255,
8.85659965593547));
#404842=CARTESIAN_POINT('Ctrl Pts',(0.16614567089128,-2.66082701923615,
8.85555568965886));
#404843=CARTESIAN_POINT('Ctrl Pts',(0.165739313269843,-2.66127129211021,
8.85434650606346));
#404844=CARTESIAN_POINT('Ctrl Pts',(0.165401420054767,-2.66176790975638,
8.85297329937117));
#404845=CARTESIAN_POINT('Ctrl Pts',(0.165211375709423,-2.66204722692299,
8.85220095427747));
#404846=CARTESIAN_POINT('Ctrl Pts',(0.165043172113078,-2.66234339408063,
8.85137579139183));
#404847=CARTESIAN_POINT('Ctrl Pts',(0.164897305964679,-2.66265786424426,
8.85049129520029));
#404848=CARTESIAN_POINT('Origin',(0.171134036480688,-2.66555075509437,7.59394543036555));
#404849=CARTESIAN_POINT('Ctrl Pts',(0.176649753622001,-2.66140845730323,
7.59443877723642));
#404850=CARTESIAN_POINT('Ctrl Pts',(0.173561327260517,-2.65651000690964,
7.58783886950016));
#404851=CARTESIAN_POINT('Ctrl Pts',(0.16552683344579,-2.65925337904586,
7.58559994247159));
#404852=CARTESIAN_POINT('Ctrl Pts',(0.193509382518766,-2.68814895428737,
7.56670252222136));
#404853=CARTESIAN_POINT('Ctrl Pts',(0.190425419810198,-2.68325758354531,
7.56004874999029));
#404854=CARTESIAN_POINT('Ctrl Pts',(0.182336414920134,-2.68599699171951,
7.55786368756704));
#404855=CARTESIAN_POINT('Ctrl Pts',(0.210337527743034,-2.71483951606508,
7.53888913333558));
#404856=CARTESIAN_POINT('Ctrl Pts',(0.207235236893097,-2.70991907566719,
7.53222002137275));
#404857=CARTESIAN_POINT('Ctrl Pts',(0.199116189248108,-2.71269099017859,
7.53005029815327));
#404858=CARTESIAN_POINT('Ctrl Pts',(0.227133427809875,-2.74147893487042,
7.51101258149734));
#404859=CARTESIAN_POINT('Ctrl Pts',(0.223993531557828,-2.73649884979426,
7.5043616886572));
#404860=CARTESIAN_POINT('Ctrl Pts',(0.215865257414856,-2.73933409951895,
7.50217374673251));
#404861=CARTESIAN_POINT('',(0.214971506492228,-2.73791238843282,7.50366116523517));
#404862=CARTESIAN_POINT('Ctrl Pts',(0.222557758686742,-2.73422161816808,
7.51860402984325));
#404863=CARTESIAN_POINT('Ctrl Pts',(0.222793285245637,-2.73459517901432,
7.51734760759493));
#404864=CARTESIAN_POINT('Ctrl Pts',(0.22295578856232,-2.7349644763634,7.51608817408572));
#404865=CARTESIAN_POINT('Ctrl Pts',(0.223032672233713,-2.73533403919153,
7.51481005913118));
#404866=CARTESIAN_POINT('Ctrl Pts',(0.223102315300454,-2.73566879803223,
7.51365231206383));
#404867=CARTESIAN_POINT('Ctrl Pts',(0.223102049090871,-2.73600419561941,
7.51247773061042));
#404868=CARTESIAN_POINT('Ctrl Pts',(0.222994953185465,-2.736334399064,7.51129758471022));
#404869=CARTESIAN_POINT('Ctrl Pts',(0.222861845205859,-2.73674480423496,
7.50983079813402));
#404870=CARTESIAN_POINT('Ctrl Pts',(0.222555569253588,-2.73713006948336,
7.50839324291155));
#404871=CARTESIAN_POINT('Ctrl Pts',(0.222009357599801,-2.73744170500765,
7.50715379678855));
#404872=CARTESIAN_POINT('Ctrl Pts',(0.221757023554462,-2.73758567164031,
7.50658120839351));
#404873=CARTESIAN_POINT('Ctrl Pts',(0.221412902846608,-2.73772613760701,
7.50598221009429));
#404874=CARTESIAN_POINT('Ctrl Pts',(0.22097658878432,-2.73783870041343,
7.50545747549612));
#404875=CARTESIAN_POINT('Ctrl Pts',(0.2207437580955,-2.73789876741109,7.50517746087247));
#404876=CARTESIAN_POINT('Ctrl Pts',(0.220482200112825,-2.73795173606975,
7.50491486231392));
#404877=CARTESIAN_POINT('Ctrl Pts',(0.220198510259517,-2.73799456886009,
7.50468370960992));
#404878=CARTESIAN_POINT('Ctrl Pts',(0.219774304443933,-2.7380586173925,
7.50433806340447));
#404879=CARTESIAN_POINT('Ctrl Pts',(0.219287809037178,-2.73810137257825,
7.50405484070984));
#404880=CARTESIAN_POINT('Ctrl Pts',(0.218771725882367,-2.73811924129067,
7.50385766036131));
#404881=CARTESIAN_POINT('Ctrl Pts',(0.218716538810708,-2.73812115207172,
7.50383657498791));
#404882=CARTESIAN_POINT('Ctrl Pts',(0.218661038309198,-2.73812279184612,
7.50381643264937));
#404883=CARTESIAN_POINT('Ctrl Pts',(0.218605282305343,-2.73812416636047,
7.50379723213559));
#404884=CARTESIAN_POINT('Ctrl Pts',(0.218233092740555,-2.73813334169338,
7.50366906242519));
#404885=CARTESIAN_POINT('Ctrl Pts',(0.217841404285952,-2.73813017779315,
7.50358235568538));
#404886=CARTESIAN_POINT('Ctrl Pts',(0.21746393812843,-2.73811805291127,
7.5035341175365));
#404887=CARTESIAN_POINT('Ctrl Pts',(0.216897970346147,-2.73809987302315,
7.50346178989176));
#404888=CARTESIAN_POINT('Ctrl Pts',(0.216289890791844,-2.7380562513047,
7.50346967198527));
#404889=CARTESIAN_POINT('Ctrl Pts',(0.215694262731985,-2.73799506025502,
7.50354272648692));
#404890=CARTESIAN_POINT('Ctrl Pts',(0.215449268582192,-2.7379698911097,
7.50357277531559));
#404891=CARTESIAN_POINT('Ctrl Pts',(0.215206692060812,-2.73794192399818,
7.50361331098761));
#404892=CARTESIAN_POINT('Ctrl Pts',(0.214971506492339,-2.73791238843424,
7.50366116523658));
#404893=CARTESIAN_POINT('',(0.171321629291032,-2.66847266454068,7.57603338622103));
#404894=CARTESIAN_POINT('Origin',(0.171884966568961,-2.67729162937223,7.5848687342763));
#404895=CARTESIAN_POINT('Ctrl Pts',(0.214971506527151,-2.73791238847831,
7.50366116529969));
#404896=CARTESIAN_POINT('Ctrl Pts',(0.200444582347945,-2.71480402911006,
7.52783573079709));
#404897=CARTESIAN_POINT('Ctrl Pts',(0.185895295086789,-2.69165855688567,
7.55196141284069));
#404898=CARTESIAN_POINT('Ctrl Pts',(0.171321630229629,-2.66847266536934,
7.57603338728831));
#404899=CARTESIAN_POINT('Ctrl Pts',(0.176949628854398,-2.66188407944157,
7.59394543036555));
#404900=CARTESIAN_POINT('Ctrl Pts',(0.170212604558692,-2.65119870914281,
7.59394543036555));
#404901=CARTESIAN_POINT('Ctrl Pts',(0.164897305964678,-2.66265786424426,
7.59394543036555));
#404902=CARTESIAN_POINT('Ctrl Pts',(0.175705296970942,-2.65991048600244,
7.58587155981959));
#404903=CARTESIAN_POINT('Ctrl Pts',(0.170587343070376,-2.65703556394579,
7.58685956158228));
#404904=CARTESIAN_POINT('Ctrl Pts',(0.165879044373256,-2.66054135235053,
7.58587155981959));
#404905=CARTESIAN_POINT('Ctrl Pts',(0.172975141359167,-2.66456245493304,
7.57982961904597));
#404906=CARTESIAN_POINT('Ctrl Pts',(0.170972652354739,-2.66303706706671,
7.58148017275036));
#404907=CARTESIAN_POINT('Ctrl Pts',(0.169181666028244,-2.66480600412994,
7.57982961904596));
#404908=CARTESIAN_POINT('Ctrl Pts',(0.17132162923821,-2.66847266371479,
7.57603338509286));
#404909=CARTESIAN_POINT('Ctrl Pts',(0.17132162923821,-2.66847266371479,
7.57603338509286));
#404910=CARTESIAN_POINT('Ctrl Pts',(0.17132162923821,-2.66847266371479,
7.57603338509286));
#404911=CARTESIAN_POINT('Origin',(0.171890661196855,-2.67729126376634,7.58486873427622));
#404912=CARTESIAN_POINT('Ctrl Pts',(0.125292469645955,-2.74804120708308,
7.51098857897448));
#404913=CARTESIAN_POINT('Ctrl Pts',(0.127769759546178,-2.74270046305981,
7.50433767179956));
#404914=CARTESIAN_POINT('Ctrl Pts',(0.13619389345922,-2.74447303714785,
7.50214974420965));
#404915=CARTESIAN_POINT('Ctrl Pts',(0.138547713792469,-2.71946446846798,
7.5388732158917));
#404916=CARTESIAN_POINT('Ctrl Pts',(0.140995321363304,-2.71418771603622,
7.53220407452064));
#404917=CARTESIAN_POINT('Ctrl Pts',(0.149402205571115,-2.71589862744197,
7.53003438070911));
#404918=CARTESIAN_POINT('Ctrl Pts',(0.151828412897425,-2.69083285197316,
7.56669465659229));
#404919=CARTESIAN_POINT('Ctrl Pts',(0.154261555562573,-2.68558728416721,
7.56004085833293));
#404920=CARTESIAN_POINT('Ctrl Pts',(0.162634477916496,-2.68726978866384,
7.55785582193789));
#404921=CARTESIAN_POINT('Ctrl Pts',(0.165133966327907,-2.66214765249215,
7.59443891967696));
#404922=CARTESIAN_POINT('Ctrl Pts',(0.167570636746966,-2.656894479266,7.58783901202978));
#404923=CARTESIAN_POINT('Ctrl Pts',(0.175889981935509,-2.65858789995271,
7.58560008491213));
#404924=CARTESIAN_POINT('',(0.136909871778145,-2.74292411166389,7.50366116523517));
#404925=CARTESIAN_POINT('Ctrl Pts',(0.136909871778163,-2.74292411166427,
7.50366116523554));
#404926=CARTESIAN_POINT('Ctrl Pts',(0.136176261638596,-2.74311372622038,
7.50350835821027));
#404927=CARTESIAN_POINT('Ctrl Pts',(0.135495726955406,-2.74326416077797,
7.50345484955999));
#404928=CARTESIAN_POINT('Ctrl Pts',(0.13484816449329,-2.74338047422534,
7.50349758195598));
#404929=CARTESIAN_POINT('Ctrl Pts',(0.134515916925741,-2.74344015164987,
7.50351950684424));
#404930=CARTESIAN_POINT('Ctrl Pts',(0.134159624361124,-2.74349685631232,
7.50357029184312));
#404931=CARTESIAN_POINT('Ctrl Pts',(0.133814552501086,-2.74354209194315,
7.50365515313923));
#404932=CARTESIAN_POINT('Ctrl Pts',(0.133283692246956,-2.74361168266108,
7.50378570417639));
#404933=CARTESIAN_POINT('Ctrl Pts',(0.132763850166139,-2.74365651668585,
7.50400001621911));
#404934=CARTESIAN_POINT('Ctrl Pts',(0.132294398701274,-2.74367091947915,
7.50428903009634));
#404935=CARTESIAN_POINT('Ctrl Pts',(0.132242293200415,-2.74367251807839,
7.50432110841318));
#404936=CARTESIAN_POINT('Ctrl Pts',(0.132190784057866,-2.74367375975199,
7.50435406373354));
#404937=CARTESIAN_POINT('Ctrl Pts',(0.132139906905781,-2.74367464975632,
7.50438785222352));
#404938=CARTESIAN_POINT('Ctrl Pts',(0.131829277437644,-2.74368008366058,
7.50459414719561));
#404939=CARTESIAN_POINT('Ctrl Pts',(0.131537252052987,-2.74367197926943,
7.50483629897752));
#404940=CARTESIAN_POINT('Ctrl Pts',(0.131274981649372,-2.74365196258472,
7.5050991045531));
#404941=CARTESIAN_POINT('Ctrl Pts',(0.130696386796431,-2.74360780376776,
7.50567888004914));
#404942=CARTESIAN_POINT('Ctrl Pts',(0.130239766303518,-2.74350444791973,
7.50637912803144));
#404943=CARTESIAN_POINT('Ctrl Pts',(0.129890662582497,-2.74336921529871,
7.50710440483569));
#404944=CARTESIAN_POINT('Ctrl Pts',(0.129805055419423,-2.74333605357529,
7.50728225710685));
#404945=CARTESIAN_POINT('Ctrl Pts',(0.129724156641004,-2.74330045095875,
7.50746498566954));
#404946=CARTESIAN_POINT('Ctrl Pts',(0.129649686880133,-2.74326361983096,
7.50764697238949));
#404947=CARTESIAN_POINT('Ctrl Pts',(0.129249357940325,-2.74306562582414,
7.50862528291181));
#404948=CARTESIAN_POINT('Ctrl Pts',(0.128996641605847,-2.74281786641564,
7.5096585683742));
#404949=CARTESIAN_POINT('Ctrl Pts',(0.128834110610838,-2.74255347021814,
7.510679598732));
#404950=CARTESIAN_POINT('Ctrl Pts',(0.128744669599277,-2.74240797265716,
7.51124147302577));
#404951=CARTESIAN_POINT('Ctrl Pts',(0.128682887795632,-2.74225717394986,
7.51180065547252));
#404952=CARTESIAN_POINT('Ctrl Pts',(0.128641559193309,-2.74210525799208,
7.512351757165));
#404953=CARTESIAN_POINT('Ctrl Pts',(0.128498752408923,-2.74158032784183,
7.51425603304536));
#404954=CARTESIAN_POINT('Ctrl Pts',(0.128588977115428,-2.740977877902,7.51626900505181));
#404955=CARTESIAN_POINT('Ctrl Pts',(0.128867104965898,-2.7403379843463,
7.51827788969244));
#404956=CARTESIAN_POINT('Ctrl Pts',(0.128882157770753,-2.74030335209783,
7.51838661432546));
#404957=CARTESIAN_POINT('Ctrl Pts',(0.128897769997591,-2.74026860594205,
7.51849533314857));
#404958=CARTESIAN_POINT('Ctrl Pts',(0.128913937383393,-2.74023375097046,
7.51860402984325));
#404959=CARTESIAN_POINT('Ctrl Pts',(0.171321628465944,-2.66847266548377,
7.57603338728985));
#404960=CARTESIAN_POINT('Ctrl Pts',(0.159832559191517,-2.69333184005413,
7.55196141284922));
#404961=CARTESIAN_POINT('Ctrl Pts',(0.148362498662249,-2.71814780985154,
7.52783573083105));
#404962=CARTESIAN_POINT('Ctrl Pts',(0.136909871748486,-2.74292411171511,
7.50366116530176));
#404963=CARTESIAN_POINT('Origin',(5.91995423665314E-17,-9.22080657369148E-16,
7.49482233047033));
#404964=CARTESIAN_POINT('Origin',(0.214279640797806,-2.72910067339766,7.49482233047033));
#404965=CARTESIAN_POINT('Origin',(0.,0.,7.50366116523517));
#404966=CARTESIAN_POINT('Origin',(0.13646924015651,-2.73409626686609,7.49482233047033));
#404967=CARTESIAN_POINT('Ctrl Pts',(0.222557194605735,-2.73422072341404,
7.51860402984325));
#404968=CARTESIAN_POINT('Ctrl Pts',(0.226614772381166,-2.74065751987086,
7.51860402984325));
#404969=CARTESIAN_POINT('Ctrl Pts',(0.234196090687522,-2.74000952390803,
7.51860402984325));
#404970=CARTESIAN_POINT('Ctrl Pts',(0.224063801999073,-2.7366107491878,
7.51041458714367));
#404971=CARTESIAN_POINT('Ctrl Pts',(0.228410872679967,-2.74050399234173,
7.51004642900443));
#404972=CARTESIAN_POINT('Ctrl Pts',(0.23419818152509,-2.74000934519844,
7.50729136483012));
#404973=CARTESIAN_POINT('Ctrl Pts',(0.22234652916971,-2.73884115525596,
7.50215815450136));
#404974=CARTESIAN_POINT('Ctrl Pts',(0.224753845205989,-2.74081672959849,
7.49877163671529));
#404975=CARTESIAN_POINT('Ctrl Pts',(0.22819346670093,-2.74054667855528,
7.49481588533168));
#404976=CARTESIAN_POINT('Ctrl Pts',(0.214971463399589,-2.73791183960396,
7.50366171572174));
#404977=CARTESIAN_POINT('Ctrl Pts',(0.215258086645813,-2.74156232030818,
7.50000045605858));
#404978=CARTESIAN_POINT('Ctrl Pts',(0.215258086645937,-2.74156232030817,
7.49482233047317));
#404979=CARTESIAN_POINT('Origin',(0.233131563002578,-2.72755493516299,7.51860402984325));
#404980=CARTESIAN_POINT('Origin',(0.233131563002578,-2.72755493516299,9.));
#404981=CARTESIAN_POINT('Origin',(0.233131563002578,-2.72755493516299,8.75721825406948));
#404982=CARTESIAN_POINT('Ctrl Pts',(0.213651009822431,-2.72009486320776,
8.78942910404912));
#404983=CARTESIAN_POINT('Ctrl Pts',(0.21660588741383,-2.72481938721781,
8.79672699501691));
#404984=CARTESIAN_POINT('Ctrl Pts',(0.22491413159174,-2.72155647982373,
8.79893251111267));
#404985=CARTESIAN_POINT('Ctrl Pts',(0.219514666098752,-2.7293950220136,
8.78111911759582));
#404986=CARTESIAN_POINT('Ctrl Pts',(0.223024018852947,-2.73499205277749,
8.78644465894813));
#404987=CARTESIAN_POINT('Ctrl Pts',(0.231029453604124,-2.73371591555135,
8.78817647674133));
#404988=CARTESIAN_POINT('Ctrl Pts',(0.22316903657846,-2.73519110279413,
8.7678092393203));
#404989=CARTESIAN_POINT('Ctrl Pts',(0.22731599665726,-2.74179545430472,
8.76988516158374));
#404990=CARTESIAN_POINT('Ctrl Pts',(0.234858960007768,-2.74130547033627,
8.77093053738832));
#404991=CARTESIAN_POINT('Ctrl Pts',(0.222456484349966,-2.73406094636595,
8.75371302330492));
#404992=CARTESIAN_POINT('Ctrl Pts',(0.226501019435815,-2.74050361175437,
8.75300828287559));
#404993=CARTESIAN_POINT('Ctrl Pts',(0.23411245922325,-2.73982499279172,
8.75267964240738));
#404994=CARTESIAN_POINT('Origin',(0.22565283473727,-2.71569317285207,8.78727029226991));
#404995=CARTESIAN_POINT('Ctrl Pts',(0.176949628854398,-2.66188407944157,
8.85049129520029));
#404996=CARTESIAN_POINT('Ctrl Pts',(0.180064098225814,-2.66682383578754,
8.85711686593484));
#404997=CARTESIAN_POINT('Ctrl Pts',(0.18814612056788,-2.66403427005498,
8.85933012996512));
#404998=CARTESIAN_POINT('Ctrl Pts',(0.189677921384504,-2.68207200113894,
8.82945683644723));
#404999=CARTESIAN_POINT('Ctrl Pts',(0.192818242734749,-2.68705276044921,
8.8360746990239));
#405000=CARTESIAN_POINT('Ctrl Pts',(0.200911757808383,-2.68421955444712,
8.8382956714852));
#405001=CARTESIAN_POINT('Ctrl Pts',(0.20238724136817,-2.70222983111105,
8.80838214965002));
#405002=CARTESIAN_POINT('Ctrl Pts',(0.205539955892651,-2.70723024682302,
8.81501364461987));
#405003=CARTESIAN_POINT('Ctrl Pts',(0.21365746521294,-2.70437457614343,
8.81722098428721));
#405004=CARTESIAN_POINT('Ctrl Pts',(0.215079030421435,-2.72235985585717,
8.78727029226991));
#405005=CARTESIAN_POINT('Ctrl Pts',(0.218232268622154,-2.72736110215464,
8.79393457792714));
#405006=CARTESIAN_POINT('Ctrl Pts',(0.226384750345669,-2.7245016516959,
8.79610912703474));
#405007=CARTESIAN_POINT('Origin',(0.187523433170234,-2.65521739643647,8.85049129520029));
#405008=CARTESIAN_POINT('Ctrl Pts',(0.164897305964679,-2.66265786424426,
8.85049129520029));
#405009=CARTESIAN_POINT('Ctrl Pts',(0.162440088364686,-2.66795533476228,
8.85711686593484));
#405010=CARTESIAN_POINT('Ctrl Pts',(0.154067697566117,-2.6662221774036,
8.85933012996512));
#405011=CARTESIAN_POINT('Ctrl Pts',(0.167071170905082,-2.65797126854675,
8.86332496987232));
#405012=CARTESIAN_POINT('Ctrl Pts',(0.162486551694914,-2.65854846961614,
8.86648636486737));
#405013=CARTESIAN_POINT('Ctrl Pts',(0.160164715441418,-2.65311844398962,
8.87206031107457));
#405014=CARTESIAN_POINT('Ctrl Pts',(0.174175579449892,-2.65748425188965,
8.86341338519876));
#405015=CARTESIAN_POINT('Ctrl Pts',(0.178809323360593,-2.65744080071698,
8.86654584966059));
#405016=CARTESIAN_POINT('Ctrl Pts',(0.180366172242112,-2.65172237660299,
8.87215952290714));
#405017=CARTESIAN_POINT('Ctrl Pts',(0.176949628854398,-2.66188407944157,
8.85049129520029));
#405018=CARTESIAN_POINT('Ctrl Pts',(0.180064098225814,-2.66682383578754,
8.85711686593484));
#405019=CARTESIAN_POINT('Ctrl Pts',(0.188146120567879,-2.66403427005498,
8.85933012996512));
#405020=CARTESIAN_POINT('Origin',(0.153557795935569,-2.65739806269859,8.85049129520029));
#405021=CARTESIAN_POINT('Ctrl Pts',(0.134814416896129,-2.72751301502058,
8.78727029226991));
#405022=CARTESIAN_POINT('Ctrl Pts',(0.132326611918855,-2.7328764283063,
8.79393457792714));
#405023=CARTESIAN_POINT('Ctrl Pts',(0.123875403548956,-2.73108297011979,
8.79610912703474));
#405024=CARTESIAN_POINT('Ctrl Pts',(0.14482783610753,-2.70592526753854,
8.80838214965003));
#405025=CARTESIAN_POINT('Ctrl Pts',(0.142340444294203,-2.71128779009168,
8.81501364461993));
#405026=CARTESIAN_POINT('Ctrl Pts',(0.133924404552021,-2.70949360848066,
8.81722098428721));
#405027=CARTESIAN_POINT('Ctrl Pts',(0.15485508666727,-2.68430770130539,
8.82945683644722));
#405028=CARTESIAN_POINT('Ctrl Pts',(0.152377472675528,-2.68964914403163,
8.83607469902389));
#405029=CARTESIAN_POINT('Ctrl Pts',(0.143988102906756,-2.68787417434732,
8.8382956714852));
#405030=CARTESIAN_POINT('Ctrl Pts',(0.164897305964678,-2.66265786424426,
8.85049129520029));
#405031=CARTESIAN_POINT('Ctrl Pts',(0.162440088364686,-2.66795533476228,
8.85711686593484));
#405032=CARTESIAN_POINT('Ctrl Pts',(0.154067697566117,-2.6662221774036,
8.85933012996512));
#405033=CARTESIAN_POINT('Origin',(0.123474906867021,-2.72225321347492,8.78727029226991));
#405034=CARTESIAN_POINT('Ctrl Pts',(0.128991833512721,-2.74006577228906,
8.75374538247847));
#405035=CARTESIAN_POINT('Ctrl Pts',(0.125806215729252,-2.74696477350121,
8.75304829418601));
#405036=CARTESIAN_POINT('Ctrl Pts',(0.118178814785805,-2.74727038445809,
8.75272238421917));
#405037=CARTESIAN_POINT('Ctrl Pts',(0.12843640572388,-2.74126320992229,
8.76769408445021));
#405038=CARTESIAN_POINT('Ctrl Pts',(0.12516999712376,-2.74833553131129,
8.7697431809397));
#405039=CARTESIAN_POINT('Ctrl Pts',(0.117634307816553,-2.74881692921888,
8.7707786988043));
#405040=CARTESIAN_POINT('Ctrl Pts',(0.131283212176553,-2.7351258267558,
8.78108014887987));
#405041=CARTESIAN_POINT('Ctrl Pts',(0.12851849783378,-2.74112095743854,
8.78639403366323));
#405042=CARTESIAN_POINT('Ctrl Pts',(0.120426966568877,-2.74089915230321,
8.78812224174741));
#405043=CARTESIAN_POINT('Ctrl Pts',(0.135948499481621,-2.72506801057236,
8.78944554828686));
#405044=CARTESIAN_POINT('Ctrl Pts',(0.13362358397994,-2.73012282862319,
8.79673892988687));
#405045=CARTESIAN_POINT('Ctrl Pts',(0.124974904203878,-2.72795398274399,
8.79894799272499));
#405046=CARTESIAN_POINT('Origin',(0.117574427354288,-2.73497394942481,8.75721825406948));
#405047=CARTESIAN_POINT('Origin',(0.117574427354288,-2.73497394942481,9.));
#405048=CARTESIAN_POINT('Origin',(0.117574427354288,-2.73497394942481,7.51860402984325));
#405049=CARTESIAN_POINT('Ctrl Pts',(0.136909832561502,-2.74292332597825,
7.50366195182966));
#405050=CARTESIAN_POINT('Ctrl Pts',(0.137092387371697,-2.74658072470567,
7.50000065167735));
#405051=CARTESIAN_POINT('Ctrl Pts',(0.13709238737158,-2.74658072470568,
7.49482233047108));
#405052=CARTESIAN_POINT('Ctrl Pts',(0.129707514805738,-2.74478891396914,
7.50215800491336));
#405053=CARTESIAN_POINT('Ctrl Pts',(0.127570877920035,-2.74705595609338,
7.49877273257266));
#405054=CARTESIAN_POINT('Ctrl Pts',(0.124123047921434,-2.74722807422352,
7.49481816995647));
#405055=CARTESIAN_POINT('Ctrl Pts',(0.127728229063037,-2.74279080378928,
7.51043025814043));
#405056=CARTESIAN_POINT('Ctrl Pts',(0.12391537177406,-2.74721289337237,
7.51006209594515));
#405057=CARTESIAN_POINT('Ctrl Pts',(0.118108767356082,-2.74746252368982,
7.50731281821701));
#405058=CARTESIAN_POINT('Ctrl Pts',(0.128914573276759,-2.74023237984243,
7.51860402984326));
#405059=CARTESIAN_POINT('Ctrl Pts',(0.125713547171854,-2.74713560005233,
7.51860402984326));
#405060=CARTESIAN_POINT('Ctrl Pts',(0.11811129688558,-2.74746241494729,
7.51860402984327));
#405061=CARTESIAN_POINT('Origin',(0.,0.,7.5));
#405062=CARTESIAN_POINT('Origin',(0.335155581859898,-2.64662214142562,7.5));
#405063=CARTESIAN_POINT('',(0.335155581859898,-2.64662214142562,7.59394543036555));
#405064=CARTESIAN_POINT('',(0.335155581859898,-2.64662214142562,8.85049129520029));
#405065=CARTESIAN_POINT('',(0.335155581859898,-2.64662214142562,7.5));
#405066=CARTESIAN_POINT('',(0.309289785090442,-2.71327145765926,8.78727029226991));
#405067=CARTESIAN_POINT('Ctrl Pts',(0.335155581859898,-2.64662214142562,
8.85049129520029));
#405068=CARTESIAN_POINT('Ctrl Pts',(0.326521116789889,-2.66887087391543,
8.82945686509571));
#405069=CARTESIAN_POINT('Ctrl Pts',(0.317899487896271,-2.69108653097411,
8.80838212259896));
#405070=CARTESIAN_POINT('Ctrl Pts',(0.309289785090442,-2.71327145765926,
8.78727029226991));
#405071=CARTESIAN_POINT('',(0.304216449096319,-2.72634410251322,8.75721825406948));
#405072=CARTESIAN_POINT('Origin',(0.319484065186767,-2.68700405222726,8.75937679713114));
#405073=CARTESIAN_POINT('',(0.304216449096319,-2.72634410251322,7.51860402984325));
#405074=CARTESIAN_POINT('',(0.304216449096319,-2.72634410251322,7.5));
#405075=CARTESIAN_POINT('Ctrl Pts',(0.304216449096319,-2.72634410251322,
7.51860402984325));
#405076=CARTESIAN_POINT('Ctrl Pts',(0.308200765466706,-2.71607757316128,
7.52834476460825));
#405077=CARTESIAN_POINT('Ctrl Pts',(0.312187668397793,-2.70580437892665,
7.53807742314407));
#405078=CARTESIAN_POINT('Ctrl Pts',(0.316177244736788,-2.69552429602699,
7.54780169004675));
#405079=CARTESIAN_POINT('Ctrl Pts',(0.322496518039553,-2.67924120030501,
7.5632044032688));
#405080=CARTESIAN_POINT('Ctrl Pts',(0.328822506613121,-2.66294080110644,
7.57858609112103));
#405081=CARTESIAN_POINT('Ctrl Pts',(0.335155581859899,-2.64662214142562,
7.59394543036555));
#405082=CARTESIAN_POINT('Origin',(0.508403499682117,-2.86782650745936,7.5));
#405083=CARTESIAN_POINT('',(0.397282670454326,-2.71434454205174,8.75721825406948));
#405084=CARTESIAN_POINT('',(0.389059322317711,-2.70298631476879,8.78727029226991));
#405085=CARTESIAN_POINT('Origin',(0.368185397592234,-2.67415489751875,8.7565864062112));
#405086=CARTESIAN_POINT('',(0.347133565397108,-2.64507775146798,8.85049129520029));
#405087=CARTESIAN_POINT('Ctrl Pts',(0.389059322317711,-2.70298631476879,
8.78727029226991));
#405088=CARTESIAN_POINT('Ctrl Pts',(0.375103892673955,-2.68371083973214,
8.80838212259895));
#405089=CARTESIAN_POINT('Ctrl Pts',(0.361129132086633,-2.66440866446988,
8.82945686509571));
#405090=CARTESIAN_POINT('Ctrl Pts',(0.347133565397108,-2.64507775146798,
8.85049129520029));
#405091=CARTESIAN_POINT('',(0.347133565397108,-2.64507775146798,7.59394543036555));
#405092=CARTESIAN_POINT('',(0.347133565397108,-2.64507775146798,7.5));
#405093=CARTESIAN_POINT('',(0.397282670454326,-2.71434454205174,7.51860402984325));
#405094=CARTESIAN_POINT('Ctrl Pts',(0.347133565397108,-2.64507775146798,
7.59394543036555));
#405095=CARTESIAN_POINT('Ctrl Pts',(0.357398819381853,-2.65925629358232,
7.57858609112103));
#405096=CARTESIAN_POINT('Ctrl Pts',(0.367652586608856,-2.67341896999297,
7.56320440326857));
#405097=CARTESIAN_POINT('Ctrl Pts',(0.377895469082877,-2.68756661219899,
7.54780169004651));
#405098=CARTESIAN_POINT('Ctrl Pts',(0.384362155931758,-2.6964985092532,
7.53807742314383));
#405099=CARTESIAN_POINT('Ctrl Pts',(0.390824509465566,-2.70542442105946,
7.52834476460825));
#405100=CARTESIAN_POINT('Ctrl Pts',(0.397282670454325,-2.71434454205173,
7.51860402984325));
#405101=CARTESIAN_POINT('',(0.397282670454326,-2.71434454205174,7.5));
#405102=CARTESIAN_POINT('Origin',(0.341564846497323,-2.6491094998251,7.5));
#405103=CARTESIAN_POINT('Ctrl Pts',(0.347133565397107,-2.64507775146798,
8.85049129520029));
#405104=CARTESIAN_POINT('Ctrl Pts',(0.34701999529408,-2.64492088652424,
8.85097269580138));
#405105=CARTESIAN_POINT('Ctrl Pts',(0.346901044882032,-2.64477093347822,
8.85143669361005));
#405106=CARTESIAN_POINT('Ctrl Pts',(0.34677055192744,-2.64462153081528,
8.8519052845931));
#405107=CARTESIAN_POINT('Ctrl Pts',(0.34651531598382,-2.64432930868135,
8.85282181883899));
#405108=CARTESIAN_POINT('Ctrl Pts',(0.346222339439965,-2.64404683890338,
8.85372622499636));
#405109=CARTESIAN_POINT('Ctrl Pts',(0.345876323146632,-2.64378078895684,
8.85462257735071));
#405110=CARTESIAN_POINT('Ctrl Pts',(0.345589072709243,-2.64355992374042,
8.85536669723986));
#405111=CARTESIAN_POINT('Ctrl Pts',(0.345265222470739,-2.6433502992131,
8.85610498449051));
#405112=CARTESIAN_POINT('Ctrl Pts',(0.344891643286429,-2.64316243027106,
8.85681338218371));
#405113=CARTESIAN_POINT('Ctrl Pts',(0.344552619589951,-2.6429919389111,
8.85745625420284));
#405114=CARTESIAN_POINT('Ctrl Pts',(0.344168657352627,-2.6428366912356,
8.85808743050666));
#405115=CARTESIAN_POINT('Ctrl Pts',(0.343718641537324,-2.64271597458123,
8.8586680450841));
#405116=CARTESIAN_POINT('Ctrl Pts',(0.343511013995289,-2.64266027853371,
8.85893592806396));
#405117=CARTESIAN_POINT('Ctrl Pts',(0.343289167465176,-2.64261211674724,
8.85919241173848));
#405118=CARTESIAN_POINT('Ctrl Pts',(0.343050165639986,-2.64257472651662,
8.85943017985534));
#405119=CARTESIAN_POINT('Ctrl Pts',(0.342727442423867,-2.6425242386366,
8.8597512372));
#405120=CARTESIAN_POINT('Ctrl Pts',(0.342365126816615,-2.64249273833371,
8.86004599534705));
#405121=CARTESIAN_POINT('Ctrl Pts',(0.34196666980205,-2.64249098002396,
8.86026130871721));
#405122=CARTESIAN_POINT('Ctrl Pts',(0.341820783455326,-2.64249033625719,
8.86034014101235));
#405123=CARTESIAN_POINT('Ctrl Pts',(0.341667861040604,-2.64249365740532,
8.86040910639692));
#405124=CARTESIAN_POINT('Ctrl Pts',(0.341512076146937,-2.64250118928493,
8.86046313645506));
#405125=CARTESIAN_POINT('Ctrl Pts',(0.341268975125058,-2.64251294271998,
8.86054744990829));
#405126=CARTESIAN_POINT('Ctrl Pts',(0.341012274757796,-2.6425354175532,
8.86059655985668));
#405127=CARTESIAN_POINT('Ctrl Pts',(0.340758412469709,-2.6425668805641,
8.86059725258815));
#405128=CARTESIAN_POINT('Ctrl Pts',(0.340503963658316,-2.64259841626712,
8.86059794692011));
#405129=CARTESIAN_POINT('Ctrl Pts',(0.340249870963067,-2.64264196806059,
8.86056369958366));
#405130=CARTESIAN_POINT('Ctrl Pts',(0.340009356994018,-2.64269145159793,
8.86048590497774));
#405131=CARTESIAN_POINT('Ctrl Pts',(0.33994659000906,-2.64270436532787,
8.86046560290182));
#405132=CARTESIAN_POINT('Ctrl Pts',(0.339883949500272,-2.64271793976287,
8.86044257503091));
#405133=CARTESIAN_POINT('Ctrl Pts',(0.339823364159044,-2.64273172336011,
8.86041778462583));
#405134=CARTESIAN_POINT('Ctrl Pts',(0.339415699992718,-2.64282446986554,
8.860250975962));
#405135=CARTESIAN_POINT('Ctrl Pts',(0.339046456499758,-2.64293945540863,
8.8599848982295));
#405136=CARTESIAN_POINT('Ctrl Pts',(0.338723891841634,-2.64306523453273,
8.85968173251461));
#405137=CARTESIAN_POINT('Ctrl Pts',(0.338553273618238,-2.6431317644831,
8.85952137522076));
#405138=CARTESIAN_POINT('Ctrl Pts',(0.338392357053016,-2.64320241876617,
8.85934740853961));
#405139=CARTESIAN_POINT('Ctrl Pts',(0.338242786451452,-2.64327477760985,
8.8591675900182));
#405140=CARTESIAN_POINT('Ctrl Pts',(0.337642182740921,-2.64356533597861,
8.85844552518695));
#405141=CARTESIAN_POINT('Ctrl Pts',(0.337189263383592,-2.64389707715724,
8.85759444184125));
#405142=CARTESIAN_POINT('Ctrl Pts',(0.336844272355963,-2.64420073065445,
8.85683498915139));
#405143=CARTESIAN_POINT('Ctrl Pts',(0.336808169963707,-2.64423250718423,
8.85675551444999));
#405144=CARTESIAN_POINT('Ctrl Pts',(0.336773265374257,-2.64426398824035,
8.85667699793651));
#405145=CARTESIAN_POINT('Ctrl Pts',(0.336739523864526,-2.64429510185888,
8.85659965593547));
#405146=CARTESIAN_POINT('Ctrl Pts',(0.336284079244452,-2.64471507506948,
8.85555568965886));
#405147=CARTESIAN_POINT('Ctrl Pts',(0.335907021189103,-2.64518447055947,
8.85434650606346));
#405148=CARTESIAN_POINT('Ctrl Pts',(0.335601640613713,-2.64570171674404,
8.85297329937118));
#405149=CARTESIAN_POINT('Ctrl Pts',(0.335429882647167,-2.64599263620658,
8.85220095427747));
#405150=CARTESIAN_POINT('Ctrl Pts',(0.335281000138092,-2.64629897169846,
8.85137579139184));
#405151=CARTESIAN_POINT('Ctrl Pts',(0.335155581859898,-2.64662214142562,
8.85049129520029));
#405152=CARTESIAN_POINT('Origin',(0.341564846497323,-2.6491094998251,7.59394543036555));
#405153=CARTESIAN_POINT('Ctrl Pts',(0.346803833075505,-2.64462231961843,
7.59443877723642));
#405154=CARTESIAN_POINT('Ctrl Pts',(0.343407907422933,-2.63993180977292,
7.58783886950016));
#405155=CARTESIAN_POINT('Ctrl Pts',(0.335565689793701,-2.64318431714299,
7.58559994247159));
#405156=CARTESIAN_POINT('Ctrl Pts',(0.365342091580689,-2.67022767525142,
7.56670252222137));
#405157=CARTESIAN_POINT('Ctrl Pts',(0.361951074004762,-2.66554394452431,
7.56004874999028));
#405158=CARTESIAN_POINT('Ctrl Pts',(0.354054203327156,-2.66879598861332,
7.55786368756704));
#405159=CARTESIAN_POINT('Ctrl Pts',(0.38384573174027,-2.69578521544099,
7.53888913333556));
#405160=CARTESIAN_POINT('Ctrl Pts',(0.380434561180908,-2.69107364907284,
7.53222002137276));
#405161=CARTESIAN_POINT('Ctrl Pts',(0.372509792162587,-2.69436005755723,
7.53005029815326));
#405162=CARTESIAN_POINT('Ctrl Pts',(0.402313916252095,-2.72129378369128,
7.51101258149734));
#405163=CARTESIAN_POINT('Ctrl Pts',(0.398861396107298,-2.7165251045776,
7.5043616886572));
#405164=CARTESIAN_POINT('Ctrl Pts',(0.390931477448869,-2.71987530929006,
7.50217374673251));
#405165=CARTESIAN_POINT('',(0.389948473491329,-2.71851378208006,7.50366116523517));
#405166=CARTESIAN_POINT('Ctrl Pts',(0.397282670454326,-2.71434454205174,
7.51860402984325));
#405167=CARTESIAN_POINT('Ctrl Pts',(0.397541647224239,-2.7147022451387,
7.51734760759494));
#405168=CARTESIAN_POINT('Ctrl Pts',(0.397727477622823,-2.71506037210353,
7.51608817408573));
#405169=CARTESIAN_POINT('Ctrl Pts',(0.397827881300162,-2.71542424967145,
7.5148100591312));
#405170=CARTESIAN_POINT('Ctrl Pts',(0.39791882935032,-2.7157538586676,7.51365231206384));
#405171=CARTESIAN_POINT('Ctrl Pts',(0.397940052684887,-2.71608858420057,
7.51247773061043));
#405172=CARTESIAN_POINT('Ctrl Pts',(0.397854333026837,-2.71642497086499,
7.51129758471022));
#405173=CARTESIAN_POINT('Ctrl Pts',(0.397747793281437,-2.71684306107205,
7.50983079813402));
#405174=CARTESIAN_POINT('Ctrl Pts',(0.397466830635174,-2.71724715791932,
7.50839324291155));
#405175=CARTESIAN_POINT('Ctrl Pts',(0.396941707788404,-2.71759314905581,
7.50715379678855));
#405176=CARTESIAN_POINT('Ctrl Pts',(0.396699116164248,-2.71775298699137,
7.5065812083935));
#405177=CARTESIAN_POINT('Ctrl Pts',(0.39636470217468,-2.71791521224513,
7.50598221009429));
#405178=CARTESIAN_POINT('Ctrl Pts',(0.395936496490198,-2.71805549851715,
7.50545747549611));
#405179=CARTESIAN_POINT('Ctrl Pts',(0.395707992682752,-2.71813035961417,
7.50517746087247));
#405180=CARTESIAN_POINT('Ctrl Pts',(0.395450365812616,-2.71819997752052,
7.50491486231392));
#405181=CARTESIAN_POINT('Ctrl Pts',(0.395170003136838,-2.71826089837762,
7.50468370960992));
#405182=CARTESIAN_POINT('Ctrl Pts',(0.394750772501156,-2.71835199427537,
7.50433806340446));
#405183=CARTESIAN_POINT('Ctrl Pts',(0.394268015985544,-2.71842583148373,
7.50405484070983));
#405184=CARTESIAN_POINT('Ctrl Pts',(0.393754138031257,-2.71847672904422,
7.5038576603613));
#405185=CARTESIAN_POINT('Ctrl Pts',(0.39369918677152,-2.71848217174719,
7.50383657498791));
#405186=CARTESIAN_POINT('Ctrl Pts',(0.393643905362452,-2.71848736408184,
7.50381643264937));
#405187=CARTESIAN_POINT('Ctrl Pts',(0.393588351980726,-2.71849230807153,
7.50379723213559));
#405188=CARTESIAN_POINT('Ctrl Pts',(0.393217514984914,-2.71852531082003,
7.50366906242518));
#405189=CARTESIAN_POINT('Ctrl Pts',(0.392826428584466,-2.71854724898582,
7.50358235568538));
#405190=CARTESIAN_POINT('Ctrl Pts',(0.392448961127797,-2.71855933335556,
7.5035341175365));
#405191=CARTESIAN_POINT('Ctrl Pts',(0.391882991397589,-2.71857745250028,
7.50346178989176));
#405192=CARTESIAN_POINT('Ctrl Pts',(0.391273366354846,-2.71857288019814,
7.50346967198527));
#405193=CARTESIAN_POINT('Ctrl Pts',(0.390675041552701,-2.71854997689285,
7.50354272648692));
#405194=CARTESIAN_POINT('Ctrl Pts',(0.39042893817699,-2.71854055628932,
7.50357277531559));
#405195=CARTESIAN_POINT('Ctrl Pts',(0.390185068196105,-2.71852818857031,
7.50361331098761));
#405196=CARTESIAN_POINT('Ctrl Pts',(0.38994847349153,-2.71851378208147,
7.50366116523658));
#405197=CARTESIAN_POINT('',(0.341939261259106,-2.65201338678245,7.57603338622103));
#405198=CARTESIAN_POINT('Origin',(0.343066474116874,-2.66077813896213,7.58486873427628));
#405199=CARTESIAN_POINT('Ctrl Pts',(0.389948473529094,-2.71851378212322,
7.50366116529969));
#405200=CARTESIAN_POINT('Ctrl Pts',(0.373970838805498,-2.69638364458546,
7.52783573079709));
#405201=CARTESIAN_POINT('Ctrl Pts',(0.357968509118452,-2.67421790325148,
7.55196141284068));
#405202=CARTESIAN_POINT('Ctrl Pts',(0.341939262248866,-2.65201338754928,
7.57603338728831));
#405203=CARTESIAN_POINT('Ctrl Pts',(0.347594250863872,-2.64601386279728,
7.59639677331372));
#405204=CARTESIAN_POINT('Ctrl Pts',(0.339350823778441,-2.62970074459047,
7.59959882295463));
#405205=CARTESIAN_POINT('Ctrl Pts',(0.334988019337696,-2.64746798269907,
7.59642833564546));
#405206=CARTESIAN_POINT('Ctrl Pts',(0.346417486467366,-2.64229494768145,
7.58707626057424));
#405207=CARTESIAN_POINT('Ctrl Pts',(0.340385787866657,-2.63920773161741,
7.58809943920598));
#405208=CARTESIAN_POINT('Ctrl Pts',(0.335273897319247,-2.64363299723925,
7.58710240504252));
#405209=CARTESIAN_POINT('Ctrl Pts',(0.343548093433333,-2.6476514592214,
7.5801537675693));
#405210=CARTESIAN_POINT('Ctrl Pts',(0.341200555278531,-2.64603333190638,
7.5820588065976));
#405211=CARTESIAN_POINT('Ctrl Pts',(0.33933172203006,-2.64813916602317,
7.58020924244129));
#405212=CARTESIAN_POINT('Ctrl Pts',(0.341939261153479,-2.65201338596165,
7.57603338509286));
#405213=CARTESIAN_POINT('Ctrl Pts',(0.341939261153479,-2.65201338596165,
7.57603338509286));
#405214=CARTESIAN_POINT('Ctrl Pts',(0.341939261153479,-2.65201338596165,
7.57603338509286));
#405215=CARTESIAN_POINT('Origin',(0.343072133619864,-2.66077740925008,7.58486873427621));
#405216=CARTESIAN_POINT('Ctrl Pts',(0.30110264748337,-2.73436754560449,
7.51098857897448));
#405217=CARTESIAN_POINT('Ctrl Pts',(0.303232664881372,-2.72887905420375,
7.50433767179956));
#405218=CARTESIAN_POINT('Ctrl Pts',(0.311753059719557,-2.73010825023526,
7.50214974420965));
#405219=CARTESIAN_POINT('Ctrl Pts',(0.312499739379771,-2.70500025455533,
7.53887321589168));
#405220=CARTESIAN_POINT('Ctrl Pts',(0.314604235389235,-2.69957752502187,
7.5322040745206));
#405221=CARTESIAN_POINT('Ctrl Pts',(0.323103465221949,-2.70074629025612,
7.53003438070912));
#405222=CARTESIAN_POINT('Ctrl Pts',(0.323918717896826,-2.67557656747421,
7.5666946565923));
#405223=CARTESIAN_POINT('Ctrl Pts',(0.326010776726132,-2.67018588526411,
7.56004085833297));
#405224=CARTESIAN_POINT('Ctrl Pts',(0.334474294446332,-2.67132847789769,
7.55785582193789));
#405225=CARTESIAN_POINT('Ctrl Pts',(0.335359066599835,-2.64609781507675,
7.59443891967696));
#405226=CARTESIAN_POINT('Ctrl Pts',(0.33745415865399,-2.64069931704862,
7.58783901202978));
#405227=CARTESIAN_POINT('Ctrl Pts',(0.345864908691513,-2.64185623614459,
7.58560008491213));
#405228=CARTESIAN_POINT('',(0.312368326987746,-2.72851663429643,7.50366116523517));
#405229=CARTESIAN_POINT('Ctrl Pts',(0.312368326987789,-2.7285166342968,
7.50366116523554));
#405230=CARTESIAN_POINT('Ctrl Pts',(0.311648372775254,-2.7287528618325,
7.50350835821027));
#405231=CARTESIAN_POINT('Ctrl Pts',(0.310978874698756,-2.72894658931301,
7.50345484956));
#405232=CARTESIAN_POINT('Ctrl Pts',(0.310340094951329,-2.72910415325133,
7.50349758195598));
#405233=CARTESIAN_POINT('Ctrl Pts',(0.310012353567758,-2.72918499523693,
7.50351950684424));
#405234=CARTESIAN_POINT('Ctrl Pts',(0.309660426124625,-2.72926441113656,
7.50357029184312));
#405235=CARTESIAN_POINT('Ctrl Pts',(0.309318961508551,-2.72933166265592,
7.50365515313924));
#405236=CARTESIAN_POINT('Ctrl Pts',(0.308793650656355,-2.72943512272552,
7.50378570417639));
#405237=CARTESIAN_POINT('Ctrl Pts',(0.308277749172678,-2.72951317103045,
7.50400001621911));
#405238=CARTESIAN_POINT('Ctrl Pts',(0.307810185036332,-2.72955762209029,
7.50428903009634));
#405239=CARTESIAN_POINT('Ctrl Pts',(0.307758289014417,-2.72956255581594,
7.50432110841318));
#405240=CARTESIAN_POINT('Ctrl Pts',(0.307706965257224,-2.72956709514048,
7.50435406373354));
#405241=CARTESIAN_POINT('Ctrl Pts',(0.307656249660477,-2.72957124302653,
7.50438785222352));
#405242=CARTESIAN_POINT('Ctrl Pts',(0.307346606565338,-2.7295965678646,
7.50459414719561));
#405243=CARTESIAN_POINT('Ctrl Pts',(0.307054661928029,-2.72960719025543,
7.50483629897752));
#405244=CARTESIAN_POINT('Ctrl Pts',(0.306791647913694,-2.7296040184196,
7.5050991045531));
#405245=CARTESIAN_POINT('Ctrl Pts',(0.306211412580815,-2.72959702103118,
7.50567888004914));
#405246=CARTESIAN_POINT('Ctrl Pts',(0.305749108231759,-2.72952313331425,
7.50637912803145));
#405247=CARTESIAN_POINT('Ctrl Pts',(0.305392057397997,-2.72941054569535,
7.50710440483569));
#405248=CARTESIAN_POINT('Ctrl Pts',(0.305304501445106,-2.72938293697602,
7.50728225710686));
#405249=CARTESIAN_POINT('Ctrl Pts',(0.305221487814431,-2.7293525907114,
7.50746498566955));
#405250=CARTESIAN_POINT('Ctrl Pts',(0.305144811281211,-2.72932060655107,
7.50764697238949));
#405251=CARTESIAN_POINT('Ctrl Pts',(0.304732619340569,-2.72914866850742,
7.50862528291182));
#405252=CARTESIAN_POINT('Ctrl Pts',(0.304464548239098,-2.72891760973833,
7.50965856837422));
#405253=CARTESIAN_POINT('Ctrl Pts',(0.304285411258914,-2.72866417016778,
7.51067959873203));
#405254=CARTESIAN_POINT('Ctrl Pts',(0.304186831952766,-2.72852470205243,
7.51124147302579));
#405255=CARTESIAN_POINT('Ctrl Pts',(0.304115515380115,-2.728378171551,7.51180065547253));
#405256=CARTESIAN_POINT('Ctrl Pts',(0.304064538403005,-2.72822921565349,
7.51235175716501));
#405257=CARTESIAN_POINT('Ctrl Pts',(0.303888392640273,-2.72771451369063,
7.51425603304536));
#405258=CARTESIAN_POINT('Ctrl Pts',(0.303939832870269,-2.72710752083202,
7.51626900505181));
#405259=CARTESIAN_POINT('Ctrl Pts',(0.304176391156363,-2.72645112229369,
7.51827788969245));
#405260=CARTESIAN_POINT('Ctrl Pts',(0.304189194137839,-2.72641559676438,
7.51838661432546));
#405261=CARTESIAN_POINT('Ctrl Pts',(0.304202548093838,-2.72637992171949,
7.51849533314857));
#405262=CARTESIAN_POINT('Ctrl Pts',(0.304216449096315,-2.72634410251322,
7.51860402984325));
#405263=CARTESIAN_POINT('Ctrl Pts',(0.341939260496137,-2.65201338777647,
7.57603338728985));
#405264=CARTESIAN_POINT('Ctrl Pts',(0.332066529529991,-2.67755759370233,
7.55196141284922));
#405265=CARTESIAN_POINT('Ctrl Pts',(0.322210000114193,-2.70305746572958,
7.52783573083105));
#405266=CARTESIAN_POINT('Ctrl Pts',(0.312368326961429,-2.72851663434944,
7.50366116530176));
#405267=CARTESIAN_POINT('Origin',(1.1815582111521E-16,-9.16393216063562E-16,
7.49482233047033));
#405268=CARTESIAN_POINT('Origin',(0.388693460788468,-2.70976449964573,7.49482233047033));
#405269=CARTESIAN_POINT('Origin',(0.,0.,7.50366116523517));
#405270=CARTESIAN_POINT('Origin',(0.311362998732885,-2.71973515861748,7.49482233047033));
#405271=CARTESIAN_POINT('Ctrl Pts',(0.397282050205201,-2.71434368527686,
7.51860402984325));
#405272=CARTESIAN_POINT('Ctrl Pts',(0.401743698216877,-2.72050728674434,
7.51860402984325));
#405273=CARTESIAN_POINT('Ctrl Pts',(0.409267922647788,-2.71937488542709,
7.51860402984325));
#405274=CARTESIAN_POINT('Ctrl Pts',(0.398938691589159,-2.71663227181923,
7.51041458714364));
#405275=CARTESIAN_POINT('Ctrl Pts',(0.403526271692425,-2.72023899811274,
7.5100464290044));
#405276=CARTESIAN_POINT('Ctrl Pts',(0.409269997739552,-2.71937457312425,
7.50729136483009));
#405277=CARTESIAN_POINT('Ctrl Pts',(0.397367849688418,-2.71896812132682,
7.50215815450138));
#405278=CARTESIAN_POINT('Ctrl Pts',(0.399896795118431,-2.72078539937199,
7.49877163671532));
#405279=CARTESIAN_POINT('Ctrl Pts',(0.403312047312363,-2.72029552587179,
7.49481588533172));
#405280=CARTESIAN_POINT('Ctrl Pts',(0.389948395323643,-2.71851323713979,
7.50366171572173));
#405281=CARTESIAN_POINT('Ctrl Pts',(0.390468316773421,-2.72213785352545,
7.50000045605858));
#405282=CARTESIAN_POINT('Ctrl Pts',(0.390468316773545,-2.72213785352543,
7.49482233047317));
#405283=CARTESIAN_POINT('Origin',(0.40740761390848,-2.70701409049333,7.51860402984325));
#405284=CARTESIAN_POINT('Origin',(0.40740761390848,-2.70701409049333,9.));
#405285=CARTESIAN_POINT('Origin',(0.40740761390848,-2.70701409049333,8.75721825406948));
#405286=CARTESIAN_POINT('Ctrl Pts',(0.387489117162883,-2.70081746938362,
8.78942910404912));
#405287=CARTESIAN_POINT('Ctrl Pts',(0.390740624933991,-2.70534296669508,
8.79672699501691));
#405288=CARTESIAN_POINT('Ctrl Pts',(0.398822743738664,-2.70155445226206,
8.79893251111267));
#405289=CARTESIAN_POINT('Ctrl Pts',(0.393936589149048,-2.70972283426823,
8.78111911759584));
#405290=CARTESIAN_POINT('Ctrl Pts',(0.39779733455391,-2.7150835203292,8.78644465894813));
#405291=CARTESIAN_POINT('Ctrl Pts',(0.40570455888801,-2.7132970950983,8.78817647674132));
#405292=CARTESIAN_POINT('Ctrl Pts',(0.397954807503326,-2.71527287005866,
8.76780923932029));
#405293=CARTESIAN_POINT('Ctrl Pts',(0.402516389461998,-2.72159795557623,
8.76988516158375));
#405294=CARTESIAN_POINT('Ctrl Pts',(0.410012461604671,-2.72062569901123,
8.77093053738833));
#405295=CARTESIAN_POINT('Ctrl Pts',(0.397171309918828,-2.71419068903609,
8.75371302330492));
#405296=CARTESIAN_POINT('Ctrl Pts',(0.401620318062267,-2.72036098302482,
8.75300828287558));
#405297=CARTESIAN_POINT('Ctrl Pts',(0.409172640064114,-2.71919609173606,
8.75267964240738));
#405298=CARTESIAN_POINT('Origin',(0.399184265771865,-2.69565586321038,8.78727029226991));
#405299=CARTESIAN_POINT('Ctrl Pts',(0.347133565397108,-2.64507775146798,
8.85049129520029));
#405300=CARTESIAN_POINT('Ctrl Pts',(0.350558127032912,-2.649807813817,8.85711686593484));
#405301=CARTESIAN_POINT('Ctrl Pts',(0.358444815903146,-2.64650616259708,
8.85933012996512));
#405302=CARTESIAN_POINT('Ctrl Pts',(0.361129150869197,-2.66440869041267,
8.82945683644721));
#405303=CARTESIAN_POINT('Ctrl Pts',(0.364582138437126,-2.66917801513903,
8.83607469902387));
#405304=CARTESIAN_POINT('Ctrl Pts',(0.372477500384207,-2.66583207697137,
8.8382956714852));
#405305=CARTESIAN_POINT('Ctrl Pts',(0.375103874792548,-2.68371081503404,
8.80838214965002));
#405306=CARTESIAN_POINT('Ctrl Pts',(0.378570489461554,-2.68849896174253,
8.81501364461987));
#405307=CARTESIAN_POINT('Ctrl Pts',(0.38648835703971,-2.68512906773677,
8.81722098428721));
#405308=CARTESIAN_POINT('Ctrl Pts',(0.389059322317711,-2.70298631476879,
8.78727029226991));
#405309=CARTESIAN_POINT('Ctrl Pts',(0.39252651280282,-2.70777525680419,
8.79393457792714));
#405310=CARTESIAN_POINT('Ctrl Pts',(0.400479038758368,-2.70439935009568,
8.79610912703474));
#405311=CARTESIAN_POINT('Origin',(0.357258508851261,-2.63774729990957,8.85049129520029));
#405312=CARTESIAN_POINT('Ctrl Pts',(0.335155581859898,-2.64662214142562,
8.85049129520029));
#405313=CARTESIAN_POINT('Ctrl Pts',(0.333042822978433,-2.65206616219449,
8.85711686593484));
#405314=CARTESIAN_POINT('Ctrl Pts',(0.324576590381463,-2.65087298671371,
8.85933012996512));
#405315=CARTESIAN_POINT('Ctrl Pts',(0.337024709144332,-2.64180589483668,
8.86332496987231));
#405316=CARTESIAN_POINT('Ctrl Pts',(0.332486490925516,-2.64267564754589,
8.86648636486738));
#405317=CARTESIAN_POINT('Ctrl Pts',(0.329821522197239,-2.6374055390489,
8.87206031107457));
#405318=CARTESIAN_POINT('Ctrl Pts',(0.344083317655487,-2.64086469778922,
8.86341338519877));
#405319=CARTESIAN_POINT('Ctrl Pts',(0.348704757116161,-2.64052445089995,
8.86654584966058));
#405320=CARTESIAN_POINT('Ctrl Pts',(0.349892026593758,-2.63471802825129,
8.87215952290715));
#405321=CARTESIAN_POINT('Ctrl Pts',(0.347133565397107,-2.64507775146798,
8.85049129520029));
#405322=CARTESIAN_POINT('Ctrl Pts',(0.350558127032912,-2.649807813817,8.85711686593484));
#405323=CARTESIAN_POINT('Ctrl Pts',(0.358444815903146,-2.64650616259708,
8.85933012996512));
#405324=CARTESIAN_POINT('Origin',(0.323502373428218,-2.64209967160839,8.85049129520029));
#405325=CARTESIAN_POINT('Ctrl Pts',(0.309289785090442,-2.71327145765926,
8.78727029226991));
#405326=CARTESIAN_POINT('Ctrl Pts',(0.307150726644374,-2.71878324544932,
8.79393457792714));
#405327=CARTESIAN_POINT('Ctrl Pts',(0.298601974927924,-2.71753494289437,
8.79610912703474));
#405328=CARTESIAN_POINT('Ctrl Pts',(0.317899498928076,-2.69108650254806,
8.80838214965002));
#405329=CARTESIAN_POINT('Ctrl Pts',(0.315760795727631,-2.6965973749641,
8.81501364461987));
#405330=CARTESIAN_POINT('Ctrl Pts',(0.307247094031223,-2.69534609720932,
8.81722098428721));
#405331=CARTESIAN_POINT('Ctrl Pts',(0.326521105202121,-2.66887090377404,
8.82945683644721));
#405332=CARTESIAN_POINT('Ctrl Pts',(0.324390809144546,-2.67436011320681,
8.83607469902389));
#405333=CARTESIAN_POINT('Ctrl Pts',(0.315904953537574,-2.67312629915468,
8.83829567148519));
#405334=CARTESIAN_POINT('Ctrl Pts',(0.335155581859898,-2.64662214142562,
8.85049129520029));
#405335=CARTESIAN_POINT('Ctrl Pts',(0.333042822978433,-2.65206616219449,
8.85711686593484));
#405336=CARTESIAN_POINT('Ctrl Pts',(0.324576590381463,-2.65087298671371,
8.85933012996512));
#405337=CARTESIAN_POINT('Origin',(0.297636576658761,-2.70874898784202,8.78727029226991));
#405338=CARTESIAN_POINT('Ctrl Pts',(0.304283422748619,-2.72617147813989,
8.75374538247849));
#405339=CARTESIAN_POINT('Ctrl Pts',(0.301546370683848,-2.7332604078463,
8.75304829418602));
#405340=CARTESIAN_POINT('Ctrl Pts',(0.293954221614916,-2.73405408014901,
8.75272238421917));
#405341=CARTESIAN_POINT('Ctrl Pts',(0.303805856238317,-2.72740204188969,
8.76769408445017));
#405342=CARTESIAN_POINT('Ctrl Pts',(0.300999284012165,-2.73466911195342,
8.76974318093968));
#405343=CARTESIAN_POINT('Ctrl Pts',(0.293509920856674,-2.73563233404902,
8.77077869880429));
#405344=CARTESIAN_POINT('Ctrl Pts',(0.306253590132223,-2.7210948731195,
8.78108014887993));
#405345=CARTESIAN_POINT('Ctrl Pts',(0.303878665533224,-2.72725482201941,
8.78639403366325));
#405346=CARTESIAN_POINT('Ctrl Pts',(0.295789548083311,-2.72755189879461,
8.78812224174741));
#405347=CARTESIAN_POINT('Ctrl Pts',(0.310264885608781,-2.71075881581417,
8.78944554828685));
#405348=CARTESIAN_POINT('Ctrl Pts',(0.308268610199825,-2.71595220604682,
8.79673892988686));
#405349=CARTESIAN_POINT('Ctrl Pts',(0.299498741631349,-2.71434193910989,
8.79894799272499));
#405350=CARTESIAN_POINT('Origin',(0.292563240664638,-2.72182163269598,8.75721825406948));
#405351=CARTESIAN_POINT('Origin',(0.292563240664638,-2.72182163269598,9.));
#405352=CARTESIAN_POINT('Origin',(0.292563240664638,-2.72182163269598,7.51860402984325));
#405353=CARTESIAN_POINT('Ctrl Pts',(0.312368237512627,-2.72851585273769,
7.50366195182966));
#405354=CARTESIAN_POINT('Ctrl Pts',(0.312784747585408,-2.73215404062032,
7.50000065167735));
#405355=CARTESIAN_POINT('Ctrl Pts',(0.312784747585292,-2.73215404062033,
7.49482233047108));
#405356=CARTESIAN_POINT('Ctrl Pts',(0.305300246324107,-2.73083906176094,
7.50215800491337));
#405357=CARTESIAN_POINT('Ctrl Pts',(0.303313249275647,-2.73323834079926,
7.49877273257269));
#405358=CARTESIAN_POINT('Ctrl Pts',(0.299883530860017,-2.73363100852074,
7.49481816995647));
#405359=CARTESIAN_POINT('Ctrl Pts',(0.30319700787747,-2.7289718701857,7.51043025814043));
#405360=CARTESIAN_POINT('Ctrl Pts',(0.299675308765078,-2.73362916471673,
7.51006209594513));
#405361=CARTESIAN_POINT('Ctrl Pts',(0.293896628507995,-2.73425031256432,
7.50731281821701));
#405362=CARTESIAN_POINT('Ctrl Pts',(0.304216995834693,-2.72634269346048,
7.51860402984326));
#405363=CARTESIAN_POINT('Ctrl Pts',(0.301464837418653,-2.7334368207108,
7.51860402984327));
#405364=CARTESIAN_POINT('Ctrl Pts',(0.293899145873147,-2.7342500419777,
7.51860402984327));
#405365=CARTESIAN_POINT('Origin',(0.,0.,7.5));
#405366=CARTESIAN_POINT('Origin',(0.50403663157861,-2.6197108805292,7.5));
#405367=CARTESIAN_POINT('',(0.50403663157861,-2.6197108805292,7.59394543036555));
#405368=CARTESIAN_POINT('',(0.50403663157861,-2.6197108805292,8.85049129520029));
#405369=CARTESIAN_POINT('',(0.50403663157861,-2.6197108805292,7.5));
#405370=CARTESIAN_POINT('',(0.482494215215367,-2.68788048588351,8.78727029226991));
#405371=CARTESIAN_POINT('Ctrl Pts',(0.50403663157861,-2.6197108805292,8.85049129520029));
#405372=CARTESIAN_POINT('Ctrl Pts',(0.496845388128044,-2.64246711268839,
8.82945686509571));
#405373=CARTESIAN_POINT('Ctrl Pts',(0.489664835330419,-2.66518951495683,
8.80838212259896));
#405374=CARTESIAN_POINT('Ctrl Pts',(0.482494215215367,-2.68788048588351,
8.78727029226991));
#405375=CARTESIAN_POINT('',(0.47826887016568,-2.70125132133976,8.75721825406948));
#405376=CARTESIAN_POINT('Origin',(0.490984591624991,-2.66101389988662,8.75937679713189));
#405377=CARTESIAN_POINT('',(0.47826887016568,-2.70125132133976,7.51860402984325));
#405378=CARTESIAN_POINT('',(0.47826887016568,-2.70125132133976,7.5));
#405379=CARTESIAN_POINT('Ctrl Pts',(0.47826887016568,-2.70125132133976,
7.51860402984325));
#405380=CARTESIAN_POINT('Ctrl Pts',(0.481587221536751,-2.69075060964714,
7.52834476460825));
#405381=CARTESIAN_POINT('Ctrl Pts',(0.484907727133655,-2.68024308104402,
7.53807742314407));
#405382=CARTESIAN_POINT('Ctrl Pts',(0.48823045928738,-2.66972850664355,
7.54780169004674));
#405383=CARTESIAN_POINT('Ctrl Pts',(0.49349348744053,-2.65307398905745,
7.5632044032688));
#405384=CARTESIAN_POINT('Ctrl Pts',(0.498762108429687,-2.63640177329775,
7.57858609112103));
#405385=CARTESIAN_POINT('Ctrl Pts',(0.50403663157861,-2.6197108805292,7.59394543036555));
#405386=CARTESIAN_POINT('Origin',(0.691101205365358,-2.82936072626276,7.5));
#405387=CARTESIAN_POINT('',(0.570375062512147,-2.68331364198702,8.75721825406948));
#405388=CARTESIAN_POINT('',(0.561440886005621,-2.67250562312428,8.78727029226991));
#405389=CARTESIAN_POINT('Origin',(0.538762613749665,-2.64507084005976,8.7565864062101));
#405390=CARTESIAN_POINT('',(0.515891055659684,-2.6174022316462,8.85049129520029));
#405391=CARTESIAN_POINT('Ctrl Pts',(0.561440886005621,-2.67250562312428,
8.78727029226991));
#405392=CARTESIAN_POINT('Ctrl Pts',(0.546279145362962,-2.6541638790656,
8.80838212259897));
#405393=CARTESIAN_POINT('Ctrl Pts',(0.531096402804887,-2.63579672817756,
8.82945686509571));
#405394=CARTESIAN_POINT('Ctrl Pts',(0.515891055659685,-2.6174022316462,
8.85049129520029));
#405395=CARTESIAN_POINT('',(0.515891055659684,-2.6174022316462,7.59394543036555));
#405396=CARTESIAN_POINT('',(0.515891055659684,-2.6174022316462,7.5));
#405397=CARTESIAN_POINT('',(0.570375062512147,-2.68331364198702,7.51860402984325));
#405398=CARTESIAN_POINT('Ctrl Pts',(0.515891055659684,-2.6174022316462,
7.59394543036555));
#405399=CARTESIAN_POINT('Ctrl Pts',(0.527043640891444,-2.63089394534417,
7.57858609112103));
#405400=CARTESIAN_POINT('Ctrl Pts',(0.538183746447113,-2.64437056189532,
7.56320440326857));
#405401=CARTESIAN_POINT('Ctrl Pts',(0.549312026368894,-2.65783287251976,
7.54780169004651));
#405402=CARTESIAN_POINT('Ctrl Pts',(0.556337695325203,-2.66633209598457,
7.53807742314383));
#405403=CARTESIAN_POINT('Ctrl Pts',(0.563358656393546,-2.67482562413523,
7.52834476460825));
#405404=CARTESIAN_POINT('Ctrl Pts',(0.570375062512147,-2.68331364198702,
7.51860402984325));
#405405=CARTESIAN_POINT('',(0.570375062512147,-2.68331364198702,7.5));
#405406=CARTESIAN_POINT('Origin',(0.510592093294271,-2.62178248538885,7.5));
#405407=CARTESIAN_POINT('Ctrl Pts',(0.515891055659684,-2.6174022316462,
8.85049129520029));
#405408=CARTESIAN_POINT('Ctrl Pts',(0.515767668527162,-2.61725296545981,
8.85097269580138));
#405409=CARTESIAN_POINT('Ctrl Pts',(0.515639354986848,-2.61711094168747,
8.85143669361005));
#405410=CARTESIAN_POINT('Ctrl Pts',(0.515499557882546,-2.61697020670063,
8.8519052845931));
#405411=CARTESIAN_POINT('Ctrl Pts',(0.515226123612142,-2.61669493799147,
8.85282181883899));
#405412=CARTESIAN_POINT('Ctrl Pts',(0.514915651119206,-2.61643181964957,
8.85372622499636));
#405413=CARTESIAN_POINT('Ctrl Pts',(0.514553299874856,-2.6161884856712,
8.85462257735071));
#405414=CARTESIAN_POINT('Ctrl Pts',(0.514252488741296,-2.61598647844477,
8.85536669723986));
#405415=CARTESIAN_POINT('Ctrl Pts',(0.513915873198261,-2.61579803376955,
8.85610498449051));
#405416=CARTESIAN_POINT('Ctrl Pts',(0.513531024768008,-2.61563448612491,
8.85681338218371));
#405417=CARTESIAN_POINT('Ctrl Pts',(0.513181774213136,-2.61548606638055,
8.85745625420285));
#405418=CARTESIAN_POINT('Ctrl Pts',(0.512788654114686,-2.61535573822306,
8.85808743050666));
#405419=CARTESIAN_POINT('Ctrl Pts',(0.512331828562537,-2.61526410220628,
8.85866804508411));
#405420=CARTESIAN_POINT('Ctrl Pts',(0.51212105915554,-2.61522182333456,
8.85893592806396));
#405421=CARTESIAN_POINT('Ctrl Pts',(0.511896582696664,-2.61518797425763,
8.85919241173849));
#405422=CARTESIAN_POINT('Ctrl Pts',(0.511655676326057,-2.61516597374877,
8.85943017985535));
#405423=CARTESIAN_POINT('Ctrl Pts',(0.511330381409818,-2.61513626654896,
8.85975123720001));
#405424=CARTESIAN_POINT('Ctrl Pts',(0.510966791987504,-2.61512804460748,
8.86004599534705));
#405425=CARTESIAN_POINT('Ctrl Pts',(0.510569040990318,-2.61515181913894,
8.86026130871721));
#405426=CARTESIAN_POINT('Ctrl Pts',(0.51042341313646,-2.61516052366518,
8.86034014101235));
#405427=CARTESIAN_POINT('Ctrl Pts',(0.510271017703931,-2.61517363576241,
8.86040910639693));
#405428=CARTESIAN_POINT('Ctrl Pts',(0.51011603545622,-2.61519113333937,
8.86046313645507));
#405429=CARTESIAN_POINT('Ctrl Pts',(0.509874186956632,-2.61521843816168,
8.8605474499083));
#405430=CARTESIAN_POINT('Ctrl Pts',(0.509619453975313,-2.61525731366694,
8.86059655985669));
#405431=CARTESIAN_POINT('Ctrl Pts',(0.509368129116552,-2.61530497704635,
8.86059725258816));
#405432=CARTESIAN_POINT('Ctrl Pts',(0.509116223596962,-2.61535275054721,
8.86059794692011));
#405433=CARTESIAN_POINT('Ctrl Pts',(0.508865443335394,-2.61541249263373,
8.86056369958366));
#405434=CARTESIAN_POINT('Ctrl Pts',(0.508628593949213,-2.61547728428474,
8.86048590497774));
#405435=CARTESIAN_POINT('Ctrl Pts',(0.508566783311275,-2.61549419297657,
8.86046560290182));
#405436=CARTESIAN_POINT('Ctrl Pts',(0.508505141221167,-2.61551175291262,
8.86044257503091));
#405437=CARTESIAN_POINT('Ctrl Pts',(0.508445563477128,-2.61552938990612,
8.86041778462583));
#405438=CARTESIAN_POINT('Ctrl Pts',(0.508044679189558,-2.61564806498672,
8.86025097596201));
#405439=CARTESIAN_POINT('Ctrl Pts',(0.507683561495995,-2.6157864717915,
8.8599848982295));
#405440=CARTESIAN_POINT('Ctrl Pts',(0.507369718277706,-2.61593265927751,
8.85968173251461));
#405441=CARTESIAN_POINT('Ctrl Pts',(0.507203713196304,-2.61600998408206,
8.85952137522076));
#405442=CARTESIAN_POINT('Ctrl Pts',(0.507047654086883,-2.61609080315806,
8.85934740853961));
#405443=CARTESIAN_POINT('Ctrl Pts',(0.506903026841193,-2.61617259635408,
8.8591675900182));
#405444=CARTESIAN_POINT('Ctrl Pts',(0.506322273274009,-2.61650103855136,
8.85844552518696));
#405445=CARTESIAN_POINT('Ctrl Pts',(0.50589153921837,-2.61686111677501,
8.85759444184127));
#405446=CARTESIAN_POINT('Ctrl Pts',(0.505566712158174,-2.61718625003458,
8.85683498915142));
#405447=CARTESIAN_POINT('Ctrl Pts',(0.505532719871405,-2.61722027436429,
8.85675551445));
#405448=CARTESIAN_POINT('Ctrl Pts',(0.505499903995364,-2.61725392708393,
8.85667699793652));
#405449=CARTESIAN_POINT('Ctrl Pts',(0.505468225267565,-2.61728713860215,
8.85659965593547));
#405450=CARTESIAN_POINT('Ctrl Pts',(0.505040624183298,-2.61773542936974,
8.85555568965886));
#405451=CARTESIAN_POINT('Ctrl Pts',(0.504694415106465,-2.61822801862891,
8.85434650606346));
#405452=CARTESIAN_POINT('Ctrl Pts',(0.504422802045048,-2.61876376787636,
8.85297329937117));
#405453=CARTESIAN_POINT('Ctrl Pts',(0.504270036247629,-2.61906509418437,
8.85220095427747));
#405454=CARTESIAN_POINT('Ctrl Pts',(0.504141086615989,-2.61938033921223,
8.85137579139183));
#405455=CARTESIAN_POINT('Ctrl Pts',(0.50403663157861,-2.6197108805292,8.85049129520029));
#405456=CARTESIAN_POINT('Origin',(0.510592093294271,-2.62178248538885,7.59394543036555));
#405457=CARTESIAN_POINT('Ctrl Pts',(0.515532821189714,-2.61696886155262,
7.59443877723642));
#405458=CARTESIAN_POINT('Ctrl Pts',(0.511843350832983,-2.61250556656624,
7.58783886950016));
#405459=CARTESIAN_POINT('Ctrl Pts',(0.504225634743635,-2.61625384391973,
7.58559994247159));
#405460=CARTESIAN_POINT('Ctrl Pts',(0.53567353162265,-2.64133385793579,
7.56670252222136));
#405461=CARTESIAN_POINT('Ctrl Pts',(0.531989393598045,-2.63687701367782,
7.56004874999028));
#405462=CARTESIAN_POINT('Ctrl Pts',(0.524317107068316,-2.64062833033498,
7.55786368756704));
#405463=CARTESIAN_POINT('Ctrl Pts',(0.555776631291165,-2.66565335512258,
7.53888913333559));
#405464=CARTESIAN_POINT('Ctrl Pts',(0.55207059825391,-2.66117002362098,
7.5322200213728));
#405465=CARTESIAN_POINT('Ctrl Pts',(0.544372672437995,-2.66495742152093,
7.53005029815327));
#405466=CARTESIAN_POINT('Ctrl Pts',(0.57584121051637,-2.68992625263927,
7.51101258149734));
#405467=CARTESIAN_POINT('Ctrl Pts',(0.572090253624662,-2.68538857501344,
7.5043616886572));
#405468=CARTESIAN_POINT('Ctrl Pts',(0.564391276187505,-2.68923996800388,
7.50217374673251));
#405469=CARTESIAN_POINT('',(0.563323058569168,-2.68794421947736,7.50366116523517));
#405470=CARTESIAN_POINT('Ctrl Pts',(0.570375062512147,-2.68331364198702,
7.51860402984325));
#405471=CARTESIAN_POINT('Ctrl Pts',(0.570656425301981,-2.68365401743601,
7.51734760759494));
#405472=CARTESIAN_POINT('Ctrl Pts',(0.570864819165499,-2.68399950239606,
7.51608817408573));
#405473=CARTESIAN_POINT('Ctrl Pts',(0.570988330268538,-2.6843561994528,
7.5148100591312));
#405474=CARTESIAN_POINT('Ctrl Pts',(0.571100209577064,-2.68467930417034,
7.51365231206384));
#405475=CARTESIAN_POINT('Ctrl Pts',(0.571142835244544,-2.68501198219009,
7.51247773061043));
#405476=CARTESIAN_POINT('Ctrl Pts',(0.571078844074313,-2.68535316978938,
7.51129758471022));
#405477=CARTESIAN_POINT('Ctrl Pts',(0.570999310357784,-2.68577722701019,
7.50983079813402));
#405478=CARTESIAN_POINT('Ctrl Pts',(0.570744815553309,-2.6861984949357,
7.50839324291155));
#405479=CARTESIAN_POINT('Ctrl Pts',(0.570242939355973,-2.6865774199326,
7.50715379678855));
#405480=CARTESIAN_POINT('Ctrl Pts',(0.57001108701402,-2.68675247236271,
7.50658120839351));
#405481=CARTESIAN_POINT('Ctrl Pts',(0.569687753921555,-2.68693579028516,
7.50598221009429));
#405482=CARTESIAN_POINT('Ctrl Pts',(0.569269416203884,-2.68710322355639,
7.50545747549611));
#405483=CARTESIAN_POINT('Ctrl Pts',(0.569046178248972,-2.68719257113246,
7.50517746087247));
#405484=CARTESIAN_POINT('Ctrl Pts',(0.568793541135446,-2.68727855221161,
7.50491486231392));
#405485=CARTESIAN_POINT('Ctrl Pts',(0.568517657707569,-2.68735731079858,
7.50468370960992));
#405486=CARTESIAN_POINT('Ctrl Pts',(0.568105124960397,-2.68747507972909,
7.50433806340446));
#405487=CARTESIAN_POINT('Ctrl Pts',(0.567628091086002,-2.68757969554714,
7.50405484070983));
#405488=CARTESIAN_POINT('Ctrl Pts',(0.567118529966979,-2.68766341280671,
7.5038576603613));
#405489=CARTESIAN_POINT('Ctrl Pts',(0.567064040325677,-2.68767236506636,
7.50383657498791));
#405490=CARTESIAN_POINT('Ctrl Pts',(0.567009205172219,-2.68768108862484,
7.50381643264937));
#405491=CARTESIAN_POINT('Ctrl Pts',(0.566954082693383,-2.68768958177396,
7.50379723213559));
#405492=CARTESIAN_POINT('Ctrl Pts',(0.566586122115307,-2.68774627632267,
7.50366906242519));
#405493=CARTESIAN_POINT('Ctrl Pts',(0.566197244826921,-2.68779322640586,
7.50358235568538));
#405494=CARTESIAN_POINT('Ctrl Pts',(0.565821327165852,-2.68782947036994,
7.5035341175365));
#405495=CARTESIAN_POINT('Ctrl Pts',(0.565257681178744,-2.68788381409206,
7.50346178989176));
#405496=CARTESIAN_POINT('Ctrl Pts',(0.564649015727631,-2.6879183099948,
7.50346967198527));
#405497=CARTESIAN_POINT('Ctrl Pts',(0.564050452828154,-2.6879337885485,
7.50354272648692));
#405498=CARTESIAN_POINT('Ctrl Pts',(0.563804251518082,-2.68794015519803,
7.50357277531559));
#405499=CARTESIAN_POINT('Ctrl Pts',(0.563560090191749,-2.68794343769315,
7.50361331098761));
#405500=CARTESIAN_POINT('Ctrl Pts',(0.563323058569459,-2.68794421947875,
7.50366116523658));
#405501=CARTESIAN_POINT('',(0.511151791456924,-2.62465641716285,7.57603338622103));
#405502=CARTESIAN_POINT('Origin',(0.512838247935187,-2.63333094044392,7.58486873427629));
#405503=CARTESIAN_POINT('Ctrl Pts',(0.563323058609621,-2.687944219518,7.50366116529969));
#405504=CARTESIAN_POINT('Ctrl Pts',(0.545960368869929,-2.66688324129277,
7.5278357307971));
#405505=CARTESIAN_POINT('Ctrl Pts',(0.528570753762145,-2.6457883146349,
7.55196141284068));
#405506=CARTESIAN_POINT('Ctrl Pts',(0.511151792493781,-2.62465641786469,
7.57603338728831));
#405507=CARTESIAN_POINT('Ctrl Pts',(0.51641077145758,-2.61830690341525,
7.5963967733137));
#405508=CARTESIAN_POINT('Ctrl Pts',(0.50713909630514,-2.60255546044574,
7.59959882295468));
#405509=CARTESIAN_POINT('Ctrl Pts',(0.503923606568037,-2.6205657196987,
7.59642833564546));
#405510=CARTESIAN_POINT('Ctrl Pts',(0.514998153140218,-2.61467102476309,
7.58707626057421));
#405511=CARTESIAN_POINT('Ctrl Pts',(0.508781048698791,-2.61197660397169,
7.58809943920599));
#405512=CARTESIAN_POINT('Ctrl Pts',(0.503963188820591,-2.61672029736263,
7.58710240504252));
#405513=CARTESIAN_POINT('Ctrl Pts',(0.5124778484545,-2.62020037341848,7.58015376756929));
#405514=CARTESIAN_POINT('Ctrl Pts',(0.510031459795584,-2.61873597800556,
7.58205880659761));
#405515=CARTESIAN_POINT('Ctrl Pts',(0.508301387520527,-2.62095722201766,
7.58020924244127));
#405516=CARTESIAN_POINT('Ctrl Pts',(0.511151791298927,-2.6246564163505,
7.57603338509286));
#405517=CARTESIAN_POINT('Ctrl Pts',(0.511151791298927,-2.6246564163505,
7.57603338509286));
#405518=CARTESIAN_POINT('Ctrl Pts',(0.511151791298927,-2.6246564163505,
7.57603338509286));
#405519=CARTESIAN_POINT('Origin',(0.512843849057621,-2.63332984962562,7.58486873427619));
#405520=CARTESIAN_POINT('Ctrl Pts',(0.47567552995596,-2.70945778136101,
7.51098857897448));
#405521=CARTESIAN_POINT('Ctrl Pts',(0.477449522153366,-2.70384409597124,
7.50433767179956));
#405522=CARTESIAN_POINT('Ctrl Pts',(0.486031165786685,-2.70452486291606,
7.50214974420965));
#405523=CARTESIAN_POINT('Ctrl Pts',(0.485167636506963,-2.67942061437602,
7.53887321589169));
#405524=CARTESIAN_POINT('Ctrl Pts',(0.486920373129621,-2.6738741908997,
7.53220407452062));
#405525=CARTESIAN_POINT('Ctrl Pts',(0.49547702342873,-2.67449600725536,
7.53003438070911));
#405526=CARTESIAN_POINT('Ctrl Pts',(0.494677971404042,-2.64932576495015,
7.56669465659233));
#405527=CARTESIAN_POINT('Ctrl Pts',(0.496420349679055,-2.64381211980541,
7.560040858333));
#405528=CARTESIAN_POINT('Ctrl Pts',(0.504939684355766,-2.6444101054177,
7.55785582193789));
#405529=CARTESIAN_POINT('Ctrl Pts',(0.504206104532811,-2.619174594153,7.59443891967696));
#405530=CARTESIAN_POINT('Ctrl Pts',(0.505951009039414,-2.61365295490927,
7.58783901202978));
#405531=CARTESIAN_POINT('Ctrl Pts',(0.514418602349914,-2.61426861838576,
7.58560008491213));
#405532=CARTESIAN_POINT('',(0.48654319373896,-2.70289709681367,7.50366116523517));
#405533=CARTESIAN_POINT('Ctrl Pts',(0.486543193739026,-2.70289709681404,
7.50366116523554));
#405534=CARTESIAN_POINT('Ctrl Pts',(0.485839853899813,-2.70317896661969,
7.50350835821027));
#405535=CARTESIAN_POINT('Ctrl Pts',(0.48518414354121,-2.70341519095536,
7.50345484956));
#405536=CARTESIAN_POINT('Ctrl Pts',(0.484556771391471,-2.70361335792061,
7.50349758195598));
#405537=CARTESIAN_POINT('Ctrl Pts',(0.484234882951524,-2.70371503227022,
7.50351950684424));
#405538=CARTESIAN_POINT('Ctrl Pts',(0.483888766775226,-2.70381683307007,
7.50357029184312));
#405539=CARTESIAN_POINT('Ctrl Pts',(0.483552312554467,-2.70390582412703,
7.50365515313923));
#405540=CARTESIAN_POINT('Ctrl Pts',(0.483034709719171,-2.70404272840868,
7.50378570417639));
#405541=CARTESIAN_POINT('Ctrl Pts',(0.482524868782483,-2.70415367027655,
7.50400001621911));
#405542=CARTESIAN_POINT('Ctrl Pts',(0.48206111329598,-2.70422798694398,
7.50428903009634));
#405543=CARTESIAN_POINT('Ctrl Pts',(0.4820096400049,-2.70423623552231,7.50432110841318));
#405544=CARTESIAN_POINT('Ctrl Pts',(0.481958712533397,-2.70424405384473,
7.50435406373354));
#405545=CARTESIAN_POINT('Ctrl Pts',(0.481908366893258,-2.70425144256795,
7.50438785222351));
#405546=CARTESIAN_POINT('Ctrl Pts',(0.481600982561012,-2.70429655427464,
7.50459414719561));
#405547=CARTESIAN_POINT('Ctrl Pts',(0.481310318334189,-2.70432585979777,
7.50483629897752));
#405548=CARTESIAN_POINT('Ctrl Pts',(0.481047641490135,-2.70433954584457,
7.50509910455309));
#405549=CARTESIAN_POINT('Ctrl Pts',(0.480468149988762,-2.70436973863845,
7.50567888004914));
#405550=CARTESIAN_POINT('Ctrl Pts',(0.480002061491295,-2.7043256226731,
7.50637912803144));
#405551=CARTESIAN_POINT('Ctrl Pts',(0.479638530743254,-2.704236142703,7.50710440483569));
#405552=CARTESIAN_POINT('Ctrl Pts',(0.479549385786738,-2.70421420043791,
7.50728225710685));
#405553=CARTESIAN_POINT('Ctrl Pts',(0.479464598424619,-2.70418923522453,
7.50746498566954));
#405554=CARTESIAN_POINT('Ctrl Pts',(0.479386030199372,-2.70416222946143,
7.50764697238949));
#405555=CARTESIAN_POINT('Ctrl Pts',(0.478963669043002,-2.70401705391124,
7.50862528291181));
#405556=CARTESIAN_POINT('Ctrl Pts',(0.478681344736196,-2.70380364525162,
7.50965856837421));
#405557=CARTESIAN_POINT('Ctrl Pts',(0.478486337883113,-2.70356220374557,
7.51067959873201));
#405558=CARTESIAN_POINT('Ctrl Pts',(0.478379025365891,-2.70342933818025,
7.51124147302578));
#405559=CARTESIAN_POINT('Ctrl Pts',(0.478298467079326,-2.70328767800995,
7.51180065547252));
#405560=CARTESIAN_POINT('Ctrl Pts',(0.478238051202762,-2.70314229426445,
7.512351757165));
#405561=CARTESIAN_POINT('Ctrl Pts',(0.478029290282408,-2.70263993550974,
7.51425603304535));
#405562=CARTESIAN_POINT('Ctrl Pts',(0.478041734656956,-2.70203089399621,
7.51626900505179));
#405563=CARTESIAN_POINT('Ctrl Pts',(0.478235751309932,-2.70136068775765,
7.51827788969242));
#405564=CARTESIAN_POINT('Ctrl Pts',(0.478246251857833,-2.70132441492951,
7.51838661432544));
#405565=CARTESIAN_POINT('Ctrl Pts',(0.478257292668725,-2.70128795759193,
7.51849533314856));
#405566=CARTESIAN_POINT('Ctrl Pts',(0.478268870165676,-2.70125132133976,
7.51860402984325));
#405567=CARTESIAN_POINT('Ctrl Pts',(0.511151790759207,-2.62465641820371,
7.57603338728985));
#405568=CARTESIAN_POINT('Ctrl Pts',(0.502935967270572,-2.65078068886369,
7.55196141284922));
#405569=CARTESIAN_POINT('Ctrl Pts',(0.494733471561858,-2.67685967867693,
7.52783573083104));
#405570=CARTESIAN_POINT('Ctrl Pts',(0.486543193716093,-2.70289709686825,
7.50366116530176));
#405571=CARTESIAN_POINT('Origin',(1.76626572250583E-16,-9.06940118467442E-16,
7.49482233047033));
#405572=CARTESIAN_POINT('Origin',(0.561510055974265,-2.6792933223221,7.49482233047033));
#405573=CARTESIAN_POINT('Origin',(0.,0.,7.50366116523517));
#405574=CARTESIAN_POINT('Origin',(0.484977299960314,-2.69419807522075,7.49482233047033));
#405575=CARTESIAN_POINT('Ctrl Pts',(0.570374388643635,-2.68331282671198,
7.51860402984325));
#405576=CARTESIAN_POINT('Ctrl Pts',(0.575221773022856,-2.68917790562962,
7.51860402984325));
#405577=CARTESIAN_POINT('Ctrl Pts',(0.582657984926202,-2.68756575223784,
7.51860402984325));
#405578=CARTESIAN_POINT('Ctrl Pts',(0.572174256523402,-2.68549056972994,
7.51041458714365));
#405579=CARTESIAN_POINT('Ctrl Pts',(0.576983494698361,-2.68879595835105,
7.5100464290044));
#405580=CARTESIAN_POINT('Ctrl Pts',(0.582660035745137,-2.68756530762508,
7.50729136483008));
#405581=CARTESIAN_POINT('Ctrl Pts',(0.570756300477624,-2.68792226417034,
7.50215815450138));
#405582=CARTESIAN_POINT('Ctrl Pts',(0.573396483322147,-2.68957377833285,
7.49877163671532));
#405583=CARTESIAN_POINT('Ctrl Pts',(0.576773332211246,-2.68886609537093,
7.49481588533172));
#405584=CARTESIAN_POINT('Ctrl Pts',(0.563322945647643,-2.68794368066494,
7.50366171572174));
#405585=CARTESIAN_POINT('Ctrl Pts',(0.564074028832216,-2.69152753840584,
7.50000045605858));
#405586=CARTESIAN_POINT('Ctrl Pts',(0.564074028832339,-2.69152753840582,
7.49482233047317));
#405587=CARTESIAN_POINT('Origin',(0.580009539540173,-2.67534954427312,7.51860402984325));
#405588=CARTESIAN_POINT('Origin',(0.580009539540173,-2.67534954427312,9.));
#405589=CARTESIAN_POINT('Origin',(0.580009539540173,-2.67534954427312,8.75721825406948));
#405590=CARTESIAN_POINT('Ctrl Pts',(0.559734948604752,-2.67044183725424,
8.78942910404913));
#405591=CARTESIAN_POINT('Ctrl Pts',(0.563269725412686,-2.67474971162796,
8.7967269950169));
#405592=CARTESIAN_POINT('Ctrl Pts',(0.571092507684352,-2.67045115797444,
8.79893251111267));
#405593=CARTESIAN_POINT('Ctrl Pts',(0.566739742255397,-2.67891581416313,
8.78111911759577));
#405594=CARTESIAN_POINT('Ctrl Pts',(0.570936015679932,-2.68401812731229,
8.78644465894813));
#405595=CARTESIAN_POINT('Ctrl Pts',(0.578712537116074,-2.68172875488109,
8.78817647674132));
#405596=CARTESIAN_POINT('Ctrl Pts',(0.571105296763092,-2.68419699867588,
8.76780923932034));
#405597=CARTESIAN_POINT('Ctrl Pts',(0.576062756082935,-2.69021682706735,
8.76988516158374));
#405598=CARTESIAN_POINT('Ctrl Pts',(0.58348113404944,-2.68876629311658,
8.77093053738833));
#405599=CARTESIAN_POINT('Ctrl Pts',(0.570254073382254,-2.68316723997289,
8.75371302330491));
#405600=CARTESIAN_POINT('Ctrl Pts',(0.575089272654503,-2.68903980750042,
8.75300828287559));
#405601=CARTESIAN_POINT('Ctrl Pts',(0.582551442759697,-2.68739343067373,
8.75267964240737));
#405602=CARTESIAN_POINT('Origin',(0.571075363033647,-2.66454152541039,8.78727029226991));
#405603=CARTESIAN_POINT('Ctrl Pts',(0.515891055659684,-2.6174022316462,
8.85049129520029));
#405604=CARTESIAN_POINT('Ctrl Pts',(0.51961163730155,-2.62190316315749,
8.85711686593484));
#405605=CARTESIAN_POINT('Ctrl Pts',(0.527270584603695,-2.61810299364326,
8.85933012996512));
#405606=CARTESIAN_POINT('Ctrl Pts',(0.531096423211032,-2.63579675286366,
8.82945683644723));
#405607=CARTESIAN_POINT('Ctrl Pts',(0.534847887930047,-2.64033504482779,
8.83607469902389));
#405608=CARTESIAN_POINT('Ctrl Pts',(0.542512653014795,-2.63649012367215,
8.8382956714852));
#405609=CARTESIAN_POINT('Ctrl Pts',(0.546279125935881,-2.65416385556391,
8.80838214965004));
#405610=CARTESIAN_POINT('Ctrl Pts',(0.550045395686181,-2.65872005774702,
8.81501364461989));
#405611=CARTESIAN_POINT('Ctrl Pts',(0.55773108530596,-2.65484978803238,
8.81722098428722));
#405612=CARTESIAN_POINT('Ctrl Pts',(0.561440886005621,-2.67250562312428,
8.78727029226991));
#405613=CARTESIAN_POINT('Ctrl Pts',(0.565207781345706,-2.67706258210756,
8.79393457792714));
#405614=CARTESIAN_POINT('Ctrl Pts',(0.572927672898325,-2.67318409147407,
8.79610912703474));
#405615=CARTESIAN_POINT('Origin',(0.52552553268771,-2.60943813393231,8.85049129520029));
#405616=CARTESIAN_POINT('Ctrl Pts',(0.50403663157861,-2.6197108805292,8.85049129520029));
#405617=CARTESIAN_POINT('Ctrl Pts',(0.502277013195099,-2.62527908089983,
8.85711686593484));
#405618=CARTESIAN_POINT('Ctrl Pts',(0.493751728365472,-2.62463079031094,
8.85933012996512));
#405619=CARTESIAN_POINT('Ctrl Pts',(0.505593340562145,-2.61478477403911,
8.86332496987232));
#405620=CARTESIAN_POINT('Ctrl Pts',(0.50112017184679,-2.61594350438771,
8.86648636486738));
#405621=CARTESIAN_POINT('Ctrl Pts',(0.498123021571862,-2.61085496902651,
8.87206031107457));
#405622=CARTESIAN_POINT('Ctrl Pts',(0.512577143703202,-2.61339326418189,
8.86341338519875));
#405623=CARTESIAN_POINT('Ctrl Pts',(0.517167288227797,-2.61275761972345,
8.86654584966055));
#405624=CARTESIAN_POINT('Ctrl Pts',(0.517980099556522,-2.60688705837627,
8.87215952290714));
#405625=CARTESIAN_POINT('Ctrl Pts',(0.515891055659684,-2.6174022316462,
8.85049129520029));
#405626=CARTESIAN_POINT('Ctrl Pts',(0.51961163730155,-2.62190316315749,
8.85711686593484));
#405627=CARTESIAN_POINT('Ctrl Pts',(0.527270584603694,-2.61810299364326,
8.85933012996512));
#405628=CARTESIAN_POINT('Origin',(0.492117610277408,-2.61594432623894,8.85049129520029));
#405629=CARTESIAN_POINT('Ctrl Pts',(0.482494215215367,-2.68788048588351,
8.78727029226991));
#405630=CARTESIAN_POINT('Ctrl Pts',(0.480712693150486,-2.69351799905962,
8.79393457792714));
#405631=CARTESIAN_POINT('Ctrl Pts',(0.47210152674199,-2.69281998167918,
8.79610912703474));
#405632=CARTESIAN_POINT('Ctrl Pts',(0.489664844518297,-2.66518948588238,
8.80838214965003));
#405633=CARTESIAN_POINT('Ctrl Pts',(0.48788361832092,-2.67082606280454,
8.81501364461989));
#405634=CARTESIAN_POINT('Ctrl Pts',(0.479307239296731,-2.67012283067463,
8.81722098428721));
#405635=CARTESIAN_POINT('Ctrl Pts',(0.496845378477128,-2.6424671432281,
8.82945683644723));
#405636=CARTESIAN_POINT('Ctrl Pts',(0.49507115419714,-2.64808156302841,
8.83607469902391));
#405637=CARTESIAN_POINT('Ctrl Pts',(0.486523682952896,-2.64739397461502,
8.8382956714852));
#405638=CARTESIAN_POINT('Ctrl Pts',(0.50403663157861,-2.6197108805292,8.85049129520029));
#405639=CARTESIAN_POINT('Ctrl Pts',(0.502277013195099,-2.62527908089983,
8.85711686593484));
#405640=CARTESIAN_POINT('Ctrl Pts',(0.493751728365472,-2.62463079031094,
8.85933012996512));
#405641=CARTESIAN_POINT('Origin',(0.470575193914165,-2.68411393159325,8.78727029226991));
#405642=CARTESIAN_POINT('Ctrl Pts',(0.478324646131857,-2.70107476062509,
8.75374538247847));
#405643=CARTESIAN_POINT('Ctrl Pts',(0.476047406919821,-2.70832448889302,
8.75304829418602));
#405644=CARTESIAN_POINT('Ctrl Pts',(0.46852170749443,-2.70960296117184,
8.75272238421917));
#405645=CARTESIAN_POINT('Ctrl Pts',(0.477926903323322,-2.70233339384104,
8.76769408445022));
#405646=CARTESIAN_POINT('Ctrl Pts',(0.475591700278409,-2.70976535062987,
8.76974318093968));
#405647=CARTESIAN_POINT('Ctrl Pts',(0.468179438674307,-2.71120643882727,
8.77077869880429));
#405648=CARTESIAN_POINT('Ctrl Pts',(0.479965506394863,-2.6958823569765,
8.78108014887987));
#405649=CARTESIAN_POINT('Ctrl Pts',(0.477990130614244,-2.70218181154225,
8.78639403366326));
#405650=CARTESIAN_POINT('Ctrl Pts',(0.469936666898026,-2.70299654947582,
8.78812224174742));
#405651=CARTESIAN_POINT('Ctrl Pts',(0.483306326769365,-2.68531053162587,
8.78944554828686));
#405652=CARTESIAN_POINT('Ctrl Pts',(0.481646894576993,-2.69062115328588,
8.79673892988685));
#405653=CARTESIAN_POINT('Ctrl Pts',(0.472791874487174,-2.68957608222346,
8.79894799272499));
#405654=CARTESIAN_POINT('Origin',(0.466349848864478,-2.6974847670495,8.75721825406948));
#405655=CARTESIAN_POINT('Origin',(0.466349848864478,-2.6974847670495,9.));
#405656=CARTESIAN_POINT('Origin',(0.466349848864479,-2.6974847670495,7.51860402984325));
#405657=CARTESIAN_POINT('Ctrl Pts',(0.486543054373036,-2.70289632259342,
7.50366195182966));
#405658=CARTESIAN_POINT('Ctrl Pts',(0.487191808179173,-2.70650034953686,
7.50000065167735));
#405659=CARTESIAN_POINT('Ctrl Pts',(0.487191808179058,-2.70650034953688,
7.49482233047108));
#405660=CARTESIAN_POINT('Ctrl Pts',(0.479638433643629,-2.70566760608482,
7.50215800491338));
#405661=CARTESIAN_POINT('Ctrl Pts',(0.477809241429477,-2.70818926288502,
7.49877273257264));
#405662=CARTESIAN_POINT('Ctrl Pts',(0.474411728045476,-2.70880086664193,
7.49481816995649));
#405663=CARTESIAN_POINT('Ctrl Pts',(0.477419885150982,-2.70393900580488,
7.51043025814042));
#405664=CARTESIAN_POINT('Ctrl Pts',(0.474203815632252,-2.70881236746162,
7.51006209594516));
#405665=CARTESIAN_POINT('Ctrl Pts',(0.468476805372746,-2.70980248040963,
7.50731281821699));
#405666=CARTESIAN_POINT('Ctrl Pts',(0.478269325502402,-2.70124988015243,
7.51860402984326));
#405667=CARTESIAN_POINT('Ctrl Pts',(0.475977343984493,-2.70850576315261,
7.51860402984326));
#405668=CARTESIAN_POINT('Ctrl Pts',(0.468479300229151,-2.70980204909082,
7.51860402984327));
#405669=CARTESIAN_POINT('Origin',(0.,0.,7.5));
#405670=CARTESIAN_POINT('Origin',(0.670846486662646,-2.58203466569846,7.5));
#405671=CARTESIAN_POINT('',(0.670846486662646,-2.58203466569846,7.59394543036555));
#405672=CARTESIAN_POINT('',(0.670846486662646,-2.58203466569846,8.85049129520029));
#405673=CARTESIAN_POINT('',(0.670846486662646,-2.58203466569846,7.5));
#405674=CARTESIAN_POINT('',(0.653715973115287,-2.65144443664272,8.78727029226991));
#405675=CARTESIAN_POINT('Ctrl Pts',(0.670846486662646,-2.58203466569846,
8.85049129520029));
#405676=CARTESIAN_POINT('Ctrl Pts',(0.665128015193379,-2.60520488728789,
8.82945686509571));
#405677=CARTESIAN_POINT('Ctrl Pts',(0.659418044923419,-2.62834066354123,
8.80838212259896));
#405678=CARTESIAN_POINT('Ctrl Pts',(0.653715973115287,-2.65144443664272,
8.78727029226991));
#405679=CARTESIAN_POINT('',(0.65035598185918,-2.66505851907033,8.75721825406948));
#405680=CARTESIAN_POINT('Origin',(0.660467557061559,-2.62408907064178,8.75937679713108));
#405681=CARTESIAN_POINT('',(0.65035598185918,-2.66505851907033,7.51860402984325));
#405682=CARTESIAN_POINT('',(0.65035598185918,-2.66505851907033,7.5));
#405683=CARTESIAN_POINT('Ctrl Pts',(0.65035598185918,-2.66505851907033,
7.51860402984325));
#405684=CARTESIAN_POINT('Ctrl Pts',(0.652994732413366,-2.65436677471377,
7.52834476460825));
#405685=CARTESIAN_POINT('Ctrl Pts',(0.655635196006342,-2.64366808943105,
7.53807742314407));
#405686=CARTESIAN_POINT('Ctrl Pts',(0.658277430155653,-2.63296223017134,
7.54780169004674));
#405687=CARTESIAN_POINT('Ctrl Pts',(0.662462586247591,-2.61600472770628,
7.5632044032688));
#405688=CARTESIAN_POINT('Ctrl Pts',(0.666652189758578,-2.59902920509617,
7.57858609112103));
#405689=CARTESIAN_POINT('Ctrl Pts',(0.670846486662646,-2.58203466569846,
7.59394543036555));
#405690=CARTESIAN_POINT('Origin',(0.870959027955008,-2.77926849494597,7.5));
#405691=CARTESIAN_POINT('',(0.741123661093039,-2.6412564305984,8.75721825406948));
#405692=CARTESIAN_POINT('',(0.731515368664242,-2.6310430326237,8.78727029226991));
#405693=CARTESIAN_POINT('Origin',(0.707125938766795,-2.60511761915769,8.75658640621103));
#405694=CARTESIAN_POINT('',(0.682528638916271,-2.57897124462358,8.85049129520029));
#405695=CARTESIAN_POINT('Ctrl Pts',(0.731515368664242,-2.6310430326237,
8.78727029226991));
#405696=CARTESIAN_POINT('Ctrl Pts',(0.715209619867144,-2.61371038970358,
8.80838212259895));
#405697=CARTESIAN_POINT('Ctrl Pts',(0.698881284484194,-2.59635373775253,
8.82945686509571));
#405698=CARTESIAN_POINT('Ctrl Pts',(0.682528638916271,-2.57897124462358,
8.85049129520029));
#405699=CARTESIAN_POINT('',(0.682528638916271,-2.57897124462358,7.59394543036555));
#405700=CARTESIAN_POINT('',(0.682528638916271,-2.57897124462358,7.5));
#405701=CARTESIAN_POINT('',(0.741123661093039,-2.6412564305984,7.51860402984325));
#405702=CARTESIAN_POINT('Ctrl Pts',(0.682528638916271,-2.57897124462358,
7.59394543036555));
#405703=CARTESIAN_POINT('Ctrl Pts',(0.694522727030107,-2.59172068955962,
7.57858609112103));
#405704=CARTESIAN_POINT('Ctrl Pts',(0.706503393831167,-2.60445586794314,
7.56320440326857));
#405705=CARTESIAN_POINT('Ctrl Pts',(0.7184713427115,-2.61717752746397,7.54780169004651));
#405706=CARTESIAN_POINT('Ctrl Pts',(0.726027123794494,-2.6252091522071,
7.53807742314383));
#405707=CARTESIAN_POINT('Ctrl Pts',(0.733577841762352,-2.63323539497312,
7.52834476460825));
#405708=CARTESIAN_POINT('Ctrl Pts',(0.74112366109304,-2.6412564305984,7.51860402984325));
#405709=CARTESIAN_POINT('',(0.741123661093039,-2.6412564305984,7.5));
#405710=CARTESIAN_POINT('Origin',(0.677521207658211,-2.58368200434955,7.5));
#405711=CARTESIAN_POINT('Ctrl Pts',(0.682528638916271,-2.57897124462358,
8.85049129520029));
#405712=CARTESIAN_POINT('Ctrl Pts',(0.682395941778447,-2.57883019056129,
8.85097269580138));
#405713=CARTESIAN_POINT('Ctrl Pts',(0.682258792377727,-2.57869667966878,
8.85143669361005));
#405714=CARTESIAN_POINT('Ctrl Pts',(0.682110265580004,-2.57856519066829,
8.8519052845931));
#405715=CARTESIAN_POINT('Ctrl Pts',(0.681819756582884,-2.57830800652207,
8.85282181883899));
#405716=CARTESIAN_POINT('Ctrl Pts',(0.681493063938937,-2.57806532082595,
8.85372622499636));
#405717=CARTESIAN_POINT('Ctrl Pts',(0.681115866722558,-2.57784570272727,
8.85462257735071));
#405718=CARTESIAN_POINT('Ctrl Pts',(0.680802730990299,-2.57766338358185,
8.85536669723986));
#405719=CARTESIAN_POINT('Ctrl Pts',(0.680454733368203,-2.57749689311832,
8.85610498449051));
#405720=CARTESIAN_POINT('Ctrl Pts',(0.680060197116754,-2.57735833882344,
8.85681338218371));
#405721=CARTESIAN_POINT('Ctrl Pts',(0.679702154848935,-2.57723260058324,
8.85745625420284));
#405722=CARTESIAN_POINT('Ctrl Pts',(0.679301492304172,-2.57712772749012,
8.85808743050665));
#405723=CARTESIAN_POINT('Ctrl Pts',(0.678839734209363,-2.57706554866298,
8.85866804508409));
#405724=CARTESIAN_POINT('Ctrl Pts',(0.678626689034105,-2.57703686070001,
8.85893592806395));
#405725=CARTESIAN_POINT('Ctrl Pts',(0.67840050506838,-2.57701746342574,
8.85919241173848));
#405726=CARTESIAN_POINT('Ctrl Pts',(0.678158684088304,-2.57701094304344,
8.85943017985534));
#405727=CARTESIAN_POINT('Ctrl Pts',(0.677832154178531,-2.5770021385971,
8.8597512372));
#405728=CARTESIAN_POINT('Ctrl Pts',(0.677468785008082,-2.57701722880275,
8.86004599534705));
#405729=CARTESIAN_POINT('Ctrl Pts',(0.677073374472439,-2.57706643848078,
8.86026130871721));
#405730=CARTESIAN_POINT('Ctrl Pts',(0.676928603527537,-2.57708445553127,
8.86034014101235));
#405731=CARTESIAN_POINT('Ctrl Pts',(0.676777361302722,-2.57710730469717,
8.86040910639692));
#405732=CARTESIAN_POINT('Ctrl Pts',(0.676623818556266,-2.57713469607019,
8.86046313645506));
#405733=CARTESIAN_POINT('Ctrl Pts',(0.676384216386331,-2.57717744007839,
8.86054744990829));
#405734=CARTESIAN_POINT('Ctrl Pts',(0.676132497543417,-2.5772325565079,
8.86059655985669));
#405735=CARTESIAN_POINT('Ctrl Pts',(0.675884742861737,-2.57729622439678,
8.86059725258816));
#405736=CARTESIAN_POINT('Ctrl Pts',(0.675636415767763,-2.57736003938391,
8.86059794692011));
#405737=CARTESIAN_POINT('Ctrl Pts',(0.675389978449765,-2.57743572627043,
8.86056369958366));
#405738=CARTESIAN_POINT('Ctrl Pts',(0.675157766911382,-2.57751555979232,
8.86048590497774));
#405739=CARTESIAN_POINT('Ctrl Pts',(0.675097166613635,-2.5775363939646,
8.86046560290182));
#405740=CARTESIAN_POINT('Ctrl Pts',(0.675036776242778,-2.57755786724414,
8.86044257503091));
#405741=CARTESIAN_POINT('Ctrl Pts',(0.674978450913656,-2.57757928515972,
8.86041778462583));
#405742=CARTESIAN_POINT('Ctrl Pts',(0.674585993824371,-2.57772340115413,
8.86025097596201));
#405743=CARTESIAN_POINT('Ctrl Pts',(0.674234485840269,-2.57788466047735,
8.8599848982295));
#405744=CARTESIAN_POINT('Ctrl Pts',(0.673930653710918,-2.57805065560952,
8.85968173251462));
#405745=CARTESIAN_POINT('Ctrl Pts',(0.673769943921998,-2.57813845752406,
8.85952137522077));
#405746=CARTESIAN_POINT('Ctrl Pts',(0.673619383548732,-2.57822910929007,
8.85934740853961));
#405747=CARTESIAN_POINT('Ctrl Pts',(0.673480293963292,-2.57832000073264,
8.8591675900182));
#405748=CARTESIAN_POINT('Ctrl Pts',(0.672921776980423,-2.57868497711901,
8.85844552518695));
#405749=CARTESIAN_POINT('Ctrl Pts',(0.672514998205092,-2.57907191274903,
8.85759444184125));
#405750=CARTESIAN_POINT('Ctrl Pts',(0.67221166989639,-2.57941718972865,
8.85683498915139));
#405751=CARTESIAN_POINT('Ctrl Pts',(0.672179927396713,-2.57945332204502,
8.85675551444998));
#405752=CARTESIAN_POINT('Ctrl Pts',(0.672149335081563,-2.57948900814192,
8.85667699793652));
#405753=CARTESIAN_POINT('Ctrl Pts',(0.672119849310388,-2.57952418108657,
8.85659965593547));
#405754=CARTESIAN_POINT('Ctrl Pts',(0.671721848866504,-2.57999894728824,
8.85555568965886));
#405755=CARTESIAN_POINT('Ctrl Pts',(0.671407911415544,-2.58051270616165,
8.85434650606346));
#405756=CARTESIAN_POINT('Ctrl Pts',(0.671171181984431,-2.58106475696341,
8.85297329937117));
#405757=CARTESIAN_POINT('Ctrl Pts',(0.671038036103566,-2.58137525190245,
8.85220095427747));
#405758=CARTESIAN_POINT('Ctrl Pts',(0.670929549231057,-2.58169811105686,
8.85137579139184));
#405759=CARTESIAN_POINT('Ctrl Pts',(0.670846486662646,-2.58203466569846,
8.85049129520029));
#405760=CARTESIAN_POINT('Origin',(0.677521207658211,-2.58368200434955,7.59394543036555));
#405761=CARTESIAN_POINT('Ctrl Pts',(0.682143374360212,-2.57856171709663,
7.59443877723642));
#405762=CARTESIAN_POINT('Ctrl Pts',(0.678175520124406,-2.57434397760585,
7.58783886950016));
#405763=CARTESIAN_POINT('Ctrl Pts',(0.670813608404349,-2.57857262246712,
7.58559994247159));
#405764=CARTESIAN_POINT('Ctrl Pts',(0.703803774221571,-2.60158623323358,
7.56670252222133));
#405765=CARTESIAN_POINT('Ctrl Pts',(0.699841654661642,-2.59737458957381,
7.56004874999028));
#405766=CARTESIAN_POINT('Ctrl Pts',(0.692425479350867,-2.60160976383429,
7.55786368756704));
#405767=CARTESIAN_POINT('Ctrl Pts',(0.725423725450355,-2.6245677533871,
7.53888913333561));
#405768=CARTESIAN_POINT('Ctrl Pts',(0.72143805881991,-2.62033107972281,
7.5322200213728));
#405769=CARTESIAN_POINT('Ctrl Pts',(0.713998608634764,-2.62460390380804,
7.53005029815326));
#405770=CARTESIAN_POINT('Ctrl Pts',(0.747002249729082,-2.64750523762779,
7.51101258149734));
#405771=CARTESIAN_POINT('Ctrl Pts',(0.742968269576908,-2.6432172077805,
7.5043616886572));
#405772=CARTESIAN_POINT('Ctrl Pts',(0.735531870110738,-2.647553962849,7.50217374673251));
#405773=CARTESIAN_POINT('',(0.73438282836693,-2.64632931751459,7.50366116523517));
#405774=CARTESIAN_POINT('Ctrl Pts',(0.74112366109304,-2.6412564305984,7.51860402984325));
#405775=CARTESIAN_POINT('Ctrl Pts',(0.741426253722739,-2.64157807973369,
7.51734760759494));
#405776=CARTESIAN_POINT('Ctrl Pts',(0.741656354716104,-2.64190950301716,
7.51608817408573));
#405777=CARTESIAN_POINT('Ctrl Pts',(0.741802465711226,-2.642257553818,7.5148100591312));
#405778=CARTESIAN_POINT('Ctrl Pts',(0.741934816542043,-2.64257282655033,
7.51365231206384));
#405779=CARTESIAN_POINT('Ctrl Pts',(0.741998669384426,-2.64290209001152,
7.51247773061043));
#405780=CARTESIAN_POINT('Ctrl Pts',(0.741956669655458,-2.64324667653265,
7.51129758471022));
#405781=CARTESIAN_POINT('Ctrl Pts',(0.741904468788902,-2.64367495822514,
7.50983079813401));
#405782=CARTESIAN_POINT('Ctrl Pts',(0.741677487599955,-2.64411166614862,
7.50839324291155));
#405783=CARTESIAN_POINT('Ctrl Pts',(0.741200920369,-2.64452196792184,7.50715379678855));
#405784=CARTESIAN_POINT('Ctrl Pts',(0.740980760040254,-2.64471151551851,
7.50658120839351));
#405785=CARTESIAN_POINT('Ctrl Pts',(0.740669836489923,-2.64491517281699,
7.50598221009429));
#405786=CARTESIAN_POINT('Ctrl Pts',(0.74026308577848,-2.6451090650682,7.50545747549611));
#405787=CARTESIAN_POINT('Ctrl Pts',(0.740046031008742,-2.64521253197498,
7.50517746087247));
#405788=CARTESIAN_POINT('Ctrl Pts',(0.739799421791916,-2.64531452291221,
7.50491486231392));
#405789=CARTESIAN_POINT('Ctrl Pts',(0.739529151276123,-2.64541079559313,
7.50468370960992));
#405790=CARTESIAN_POINT('Ctrl Pts',(0.739125011603008,-2.64555475361861,
7.50433806340446));
#405791=CARTESIAN_POINT('Ctrl Pts',(0.738655660604345,-2.64568971815751,
7.50405484070983));
#405792=CARTESIAN_POINT('Ctrl Pts',(0.738152510216528,-2.64580591110398,
7.5038576603613));
#405793=CARTESIAN_POINT('Ctrl Pts',(0.738098706103284,-2.64581833613356,
7.50383657498791));
#405794=CARTESIAN_POINT('Ctrl Pts',(0.738044542534841,-2.64583055506889,
7.50381643264937));
#405795=CARTESIAN_POINT('Ctrl Pts',(0.737990077468983,-2.64584256247728,
7.50379723213559));
#405796=CARTESIAN_POINT('Ctrl Pts',(0.737626505337586,-2.64592271585613,
7.50366906242519));
#405797=CARTESIAN_POINT('Ctrl Pts',(0.737241435141454,-2.64599448492876,
7.50358235568538));
#405798=CARTESIAN_POINT('Ctrl Pts',(0.736868612002289,-2.64605473955297,
7.5035341175365));
#405799=CARTESIAN_POINT('Ctrl Pts',(0.736309605900543,-2.64614508454246,
7.50346178989176));
#405800=CARTESIAN_POINT('Ctrl Pts',(0.735704401177955,-2.64621850689902,
7.50346967198527));
#405801=CARTESIAN_POINT('Ctrl Pts',(0.735108059804492,-2.64627230370701,
7.50354272648692));
#405802=CARTESIAN_POINT('Ctrl Pts',(0.734862772254051,-2.64629443144767,
7.50357277531559));
#405803=CARTESIAN_POINT('Ctrl Pts',(0.734619322893534,-2.64631335066844,
7.50361331098761));
#405804=CARTESIAN_POINT('Ctrl Pts',(0.734382828367309,-2.64632931751596,
7.50366116523658));
#405805=CARTESIAN_POINT('',(0.678263889301933,-2.58651417133809,7.57603338622103));
#405806=CARTESIAN_POINT('Origin',(0.680502659389328,-2.59506282024291,7.58486873427627));
#405807=CARTESIAN_POINT('Ctrl Pts',(0.734382828409904,-2.64632931755256,
7.50366116529968));
#405808=CARTESIAN_POINT('Ctrl Pts',(0.715706430670521,-2.62642404271696,
7.52783573079709));
#405809=CARTESIAN_POINT('Ctrl Pts',(0.697000987800557,-2.60648661431366,
7.55196141284068));
#405810=CARTESIAN_POINT('Ctrl Pts',(0.678263890381624,-2.58651417197205,
7.57603338728831));
#405811=CARTESIAN_POINT('Ctrl Pts',(0.683105249421544,-2.57984075934191,
7.59639677331371));
#405812=CARTESIAN_POINT('Ctrl Pts',(0.67284342550402,-2.56471571766823,
7.59959882295463));
#405813=CARTESIAN_POINT('Ctrl Pts',(0.670788463607718,-2.58289499004649,
7.59642833564546));
#405814=CARTESIAN_POINT('Ctrl Pts',(0.681462581934917,-2.57630285775875,
7.58707626057423));
#405815=CARTESIAN_POINT('Ctrl Pts',(0.675085619068564,-2.57401230419309,
7.58809943920599));
#405816=CARTESIAN_POINT('Ctrl Pts',(0.67058158747929,-2.57905493249942,
7.58710240504253));
#405817=CARTESIAN_POINT('Ctrl Pts',(0.679301722070263,-2.58198232224996,
7.58015376756929));
#405818=CARTESIAN_POINT('Ctrl Pts',(0.676766535642928,-2.58067767625402,
7.5820588065976));
#405819=CARTESIAN_POINT('Ctrl Pts',(0.675182333579464,-2.58300520259328,
7.58020924244128));
#405820=CARTESIAN_POINT('Ctrl Pts',(0.678263889092213,-2.58651417053753,
7.57603338509286));
#405821=CARTESIAN_POINT('Ctrl Pts',(0.678263889092213,-2.58651417053753,
7.57603338509286));
#405822=CARTESIAN_POINT('Ctrl Pts',(0.678263889092213,-2.58651417053753,
7.57603338509286));
#405823=CARTESIAN_POINT('Origin',(0.680508179114493,-2.59506137280058,7.58486873427621));
#405824=CARTESIAN_POINT('Ctrl Pts',(0.64829375964388,-2.67341427391705,
7.51098857897448));
#405825=CARTESIAN_POINT('Ctrl Pts',(0.649704436926231,-2.66769846237564,
7.50433767179956));
#405826=CARTESIAN_POINT('Ctrl Pts',(0.658312065540237,-2.66782800281639,
7.50214974420965));
#405827=CARTESIAN_POINT('Ctrl Pts',(0.655841875747635,-2.64283066015825,
7.53887321589163));
#405828=CARTESIAN_POINT('Ctrl Pts',(0.657235650612657,-2.63718333418287,
7.5322040745206));
#405829=CARTESIAN_POINT('Ctrl Pts',(0.66581456026676,-2.63725564648319,
7.53003438070911));
#405830=CARTESIAN_POINT('Ctrl Pts',(0.663404487018678,-2.61218831457927,
7.56669465659231));
#405831=CARTESIAN_POINT('Ctrl Pts',(0.664790024933336,-2.60657436325043,
7.56004085833297));
#405832=CARTESIAN_POINT('Ctrl Pts',(0.673330168792996,-2.60662528459036,
7.55785582193789));
#405833=CARTESIAN_POINT('Ctrl Pts',(0.67098125143039,-2.58148862301068,
7.59443891967696));
#405834=CARTESIAN_POINT('Ctrl Pts',(0.672368798202544,-2.57586653215138,
7.58783901202978));
#405835=CARTESIAN_POINT('Ctrl Pts',(0.680858439628815,-2.57593841011513,
7.58560008491213));
#405836=CARTESIAN_POINT('',(0.658718750143912,-2.66617077539049,7.50366116523517));
#405837=CARTESIAN_POINT('Ctrl Pts',(0.658718750144001,-2.66617077539085,
7.50366116523554));
#405838=CARTESIAN_POINT('Ctrl Pts',(0.658034914852376,-2.66649712920298,
7.50350835821027));
#405839=CARTESIAN_POINT('Ctrl Pts',(0.65739568666618,-2.66677487969734,
7.50345484956));
#405840=CARTESIAN_POINT('Ctrl Pts',(0.656782300120865,-2.66701283537894,
7.50349758195598));
#405841=CARTESIAN_POINT('Ctrl Pts',(0.656467587333186,-2.66713492429085,
7.50351950684424));
#405842=CARTESIAN_POINT('Ctrl Pts',(0.656128704689333,-2.66725869166959,
7.50357029184312));
#405843=CARTESIAN_POINT('Ctrl Pts',(0.655798643426452,-2.66736905658083,
7.50365515313923));
#405844=CARTESIAN_POINT('Ctrl Pts',(0.655290875549136,-2.66753884250547,
7.50378570417639));
#405845=CARTESIAN_POINT('Ctrl Pts',(0.654789190205213,-2.66768222205233,
7.50400001621911));
#405846=CARTESIAN_POINT('Ctrl Pts',(0.654331149039327,-2.66778609894424,
7.50428903009635));
#405847=CARTESIAN_POINT('Ctrl Pts',(0.654280309993871,-2.66779762848007,
7.50432110841318));
#405848=CARTESIAN_POINT('Ctrl Pts',(0.654229988079957,-2.66780869367321,
7.50435406373354));
#405849=CARTESIAN_POINT('Ctrl Pts',(0.654180219277456,-2.66781929287174,
7.50438785222352));
#405850=CARTESIAN_POINT('Ctrl Pts',(0.65387635681626,-2.66788400607338,
7.50459414719561));
#405851=CARTESIAN_POINT('Ctrl Pts',(0.653588167401578,-2.66793187430612,
7.50483629897752));
#405852=CARTESIAN_POINT('Ctrl Pts',(0.653326907123302,-2.66796236199665,
7.5050991045531));
#405853=CARTESIAN_POINT('Ctrl Pts',(0.652750540708314,-2.66802962090416,
7.50567888004914));
#405854=CARTESIAN_POINT('Ctrl Pts',(0.65228258332005,-2.66801545797236,
7.50637912803144));
#405855=CARTESIAN_POINT('Ctrl Pts',(0.651914066483551,-2.66794945334346,
7.50710440483569));
#405856=CARTESIAN_POINT('Ctrl Pts',(0.651823698839158,-2.66793326769808,
7.50728225710685));
#405857=CARTESIAN_POINT('Ctrl Pts',(0.651737486155056,-2.66791378612335,
7.50746498566954));
#405858=CARTESIAN_POINT('Ctrl Pts',(0.651657349091471,-2.66789186972997,
7.50764697238949));
#405859=CARTESIAN_POINT('Ctrl Pts',(0.651226554291956,-2.66777405323071,
7.50862528291182));
#405860=CARTESIAN_POINT('Ctrl Pts',(0.650931136910949,-2.66757917162251,
7.50965856837422));
#405861=CARTESIAN_POINT('Ctrl Pts',(0.650721061509954,-2.6673507203159,
7.51067959873203));
#405862=CARTESIAN_POINT('Ctrl Pts',(0.650605456751812,-2.66722500327372,
7.51124147302579));
#405863=CARTESIAN_POINT('Ctrl Pts',(0.650515987782613,-2.66708879554658,
7.51180065547253));
#405864=CARTESIAN_POINT('Ctrl Pts',(0.650446381268391,-2.66694758136607,
7.51235175716501));
#405865=CARTESIAN_POINT('Ctrl Pts',(0.650205863033812,-2.66645963011939,
7.51425603304536));
#405866=CARTESIAN_POINT('Ctrl Pts',(0.650179260416308,-2.66585104263315,
7.5162690050518));
#405867=CARTESIAN_POINT('Ctrl Pts',(0.650329938180127,-2.66516978271555,
7.51827788969243));
#405868=CARTESIAN_POINT('Ctrl Pts',(0.650338093145447,-2.66513291164141,
7.51838661432545));
#405869=CARTESIAN_POINT('Ctrl Pts',(0.65034677544217,-2.66509582182216,
7.51849533314856));
#405870=CARTESIAN_POINT('Ctrl Pts',(0.650355981859176,-2.66505851907033,
7.51860402984325));
#405871=CARTESIAN_POINT('Ctrl Pts',(0.678263888672342,-2.58651417242151,
7.57603338728985));
#405872=CARTESIAN_POINT('Ctrl Pts',(0.671738733242242,-2.61311115758385,
7.55196141284922));
#405873=CARTESIAN_POINT('Ctrl Pts',(0.665223977054884,-2.63966210102,7.52783573083104));
#405874=CARTESIAN_POINT('Ctrl Pts',(0.65871875012459,-2.66617077544642,
7.50366116530176));
#405875=CARTESIAN_POINT('Origin',(2.34371526914296E-16,-8.93760209386494E-16,
7.49482233047033));
#405876=CARTESIAN_POINT('Origin',(0.732019285896533,-2.63781235403043,7.49482233047033));
#405877=CARTESIAN_POINT('Origin',(0.,0.,7.50366116523517));
#405878=CARTESIAN_POINT('Origin',(0.6565987254349,-2.65758995402927,7.49482233047033));
#405879=CARTESIAN_POINT('Ctrl Pts',(0.74112293637421,-2.64125566017333,
7.51860402984325));
#405880=CARTESIAN_POINT('Ctrl Pts',(0.746336138178801,-2.6467981156738,
7.51860402984325));
#405881=CARTESIAN_POINT('Ctrl Pts',(0.753653780564807,-2.6447128348916,
7.51860402984325));
#405882=CARTESIAN_POINT('Ctrl Pts',(0.743058634706615,-2.64331361085372,
7.51041458714365));
#405883=CARTESIAN_POINT('Ctrl Pts',(0.748069768762033,-2.64630407925162,
7.51004642900442));
#405884=CARTESIAN_POINT('Ctrl Pts',(0.753655798683693,-2.64471225979592,
7.50729136483009));
#405885=CARTESIAN_POINT('Ctrl Pts',(0.741799391201317,-2.64583115787286,
7.50215815450138));
#405886=CARTESIAN_POINT('Ctrl Pts',(0.744539962382722,-2.64731012172677,
7.4987716367153));
#405887=CARTESIAN_POINT('Ctrl Pts',(0.747864531770558,-2.64638753732422,
7.49481588533172));
#405888=CARTESIAN_POINT('Ctrl Pts',(0.734382681155584,-2.64632878704413,
7.50366171572174));
#405889=CARTESIAN_POINT('Ctrl Pts',(0.735361839713041,-2.64985715930008,
7.50000045605858));
#405890=CARTESIAN_POINT('Ctrl Pts',(0.735361839713161,-2.64985715930004,
7.49482233047317));
#405891=CARTESIAN_POINT('Origin',(0.750228081562239,-2.63269141291482,7.51860402984325));
#405892=CARTESIAN_POINT('Origin',(0.750228081562239,-2.63269141291482,9.));
#405893=CARTESIAN_POINT('Origin',(0.750228081562239,-2.63269141291482,8.75721825406948));
#405894=CARTESIAN_POINT('Ctrl Pts',(0.729680709080038,-2.62909278680761,
8.78942910404913));
#405895=CARTESIAN_POINT('Ctrl Pts',(0.733484229768694,-2.63316533626375,
8.7967269950169));
#405896=CARTESIAN_POINT('Ctrl Pts',(0.741015530017009,-2.62837440706871,
8.79893251111267));
#405897=CARTESIAN_POINT('Ctrl Pts',(0.73721404019554,-2.637100554352,8.78111911759582));
#405898=CARTESIAN_POINT('Ctrl Pts',(0.741728598252154,-2.64192352809015,
8.78644465894813));
#405899=CARTESIAN_POINT('Ctrl Pts',(0.749342461395685,-2.63914061598106,
8.78817647674132));
#405900=CARTESIAN_POINT('Ctrl Pts',(0.741908991856784,-2.64209118606713,
8.76780923932031));
#405901=CARTESIAN_POINT('Ctrl Pts',(0.747241957274032,-2.64778102056637,
8.76988516158374));
#405902=CARTESIAN_POINT('Ctrl Pts',(0.754552157358074,-2.64585816978495,
8.77093053738833));
#405903=CARTESIAN_POINT('Ctrl Pts',(0.740993540539042,-2.64111808118309,
8.75371302330492));
#405904=CARTESIAN_POINT('Ctrl Pts',(0.746195062069161,-2.64666879060977,
8.75300828287559));
#405905=CARTESIAN_POINT('Ctrl Pts',(0.753536416620095,-2.64454769356067,
8.75267964240738));
#405906=CARTESIAN_POINT('Origin',(0.740619789133442,-2.62247801494012,8.78727029226991));
#405907=CARTESIAN_POINT('Ctrl Pts',(0.682528638916271,-2.57897124462358,
8.85049129520029));
#405908=CARTESIAN_POINT('Ctrl Pts',(0.686529951896168,-2.5832245500041,
8.85711686593484));
#405909=CARTESIAN_POINT('Ctrl Pts',(0.693929685372921,-2.57894147790724,
8.85933012996512));
#405910=CARTESIAN_POINT('Ctrl Pts',(0.698881306430053,-2.59635376108048,
8.82945683644722));
#405911=CARTESIAN_POINT('Ctrl Pts',(0.702915832726909,-2.60064237146728,
8.83607469902389));
#405912=CARTESIAN_POINT('Ctrl Pts',(0.710318504785506,-2.59631426692943,
8.83829567148519));
#405913=CARTESIAN_POINT('Ctrl Pts',(0.71520959897422,-2.61371036749488,
8.80838214965002));
#405914=CARTESIAN_POINT('Ctrl Pts',(0.719260047395548,-2.61801590274054,
8.81501364461988));
#405915=CARTESIAN_POINT('Ctrl Pts',(0.726681976909678,-2.6136611610855,
8.81722098428721));
#405916=CARTESIAN_POINT('Ctrl Pts',(0.731515368664242,-2.6310430326237,
8.78727029226991));
#405917=CARTESIAN_POINT('Ctrl Pts',(0.735566489878354,-2.63534928303293,
8.79393457792714));
#405918=CARTESIAN_POINT('Ctrl Pts',(0.743022024337742,-2.63098414602441,
8.79610912703474));
#405919=CARTESIAN_POINT('Origin',(0.69163305938547,-2.57040622694,8.85049129520029));
#405920=CARTESIAN_POINT('Ctrl Pts',(0.670846486662646,-2.58203466569846,
8.85049129520029));
#405921=CARTESIAN_POINT('Ctrl Pts',(0.669447239426466,-2.58770416474116,
8.85711686593484));
#405922=CARTESIAN_POINT('Ctrl Pts',(0.660897934588214,-2.58760342300925,
8.85933012996512));
#405923=CARTESIAN_POINT('Ctrl Pts',(0.672084380494145,-2.57701894173548,
8.86332496987231));
#405924=CARTESIAN_POINT('Ctrl Pts',(0.667694642491991,-2.57846188825189,
8.86648636486738));
#405925=CARTESIAN_POINT('Ctrl Pts',(0.664377626603774,-2.57357583590977,
8.87206031107456));
#405926=CARTESIAN_POINT('Ctrl Pts',(0.678964680319988,-2.57518283708093,
8.86341338519877));
#405927=CARTESIAN_POINT('Ctrl Pts',(0.683504668020099,-2.57425440705279,
8.86654584966058));
#405928=CARTESIAN_POINT('Ctrl Pts',(0.683939681183841,-2.56834383040285,
8.87215952290715));
#405929=CARTESIAN_POINT('Ctrl Pts',(0.682528638916271,-2.57897124462358,
8.85049129520029));
#405930=CARTESIAN_POINT('Ctrl Pts',(0.686529951896168,-2.5832245500041,
8.85711686593484));
#405931=CARTESIAN_POINT('Ctrl Pts',(0.693929685372921,-2.57894147790724,
8.85933012996512));
#405932=CARTESIAN_POINT('Origin',(0.658710630307072,-2.57903950451467,8.85049129520029));
#405933=CARTESIAN_POINT('Ctrl Pts',(0.653715973115287,-2.65144443664272,
8.78727029226991));
#405934=CARTESIAN_POINT('Ctrl Pts',(0.652299308087893,-2.65718450945398,
8.79393457792714));
#405935=CARTESIAN_POINT('Ctrl Pts',(0.643661112117213,-2.65703964555119,
8.79610912703474));
#405936=CARTESIAN_POINT('Ctrl Pts',(0.659418052229611,-2.62834063393785,
8.80838214965002));
#405937=CARTESIAN_POINT('Ctrl Pts',(0.658001622475823,-2.63407975346255,
8.81501364461996));
#405938=CARTESIAN_POINT('Ctrl Pts',(0.649397808304912,-2.63392745668914,
8.81722098428721));
#405939=CARTESIAN_POINT('Ctrl Pts',(0.665128007518977,-2.60520491838319,
8.82945683644723));
#405940=CARTESIAN_POINT('Ctrl Pts',(0.66371714568474,-2.61092147769581,
8.83607469902391));
#405941=CARTESIAN_POINT('Ctrl Pts',(0.655143182195968,-2.61078294036944,
8.83829567148519));
#405942=CARTESIAN_POINT('Ctrl Pts',(0.670846486662646,-2.58203466569846,
8.85049129520029));
#405943=CARTESIAN_POINT('Ctrl Pts',(0.669447239426466,-2.58770416474116,
8.85711686593484));
#405944=CARTESIAN_POINT('Ctrl Pts',(0.660897934588214,-2.58760342300925,
8.85933012996512));
#405945=CARTESIAN_POINT('Origin',(0.641580116759713,-2.64844927545893,8.78727029226991));
#405946=CARTESIAN_POINT('Ctrl Pts',(0.650400330943821,-2.66487874754016,
8.75374538247848));
#405947=CARTESIAN_POINT('Ctrl Pts',(0.648592262248902,-2.67225948368109,
8.75304829418603));
#405948=CARTESIAN_POINT('Ctrl Pts',(0.64116393718026,-2.6740175024192,8.75272238421917));
#405949=CARTESIAN_POINT('Ctrl Pts',(0.650084046247561,-2.66616027822844,
8.76769408445017));
#405950=CARTESIAN_POINT('Ctrl Pts',(0.648229808234099,-2.67372658223775,
8.76974318093967));
#405951=CARTESIAN_POINT('Ctrl Pts',(0.640925106754247,-2.67563961479641,
8.77077869880429));
#405952=CARTESIAN_POINT('Ctrl Pts',(0.651705141439437,-2.65959188196376,
8.78108014887994));
#405953=CARTESIAN_POINT('Ctrl Pts',(0.650137431720011,-2.66600495638528,
8.78639403366327));
#405954=CARTESIAN_POINT('Ctrl Pts',(0.642152715147357,-2.66733400754429,
8.78812224174742));
#405955=CARTESIAN_POINT('Ctrl Pts',(0.65436175856437,-2.64882773046581,
8.78944554828685));
#405956=CARTESIAN_POINT('Ctrl Pts',(0.653045988551392,-2.65423376106967,
8.79673892988685));
#405957=CARTESIAN_POINT('Ctrl Pts',(0.644142204117193,-2.65375818030291,
8.79894799272499));
#405958=CARTESIAN_POINT('Origin',(0.638220125503606,-2.66206335788654,8.75721825406948));
#405959=CARTESIAN_POINT('Origin',(0.638220125503606,-2.66206335788654,9.));
#405960=CARTESIAN_POINT('Origin',(0.638220125503606,-2.66206335788654,7.51860402984325));
#405961=CARTESIAN_POINT('Ctrl Pts',(0.658718561459868,-2.66617001169015,
7.50366195182966));
#405962=CARTESIAN_POINT('Ctrl Pts',(0.659596893130815,-2.66972506797464,
7.50000065167735));
#405963=CARTESIAN_POINT('Ctrl Pts',(0.659596893130701,-2.66972506797467,
7.49482233047108));
#405964=CARTESIAN_POINT('Ctrl Pts',(0.652005683757201,-2.66937798185144,
7.50215800491337));
#405965=CARTESIAN_POINT('Ctrl Pts',(0.65034181292054,-2.67201165438486,
7.49877273257267));
#405966=CARTESIAN_POINT('Ctrl Pts',(0.646990465679411,-2.67283968096613,
7.49481816995647));
#405967=CARTESIAN_POINT('Ctrl Pts',(0.649680941710166,-2.66779507605612,
7.51043025814043));
#405968=CARTESIAN_POINT('Ctrl Pts',(0.646783717304577,-2.67286447915022,
7.51006209594514));
#405969=CARTESIAN_POINT('Ctrl Pts',(0.641131910556243,-2.67421948861213,
7.50731281821701));
#405970=CARTESIAN_POINT('Ctrl Pts',(0.650356343923175,-2.66505705167055,
7.51860402984326));
#405971=CARTESIAN_POINT('Ctrl Pts',(0.648533957547086,-2.67244487444095,
7.51860402984326));
#405972=CARTESIAN_POINT('Ctrl Pts',(0.641134372652019,-2.67421889833351,
7.51860402984327));
#405973=CARTESIAN_POINT('Origin',(0.,0.,7.5));
#405974=CARTESIAN_POINT('Origin',(0.834899689636865,-2.53374831658167,7.5));
#405975=CARTESIAN_POINT('',(0.834899689636865,-2.53374831658167,7.59394543036555));
#405976=CARTESIAN_POINT('',(0.834899689636865,-2.53374831658167,8.85049129520029));
#405977=CARTESIAN_POINT('',(0.834899689636865,-2.53374831658167,7.5));
#405978=CARTESIAN_POINT('',(0.82225147186004,-2.60411303347871,8.78727029226991));
#405979=CARTESIAN_POINT('Ctrl Pts',(0.834899689636865,-2.53374831658167,
8.85049129520029));
#405980=CARTESIAN_POINT('Ctrl Pts',(0.830677488574773,-2.55723731619084,
8.82945686509571));
#405981=CARTESIAN_POINT('Ctrl Pts',(0.826461564325102,-2.58069139656183,
8.80838212259895));
#405982=CARTESIAN_POINT('Ctrl Pts',(0.82225147186004,-2.60411303347871,
8.78727029226991));
#405983=CARTESIAN_POINT('',(0.819770641322299,-2.61791441969278,8.75721825406948));
#405984=CARTESIAN_POINT('Origin',(0.827236519635628,-2.57638129654257,8.75937679713113));
#405985=CARTESIAN_POINT('',(0.819770641322299,-2.61791441969278,7.51860402984325));
#405986=CARTESIAN_POINT('',(0.819770641322299,-2.61791441969278,7.5));
#405987=CARTESIAN_POINT('Ctrl Pts',(0.819770641322299,-2.61791441969278,
7.51860402984325));
#405988=CARTESIAN_POINT('Ctrl Pts',(0.821718947867565,-2.6070755773432,
7.52834476460825));
#405989=CARTESIAN_POINT('Ctrl Pts',(0.823668519225332,-2.59622969857357,
7.53807742314407));
#405990=CARTESIAN_POINT('Ctrl Pts',(0.825619397863352,-2.58537654712672,
7.54780169004674));
#405991=CARTESIAN_POINT('Ctrl Pts',(0.828709484189983,-2.5681857417977,
7.5632044032688));
#405992=CARTESIAN_POINT('Ctrl Pts',(0.831802854243305,-2.55097666840083,
7.57858609112103));
#405993=CARTESIAN_POINT('Ctrl Pts',(0.834899689636865,-2.53374831658167,
7.59394543036555));
#405994=CARTESIAN_POINT('Origin',(1.04723789307866,-2.71775565323223,7.5));
#405995=CARTESIAN_POINT('',(0.908826823579973,-2.58834572998873,8.75721825406948));
#405996=CARTESIAN_POINT('',(0.898583897763467,-2.5787689219451,8.78727029226991));
#405997=CARTESIAN_POINT('Origin',(0.872583531618111,-2.55445941115698,8.7565864062094));
#405998=CARTESIAN_POINT('',(0.846361565593617,-2.5299427115692,8.85049129520029));
#405999=CARTESIAN_POINT('Ctrl Pts',(0.898583897763467,-2.5787689219451,
8.78727029226991));
#406000=CARTESIAN_POINT('Ctrl Pts',(0.881201144631321,-2.56251660371117,
8.80838212259895));
#406001=CARTESIAN_POINT('Ctrl Pts',(0.863794313055989,-2.54624177290295,
8.82945686509571));
#406002=CARTESIAN_POINT('Ctrl Pts',(0.846361565593617,-2.5299427115692,
8.85049129520029));
#406003=CARTESIAN_POINT('',(0.846361565593617,-2.5299427115692,7.59394543036555));
#406004=CARTESIAN_POINT('',(0.846361565593617,-2.5299427115692,7.5));
#406005=CARTESIAN_POINT('',(0.908826823579973,-2.58834572998873,7.51860402984325));
#406006=CARTESIAN_POINT('Ctrl Pts',(0.846361565593617,-2.5299427115692,
7.59394543036555));
#406007=CARTESIAN_POINT('Ctrl Pts',(0.859147870308745,-2.54189749753932,
7.57858609112103));
#406008=CARTESIAN_POINT('Ctrl Pts',(0.871919867225465,-2.55383890617555,
7.56320440326857));
#406009=CARTESIAN_POINT('Ctrl Pts',(0.884678306195284,-2.56576763856503,
7.54780169004651));
#406010=CARTESIAN_POINT('Ctrl Pts',(0.892733151079782,-2.57329866091762,
7.53807742314383));
#406011=CARTESIAN_POINT('Ctrl Pts',(0.9007825984274,-2.58082463674584,7.52834476460825));
#406012=CARTESIAN_POINT('Ctrl Pts',(0.908826823579971,-2.58834572998873,
7.51860402984325));
#406013=CARTESIAN_POINT('',(0.908826823579973,-2.58834572998873,7.5));
#406014=CARTESIAN_POINT('Origin',(0.841666242052041,-2.53496461975633,7.5));
#406015=CARTESIAN_POINT('Ctrl Pts',(0.846361565593617,-2.5299427115692,
8.85049129520029));
#406016=CARTESIAN_POINT('Ctrl Pts',(0.846220103731495,-2.52981044925243,
8.85097269580138));
#406017=CARTESIAN_POINT('Ctrl Pts',(0.846074682046675,-2.52968599986464,
8.85143669361005));
#406018=CARTESIAN_POINT('Ctrl Pts',(0.845918035884,-2.529564297167,8.8519052845931));
#406019=CARTESIAN_POINT('Ctrl Pts',(0.845611645923948,-2.52932625440854,
8.85282181883899));
#406020=CARTESIAN_POINT('Ctrl Pts',(0.845270075579139,-2.52910499860577,
8.85372622499635));
#406021=CARTESIAN_POINT('Ctrl Pts',(0.844879582375002,-2.52890999884467,
8.8546225773507));
#406022=CARTESIAN_POINT('Ctrl Pts',(0.844555408785934,-2.52874811696874,
8.85536669723986));
#406023=CARTESIAN_POINT('Ctrl Pts',(0.844197459081652,-2.52860426486191,
8.85610498449051));
#406024=CARTESIAN_POINT('Ctrl Pts',(0.843794856243094,-2.52849127326612,
8.85681338218371));
#406025=CARTESIAN_POINT('Ctrl Pts',(0.843429493534804,-2.52838873321548,
8.85745625420284));
#406026=CARTESIAN_POINT('Ctrl Pts',(0.843022934952063,-2.52830974613275,
8.85808743050665));
#406027=CARTESIAN_POINT('Ctrl Pts',(0.842558141777651,-2.5282772800014,
8.8586680450841));
#406028=CARTESIAN_POINT('Ctrl Pts',(0.842343696282456,-2.52826230083217,
8.85893592806395));
#406029=CARTESIAN_POINT('Ctrl Pts',(0.842116734248318,-2.52825743506811,
8.85919241173848));
#406030=CARTESIAN_POINT('Ctrl Pts',(0.841874992353052,-2.52826642160603,
8.85943017985534));
#406031=CARTESIAN_POINT('Ctrl Pts',(0.841548569231186,-2.52827855609252,
8.8597512372));
#406032=CARTESIAN_POINT('Ctrl Pts',(0.841186913474463,-2.52831689643641,
8.86004599534706));
#406033=CARTESIAN_POINT('Ctrl Pts',(0.84079546822707,-2.52839133904788,
8.86026130871721));
#406034=CARTESIAN_POINT('Ctrl Pts',(0.840652149085989,-2.5284185945867,
8.86034014101236));
#406035=CARTESIAN_POINT('Ctrl Pts',(0.840502681555632,-2.52845108692915,
8.86040910639693));
#406036=CARTESIAN_POINT('Ctrl Pts',(0.84035120925051,-2.5284882595412,8.86046313645507));
#406037=CARTESIAN_POINT('Ctrl Pts',(0.840114837986938,-2.52854626709098,
8.8605474499083));
#406038=CARTESIAN_POINT('Ctrl Pts',(0.839867167649147,-2.52861739795951,
8.86059655985669));
#406039=CARTESIAN_POINT('Ctrl Pts',(0.839624001221678,-2.52869680873284,
8.86059725258816));
#406040=CARTESIAN_POINT('Ctrl Pts',(0.839380272982615,-2.52877640297677,
8.86059794692011));
#406041=CARTESIAN_POINT('Ctrl Pts',(0.839139191271985,-2.52886772364964,
8.86056369958366));
#406042=CARTESIAN_POINT('Ctrl Pts',(0.838912571788422,-2.52896227098934,
8.86048590497774));
#406043=CARTESIAN_POINT('Ctrl Pts',(0.838853430850487,-2.52898694502999,
8.86046560290182));
#406044=CARTESIAN_POINT('Ctrl Pts',(0.838794540355868,-2.52901224341473,
8.86044257503091));
#406045=CARTESIAN_POINT('Ctrl Pts',(0.838737707112953,-2.52903735424157,
8.86041778462583));
#406046=CARTESIAN_POINT('Ctrl Pts',(0.838355289912312,-2.52920631894625,
8.860250975962));
#406047=CARTESIAN_POINT('Ctrl Pts',(0.838014836059376,-2.52938976813877,
8.8599848982295));
#406048=CARTESIAN_POINT('Ctrl Pts',(0.837722263530355,-2.5295748888075,
8.85968173251461));
#406049=CARTESIAN_POINT('Ctrl Pts',(0.837567509424911,-2.52967280703511,
8.85952137522076));
#406050=CARTESIAN_POINT('Ctrl Pts',(0.837423066472669,-2.52977291898358,
8.85934740853961));
#406051=CARTESIAN_POINT('Ctrl Pts',(0.83729008609642,-2.52987253518028,
8.8591675900182));
#406052=CARTESIAN_POINT('Ctrl Pts',(0.83675610076395,-2.53027254598948,
8.85844552518695));
#406053=CARTESIAN_POINT('Ctrl Pts',(0.836374948810173,-2.53068474902437,
8.85759444184123));
#406054=CARTESIAN_POINT('Ctrl Pts',(0.836094365694051,-2.53104875090687,
8.85683498915137));
#406055=CARTESIAN_POINT('Ctrl Pts',(0.836065003418205,-2.53108684273445,
8.85675551444997));
#406056=CARTESIAN_POINT('Ctrl Pts',(0.836036760374328,-2.5311244155668,
8.85667699793651));
#406057=CARTESIAN_POINT('Ctrl Pts',(0.836009588723137,-2.53116140540471,
8.85659965593547));
#406058=CARTESIAN_POINT('Ctrl Pts',(0.83564282438883,-2.53166069612428,
8.85555568965886));
#406059=CARTESIAN_POINT('Ctrl Pts',(0.835362448600069,-2.53219351346653,
8.85434650606346));
#406060=CARTESIAN_POINT('Ctrl Pts',(0.835161575571271,-2.53275959732744,
8.85297329937117));
#406061=CARTESIAN_POINT('Ctrl Pts',(0.835048596731946,-2.53307798500721,
8.85220095427747));
#406062=CARTESIAN_POINT('Ctrl Pts',(0.834961018414397,-2.53340713159064,
8.85137579139183));
#406063=CARTESIAN_POINT('Ctrl Pts',(0.834899689636865,-2.53374831658167,
8.85049129520029));
#406064=CARTESIAN_POINT('Origin',(0.841666242052041,-2.53496461975633,7.59394543036555));
#406065=CARTESIAN_POINT('Ctrl Pts',(0.845950854086167,-2.52955870944533,
7.59443877723642));
#406066=CARTESIAN_POINT('Ctrl Pts',(0.841720920735444,-2.52560385704642,
7.58783886950016));
#406067=CARTESIAN_POINT('Ctrl Pts',(0.83464506505906,-2.53029549300669,
7.58559994247159));
#406068=CARTESIAN_POINT('Ctrl Pts',(0.869041936146793,-2.55114813266053,
7.56670252222135));
#406069=CARTESIAN_POINT('Ctrl Pts',(0.864818116250616,-2.54719899614619,
7.56004874999028));
#406070=CARTESIAN_POINT('Ctrl Pts',(0.857688526813998,-2.55190062477045,
7.55786368756704));
#406071=CARTESIAN_POINT('Ctrl Pts',(0.892089897918742,-2.5726972397849,
7.53888913333557));
#406072=CARTESIAN_POINT('Ctrl Pts',(0.887840975654144,-2.56872463335888,
7.53222002137276));
#406073=CARTESIAN_POINT('Ctrl Pts',(0.88069057139642,-2.57346532567864,
7.53005029815327));
#406074=CARTESIAN_POINT('Ctrl Pts',(0.915093696466176,-2.59420505570681,
7.51101258149734));
#406075=CARTESIAN_POINT('Ctrl Pts',(0.910793269543267,-2.59018429407247,
7.5043616886572));
#406076=CARTESIAN_POINT('Ctrl Pts',(0.903650005808594,-2.59498859056224,
7.50217374673251));
#406077=CARTESIAN_POINT('',(0.902424861598309,-2.5938400807503,7.50366116523517));
#406078=CARTESIAN_POINT('Ctrl Pts',(0.908826823579973,-2.58834572998873,
7.51860402984325));
#406079=CARTESIAN_POINT('Ctrl Pts',(0.909149402631517,-2.58864733108503,
7.51734760759493));
#406080=CARTESIAN_POINT('Ctrl Pts',(0.909400265220393,-2.58896333080256,
7.51608817408572));
#406081=CARTESIAN_POINT('Ctrl Pts',(0.909568375706178,-2.58930130513209,
7.51481005913119));
#406082=CARTESIAN_POINT('Ctrl Pts',(0.909720654201332,-2.58960745035594,
7.51365231206383));
#406083=CARTESIAN_POINT('Ctrl Pts',(0.909805471833591,-2.58993194624438,
7.51247773061042));
#406084=CARTESIAN_POINT('Ctrl Pts',(0.909785636131782,-2.59027851570741,
7.51129758471022));
#406085=CARTESIAN_POINT('Ctrl Pts',(0.909760982619756,-2.59070926197024,
7.50983079813402));
#406086=CARTESIAN_POINT('Ctrl Pts',(0.90956244776073,-2.59115961536516,
7.50839324291155));
#406087=CARTESIAN_POINT('Ctrl Pts',(0.909113147813133,-2.5915996078967,
7.50715379678855));
#406088=CARTESIAN_POINT('Ctrl Pts',(0.90890558418361,-2.5918028717682,7.50658120839351));
#406089=CARTESIAN_POINT('Ctrl Pts',(0.908608347826973,-2.59202603157119,
7.50598221009429));
#406090=CARTESIAN_POINT('Ctrl Pts',(0.908214855547679,-2.59224558605754,
7.50545747549611));
#406091=CARTESIAN_POINT('Ctrl Pts',(0.908004875887722,-2.5923627471273,
7.50517746087247));
#406092=CARTESIAN_POINT('Ctrl Pts',(0.907765307937765,-2.59248032881998,
7.50491486231392));
#406093=CARTESIAN_POINT('Ctrl Pts',(0.907501760933578,-2.59259371998976,
7.50468370960993));
#406094=CARTESIAN_POINT('Ctrl Pts',(0.907107675031134,-2.59276327555579,
7.50433806340447));
#406095=CARTESIAN_POINT('Ctrl Pts',(0.906647935572143,-2.5929280342173,
7.50405484070984));
#406096=CARTESIAN_POINT('Ctrl Pts',(0.906153263468412,-2.59307622538893,
7.50385766036132));
#406097=CARTESIAN_POINT('Ctrl Pts',(0.906100365975858,-2.59309207213132,
7.50383657498791));
#406098=CARTESIAN_POINT('Ctrl Pts',(0.90604709656214,-2.59310773623329,
7.50381643264937));
#406099=CARTESIAN_POINT('Ctrl Pts',(0.905993512717888,-2.59312320855992,
7.50379723213559));
#406100=CARTESIAN_POINT('Ctrl Pts',(0.905635823029044,-2.5932264914015,
7.50366906242519));
#406101=CARTESIAN_POINT('Ctrl Pts',(0.905256142261199,-2.59332278454904,
7.50358235568538));
#406102=CARTESIAN_POINT('Ctrl Pts',(0.904887945654187,-2.59340680223421,
7.5035341175365));
#406103=CARTESIAN_POINT('Ctrl Pts',(0.904335876513782,-2.59353277724414,
7.50346178989176));
#406104=CARTESIAN_POINT('Ctrl Pts',(0.903736619435742,-2.5936448243463,
7.50346967198527));
#406105=CARTESIAN_POINT('Ctrl Pts',(0.903144950082912,-2.59373671834596,
7.50354272648692));
#406106=CARTESIAN_POINT('Ctrl Pts',(0.902901584231261,-2.59377451625012,
7.50357277531559));
#406107=CARTESIAN_POINT('Ctrl Pts',(0.9026598472222,-2.5938089944534,7.50361331098761));
#406108=CARTESIAN_POINT('Ctrl Pts',(0.902424861598775,-2.59384008075164,
7.50366116523658));
#406109=CARTESIAN_POINT('',(0.842588855338652,-2.53774338397775,7.57603338622103));
#406110=CARTESIAN_POINT('Origin',(0.845370739448648,-2.5461310302743,7.5848687342763));
#406111=CARTESIAN_POINT('Ctrl Pts',(0.902424861643628,-2.59384008078544,
7.50366116529969));
#406112=CARTESIAN_POINT('Ctrl Pts',(0.882511501228937,-2.57517230438344,
7.52783573079709));
#406113=CARTESIAN_POINT('Ctrl Pts',(0.862567095273873,-2.55647430140458,
7.55196141284069));
#406114=CARTESIAN_POINT('Ctrl Pts',(0.842588856456747,-2.53774338454123,
7.57603338728831));
#406115=CARTESIAN_POINT('Ctrl Pts',(0.846992701390038,-2.53077349621436,
7.59639677331372));
#406116=CARTESIAN_POINT('Ctrl Pts',(0.835782896743083,-2.5163370078768,
7.59959882295463));
#406117=CARTESIAN_POINT('Ctrl Pts',(0.83489690696676,-2.53461059085095,
7.59642833564546));
#406118=CARTESIAN_POINT('Ctrl Pts',(0.845126734807235,-2.52734810969668,
7.58707626057424));
#406119=CARTESIAN_POINT('Ctrl Pts',(0.83861611782419,-2.52547083573265,
7.58809943920598));
#406120=CARTESIAN_POINT('Ctrl Pts',(0.834444422555743,-2.53079167771301,
7.58710240504252));
#406121=CARTESIAN_POINT('Ctrl Pts',(0.84333419920026,-2.53315435188584,
7.5801537675693));
#406122=CARTESIAN_POINT('Ctrl Pts',(0.840720632629399,-2.53201481637711,
7.5820588065976));
#406123=CARTESIAN_POINT('Ctrl Pts',(0.839288810603534,-2.53443906073858,
7.58020924244128));
#406124=CARTESIAN_POINT('Ctrl Pts',(0.84258885507807,-2.53774338319228,
7.57603338509286));
#406125=CARTESIAN_POINT('Ctrl Pts',(0.84258885507807,-2.53774338319228,
7.57603338509286));
#406126=CARTESIAN_POINT('Ctrl Pts',(0.84258885507807,-2.53774338319228,
7.57603338509286));
#406127=CARTESIAN_POINT('Origin',(0.845376155095157,-2.54612923215639,7.5848687342762));
#406128=CARTESIAN_POINT('Ctrl Pts',(0.818248011214847,-2.626385133776,7.51098857897448));
#406129=CARTESIAN_POINT('Ctrl Pts',(0.819289576806601,-2.62059068357862,
7.50433767179956));
#406130=CARTESIAN_POINT('Ctrl Pts',(0.82788781980899,-2.62016846520582,
7.50214974420965));
#406131=CARTESIAN_POINT('Ctrl Pts',(0.823821120043198,-2.59538074787257,
7.53887321589166));
#406132=CARTESIAN_POINT('Ctrl Pts',(0.824850205830722,-2.58965572547184,
7.53220407452059));
#406133=CARTESIAN_POINT('Ctrl Pts',(0.83341612225984,-2.58917823657005,
7.53003438070911));
#406134=CARTESIAN_POINT('Ctrl Pts',(0.829404931296325,-2.56431682211121,
7.56669465659236));
#406135=CARTESIAN_POINT('Ctrl Pts',(0.830427935378149,-2.55862563352851,
7.56004085833304));
#406136=CARTESIAN_POINT('Ctrl Pts',(0.838953795137752,-2.55812928134927,
7.55785582193789));
#406137=CARTESIAN_POINT('Ctrl Pts',(0.834999192440815,-2.53319476138884,
7.59443891967696));
#406138=CARTESIAN_POINT('Ctrl Pts',(0.836023679751206,-2.52749532129125,
7.58783901202978));
#406139=CARTESIAN_POINT('Ctrl Pts',(0.844500483535603,-2.52702311838028,
7.58560008491213));
#406140=CARTESIAN_POINT('',(0.828187489909793,-2.61848858635939,7.50366116523517));
#406141=CARTESIAN_POINT('Ctrl Pts',(0.828187489909906,-2.61848858635974,
7.50366116523554));
#406142=CARTESIAN_POINT('Ctrl Pts',(0.827525969191762,-2.61885808312053,
7.50350835821027));
#406143=CARTESIAN_POINT('Ctrl Pts',(0.826905849903705,-2.61917621843721,
7.50345484955999));
#406144=CARTESIAN_POINT('Ctrl Pts',(0.826308969499699,-2.61945298502424,
7.50349758195598));
#406145=CARTESIAN_POINT('Ctrl Pts',(0.826002725586639,-2.61959498680893,
7.50351950684424));
#406146=CARTESIAN_POINT('Ctrl Pts',(0.825672469016706,-2.61974021217986,
7.50357029184312));
#406147=CARTESIAN_POINT('Ctrl Pts',(0.825350157004229,-2.61987149743226,
7.50365515313924));
#406148=CARTESIAN_POINT('Ctrl Pts',(0.824854310612016,-2.62007346731311,
7.50378570417639));
#406149=CARTESIAN_POINT('Ctrl Pts',(0.824362842393546,-2.62024869536167,
7.50400001621911));
#406150=CARTESIAN_POINT('Ctrl Pts',(0.823912397737676,-2.62038170562562,
7.50428903009635));
#406151=CARTESIAN_POINT('Ctrl Pts',(0.823862401846387,-2.6203964687416,
7.50432110841318));
#406152=CARTESIAN_POINT('Ctrl Pts',(0.823812892273602,-2.62041073533621,
7.50435406373354));
#406153=CARTESIAN_POINT('Ctrl Pts',(0.823763904819425,-2.62042450145567,
7.50438785222352));
#406154=CARTESIAN_POINT('Ctrl Pts',(0.823464812865309,-2.62050855023183,
7.50459414719561));
#406155=CARTESIAN_POINT('Ctrl Pts',(0.823180282494888,-2.62057478447335,
7.50483629897752));
#406156=CARTESIAN_POINT('Ctrl Pts',(0.822921512356913,-2.62062194852715,
7.5050991045531));
#406157=CARTESIAN_POINT('Ctrl Pts',(0.82235063944154,-2.62072599716703,
7.50567888004914));
#406158=CARTESIAN_POINT('Ctrl Pts',(0.821882736099762,-2.6207418454673,
7.50637912803145));
#406159=CARTESIAN_POINT('Ctrl Pts',(0.821510747489535,-2.62069958740676,
7.50710440483569));
#406160=CARTESIAN_POINT('Ctrl Pts',(0.821419528497299,-2.62068922489138,
7.50728225710685));
#406161=CARTESIAN_POINT('Ctrl Pts',(0.821332244757623,-2.62067530700927,
7.50746498566954));
#406162=CARTESIAN_POINT('Ctrl Pts',(0.821250868156086,-2.62065857004476,
7.50764697238949));
#406163=CARTESIAN_POINT('Ctrl Pts',(0.820813409941663,-2.62056859672971,
7.50862528291182));
#406164=CARTESIAN_POINT('Ctrl Pts',(0.820506113419842,-2.62039304298326,
7.50965856837422));
#406165=CARTESIAN_POINT('Ctrl Pts',(0.820281832715819,-2.62017852063152,
7.51067959873203));
#406166=CARTESIAN_POINT('Ctrl Pts',(0.820158410761503,-2.62006046871077,
7.51124147302579));
#406167=CARTESIAN_POINT('Ctrl Pts',(0.820060398756856,-2.61993027313354,
7.51180065547253));
#406168=CARTESIAN_POINT('Ctrl Pts',(0.819981887633074,-2.6197938087974,
7.51235175716501));
#406169=CARTESIAN_POINT('Ctrl Pts',(0.819710600425289,-2.61932227015509,
7.51425603304536));
#406170=CARTESIAN_POINT('Ctrl Pts',(0.819645060131596,-2.61871663751266,
7.5162690050518));
#406171=CARTESIAN_POINT('Ctrl Pts',(0.819751779839004,-2.61802712335916,
7.51827788969244));
#406172=CARTESIAN_POINT('Ctrl Pts',(0.819757555711242,-2.61798980555017,
7.51838661432545));
#406173=CARTESIAN_POINT('Ctrl Pts',(0.819763843816376,-2.61795223565927,
7.51849533314856));
#406174=CARTESIAN_POINT('Ctrl Pts',(0.819770641322295,-2.61791441969278,
7.51860402984325));
#406175=CARTESIAN_POINT('Ctrl Pts',(0.842588854779764,-2.53774338509928,
7.57603338728985));
#406176=CARTESIAN_POINT('Ctrl Pts',(0.837781180671478,-2.5647037920469,
7.55196141284922));
#406177=CARTESIAN_POINT('Ctrl Pts',(0.832980934536062,-2.59161758558423,
7.52783573083104));
#406178=CARTESIAN_POINT('Ctrl Pts',(0.828187489894095,-2.61848858641645,
7.50366116530176));
#406179=CARTESIAN_POINT('Origin',(2.91153398701384E-16,-8.76907647894213E-16,
7.49482233047033));
#406180=CARTESIAN_POINT('Origin',(0.899520491555409,-2.58549204896707,7.49482233047033));
#406181=CARTESIAN_POINT('Origin',(0.,0.,7.50366116523517));
#406182=CARTESIAN_POINT('Origin',(0.82552204590669,-2.61006122566541,7.49482233047033));
#406183=CARTESIAN_POINT('Ctrl Pts',(0.908826050988849,-2.58834500757948,
7.51860402984325));
#406184=CARTESIAN_POINT('Ctrl Pts',(0.914383648054368,-2.59354206452427,
7.51860402984325));
#406185=CARTESIAN_POINT('Ctrl Pts',(0.921552651160842,-2.59099222521767,
7.51860402984325));
#406186=CARTESIAN_POINT('Ctrl Pts',(0.910889625574226,-2.5902747093615,
7.51041458714367));
#406187=CARTESIAN_POINT('Ctrl Pts',(0.916082063685389,-2.59293796906005,
7.51004642900442));
#406188=CARTESIAN_POINT('Ctrl Pts',(0.921554628286784,-2.59099152200227,
7.5072913648301));
#406189=CARTESIAN_POINT('Ctrl Pts',(0.9097942691111,-2.5928677638187,7.50215815450137));
#406190=CARTESIAN_POINT('Ctrl Pts',(0.91262396703454,-2.59416809998427,
7.49877163671531));
#406191=CARTESIAN_POINT('Ctrl Pts',(0.915882595552394,-2.5930344052383,
7.4948158853317));
#406192=CARTESIAN_POINT('Ctrl Pts',(0.902424680702065,-2.59383956080161,
7.50366171572174));
#406193=CARTESIAN_POINT('Ctrl Pts',(0.903627891059863,-2.59729794873417,
7.50000045605858));
#406194=CARTESIAN_POINT('Ctrl Pts',(0.903627891059981,-2.59729794873413,
7.49482233047317));
#406195=CARTESIAN_POINT('Origin',(0.917363775473747,-2.57921498783032,7.51860402984325));
#406196=CARTESIAN_POINT('Origin',(0.917363775473747,-2.57921498783032,9.));
#406197=CARTESIAN_POINT('Origin',(0.917363775473747,-2.57921498783032,8.75721825406948));
#406198=CARTESIAN_POINT('Ctrl Pts',(0.896628055005695,-2.57694023016136,
8.78942910404912));
#406199=CARTESIAN_POINT('Ctrl Pts',(0.900684690092706,-2.58076071972063,
8.7967269950169));
#406200=CARTESIAN_POINT('Ctrl Pts',(0.90789356058949,-2.57549710193981,
8.79893251111266));
#406201=CARTESIAN_POINT('Ctrl Pts',(0.904658967512584,-2.58444888270673,
8.78111911759584));
#406202=CARTESIAN_POINT('Ctrl Pts',(0.909473258913846,-2.58897269840027,
8.78644465894814));
#406203=CARTESIAN_POINT('Ctrl Pts',(0.916893176767956,-2.58570768219606,
8.78817647674132));
#406204=CARTESIAN_POINT('Ctrl Pts',(0.909664023763959,-2.58912845404804,
8.76780923932029));
#406205=CARTESIAN_POINT('Ctrl Pts',(0.91535058097983,-2.59446491390464,
8.76988516158373));
#406206=CARTESIAN_POINT('Ctrl Pts',(0.922522564001213,-2.59207764769887,
8.77093053738833));
#406207=CARTESIAN_POINT('Ctrl Pts',(0.908688106295134,-2.58821600167965,
8.75371302330492));
#406208=CARTESIAN_POINT('Ctrl Pts',(0.91423457591542,-2.59342204394983,
8.75300828287559));
#406209=CARTESIAN_POINT('Ctrl Pts',(0.921424947711537,-2.59083494272107,
8.75267964240738));
#406210=CARTESIAN_POINT('Origin',(0.907120849657241,-2.56963817978669,8.78727029226991));
#406211=CARTESIAN_POINT('Ctrl Pts',(0.846361565593617,-2.5299427115692,
8.85049129520029));
#406212=CARTESIAN_POINT('Ctrl Pts',(0.850627167658232,-2.53393091307482,
8.85711686593484));
#406213=CARTESIAN_POINT('Ctrl Pts',(0.857737280217499,-2.52918253845728,
8.85933012996512));
#406214=CARTESIAN_POINT('Ctrl Pts',(0.863794336451385,-2.54624179477689,
8.82945683644722));
#406215=CARTESIAN_POINT('Ctrl Pts',(0.868095345592174,-2.55026310076631,
8.8360746990239));
#406216=CARTESIAN_POINT('Ctrl Pts',(0.875205505457256,-2.54546959795619,
8.8382956714852));
#406217=CARTESIAN_POINT('Ctrl Pts',(0.881201122358403,-2.5625165828867,
8.80838214965003));
#406218=CARTESIAN_POINT('Ctrl Pts',(0.885519105289387,-2.56655375882711,
8.81501364461992));
#406219=CARTESIAN_POINT('Ctrl Pts',(0.892646776397513,-2.56173243979915,
8.81722098428721));
#406220=CARTESIAN_POINT('Ctrl Pts',(0.898583897763467,-2.5787689219451,
8.78727029226991));
#406221=CARTESIAN_POINT('Ctrl Pts',(0.902902597925574,-2.58280676847366,
8.79393457792714));
#406222=CARTESIAN_POINT('Ctrl Pts',(0.91006313890143,-2.57797292237441,
8.79610912703474));
#406223=CARTESIAN_POINT('Origin',(0.854898517487391,-2.52081196941079,8.85049129520029));
#406224=CARTESIAN_POINT('Ctrl Pts',(0.834899689636865,-2.53374831658167,
8.85049129520029));
#406225=CARTESIAN_POINT('Ctrl Pts',(0.833866563355046,-2.53949581710876,
8.85711686593484));
#406226=CARTESIAN_POINT('Ctrl Pts',(0.82532836943557,-2.53994303820321,
8.85933012996512));
#406227=CARTESIAN_POINT('Ctrl Pts',(0.835813681545056,-2.52866358583139,
8.86332496987232));
#406228=CARTESIAN_POINT('Ctrl Pts',(0.83152541263115,-2.5303848191389,8.86648636486737));
#406229=CARTESIAN_POINT('Ctrl Pts',(0.827902161459422,-2.52572132765299,
8.87206031107457));
#406230=CARTESIAN_POINT('Ctrl Pts',(0.842562205427872,-2.52639043132742,
8.86341338519876));
#406231=CARTESIAN_POINT('Ctrl Pts',(0.8470333805202,-2.52517303084769,8.86654584966058));
#406232=CARTESIAN_POINT('Ctrl Pts',(0.847088807956572,-2.51924672672229,
8.87215952290715));
#406233=CARTESIAN_POINT('Ctrl Pts',(0.846361565593616,-2.5299427115692,
8.85049129520029));
#406234=CARTESIAN_POINT('Ctrl Pts',(0.850627167658232,-2.53393091307482,
8.85711686593484));
#406235=CARTESIAN_POINT('Ctrl Pts',(0.857737280217499,-2.52918253845728,
8.85933012996512));
#406236=CARTESIAN_POINT('Origin',(0.822596867063817,-2.53153685626412,8.85049129520029));
#406237=CARTESIAN_POINT('Ctrl Pts',(0.82225147186004,-2.60411303347871,
8.78727029226991));
#406238=CARTESIAN_POINT('Ctrl Pts',(0.821205485250605,-2.6099320787347,
8.79393457792714));
#406239=CARTESIAN_POINT('Ctrl Pts',(0.812575755917871,-2.61034096358642,
8.79610912703474));
#406240=CARTESIAN_POINT('Ctrl Pts',(0.826461569719588,-2.58069136655116,
8.80838214965001));
#406241=CARTESIAN_POINT('Ctrl Pts',(0.825415756823118,-2.58650944540513,
8.81501364461986));
#406242=CARTESIAN_POINT('Ctrl Pts',(0.816819862423375,-2.58690870980845,
8.81722098428722));
#406243=CARTESIAN_POINT('Ctrl Pts',(0.83067748290842,-2.55723734771396,
8.82945683644724));
#406244=CARTESIAN_POINT('Ctrl Pts',(0.829635781053824,-2.56303255597043,
8.83607469902391));
#406245=CARTESIAN_POINT('Ctrl Pts',(0.821070557575618,-2.56344363901071,
8.83829567148519));
#406246=CARTESIAN_POINT('Ctrl Pts',(0.834899689636865,-2.53374831658167,
8.85049129520029));
#406247=CARTESIAN_POINT('Ctrl Pts',(0.833866563355046,-2.53949581710876,
8.85711686593484));
#406248=CARTESIAN_POINT('Ctrl Pts',(0.82532836943557,-2.53994303820321,
8.85933012996512));
#406249=CARTESIAN_POINT('Origin',(0.809948649286992,-2.60190157316116,8.78727029226991));
#406250=CARTESIAN_POINT('Ctrl Pts',(0.819803381285507,-2.61773217606689,
8.75374538247848));
#406251=CARTESIAN_POINT('Ctrl Pts',(0.818471912849805,-2.62521359105286,
8.75304829418602));
#406252=CARTESIAN_POINT('Ctrl Pts',(0.811171486718982,-2.62744393217416,
8.75272238421917));
#406253=CARTESIAN_POINT('Ctrl Pts',(0.819569854383186,-2.619031338143,8.76769408445019));
#406254=CARTESIAN_POINT('Ctrl Pts',(0.818204200862904,-2.62670089780666,
8.76974318093968));
#406255=CARTESIAN_POINT('Ctrl Pts',(0.811037076092532,-2.62907801366545,
8.77077869880429));
#406256=CARTESIAN_POINT('Ctrl Pts',(0.820766780267531,-2.61237257342734,
8.78108014887992));
#406257=CARTESIAN_POINT('Ctrl Pts',(0.819613178664803,-2.61887291500624,
8.78639403366326));
#406258=CARTESIAN_POINT('Ctrl Pts',(0.811730020148829,-2.62071081803441,
8.78812224174742));
#406259=CARTESIAN_POINT('Ctrl Pts',(0.822728277533278,-2.6014603279895,
8.78944554828685));
#406260=CARTESIAN_POINT('Ctrl Pts',(0.821761576480921,-2.60693955299787,
8.79673892988686));
#406261=CARTESIAN_POINT('Ctrl Pts',(0.812845615262423,-2.60703541679016,
8.79894799272499));
#406262=CARTESIAN_POINT('Origin',(0.807467818749251,-2.61570295937523,8.75721825406948));
#406263=CARTESIAN_POINT('Origin',(0.807467818749251,-2.61570295937523,9.));
#406264=CARTESIAN_POINT('Origin',(0.807467818749251,-2.61570295937523,7.51860402984325));
#406265=CARTESIAN_POINT('Ctrl Pts',(0.828187252682973,-2.61848783631719,
7.50366195182966));
#406266=CARTESIAN_POINT('Ctrl Pts',(0.829291552965492,-2.62197931345388,
7.50000065167736));
#406267=CARTESIAN_POINT('Ctrl Pts',(0.82929155296538,-2.62197931345392,
7.49482233047108));
#406268=CARTESIAN_POINT('Ctrl Pts',(0.821693702661423,-2.62211931091083,
7.50215800491337));
#406269=CARTESIAN_POINT('Ctrl Pts',(0.820201990404422,-2.6248541768521,
7.49877273257264));
#406270=CARTESIAN_POINT('Ctrl Pts',(0.816910580710839,-2.62589522371893,
7.49481816995647));
#406271=CARTESIAN_POINT('Ctrl Pts',(0.819272319923741,-2.62068860409959,
7.51043025814043));
#406272=CARTESIAN_POINT('Ctrl Pts',(0.816705845947828,-2.62593321736634,
7.51006209594516));
#406273=CARTESIAN_POINT('Ctrl Pts',(0.811152467196917,-2.62764755531764,
7.50731281821702));
#406274=CARTESIAN_POINT('Ctrl Pts',(0.819770908625769,-2.61791293211041,
7.51860402984326));
#406275=CARTESIAN_POINT('Ctrl Pts',(0.818425605968019,-2.6254023365026,
7.51860402984327));
#406276=CARTESIAN_POINT('Ctrl Pts',(0.811154886414768,-2.6276468085048,
7.51860402984327));
#406277=CARTESIAN_POINT('Origin',(0.,0.,7.5));
#406278=CARTESIAN_POINT('Origin',(0.995522110700944,-2.47505025214474,7.5));
#406279=CARTESIAN_POINT('',(0.995522110700944,-2.47505025214474,7.59394543036555));
#406280=CARTESIAN_POINT('',(0.995522110700944,-2.47505025214474,8.85049129520029));
#406281=CARTESIAN_POINT('',(0.995522110700944,-2.47505025214474,7.5));
#406282=CARTESIAN_POINT('',(0.987408162934533,-2.54608077127964,8.78727029226991));
#406283=CARTESIAN_POINT('Ctrl Pts',(0.995522110700944,-2.47505025214474,
8.85049129520029));
#406284=CARTESIAN_POINT('Ctrl Pts',(0.99281352997585,-2.49876150843587,
8.82945686509571));
#406285=CARTESIAN_POINT('Ctrl Pts',(0.990108975883521,-2.5224375150774,
8.80838212259895));
#406286=CARTESIAN_POINT('Ctrl Pts',(0.987408162934533,-2.54608077127964,
8.78727029226991));
#406287=CARTESIAN_POINT('',(0.985816687379975,-2.56001274842383,8.75721825406948));
#406288=CARTESIAN_POINT('Origin',(0.990606189908979,-2.51808661906274,8.75937679713083));
#406289=CARTESIAN_POINT('',(0.985816687379975,-2.56001274842383,7.51860402984325));
#406290=CARTESIAN_POINT('',(0.985816687379975,-2.56001274842383,7.5));
#406291=CARTESIAN_POINT('Ctrl Pts',(0.985816687379975,-2.56001274842383,
7.51860402984325));
#406292=CARTESIAN_POINT('Ctrl Pts',(0.987066543906813,-2.54907134720937,
7.52834476460825));
#406293=CARTESIAN_POINT('Ctrl Pts',(0.988317211822481,-2.53812284299513,
7.53807742314407));
#406294=CARTESIAN_POINT('Ctrl Pts',(0.989568718370425,-2.52716699728844,
7.54780169004674));
#406295=CARTESIAN_POINT('Ctrl Pts',(0.991551037104211,-2.50981352980197,
7.5632044032688));
#406296=CARTESIAN_POINT('Ctrl Pts',(0.993535462378795,-2.49244162139226,
7.57858609112103));
#406297=CARTESIAN_POINT('Ctrl Pts',(0.995522110700944,-2.47505025214474,
7.59394543036555));
#406298=CARTESIAN_POINT('Origin',(1.21921343306784,-2.64507497058259,7.5));
#406299=CARTESIAN_POINT('',(1.07279542170607,-2.52479896157612,8.75721825406948));
#406300=CARTESIAN_POINT('',(1.06195995288114,-2.51589809662203,8.78727029226991));
#406301=CARTESIAN_POINT('Origin',(1.03445549157553,-2.49330438151181,8.75658640621066));
#406302=CARTESIAN_POINT('',(1.00671661105395,-2.47051810124197,8.85049129520029));
#406303=CARTESIAN_POINT('Ctrl Pts',(1.06195995288114,-2.51589809662203,
8.78727029226991));
#406304=CARTESIAN_POINT('Ctrl Pts',(1.04357162487516,-2.50079288733602,
8.80838212259896));
#406305=CARTESIAN_POINT('Ctrl Pts',(1.02515782551214,-2.48566675444136,
8.82945686509571));
#406306=CARTESIAN_POINT('Ctrl Pts',(1.00671661105395,-2.47051810124197,
8.85049129520029));
#406307=CARTESIAN_POINT('',(1.00671661105395,-2.47051810124197,7.59394543036555));
#406308=CARTESIAN_POINT('',(1.00671661105395,-2.47051810124197,7.5));
#406309=CARTESIAN_POINT('',(1.07279542170607,-2.52479896157612,7.51860402984325));
#406310=CARTESIAN_POINT('Ctrl Pts',(1.00671661105395,-2.47051810124197,
7.59394543036555));
#406311=CARTESIAN_POINT('Ctrl Pts',(1.02024259070164,-2.48162910346633,
7.57858609112103));
#406312=CARTESIAN_POINT('Ctrl Pts',(1.03375343485911,-2.49272767254576,
7.56320440326857));
#406313=CARTESIAN_POINT('Ctrl Pts',(1.04724993675601,-2.50381446008378,
7.54780169004651));
#406314=CARTESIAN_POINT('Ctrl Pts',(1.05577074635663,-2.51081393345959,
7.53807742314383));
#406315=CARTESIAN_POINT('Ctrl Pts',(1.06428584617825,-2.51780871650103,
7.52834476460825));
#406316=CARTESIAN_POINT('Ctrl Pts',(1.07279542170607,-2.52479896157612,
7.51860402984325));
#406317=CARTESIAN_POINT('',(1.07279542170607,-2.52479896157612,7.5));
#406318=CARTESIAN_POINT('Origin',(1.00235268932044,-2.47583052179232,7.5));
#406319=CARTESIAN_POINT('Ctrl Pts',(1.00671661105395,-2.47051810124197,
8.85049129520029));
#406320=CARTESIAN_POINT('Ctrl Pts',(1.00656696576467,-2.47039517416494,
8.85097269580138));
#406321=CARTESIAN_POINT('Ctrl Pts',(1.00641386936464,-2.4702802976711,8.85143669361005));
#406322=CARTESIAN_POINT('Ctrl Pts',(1.0062497475297,-2.47016888137881,8.8519052845931));
#406323=CARTESIAN_POINT('Ctrl Pts',(1.00592873562878,-2.46995095817687,
8.85282181883899));
#406324=CARTESIAN_POINT('Ctrl Pts',(1.00557369116892,-2.46975204145501,
8.85372622499635));
#406325=CARTESIAN_POINT('Ctrl Pts',(1.00517150659736,-2.46958246132731,
8.85462257735071));
#406326=CARTESIAN_POINT('Ctrl Pts',(1.0048376272503,-2.46944168192822,8.85536669723986));
#406327=CARTESIAN_POINT('Ctrl Pts',(1.00447119635595,-2.46932105929728,
8.85610498449051));
#406328=CARTESIAN_POINT('Ctrl Pts',(1.0040621813117,-2.46923409470727,8.85681338218371));
#406329=CARTESIAN_POINT('Ctrl Pts',(1.00369099951668,-2.46915517420525,
8.85745625420284));
#406330=CARTESIAN_POINT('Ctrl Pts',(1.00328021553239,-2.46910239770779,
8.85808743050665));
#406331=CARTESIAN_POINT('Ctrl Pts',(1.00281429721322,-2.46909977768251,
8.85866804508409));
#406332=CARTESIAN_POINT('Ctrl Pts',(1.00259933260063,-2.46909856885964,
8.85893592806395));
#406333=CARTESIAN_POINT('Ctrl Pts',(1.00237252513376,-2.46910825460028,
8.85919241173848));
#406334=CARTESIAN_POINT('Ctrl Pts',(1.0021318556926,-2.4691327111308,8.85943017985534));
#406335=CARTESIAN_POINT('Ctrl Pts',(1.00180688070127,-2.46916573468691,
8.8597512372));
#406336=CARTESIAN_POINT('Ctrl Pts',(1.00144842447935,-2.46922716762034,
8.86004599534706));
#406337=CARTESIAN_POINT('Ctrl Pts',(1.00106255305269,-2.46932653726459,
8.86026130871721));
#406338=CARTESIAN_POINT('Ctrl Pts',(1.00092127464453,-2.46936291929287,
8.86034014101235));
#406339=CARTESIAN_POINT('Ctrl Pts',(1.00077419600277,-2.46940492129387,
8.86040910639693));
#406340=CARTESIAN_POINT('Ctrl Pts',(1.00062541657118,-2.46945172239471,
8.86046313645507));
#406341=CARTESIAN_POINT('Ctrl Pts',(1.00039324751419,-2.46952475512062,
8.8605474499083));
#406342=CARTESIAN_POINT('Ctrl Pts',(1.00015064341207,-2.46961160813618,
8.86059655985669));
#406343=CARTESIAN_POINT('Ctrl Pts',(0.999913064461816,-2.46970643547805,
8.86059725258816));
#406344=CARTESIAN_POINT('Ctrl Pts',(0.999674936609278,-2.46980148190897,
8.86059794692011));
#406345=CARTESIAN_POINT('Ctrl Pts',(0.999440201162479,-2.46990806111196,
8.86056369958366));
#406346=CARTESIAN_POINT('Ctrl Pts',(0.999220104961803,-2.47001693375417,
8.86048590497774));
#406347=CARTESIAN_POINT('Ctrl Pts',(0.99916266640648,-2.47004534627226,
8.86046560290182));
#406348=CARTESIAN_POINT('Ctrl Pts',(0.999105517781774,-2.4700743658057,
8.86044257503091));
#406349=CARTESIAN_POINT('Ctrl Pts',(0.999050410165051,-2.47010306635803,
8.86041778462584));
#406350=CARTESIAN_POINT('Ctrl Pts',(0.998679604287361,-2.47029618546077,
8.86025097596201));
#406351=CARTESIAN_POINT('Ctrl Pts',(0.998351603563499,-2.4705010706905,
8.8599848982295));
#406352=CARTESIAN_POINT('Ctrl Pts',(0.998071492878086,-2.47070455619526,
8.85968173251461));
#406353=CARTESIAN_POINT('Ctrl Pts',(0.997923330373931,-2.47081218836895,
8.85952137522076));
#406354=CARTESIAN_POINT('Ctrl Pts',(0.997785598389788,-2.47092134911841,
8.85934740853961));
#406355=CARTESIAN_POINT('Ctrl Pts',(0.99765927366762,-2.4710292807249,8.8591675900182));
#406356=CARTESIAN_POINT('Ctrl Pts',(0.997152014245821,-2.47146268222672,
8.85844552518694));
#406357=CARTESIAN_POINT('Ctrl Pts',(0.996798055348731,-2.4718984588358,
8.85759444184121));
#406358=CARTESIAN_POINT('Ctrl Pts',(0.996541370401398,-2.47227968985936,
8.85683498915135));
#406359=CARTESIAN_POINT('Ctrl Pts',(0.996514509005272,-2.47231958467067,
8.85675551444995));
#406360=CARTESIAN_POINT('Ctrl Pts',(0.996488731289395,-2.47235888984364,
8.8566769979365));
#406361=CARTESIAN_POINT('Ctrl Pts',(0.996463985412329,-2.47239754457562,
8.85659965593547));
#406362=CARTESIAN_POINT('Ctrl Pts',(0.99612996430092,-2.47291930812044,
8.85555568965886));
#406363=CARTESIAN_POINT('Ctrl Pts',(0.995884302298615,-2.47346899447078,
8.85434650606346));
#406364=CARTESIAN_POINT('Ctrl Pts',(0.995720111102494,-2.47404678523083,
8.85297329937117));
#406365=CARTESIAN_POINT('Ctrl Pts',(0.995627763558993,-2.47437175732804,
8.85220095427747));
#406366=CARTESIAN_POINT('Ctrl Pts',(0.995561453674497,-2.4747058388066,
8.85137579139184));
#406367=CARTESIAN_POINT('Ctrl Pts',(0.995522110700944,-2.47505025214474,
8.85049129520029));
#406368=CARTESIAN_POINT('Origin',(1.00235268932044,-2.47583052179232,7.59394543036555));
#406369=CARTESIAN_POINT('Ctrl Pts',(1.00628214029679,-2.47016120246828,
7.59443877723642));
#406370=CARTESIAN_POINT('Ctrl Pts',(1.00180750953461,-2.46648548849807,
7.58783886950016));
#406371=CARTESIAN_POINT('Ctrl Pts',(0.995046786110639,-2.47162083661881,
7.58559994247159));
#406372=CARTESIAN_POINT('Ctrl Pts',(1.03070901834745,-2.49022681719079,
7.56670252222132));
#406373=CARTESIAN_POINT('Ctrl Pts',(1.02624085469712,-2.48655641567082,
7.56004874999026));
#406374=CARTESIAN_POINT('Ctrl Pts',(1.0194271481468,-2.49170517865848,7.55786368756704));
#406375=CARTESIAN_POINT('Ctrl Pts',(1.05509028164394,-2.51025496138264,
7.5388891333356));
#406376=CARTESIAN_POINT('Ctrl Pts',(1.05059556347821,-2.50656274648674,
7.53222002137279));
#406377=CARTESIAN_POINT('Ctrl Pts',(1.0437635876927,-2.51175182651942,7.53005029815327));
#406378=CARTESIAN_POINT('Ctrl Pts',(1.07942482691751,-2.53024472875669,
7.51101258149734));
#406379=CARTESIAN_POINT('Ctrl Pts',(1.07487562460053,-2.52650775750732,
7.5043616886572));
#406380=CARTESIAN_POINT('Ctrl Pts',(1.06805484980026,-2.53175985353354,
7.50217374673251));
#406381=CARTESIAN_POINT('',(1.06675863750385,-2.53069219871726,7.50366116523517));
#406382=CARTESIAN_POINT('Ctrl Pts',(1.07279542170607,-2.52479896157612,
7.51860402984325));
#406383=CARTESIAN_POINT('Ctrl Pts',(1.07313666163295,-2.52507927528982,
7.51734760759494));
#406384=CARTESIAN_POINT('Ctrl Pts',(1.07340725496914,-2.52537855293079,
7.51608817408573));
#406385=CARTESIAN_POINT('Ctrl Pts',(1.07359667414355,-2.52570506198001,
7.5148100591312));
#406386=CARTESIAN_POINT('Ctrl Pts',(1.07376825455804,-2.52600082167898,
7.51365231206384));
#406387=CARTESIAN_POINT('Ctrl Pts',(1.07387368844633,-2.52631921657145,
7.51247773061043));
#406388=CARTESIAN_POINT('Ctrl Pts',(1.07387609828084,-2.52666634484814,
7.51129758471022));
#406389=CARTESIAN_POINT('Ctrl Pts',(1.07387909342991,-2.5270977856525,7.50983079813402));
#406390=CARTESIAN_POINT('Ctrl Pts',(1.07370982072313,-2.52755993392016,
7.50839324291155));
#406391=CARTESIAN_POINT('Ctrl Pts',(1.07328963432874,-2.52802780918635,
7.50715379678855));
#406392=CARTESIAN_POINT('Ctrl Pts',(1.07309552032192,-2.52824395407782,
7.50658120839351));
#406393=CARTESIAN_POINT('Ctrl Pts',(1.07281319256692,-2.52848569937381,
7.50598221009429));
#406394=CARTESIAN_POINT('Ctrl Pts',(1.07243457566396,-2.52873001389882,
7.50545747549611));
#406395=CARTESIAN_POINT('Ctrl Pts',(1.07223253396525,-2.52886038769161,
7.50517746087247));
#406396=CARTESIAN_POINT('Ctrl Pts',(1.07200099171825,-2.52899307697135,
7.50491486231392));
#406397=CARTESIAN_POINT('Ctrl Pts',(1.07174525119684,-2.52912312068133,
7.50468370960992));
#406398=CARTESIAN_POINT('Ctrl Pts',(1.07136283844856,-2.52931757704773,
7.50433806340447));
#406399=CARTESIAN_POINT('Ctrl Pts',(1.07091459969728,-2.52951145280317,
7.50405484070984));
#406400=CARTESIAN_POINT('Ctrl Pts',(1.0704304385914,-2.52969103325065,7.50385766036131));
#406401=CARTESIAN_POINT('Ctrl Pts',(1.07037866508669,-2.5297102365882,7.50383657498791));
#406402=CARTESIAN_POINT('Ctrl Pts',(1.07032650872316,-2.52972928148965,
7.50381643264937));
#406403=CARTESIAN_POINT('Ctrl Pts',(1.07027402628804,-2.52974815515541,
7.50379723213559));
#406404=CARTESIAN_POINT('Ctrl Pts',(1.0699236888654,-2.52987414304837,7.50366906242519));
#406405=CARTESIAN_POINT('Ctrl Pts',(1.06955095771556,-2.52999456458162,
7.50358235568538));
#406406=CARTESIAN_POINT('Ctrl Pts',(1.06918890063954,-2.53010200008105,
7.5035341175365));
#406407=CARTESIAN_POINT('Ctrl Pts',(1.06864603703099,-2.53026308745309,
7.50346178989176));
#406408=CARTESIAN_POINT('Ctrl Pts',(1.06805519007336,-2.53041329887527,
7.50346967198527));
#406409=CARTESIAN_POINT('Ctrl Pts',(1.06747062403745,-2.53054291245445,
7.50354272648692));
#406410=CARTESIAN_POINT('Ctrl Pts',(1.06723017992708,-2.53059622520241,
7.50357277531559));
#406411=CARTESIAN_POINT('Ctrl Pts',(1.0669911486187,-2.53064612070987,7.50361331098761));
#406412=CARTESIAN_POINT('Ctrl Pts',(1.06675863750441,-2.53069219871856,
7.50366116523659));
#406413=CARTESIAN_POINT('',(1.00345144303404,-2.4785444647084,7.57603338622103));
#406414=CARTESIAN_POINT('Origin',(1.00676500980812,-2.48673664175929,7.58486873427625));
#406415=CARTESIAN_POINT('Ctrl Pts',(1.06675863755133,-2.53069219874942,
7.50366116529969));
#406416=CARTESIAN_POINT('Ctrl Pts',(1.0456901427307,-2.51333863067846,7.5278357307971));
#406417=CARTESIAN_POINT('Ctrl Pts',(1.02458872953262,-2.49595688722902,
7.55196141284068));
#406418=CARTESIAN_POINT('Ctrl Pts',(1.00345144418594,-2.47854446519909,
7.57603338728831));
#406419=CARTESIAN_POINT('Ctrl Pts',(1.00739967866916,-2.47130674194166,
7.59639677331372));
#406420=CARTESIAN_POINT('Ctrl Pts',(0.995287956784576,-2.45761812956736,
7.59959882295463));
#406421=CARTESIAN_POINT('Ctrl Pts',(0.99557457985025,-2.47591093306534,
7.59642833564546));
#406422=CARTESIAN_POINT('Ctrl Pts',(1.00531808064712,-2.46800794613739,
7.58707626057423));
#406423=CARTESIAN_POINT('Ctrl Pts',(0.998700563069069,-2.46655166589637,
7.58809943920599));
#406424=CARTESIAN_POINT('Ctrl Pts',(0.994878346512149,-2.47212885706977,
7.58710240504253));
#406425=CARTESIAN_POINT('Ctrl Pts',(1.00390123521112,-2.47391710692992,
7.58015376756929));
#406426=CARTESIAN_POINT('Ctrl Pts',(1.00122002820245,-2.4729473645042,7.5820588065976));
#406427=CARTESIAN_POINT('Ctrl Pts',(0.999946469877937,-2.47545836514784,
7.58020924244128));
#406428=CARTESIAN_POINT('Ctrl Pts',(1.00345144272367,-2.47854446394124,
7.57603338509286));
#406429=CARTESIAN_POINT('Ctrl Pts',(1.00345144272367,-2.47854446394124,
7.57603338509286));
#406430=CARTESIAN_POINT('Ctrl Pts',(1.00345144272367,-2.47854446394124,
7.57603338509286));
#406431=CARTESIAN_POINT('Origin',(1.00677029912178,-2.48673450035402,7.58486873427622));
#406432=CARTESIAN_POINT('Ctrl Pts',(0.984839906194085,-2.56856361376242,
7.51098857897448));
#406433=CARTESIAN_POINT('Ctrl Pts',(0.98550808007881,-2.56271433554783,
7.50433767179956));
#406434=CARTESIAN_POINT('Ctrl Pts',(0.994061605444767,-2.56174209334736,
7.50214974420965));
#406435=CARTESIAN_POINT('Ctrl Pts',(0.988415106647427,-2.53726585938649,
7.53887321589173));
#406436=CARTESIAN_POINT('Ctrl Pts',(0.989075274623224,-2.53148666590551,
7.53220407452067));
#406437=CARTESIAN_POINT('Ctrl Pts',(0.997592998639344,-2.53046133790587,
7.53003438070912));
#406438=CARTESIAN_POINT('Ctrl Pts',(0.991997172804488,-2.5059080017768,
7.56669465659233));
#406439=CARTESIAN_POINT('Ctrl Pts',(0.99265343931025,-2.50016296225485,
7.56004085833301));
#406440=CARTESIAN_POINT('Ctrl Pts',(1.00112998038329,-2.4991213761741,7.55785582193789));
#406441=CARTESIAN_POINT('Ctrl Pts',(0.995585942662736,-2.47449145912388,
7.59443891967696));
#406442=CARTESIAN_POINT('Ctrl Pts',(0.996243160673252,-2.46873809000989,
7.58783901202978));
#406443=CARTESIAN_POINT('Ctrl Pts',(1.00467229381076,-2.46772374660724,
7.58560008491213));
#406444=CARTESIAN_POINT('',(0.994253029633976,-2.5600464660629,7.50366116523517));
#406445=CARTESIAN_POINT('Ctrl Pts',(0.994253029634111,-2.56004646606324,
7.50366116523554));
#406446=CARTESIAN_POINT('Ctrl Pts',(0.993616541819977,-2.56045758743124,
7.50350835821026));
#406447=CARTESIAN_POINT('Ctrl Pts',(0.993018079633229,-2.560814800284,7.50345484956));
#406448=CARTESIAN_POINT('Ctrl Pts',(0.992440158080142,-2.56112924048317,
7.50349758195598));
#406449=CARTESIAN_POINT('Ctrl Pts',(0.992143641463629,-2.56129057162485,
7.50351950684424));
#406450=CARTESIAN_POINT('Ctrl Pts',(0.991823368062701,-2.56145665822576,
7.50357029184312));
#406451=CARTESIAN_POINT('Ctrl Pts',(0.991510129749823,-2.56160832434007,
7.50365515313923));
#406452=CARTESIAN_POINT('Ctrl Pts',(0.9910282423819,-2.56184164823956,7.50378570417639));
#406453=CARTESIAN_POINT('Ctrl Pts',(0.990549010837215,-2.56204800474017,
7.50400001621911));
#406454=CARTESIAN_POINT('Ctrl Pts',(0.990108013665073,-2.56220960180846,
7.50428903009634));
#406455=CARTESIAN_POINT('Ctrl Pts',(0.990059066371791,-2.56222753783979,
7.50432110841318));
#406456=CARTESIAN_POINT('Ctrl Pts',(0.990010572585586,-2.56224494721138,
7.50435406373354));
#406457=CARTESIAN_POINT('Ctrl Pts',(0.989962567779687,-2.56226182368384,
7.50438785222352));
#406458=CARTESIAN_POINT('Ctrl Pts',(0.989669475365647,-2.56236486266006,
7.50459414719561));
#406459=CARTESIAN_POINT('Ctrl Pts',(0.989389773235812,-2.56244919073965,
7.50483629897752));
#406460=CARTESIAN_POINT('Ctrl Pts',(0.989134556580141,-2.56251283734951,
7.5050991045531));
#406461=CARTESIAN_POINT('Ctrl Pts',(0.988571523003644,-2.56265324816356,
7.50567888004914));
#406462=CARTESIAN_POINT('Ctrl Pts',(0.988105596423548,-2.56269904257184,
7.50637912803145));
#406463=CARTESIAN_POINT('Ctrl Pts',(0.987731664620582,-2.56268070472711,
7.50710440483569));
#406464=CARTESIAN_POINT('Ctrl Pts',(0.987639969118908,-2.56267620792353,
7.50728225710685));
#406465=CARTESIAN_POINT('Ctrl Pts',(0.987551972991268,-2.5626679109256,
7.50746498566955));
#406466=CARTESIAN_POINT('Ctrl Pts',(0.987469691245689,-2.56265642216574,
7.50764697238949));
#406467=CARTESIAN_POINT('Ctrl Pts',(0.987027367225998,-2.56259466175454,
7.50862528291182));
#406468=CARTESIAN_POINT('Ctrl Pts',(0.986709454310686,-2.56243915725785,
7.50965856837422));
#406469=CARTESIAN_POINT('Ctrl Pts',(0.986471889921157,-2.56223944537933,
7.51067959873203));
#406470=CARTESIAN_POINT('Ctrl Pts',(0.986341157937951,-2.56212954368068,
7.51124147302579));
#406471=CARTESIAN_POINT('Ctrl Pts',(0.986235005650205,-2.56200589525493,
7.51180065547253));
#406472=CARTESIAN_POINT('Ctrl Pts',(0.98614791253591,-2.56187474152437,
7.51235175716501));
#406473=CARTESIAN_POINT('Ctrl Pts',(0.985846971132247,-2.56142155313985,
7.51425603304536));
#406474=CARTESIAN_POINT('Ctrl Pts',(0.985742762481488,-2.56082136401568,
7.5162690050518));
#406475=CARTESIAN_POINT('Ctrl Pts',(0.985805085598317,-2.56012642898782,
7.51827788969243));
#406476=CARTESIAN_POINT('Ctrl Pts',(0.985808458643174,-2.56008881779087,
7.51838661432545));
#406477=CARTESIAN_POINT('Ctrl Pts',(0.985812326717548,-2.56005092221106,
7.51849533314857));
#406478=CARTESIAN_POINT('Ctrl Pts',(0.98581668737997,-2.56001274842383,
7.51860402984325));
#406479=CARTESIAN_POINT('Ctrl Pts',(1.00345144254816,-2.47854446586344,
7.57603338728985));
#406480=CARTESIAN_POINT('Ctrl Pts',(1.00038100552585,-2.5057575085012,7.55196141284922));
#406481=CARTESIAN_POINT('Ctrl Pts',(0.997314994683372,-2.53292355758907,
7.52783573083105));
#406482=CARTESIAN_POINT('Ctrl Pts',(0.994253029621964,-2.56004646612085,
7.50366116530176));
#406483=CARTESIAN_POINT('Origin',(3.46738858721E-16,-8.56451684780634E-16,
7.49482233047033));
#406484=CARTESIAN_POINT('Origin',(1.06332537456794,-2.5225474024882,7.49482233047033));
#406485=CARTESIAN_POINT('Origin',(0.,0.,7.50366116523517));
#406486=CARTESIAN_POINT('Origin',(0.991053119217926,-2.55180719586893,7.49482233047033));
#406487=CARTESIAN_POINT('Ctrl Pts',(1.07279460441741,-2.52479829015122,
7.51860402984325));
#406488=CARTESIAN_POINT('Ctrl Pts',(1.07867375938541,-2.52962859271858,
7.51860402984325));
#406489=CARTESIAN_POINT('Ctrl Pts',(1.08566466424083,-2.52662467272424,
7.51860402984325));
#406490=CARTESIAN_POINT('Ctrl Pts',(1.07497757558516,-2.52659181347634,
7.51041458714365));
#406491=CARTESIAN_POINT('Ctrl Pts',(1.08032998091007,-2.5289169205702,7.5100464290044));
#406492=CARTESIAN_POINT('Ctrl Pts',(1.08566659224939,-2.52662384427877,
7.50729136483009));
#406493=CARTESIAN_POINT('Ctrl Pts',(1.07405060721884,-2.52924971995458,
7.50215815450138));
#406494=CARTESIAN_POINT('Ctrl Pts',(1.0769578040486,-2.5303660850716,7.49877163671533));
#406495=CARTESIAN_POINT('Ctrl Pts',(1.08013710129291,-2.52902593857712,
7.49481588533172));
#406496=CARTESIAN_POINT('Ctrl Pts',(1.06675842366606,-2.53069169142692,
7.50366171572174));
#406497=CARTESIAN_POINT('Ctrl Pts',(1.06818074157475,-2.53406588377825,
7.50000045605858));
#406498=CARTESIAN_POINT('Ctrl Pts',(1.06818074157486,-2.5340658837782,7.49482233047317));
#406499=CARTESIAN_POINT('Origin',(1.08072982485792,-2.51514001512094,7.51860402984325));
#406500=CARTESIAN_POINT('Origin',(1.08072982485792,-2.51514001512094,9.));
#406501=CARTESIAN_POINT('Origin',(1.08072982485792,-2.51514001512094,8.75721825406948));
#406502=CARTESIAN_POINT('Ctrl Pts',(1.05989096392722,-2.51419847335743,
8.78942910404913));
#406503=CARTESIAN_POINT('Ctrl Pts',(1.06418404382886,-2.51775120380875,
8.7967269950169));
#406504=CARTESIAN_POINT('Ctrl Pts',(1.07104086177895,-2.51203652677664,
8.79893251111267));
#406505=CARTESIAN_POINT('Ctrl Pts',(1.06838645708339,-2.52117715623988,
8.78111911759584));
#406506=CARTESIAN_POINT('Ctrl Pts',(1.07348069887328,-2.52538322455977,
8.78644465894813));
#406507=CARTESIAN_POINT('Ctrl Pts',(1.08067618140392,-2.52164952091238,
8.78817647674133));
#406508=CARTESIAN_POINT('Ctrl Pts',(1.07368105107517,-2.52552643784495,
8.76780923932029));
#406509=CARTESIAN_POINT('Ctrl Pts',(1.07969783280627,-2.53048759440067,
8.76988516158373));
#406510=CARTESIAN_POINT('Ctrl Pts',(1.0867021275484,-2.52764572255948,8.77093053738832));
#406511=CARTESIAN_POINT('Ctrl Pts',(1.07264867770947,-2.52467838745471,
8.75371302330492));
#406512=CARTESIAN_POINT('Ctrl Pts',(1.07851730378655,-2.52951836982402,
8.75300828287559));
#406513=CARTESIAN_POINT('Ctrl Pts',(1.0855271460478,-2.52647589536948,8.75267964240738));
#406514=CARTESIAN_POINT('Origin',(1.06989435603299,-2.50623915016686,8.78727029226991));
#406515=CARTESIAN_POINT('Ctrl Pts',(1.00671661105395,-2.47051810124197,
8.85049129520029));
#406516=CARTESIAN_POINT('Ctrl Pts',(1.01122897392943,-2.47422481049724,
8.85711686593484));
#406517=CARTESIAN_POINT('Ctrl Pts',(1.01802024859359,-2.46903064544885,
8.85933012996512));
#406518=CARTESIAN_POINT('Ctrl Pts',(1.02515785026094,-2.48566677477142,
8.82945683644723));
#406519=CARTESIAN_POINT('Ctrl Pts',(1.02970766847652,-2.48940425195461,
8.83607469902389));
#406520=CARTESIAN_POINT('Ctrl Pts',(1.03649609897605,-2.48416504840347,
8.83829567148519));
#406521=CARTESIAN_POINT('Ctrl Pts',(1.04357160131378,-2.50079286798137,
8.80838214965003));
#406522=CARTESIAN_POINT('Ctrl Pts',(1.0481393752363,-2.50454509499454,8.81501364461989));
#406523=CARTESIAN_POINT('Ctrl Pts',(1.05494349880901,-2.49927701042776,
8.81722098428721));
#406524=CARTESIAN_POINT('Ctrl Pts',(1.06195995288114,-2.51589809662203,
8.78727029226991));
#406525=CARTESIAN_POINT('Ctrl Pts',(1.06652848552592,-2.51965094689243,
8.79393457792714));
#406526=CARTESIAN_POINT('Ctrl Pts',(1.07336460881944,-2.51436825501291,
8.79610912703474));
#406527=CARTESIAN_POINT('Origin',(1.0146510142058,-2.4608591547868,8.85049129520029));
#406528=CARTESIAN_POINT('Ctrl Pts',(0.995522110700944,-2.47505025214474,
8.85049129520029));
#406529=CARTESIAN_POINT('Ctrl Pts',(0.994859350710984,-2.48085213644372,
8.85711686593484));
#406530=CARTESIAN_POINT('Ctrl Pts',(0.986367352980535,-2.48184548263713,
8.85933012996512));
#406531=CARTESIAN_POINT('Ctrl Pts',(0.996108444897021,-2.46991740885651,
8.86332496987232));
#406532=CARTESIAN_POINT('Ctrl Pts',(0.991939266488174,-2.47190985603824,
8.86648636486737));
#406533=CARTESIAN_POINT('Ctrl Pts',(0.988024668749186,-2.46748808869534,
8.87206031107457));
#406534=CARTESIAN_POINT('Ctrl Pts',(1.00269746170462,-2.46721654538254,
8.86341338519876));
#406535=CARTESIAN_POINT('Ctrl Pts',(1.00708145117165,-2.4657151770109,8.86654584966058));
#406536=CARTESIAN_POINT('Ctrl Pts',(1.00675706511742,-2.4597974978649,8.87215952290714));
#406537=CARTESIAN_POINT('Ctrl Pts',(1.00671661105395,-2.47051810124197,
8.85049129520029));
#406538=CARTESIAN_POINT('Ctrl Pts',(1.01122897392943,-2.47422481049724,
8.85711686593484));
#406539=CARTESIAN_POINT('Ctrl Pts',(1.01802024859359,-2.46903064544885,
8.85933012996512));
#406540=CARTESIAN_POINT('Origin',(0.983102876847322,-2.47363158005823,8.85049129520029));
#406541=CARTESIAN_POINT('Ctrl Pts',(0.987408162934533,-2.54608077127964,
8.78727029226991));
#406542=CARTESIAN_POINT('Ctrl Pts',(0.986737152926397,-2.55195487727523,
8.79393457792714));
#406543=CARTESIAN_POINT('Ctrl Pts',(0.97815135164051,-2.55291583068589,
8.79610912703474));
#406544=CARTESIAN_POINT('Ctrl Pts',(0.990108979344133,-2.52243748478276,
8.80838214965001));
#406545=CARTESIAN_POINT('Ctrl Pts',(0.989438080774451,-2.52831061523213,
8.81501364461994));
#406546=CARTESIAN_POINT('Ctrl Pts',(0.980885428519814,-2.52925980014898,
8.81722098428721));
#406547=CARTESIAN_POINT('Ctrl Pts',(0.992813526340833,-2.49876154025726,
8.82945683644724));
#406548=CARTESIAN_POINT('Ctrl Pts',(0.992145265042246,-2.50461158370382,
8.8360746990239));
#406549=CARTESIAN_POINT('Ctrl Pts',(0.983623977915115,-2.50557059788233,
8.8382956714852));
#406550=CARTESIAN_POINT('Ctrl Pts',(0.995522110700944,-2.47505025214474,
8.85049129520029));
#406551=CARTESIAN_POINT('Ctrl Pts',(0.994859350710984,-2.48085213644372,
8.85711686593484));
#406552=CARTESIAN_POINT('Ctrl Pts',(0.986367352980535,-2.48184548263713,
8.85933012996512));
#406553=CARTESIAN_POINT('Origin',(0.974988929080911,-2.54466209919313,8.78727029226991));
#406554=CARTESIAN_POINT('Ctrl Pts',(0.985837683686217,-2.55982878158036,
8.75374538247848));
#406555=CARTESIAN_POINT('Ctrl Pts',(0.98498828679914,-2.56738013267245,
8.75304829418601));
#406556=CARTESIAN_POINT('Ctrl Pts',(0.977845758623038,-2.57007363122686,
8.75272238421917));
#406557=CARTESIAN_POINT('Ctrl Pts',(0.985687874189968,-2.56114023650866,
8.76769408445021));
#406558=CARTESIAN_POINT('Ctrl Pts',(0.98481641692612,-2.5688815359609,8.76974318093971));
#406559=CARTESIAN_POINT('Ctrl Pts',(0.977816320118244,-2.57171296704088,
8.77077869880429));
#406560=CARTESIAN_POINT('Ctrl Pts',(0.986455712341585,-2.55441846563452,
8.78108014887987));
#406561=CARTESIAN_POINT('Ctrl Pts',(0.985720959251978,-2.56097936307296,
8.78639403366322));
#406562=CARTESIAN_POINT('Ctrl Pts',(0.977971752381973,-2.56331856563252,
8.78812224174741));
#406563=CARTESIAN_POINT('Ctrl Pts',(0.987714029535141,-2.54340296701399,
8.78944554828685));
#406564=CARTESIAN_POINT('Ctrl Pts',(0.987100369825394,-2.54893287111602,
8.79673892988687));
#406565=CARTESIAN_POINT('Ctrl Pts',(0.9782088694197,-2.54959978554247,8.79894799272499));
#406566=CARTESIAN_POINT('Origin',(0.973397453526352,-2.55859407633732,8.75721825406948));
#406567=CARTESIAN_POINT('Origin',(0.973397453526352,-2.55859407633732,9.));
#406568=CARTESIAN_POINT('Origin',(0.973397453526352,-2.55859407633732,7.51860402984325));
#406569=CARTESIAN_POINT('Ctrl Pts',(0.994252744839196,-2.56004573276091,
7.50366195182966));
#406570=CARTESIAN_POINT('Ctrl Pts',(0.995578475926554,-2.56345928352135,
7.50000065167735));
#406571=CARTESIAN_POINT('Ctrl Pts',(0.995578475926445,-2.56345928352139,
7.49482233047108));
#406572=CARTESIAN_POINT('Ctrl Pts',(0.988005205888665,-2.56408578927886,
7.50215800491337));
#406573=CARTESIAN_POINT('Ctrl Pts',(0.986691781976957,-2.5669106104772,
7.49877273257268));
#406574=CARTESIAN_POINT('Ctrl Pts',(0.983473834939363,-2.5681603997447,
7.49481816995647));
#406575=CARTESIAN_POINT('Ctrl Pts',(0.985497132441383,-2.56281316053288,
7.51043025814043));
#406576=CARTESIAN_POINT('Ctrl Pts',(0.983271955087221,-2.5682114327314,
7.51006209594514));
#406577=CARTESIAN_POINT('Ctrl Pts',(0.97783982435821,-2.57027805458972,
7.50731281821702));
#406578=CARTESIAN_POINT('Ctrl Pts',(0.98581685882451,-2.56001124677167,
7.51860402984326));
#406579=CARTESIAN_POINT('Ctrl Pts',(0.984954168022284,-2.56757145721651,
7.51860402984326));
#406580=CARTESIAN_POINT('Ctrl Pts',(0.977842190757062,-2.57027715431147,
7.51860402984327));
#406581=CARTESIAN_POINT('Origin',(0.,0.,7.5));
#406582=CARTESIAN_POINT('Origin',(1.15205371787333,-2.40618167532513,7.5));
#406583=CARTESIAN_POINT('',(1.15205371787333,-2.40618167532513,7.59394543036555));
#406584=CARTESIAN_POINT('',(1.15205371787333,-2.40618167532513,8.85049129520029));
#406585=CARTESIAN_POINT('',(1.15205371787333,-2.40618167532513,7.5));
#406586=CARTESIAN_POINT('',(1.14850738206914,-2.47758611705877,8.78727029226991));
#406587=CARTESIAN_POINT('Ctrl Pts',(1.15205371787333,-2.40618167532513,
8.85049129520029));
#406588=CARTESIAN_POINT('Ctrl Pts',(1.15086988762442,-2.43001775366008,
8.82945686509571));
#406589=CARTESIAN_POINT('Ctrl Pts',(1.14968781728233,-2.45381839678236,
8.80838212259895));
#406590=CARTESIAN_POINT('Ctrl Pts',(1.14850738206914,-2.47758611705877,
8.78727029226991));
#406591=CARTESIAN_POINT('',(1.14781180121219,-2.4915914356506,8.75721825406948));
#406592=CARTESIAN_POINT('Origin',(1.14990524686342,-2.44944458353935,8.7593767971312));
#406593=CARTESIAN_POINT('',(1.14781180121219,-2.4915914356506,7.51860402984325));
#406594=CARTESIAN_POINT('',(1.14781180121219,-2.4915914356506,7.5));
#406595=CARTESIAN_POINT('Ctrl Pts',(1.14781180121219,-2.4915914356506,7.51860402984325));
#406596=CARTESIAN_POINT('Ctrl Pts',(1.14835807179204,-2.48059243613578,
7.52834476460825));
#406597=CARTESIAN_POINT('Ctrl Pts',(1.14890469700287,-2.46958629622919,
7.53807742314407));
#406598=CARTESIAN_POINT('Ctrl Pts',(1.14945168875189,-2.45857277618267,
7.54780169004674));
#406599=CARTESIAN_POINT('Ctrl Pts',(1.15031809411995,-2.44112795565896,
7.5632044032688));
#406600=CARTESIAN_POINT('Ctrl Pts',(1.15118542018668,-2.42366459713434,
7.57858609112103));
#406601=CARTESIAN_POINT('Ctrl Pts',(1.15205371787333,-2.40618167532513,
7.59394543036555));
#406602=CARTESIAN_POINT('Origin',(1.38617896354007,-2.56152510751203,7.5));
#406603=CARTESIAN_POINT('',(1.23235567333049,-2.45087725266271,8.75721825406948));
#406604=CARTESIAN_POINT('',(1.22097218676273,-2.4426889063615,8.78727029226991));
#406605=CARTESIAN_POINT('Origin',(1.19207665202558,-2.42190382934856,8.75658640621066));
#406606=CARTESIAN_POINT('',(1.16293484201943,-2.40094160211227,8.85049129520029));
#406607=CARTESIAN_POINT('Ctrl Pts',(1.22097218676273,-2.44268890636149,
8.78727029226991));
#406608=CARTESIAN_POINT('Ctrl Pts',(1.20165384546697,-2.42879287656841,
8.80838212259896));
#406609=CARTESIAN_POINT('Ctrl Pts',(1.1823087445676,-2.41487759811192,8.82945686509571));
#406610=CARTESIAN_POINT('Ctrl Pts',(1.16293484201943,-2.40094160211227,
8.85049129520029));
#406611=CARTESIAN_POINT('',(1.16293484201943,-2.40094160211227,7.59394543036555));
#406612=CARTESIAN_POINT('',(1.16293484201943,-2.40094160211227,7.5));
#406613=CARTESIAN_POINT('',(1.23235567333049,-2.45087725266271,7.51860402984325));
#406614=CARTESIAN_POINT('Ctrl Pts',(1.16293484201943,-2.40094160211227,
7.59394543036555));
#406615=CARTESIAN_POINT('Ctrl Pts',(1.177144915448,-2.41116316309943,7.57858609112103));
#406616=CARTESIAN_POINT('Ctrl Pts',(1.1913390878895,-2.42137328622107,7.56320440326857));
#406617=CARTESIAN_POINT('Ctrl Pts',(1.2055181926922,-2.43157257091954,7.54780169004651));
#406618=CARTESIAN_POINT('Ctrl Pts',(1.21446995317457,-2.43801173298108,
7.53807742314383));
#406619=CARTESIAN_POINT('Ctrl Pts',(1.22341571509856,-2.44444658017184,
7.52834476460825));
#406620=CARTESIAN_POINT('Ctrl Pts',(1.23235567333049,-2.45087725266271,
7.51860402984325));
#406621=CARTESIAN_POINT('',(1.23235567333049,-2.45087725266271,7.5));
#406622=CARTESIAN_POINT('Origin',(1.15892025438444,-2.40652270515029,7.5));
#406623=CARTESIAN_POINT('Ctrl Pts',(1.16293484201943,-2.40094160211227,
8.85049129520029));
#406624=CARTESIAN_POINT('Ctrl Pts',(1.16277762822757,-2.4008285154087,8.85097269580138));
#406625=CARTESIAN_POINT('Ctrl Pts',(1.16261748621829,-2.40072368386097,
8.85143669361005));
#406626=CARTESIAN_POINT('Ctrl Pts',(1.16244656312291,-2.40062301180747,
8.8519052845931));
#406627=CARTESIAN_POINT('Ctrl Pts',(1.16211224838788,-2.40042610365523,
8.85282181883899));
#406628=CARTESIAN_POINT('Ctrl Pts',(1.16174518876681,-2.40025034340575,
8.85372622499635));
#406629=CARTESIAN_POINT('Ctrl Pts',(1.16133296549051,-2.40010687975259,
8.8546225773507));
#406630=CARTESIAN_POINT('Ctrl Pts',(1.1609907523673,-2.39998778132309,8.85536669723986));
#406631=CARTESIAN_POINT('Ctrl Pts',(1.16061734602602,-2.39989088383228,
8.85610498449051));
#406632=CARTESIAN_POINT('Ctrl Pts',(1.16020359950664,-2.39983030360421,
8.85681338218371));
#406633=CARTESIAN_POINT('Ctrl Pts',(1.1598281238905,-2.39977532695209,8.85745625420284));
#406634=CARTESIAN_POINT('Ctrl Pts',(1.15941480250415,-2.39974897790984,
8.85808743050665));
#406635=CARTESIAN_POINT('Ctrl Pts',(1.15894967359855,-2.39977621475689,
8.8586680450841));
#406636=CARTESIAN_POINT('Ctrl Pts',(1.15873507320426,-2.39978878124769,
8.85893592806395));
#406637=CARTESIAN_POINT('Ctrl Pts',(1.15850935230519,-2.39981297869223,
8.85919241173848));
#406638=CARTESIAN_POINT('Ctrl Pts',(1.1582707442805,-2.39985280471822,8.85943017985534));
#406639=CARTESIAN_POINT('Ctrl Pts',(1.15794855281164,-2.39990658164308,
8.8597512372));
#406640=CARTESIAN_POINT('Ctrl Pts',(1.15759476909804,-2.39999085472495,
8.86004599534705));
#406641=CARTESIAN_POINT('Ctrl Pts',(1.15721605712058,-2.4001147430708,8.86026130871721));
#406642=CARTESIAN_POINT('Ctrl Pts',(1.15707739998861,-2.40016010208699,
8.86034014101235));
#406643=CARTESIAN_POINT('Ctrl Pts',(1.15693331461314,-2.40021144115131,
8.86040910639692));
#406644=CARTESIAN_POINT('Ctrl Pts',(1.15678783942167,-2.40026767842518,
8.86046313645507));
#406645=CARTESIAN_POINT('Ctrl Pts',(1.15656082660373,-2.40035543622007,
8.8605474499083));
#406646=CARTESIAN_POINT('Ctrl Pts',(1.15632428564956,-2.40045765448499,
8.86059655985669));
#406647=CARTESIAN_POINT('Ctrl Pts',(1.1560932704394,-2.40056750872952,8.86059725258816));
#406648=CARTESIAN_POINT('Ctrl Pts',(1.15586172149181,-2.40067761678125,
8.86059794692011));
#406649=CARTESIAN_POINT('Ctrl Pts',(1.15563429688715,-2.40079901655755,
8.86056369958366));
#406650=CARTESIAN_POINT('Ctrl Pts',(1.15542162839186,-2.40092176712124,
8.86048590497774));
#406651=CARTESIAN_POINT('Ctrl Pts',(1.15536612824649,-2.40095380136364,
8.86046560290182));
#406652=CARTESIAN_POINT('Ctrl Pts',(1.15531095632765,-2.40098642279828,
8.86044257503091));
#406653=CARTESIAN_POINT('Ctrl Pts',(1.15525780078614,-2.40101859513937,
8.86041778462583));
#406654=CARTESIAN_POINT('Ctrl Pts',(1.15490012995229,-2.40123507507237,
8.860250975962));
#406655=CARTESIAN_POINT('Ctrl Pts',(1.15458593018283,-2.40146055442195,
8.8599848982295));
#406656=CARTESIAN_POINT('Ctrl Pts',(1.15431943237592,-2.40168156859715,
8.85968173251462));
#406657=CARTESIAN_POINT('Ctrl Pts',(1.15417847030456,-2.40179847243323,
8.85952137522077));
#406658=CARTESIAN_POINT('Ctrl Pts',(1.15404801525878,-2.40191623341874,
8.85934740853961));
#406659=CARTESIAN_POINT('Ctrl Pts',(1.15392886528608,-2.40203203692091,
8.8591675900182));
#406660=CARTESIAN_POINT('Ctrl Pts',(1.15345041621273,-2.40249704817559,
8.85844552518695));
#406661=CARTESIAN_POINT('Ctrl Pts',(1.15312510486536,-2.40295460765929,
8.85759444184123));
#406662=CARTESIAN_POINT('Ctrl Pts',(1.15289337286033,-2.40335150126387,
8.85683498915137));
#406663=CARTESIAN_POINT('Ctrl Pts',(1.15286912272316,-2.40339303512257,
8.85675551444997));
#406664=CARTESIAN_POINT('Ctrl Pts',(1.15284591626144,-2.40343391112278,
8.85667699793651));
#406665=CARTESIAN_POINT('Ctrl Pts',(1.15282369784461,-2.40347407190826,
8.85659965593547));
#406666=CARTESIAN_POINT('Ctrl Pts',(1.15252379252049,-2.40401616424,8.85555568965886));
#406667=CARTESIAN_POINT('Ctrl Pts',(1.1523138537825,-2.40458046081931,8.85434650606346));
#406668=CARTESIAN_POINT('Ctrl Pts',(1.1521870191159,-2.40516758421233,8.85297329937117));
#406669=CARTESIAN_POINT('Ctrl Pts',(1.15211568234409,-2.40549780534694,
8.85220095427747));
#406670=CARTESIAN_POINT('Ctrl Pts',(1.15207091337418,-2.40583544890816,
8.85137579139183));
#406671=CARTESIAN_POINT('Ctrl Pts',(1.15205371787333,-2.40618167532513,
8.85049129520029));
#406672=CARTESIAN_POINT('Origin',(1.15892025438444,-2.40652270515029,7.59394543036555));
#406673=CARTESIAN_POINT('Ctrl Pts',(1.1624783973461,-2.40061327326238,7.59443877723642));
#406674=CARTESIAN_POINT('Ctrl Pts',(1.15777745639006,-2.397231802018,7.58783886950016));
#406675=CARTESIAN_POINT('Ctrl Pts',(1.15135964648122,-2.40278976005227,
7.58559994247159));
#406676=CARTESIAN_POINT('Ctrl Pts',(1.18814069610536,-2.41907262557727,
7.56670252222135));
#406677=CARTESIAN_POINT('Ctrl Pts',(1.1834465493436,-2.41569604151888,7.56004874999026));
#406678=CARTESIAN_POINT('Ctrl Pts',(1.17697672466145,-2.4212707814983,7.55786368756704));
#406679=CARTESIAN_POINT('Ctrl Pts',(1.21375507308567,-2.43749750689603,
7.53888913333558));
#406680=CARTESIAN_POINT('Ctrl Pts',(1.2090330287799,-2.43410085563323,7.53222002137276));
#406681=CARTESIAN_POINT('Ctrl Pts',(1.20254755552053,-2.43971700033598,
7.53005029815327));
#406682=CARTESIAN_POINT('Ctrl Pts',(1.23932036921914,-2.45588708348031,
7.51101258149734));
#406683=CARTESIAN_POINT('Ctrl Pts',(1.23454108515621,-2.45244925863235,
7.5043616886572));
#406684=CARTESIAN_POINT('Ctrl Pts',(1.22807082731706,-2.4581275722059,7.50217374673251));
#406685=CARTESIAN_POINT('',(1.22670887334889,-2.45714515960791,7.50366116523517));
#406686=CARTESIAN_POINT('Ctrl Pts',(1.23235567333049,-2.45087725266271,
7.51860402984325));
#406687=CARTESIAN_POINT('Ctrl Pts',(1.23271417190463,-2.45113512712465,
7.51734760759493));
#406688=CARTESIAN_POINT('Ctrl Pts',(1.23300338406209,-2.45141645289302,
7.51608817408573));
#406689=CARTESIAN_POINT('Ctrl Pts',(1.2332133335611,-2.45173015496621,7.5148100591312));
#406690=CARTESIAN_POINT('Ctrl Pts',(1.2334035108342,-2.45201431380026,7.51365231206384));
#406691=CARTESIAN_POINT('Ctrl Pts',(1.23352912772806,-2.45232529934387,
7.51247773061042));
#406692=CARTESIAN_POINT('Ctrl Pts',(1.23355377319635,-2.45267156000965,
7.51129758471022));
#406693=CARTESIAN_POINT('Ctrl Pts',(1.23358440469881,-2.45310192247275,
7.50983079813402));
#406694=CARTESIAN_POINT('Ctrl Pts',(1.23344508972213,-2.45357396654679,
7.50839324291155));
#406695=CARTESIAN_POINT('Ctrl Pts',(1.23305574351699,-2.45406780194778,
7.50715379678855));
#406696=CARTESIAN_POINT('Ctrl Pts',(1.23287587678896,-2.45429593967351,
7.50658120839351));
#406697=CARTESIAN_POINT('Ctrl Pts',(1.23260961778091,-2.45455527707924,
7.50598221009429));
#406698=CARTESIAN_POINT('Ctrl Pts',(1.23224743207234,-2.45482334770211,
7.50545747549611));
#406699=CARTESIAN_POINT('Ctrl Pts',(1.23205415856755,-2.45496639848404,
7.50517746087247));
#406700=CARTESIAN_POINT('Ctrl Pts',(1.23183159348028,-2.45511365010212,
7.50491486231392));
#406701=CARTESIAN_POINT('Ctrl Pts',(1.2315847103343,-2.45525981197482,7.50468370960992));
#406702=CARTESIAN_POINT('Ctrl Pts',(1.23121554215619,-2.45547837007867,
7.50433806340446));
#406703=CARTESIAN_POINT('Ctrl Pts',(1.23078064602179,-2.45570056625098,
7.50405484070983));
#406704=CARTESIAN_POINT('Ctrl Pts',(1.2303089854356,-2.45591079803973,7.50385766036131));
#406705=CARTESIAN_POINT('Ctrl Pts',(1.23025854866718,-2.45593327906179,
7.50383657498791));
#406706=CARTESIAN_POINT('Ctrl Pts',(1.23020771967552,-2.45595562650313,
7.50381643264937));
#406707=CARTESIAN_POINT('Ctrl Pts',(1.23015655431111,-2.45597782395208,
7.50379723213559));
#406708=CARTESIAN_POINT('Ctrl Pts',(1.2298150087663,-2.45612599918514,7.50366906242519));
#406709=CARTESIAN_POINT('Ctrl Pts',(1.22945075886671,-2.45627005426621,
7.50358235568538));
#406710=CARTESIAN_POINT('Ctrl Pts',(1.22909632909186,-2.45640046610438,
7.5035341175365));
#406711=CARTESIAN_POINT('Ctrl Pts',(1.22856490175818,-2.45659600389596,
7.50346178989176));
#406712=CARTESIAN_POINT('Ctrl Pts',(1.22798489283786,-2.45678376238721,
7.50346967198527));
#406713=CARTESIAN_POINT('Ctrl Pts',(1.22740983222609,-2.45695056293591,
7.50354272648692));
#406714=CARTESIAN_POINT('Ctrl Pts',(1.22717329789342,-2.45701917145415,
7.50357277531559));
#406715=CARTESIAN_POINT('Ctrl Pts',(1.22693795451664,-2.45708427923446,
7.50361331098761));
#406716=CARTESIAN_POINT('Ctrl Pts',(1.22670887334952,-2.45714515960918,
7.50366116523659));
#406717=CARTESIAN_POINT('',(1.16019063351034,-2.40916067458744,7.57603338622103));
#406718=CARTESIAN_POINT('Origin',(1.16402226679194,-2.41712371898013,7.58486873427627));
#406719=CARTESIAN_POINT('Ctrl Pts',(1.22670887339833,-2.45714515963696,
7.50366116529969));
#406720=CARTESIAN_POINT('Ctrl Pts',(1.20457181913612,-2.4411771094306,7.52783573079709));
#406721=CARTESIAN_POINT('Ctrl Pts',(1.18240010892814,-2.42518305082275,
7.55196141284068));
#406722=CARTESIAN_POINT('Ctrl Pts',(1.16019063469131,-2.40916067500332,
7.57603338728831));
#406723=CARTESIAN_POINT('Ctrl Pts',(1.16366703458207,-2.40168485817268,
7.59639677331372));
#406724=CARTESIAN_POINT('Ctrl Pts',(1.15070316512304,-2.38880037120621,
7.59959882295461));
#406725=CARTESIAN_POINT('Ctrl Pts',(1.15216122323506,-2.40703722617453,
7.59642833564546));
#406726=CARTESIAN_POINT('Ctrl Pts',(1.16137835885355,-2.39852620854137,
7.58707626057423));
#406727=CARTESIAN_POINT('Ctrl Pts',(1.15468113347971,-2.39749690619127,
7.58809943920598));
#406728=CARTESIAN_POINT('Ctrl Pts',(1.151224101942,-2.40330752868284,7.58710240504251));
#406729=CARTESIAN_POINT('Ctrl Pts',(1.16034302571037,-2.40451400592806,
7.5801537675693));
#406730=CARTESIAN_POINT('Ctrl Pts',(1.15760519591849,-2.40371804146504,
7.5820588065976));
#406731=CARTESIAN_POINT('Ctrl Pts',(1.15649513461978,-2.40630548015053,
7.58020924244129));
#406732=CARTESIAN_POINT('Ctrl Pts',(1.16019063315146,-2.40916067384174,
7.57603338509286));
#406733=CARTESIAN_POINT('Ctrl Pts',(1.16019063315146,-2.40916067384174,
7.57603338509286));
#406734=CARTESIAN_POINT('Ctrl Pts',(1.16019063315146,-2.40916067384174,
7.57603338509286));
#406735=CARTESIAN_POINT('Origin',(1.16402740803763,-2.41712124308664,7.58486873427621));
#406736=CARTESIAN_POINT('Ctrl Pts',(1.14738488275127,-2.50018731490472,
7.51098857897448));
#406737=CARTESIAN_POINT('Ctrl Pts',(1.14767691925915,-2.49430724461178,
7.50433767179956));
#406738=CARTESIAN_POINT('Ctrl Pts',(1.15615057871823,-2.49278897373537,
7.50214974420965));
#406739=CARTESIAN_POINT('Ctrl Pts',(1.14894748356408,-2.46872480124225,
7.53887321589167));
#406740=CARTESIAN_POINT('Ctrl Pts',(1.14923602095633,-2.46291518462664,
7.53220407452059));
#406741=CARTESIAN_POINT('Ctrl Pts',(1.15767055140447,-2.46134623082197,
7.53003438070911));
#406742=CARTESIAN_POINT('Ctrl Pts',(1.15051308514687,-2.43720186794752,
7.56669465659231));
#406743=CARTESIAN_POINT('Ctrl Pts',(1.15079991733674,-2.43142658508602,
7.56004085833299));
#406744=CARTESIAN_POINT('Ctrl Pts',(1.15919230779771,-2.42984404520438,
7.55785582193789));
#406745=CARTESIAN_POINT('Ctrl Pts',(1.15208161669374,-2.40561994067662,
7.59443891967696));
#406746=CARTESIAN_POINT('Ctrl Pts',(1.1523688647546,-2.39983628437402,7.58783901202978));
#406747=CARTESIAN_POINT('Ctrl Pts',(1.16071569012911,-2.39828396863431,
7.58560008491213));
#406748=CARTESIAN_POINT('',(1.15623297039279,-2.49108456570911,7.50366116523517));
#406749=CARTESIAN_POINT('Ctrl Pts',(1.15623297039294,-2.49108456570945,
7.50366116523554));
#406750=CARTESIAN_POINT('Ctrl Pts',(1.15562413094777,-2.49153562229877,
7.50350835821027));
#406751=CARTESIAN_POINT('Ctrl Pts',(1.15504978507183,-2.49193044482336,
7.50345484956));
#406752=CARTESIAN_POINT('Ctrl Pts',(1.15449319717329,-2.49228126653246,
7.50349758195598));
#406753=CARTESIAN_POINT('Ctrl Pts',(1.1542076263037,-2.49246126408685,7.50351950684424));
#406754=CARTESIAN_POINT('Ctrl Pts',(1.15389865214388,-2.49264752943228,
7.50357029184312));
#406755=CARTESIAN_POINT('Ctrl Pts',(1.15359577469402,-2.49281895317991,
7.50365515313923));
#406756=CARTESIAN_POINT('Ctrl Pts',(1.15312982652894,-2.49308267232009,
7.50378570417639));
#406757=CARTESIAN_POINT('Ctrl Pts',(1.15266480092325,-2.49331930930963,
7.50400001621911));
#406758=CARTESIAN_POINT('Ctrl Pts',(1.1522350633868,-2.49350882914524,7.50428903009635));
#406759=CARTESIAN_POINT('Ctrl Pts',(1.15218736582646,-2.49352986438892,
7.50432110841318));
#406760=CARTESIAN_POINT('Ctrl Pts',(1.15214008709821,-2.49355034499863,
7.50435406373354));
#406761=CARTESIAN_POINT('Ctrl Pts',(1.15209326220264,-2.49357026247504,
7.50438785222352));
#406762=CARTESIAN_POINT('Ctrl Pts',(1.15180737370827,-2.49369186824209,
7.50459414719561));
#406763=CARTESIAN_POINT('Ctrl Pts',(1.15153364917507,-2.49379394363758,
7.50483629897752));
#406764=CARTESIAN_POINT('Ctrl Pts',(1.15128303474168,-2.49387381126592,
7.5050991045531));
#406765=CARTESIAN_POINT('Ctrl Pts',(1.1507301541298,-2.494050007276,7.50567888004914));
#406766=CARTESIAN_POINT('Ctrl Pts',(1.15026811890364,-2.49412555961323,
7.50637912803145));
#406767=CARTESIAN_POINT('Ctrl Pts',(1.14989378047392,-2.49413121733845,
7.50710440483569));
#406768=CARTESIAN_POINT('Ctrl Pts',(1.1498019852593,-2.49413260472499,7.50728225710685));
#406769=CARTESIAN_POINT('Ctrl Pts',(1.14971363833866,-2.49412996270539,
7.50746498566955));
#406770=CARTESIAN_POINT('Ctrl Pts',(1.14963078956238,-2.49412376935996,
7.50764697238949));
#406771=CARTESIAN_POINT('Ctrl Pts',(1.14918541734169,-2.4940904756394,7.50862528291181));
#406772=CARTESIAN_POINT('Ctrl Pts',(1.14885819440525,-2.49395565939379,
7.50965856837421));
#406773=CARTESIAN_POINT('Ctrl Pts',(1.14860832253325,-2.49377157864745,
7.51067959873201));
#406774=CARTESIAN_POINT('Ctrl Pts',(1.14847081772692,-2.49367027878054,
7.51124147302578));
#406775=CARTESIAN_POINT('Ctrl Pts',(1.14835696135859,-2.49355368560417,
7.51180065547253));
#406776=CARTESIAN_POINT('Ctrl Pts',(1.14826164413807,-2.49342838141801,
7.51235175716501));
#406777=CARTESIAN_POINT('Ctrl Pts',(1.14793228517131,-2.49299540553956,
7.51425603304536));
#406778=CARTESIAN_POINT('Ctrl Pts',(1.14778983637918,-2.49240312623949,
7.51626900505181));
#406779=CARTESIAN_POINT('Ctrl Pts',(1.14780750680638,-2.49170562597437,
7.51827788969244));
#406780=CARTESIAN_POINT('Ctrl Pts',(1.14780846316329,-2.49166787594193,
7.51838661432546));
#406781=CARTESIAN_POINT('Ctrl Pts',(1.14780989531216,-2.49162981039429,
7.51849533314857));
#406782=CARTESIAN_POINT('Ctrl Pts',(1.14781180121218,-2.4915914356506,7.51860402984325));
#406783=CARTESIAN_POINT('Ctrl Pts',(1.16019063309946,-2.40916067577124,
7.57603338728985));
#406784=CARTESIAN_POINT('Ctrl Pts',(1.15887005024747,-2.43651452986977,
7.55196141284922));
#406785=CARTESIAN_POINT('Ctrl Pts',(1.15755087359419,-2.46382120338538,
7.52783573083105));
#406786=CARTESIAN_POINT('Ctrl Pts',(1.15623297038451,-2.49108456576771,
7.50366116530176));
#406787=CARTESIAN_POINT('Origin',(4.00899494394879E-16,-8.32476377985981E-16,
7.49482233047033));
#406788=CARTESIAN_POINT('Origin',(1.2227608255338,-2.44923706764778,7.49482233047033));
#406789=CARTESIAN_POINT('Origin',(0.,0.,7.50366116523517));
#406790=CARTESIAN_POINT('Origin',(1.15251174268207,-2.48306724294369,7.49482233047033));
#406791=CARTESIAN_POINT('Ctrl Pts',(1.23235481470268,-2.45087663498119,
7.51860402984325));
#406792=CARTESIAN_POINT('Ctrl Pts',(1.23853136886433,-2.45532033442178,
7.51860402984325));
#406793=CARTESIAN_POINT('Ctrl Pts',(1.24531544834112,-2.45187467749128,
7.51860402984325));
#406794=CARTESIAN_POINT('Ctrl Pts',(1.23464821215602,-2.45252660987735,
7.51041458714366));
#406795=CARTESIAN_POINT('Ctrl Pts',(1.24013859051314,-2.45450401000272,
7.51004642900443));
#406796=CARTESIAN_POINT('Ctrl Pts',(1.24531731930969,-2.45187372722001,
7.5072913648301));
#406797=CARTESIAN_POINT('Ctrl Pts',(1.2338934409984,-2.45523844646883,7.50215815450137));
#406798=CARTESIAN_POINT('Ctrl Pts',(1.2368661904391,-2.4561662531536,7.49877163671529));
#406799=CARTESIAN_POINT('Ctrl Pts',(1.23995309199553,-2.45462516185997,
7.4948158853317));
#406800=CARTESIAN_POINT('Ctrl Pts',(1.22670862744824,-2.45714466706049,
7.50366171572174));
#406801=CARTESIAN_POINT('Ctrl Pts',(1.22834420829845,-2.46042079855046,
7.50000045605858));
#406802=CARTESIAN_POINT('Ctrl Pts',(1.22834420829856,-2.4604207985504,7.49482233047317));
#406803=CARTESIAN_POINT('Origin',(1.23965492357593,-2.44072979259359,7.51860402984325));
#406804=CARTESIAN_POINT('Origin',(1.23965492357593,-2.44072979259359,9.));
#406805=CARTESIAN_POINT('Origin',(1.23965492357593,-2.44072979259359,8.75721825406948));
#406806=CARTESIAN_POINT('Ctrl Pts',(1.21879855353206,-2.44112533573259,
8.78942910404913));
#406807=CARTESIAN_POINT('Ctrl Pts',(1.22331043706217,-2.44439570814448,
8.79672699501692));
#406808=CARTESIAN_POINT('Ctrl Pts',(1.22978702632982,-2.43825345469478,
8.79893251111267));
#406809=CARTESIAN_POINT('Ctrl Pts',(1.22772371753385,-2.44754537204723,
8.7811191175958));
#406810=CARTESIAN_POINT('Ctrl Pts',(1.23307697638015,-2.45141640935655,
8.7864446589481));
#406811=CARTESIAN_POINT('Ctrl Pts',(1.24001845580619,-2.44722936085514,
8.78817647674131));
#406812=CARTESIAN_POINT('Ctrl Pts',(1.23328609264361,-2.45154649178501,
8.76780923932032));
#406813=CARTESIAN_POINT('Ctrl Pts',(1.23960837464324,-2.45611195858344,
8.76988516158377));
#406814=CARTESIAN_POINT('Ctrl Pts',(1.2464161989566,-2.4528271589678,8.77093053738834));
#406815=CARTESIAN_POINT('Ctrl Pts',(1.23220150562468,-2.45076632819391,
8.75371302330492));
#406816=CARTESIAN_POINT('Ctrl Pts',(1.23836817271518,-2.45522036213662,
8.75300828287558));
#406817=CARTESIAN_POINT('Ctrl Pts',(1.24516868049613,-2.45173501663643,
8.75267964240738));
#406818=CARTESIAN_POINT('Origin',(1.22827143700817,-2.43254144629237,8.78727029226991));
#406819=CARTESIAN_POINT('Ctrl Pts',(1.16293484201943,-2.40094160211227,
8.85049129520029));
#406820=CARTESIAN_POINT('Ctrl Pts',(1.16767542343882,-2.40435158745376,
8.85711686593484));
#406821=CARTESIAN_POINT('Ctrl Pts',(1.17411995340356,-2.39873297591286,
8.85933012996512));
#406822=CARTESIAN_POINT('Ctrl Pts',(1.18230877056809,-2.41487761681454,
8.82945683644721));
#406823=CARTESIAN_POINT('Ctrl Pts',(1.18708870167946,-2.41831590709608,
8.83607469902387));
#406824=CARTESIAN_POINT('Ctrl Pts',(1.19352750769644,-2.41265253181512,
8.83829567148519));
#406825=CARTESIAN_POINT('Ctrl Pts',(1.20165382071394,-2.42879285876311,
8.80838214965003));
#406826=CARTESIAN_POINT('Ctrl Pts',(1.20645261566523,-2.43224471814344,
8.81501364461995));
#406827=CARTESIAN_POINT('Ctrl Pts',(1.21290523209922,-2.42655151572731,
8.81722098428721));
#406828=CARTESIAN_POINT('Ctrl Pts',(1.22097218676273,-2.44268890636149,
8.78727029226991));
#406829=CARTESIAN_POINT('Ctrl Pts',(1.22577177880959,-2.44614133910698,
8.79393457792714));
#406830=CARTESIAN_POINT('Ctrl Pts',(1.23225539332383,-2.44043150916126,
8.79610912703474));
#406831=CARTESIAN_POINT('Origin',(1.17023409226487,-2.39079414204315,8.85049129520029));
#406832=CARTESIAN_POINT('Ctrl Pts',(1.15205371787333,-2.40618167532513,
8.85049129520029));
#406833=CARTESIAN_POINT('Ctrl Pts',(1.15176404759819,-2.41201410220892,
8.85711686593484));
#406834=CARTESIAN_POINT('Ctrl Pts',(1.14335314149697,-2.4135494916287,8.85933012996512));
#406835=CARTESIAN_POINT('Ctrl Pts',(1.15230998498431,-2.40102181145301,
8.86332496987232));
#406836=CARTESIAN_POINT('Ctrl Pts',(1.14827702912889,-2.40327728511609,
8.86648636486737));
#406837=CARTESIAN_POINT('Ctrl Pts',(1.14408717074443,-2.39911541190671,
8.87206031107457));
#406838=CARTESIAN_POINT('Ctrl Pts',(1.1587124190333,-2.39790433743638,8.86341338519876));
#406839=CARTESIAN_POINT('Ctrl Pts',(1.16299120812194,-2.39612517061756,
8.86654584966059));
#406840=CARTESIAN_POINT('Ctrl Pts',(1.16228834154898,-2.39024043346388,
8.87215952290714));
#406841=CARTESIAN_POINT('Ctrl Pts',(1.16293484201943,-2.40094160211227,
8.85049129520029));
#406842=CARTESIAN_POINT('Ctrl Pts',(1.16767542343882,-2.40435158745376,
8.85711686593484));
#406843=CARTESIAN_POINT('Ctrl Pts',(1.17411995340356,-2.39873297591286,
8.85933012996512));
#406844=CARTESIAN_POINT('Origin',(1.13956910603496,-2.40556162109756,8.85049129520029));
#406845=CARTESIAN_POINT('Ctrl Pts',(1.14850738206914,-2.47758611705877,
8.78727029226991));
#406846=CARTESIAN_POINT('Ctrl Pts',(1.14821410598636,-2.48349114583243,
8.79393457792714));
#406847=CARTESIAN_POINT('Ctrl Pts',(1.13970751364645,-2.48500021903834,
8.79610912703474));
#406848=CARTESIAN_POINT('Ctrl Pts',(1.14968781879484,-2.45381836632824,
8.80838214965001));
#406849=CARTESIAN_POINT('Ctrl Pts',(1.14939459141809,-2.45972241442015,
8.81501364461992));
#406850=CARTESIAN_POINT('Ctrl Pts',(1.1409203259912,-2.46121761944617,8.81722098428721));
#406851=CARTESIAN_POINT('Ctrl Pts',(1.15086988603568,-2.43001778564902,
8.82945683644727));
#406852=CARTESIAN_POINT('Ctrl Pts',(1.15057781132211,-2.4358986252023,8.83607469902394));
#406853=CARTESIAN_POINT('Ctrl Pts',(1.14213547634265,-2.43740162972406,
8.8382956714852));
#406854=CARTESIAN_POINT('Ctrl Pts',(1.15205371787333,-2.40618167532513,
8.85049129520029));
#406855=CARTESIAN_POINT('Ctrl Pts',(1.15176404759819,-2.41201410220892,
8.85711686593484));
#406856=CARTESIAN_POINT('Ctrl Pts',(1.14335314149697,-2.4135494916287,8.85933012996512));
#406857=CARTESIAN_POINT('Origin',(1.13602277023077,-2.47696606283121,8.78727029226991));
#406858=CARTESIAN_POINT('Ctrl Pts',(1.14782096758314,-2.49140650154879,
8.75374538247848));
#406859=CARTESIAN_POINT('Ctrl Pts',(1.14745713259868,-2.49899675862557,
8.75304829418601));
#406860=CARTESIAN_POINT('Ctrl Pts',(1.14050185255765,-2.50214234644979,
8.75272238421917));
#406861=CARTESIAN_POINT('Ctrl Pts',(1.14775549109232,-2.49272486027965,
8.76769408445019));
#406862=CARTESIAN_POINT('Ctrl Pts',(1.14738181108972,-2.50050608886051,
8.76974318093969));
#406863=CARTESIAN_POINT('Ctrl Pts',(1.14057750714366,-2.50378020020404,
8.7707786988043));
#406864=CARTESIAN_POINT('Ctrl Pts',(1.14809108629953,-2.48596770444542,
8.78108014887992));
#406865=CARTESIAN_POINT('Ctrl Pts',(1.14777820098111,-2.4925621976085,8.78639403366325));
#406866=CARTESIAN_POINT('Ctrl Pts',(1.14019478891027,-2.49539308741434,
8.78812224174741));
#406867=CARTESIAN_POINT('Ctrl Pts',(1.14864105272565,-2.47489421768879,
8.78944554828685));
#406868=CARTESIAN_POINT('Ctrl Pts',(1.14838295601787,-2.48045207732235,
8.79673892988686));
#406869=CARTESIAN_POINT('Ctrl Pts',(1.13955245350739,-2.48168730188855,
8.79894799272499));
#406870=CARTESIAN_POINT('Origin',(1.13532718937381,-2.49097138142303,8.75721825406948));
#406871=CARTESIAN_POINT('Origin',(1.13532718937381,-2.49097138142303,9.));
#406872=CARTESIAN_POINT('Origin',(1.13532718937381,-2.49097138142303,7.51860402984325));
#406873=CARTESIAN_POINT('Ctrl Pts',(1.15623263920033,-2.49108385216064,
7.50366195182966));
#406874=CARTESIAN_POINT('Ctrl Pts',(1.15777435337912,-2.49440544953253,
7.50000065167736));
#406875=CARTESIAN_POINT('Ctrl Pts',(1.15777435337901,-2.49440544953258,
7.49482233047108));
#406876=CARTESIAN_POINT('Ctrl Pts',(1.15025678379846,-2.49551588914408,
7.50215800491337));
#406877=CARTESIAN_POINT('Ctrl Pts',(1.14912704537263,-2.49841905780325,
7.49877273257265));
#406878=CARTESIAN_POINT('Ctrl Pts',(1.14599578422564,-2.49987245381924,
7.49481816995649));
#406879=CARTESIAN_POINT('Ctrl Pts',(1.14767232585336,-2.49440656796782,
7.51043025814043));
#406880=CARTESIAN_POINT('Ctrl Pts',(1.14579758885199,-2.49993631643975,
7.51006209594516));
#406881=CARTESIAN_POINT('Ctrl Pts',(1.14050902793524,-2.50234673001258,
7.50731281821699));
#406882=CARTESIAN_POINT('Ctrl Pts',(1.14781187609329,-2.49158992609924,
7.51860402984326));
#406883=CARTESIAN_POINT('Ctrl Pts',(1.14743534212814,-2.49918987607038,
7.51860402984326));
#406884=CARTESIAN_POINT('Ctrl Pts',(1.14051133179104,-2.50234567996835,
7.51860402984327));
#406885=CARTESIAN_POINT('Origin',(0.,0.,7.5));
#406886=CARTESIAN_POINT('Origin',(1.30385128920423,-2.32742558187725,7.5));
#406887=CARTESIAN_POINT('',(1.30385128920423,-2.32742558187725,7.59394543036555));
#406888=CARTESIAN_POINT('',(1.30385128920423,-2.32742558187725,8.85049129520029));
#406889=CARTESIAN_POINT('',(1.30385128920423,-2.32742558187725,7.5));
#406890=CARTESIAN_POINT('',(1.30488713801677,-2.39891053004235,8.78727029226991));
#406891=CARTESIAN_POINT('Ctrl Pts',(1.30385128920423,-2.32742558187725,
8.85049129520029));
#406892=CARTESIAN_POINT('Ctrl Pts',(1.30419707404393,-2.35128853469732,
8.82945686509571));
#406893=CARTESIAN_POINT('Ctrl Pts',(1.30454234483265,-2.37511601235255,
8.80838212259895));
#406894=CARTESIAN_POINT('Ctrl Pts',(1.30488713801677,-2.39891053004236,
8.78727029226991));
#406895=CARTESIAN_POINT('',(1.30509031014836,-2.41293163922358,8.75721825406948));
#406896=CARTESIAN_POINT('Origin',(1.30447909650471,-2.37073725481645,8.75937679713112));
#406897=CARTESIAN_POINT('',(1.30509031014836,-2.41293163922358,7.51860402984325));
#406898=CARTESIAN_POINT('',(1.30509031014836,-2.41293163922358,7.5));
#406899=CARTESIAN_POINT('Ctrl Pts',(1.30509031014836,-2.41293163922358,
7.51860402984325));
#406900=CARTESIAN_POINT('Ctrl Pts',(1.30493075003824,-2.40192023865669,
7.52834476460825));
#406901=CARTESIAN_POINT('Ctrl Pts',(1.304771086344,-2.39090168964744,7.53807742314407));
#406902=CARTESIAN_POINT('Ctrl Pts',(1.30461131558766,-2.37987575217737,
7.54780169004674));
#406903=CARTESIAN_POINT('Ctrl Pts',(1.30435824734449,-2.36241126312585,
7.5632044032688));
#406904=CARTESIAN_POINT('Ctrl Pts',(1.30410491017452,-2.34492821517236,
7.57858609112103));
#406905=CARTESIAN_POINT('Ctrl Pts',(1.30385128920423,-2.32742558187725,
7.59394543036555));
#406906=CARTESIAN_POINT('Origin',(1.54744838731667,-2.46744938832929,7.5));
#406907=CARTESIAN_POINT('',(1.38685191115373,-2.36688436340659,8.75721825406948));
#406908=CARTESIAN_POINT('',(1.3749671840312,-2.35944218342959,8.78727029226991));
#406909=CARTESIAN_POINT('Origin',(1.34479931381015,-2.34055115485206,8.75658640620957));
#406910=CARTESIAN_POINT('',(1.31437432427031,-2.32149911893913,8.85049129520029));
#406911=CARTESIAN_POINT('Ctrl Pts',(1.3749671840312,-2.35944218342959,8.78727029226991));
#406912=CARTESIAN_POINT('Ctrl Pts',(1.35479821265381,-2.34681243489654,
8.80838212259896));
#406913=CARTESIAN_POINT('Ctrl Pts',(1.33460130338719,-2.33416519174222,
8.82945686509571));
#406914=CARTESIAN_POINT('Ctrl Pts',(1.31437432427031,-2.32149911893913,
8.85049129520029));
#406915=CARTESIAN_POINT('',(1.31437432427031,-2.32149911893913,7.59394543036555));
#406916=CARTESIAN_POINT('',(1.31437432427031,-2.32149911893913,7.5));
#406917=CARTESIAN_POINT('',(1.38685191115373,-2.36688436340659,7.51860402984325));
#406918=CARTESIAN_POINT('Ctrl Pts',(1.31437432427031,-2.32149911893913,
7.59394543036555));
#406919=CARTESIAN_POINT('Ctrl Pts',(1.32921009923999,-2.33078923610247,
7.57858609112103));
#406920=CARTESIAN_POINT('Ctrl Pts',(1.34402927306632,-2.34006895768036,
7.56320440326857));
#406921=CARTESIAN_POINT('Ctrl Pts',(1.35883271579178,-2.3493388284907,7.54780169004651));
#406922=CARTESIAN_POINT('Ctrl Pts',(1.36817864245194,-2.35519121933987,
7.53807742314383));
#406923=CARTESIAN_POINT('Ctrl Pts',(1.37751830642368,-2.36103968851258,
7.52834476460825));
#406924=CARTESIAN_POINT('Ctrl Pts',(1.38685191115373,-2.36688436340659,
7.51860402984325));
#406925=CARTESIAN_POINT('',(1.38685191115373,-2.36688436340659,7.5));
#406926=CARTESIAN_POINT('Origin',(1.31072556753556,-2.32732597051529,7.5));
#406927=CARTESIAN_POINT('Ctrl Pts',(1.31437432427031,-2.32149911893913,
8.85049129520029));
#406928=CARTESIAN_POINT('Ctrl Pts',(1.31421018800108,-2.32139633730655,
8.85097269580138));
#406929=CARTESIAN_POINT('Ctrl Pts',(1.3140436584404,-2.32130198148024,8.85143669361005));
#406930=CARTESIAN_POINT('Ctrl Pts',(1.31386663644423,-2.3212124673486,8.8519052845931));
#406931=CARTESIAN_POINT('Ctrl Pts',(1.31352039264605,-2.32103738338388,
8.85282181883899));
#406932=CARTESIAN_POINT('Ctrl Pts',(1.3131428261905,-2.32088550184336,8.85372622499635));
#406933=CARTESIAN_POINT('Ctrl Pts',(1.31272225812331,-2.32076874418765,
8.85462257735071));
#406934=CARTESIAN_POINT('Ctrl Pts',(1.31237311745109,-2.32067181612873,
8.85536669723986));
#406935=CARTESIAN_POINT('Ctrl Pts',(1.31199427006963,-2.32059904195064,
8.85610498449051));
#406936=CARTESIAN_POINT('Ctrl Pts',(1.31157749224831,-2.32056509502165,
8.85681338218371));
#406937=CARTESIAN_POINT('Ctrl Pts',(1.31119926572089,-2.32053428813029,
8.85745625420284));
#406938=CARTESIAN_POINT('Ctrl Pts',(1.31078510535873,-2.32053447481711,
8.85808743050666));
#406939=CARTESIAN_POINT('Ctrl Pts',(1.31032267718113,-2.32059145661444,
8.85866804508411));
#406940=CARTESIAN_POINT('Ctrl Pts',(1.3101093228442,-2.32061774678051,8.85893592806396));
#406941=CARTESIAN_POINT('Ctrl Pts',(1.30988561604852,-2.32065635649647,
8.85919241173848));
#406942=CARTESIAN_POINT('Ctrl Pts',(1.30965004993186,-2.32071138836425,
8.85943017985534));
#406943=CARTESIAN_POINT('Ctrl Pts',(1.30933196593933,-2.32078569767693,
8.8597512372));
#406944=CARTESIAN_POINT('Ctrl Pts',(1.30898430850721,-2.32089246461107,
8.86004599534706));
#406945=CARTESIAN_POINT('Ctrl Pts',(1.30861431218769,-2.32104036257473,
8.86026130871721));
#406946=CARTESIAN_POINT('Ctrl Pts',(1.30847884610382,-2.32109451218891,
8.86034014101235));
#406947=CARTESIAN_POINT('Ctrl Pts',(1.30833834607235,-2.32115497735332,
8.86040910639692));
#406948=CARTESIAN_POINT('Ctrl Pts',(1.30819677290977,-2.32122041970919,
8.86046313645506));
#406949=CARTESIAN_POINT('Ctrl Pts',(1.30797584917523,-2.32132254195747,
8.86054744990829));
#406950=CARTESIAN_POINT('Ctrl Pts',(1.30774634336655,-2.32143970543497,
8.86059655985669));
#406951=CARTESIAN_POINT('Ctrl Pts',(1.30752284118752,-2.32156413516751,
8.86059725258816));
#406952=CARTESIAN_POINT('Ctrl Pts',(1.30729882262918,-2.32168885238244,
8.86059794692012));
#406953=CARTESIAN_POINT('Ctrl Pts',(1.30707964340312,-2.32182457387433,
8.86056369958366));
#406954=CARTESIAN_POINT('Ctrl Pts',(1.30687527651368,-2.3219606979511,8.86048590497774));
#406955=CARTESIAN_POINT('Ctrl Pts',(1.30682194284028,-2.32199622228223,
8.86046560290182));
#406956=CARTESIAN_POINT('Ctrl Pts',(1.30676897434056,-2.32203231156962,
8.86044257503091));
#406957=CARTESIAN_POINT('Ctrl Pts',(1.30671798930178,-2.32206782349642,
8.86041778462583));
#406958=CARTESIAN_POINT('Ctrl Pts',(1.30637492325794,-2.32230677469718,
8.86025097596201));
#406959=CARTESIAN_POINT('Ctrl Pts',(1.30607581555714,-2.3225519216236,8.8599848982295));
#406960=CARTESIAN_POINT('Ctrl Pts',(1.30582402572537,-2.32278955627459,
8.85968173251461));
#406961=CARTESIAN_POINT('Ctrl Pts',(1.30569084333021,-2.32291525139012,
8.85952137522076));
#406962=CARTESIAN_POINT('Ctrl Pts',(1.30556820129056,-2.32304112870654,
8.85934740853961));
#406963=CARTESIAN_POINT('Ctrl Pts',(1.30545671568011,-2.32316432824296,
8.8591675900182));
#406964=CARTESIAN_POINT('Ctrl Pts',(1.30500904300508,-2.32365903841951,
8.85844552518696));
#406965=CARTESIAN_POINT('Ctrl Pts',(1.30471371598155,-2.32413650056776,
8.85759444184126));
#406966=CARTESIAN_POINT('Ctrl Pts',(1.30450788915532,-2.32454742583239,
8.85683498915141));
#406967=CARTESIAN_POINT('Ctrl Pts',(1.30448634992612,-2.32459042806696,
8.85675551445));
#406968=CARTESIAN_POINT('Ctrl Pts',(1.30446581007889,-2.32463270692615,
8.85667699793652));
#406969=CARTESIAN_POINT('Ctrl Pts',(1.30444621042253,-2.32467420873585,
8.85659965593547));
#406970=CARTESIAN_POINT('Ctrl Pts',(1.30418165326101,-2.32523440228085,
8.85555568965886));
#406971=CARTESIAN_POINT('Ctrl Pts',(1.30400830047065,-2.32581099027345,
8.85434650606346));
#406972=CARTESIAN_POINT('Ctrl Pts',(1.30391934352442,-2.32640503368347,
8.85297329937117));
#406973=CARTESIAN_POINT('Ctrl Pts',(1.3038693106624,-2.32673914690601,8.85220095427747));
#406974=CARTESIAN_POINT('Ctrl Pts',(1.30384626657238,-2.32707896510007,
8.85137579139183));
#406975=CARTESIAN_POINT('Ctrl Pts',(1.30385128920423,-2.32742558187725,
8.85049129520029));
#406976=CARTESIAN_POINT('Origin',(1.31072556753556,-2.32732597051529,7.59394543036555));
#406977=CARTESIAN_POINT('Ctrl Pts',(1.31389778130987,-2.3212007091867,7.59443877723642));
#406978=CARTESIAN_POINT('Ctrl Pts',(1.30898984733472,-2.31812737585883,
7.58783886950016));
#406979=CARTESIAN_POINT('Ctrl Pts',(1.30294132309855,-2.32408510496488,
7.58559994247159));
#406980=CARTESIAN_POINT('Ctrl Pts',(1.34069004888756,-2.33797794565578,
7.56670252222133));
#406981=CARTESIAN_POINT('Ctrl Pts',(1.33578920827041,-2.33490905416709,
7.56004874999026));
#406982=CARTESIAN_POINT('Ctrl Pts',(1.32968985135374,-2.340886863336,7.55786368756704));
#406983=CARTESIAN_POINT('Ctrl Pts',(1.36743228458249,-2.35472385231203,
7.53888913333561));
#406984=CARTESIAN_POINT('Ctrl Pts',(1.36250231802957,-2.35163672225099,
7.53222002137281));
#406985=CARTESIAN_POINT('Ctrl Pts',(1.35638999749712,-2.35765685368048,
7.53005029815327));
#406986=CARTESIAN_POINT('Ctrl Pts',(1.39412327829026,-2.37143767139179,
7.51101258149734));
#406987=CARTESIAN_POINT('Ctrl Pts',(1.38913355158475,-2.36831311970494,
7.5043616886572));
#406988=CARTESIAN_POINT('Ctrl Pts',(1.38304039838404,-2.37439431741734,
7.50217374673251));
#406989=CARTESIAN_POINT('',(1.3816182993051,-2.37350118398174,7.50366116523517));
#406990=CARTESIAN_POINT('Ctrl Pts',(1.38685191115373,-2.36688436340659,
7.51860402984325));
#406991=CARTESIAN_POINT('Ctrl Pts',(1.3872261952276,-2.36711873895528,7.51734760759493));
#406992=CARTESIAN_POINT('Ctrl Pts',(1.38753283777153,-2.36738095682314,
7.51608817408573));
#406993=CARTESIAN_POINT('Ctrl Pts',(1.38776245486761,-2.36768056285119,
7.5148100591312));
#406994=CARTESIAN_POINT('Ctrl Pts',(1.38797044752012,-2.36795195315072,
7.51365231206384));
#406995=CARTESIAN_POINT('Ctrl Pts',(1.38811573123279,-2.36825425143914,
7.51247773061043));
#406996=CARTESIAN_POINT('Ctrl Pts',(1.38816251106135,-2.36859822163467,
7.51129758471022));
#406997=CARTESIAN_POINT('Ctrl Pts',(1.38822065304579,-2.36902573730484,
7.50983079813401));
#406998=CARTESIAN_POINT('Ctrl Pts',(1.38811186827433,-2.36950573745491,
7.50839324291155));
#406999=CARTESIAN_POINT('Ctrl Pts',(1.3877549621655,-2.37002350371511,7.50715379678855));
#407000=CARTESIAN_POINT('Ctrl Pts',(1.38759008182723,-2.37026269680825,
7.50658120839351));
#407001=CARTESIAN_POINT('Ctrl Pts',(1.3873409856815,-2.37053856065068,7.50598221009429));
#407002=CARTESIAN_POINT('Ctrl Pts',(1.38699671946609,-2.37082928581173,
7.50545747549611));
#407003=CARTESIAN_POINT('Ctrl Pts',(1.38681300835751,-2.37098442575645,
7.50517746087247));
#407004=CARTESIAN_POINT('Ctrl Pts',(1.38660033499764,-2.3711456346244,7.50491486231392));
#407005=CARTESIAN_POINT('Ctrl Pts',(1.3863633237229,-2.37130731404933,7.50468370960992));
#407006=CARTESIAN_POINT('Ctrl Pts',(1.3860089171062,-2.37154907578849,7.50433806340446));
#407007=CARTESIAN_POINT('Ctrl Pts',(1.38558915067019,-2.37179867932594,
7.50405484070983));
#407008=CARTESIAN_POINT('Ctrl Pts',(1.3851319287582,-2.37203869856845,7.5038576603613));
#407009=CARTESIAN_POINT('Ctrl Pts',(1.38508303598156,-2.37206436489568,
7.50383657498791));
#407010=CARTESIAN_POINT('Ctrl Pts',(1.385033743229,-2.37208992304648,7.50381643264937));
#407011=CARTESIAN_POINT('Ctrl Pts',(1.38498410518476,-2.37211535306455,
7.50379723213559));
#407012=CARTESIAN_POINT('Ctrl Pts',(1.38465275500168,-2.37228510675388,
7.50366906242519));
#407013=CARTESIAN_POINT('Ctrl Pts',(1.38429848313331,-2.37245220342953,
7.50358235568538));
#407014=CARTESIAN_POINT('Ctrl Pts',(1.3839531370876,-2.37260505571624,7.5035341175365));
#407015=CARTESIAN_POINT('Ctrl Pts',(1.3834353297777,-2.37283424042062,7.50346178989176));
#407016=CARTESIAN_POINT('Ctrl Pts',(1.38286854227575,-2.37305877444104,
7.50346967198527));
#407017=CARTESIAN_POINT('Ctrl Pts',(1.38230535013553,-2.37326207654002,
7.50354272648692));
#407018=CARTESIAN_POINT('Ctrl Pts',(1.38207369755087,-2.37334569890143,
7.50357277531559));
#407019=CARTESIAN_POINT('Ctrl Pts',(1.38184300918211,-2.37342575141274,
7.50361331098761));
#407020=CARTESIAN_POINT('Ctrl Pts',(1.38161829930581,-2.37350118398297,
7.50366116523659));
#407021=CARTESIAN_POINT('',(1.31216235181344,-2.32987712649126,7.57603338622103));
#407022=CARTESIAN_POINT('Origin',(1.31649630659949,-2.33757831636798,7.58486873427628));
#407023=CARTESIAN_POINT('Ctrl Pts',(1.3816182993563,-2.37350118400757,7.50366116529969));
#407024=CARTESIAN_POINT('Ctrl Pts',(1.3585036515569,-2.35898426780922,7.5278357307971));
#407025=CARTESIAN_POINT('Ctrl Pts',(1.33535275265204,-2.34444361706053,
7.55196141284068));
#407026=CARTESIAN_POINT('Ctrl Pts',(1.31216235301863,-2.32987712683062,
7.57603338728831));
#407027=CARTESIAN_POINT('Ctrl Pts',(1.3151526330441,-2.3221939361617,7.59639677331372));
#407028=CARTESIAN_POINT('Ctrl Pts',(1.30074331794073,-2.30960147554746,
7.59974925422225));
#407029=CARTESIAN_POINT('Ctrl Pts',(1.30404198763954,-2.3284513350771,7.59639677331371));
#407030=CARTESIAN_POINT('Ctrl Pts',(1.31266628426861,-2.31918841227221,
7.58707626057423));
#407031=CARTESIAN_POINT('Ctrl Pts',(1.30579990181469,-2.31857995225022,
7.58811717123966));
#407032=CARTESIAN_POINT('Ctrl Pts',(1.30276074036381,-2.32476711066725,
7.58707626057422));
#407033=CARTESIAN_POINT('Ctrl Pts',(1.31201671782416,-2.32523024110921,
7.5801537675693));
#407034=CARTESIAN_POINT('Ctrl Pts',(1.30919143812989,-2.32460196840805,
7.5820876076604));
#407035=CARTESIAN_POINT('Ctrl Pts',(1.30826409698657,-2.32734367779122,
7.58015376756929));
#407036=CARTESIAN_POINT('Ctrl Pts',(1.31216235140752,-2.32987712577008,
7.57603338509286));
#407037=CARTESIAN_POINT('Ctrl Pts',(1.31216235140752,-2.32987712577008,
7.57603338509286));
#407038=CARTESIAN_POINT('Ctrl Pts',(1.31216235140752,-2.32987712577008,
7.57603338509286));
#407039=CARTESIAN_POINT('Origin',(1.31650127865133,-2.3375755161612,7.58486873427622));
#407040=CARTESIAN_POINT('Ctrl Pts',(1.30521500871195,-2.42153721008158,
7.51098857897448));
#407041=CARTESIAN_POINT('Ctrl Pts',(1.30512970780234,-2.41565051018039,
7.50433767179956));
#407042=CARTESIAN_POINT('Ctrl Pts',(1.31348868127021,-2.41359244952874,
7.50214974420965));
#407043=CARTESIAN_POINT('Ctrl Pts',(1.3047585888223,-2.39003922334996,7.53887321589166));
#407044=CARTESIAN_POINT('Ctrl Pts',(1.30467430996897,-2.38422305656059,
7.53220407452061));
#407045=CARTESIAN_POINT('Ctrl Pts',(1.31299098755429,-2.38211692411852,
7.53003438070911));
#407046=CARTESIAN_POINT('Ctrl Pts',(1.30430129243809,-2.35848074886471,
7.56669465659234));
#407047=CARTESIAN_POINT('Ctrl Pts',(1.30421751165708,-2.35269895453973,
7.56004085833299));
#407048=CARTESIAN_POINT('Ctrl Pts',(1.31249126537343,-2.350581963853,7.55785582193789));
#407049=CARTESIAN_POINT('Ctrl Pts',(1.30384314024102,-2.32686321388927,
7.59443891967696));
#407050=CARTESIAN_POINT('Ctrl Pts',(1.30375923798833,-2.32107303668239,
7.58783901202978));
#407051=CARTESIAN_POINT('Ctrl Pts',(1.31198945670399,-2.31898912740396,
7.58560008491213));
#407052=CARTESIAN_POINT('',(1.31346170186506,-2.41188626453886,7.50366116523517));
#407053=CARTESIAN_POINT('Ctrl Pts',(1.31346170186524,-2.41188626453919,
7.50366116523554));
#407054=CARTESIAN_POINT('Ctrl Pts',(1.31288301264091,-2.41237540286155,
7.50350835821027));
#407055=CARTESIAN_POINT('Ctrl Pts',(1.31233514318617,-2.41280621264754,
7.50345484956));
#407056=CARTESIAN_POINT('Ctrl Pts',(1.31180217608123,-2.41319197426492,
7.50349758195598));
#407057=CARTESIAN_POINT('Ctrl Pts',(1.31152872443053,-2.41338989858346,
7.50351950684424));
#407058=CARTESIAN_POINT('Ctrl Pts',(1.31123231915291,-2.41359557726914,
7.50357029184312));
#407059=CARTESIAN_POINT('Ctrl Pts',(1.31094104715448,-2.41378605423314,
7.50365515313923));
#407060=CARTESIAN_POINT('Ctrl Pts',(1.3104929528732,-2.4140790849355,7.50378570417639));
#407061=CARTESIAN_POINT('Ctrl Pts',(1.31004404409646,-2.41434503002182,
7.50400001621911));
#407062=CARTESIAN_POINT('Ctrl Pts',(1.30962733207943,-2.4145616938471,7.50428903009635));
#407063=CARTESIAN_POINT('Ctrl Pts',(1.30958108025154,-2.4145857418648,7.50432110841318));
#407064=CARTESIAN_POINT('Ctrl Pts',(1.30953521085967,-2.41460920955342,
7.50435406373355));
#407065=CARTESIAN_POINT('Ctrl Pts',(1.30948975828797,-2.4146320861886,7.50438785222352));
#407066=CARTESIAN_POINT('Ctrl Pts',(1.30921224849042,-2.41477175904227,
7.50459414719561));
#407067=CARTESIAN_POINT('Ctrl Pts',(1.30894562634667,-2.41489116230397,
7.50483629897752));
#407068=CARTESIAN_POINT('Ctrl Pts',(1.30870064396404,-2.41498692275759,
7.5050991045531));
#407069=CARTESIAN_POINT('Ctrl Pts',(1.30816018822179,-2.41519817993649,
7.50567888004914));
#407070=CARTESIAN_POINT('Ctrl Pts',(1.30770394295143,-2.41530317974192,
7.50637912803145));
#407071=CARTESIAN_POINT('Ctrl Pts',(1.30733073613186,-2.41533280978828,
7.50710440483569));
#407072=CARTESIAN_POINT('Ctrl Pts',(1.30723921841051,-2.41534007566388,
7.50728225710685));
#407073=CARTESIAN_POINT('Ctrl Pts',(1.30715088373331,-2.41534309947923,
7.50746498566954));
#407074=CARTESIAN_POINT('Ctrl Pts',(1.30706780836973,-2.41534222699802,
7.50764697238949));
#407075=CARTESIAN_POINT('Ctrl Pts',(1.30662121807804,-2.41533753677912,
7.50862528291181));
#407076=CARTESIAN_POINT('Ctrl Pts',(1.3062860297497,-2.41522396277347,7.50965856837421));
#407077=CARTESIAN_POINT('Ctrl Pts',(1.30602487717234,-2.41505626958657,
7.51067959873201));
#407078=CARTESIAN_POINT('Ctrl Pts',(1.30588116457962,-2.4149639878143,7.51124147302578));
#407079=CARTESIAN_POINT('Ctrl Pts',(1.30576007199096,-2.41485492899367,
7.51180065547252));
#407080=CARTESIAN_POINT('Ctrl Pts',(1.30565692234312,-2.41473598925369,
7.512351757165));
#407081=CARTESIAN_POINT('Ctrl Pts',(1.3053004992199,-2.41432500507207,7.51425603304536));
#407082=CARTESIAN_POINT('Ctrl Pts',(1.30512039563905,-2.4137430693988,7.51626900505181));
#407083=CARTESIAN_POINT('Ctrl Pts',(1.30509334076503,-2.41304587007462,
7.51827788969244));
#407084=CARTESIAN_POINT('Ctrl Pts',(1.30509187650413,-2.41300813632967,
7.51838661432546));
#407085=CARTESIAN_POINT('Ctrl Pts',(1.30509086684248,-2.41297005723368,
7.51849533314857));
#407086=CARTESIAN_POINT('Ctrl Pts',(1.30509031014836,-2.41293163922358,
7.51860402984325));
#407087=CARTESIAN_POINT('Ctrl Pts',(1.31216235147925,-2.32987712769895,
7.57603338728985));
#407088=CARTESIAN_POINT('Ctrl Pts',(1.31259704935578,-2.35725939040437,
7.55196141284922));
#407089=CARTESIAN_POINT('Ctrl Pts',(1.31303012767148,-2.38459447936898,
7.52783573083105));
#407090=CARTESIAN_POINT('Ctrl Pts',(1.31346170186056,-2.41188626459787,
7.50366116530176));
#407091=CARTESIAN_POINT('Origin',(4.53412748053618E-16,-8.0508024718856E-16,
7.49482233047033));
#407092=CARTESIAN_POINT('Origin',(1.37717168998616,-2.3658622923367,7.49482233047033));
#407093=CARTESIAN_POINT('Origin',(0.,0.,7.50366116523517));
#407094=CARTESIAN_POINT('Origin',(1.30923444818254,-2.40412383410094,7.49482233047033));
#407095=CARTESIAN_POINT('Ctrl Pts',(1.38685101471507,-2.36688380200663,
7.51860402984325));
#407096=CARTESIAN_POINT('Ctrl Pts',(1.39329958728445,-2.37092263820628,
7.51860402984325));
#407097=CARTESIAN_POINT('Ctrl Pts',(1.39984896414485,-2.36704940328304,
7.51860402984325));
#407098=CARTESIAN_POINT('Ctrl Pts',(1.38924541439193,-2.36838344837307,
7.51041458714365));
#407099=CARTESIAN_POINT('Ctrl Pts',(1.39485120463891,-2.37000501596869,
7.51004642900441));
#407100=CARTESIAN_POINT('Ctrl Pts',(1.39985077038522,-2.36704833509084,
7.50729136483009));
#407101=CARTESIAN_POINT('Ctrl Pts',(1.38866594195957,-2.37113807155953,
7.50215815450138));
#407102=CARTESIAN_POINT('Ctrl Pts',(1.39169202834611,-2.37187350725535,
7.49877163671532));
#407103=CARTESIAN_POINT('Ctrl Pts',(1.39467384947403,-2.37013780383728,
7.49481588533172));
#407104=CARTESIAN_POINT('Ctrl Pts',(1.38161802235206,-2.37350070820122,
7.50366171572174));
#407105=CARTESIAN_POINT('Ctrl Pts',(1.38346014519125,-2.37666531650282,
7.50000045605858));
#407106=CARTESIAN_POINT('Ctrl Pts',(1.38346014519135,-2.37666531650275,
7.49482233047317));
#407107=CARTESIAN_POINT('Origin',(1.39348601430782,-2.35629008781358,7.51860402984325));
#407108=CARTESIAN_POINT('Origin',(1.39348601430782,-2.35629008781358,9.));
#407109=CARTESIAN_POINT('Origin',(1.39348601430782,-2.35629008781358,8.75721825406948));
#407110=CARTESIAN_POINT('Ctrl Pts',(1.37269783844897,-2.35802109048348,
8.78942910404912));
#407111=CARTESIAN_POINT('Ctrl Pts',(1.37740998531032,-2.3609956661942,8.79672699501691));
#407112=CARTESIAN_POINT('Ctrl Pts',(1.38347973220101,-2.35445107616387,
8.79893251111267));
#407113=CARTESIAN_POINT('Ctrl Pts',(1.38201599788308,-2.36385609892402,
8.78111911759583));
#407114=CARTESIAN_POINT('Ctrl Pts',(1.38760627609689,-2.36737619830013,
8.78644465894813));
#407115=CARTESIAN_POINT('Ctrl Pts',(1.39426522839043,-2.36275301042509,
8.78817647674131));
#407116=CARTESIAN_POINT('Ctrl Pts',(1.38782329711837,-2.36749261533527,
8.76780923932029));
#407117=CARTESIAN_POINT('Ctrl Pts',(1.39442509977367,-2.37164363189401,
8.76988516158374));
#407118=CARTESIAN_POINT('Ctrl Pts',(1.40100847884786,-2.36792940245014,
8.77093053738833));
#407119=CARTESIAN_POINT('Ctrl Pts',(1.38669095324689,-2.36678354440284,
8.75371302330492));
#407120=CARTESIAN_POINT('Ctrl Pts',(1.39313032119299,-2.37083332733808,
8.75300828287559));
#407121=CARTESIAN_POINT('Ctrl Pts',(1.39969354974844,-2.36691943282451,
8.75267964240738));
#407122=CARTESIAN_POINT('Origin',(1.3816012871853,-2.34884790783658,8.78727029226991));
#407123=CARTESIAN_POINT('Ctrl Pts',(1.31437432427031,-2.32149911893913,
8.85049129520029));
#407124=CARTESIAN_POINT('Ctrl Pts',(1.31932364416771,-2.32459836800564,
8.85711686593484));
#407125=CARTESIAN_POINT('Ctrl Pts',(1.32539494747705,-2.31857839805223,
8.85933012996512));
#407126=CARTESIAN_POINT('Ctrl Pts',(1.33460133053255,-2.33416520874056,
8.82945683644721));
#407127=CARTESIAN_POINT('Ctrl Pts',(1.33959173277752,-2.33729018344815,
8.83607469902389));
#407128=CARTESIAN_POINT('Ctrl Pts',(1.34565445587691,-2.33122590846116,
8.8382956714852));
#407129=CARTESIAN_POINT('Ctrl Pts',(1.35479818681085,-2.34681241871376,
8.80838214965003));
#407130=CARTESIAN_POINT('Ctrl Pts',(1.35980828351311,-2.34994972603058,
8.81501364461993));
#407131=CARTESIAN_POINT('Ctrl Pts',(1.36588287762337,-2.34385480035506,
8.81722098428721));
#407132=CARTESIAN_POINT('Ctrl Pts',(1.3749671840312,-2.35944218342959,8.78727029226991));
#407133=CARTESIAN_POINT('Ctrl Pts',(1.37997811292692,-2.36258001186347,
8.79393457792714));
#407134=CARTESIAN_POINT('Ctrl Pts',(1.38608257609909,-2.35646650676755,
8.79610912703474));
#407135=CARTESIAN_POINT('Origin',(1.32100842742441,-2.31090484334611,8.85049129520029));
#407136=CARTESIAN_POINT('Ctrl Pts',(1.30385128920423,-2.32742558187725,
8.85049129520029));
#407137=CARTESIAN_POINT('Ctrl Pts',(1.3039358989612,-2.33326458465274,8.85711686593484));
#407138=CARTESIAN_POINT('Ctrl Pts',(1.29564064670651,-2.33533570805443,
8.85933012996512));
#407139=CARTESIAN_POINT('Ctrl Pts',(1.30377643617359,-2.32225990040868,
8.86332496987232));
#407140=CARTESIAN_POINT('Ctrl Pts',(1.29989627515225,-2.32476913232805,
8.86648636486736));
#407141=CARTESIAN_POINT('Ctrl Pts',(1.29544837314915,-2.32088425528192,
8.87206031107457));
#407142=CARTESIAN_POINT('Ctrl Pts',(1.30996597848913,-2.31873862621884,
8.86341338519877));
#407143=CARTESIAN_POINT('Ctrl Pts',(1.31412198473723,-2.31668897193089,
8.86654584966059));
#407144=CARTESIAN_POINT('Ctrl Pts',(1.31304352587506,-2.31086135841679,
8.87215952290714));
#407145=CARTESIAN_POINT('Ctrl Pts',(1.31437432427031,-2.32149911893913,
8.85049129520029));
#407146=CARTESIAN_POINT('Ctrl Pts',(1.31932364416771,-2.32459836800564,
8.85711686593484));
#407147=CARTESIAN_POINT('Ctrl Pts',(1.32539494747705,-2.31857839805223,
8.85933012996512));
#407148=CARTESIAN_POINT('Origin',(1.29135260132909,-2.32760669344446,8.85049129520029));
#407149=CARTESIAN_POINT('Ctrl Pts',(1.30488713801677,-2.39891053004235,
8.78727029226991));
#407150=CARTESIAN_POINT('Ctrl Pts',(1.30497280099367,-2.40482221656422,
8.79393457792714));
#407151=CARTESIAN_POINT('Ctrl Pts',(1.29658037301232,-2.40687320845989,
8.79610912703474));
#407152=CARTESIAN_POINT('Ctrl Pts',(1.30454234439086,-2.3751159818641,8.80838214965001));
#407153=CARTESIAN_POINT('Ctrl Pts',(1.30462799314122,-2.38102668659853,
8.81501364461992));
#407154=CARTESIAN_POINT('Ctrl Pts',(1.29626693711645,-2.38306176761555,
8.8172209842872));
#407155=CARTESIAN_POINT('Ctrl Pts',(1.30419707450798,-2.35128856672228,
8.82945683644722));
#407156=CARTESIAN_POINT('Ctrl Pts',(1.3042823865771,-2.35717603675113,8.83607469902389));
#407157=CARTESIAN_POINT('Ctrl Pts',(1.29595369511065,-2.35921685544822,
8.83829567148521));
#407158=CARTESIAN_POINT('Ctrl Pts',(1.30385128920423,-2.32742558187725,
8.85049129520029));
#407159=CARTESIAN_POINT('Ctrl Pts',(1.3039358989612,-2.33326458465274,8.85711686593484));
#407160=CARTESIAN_POINT('Ctrl Pts',(1.29564064670651,-2.33533570805443,
8.85933012996512));
#407161=CARTESIAN_POINT('Origin',(1.29238845014162,-2.39909164160956,8.78727029226991));
#407162=CARTESIAN_POINT('Ctrl Pts',(1.30508760891743,-2.41274649779731,
8.75374538247848));
#407163=CARTESIAN_POINT('Ctrl Pts',(1.3052108309116,-2.42034447086437,8.75304829418602));
#407164=CARTESIAN_POINT('Ctrl Pts',(1.29847137974323,-2.4239292220633,8.75272238421917));
#407165=CARTESIAN_POINT('Ctrl Pts',(1.30510673448899,-2.41406634291195,
8.76769408445019));
#407166=CARTESIAN_POINT('Ctrl Pts',(1.30523236727893,-2.42185552588413,
8.76974318093968));
#407167=CARTESIAN_POINT('Ctrl Pts',(1.2986518165391,-2.42555886346539,8.7707786988043));
#407168=CARTESIAN_POINT('Ctrl Pts',(1.30500870771911,-2.4073015687203,8.78108014887989));
#407169=CARTESIAN_POINT('Ctrl Pts',(1.30511897588475,-2.41390255942111,
8.78639403366326));
#407170=CARTESIAN_POINT('Ctrl Pts',(1.29773252047994,-2.41721350373984,
8.78812224174741));
#407171=CARTESIAN_POINT('Ctrl Pts',(1.30484806344777,-2.39621559715997,
8.78944554828685));
#407172=CARTESIAN_POINT('Ctrl Pts',(1.30494659031671,-2.40177857388768,
8.79673892988685));
#407173=CARTESIAN_POINT('Ctrl Pts',(1.29621337213039,-2.40357703279091,
8.79894799272499));
#407174=CARTESIAN_POINT('Origin',(1.29259162227322,-2.41311275079079,8.75721825406948));
#407175=CARTESIAN_POINT('Origin',(1.29259162227322,-2.41311275079079,9.));
#407176=CARTESIAN_POINT('Origin',(1.29259162227322,-2.41311275079079,7.51860402984325));
#407177=CARTESIAN_POINT('Ctrl Pts',(1.31346132563586,-2.41188557367602,
7.50366195182966));
#407178=CARTESIAN_POINT('Ctrl Pts',(1.31521268767183,-2.41510156850329,
7.50000065167735));
#407179=CARTESIAN_POINT('Ctrl Pts',(1.31521268767173,-2.41510156850335,
7.49482233047108));
#407180=CARTESIAN_POINT('Ctrl Pts',(1.30778170985432,-2.41669137893432,
7.50215800491337));
#407181=CARTESIAN_POINT('Ctrl Pts',(1.30684029925188,-2.41966096531158,
7.49877273257265));
#407182=CARTESIAN_POINT('Ctrl Pts',(1.30380859101921,-2.42131199576008,
7.49481816995649));
#407183=CARTESIAN_POINT('Ctrl Pts',(1.30513148750345,-2.41574992376647,
7.51043025814043));
#407184=CARTESIAN_POINT('Ctrl Pts',(1.30361489455136,-2.42138842558917,
7.51006209594515));
#407185=CARTESIAN_POINT('Ctrl Pts',(1.29849163527805,-2.42413272597012,
7.50731281821699));
#407186=CARTESIAN_POINT('Ctrl Pts',(1.30509028815832,-2.41293012797612,
7.51860402984326));
#407187=CARTESIAN_POINT('Ctrl Pts',(1.30520145828909,-2.42053858764892,
7.51860402984326));
#407188=CARTESIAN_POINT('Ctrl Pts',(1.29849386712378,-2.42413153047477,
7.51860402984327));
#407189=CARTESIAN_POINT('Origin',(0.,0.,7.5));
#407190=CARTESIAN_POINT('Origin',(1.45029105591256,-2.23910559748222,7.5));
#407191=CARTESIAN_POINT('',(1.45029105591256,-2.23910559748222,7.59394543036555));
#407192=CARTESIAN_POINT('',(1.45029105591256,-2.23910559748222,8.85049129520029));
#407193=CARTESIAN_POINT('',(1.45029105591256,-2.23910559748222,7.5));
#407194=CARTESIAN_POINT('',(1.45590483281687,-2.3103773050933,8.78727029226991));
#407195=CARTESIAN_POINT('Ctrl Pts',(1.45029105591256,-2.23910559748222,
8.85049129520029));
#407196=CARTESIAN_POINT('Ctrl Pts',(1.45216503493679,-2.26289736679568,
8.82945686509571));
#407197=CARTESIAN_POINT('Ctrl Pts',(1.45403622806461,-2.2866537667672,8.80838212259896));
#407198=CARTESIAN_POINT('Ctrl Pts',(1.45590483281687,-2.3103773050933,8.78727029226991));
#407199=CARTESIAN_POINT('',(1.45700592305914,-2.32435658911879,8.75721825406948));
#407200=CARTESIAN_POINT('Origin',(1.45369256172862,-2.28228805819315,8.75937679713143));
#407201=CARTESIAN_POINT('',(1.45700592305914,-2.32435658911879,7.51860402984325));
#407202=CARTESIAN_POINT('',(1.45700592305914,-2.32435658911879,7.5));
#407203=CARTESIAN_POINT('Ctrl Pts',(1.45700592305915,-2.32435658911879,
7.51860402984325));
#407204=CARTESIAN_POINT('Ctrl Pts',(1.45614118792576,-2.31337803570668,
7.52834476460825));
#407205=CARTESIAN_POINT('Ctrl Pts',(1.45527589141882,-2.30239235517612,
7.53807742314407));
#407206=CARTESIAN_POINT('Ctrl Pts',(1.45441001468943,-2.29139930822462,
7.54780169004674));
#407207=CARTESIAN_POINT('Ctrl Pts',(1.45303851274672,-2.27398691597693,
7.5632044032688));
#407208=CARTESIAN_POINT('Ctrl Pts',(1.45166555335683,-2.25655602018872,
7.57858609112103));
#407209=CARTESIAN_POINT('Ctrl Pts',(1.45029105591256,-2.23910559748222,
7.59394543036555));
#407210=CARTESIAN_POINT('Origin',(1.70235901374314,-2.36323439034367,7.5));
#407211=CARTESIAN_POINT('',(1.53564927699523,-2.27316543860613,8.75721825406948));
#407212=CARTESIAN_POINT('',(1.52331214621094,-2.26650000646721,8.78727029226991));
#407213=CARTESIAN_POINT('Origin',(1.49199590675922,-2.24958065361595,8.75658640621018));
#407214=CARTESIAN_POINT('',(1.46041276049035,-2.23251709792627,8.85049129520029));
#407215=CARTESIAN_POINT('Ctrl Pts',(1.52331214621094,-2.26650000646721,
8.78727029226991));
#407216=CARTESIAN_POINT('Ctrl Pts',(1.50237542338155,-2.25518843753999,
8.80838212259896));
#407217=CARTESIAN_POINT('Ctrl Pts',(1.48140969918009,-2.2438611999228,8.82945686509571));
#407218=CARTESIAN_POINT('Ctrl Pts',(1.46041276049035,-2.23251709792627,
8.85049129520029));
#407219=CARTESIAN_POINT('',(1.46041276049035,-2.23251709792627,7.59394543036555));
#407220=CARTESIAN_POINT('',(1.46041276049035,-2.23251709792627,7.5));
#407221=CARTESIAN_POINT('',(1.53564927699523,-2.27316543860613,7.51860402984325));
#407222=CARTESIAN_POINT('Ctrl Pts',(1.46041276049035,-2.23251709792627,
7.59394543036555));
#407223=CARTESIAN_POINT('Ctrl Pts',(1.47581327361953,-2.24083759618164,
7.57858609112103));
#407224=CARTESIAN_POINT('Ctrl Pts',(1.49119655366674,-2.24914878384932,
7.56320440326857));
#407225=CARTESIAN_POINT('Ctrl Pts',(1.50656350379346,-2.257451148884,7.54780169004651));
#407226=CARTESIAN_POINT('Ctrl Pts',(1.51626519221407,-2.26269271979146,
7.53807742314383));
#407227=CARTESIAN_POINT('Ctrl Pts',(1.52596037955095,-2.2679307783318,7.52834476460825));
#407228=CARTESIAN_POINT('Ctrl Pts',(1.53564927699523,-2.27316543860613,
7.51860402984325));
#407229=CARTESIAN_POINT('',(1.53564927699523,-2.27316543860613,7.5));
#407230=CARTESIAN_POINT('Origin',(1.45714482817992,-2.23856575425759,7.5));
#407231=CARTESIAN_POINT('Ctrl Pts',(1.46041276049035,-2.23251709792627,
8.85049129520029));
#407232=CARTESIAN_POINT('Ctrl Pts',(1.46024237621488,-2.23242504371646,
8.85097269580138));
#407233=CARTESIAN_POINT('Ctrl Pts',(1.4600701434085,-2.23234155133989,8.85143669361005));
#407234=CARTESIAN_POINT('Ctrl Pts',(1.4598877499329,-2.23226356296287,8.8519052845931));
#407235=CARTESIAN_POINT('Ctrl Pts',(1.45953099986161,-2.23211102264326,
8.85282181883899));
#407236=CARTESIAN_POINT('Ctrl Pts',(1.45914447807312,-2.23198364392551,
8.85372622499635));
#407237=CARTESIAN_POINT('Ctrl Pts',(1.45871729341944,-2.23189407204951,
8.85462257735071));
#407238=CARTESIAN_POINT('Ctrl Pts',(1.45836265989212,-2.23181971265935,
8.85536669723986));
#407239=CARTESIAN_POINT('Ctrl Pts',(1.45797992823564,-2.23177136083869,
8.85610498449051));
#407240=CARTESIAN_POINT('Ctrl Pts',(1.45756183174184,-2.231764186704,8.85681338218371));
#407241=CARTESIAN_POINT('Ctrl Pts',(1.45718240851709,-2.23175767616551,
8.85745625420284));
#407242=CARTESIAN_POINT('Ctrl Pts',(1.45676911105288,-2.23178439781428,
8.85808743050665));
#407243=CARTESIAN_POINT('Ctrl Pts',(1.45631128381985,-2.23187089041146,
8.85866804508409));
#407244=CARTESIAN_POINT('Ctrl Pts',(1.45610005225901,-2.23191079622087,
8.85893592806395));
#407245=CARTESIAN_POINT('Ctrl Pts',(1.45587927882592,-2.23196365955263,
8.85919241173848));
#407246=CARTESIAN_POINT('Ctrl Pts',(1.45564772260899,-2.23203367112445,
8.85943017985534));
#407247=CARTESIAN_POINT('Ctrl Pts',(1.45533505316815,-2.23212820747205,
8.8597512372));
#407248=CARTESIAN_POINT('Ctrl Pts',(1.45499495061646,-2.23225702953023,
8.86004599534706));
#407249=CARTESIAN_POINT('Ctrl Pts',(1.45463519034913,-2.23242832936725,
8.86026130871721));
#407250=CARTESIAN_POINT('Ctrl Pts',(1.45450347197255,-2.23249104706703,
8.86034014101236));
#407251=CARTESIAN_POINT('Ctrl Pts',(1.45436713462985,-2.23256038986719,
8.86040910639693));
#407252=CARTESIAN_POINT('Ctrl Pts',(1.45423004525065,-2.2326347683884,8.86046313645507));
#407253=CARTESIAN_POINT('Ctrl Pts',(1.45401611842253,-2.23275083544783,
8.8605474499083));
#407254=CARTESIAN_POINT('Ctrl Pts',(1.45379459084792,-2.23288246268805,
8.86059655985668));
#407255=CARTESIAN_POINT('Ctrl Pts',(1.45357952011843,-2.23302095660014,
8.86059725258816));
#407256=CARTESIAN_POINT('Ctrl Pts',(1.45336395248964,-2.23315977048849,
8.86059794692011));
#407257=CARTESIAN_POINT('Ctrl Pts',(1.45315391929665,-2.23330925598724,
8.86056369958366));
#407258=CARTESIAN_POINT('Ctrl Pts',(1.45295869380045,-2.23345819421406,
8.86048590497774));
#407259=CARTESIAN_POINT('Ctrl Pts',(1.4529077457585,-2.23349706265684,8.86046560290182));
#407260=CARTESIAN_POINT('Ctrl Pts',(1.45285719833683,-2.23353647149834,
8.86044257503091));
#407261=CARTESIAN_POINT('Ctrl Pts',(1.45280859330924,-2.23357517708473,
8.86041778462583));
#407262=CARTESIAN_POINT('Ctrl Pts',(1.45248154178738,-2.23383561765152,
8.86025097596201));
#407263=CARTESIAN_POINT('Ctrl Pts',(1.45219875525293,-2.23409942479347,
8.8599848982295));
#407264=CARTESIAN_POINT('Ctrl Pts',(1.45196270805475,-2.23435270342849,
8.85968173251461));
#407265=CARTESIAN_POINT('Ctrl Pts',(1.4518378526108,-2.23448667331529,8.85952137522076));
#407266=CARTESIAN_POINT('Ctrl Pts',(1.45172352753973,-2.23462014970572,
8.85934740853961));
#407267=CARTESIAN_POINT('Ctrl Pts',(1.45162016440982,-2.23475023902306,
8.8591675900182));
#407268=CARTESIAN_POINT('Ctrl Pts',(1.45120510771616,-2.23527261525127,
8.85844552518697));
#407269=CARTESIAN_POINT('Ctrl Pts',(1.45094097857854,-2.23576801806967,
8.85759444184129));
#407270=CARTESIAN_POINT('Ctrl Pts',(1.45076190271771,-2.23619128641431,
8.85683498915145));
#407271=CARTESIAN_POINT('Ctrl Pts',(1.45074316290579,-2.23623558031934,
8.85675551445002));
#407272=CARTESIAN_POINT('Ctrl Pts',(1.45072537407568,-2.23627908830462,
8.85667699793653));
#407273=CARTESIAN_POINT('Ctrl Pts',(1.450708473719,-2.2363217605987,8.85659965593547));
#407274=CARTESIAN_POINT('Ctrl Pts',(1.4504803518422,-2.23689775340152,8.85555568965886));
#407275=CARTESIAN_POINT('Ctrl Pts',(1.45034429734326,-2.23748426348365,
8.85434650606346));
#407276=CARTESIAN_POINT('Ctrl Pts',(1.45029358366058,-2.23808278585889,
8.85297329937117));
#407277=CARTESIAN_POINT('Ctrl Pts',(1.4502650603041,-2.23841941822646,8.85220095427747));
#407278=CARTESIAN_POINT('Ctrl Pts',(1.45026383578709,-2.23876001466751,
8.85137579139183));
#407279=CARTESIAN_POINT('Ctrl Pts',(1.45029105591256,-2.23910559748222,
8.85049129520029));
#407280=CARTESIAN_POINT('Origin',(1.45714482817992,-2.23856575425759,7.59394543036555));
#407281=CARTESIAN_POINT('Ctrl Pts',(1.45991807746006,-2.23224983350099,
7.59443877723642));
#407282=CARTESIAN_POINT('Ctrl Pts',(1.45482331821924,-2.22949726707549,
7.58783886950016));
#407283=CARTESIAN_POINT('Ctrl Pts',(1.44916893433922,-2.2358302856665,7.58559994247159));
#407284=CARTESIAN_POINT('Ctrl Pts',(1.48773021868178,-2.2472760128609,7.56670252222132));
#407285=CARTESIAN_POINT('Ctrl Pts',(1.48264282281451,-2.24452742467538,
7.56004874999026));
#407286=CARTESIAN_POINT('Ctrl Pts',(1.47693899722923,-2.2508837389336,7.55786368756704));
#407287=CARTESIAN_POINT('Ctrl Pts',(1.51549042350862,-2.26227413233219,
7.53888913333561));
#407288=CARTESIAN_POINT('Ctrl Pts',(1.51037279299857,-2.25950920915251,
7.53222002137279));
#407289=CARTESIAN_POINT('Ctrl Pts',(1.50465874202924,-2.26590858929742,
7.53005029815326));
#407290=CARTESIAN_POINT('Ctrl Pts',(1.54319743577238,-2.27724351323973,
7.51101258149734));
#407291=CARTESIAN_POINT('Ctrl Pts',(1.53801777028162,-2.2744450741671,7.5043616886572));
#407292=CARTESIAN_POINT('Ctrl Pts',(1.53232675979283,-2.28090416707254,
7.50217374673251));
#407293=CARTESIAN_POINT('',(1.53085035931327,-2.28010398287619,7.50366116523517));
#407294=CARTESIAN_POINT('Ctrl Pts',(1.53564927699523,-2.27316543860613,
7.51860402984325));
#407295=CARTESIAN_POINT('Ctrl Pts',(1.5360378085553,-2.27337535214216,7.51734760759494));
#407296=CARTESIAN_POINT('Ctrl Pts',(1.53636062142571,-2.27361738460005,
7.51608817408573));
#407297=CARTESIAN_POINT('Ctrl Pts',(1.53660896257297,-2.27390166343753,
7.5148100591312));
#407298=CARTESIAN_POINT('Ctrl Pts',(1.53683391591845,-2.27415917000158,
7.51365231206384));
#407299=CARTESIAN_POINT('Ctrl Pts',(1.53699826944799,-2.27445153882632,
7.51247773061043));
#407300=CARTESIAN_POINT('Ctrl Pts',(1.53706699140847,-2.27479180510429,
7.51129758471022));
#407301=CARTESIAN_POINT('Ctrl Pts',(1.537152404957,-2.27521471722792,7.50983079813402));
#407302=CARTESIAN_POINT('Ctrl Pts',(1.53707459741073,-2.27570070103044,
7.50839324291155));
#407303=CARTESIAN_POINT('Ctrl Pts',(1.53675159800197,-2.27624027053724,
7.50715379678855));
#407304=CARTESIAN_POINT('Ctrl Pts',(1.53660238158212,-2.27648953610206,
7.50658120839351));
#407305=CARTESIAN_POINT('Ctrl Pts',(1.53637147188821,-2.27678079279749,
7.50598221009429));
#407306=CARTESIAN_POINT('Ctrl Pts',(1.53604653982969,-2.27709297784467,
7.50545747549611));
#407307=CARTESIAN_POINT('Ctrl Pts',(1.53587314602567,-2.27725956944888,
7.50517746087247));
#407308=CARTESIAN_POINT('Ctrl Pts',(1.53567123831366,-2.27743407312486,
7.50491486231392));
#407309=CARTESIAN_POINT('Ctrl Pts',(1.53544507284033,-2.27761060572659,
7.50468370960992));
#407310=CARTESIAN_POINT('Ctrl Pts',(1.53510688411784,-2.27787457765022,
7.50433806340446));
#407311=CARTESIAN_POINT('Ctrl Pts',(1.53470397229055,-2.27815056287832,
7.50405484070983));
#407312=CARTESIAN_POINT('Ctrl Pts',(1.53426306787569,-2.27841938328404,
7.5038576603613));
#407313=CARTESIAN_POINT('Ctrl Pts',(1.53421592000173,-2.27844812944801,
7.50383657498791));
#407314=CARTESIAN_POINT('Ctrl Pts',(1.53416836604276,-2.27847679328435,
7.50381643264937));
#407315=CARTESIAN_POINT('Ctrl Pts',(1.53412045929205,-2.27850535137413,
7.50379723213559));
#407316=CARTESIAN_POINT('Ctrl Pts',(1.53380066605968,-2.27869598596542,
7.50366906242519));
#407317=CARTESIAN_POINT('Ctrl Pts',(1.53345782800162,-2.27888543759957,
7.50358235568538));
#407318=CARTESIAN_POINT('Ctrl Pts',(1.53312298478604,-2.27906010223198,
7.5035341175365));
#407319=CARTESIAN_POINT('Ctrl Pts',(1.53262092528121,-2.27932199208006,
7.50346178989176));
#407320=CARTESIAN_POINT('Ctrl Pts',(1.53206968824905,-2.27958237897118,
7.50346967198527));
#407321=CARTESIAN_POINT('Ctrl Pts',(1.53152067885769,-2.27982134720851,
7.50354272648692));
#407322=CARTESIAN_POINT('Ctrl Pts',(1.5312948599312,-2.27991963979087,7.50357277531559));
#407323=CARTESIAN_POINT('Ctrl Pts',(1.53106977451844,-2.28001430808024,
7.50361331098761));
#407324=CARTESIAN_POINT('Ctrl Pts',(1.53085035931406,-2.28010398287737,
7.50366116523658));
#407325=CARTESIAN_POINT('',(1.458742113555,-2.24101961352525,7.57603338622103));
#407326=CARTESIAN_POINT('Origin',(1.46356058069564,-2.24842730304492,7.58486873427628));
#407327=CARTESIAN_POINT('Ctrl Pts',(1.53085035936602,-2.28010398289869,
7.50366116529969));
#407328=CARTESIAN_POINT('Ctrl Pts',(1.50685310107529,-2.26709785383089,
7.52783573079709));
#407329=CARTESIAN_POINT('Ctrl Pts',(1.48281814548303,-2.25407036159423,
7.55196141284068));
#407330=CARTESIAN_POINT('Ctrl Pts',(1.45874211477945,-2.2410196137867,7.57603338728831));
#407331=CARTESIAN_POINT('Ctrl Pts',(1.4612339872377,-2.23316062115808,7.5963967733137));
#407332=CARTESIAN_POINT('Ctrl Pts',(1.44672891934441,-2.2220396984816,7.59959882295473));
#407333=CARTESIAN_POINT('Ctrl Pts',(1.45050708407105,-2.23994037679046,
7.59642833564546));
#407334=CARTESIAN_POINT('Ctrl Pts',(1.45856018235572,-2.23032057335266,
7.58707626057419));
#407335=CARTESIAN_POINT('Ctrl Pts',(1.4517863168465,-2.23015614373247,7.58809943920599));
#407336=CARTESIAN_POINT('Ctrl Pts',(1.44910071340169,-2.23636113647472,
7.58710240504253));
#407337=CARTESIAN_POINT('Ctrl Pts',(1.45829905181767,-2.23639160646937,
7.58015376756929));
#407338=CARTESIAN_POINT('Ctrl Pts',(1.45548191389407,-2.23595228276659,
7.58205880659762));
#407339=CARTESIAN_POINT('Ctrl Pts',(1.45471184049851,-2.23866043010443,
7.58020924244126));
#407340=CARTESIAN_POINT('Ctrl Pts',(1.4587421131037,-2.24101961283156,7.57603338509286));
#407341=CARTESIAN_POINT('Ctrl Pts',(1.4587421131037,-2.24101961283156,7.57603338509286));
#407342=CARTESIAN_POINT('Ctrl Pts',(1.4587421131037,-2.24101961283156,7.57603338509286));
#407343=CARTESIAN_POINT('Origin',(1.46356536312188,-2.24842419003088,7.58486873427622));
#407344=CARTESIAN_POINT('Ctrl Pts',(1.45768172623409,-2.33293648944411,
7.51098857897448));
#407345=CARTESIAN_POINT('Ctrl Pts',(1.45721943842671,-2.32706734964726,
7.50433767179956));
#407346=CARTESIAN_POINT('Ctrl Pts',(1.46542937708842,-2.32447795623305,
7.50214974420965));
#407347=CARTESIAN_POINT('Ctrl Pts',(1.45520816116921,-2.30153246162714,
7.5388732158917));
#407348=CARTESIAN_POINT('Ctrl Pts',(1.45475141239017,-2.29573364454088,
7.53220407452063));
#407349=CARTESIAN_POINT('Ctrl Pts',(1.46291606210059,-2.29309898801137,
7.53003438070911));
#407350=CARTESIAN_POINT('Ctrl Pts',(1.45272984594694,-2.27006812649224,
7.56669465659231));
#407351=CARTESIAN_POINT('Ctrl Pts',(1.45227579646826,-2.26430357933689,
7.56004085833298));
#407352=CARTESIAN_POINT('Ctrl Pts',(1.46039691481123,-2.2616608370139,7.55785582193789));
#407353=CARTESIAN_POINT('Ctrl Pts',(1.45024689265157,-2.23854490704545,
7.59443891967696));
#407354=CARTESIAN_POINT('Ctrl Pts',(1.44979218485769,-2.23277200201442,
7.58783901202978));
#407355=CARTESIAN_POINT('Ctrl Pts',(1.45787197718042,-2.23016506242751,
7.58560008491213));
#407356=CARTESIAN_POINT('',(1.46529313746772,-2.32277700535964,7.50366116523517));
#407357=CARTESIAN_POINT('Ctrl Pts',(1.46529313746792,-2.32277700535995,
7.50366116523554));
#407358=CARTESIAN_POINT('Ctrl Pts',(1.46474697642258,-2.32330221544108,
7.50350835821027));
#407359=CARTESIAN_POINT('Ctrl Pts',(1.46422783470215,-2.32376724219865,
7.50345484955999));
#407360=CARTESIAN_POINT('Ctrl Pts',(1.46372067846698,-2.32418635854706,
7.50349758195598));
#407361=CARTESIAN_POINT('Ctrl Pts',(1.46346046970665,-2.32440139631627,
7.50351950684424));
#407362=CARTESIAN_POINT('Ctrl Pts',(1.4631778513041,-2.32462564316438,7.50357029184312));
#407363=CARTESIAN_POINT('Ctrl Pts',(1.46289938165621,-2.32483439063404,
7.50365515313924));
#407364=CARTESIAN_POINT('Ctrl Pts',(1.46247098257425,-2.32515552877257,
7.50378570417639));
#407365=CARTESIAN_POINT('Ctrl Pts',(1.46204003528892,-2.32544968913026,
7.50400001621911));
#407366=CARTESIAN_POINT('Ctrl Pts',(1.46163806115038,-2.32569260662708,
7.50428903009635));
#407367=CARTESIAN_POINT('Ctrl Pts',(1.4615934451136,-2.32571956860033,7.50432110841318));
#407368=CARTESIAN_POINT('Ctrl Pts',(1.4615491735453,-2.32574592693409,7.50435406373354));
#407369=CARTESIAN_POINT('Ctrl Pts',(1.46150528007182,-2.32577166872304,
7.50438785222352));
#407370=CARTESIAN_POINT('Ctrl Pts',(1.46123728931837,-2.32592883471764,
7.50459414719561));
#407371=CARTESIAN_POINT('Ctrl Pts',(1.46097886517166,-2.32606507519193,
7.50483629897752));
#407372=CARTESIAN_POINT('Ctrl Pts',(1.46074052152493,-2.32617633497057,
7.5050991045531));
#407373=CARTESIAN_POINT('Ctrl Pts',(1.4602147115009,-2.32642178521724,7.50567888004914));
#407374=CARTESIAN_POINT('Ctrl Pts',(1.45976613099601,-2.32655580102415,
7.50637912803145));
#407375=CARTESIAN_POINT('Ctrl Pts',(1.45939558937346,-2.32660928163542,
7.50710440483569));
#407376=CARTESIAN_POINT('Ctrl Pts',(1.45930472521133,-2.32662239614304,
7.50728225710685));
#407377=CARTESIAN_POINT('Ctrl Pts',(1.45921676576372,-2.32663107336784,
7.50746498566954));
#407378=CARTESIAN_POINT('Ctrl Pts',(1.45913380518732,-2.32663552533605,
7.50764697238949));
#407379=CARTESIAN_POINT('Ctrl Pts',(1.45868783195992,-2.32665945789195,
7.50862528291182));
#407380=CARTESIAN_POINT('Ctrl Pts',(1.45834605560042,-2.3265675928262,7.50965856837423));
#407381=CARTESIAN_POINT('Ctrl Pts',(1.45807469544967,-2.32641697628601,
7.51067959873204));
#407382=CARTESIAN_POINT('Ctrl Pts',(1.45792536561644,-2.32633409181397,
7.5112414730258));
#407383=CARTESIAN_POINT('Ctrl Pts',(1.45779753440286,-2.32623301549518,
7.51180065547253));
#407384=CARTESIAN_POINT('Ctrl Pts',(1.45768697619173,-2.32612092895028,
7.51235175716501));
#407385=CARTESIAN_POINT('Ctrl Pts',(1.45730495353112,-2.32573362528765,
7.51425603304537));
#407386=CARTESIAN_POINT('Ctrl Pts',(1.45708793524579,-2.32516442453967,
7.51626900505183));
#407387=CARTESIAN_POINT('Ctrl Pts',(1.45701626624484,-2.32447039109801,
7.51827788969247));
#407388=CARTESIAN_POINT('Ctrl Pts',(1.45701238738308,-2.32443282869661,
7.51838661432547));
#407389=CARTESIAN_POINT('Ctrl Pts',(1.45700894005983,-2.32439489252745,
7.51849533314857));
#407390=CARTESIAN_POINT('Ctrl Pts',(1.45700592305914,-2.32435658911879,
7.51860402984325));
#407391=CARTESIAN_POINT('Ctrl Pts',(1.45874211329887,-2.24101961475187,
7.57603338728985));
#407392=CARTESIAN_POINT('Ctrl Pts',(1.46093030563709,-2.26831776647325,
7.55196141284922));
#407393=CARTESIAN_POINT('Ctrl Pts',(1.46311385931012,-2.29556894514294,
7.52783573083104));
#407394=CARTESIAN_POINT('Ctrl Pts',(1.46529313746701,-2.32277700541881,
7.50366116530176));
#407395=CARTESIAN_POINT('Origin',(5.04062831473875E-16,-7.74375868966271E-16,
7.49482233047033));
#407396=CARTESIAN_POINT('Origin',(1.52592346056197,-2.27276568139054,7.49482233047033));
#407397=CARTESIAN_POINT('Origin',(0.,0.,7.50366116523517));
#407398=CARTESIAN_POINT('Origin',(1.46057722850551,-2.31530136474092,7.49482233047033));
#407399=CARTESIAN_POINT('Ctrl Pts',(1.53564834642939,-2.27316493579465,
7.51860402984325));
#407400=CARTESIAN_POINT('Ctrl Pts',(1.54234243883859,-2.27678231230908,
7.51860402984325));
#407401=CARTESIAN_POINT('Ctrl Pts',(1.54863020028824,-2.27249741534621,
7.51860402984325));
#407402=CARTESIAN_POINT('Ctrl Pts',(1.53813390922792,-2.27450809126278,
7.51041458714365));
#407403=CARTESIAN_POINT('Ctrl Pts',(1.54383207597018,-2.27576716295959,
7.51004642900442));
#407404=CARTESIAN_POINT('Ctrl Pts',(1.5486319343782,-2.2724962336225,7.5072913648301));
#407405=CARTESIAN_POINT('Ctrl Pts',(1.53773211669732,-2.27729418170668,
7.50215815450138));
#407406=CARTESIAN_POINT('Ctrl Pts',(1.54079910519163,-2.27783422435049,
7.4987716367153));
#407407=CARTESIAN_POINT('Ctrl Pts',(1.54366359294844,-2.27591104118567,
7.4948158853317));
#407408=CARTESIAN_POINT('Ctrl Pts',(1.5308500524459,-2.28010352581766,7.50366171572173));
#407409=CARTESIAN_POINT('Ctrl Pts',(1.53289114759618,-2.28314360687655,
7.50000045605858));
#407410=CARTESIAN_POINT('Ctrl Pts',(1.53289114759628,-2.28314360687648,
7.49482233047317));
#407411=CARTESIAN_POINT('Origin',(1.54159097210511,-2.26216788164009,7.51860402984325));
#407412=CARTESIAN_POINT('Origin',(1.54159097210511,-2.26216788164009,9.));
#407413=CARTESIAN_POINT('Origin',(1.54159097210511,-2.26216788164009,8.75721825406948));
#407414=CARTESIAN_POINT('Ctrl Pts',(1.52095641350494,-2.26522723077964,
8.78942910404912));
#407415=CARTESIAN_POINT('Ctrl Pts',(1.52584946047531,-2.26789378661955,
8.79672699501691));
#407416=CARTESIAN_POINT('Ctrl Pts',(1.53148742309712,-2.26097375313283,
8.79893251111267));
#407417=CARTESIAN_POINT('Ctrl Pts',(1.53062927805548,-2.27045323404477,
8.78111911759583));
#407418=CARTESIAN_POINT('Ctrl Pts',(1.53643360398454,-2.27360793064426,
8.78644465894813));
#407419=CARTESIAN_POINT('Ctrl Pts',(1.54278266608224,-2.26856760106627,
8.78817647674131));
#407420=CARTESIAN_POINT('Ctrl Pts',(1.53665763797811,-2.27371020390355,
8.76780923932029));
#407421=CARTESIAN_POINT('Ctrl Pts',(1.54351183306588,-2.27742971280518,
8.76988516158374));
#407422=CARTESIAN_POINT('Ctrl Pts',(1.54984371438416,-2.27330131609855,
8.77093053738832));
#407423=CARTESIAN_POINT('Ctrl Pts',(1.53548219029793,-2.27307513935433,
8.75371302330492));
#407424=CARTESIAN_POINT('Ctrl Pts',(1.54216779835549,-2.27670402985534,
8.75300828287558));
#407425=CARTESIAN_POINT('Ctrl Pts',(1.54846677797151,-2.2723776693605,8.75267964240737));
#407426=CARTESIAN_POINT('Origin',(1.52925384132083,-2.25550244950118,8.78727029226991));
#407427=CARTESIAN_POINT('Ctrl Pts',(1.46041276049035,-2.23251709792627,
8.85049129520029));
#407428=CARTESIAN_POINT('Ctrl Pts',(1.46555048104868,-2.2352928752386,8.85711686593484));
#407429=CARTESIAN_POINT('Ctrl Pts',(1.47122360941503,-2.2288962842205,8.85933012996512));
#407430=CARTESIAN_POINT('Ctrl Pts',(1.48140972735875,-2.243861215147,8.82945683644721));
#407431=CARTESIAN_POINT('Ctrl Pts',(1.48659009410405,-2.24666003308928,
8.83607469902388));
#407432=CARTESIAN_POINT('Ctrl Pts',(1.49225182125615,-2.24021977780299,
8.8382956714852));
#407433=CARTESIAN_POINT('Ctrl Pts',(1.50237539655486,-2.25518842304623,
8.80838214965002));
#407434=CARTESIAN_POINT('Ctrl Pts',(1.50757620744598,-2.25799828643083,
8.81501364461988));
#407435=CARTESIAN_POINT('Ctrl Pts',(1.51324781742242,-2.25152668285287,
8.81722098428721));
#407436=CARTESIAN_POINT('Ctrl Pts',(1.52331214621094,-2.26650000646721,
8.78727029226991));
#407437=CARTESIAN_POINT('Ctrl Pts',(1.52851382097385,-2.26931033657938,
8.79393457792714));
#407438=CARTESIAN_POINT('Ctrl Pts',(1.53421404825539,-2.26281827803705,
8.79610912703474));
#407439=CARTESIAN_POINT('Origin',(1.46635445560024,-2.22151954096023,8.85049129520029));
#407440=CARTESIAN_POINT('Ctrl Pts',(1.45029105591256,-2.23910559748222,
8.85049129520029));
#407441=CARTESIAN_POINT('Ctrl Pts',(1.45074959802201,-2.24492718243453,
8.85711686593484));
#407442=CARTESIAN_POINT('Ctrl Pts',(1.44260408658469,-2.24752552912782,
8.85933012996512));
#407443=CARTESIAN_POINT('Ctrl Pts',(1.44988539032746,-2.23395532531037,
8.86332496987232));
#407444=CARTESIAN_POINT('Ctrl Pts',(1.44617396855413,-2.23670800451386,
8.86648636486737));
#407445=CARTESIAN_POINT('Ctrl Pts',(1.44148630031579,-2.23311608742407,
8.87206031107458));
#407446=CARTESIAN_POINT('Ctrl Pts',(1.45583660675253,-2.23004472061829,
8.86341338519876));
#407447=CARTESIAN_POINT('Ctrl Pts',(1.45985275223894,-2.22773300133033,
8.86654584966057));
#407448=CARTESIAN_POINT('Ctrl Pts',(1.45840313270637,-2.22198645836975,
8.87215952290713));
#407449=CARTESIAN_POINT('Ctrl Pts',(1.46041276049035,-2.23251709792627,
8.85049129520029));
#407450=CARTESIAN_POINT('Ctrl Pts',(1.46555048104868,-2.2352928752386,8.85711686593484));
#407451=CARTESIAN_POINT('Ctrl Pts',(1.47122360941503,-2.2288962842205,8.85933012996512));
#407452=CARTESIAN_POINT('Origin',(1.43782965179009,-2.24008713061792,8.85049129520029));
#407453=CARTESIAN_POINT('Ctrl Pts',(1.45590483281687,-2.3103773050933,8.78727029226991));
#407454=CARTESIAN_POINT('Ctrl Pts',(1.45636908284591,-2.3162713569754,8.79393457792714));
#407455=CARTESIAN_POINT('Ctrl Pts',(1.44812530550987,-2.31885583959519,
8.79610912703474));
#407456=CARTESIAN_POINT('Ctrl Pts',(1.45403622567033,-2.2866537363697,8.80838214965002));
#407457=CARTESIAN_POINT('Ctrl Pts',(1.45450039859872,-2.29254680939304,
8.81501364461991));
#407458=CARTESIAN_POINT('Ctrl Pts',(1.44628690934872,-2.29511340381661,
8.81722098428722));
#407459=CARTESIAN_POINT('Ctrl Pts',(1.45216503745174,-2.26289739872511,
8.82945683644722));
#407460=CARTESIAN_POINT('Ctrl Pts',(1.45262738573792,-2.26876730635232,
8.83607469902389));
#407461=CARTESIAN_POINT('Ctrl Pts',(1.44444656216423,-2.27133755306294,
8.83829567148519));
#407462=CARTESIAN_POINT('Ctrl Pts',(1.45029105591256,-2.23910559748222,
8.85049129520029));
#407463=CARTESIAN_POINT('Ctrl Pts',(1.45074959802201,-2.24492718243453,
8.85711686593484));
#407464=CARTESIAN_POINT('Ctrl Pts',(1.44260408658469,-2.24752552912782,
8.85933012996512));
#407465=CARTESIAN_POINT('Origin',(1.4434434286944,-2.31135883822899,8.78727029226991));
#407466=CARTESIAN_POINT('Ctrl Pts',(1.45699136532628,-2.3241720011539,8.75374538247848));
#407467=CARTESIAN_POINT('Ctrl Pts',(1.45760113795345,-2.33174646851014,
8.75304829418601));
#407468=CARTESIAN_POINT('Ctrl Pts',(1.4511052095082,-2.33575565257217,8.75272238421917));
#407469=CARTESIAN_POINT('Ctrl Pts',(1.45709501436912,-2.3254879091256,8.76769408445022));
#407470=CARTESIAN_POINT('Ctrl Pts',(1.45771944369952,-2.33325303906549,
8.76974318093971));
#407471=CARTESIAN_POINT('Ctrl Pts',(1.45138968706045,-2.33737038507601,
8.7707786988043));
#407472=CARTESIAN_POINT('Ctrl Pts',(1.45656376843519,-2.31874331448478,
8.78108014887987));
#407473=CARTESIAN_POINT('Ctrl Pts',(1.45709673696933,-2.32532367783662,
8.78639403366323));
#407474=CARTESIAN_POINT('Ctrl Pts',(1.4499375907602,-2.32910107128779,8.78812224174741));
#407475=CARTESIAN_POINT('Ctrl Pts',(1.45569317358816,-2.30769041275578,
8.78944554828686));
#407476=CARTESIAN_POINT('Ctrl Pts',(1.45614791916577,-2.31323564711301,
8.79673892988686));
#407477=CARTESIAN_POINT('Ctrl Pts',(1.4475478719704,-2.31558995009988,8.79894799272499));
#407478=CARTESIAN_POINT('Origin',(1.44454451893667,-2.32533812225449,8.75721825406948));
#407479=CARTESIAN_POINT('Origin',(1.44454451893667,-2.32533812225449,9.));
#407480=CARTESIAN_POINT('Origin',(1.44454451893667,-2.32533812225449,7.51860402984325));
#407481=CARTESIAN_POINT('Ctrl Pts',(1.46529271774779,-2.32277634002134,
7.50366195182966));
#407482=CARTESIAN_POINT('Ctrl Pts',(1.46724653091866,-2.32587351709141,
7.50000065167736));
#407483=CARTESIAN_POINT('Ctrl Pts',(1.46724653091856,-2.32587351709147,
7.49482233047108));
#407484=CARTESIAN_POINT('Ctrl Pts',(1.4599326803461,-2.32793616546985,7.50215800491336));
#407485=CARTESIAN_POINT('Ctrl Pts',(1.45918346602515,-2.33095996689781,
7.49877273257263));
#407486=CARTESIAN_POINT('Ctrl Pts',(1.45626376864621,-2.33280184734056,
7.49481816995647));
#407487=CARTESIAN_POINT('Ctrl Pts',(1.45722758392157,-2.32716644495161,
7.51043025814044));
#407488=CARTESIAN_POINT('Ctrl Pts',(1.4560753670245,-2.33289053031165,7.51006209594517));
#407489=CARTESIAN_POINT('Ctrl Pts',(1.45113846196595,-2.33595744058181,
7.50731281821701));
#407490=CARTESIAN_POINT('Ctrl Pts',(1.45700580428833,-2.32435508238524,
7.51860402984326));
#407491=CARTESIAN_POINT('Ctrl Pts',(1.45760422169309,-2.33194078696692,
7.51860402984326));
#407492=CARTESIAN_POINT('Ctrl Pts',(1.45114061263044,-2.33595610454789,
7.51860402984327));
#407493=CARTESIAN_POINT('Origin',(0.,0.,7.5));
#407494=CARTESIAN_POINT('Origin',(1.59077126558569,-2.1415846479005,7.5));
#407495=CARTESIAN_POINT('',(1.59077126558569,-2.1415846479005,7.59394543036555));
#407496=CARTESIAN_POINT('',(1.59077126558569,-2.1415846479005,8.85049129520029));
#407497=CARTESIAN_POINT('',(1.59077126558569,-2.1415846479005,7.5));
#407498=CARTESIAN_POINT('',(1.60093990236831,-2.21235024422324,8.78727029226991));
#407499=CARTESIAN_POINT('Ctrl Pts',(1.59077126558569,-2.1415846479005,8.85049129520029));
#407500=CARTESIAN_POINT('Ctrl Pts',(1.59416573821268,-2.16520746822392,
8.82945686509571));
#407501=CARTESIAN_POINT('Ctrl Pts',(1.59755516454566,-2.18879517036851,
8.80838212259896));
#407502=CARTESIAN_POINT('Ctrl Pts',(1.60093990236831,-2.21235024422324,
8.78727029226991));
#407503=CARTESIAN_POINT('',(1.60293438610528,-2.22623025921638,8.75721825406948));
#407504=CARTESIAN_POINT('Origin',(1.59693249240026,-2.18446045038842,8.75937679713133));
#407505=CARTESIAN_POINT('',(1.60293438610528,-2.22623025921638,7.51860402984325));
#407506=CARTESIAN_POINT('',(1.60293438610528,-2.22623025921638,7.5));
#407507=CARTESIAN_POINT('Ctrl Pts',(1.60293438610528,-2.22623025921638,
7.51860402984325));
#407508=CARTESIAN_POINT('Ctrl Pts',(1.60136802933079,-2.21532966618993,
7.52834476460825));
#407509=CARTESIAN_POINT('Ctrl Pts',(1.59980065570009,-2.20442199665577,
7.53807742314407));
#407510=CARTESIAN_POINT('Ctrl Pts',(1.59823223107087,-2.19350701301076,
7.54780169004674));
#407511=CARTESIAN_POINT('Ctrl Pts',(1.5957479312243,-2.17621826882159,7.5632044032688));
#407512=CARTESIAN_POINT('Ctrl Pts',(1.59326099139911,-2.15891115248837,
7.57858609112102));
#407513=CARTESIAN_POINT('Ctrl Pts',(1.59077126558569,-2.1415846479005,7.59394543036555));
#407514=CARTESIAN_POINT('Origin',(1.85027428182728,-2.24930835533595,7.5));
#407515=CARTESIAN_POINT('',(1.67813633056182,-2.17010558942598,8.75721825406948));
#407516=CARTESIAN_POINT('',(1.66539749203248,-2.16424429481554,8.78727029226991));
#407517=CARTESIAN_POINT('Origin',(1.63306156849261,-2.14936614293919,8.75658640620944));
#407518=CARTESIAN_POINT('',(1.60045004741999,-2.13436118528462,8.85049129520029));
#407519=CARTESIAN_POINT('Ctrl Pts',(1.66539749203248,-2.16424429481554,
8.78727029226991));
#407520=CARTESIAN_POINT('Ctrl Pts',(1.6437790512361,-2.15429738715719,8.80838212259895));
#407521=CARTESIAN_POINT('Ctrl Pts',(1.62213066475767,-2.14433670112617,
8.82945686509571));
#407522=CARTESIAN_POINT('Ctrl Pts',(1.60045004741999,-2.13436118528462,
8.85049129520029));
#407523=CARTESIAN_POINT('',(1.60045004741999,-2.13436118528462,7.59394543036555));
#407524=CARTESIAN_POINT('',(1.60045004741999,-2.13436118528462,7.5));
#407525=CARTESIAN_POINT('',(1.67813633056182,-2.17010558942598,7.51860402984325));
#407526=CARTESIAN_POINT('Ctrl Pts',(1.60045004741999,-2.13436118528462,
7.59394543036555));
#407527=CARTESIAN_POINT('Ctrl Pts',(1.61635201469681,-2.14167787391995,
7.57858609112103));
#407528=CARTESIAN_POINT('Ctrl Pts',(1.63223618776748,-2.14898637522454,
7.56320440326857));
#407529=CARTESIAN_POINT('Ctrl Pts',(1.6481034992012,-2.15628711828478,7.54780169004651));
#407530=CARTESIAN_POINT('Ctrl Pts',(1.65812108306353,-2.16089633051136,
7.53807742314383));
#407531=CARTESIAN_POINT('Ctrl Pts',(1.66813195416117,-2.16550245411322,
7.52834476460825));
#407532=CARTESIAN_POINT('Ctrl Pts',(1.67813633056182,-2.17010558942598,
7.51860402984325));
#407533=CARTESIAN_POINT('',(1.67813633056182,-2.17010558942598,7.5));
#407534=CARTESIAN_POINT('Origin',(1.5975763681687,-2.1406067911448,7.5));
#407535=CARTESIAN_POINT('Ctrl Pts',(1.60045004741999,-2.13436118528462,
8.85049129520029));
#407536=CARTESIAN_POINT('Ctrl Pts',(1.60027411528381,-2.13428023676806,
8.85097269580138));
#407537=CARTESIAN_POINT('Ctrl Pts',(1.60009688697327,-2.13420795092933,
8.85143669361005));
#407538=CARTESIAN_POINT('Ctrl Pts',(1.59990987151216,-2.1341418087779,8.8519052845931));
#407539=CARTESIAN_POINT('Ctrl Pts',(1.59954408113031,-2.13401243892428,
8.85282181883899));
#407540=CARTESIAN_POINT('Ctrl Pts',(1.59915019230982,-2.13391008645578,
8.85372622499635));
#407541=CARTESIAN_POINT('Ctrl Pts',(1.59871814646303,-2.13384806842955,
8.8546225773507));
#407542=CARTESIAN_POINT('Ctrl Pts',(1.59835947734584,-2.13379658326684,
8.85536669723986));
#407543=CARTESIAN_POINT('Ctrl Pts',(1.59797443414081,-2.1337728524916,8.85610498449051));
#407544=CARTESIAN_POINT('Ctrl Pts',(1.59755673702271,-2.13379248063127,
8.8568133821837));
#407545=CARTESIAN_POINT('Ctrl Pts',(1.59717767623203,-2.13381029319885,
8.85745625420284));
#407546=CARTESIAN_POINT('Ctrl Pts',(1.5967669399937,-2.13386344000458,8.85808743050665));
#407547=CARTESIAN_POINT('Ctrl Pts',(1.59631559501555,-2.13397908798497,
8.8586680450841));
#407548=CARTESIAN_POINT('Ctrl Pts',(1.5961073542266,-2.13403244545619,8.85893592806395));
#407549=CARTESIAN_POINT('Ctrl Pts',(1.59589042136151,-2.13409934517698,
8.85919241173848));
#407550=CARTESIAN_POINT('Ctrl Pts',(1.59566382655846,-2.13418404876028,
8.85943017985534));
#407551=CARTESIAN_POINT('Ctrl Pts',(1.59535785649511,-2.13429842367267,
8.8597512372));
#407552=CARTESIAN_POINT('Ctrl Pts',(1.59502670637819,-2.13444877149742,
8.86004599534705));
#407553=CARTESIAN_POINT('Ctrl Pts',(1.59467866049516,-2.13464276930002,
8.86026130871721));
#407554=CARTESIAN_POINT('Ctrl Pts',(1.59455123108493,-2.13471379736492,
8.86034014101235));
#407555=CARTESIAN_POINT('Ctrl Pts',(1.59441961667038,-2.1347917328564,8.86040910639693));
#407556=CARTESIAN_POINT('Ctrl Pts',(1.59428757440423,-2.13487474190565,
8.86046313645507));
#407557=CARTESIAN_POINT('Ctrl Pts',(1.59408152355376,-2.13500427683179,
8.8605474499083));
#407558=CARTESIAN_POINT('Ctrl Pts',(1.59386888451754,-2.13514982695017,
8.86059655985669));
#407559=CARTESIAN_POINT('Ctrl Pts',(1.59366312900935,-2.13530181594061,
8.86059725258816));
#407560=CARTESIAN_POINT('Ctrl Pts',(1.59345689812372,-2.13545415608633,
8.86059794692012));
#407561=CARTESIAN_POINT('Ctrl Pts',(1.59325687403525,-2.13561679132398,
8.86056369958366));
#407562=CARTESIAN_POINT('Ctrl Pts',(1.59307159215572,-2.13577793168172,
8.86048590497774));
#407563=CARTESIAN_POINT('Ctrl Pts',(1.59302323910167,-2.13581998451737,
8.86046560290182));
#407564=CARTESIAN_POINT('Ctrl Pts',(1.59297532046824,-2.13586255097361,
8.86044257503091));
#407565=CARTESIAN_POINT('Ctrl Pts',(1.59292929518033,-2.13590429117003,
8.86041778462584));
#407566=CARTESIAN_POINT('Ctrl Pts',(1.59261960210531,-2.13618515089669,
8.86025097596201));
#407567=CARTESIAN_POINT('Ctrl Pts',(1.59235429876774,-2.13646653421405,
8.8599848982295));
#407568=CARTESIAN_POINT('Ctrl Pts',(1.5921349641717,-2.13673441605687,8.85968173251461));
#407569=CARTESIAN_POINT('Ctrl Pts',(1.59201894873677,-2.13687611020392,
8.85952137522076));
#407570=CARTESIAN_POINT('Ctrl Pts',(1.59191341042051,-2.13701663718524,
8.85934740853961));
#407571=CARTESIAN_POINT('Ctrl Pts',(1.59181859451242,-2.1371530817186,8.8591675900182));
#407572=CARTESIAN_POINT('Ctrl Pts',(1.5914378593571,-2.1377009774425,8.85844552518695));
#407573=CARTESIAN_POINT('Ctrl Pts',(1.59120601346868,-2.13821228521465,
8.85759444184125));
#407574=CARTESIAN_POINT('Ctrl Pts',(1.59105442443436,-2.13864615733888,
8.8568349891514));
#407575=CARTESIAN_POINT('Ctrl Pts',(1.59103856104563,-2.13869156090119,
8.85675551444999));
#407576=CARTESIAN_POINT('Ctrl Pts',(1.59102359633077,-2.13873611922889,
8.85667699793652));
#407577=CARTESIAN_POINT('Ctrl Pts',(1.59100946472096,-2.13877978665773,
8.85659965593547));
#407578=CARTESIAN_POINT('Ctrl Pts',(1.59081871553061,-2.13936921184039,
8.85555568965886));
#407579=CARTESIAN_POINT('Ctrl Pts',(1.59072051840021,-2.13996323391634,
8.85434650606346));
#407580=CARTESIAN_POINT('Ctrl Pts',(1.59070825637447,-2.14056377579997,
8.85297329937117));
#407581=CARTESIAN_POINT('Ctrl Pts',(1.59070135973213,-2.14090154401796,
8.85220095427747));
#407582=CARTESIAN_POINT('Ctrl Pts',(1.59072195981993,-2.14124151912216,
8.85137579139183));
#407583=CARTESIAN_POINT('Ctrl Pts',(1.59077126558569,-2.1415846479005,8.85049129520029));
#407584=CARTESIAN_POINT('Origin',(1.5975763681687,-2.1406067911448,7.59394543036555));
#407585=CARTESIAN_POINT('Ctrl Pts',(1.59993925707851,-2.13412616443333,
7.59443877723642));
#407586=CARTESIAN_POINT('Ctrl Pts',(1.59467860803057,-2.13170567579607,
7.58783886950016));
#407587=CARTESIAN_POINT('Ctrl Pts',(1.58944159958293,-2.13838796014022,
7.58559994247159));
#407588=CARTESIAN_POINT('Ctrl Pts',(1.62865698589034,-2.14733954089,7.56670252222137));
#407589=CARTESIAN_POINT('Ctrl Pts',(1.62340393997382,-2.14492255054604,
7.56004874999031));
#407590=CARTESIAN_POINT('Ctrl Pts',(1.61811908396272,-2.15163125043485,
7.55786368756704));
#407591=CARTESIAN_POINT('Ctrl Pts',(1.65732108721284,-2.16052824268629,
7.53888913333555));
#407592=CARTESIAN_POINT('Ctrl Pts',(1.65203682218725,-2.15809688805033,
7.53222002137276));
#407593=CARTESIAN_POINT('Ctrl Pts',(1.64674452104206,-2.16484922048506,
7.53005029815326));
#407594=CARTESIAN_POINT('Ctrl Pts',(1.6859302639761,-2.17369167302457,7.51101258149734));
#407595=CARTESIAN_POINT('Ctrl Pts',(1.68058194405662,-2.17123084595257,
7.5043616886572));
#407596=CARTESIAN_POINT('Ctrl Pts',(1.67531646186256,-2.17804129225283,
7.50217374673251));
#407597=CARTESIAN_POINT('',(1.67379182682866,-2.17733734542424,7.50366116523517));
#407598=CARTESIAN_POINT('Ctrl Pts',(1.67813633056182,-2.17010558942598,
7.51860402984325));
#407599=CARTESIAN_POINT('Ctrl Pts',(1.67853751304856,-2.17029017836962,
7.51734760759494));
#407600=CARTESIAN_POINT('Ctrl Pts',(1.67887516973813,-2.17051103085424,
7.51608817408573));
#407601=CARTESIAN_POINT('Ctrl Pts',(1.67914121444952,-2.17077881433842,
7.5148100591312));
#407602=CARTESIAN_POINT('Ctrl Pts',(1.67938220410643,-2.17102137901729,
7.51365231206384));
#407603=CARTESIAN_POINT('Ctrl Pts',(1.67956495208894,-2.17130261697213,
7.51247773061042));
#407604=CARTESIAN_POINT('Ctrl Pts',(1.67965533378806,-2.17163778110541,
7.51129758471022));
#407605=CARTESIAN_POINT('Ctrl Pts',(1.67976766791808,-2.17205435184589,
7.50983079813402));
#407606=CARTESIAN_POINT('Ctrl Pts',(1.6797211573249,-2.17254432228916,7.50839324291155));
#407607=CARTESIAN_POINT('Ctrl Pts',(1.67943339189006,-2.17310347783572,
7.50715379678855));
#407608=CARTESIAN_POINT('Ctrl Pts',(1.67930045255092,-2.17336179158654,
7.50658120839351));
#407609=CARTESIAN_POINT('Ctrl Pts',(1.67908867816629,-2.17366724429874,
7.50598221009429));
#407610=CARTESIAN_POINT('Ctrl Pts',(1.67878441548018,-2.17399960639673,
7.50545747549611));
#407611=CARTESIAN_POINT('Ctrl Pts',(1.67862205149305,-2.17417696509979,
7.50517746087247));
#407612=CARTESIAN_POINT('Ctrl Pts',(1.678431739111,-2.17436404651078,7.50491486231392));
#407613=CARTESIAN_POINT('Ctrl Pts',(1.67821734880152,-2.17455470687897,
7.50468370960992));
#407614=CARTESIAN_POINT('Ctrl Pts',(1.67789676766325,-2.17483980426981,
7.50433806340447));
#407615=CARTESIAN_POINT('Ctrl Pts',(1.6775123660958,-2.17514103710607,7.50405484070984));
#407616=CARTESIAN_POINT('Ctrl Pts',(1.67708959094888,-2.17543755403427,
7.50385766036131));
#407617=CARTESIAN_POINT('Ctrl Pts',(1.67704438171833,-2.17546926191083,
7.50383657498791));
#407618=CARTESIAN_POINT('Ctrl Pts',(1.67699876196236,-2.17550091364686,
7.50381643264937));
#407619=CARTESIAN_POINT('Ctrl Pts',(1.67695278336431,-2.17553248245704,
7.50379723213559));
#407620=CARTESIAN_POINT('Ctrl Pts',(1.67664586118162,-2.17574321459187,
7.50366906242519));
#407621=CARTESIAN_POINT('Ctrl Pts',(1.676315865729,-2.17595424268711,7.50358235568538));
#407622=CARTESIAN_POINT('Ctrl Pts',(1.67599290128614,-2.17615000193079,
7.5035341175365));
#407623=CARTESIAN_POINT('Ctrl Pts',(1.67550865265659,-2.176443520761,7.50346178989176));
#407624=CARTESIAN_POINT('Ctrl Pts',(1.67497523124543,-2.17673869053724,
7.50346967198527));
#407625=CARTESIAN_POINT('Ctrl Pts',(1.67444266060028,-2.17701234294117,
7.50354272648692));
#407626=CARTESIAN_POINT('Ctrl Pts',(1.67422360327037,-2.17712490183918,
7.50357277531559));
#407627=CARTESIAN_POINT('Ctrl Pts',(1.67400504573785,-2.1772337968943,7.50361331098761));
#407628=CARTESIAN_POINT('Ctrl Pts',(1.67379182682952,-2.17733734542536,
7.50366116523659));
#407629=CARTESIAN_POINT('',(1.59932759105275,-2.14295327027006,7.57603338622103));
#407630=CARTESIAN_POINT('Origin',(1.60461077043291,-2.15003701964738,7.58486873427624));
#407631=CARTESIAN_POINT('Ctrl Pts',(1.67379182688274,-2.17733734544331,
7.50366116529968));
#407632=CARTESIAN_POINT('Ctrl Pts',(1.64901056798238,-2.16589544848021,
7.52783573079709));
#407633=CARTESIAN_POINT('Ctrl Pts',(1.62419032049075,-2.15443464751554,
7.55196141284069));
#407634=CARTESIAN_POINT('Ctrl Pts',(1.59932759229144,-2.14295327045252,
7.57603338728831));
#407635=CARTESIAN_POINT('Ctrl Pts',(1.60045004741999,-2.13436118528462,
7.59394543036555));
#407636=CARTESIAN_POINT('Ctrl Pts',(1.58897458506506,-2.12908118542448,
7.59394543036555));
#407637=CARTESIAN_POINT('Ctrl Pts',(1.59077126558569,-2.1415846479005,7.59394543036555));
#407638=CARTESIAN_POINT('Ctrl Pts',(1.59833052356808,-2.1333859665705,7.58587155981958));
#407639=CARTESIAN_POINT('Ctrl Pts',(1.59247285696246,-2.13376855106787,
7.58685956158229));
#407640=CARTESIAN_POINT('Ctrl Pts',(1.59043941776118,-2.13927525189277,
7.58587155981959));
#407641=CARTESIAN_POINT('Ctrl Pts',(1.59858022403627,-2.13877412156755,
7.579829619046));
#407642=CARTESIAN_POINT('Ctrl Pts',(1.59606980950254,-2.13858813978266,
7.58148017275035));
#407643=CARTESIAN_POINT('Ctrl Pts',(1.59553382207232,-2.14104771044236,
7.57982961904594));
#407644=CARTESIAN_POINT('Ctrl Pts',(1.59932759055794,-2.14295326960672,
7.57603338509286));
#407645=CARTESIAN_POINT('Ctrl Pts',(1.59932759055794,-2.14295326960672,
7.57603338509286));
#407646=CARTESIAN_POINT('Ctrl Pts',(1.59932759055794,-2.14295326960672,
7.57603338509286));
#407647=CARTESIAN_POINT('Origin',(1.60461534358175,-2.1500336066184,7.58486873427624));
#407648=CARTESIAN_POINT('Ctrl Pts',(1.60415851687139,-2.23474923235821,
7.51098857897448));
#407649=CARTESIAN_POINT('Ctrl Pts',(1.60332114180601,-2.22892177022005,
7.50433767179956));
#407650=CARTESIAN_POINT('Ctrl Pts',(1.61134830926255,-2.22581168441624,
7.50214974420965));
#407651=CARTESIAN_POINT('Ctrl Pts',(1.5996779710407,-2.20356820934228,7.53887321589168));
#407652=CARTESIAN_POINT('Ctrl Pts',(1.59885062921467,-2.19781057054241,
7.53220407452061));
#407653=CARTESIAN_POINT('Ctrl Pts',(1.60682970075317,-2.19465821629431,
7.53003438070911));
#407654=CARTESIAN_POINT('Ctrl Pts',(1.59518882090922,-2.17232730725995,
7.56669465659231));
#407655=CARTESIAN_POINT('Ctrl Pts',(1.59436636851955,-2.16660369503496,
7.56004085833299));
#407656=CARTESIAN_POINT('Ctrl Pts',(1.60230148007192,-2.16344606067077,
7.55785582193789));
#407657=CARTESIAN_POINT('Ctrl Pts',(1.59069126950323,-2.14102793901221,
7.59443891967696));
#407658=CARTESIAN_POINT('Ctrl Pts',(1.58986762466002,-2.13529602826209,
7.58783901202978));
#407659=CARTESIAN_POINT('Ctrl Pts',(1.59776378899006,-2.13217677084063,
7.58560008491213));
#407660=CARTESIAN_POINT('',(1.61110336926413,-2.22412295723129,7.50366116523517));
#407661=CARTESIAN_POINT('Ctrl Pts',(1.61110336926435,-2.22412295723159,
7.50366116523554));
#407662=CARTESIAN_POINT('Ctrl Pts',(1.61059198069088,-2.22468208087059,
7.50350835821027));
#407663=CARTESIAN_POINT('Ctrl Pts',(1.61010369996945,-2.22517941370504,
7.50345484955999));
#407664=CARTESIAN_POINT('Ctrl Pts',(1.6096244386178,-2.22563016254552,7.50349758195598));
#407665=CARTESIAN_POINT('Ctrl Pts',(1.60937854200145,-2.22586143012909,
7.50351950684424));
#407666=CARTESIAN_POINT('Ctrl Pts',(1.60911087181361,-2.22610332366122,
7.50357029184312));
#407667=CARTESIAN_POINT('Ctrl Pts',(1.60884634880778,-2.22632948384842,
7.50365515313923));
#407668=CARTESIAN_POINT('Ctrl Pts',(1.60843940530886,-2.22667740979762,
7.50378570417639));
#407669=CARTESIAN_POINT('Ctrl Pts',(1.60802819036978,-2.22699857665867,
7.50400001621911));
#407670=CARTESIAN_POINT('Ctrl Pts',(1.60764260590767,-2.22726674962692,
7.50428903009634));
#407671=CARTESIAN_POINT('Ctrl Pts',(1.60759980899889,-2.2272965147632,7.50432110841318));
#407672=CARTESIAN_POINT('Ctrl Pts',(1.60755731717551,-2.22732565543006,
7.50435406373354));
#407673=CARTESIAN_POINT('Ctrl Pts',(1.60751516316796,-2.22735415659424,
7.50438785222352));
#407674=CARTESIAN_POINT('Ctrl Pts',(1.6072577926901,-2.22752816990097,7.50459414719561));
#407675=CARTESIAN_POINT('Ctrl Pts',(1.60700862846067,-2.22768068774653,
7.50483629897752));
#407676=CARTESIAN_POINT('Ctrl Pts',(1.60677790295502,-2.2278069896599,7.5050991045531));
#407677=CARTESIAN_POINT('Ctrl Pts',(1.60626889931537,-2.22808562436662,
7.50567888004914));
#407678=CARTESIAN_POINT('Ctrl Pts',(1.60582982688947,-2.22824810547531,
7.50637912803145));
#407679=CARTESIAN_POINT('Ctrl Pts',(1.60546347309896,-2.2283252168882,7.50710440483569));
#407680=CARTESIAN_POINT('Ctrl Pts',(1.60537363587638,-2.22834412613751,
7.50728225710685));
#407681=CARTESIAN_POINT('Ctrl Pts',(1.60528641310259,-2.22835842111518,
7.50746498566955));
#407682=CARTESIAN_POINT('Ctrl Pts',(1.60520390821617,-2.22836817923873,
7.50764697238949));
#407683=CARTESIAN_POINT('Ctrl Pts',(1.60476038465272,-2.2284206362254,7.50862528291182));
#407684=CARTESIAN_POINT('Ctrl Pts',(1.60441342469444,-2.22835085759283,
7.50965856837421));
#407685=CARTESIAN_POINT('Ctrl Pts',(1.60413297204736,-2.22821793661503,
7.51067959873201));
#407686=CARTESIAN_POINT('Ctrl Pts',(1.60397863860193,-2.22814479003328,
7.51124147302578));
#407687=CARTESIAN_POINT('Ctrl Pts',(1.60384459404931,-2.22805211156061,
7.51180065547252));
#407688=CARTESIAN_POINT('Ctrl Pts',(1.60372708158229,-2.22794733879844,
7.512351757165));
#407689=CARTESIAN_POINT('Ctrl Pts',(1.60332102919734,-2.22758530716863,
7.51425603304535));
#407690=CARTESIAN_POINT('Ctrl Pts',(1.60306798798222,-2.22703118031392,
7.5162690050518));
#407691=CARTESIAN_POINT('Ctrl Pts',(1.60295199935764,-2.22634316468706,
7.51827788969243));
#407692=CARTESIAN_POINT('Ctrl Pts',(1.60294572183409,-2.22630592798116,
7.51838661432545));
#407693=CARTESIAN_POINT('Ctrl Pts',(1.60293985101504,-2.22626829062669,
7.51849533314856));
#407694=CARTESIAN_POINT('Ctrl Pts',(1.60293438610528,-2.22623025921638,
7.51860402984325));
#407695=CARTESIAN_POINT('Ctrl Pts',(1.59932759087574,-2.14295327151057,
7.57603338728985));
#407696=CARTESIAN_POINT('Ctrl Pts',(1.60326028592398,-2.17005513828705,
7.55196141284922));
#407697=CARTESIAN_POINT('Ctrl Pts',(1.60718534226389,-2.19711042572332,
7.52783573083105));
#407698=CARTESIAN_POINT('Ctrl Pts',(1.61110336926721,-2.22412295729039,
7.50366116530176));
#407699=CARTESIAN_POINT('Origin',(5.52641612598468E-16,-7.40489414195296E-16,
7.49482233047033));
#407700=CARTESIAN_POINT('Origin',(1.66840488432878,-2.17032978875283,7.49482233047033));
#407701=CARTESIAN_POINT('Origin',(0.,0.,7.50366116523517));
#407702=CARTESIAN_POINT('Origin',(1.60591818370373,-2.2169648254426,7.49482233047033));
#407703=CARTESIAN_POINT('Ctrl Pts',(1.67813536969269,-2.17010514726914,
7.51860402984325));
#407704=CARTESIAN_POINT('Ctrl Pts',(1.68504747448013,-2.17328619952233,
7.51860402984325));
#407705=CARTESIAN_POINT('Ctrl Pts',(1.69104778275851,-2.16860724808056,
7.51860402984325));
#407706=CARTESIAN_POINT('Ctrl Pts',(1.68070188190216,-2.17128629252502,
7.51041458714365));
#407707=CARTESIAN_POINT('Ctrl Pts',(1.6864690101503,-2.17217769452731,7.51004642900442));
#407708=CARTESIAN_POINT('Ctrl Pts',(1.69104943757229,-2.16860595768131,
7.50729136483009));
#407709=CARTESIAN_POINT('Ctrl Pts',(1.68047942032506,-2.17409240158313,
7.50215815450137));
#407710=CARTESIAN_POINT('Ctrl Pts',(1.68357470801357,-2.1744348320239,7.49877163671531));
#407711=CARTESIAN_POINT('Ctrl Pts',(1.68631009160464,-2.17233207188443,
7.49481588533172));
#407712=CARTESIAN_POINT('Ctrl Pts',(1.67379149130793,-2.17733690896584,
7.50366171572174));
#407713=CARTESIAN_POINT('Ctrl Pts',(1.67602317147152,-2.18023997043687,
7.50000045605858));
#407714=CARTESIAN_POINT('Ctrl Pts',(1.67602317147162,-2.18023997043679,
7.49482233047317));
#407715=CARTESIAN_POINT('Origin',(1.68336120192779,-2.15874994240746,7.51860402984325));
#407716=CARTESIAN_POINT('Origin',(1.68336120192779,-2.15874994240746,9.));
#407717=CARTESIAN_POINT('Origin',(1.68336120192779,-2.15874994240746,8.75721825406948));
#407718=CARTESIAN_POINT('Ctrl Pts',(1.66296505241367,-2.1631250664948,8.78942910404913));
#407719=CARTESIAN_POINT('Ctrl Pts',(1.66801889291353,-2.16547264501399,
8.79672699501691));
#407720=CARTESIAN_POINT('Ctrl Pts',(1.67320190366869,-2.15820560397282,
8.79893251111267));
#407721=CARTESIAN_POINT('Ctrl Pts',(1.67295287420541,-2.16772058981614,
8.78111911759576));
#407722=CARTESIAN_POINT('Ctrl Pts',(1.67894739662943,-2.17049692031404,
8.78644465894812));
#407723=CARTESIAN_POINT('Ctrl Pts',(1.6849604788733,-2.16506016082844,8.78817647674131));
#407724=CARTESIAN_POINT('Ctrl Pts',(1.67917752299134,-2.17058462953467,
8.76780923932034));
#407725=CARTESIAN_POINT('Ctrl Pts',(1.68625594515373,-2.17385734651929,
8.76988516158375));
#407726=CARTESIAN_POINT('Ctrl Pts',(1.69231030965761,-2.16933174701751,
8.77093053738834));
#407727=CARTESIAN_POINT('Ctrl Pts',(1.67796380166913,-2.17002618098512,
8.75371302330491));
#407728=CARTESIAN_POINT('Ctrl Pts',(1.6848681772406,-2.17321926716246,8.75300828287559));
#407729=CARTESIAN_POINT('Ctrl Pts',(1.69087702405881,-2.16849821862959,
8.75267964240738));
#407730=CARTESIAN_POINT('Origin',(1.67062236339845,-2.15288864779702,8.78727029226991));
#407731=CARTESIAN_POINT('Ctrl Pts',(1.60045004741999,-2.13436118528462,
8.85049129520029));
#407732=CARTESIAN_POINT('Ctrl Pts',(1.60575505664343,-2.13680208457838,
8.85711686593484));
#407733=CARTESIAN_POINT('Ctrl Pts',(1.61100669796545,-2.13005515746015,
8.85933012996512));
#407734=CARTESIAN_POINT('Ctrl Pts',(1.62213069385386,-2.14433671451368,
8.82945683644722));
#407735=CARTESIAN_POINT('Ctrl Pts',(1.62747973786134,-2.14679787474736,
8.83607469902389));
#407736=CARTESIAN_POINT('Ctrl Pts',(1.63271720381485,-2.14000810355218,
8.83829567148519));
#407737=CARTESIAN_POINT('Ctrl Pts',(1.64377902353591,-2.154297374412,8.80838214965002));
#407738=CARTESIAN_POINT('Ctrl Pts',(1.64914917736847,-2.15676824753308,
8.81501364461992));
#407739=CARTESIAN_POINT('Ctrl Pts',(1.65439449734903,-2.14994655925988,
8.81722098428722));
#407740=CARTESIAN_POINT('Ctrl Pts',(1.66539749203248,-2.16424429481554,
8.78727029226991));
#407741=CARTESIAN_POINT('Ctrl Pts',(1.67076853786521,-2.16671557835676,
8.79393457792714));
#407742=CARTESIAN_POINT('Ctrl Pts',(1.67604110579952,-2.15987164362911,
8.79610912703474));
#407743=CARTESIAN_POINT('Origin',(1.60567491878596,-2.1230055382661,8.85049129520029));
#407744=CARTESIAN_POINT('Ctrl Pts',(1.59077126558569,-2.1415846479005,8.85049129520029));
#407745=CARTESIAN_POINT('Ctrl Pts',(1.59160185579972,-2.14736489288834,
8.85711686593484));
#407746=CARTESIAN_POINT('Ctrl Pts',(1.58363955683349,-2.15047978570931,
8.85933012996512));
#407747=CARTESIAN_POINT('Ctrl Pts',(1.59003645441303,-2.13647094859846,
8.86332496987231));
#407748=CARTESIAN_POINT('Ctrl Pts',(1.58650902291591,-2.13945576373675,
8.86648636486736));
#407749=CARTESIAN_POINT('Ctrl Pts',(1.58160085107661,-2.13617156656108,
8.87206031107458));
#407750=CARTESIAN_POINT('Ctrl Pts',(1.5957248901228,-2.13218708291762,8.86341338519877));
#407751=CARTESIAN_POINT('Ctrl Pts',(1.59958467164427,-2.1296227979801,8.86654584966057));
#407752=CARTESIAN_POINT('Ctrl Pts',(1.59776984823889,-2.12398093935068,
8.87215952290713));
#407753=CARTESIAN_POINT('Ctrl Pts',(1.60045004741999,-2.13436118528462,
8.85049129520029));
#407754=CARTESIAN_POINT('Ctrl Pts',(1.60575505664343,-2.13680208457838,
8.85711686593484));
#407755=CARTESIAN_POINT('Ctrl Pts',(1.61100669796545,-2.13005515746015,
8.85933012996512));
#407756=CARTESIAN_POINT('Origin',(1.57839835179839,-2.14336256927449,8.85049129520029));
#407757=CARTESIAN_POINT('Ctrl Pts',(1.60093990236831,-2.21235024422324,
8.78727029226991));
#407758=CARTESIAN_POINT('Ctrl Pts',(1.60178083174655,-2.21820244154213,
8.79393457792714));
#407759=CARTESIAN_POINT('Ctrl Pts',(1.59371958050517,-2.22130979469258,
8.79610912703474));
#407760=CARTESIAN_POINT('Ctrl Pts',(1.59755516020871,-2.18879514018686,
8.80838214965003));
#407761=CARTESIAN_POINT('Ctrl Pts',(1.598395949929,-2.19464636559799,8.8150136446199));
#407762=CARTESIAN_POINT('Ctrl Pts',(1.59036377844287,-2.19773392674114,
8.81722098428722));
#407763=CARTESIAN_POINT('Ctrl Pts',(1.59416574276819,-2.16520749992663,
8.82945683644723));
#407764=CARTESIAN_POINT('Ctrl Pts',(1.59500322738317,-2.17103572444266,
8.83607469902388));
#407765=CARTESIAN_POINT('Ctrl Pts',(1.58700388846104,-2.17412483747174,
8.8382956714852));
#407766=CARTESIAN_POINT('Ctrl Pts',(1.59077126558569,-2.1415846479005,8.85049129520029));
#407767=CARTESIAN_POINT('Ctrl Pts',(1.59160185579972,-2.14736489288834,
8.85711686593484));
#407768=CARTESIAN_POINT('Ctrl Pts',(1.58363955683349,-2.15047978570931,
8.85933012996512));
#407769=CARTESIAN_POINT('Origin',(1.58856698858102,-2.21412816559723,8.78727029226991));
#407770=CARTESIAN_POINT('Ctrl Pts',(1.60290803169132,-2.22604698322441,
8.75374538247847));
#407771=CARTESIAN_POINT('Ctrl Pts',(1.60400184926499,-2.23356681975875,
8.75304829418601));
#407772=CARTESIAN_POINT('Ctrl Pts',(1.59777613670621,-2.23798396208661,
8.75272238421917));
#407773=CARTESIAN_POINT('Ctrl Pts',(1.60309577828932,-2.22735354670507,
8.76769408445022));
#407774=CARTESIAN_POINT('Ctrl Pts',(1.60421643824611,-2.23506271502813,
8.7697431809397));
#407775=CARTESIAN_POINT('Ctrl Pts',(1.59816348603556,-2.23957715040998,
8.77077869880429));
#407776=CARTESIAN_POINT('Ctrl Pts',(1.60213349619481,-2.22065684660117,
8.78108014887987));
#407777=CARTESIAN_POINT('Ctrl Pts',(1.60308697501545,-2.22718954247952,
8.78639403366323));
#407778=CARTESIAN_POINT('Ctrl Pts',(1.59618455646938,-2.23141786294321,
8.78812224174742));
#407779=CARTESIAN_POINT('Ctrl Pts',(1.60055652823306,-2.20968243344753,
8.78944554828686));
#407780=CARTESIAN_POINT('Ctrl Pts',(1.60136562387223,-2.21518713887686,
8.79673892988686));
#407781=CARTESIAN_POINT('Ctrl Pts',(1.59293408710644,-2.2180876116114,8.79894799272499));
#407782=CARTESIAN_POINT('Origin',(1.59056147231799,-2.22800818059038,8.75721825406948));
#407783=CARTESIAN_POINT('Origin',(1.59056147231799,-2.22800818059038,9.));
#407784=CARTESIAN_POINT('Origin',(1.59056147231799,-2.22800818059038,7.51860402984325));
#407785=CARTESIAN_POINT('Ctrl Pts',(1.61110290777819,-2.22412232015155,
7.50366195182966));
#407786=CARTESIAN_POINT('Ctrl Pts',(1.61325114344655,-2.2270879524995,7.50000065167735));
#407787=CARTESIAN_POINT('Ctrl Pts',(1.61325114344646,-2.22708795249957,
7.49482233047108));
#407788=CARTESIAN_POINT('Ctrl Pts',(1.60608447429974,-2.2296149629607,7.50215800491337));
#407789=CARTESIAN_POINT('Ctrl Pts',(1.60553053494263,-2.23268055399066,
7.49877273257264));
#407790=CARTESIAN_POINT('Ctrl Pts',(1.60273484608026,-2.23470571574587,
7.49481816995649));
#407791=CARTESIAN_POINT('Ctrl Pts',(1.60333561962302,-2.22902014003884,
7.51043025814043));
#407792=CARTESIAN_POINT('Ctrl Pts',(1.60255251348734,-2.23480628744168,
7.51006209594517));
#407793=CARTESIAN_POINT('Ctrl Pts',(1.59782224944538,-2.23818320500886,
7.50731281821699));
#407794=CARTESIAN_POINT('Ctrl Pts',(1.60293417104175,-2.22622876318826,
7.51860402984326));
#407795=CARTESIAN_POINT('Ctrl Pts',(1.60401737669502,-2.23376054139154,
7.51860402984327));
#407796=CARTESIAN_POINT('Ctrl Pts',(1.59782431009112,-2.23818173392641,
7.51860402984327));
#407797=CARTESIAN_POINT('Origin',(0.,0.,7.5));
#407798=CARTESIAN_POINT('Origin',(1.72471465490916,-2.03526346763208,7.5));
#407799=CARTESIAN_POINT('',(1.72471465490916,-2.03526346763208,7.59394543036555));
#407800=CARTESIAN_POINT('',(1.72471465490916,-2.03526346763208,8.85049129520029));
#407801=CARTESIAN_POINT('',(1.72471465490916,-2.03526346763208,7.5));
#407802=CARTESIAN_POINT('',(1.7393963664604,-2.10523216165202,8.78727029226991));
#407803=CARTESIAN_POINT('Ctrl Pts',(1.72471465490916,-2.03526346763208,
8.85049129520029));
#407804=CARTESIAN_POINT('Ctrl Pts',(1.72961567252277,-2.05862026772968,
8.82945686509571));
#407805=CARTESIAN_POINT('Ctrl Pts',(1.73450940418107,-2.08194234511967,
8.80838212259896));
#407806=CARTESIAN_POINT('Ctrl Pts',(1.7393963664604,-2.10523216165202,8.78727029226991));
#407807=CARTESIAN_POINT('',(1.74227604793057,-2.11895587165396,8.75721825406948));
#407808=CARTESIAN_POINT('Origin',(1.73361028491986,-2.07765642602876,8.75937679713156));
#407809=CARTESIAN_POINT('',(1.74227604793057,-2.11895587165396,7.51860402984325));
#407810=CARTESIAN_POINT('',(1.74227604793057,-2.11895587165396,7.5));
#407811=CARTESIAN_POINT('Ctrl Pts',(1.74227604793057,-2.11895587165396,
7.51860402984325));
#407812=CARTESIAN_POINT('Ctrl Pts',(1.74001450601094,-2.10817803188807,
7.52834476460825));
#407813=CARTESIAN_POINT('Ctrl Pts',(1.73775149593093,-2.09739319530413,
7.53807742314407));
#407814=CARTESIAN_POINT('Ctrl Pts',(1.7354869683951,-2.08660112697466,7.54780169004674));
#407815=CARTESIAN_POINT('Ctrl Pts',(1.73190007916561,-2.06950707400231,
7.5632044032688));
#407816=CARTESIAN_POINT('Ctrl Pts',(1.72830937827432,-2.05239485577746,
7.57858609112103));
#407817=CARTESIAN_POINT('Ctrl Pts',(1.72471465490916,-2.03526346763208,
7.59394543036555));
#407818=CARTESIAN_POINT('Origin',(1.9905863760048,-2.12613942982102,7.5));
#407819=CARTESIAN_POINT('',(1.81372756198702,-2.05812831089268,8.75721825406948));
#407820=CARTESIAN_POINT('',(1.80063936233261,-2.05309523912752,8.78727029226991));
#407821=CARTESIAN_POINT('Origin',(1.76741662995361,-2.04031942574495,8.75658640621003));
#407822=CARTESIAN_POINT('',(1.73391074180931,-2.02743472471359,8.85049129520029));
#407823=CARTESIAN_POINT('Ctrl Pts',(1.80063936233261,-2.05309523912752,
8.78727029226991));
#407824=CARTESIAN_POINT('Ctrl Pts',(1.77842803837963,-2.04455386671523,
8.80838212259896));
#407825=CARTESIAN_POINT('Ctrl Pts',(1.75618594748783,-2.03600066286583,
8.82945686509571));
#407826=CARTESIAN_POINT('Ctrl Pts',(1.73391074180931,-2.02743472471359,
8.85049129520029));
#407827=CARTESIAN_POINT('',(1.73391074180931,-2.02743472471359,7.59394543036555));
#407828=CARTESIAN_POINT('',(1.73391074180931,-2.02743472471359,7.5));
#407829=CARTESIAN_POINT('',(1.81372756198702,-2.05812831089268,7.51860402984325));
#407830=CARTESIAN_POINT('Ctrl Pts',(1.73391074180931,-2.02743472471359,
7.59394543036555));
#407831=CARTESIAN_POINT('Ctrl Pts',(1.75024881863928,-2.03371753788586,
7.57858609112103));
#407832=CARTESIAN_POINT('Ctrl Pts',(1.76656861325912,-2.03999332062783,
7.56320440326857));
#407833=CARTESIAN_POINT('Ctrl Pts',(1.78287108381363,-2.04626244139439,
7.54780169004651));
#407834=CARTESIAN_POINT('Ctrl Pts',(1.79316339871683,-2.05022035469838,
7.53807742314383));
#407835=CARTESIAN_POINT('Ctrl Pts',(1.80344881675856,-2.05417561581187,
7.52834476460825));
#407836=CARTESIAN_POINT('Ctrl Pts',(1.81372756198702,-2.05812831089268,
7.51860402984324));
#407837=CARTESIAN_POINT('',(1.81372756198702,-2.05812831089268,7.5));
#407838=CARTESIAN_POINT('Origin',(1.73144312418163,-2.03385161556848,7.5));
#407839=CARTESIAN_POINT('Ctrl Pts',(1.73391074180931,-2.02743472471359,
8.85049129520029));
#407840=CARTESIAN_POINT('Ctrl Pts',(1.73372998475531,-2.02736521452511,
8.85097269580138));
#407841=CARTESIAN_POINT('Ctrl Pts',(1.73354848920976,-2.02730443226223,
8.85143669361005));
#407842=CARTESIAN_POINT('Ctrl Pts',(1.73335762024977,-2.02725040812867,
8.8519052845931));
#407843=CARTESIAN_POINT('Ctrl Pts',(1.73298429266852,-2.02714474034953,
8.85282181883899));
#407844=CARTESIAN_POINT('Ctrl Pts',(1.73258465538969,-2.02706783471853,
8.85372622499635));
#407845=CARTESIAN_POINT('Ctrl Pts',(1.73214952371884,-2.02703362538743,
8.8546225773507));
#407846=CARTESIAN_POINT('Ctrl Pts',(1.73178829286012,-2.02700522601574,
8.85536669723986));
#407847=CARTESIAN_POINT('Ctrl Pts',(1.73140252033166,-2.02700621380077,
8.85610498449051));
#407848=CARTESIAN_POINT('Ctrl Pts',(1.73098693899631,-2.02705256355857,
8.85681338218371));
#407849=CARTESIAN_POINT('Ctrl Pts',(1.7306097982818,-2.02709462603657,8.85745625420285));
#407850=CARTESIAN_POINT('Ctrl Pts',(1.73020331107266,-2.02717397960763,
8.85808743050666));
#407851=CARTESIAN_POINT('Ctrl Pts',(1.72976030302272,-2.02731830774888,
8.85866804508411));
#407852=CARTESIAN_POINT('Ctrl Pts',(1.72955590871172,-2.02738489762461,
8.85893592806396));
#407853=CARTESIAN_POINT('Ctrl Pts',(1.72934370783829,-2.02746555882914,
8.85919241173848));
#407854=CARTESIAN_POINT('Ctrl Pts',(1.72912300557579,-2.02756460635871,
8.85943017985534));
#407855=CARTESIAN_POINT('Ctrl Pts',(1.72882499218654,-2.02769834984485,
8.8597512372));
#407856=CARTESIAN_POINT('Ctrl Pts',(1.72850415527126,-2.02786960562471,
8.86004599534705));
#407857=CARTESIAN_POINT('Ctrl Pts',(1.72816925396771,-2.0280855042143,8.86026130871721));
#407858=CARTESIAN_POINT('Ctrl Pts',(1.72804663715862,-2.02816455077478,
8.86034014101235));
#407859=CARTESIAN_POINT('Ctrl Pts',(1.72792028650408,-2.02825075870392,
8.86040910639692));
#407860=CARTESIAN_POINT('Ctrl Pts',(1.72779383394098,-2.02834205717921,
8.86046313645506));
#407861=CARTESIAN_POINT('Ctrl Pts',(1.72759650577529,-2.02848452768528,
8.86054744990829));
#407862=CARTESIAN_POINT('Ctrl Pts',(1.72739362905688,-2.02864340258515,
8.86059655985669));
#407863=CARTESIAN_POINT('Ctrl Pts',(1.72719803426349,-2.02880826209858,
8.86059725258816));
#407864=CARTESIAN_POINT('Ctrl Pts',(1.727001987568,-2.02897350250335,8.86059794692012));
#407865=CARTESIAN_POINT('Ctrl Pts',(1.72681279452592,-2.0291486191768,8.86056369958366));
#407866=CARTESIAN_POINT('Ctrl Pts',(1.72663821762605,-2.02932129950518,
8.86048590497774));
#407867=CARTESIAN_POINT('Ctrl Pts',(1.72659265825296,-2.02936636392957,
8.86046560290182));
#407868=CARTESIAN_POINT('Ctrl Pts',(1.72654756531572,-2.02941191308585,
8.86044257503091));
#407869=CARTESIAN_POINT('Ctrl Pts',(1.72650430889527,-2.02945651637288,
8.86041778462583));
#407870=CARTESIAN_POINT('Ctrl Pts',(1.72621324686235,-2.02975664114655,
8.86025097596201));
#407871=CARTESIAN_POINT('Ctrl Pts',(1.72596651690999,-2.03005444437491,
8.8599848982295));
#407872=CARTESIAN_POINT('Ctrl Pts',(1.72576479620899,-2.03033582864157,
8.85968173251462));
#407873=CARTESIAN_POINT('Ctrl Pts',(1.72565809751539,-2.03048466479723,
8.85952137522077));
#407874=CARTESIAN_POINT('Ctrl Pts',(1.72556177963353,-2.03063166491394,
8.85934740853961));
#407875=CARTESIAN_POINT('Ctrl Pts',(1.72547590056616,-2.03077390398346,
8.8591675900182));
#407876=CARTESIAN_POINT('Ctrl Pts',(1.72513105147161,-2.03134506778199,
8.85844552518696));
#407877=CARTESIAN_POINT('Ctrl Pts',(1.72493244153686,-2.03187017943455,
8.85759444184125));
#407878=CARTESIAN_POINT('Ctrl Pts',(1.72480896224092,-2.03231287246475,
8.8568349891514));
#407879=CARTESIAN_POINT('Ctrl Pts',(1.72479604046145,-2.03235919911137,
8.85675551444999));
#407880=CARTESIAN_POINT('Ctrl Pts',(1.72478396135506,-2.03240462468179,
8.85667699793652));
#407881=CARTESIAN_POINT('Ctrl Pts',(1.72477265656193,-2.03244910780656,
8.85659965593547));
#407882=CARTESIAN_POINT('Ctrl Pts',(1.72462006388736,-2.03304954329455,
8.85555568965886));
#407883=CARTESIAN_POINT('Ctrl Pts',(1.72456012763858,-2.03364863640018,
8.85434650606346));
#407884=CARTESIAN_POINT('Ctrl Pts',(1.72458636765708,-2.0342487300368,8.85297329937117));
#407885=CARTESIAN_POINT('Ctrl Pts',(1.72460112606866,-2.03458624614315,
8.85220095427747));
#407886=CARTESIAN_POINT('Ctrl Pts',(1.72464346611107,-2.03492420287988,
8.85137579139183));
#407887=CARTESIAN_POINT('Ctrl Pts',(1.72471465490916,-2.03526346763208,
8.85049129520029));
#407888=CARTESIAN_POINT('Origin',(1.73144312418163,-2.03385161556848,7.59394543036555));
#407889=CARTESIAN_POINT('Ctrl Pts',(1.73338594310373,-2.02723291318739,
7.59443877723642));
#407890=CARTESIAN_POINT('Ctrl Pts',(1.72798102138401,-2.02515444864538,
7.58783886950016));
#407891=CARTESIAN_POINT('Ctrl Pts',(1.7231829083598,-2.03215853980295,7.58559994247159));
#407892=CARTESIAN_POINT('Ctrl Pts',(1.76289125219805,-2.03857919014268,
7.5667025222214));
#407893=CARTESIAN_POINT('Ctrl Pts',(1.75749414212467,-2.03650372957208,
7.5600487499903));
#407894=CARTESIAN_POINT('Ctrl Pts',(1.75264997229473,-2.04353724760462,
7.55786368756704));
#407895=CARTESIAN_POINT('Ctrl Pts',(1.79234146307551,-2.04990427905937,
7.53888913333558));
#407896=CARTESIAN_POINT('Ctrl Pts',(1.78691227771274,-2.04781648392493,
7.53222002137277));
#407897=CARTESIAN_POINT('Ctrl Pts',(1.78206347359233,-2.05489402186702,
7.53005029815327));
#407898=CARTESIAN_POINT('Ctrl Pts',(1.82173524309424,-2.06120766746955,
7.51101258149734));
#407899=CARTESIAN_POINT('Ctrl Pts',(1.8162402461398,-2.05909456446446,7.5043616886572));
#407900=CARTESIAN_POINT('Ctrl Pts',(1.81142192923626,-2.06622837857485,
7.50217374673251));
#407901=CARTESIAN_POINT('',(1.80985532470038,-2.06562356178253,7.50366116523517));
#407902=CARTESIAN_POINT('Ctrl Pts',(1.81372756198702,-2.05812831089268,
7.51860402984325));
#407903=CARTESIAN_POINT('Ctrl Pts',(1.81413974685554,-2.05828681672836,
7.51734760759493));
#407904=CARTESIAN_POINT('Ctrl Pts',(1.8144908598605,-2.05848558170949,7.51608817408573));
#407905=CARTESIAN_POINT('Ctrl Pts',(1.81477351490123,-2.0587357694606,7.5148100591312));
#407906=CARTESIAN_POINT('Ctrl Pts',(1.81502955059139,-2.05896239550399,
7.51365231206384));
#407907=CARTESIAN_POINT('Ctrl Pts',(1.8152299420762,-2.05923134692185,7.51247773061042));
#407908=CARTESIAN_POINT('Ctrl Pts',(1.81534161211617,-2.05956003164913,
7.51129758471022));
#407909=CARTESIAN_POINT('Ctrl Pts',(1.81548040522266,-2.05996854922792,
7.50983079813402));
#407910=CARTESIAN_POINT('Ctrl Pts',(1.81546538270456,-2.06046049291831,
7.50839324291155));
#407911=CARTESIAN_POINT('Ctrl Pts',(1.81521403373354,-2.06103693681454,
7.50715379678855));
#407912=CARTESIAN_POINT('Ctrl Pts',(1.81509791775138,-2.06130323728476,
7.50658120839351));
#407913=CARTESIAN_POINT('Ctrl Pts',(1.81490614890239,-2.06162163084301,
7.50598221009429));
#407914=CARTESIAN_POINT('Ctrl Pts',(1.81462380586933,-2.06197280424466,
7.50545747549611));
#407915=CARTESIAN_POINT('Ctrl Pts',(1.81447313888755,-2.06216020124161,
7.50517746087247));
#407916=CARTESIAN_POINT('Ctrl Pts',(1.81429520386986,-2.06235909162996,
7.50491486231392));
#407917=CARTESIAN_POINT('Ctrl Pts',(1.81409346969999,-2.06256309630026,
7.50468370960992));
#407918=CARTESIAN_POINT('Ctrl Pts',(1.8137918134826,-2.06286814763199,7.50433806340447));
#407919=CARTESIAN_POINT('Ctrl Pts',(1.81342750176348,-2.06319339024607,
7.50405484070984));
#407920=CARTESIAN_POINT('Ctrl Pts',(1.81302459315826,-2.06351638524511,
7.50385766036131));
#407921=CARTESIAN_POINT('Ctrl Pts',(1.81298150834555,-2.06355092453978,
7.50383657498791));
#407922=CARTESIAN_POINT('Ctrl Pts',(1.81293801025395,-2.06358543411172,
7.50381643264937));
#407923=CARTESIAN_POINT('Ctrl Pts',(1.81289414874447,-2.06361988391929,
7.50379723213559));
#407924=CARTESIAN_POINT('Ctrl Pts',(1.81260135882057,-2.0638498476541,7.50366906242519));
#407925=CARTESIAN_POINT('Ctrl Pts',(1.81228556199548,-2.06408158505074,
7.50358235568538));
#407926=CARTESIAN_POINT('Ctrl Pts',(1.81197580345551,-2.06429763448895,
7.5035341175365));
#407927=CARTESIAN_POINT('Ctrl Pts',(1.81151135558272,-2.06462157616947,
7.50346178989177));
#407928=CARTESIAN_POINT('Ctrl Pts',(1.81099794173556,-2.0649503159149,7.50346967198527));
#407929=CARTESIAN_POINT('Ctrl Pts',(1.81048399828363,-2.06525752798901,
7.50354272648693));
#407930=CARTESIAN_POINT('Ctrl Pts',(1.81027260270386,-2.065383890674,7.50357277531559));
#407931=CARTESIAN_POINT('Ctrl Pts',(1.81006147115137,-2.06550656502174,
7.50361331098761));
#407932=CARTESIAN_POINT('Ctrl Pts',(1.80985532470131,-2.0656235617836,7.50366116523659));
#407933=CARTESIAN_POINT('',(1.73334108842418,-2.0360810723653,7.57603338622103));
#407934=CARTESIAN_POINT('Origin',(1.73906727032635,-2.04281177295423,7.58486873427629));
#407935=CARTESIAN_POINT('Ctrl Pts',(1.80985532475557,-2.0656235617981,7.50366116529968));
#407936=CARTESIAN_POINT('Ctrl Pts',(1.78439189675399,-2.05579291414859,
7.52783573079709));
#407937=CARTESIAN_POINT('Ctrl Pts',(1.75888834908382,-2.04594589934544,
7.55196141284069));
#407938=CARTESIAN_POINT('Ctrl Pts',(1.73334108967202,-2.03608107246802,
7.57603338728831));
#407939=CARTESIAN_POINT('Ctrl Pts',(1.73480751822065,-2.02796794848293,
7.59639677331372));
#407940=CARTESIAN_POINT('Ctrl Pts',(1.71899942470746,-2.01879319534087,
7.5995988229546));
#407941=CARTESIAN_POINT('Ctrl Pts',(1.72503565868803,-2.03606376834598,
7.59642833564546));
#407942=CARTESIAN_POINT('Ctrl Pts',(1.73179248798734,-2.02549313601005,
7.58707626057424));
#407943=CARTESIAN_POINT('Ctrl Pts',(1.72505320902729,-2.02619627904982,
7.58809943920598));
#407944=CARTESIAN_POINT('Ctrl Pts',(1.72318313120985,-2.03269375623325,
7.58710240504251));
#407945=CARTESIAN_POINT('Ctrl Pts',(1.73230984781107,-2.03154771866075,
7.5801537675693));
#407946=CARTESIAN_POINT('Ctrl Pts',(1.72945965908282,-2.0314722494012,7.58205880659759));
#407947=CARTESIAN_POINT('Ctrl Pts',(1.7290422181741,-2.03425663768693,7.58020924244129));
#407948=CARTESIAN_POINT('Ctrl Pts',(1.73334108788788,-2.03608107173502,
7.57603338509286));
#407949=CARTESIAN_POINT('Ctrl Pts',(1.73334108788788,-2.03608107173502,
7.57603338509286));
#407950=CARTESIAN_POINT('Ctrl Pts',(1.73334108788788,-2.03608107173502,
7.57603338509286));
#407951=CARTESIAN_POINT('Origin',(1.73907161540585,-2.04280807393549,7.5848687342762));
#407952=CARTESIAN_POINT('Ctrl Pts',(1.74404347607193,-2.12737891132435,
7.51098857897448));
#407953=CARTESIAN_POINT('Ctrl Pts',(1.74283445470231,-2.12161707313678,
7.50433767179957));
#407954=CARTESIAN_POINT('Ctrl Pts',(1.75064586560079,-2.11799907495305,
7.50214974420965));
#407955=CARTESIAN_POINT('Ctrl Pts',(1.73757436099934,-2.09654902262137,
7.53887321589169));
#407956=CARTESIAN_POINT('Ctrl Pts',(1.73637982585136,-2.09085622148072,
7.53220407452065));
#407957=CARTESIAN_POINT('Ctrl Pts',(1.74414053150149,-2.08719912321377,
7.53003438070911));
#407958=CARTESIAN_POINT('Ctrl Pts',(1.73109282283946,-2.0656599291594,7.56669465659233));
#407959=CARTESIAN_POINT('Ctrl Pts',(1.72990534717208,-2.06000077141512,
7.56004085833302));
#407960=CARTESIAN_POINT('Ctrl Pts',(1.7376218448584,-2.05634122040663,7.55785582193789));
#407961=CARTESIAN_POINT('Ctrl Pts',(1.7245991547263,-2.03471302792851,7.59443891967696));
#407962=CARTESIAN_POINT('Ctrl Pts',(1.72340995736708,-2.02904566511006,
7.58783901202978));
#407963=CARTESIAN_POINT('Ctrl Pts',(1.73109004667147,-2.02542690755189,
7.58560008491213));
#407964=CARTESIAN_POINT('',(1.75029323173564,-2.1163295107988,7.50366116523517));
#407965=CARTESIAN_POINT('Ctrl Pts',(1.75029323173588,-2.11632951079908,
7.50366116523554));
#407966=CARTESIAN_POINT('Ctrl Pts',(1.74981871703963,-2.116920250437,7.50350835821027));
#407967=CARTESIAN_POINT('Ctrl Pts',(1.74936330376742,-2.11744784570104,
7.50345484956));
#407968=CARTESIAN_POINT('Ctrl Pts',(1.74891390668698,-2.11792837480991,
7.50349758195598));
#407969=CARTESIAN_POINT('Ctrl Pts',(1.74868333265656,-2.11817492187973,
7.50351950684424));
#407970=CARTESIAN_POINT('Ctrl Pts',(1.74843171059764,-2.11843346810347,
7.50357029184312));
#407971=CARTESIAN_POINT('Ctrl Pts',(1.74818222121564,-2.11867611166748,
7.50365515313923));
#407972=CARTESIAN_POINT('Ctrl Pts',(1.74779840551789,-2.119049395725,7.50378570417639));
#407973=CARTESIAN_POINT('Ctrl Pts',(1.74740861269544,-2.1193962493459,7.50400001621911));
#407974=CARTESIAN_POINT('Ctrl Pts',(1.74704100235903,-2.11968857580533,
7.50428903009634));
#407975=CARTESIAN_POINT('Ctrl Pts',(1.74700020043991,-2.1197210217933,7.50432110841318));
#407976=CARTESIAN_POINT('Ctrl Pts',(1.74695966296948,-2.11975282504801,
7.50435406373354));
#407977=CARTESIAN_POINT('Ctrl Pts',(1.74691942164772,-2.11978396847003,
7.50438785222352));
#407978=CARTESIAN_POINT('Ctrl Pts',(1.74667372903595,-2.11997411403089,
7.50459414719561));
#407979=CARTESIAN_POINT('Ctrl Pts',(1.74643484859307,-2.12014228251917,
7.50483629897752));
#407980=CARTESIAN_POINT('Ctrl Pts',(1.74621268932909,-2.12028310756562,
7.5050991045531));
#407981=CARTESIAN_POINT('Ctrl Pts',(1.74572258367896,-2.12059378176261,
7.50567888004914));
#407982=CARTESIAN_POINT('Ctrl Pts',(1.74529482357482,-2.12078406050335,
7.50637912803144));
#407983=CARTESIAN_POINT('Ctrl Pts',(1.74493416304265,-2.12088448585052,
7.50710440483569));
#407984=CARTESIAN_POINT('Ctrl Pts',(1.74484572192005,-2.12090911213937,
7.50728225710685));
#407985=CARTESIAN_POINT('Ctrl Pts',(1.74475959423717,-2.12092896612877,
7.50746498566954));
#407986=CARTESIAN_POINT('Ctrl Pts',(1.744677884071,-2.12094399030943,7.50764697238949));
#407987=CARTESIAN_POINT('Ctrl Pts',(1.74423863270496,-2.12102475616988,
7.50862528291182));
#407988=CARTESIAN_POINT('Ctrl Pts',(1.74388791488079,-2.12097735070584,
7.50965856837421));
#407989=CARTESIAN_POINT('Ctrl Pts',(1.74359952217746,-2.12086267149124,
7.51067959873202));
#407990=CARTESIAN_POINT('Ctrl Pts',(1.74344081930906,-2.12079956337479,
7.51124147302578));
#407991=CARTESIAN_POINT('Ctrl Pts',(1.74330111223522,-2.12071566358395,
7.51180065547253));
#407992=CARTESIAN_POINT('Ctrl Pts',(1.74317712839625,-2.12061863513827,
7.512351757165));
#407993=CARTESIAN_POINT('Ctrl Pts',(1.74274871484331,-2.1202833632069,7.51425603304535));
#407994=CARTESIAN_POINT('Ctrl Pts',(1.74246069049903,-2.11974658727156,
7.5162690050518));
#407995=CARTESIAN_POINT('Ctrl Pts',(1.74230085887296,-2.11906741666329,
7.51827788969243));
#407996=CARTESIAN_POINT('Ctrl Pts',(1.74229220848331,-2.11903065866651,
7.51838661432545));
#407997=CARTESIAN_POINT('Ctrl Pts',(1.7422839382929,-2.11899347478669,7.51849533314857));
#407998=CARTESIAN_POINT('Ctrl Pts',(1.74227604793057,-2.11895587165396,
7.51860402984325));
#407999=CARTESIAN_POINT('Ctrl Pts',(1.73334108832701,-2.0360810736146,7.57603338728985));
#408000=CARTESIAN_POINT('Ctrl Pts',(1.73900212579776,-2.06287528806226,
7.55196141284922));
#408001=CARTESIAN_POINT('Ctrl Pts',(1.74465255590614,-2.08962350828569,
7.52783573083105));
#408002=CARTESIAN_POINT('Ctrl Pts',(1.7502932317425,-2.11632951085758,7.50366116530176));
#408003=CARTESIAN_POINT('Origin',(5.98949470795639E-16,-7.03560129586911E-16,
7.49482233047033));
#408004=CARTESIAN_POINT('Origin',(1.80403047455415,-2.05897554547885,7.49482233047033));
#408005=CARTESIAN_POINT('Origin',(0.,0.,7.50366116523517));
#408006=CARTESIAN_POINT('Origin',(1.74466007661673,-2.10951830213907,7.49482233047033));
#408007=CARTESIAN_POINT('Ctrl Pts',(1.81372657476301,-2.0581279312074,7.51860402984325));
#408008=CARTESIAN_POINT('Ctrl Pts',(1.82082828860748,-2.06085958757331,
7.51860402984325));
#408009=CARTESIAN_POINT('Ctrl Pts',(1.82651648716082,-2.05580580846774,
7.51860402984325));
#408010=CARTESIAN_POINT('Ctrl Pts',(1.81636349003428,-2.05914221267183,
7.51041458714366));
#408011=CARTESIAN_POINT('Ctrl Pts',(1.82217588142129,-2.0596622820176,7.51004642900441));
#408012=CARTESIAN_POINT('Ctrl Pts',(1.82651805589845,-2.05580441469547,
7.5072913648301));
#408013=CARTESIAN_POINT('Ctrl Pts',(1.81632127355298,-2.06195680944011,
7.50215815450138));
#408014=CARTESIAN_POINT('Ctrl Pts',(1.81943214123463,-2.06210022055771,
7.49877163671531));
#408015=CARTESIAN_POINT('Ctrl Pts',(1.82202718038203,-2.05982652413606,
7.49481588533171));
#408016=CARTESIAN_POINT('Ctrl Pts',(1.80985496190503,-2.06562314771777,
7.50366171572174));
#408017=CARTESIAN_POINT('Ctrl Pts',(1.81226805662945,-2.06837726029865,
7.50000045605858));
#408018=CARTESIAN_POINT('Ctrl Pts',(1.81226805662954,-2.06837726029857,
7.49482233047317));
#408019=CARTESIAN_POINT('Origin',(1.81821413949191,-2.04646123661107,7.51860402984325));
#408020=CARTESIAN_POINT('Origin',(1.81821413949191,-2.04646123661107,9.));
#408021=CARTESIAN_POINT('Origin',(1.81821413949191,-2.04646123661107,8.75721825406948));
#408022=CARTESIAN_POINT('Ctrl Pts',(1.79814021121717,-2.05213415732287,
8.78942910404913));
#408023=CARTESIAN_POINT('Ctrl Pts',(1.80333407793184,-2.05415311181764,
8.79672699501691));
#408024=CARTESIAN_POINT('Ctrl Pts',(1.8080408387174,-2.04656892505244,8.79893251111267));
#408025=CARTESIAN_POINT('Ctrl Pts',(1.80840194814797,-2.05608031670936,
8.78111911759583));
#408026=CARTESIAN_POINT('Ctrl Pts',(1.81456203428848,-2.05846687256808,
8.78644465894813));
#408027=CARTESIAN_POINT('Ctrl Pts',(1.82021442763375,-2.05265602398582,
8.78817647674133));
#408028=CARTESIAN_POINT('Ctrl Pts',(1.8147973073802,-2.0585396573341,8.7678092393203));
#408029=CARTESIAN_POINT('Ctrl Pts',(1.82207086986224,-2.06135213410561,
8.76988516158373));
#408030=CARTESIAN_POINT('Ctrl Pts',(1.82782283886928,-2.05644792846776,
8.77093053738832));
#408031=CARTESIAN_POINT('Ctrl Pts',(1.81355029985717,-2.0580601195691,8.75371302330492));
#408032=CARTESIAN_POINT('Ctrl Pts',(1.82064507138233,-2.06080428034673,
8.75300828287559));
#408033=CARTESIAN_POINT('Ctrl Pts',(1.82633909376226,-2.05570794357694,
8.75267964240738));
#408034=CARTESIAN_POINT('Origin',(1.8051259398375,-2.0414281648459,8.78727029226991));
#408035=CARTESIAN_POINT('Ctrl Pts',(1.73391074180931,-2.02743472471359,
8.85049129520029));
#408036=CARTESIAN_POINT('Ctrl Pts',(1.73936124027705,-2.02953071581002,
8.85711686593484));
#408037=CARTESIAN_POINT('Ctrl Pts',(1.74416981443408,-2.0224611771624,8.85933012996512));
#408038=CARTESIAN_POINT('Ctrl Pts',(1.75618597738197,-2.03600067436163,
8.82945683644721));
#408039=CARTESIAN_POINT('Ctrl Pts',(1.76168171828244,-2.0381140634514,8.83607469902389));
#408040=CARTESIAN_POINT('Ctrl Pts',(1.76647340116635,-2.03100267697354,
8.8382956714852));
#408041=CARTESIAN_POINT('Ctrl Pts',(1.77842800991976,-2.04455385577097,
8.80838214965003));
#408042=CARTESIAN_POINT('Ctrl Pts',(1.78394543957975,-2.04667558528086,
8.81501364461993));
#408043=CARTESIAN_POINT('Ctrl Pts',(1.78874291541953,-2.03953184409282,
8.8172209842872));
#408044=CARTESIAN_POINT('Ctrl Pts',(1.80063936233261,-2.05309523912752,
8.78727029226991));
#408045=CARTESIAN_POINT('Ctrl Pts',(1.80615770845576,-2.05521732106363,
8.79393457792714));
#408046=CARTESIAN_POINT('Ctrl Pts',(1.81098095093023,-2.04804963334647,
8.79610912703474));
#408047=CARTESIAN_POINT('Origin',(1.7383973193142,-2.01576765043198,8.85049129520029));
#408048=CARTESIAN_POINT('Ctrl Pts',(1.72471465490916,-2.03526346763208,
8.85049129520029));
#408049=CARTESIAN_POINT('Ctrl Pts',(1.72591388015444,-2.04097862038893,
8.85711686593484));
#408050=CARTESIAN_POINT('Ctrl Pts',(1.71816751245364,-2.04459725957486,
8.85933012996512));
#408051=CARTESIAN_POINT('Ctrl Pts',(1.72365371764567,-2.0302073544872,8.86332496987231));
#408052=CARTESIAN_POINT('Ctrl Pts',(1.72032477139737,-2.03341204031464,
8.86648636486737));
#408053=CARTESIAN_POINT('Ctrl Pts',(1.71521626468802,-2.03044905852375,
8.87206031107457));
#408054=CARTESIAN_POINT('Ctrl Pts',(1.72905599763766,-2.02556783114055,
8.86341338519877));
#408055=CARTESIAN_POINT('Ctrl Pts',(1.732743554524,-2.0227615177503,8.86654584966058));
#408056=CARTESIAN_POINT('Ctrl Pts',(1.73057098474445,-2.01724752705931,
8.87215952290714));
#408057=CARTESIAN_POINT('Ctrl Pts',(1.73391074180931,-2.02743472471359,
8.85049129520029));
#408058=CARTESIAN_POINT('Ctrl Pts',(1.73936124027705,-2.02953071581002,
8.85711686593484));
#408059=CARTESIAN_POINT('Ctrl Pts',(1.74416981443408,-2.0224611771624,8.85933012996512));
#408060=CARTESIAN_POINT('Origin',(1.71248107441377,-2.03783047138408,8.85049129520029));
#408061=CARTESIAN_POINT('Ctrl Pts',(1.7393963664604,-2.10523216165202,8.78727029226991));
#408062=CARTESIAN_POINT('Ctrl Pts',(1.74061051962863,-2.11101845647362,
8.79393457792714));
#408063=CARTESIAN_POINT('Ctrl Pts',(1.7327649198924,-2.11463591137412,8.79610912703474));
#408064=CARTESIAN_POINT('Ctrl Pts',(1.7345093979193,-2.0819423152779,8.80838214965003));
#408065=CARTESIAN_POINT('Ctrl Pts',(1.73572334944618,-2.08772764913654,
8.81501364461988));
#408066=CARTESIAN_POINT('Ctrl Pts',(1.72790550163947,-2.09132348954823,
8.81722098428722));
#408067=CARTESIAN_POINT('Ctrl Pts',(1.72961567910012,-2.05862029907537,
8.82945683644722));
#408068=CARTESIAN_POINT('Ctrl Pts',(1.73082485863999,-2.06438289105554,
8.83607469902389));
#408069=CARTESIAN_POINT('Ctrl Pts',(1.72303987536893,-2.06797817657504,
8.83829567148518));
#408070=CARTESIAN_POINT('Ctrl Pts',(1.72471465490916,-2.03526346763208,
8.85049129520029));
#408071=CARTESIAN_POINT('Ctrl Pts',(1.72591388015444,-2.04097862038893,
8.85711686593484));
#408072=CARTESIAN_POINT('Ctrl Pts',(1.71816751245364,-2.04459725957486,
8.85933012996512));
#408073=CARTESIAN_POINT('Origin',(1.72716278596501,-2.10779916540403,8.78727029226991));
#408074=CARTESIAN_POINT('Ctrl Pts',(1.74223800513146,-2.11877466075527,
8.75374538247848));
#408075=CARTESIAN_POINT('Ctrl Pts',(1.74381137292058,-2.12620896584639,
8.75304829418602));
#408076=CARTESIAN_POINT('Ctrl Pts',(1.73788145903659,-2.13101591545477,
8.75272238421917));
#408077=CARTESIAN_POINT('Ctrl Pts',(1.74250907779356,-2.12006651079531,
8.76769408445017));
#408078=CARTESIAN_POINT('Ctrl Pts',(1.7441213633446,-2.12768803887529,8.76974318093967));
#408079=CARTESIAN_POINT('Ctrl Pts',(1.73837008844154,-2.13258101284513,
8.7707786988043));
#408080=CARTESIAN_POINT('Ctrl Pts',(1.74111971376202,-2.11344522340546,
8.78108014887993));
#408081=CARTESIAN_POINT('Ctrl Pts',(1.74248978482015,-2.11990340756171,
8.78639403366328));
#408082=CARTESIAN_POINT('Ctrl Pts',(1.73587245745552,-2.12456527996217,
8.78812224174742));
#408083=CARTESIAN_POINT('Ctrl Pts',(1.73884285278516,-2.10259439504486,
8.78944554828685));
#408084=CARTESIAN_POINT('Ctrl Pts',(1.74000297373834,-2.10803595153092,
8.79673892988685));
#408085=CARTESIAN_POINT('Ctrl Pts',(1.73177459439527,-2.11147067534851,
8.79894799272499));
#408086=CARTESIAN_POINT('Origin',(1.73004246743518,-2.12152287540597,8.75721825406948));
#408087=CARTESIAN_POINT('Origin',(1.73004246743518,-2.12152287540597,9.));
#408088=CARTESIAN_POINT('Origin',(1.73004246743518,-2.12152287540597,7.51860402984325));
#408089=CARTESIAN_POINT('Ctrl Pts',(1.75029273038004,-2.11632890459551,
7.50366195182966));
#408090=CARTESIAN_POINT('Ctrl Pts',(1.75262656098474,-2.1191508058019,7.50000065167735));
#408091=CARTESIAN_POINT('Ctrl Pts',(1.75262656098465,-2.11915080580197,
7.49482233047108));
#408092=CARTESIAN_POINT('Ctrl Pts',(1.74563652264445,-2.12213179431785,
7.50215800491337));
#408093=CARTESIAN_POINT('Ctrl Pts',(1.74528013450683,-2.12522657777872,
7.49877273257269));
#408094=CARTESIAN_POINT('Ctrl Pts',(1.74261994224621,-2.12742669902232,
7.49481816995647));
#408095=CARTESIAN_POINT('Ctrl Pts',(1.74285520534903,-2.1217143132473,7.51043025814041));
#408096=CARTESIAN_POINT('Ctrl Pts',(1.74244442792581,-2.1275387461721,7.51006209594511));
#408097=CARTESIAN_POINT('Ctrl Pts',(1.73794024257006,-2.13121179455772,
7.50731281821699));
#408098=CARTESIAN_POINT('Ctrl Pts',(1.74227573745806,-2.11895439247877,
7.51860402984325));
#408099=CARTESIAN_POINT('Ctrl Pts',(1.74383928023547,-2.12640129461145,
7.51860402984325));
#408100=CARTESIAN_POINT('Ctrl Pts',(1.7379422047294,-2.13121019447175,7.51860402984325));
#408101=CARTESIAN_POINT('Origin',(0.,0.,7.5));
#408102=CARTESIAN_POINT('Origin',(1.85157082176548,-1.92057895321252,7.5));
#408103=CARTESIAN_POINT('',(1.85157082176548,-1.92057895321252,7.59394543036555));
#408104=CARTESIAN_POINT('',(1.85157082176548,-1.92057895321252,8.85049129520029));
#408105=CARTESIAN_POINT('',(1.85157082176548,-1.92057895321252,7.5));
#408106=CARTESIAN_POINT('',(1.87070527778335,-1.98946322855769,8.78727029226991));
#408107=CARTESIAN_POINT('Ctrl Pts',(1.85157082176548,-1.92057895321252,
8.85049129520029));
#408108=CARTESIAN_POINT('Ctrl Pts',(1.85795824503307,-1.94357375498267,
8.82945686509571));
#408109=CARTESIAN_POINT('Ctrl Pts',(1.86433617262361,-1.9665343721995,8.80838212259895));
#408110=CARTESIAN_POINT('Ctrl Pts',(1.87070527778335,-1.98946322855769,
8.78727029226991));
#408111=CARTESIAN_POINT('',(1.87445832375787,-2.0029742399003,8.75721825406948));
#408112=CARTESIAN_POINT('Origin',(1.86316430091954,-1.96231486575488,8.75937679713047));
#408113=CARTESIAN_POINT('',(1.87445832375787,-2.0029742399003,7.51860402984325));
#408114=CARTESIAN_POINT('',(1.87445832375787,-2.0029742399003,7.5));
#408115=CARTESIAN_POINT('Ctrl Pts',(1.87445832375787,-2.0029742399003,7.51860402984325));
#408116=CARTESIAN_POINT('Ctrl Pts',(1.87151088985394,-1.99236344185042,
7.52834476460825));
#408117=CARTESIAN_POINT('Ctrl Pts',(1.86856154251846,-1.98174575542356,
7.53807742314407));
#408118=CARTESIAN_POINT('Ctrl Pts',(1.86561021750541,-1.97112094933329,
7.54780169004674));
#408119=CARTESIAN_POINT('Ctrl Pts',(1.86093547819024,-1.95429183070808,
7.5632044032688));
#408120=CARTESIAN_POINT('Ctrl Pts',(1.856255771193,-1.93744482836684,7.57858609112103));
#408121=CARTESIAN_POINT('Ctrl Pts',(1.85157082176548,-1.92057895321252,
7.59394543036555));
#408122=CARTESIAN_POINT('Origin',(2.12271872378388,-1.99423374133347,7.5));
#408123=CARTESIAN_POINT('',(1.94186579781668,-1.9376937416628,8.75721825406948));
#408124=CARTESIAN_POINT('',(1.92848201925699,-1.93350957471437,8.78727029226991));
#408125=CARTESIAN_POINT('Origin',(1.89450899737204,-1.92288859838283,8.75658640621046));
#408126=CARTESIAN_POINT('',(1.86024642503786,-1.91217709997533,8.85049129520029));
#408127=CARTESIAN_POINT('Ctrl Pts',(1.92848201925699,-1.93350957471437,
8.78727029226991));
#408128=CARTESIAN_POINT('Ctrl Pts',(1.90576908324183,-1.92640883587949,
8.80838212259896));
#408129=CARTESIAN_POINT('Ctrl Pts',(1.88302468545905,-1.919298261161,8.82945686509571));
#408130=CARTESIAN_POINT('Ctrl Pts',(1.86024642503786,-1.91217709997533,
8.85049129520029));
#408131=CARTESIAN_POINT('',(1.86024642503786,-1.91217709997533,7.59394543036555));
#408132=CARTESIAN_POINT('',(1.86024642503786,-1.91217709997533,7.5));
#408133=CARTESIAN_POINT('',(1.94186579781668,-1.9376937416628,7.51860402984325));
#408134=CARTESIAN_POINT('Ctrl Pts',(1.86024642503786,-1.91217709997533,
7.59394543036555));
#408135=CARTESIAN_POINT('Ctrl Pts',(1.87695347475877,-1.91740022025755,
7.57858609112103));
#408136=CARTESIAN_POINT('Ctrl Pts',(1.8936418293911,-1.92261749589947,7.56320440326857));
#408137=CARTESIAN_POINT('Ctrl Pts',(1.91031246871802,-1.9278292332104,7.54780169004651));
#408138=CARTESIAN_POINT('Ctrl Pts',(1.92083722133245,-1.93111958367706,
7.53807742314383));
#408139=CARTESIAN_POINT('Ctrl Pts',(1.93135492132934,-1.93440772928586,
7.52834476460825));
#408140=CARTESIAN_POINT('Ctrl Pts',(1.94186579781668,-1.93769374166279,
7.51860402984324));
#408141=CARTESIAN_POINT('',(1.94186579781668,-1.9376937416628,7.5));
#408142=CARTESIAN_POINT('Origin',(1.85819500900391,-1.91873890744398,7.5));
#408143=CARTESIAN_POINT('Ctrl Pts',(1.86024642503786,-1.91217709997533,
8.85049129520029));
#408144=CARTESIAN_POINT('Ctrl Pts',(1.86006158583555,-1.9121193137472,8.85097269580138));
#408145=CARTESIAN_POINT('Ctrl Pts',(1.8598765688591,-1.91207028482753,8.85143669361005));
#408146=CARTESIAN_POINT('Ctrl Pts',(1.85968263072174,-1.9120286007086,8.8519052845931));
#408147=CARTESIAN_POINT('Ctrl Pts',(1.85930330002419,-1.91194706921549,
8.85282181883899));
#408148=CARTESIAN_POINT('Ctrl Pts',(1.85889955648231,-1.91189592644373,
8.85372622499635));
#408149=CARTESIAN_POINT('Ctrl Pts',(1.85846312703678,-1.91188966638124,
8.8546225773507));
#408150=CARTESIAN_POINT('Ctrl Pts',(1.85810081881161,-1.91188446949969,
8.85536669723986));
#408151=CARTESIAN_POINT('Ctrl Pts',(1.85771590218179,-1.91191017178598,
8.85610498449051));
#408152=CARTESIAN_POINT('Ctrl Pts',(1.85730414434205,-1.9119830527008,8.85681338218371));
#408153=CARTESIAN_POINT('Ctrl Pts',(1.8569304734558,-1.91204919224547,8.85745625420285));
#408154=CARTESIAN_POINT('Ctrl Pts',(1.85652990561897,-1.91215442650102,
8.85808743050666));
#408155=CARTESIAN_POINT('Ctrl Pts',(1.85609705491235,-1.91232684172784,
8.85866804508411));
#408156=CARTESIAN_POINT('Ctrl Pts',(1.85589734697936,-1.91240639037599,
8.85893592806396));
#408157=CARTESIAN_POINT('Ctrl Pts',(1.85569075007651,-1.91250048161007,
8.85919241173848));
#408158=CARTESIAN_POINT('Ctrl Pts',(1.85547684726748,-1.91261346607838,
8.85943017985534));
#408159=CARTESIAN_POINT('Ctrl Pts',(1.85518801515329,-1.91276602855758,
8.8597512372));
#408160=CARTESIAN_POINT('Ctrl Pts',(1.85487880982735,-1.91295748856581,
8.86004599534706));
#408161=CARTESIAN_POINT('Ctrl Pts',(1.85455842928457,-1.91319440076879,
8.86026130871721));
#408162=CARTESIAN_POINT('Ctrl Pts',(1.85444112893538,-1.91328114100556,
8.86034014101236));
#408163=CARTESIAN_POINT('Ctrl Pts',(1.8543205612428,-1.9133752671255,8.86040910639693));
#408164=CARTESIAN_POINT('Ctrl Pts',(1.85420021800344,-1.91347447986182,
8.86046313645507));
#408165=CARTESIAN_POINT('Ctrl Pts',(1.8540124233863,-1.91362930050593,8.8605474499083));
#408166=CARTESIAN_POINT('Ctrl Pts',(1.85382014264965,-1.91380084733626,
8.86059655985668));
#408167=CARTESIAN_POINT('Ctrl Pts',(1.85363551231204,-1.91397789992958,
8.86059725258816));
#408168=CARTESIAN_POINT('Ctrl Pts',(1.85345045540458,-1.91415536158512,
8.86059794692011));
#408169=CARTESIAN_POINT('Ctrl Pts',(1.85327287084369,-1.91434224010241,
8.86056369958366));
#408170=CARTESIAN_POINT('Ctrl Pts',(1.85310971629741,-1.91452575082091,
8.86048590497774));
#408171=CARTESIAN_POINT('Ctrl Pts',(1.85306713781853,-1.91457364165467,
8.86046560290182));
#408172=CARTESIAN_POINT('Ctrl Pts',(1.85302505587403,-1.91462198633973,
8.86044257503091));
#408173=CARTESIAN_POINT('Ctrl Pts',(1.85298474607094,-1.9146692694329,8.86041778462584));
#408174=CARTESIAN_POINT('Ctrl Pts',(1.85271351111646,-1.91498742597651,
8.86025097596201));
#408175=CARTESIAN_POINT('Ctrl Pts',(1.85248636841559,-1.91530042537852,
8.8599848982295));
#408176=CARTESIAN_POINT('Ctrl Pts',(1.85230309052328,-1.91559415580071,
8.85968173251461));
#408177=CARTESIAN_POINT('Ctrl Pts',(1.85220614701882,-1.9157495223653,8.85952137522076));
#408178=CARTESIAN_POINT('Ctrl Pts',(1.85211944536219,-1.91590239156238,
8.85934740853961));
#408179=CARTESIAN_POINT('Ctrl Pts',(1.85204285603105,-1.91604984067722,
8.8591675900182));
#408180=CARTESIAN_POINT('Ctrl Pts',(1.85173531005616,-1.91664192551581,
8.85844552518695));
#408181=CARTESIAN_POINT('Ctrl Pts',(1.85157075220592,-1.91717868325238,
8.85759444184125));
#408182=CARTESIAN_POINT('Ctrl Pts',(1.85147589005126,-1.91762837806792,
8.85683498915139));
#408183=CARTESIAN_POINT('Ctrl Pts',(1.85146596297942,-1.91767543743273,
8.85675551444998));
#408184=CARTESIAN_POINT('Ctrl Pts',(1.85145681911714,-1.91772154358245,
8.85667699793651));
#408185=CARTESIAN_POINT('Ctrl Pts',(1.8514483875945,-1.91776665961245,8.85659965593547));
#408186=CARTESIAN_POINT('Ctrl Pts',(1.85133457847175,-1.91837563808756,
8.85555568965886));
#408187=CARTESIAN_POINT('Ctrl Pts',(1.85131314939549,-1.91897734042079,
8.85434650606346));
#408188=CARTESIAN_POINT('Ctrl Pts',(1.85137778363236,-1.91957451989692,
8.85297329937117));
#408189=CARTESIAN_POINT('Ctrl Pts',(1.85141413645238,-1.91991039696556,
8.85220095427747));
#408190=CARTESIAN_POINT('Ctrl Pts',(1.85147804246511,-1.92024494659809,
8.85137579139183));
#408191=CARTESIAN_POINT('Ctrl Pts',(1.85157082176548,-1.92057895321252,
8.85049129520029));
#408192=CARTESIAN_POINT('Origin',(1.85819500900391,-1.91873890744398,7.59394543036555));
#408193=CARTESIAN_POINT('Ctrl Pts',(1.85970977447863,-1.91200932706107,
7.59443877723642));
#408194=CARTESIAN_POINT('Ctrl Pts',(1.85418279006983,-1.91028142747093,
7.58783886950016));
#408195=CARTESIAN_POINT('Ctrl Pts',(1.84984328894465,-1.91757854412898,
7.58559994247159));
#408196=CARTESIAN_POINT('Ctrl Pts',(1.88988142021141,-1.92144188022918,
7.56670252222134));
#408197=CARTESIAN_POINT('Ctrl Pts',(1.88436242386425,-1.9197164779445,7.56004874999027));
#408198=CARTESIAN_POINT('Ctrl Pts',(1.87997884594833,-1.92704591188663,
7.55786368756704));
#408199=CARTESIAN_POINT('Ctrl Pts',(1.91999672341034,-1.9308568190467,7.53888913333558));
#408200=CARTESIAN_POINT('Ctrl Pts',(1.91444492739765,-1.92912116261176,
7.53222002137278));
#408201=CARTESIAN_POINT('Ctrl Pts',(1.9100595450782,-1.93649482293976,7.53005029815326));
#408202=CARTESIAN_POINT('Ctrl Pts',(1.95005432133752,-1.94025371748124,
7.51101258149734));
#408203=CARTESIAN_POINT('Ctrl Pts',(1.94443522746928,-1.93849702173656,
7.5043616886572));
#408204=CARTESIAN_POINT('Ctrl Pts',(1.94008387535393,-1.94592488928472,
7.50217374673251));
#408205=CARTESIAN_POINT('',(1.93848173883016,-1.9454216878506,7.50366116523517));
#408206=CARTESIAN_POINT('Ctrl Pts',(1.94186579781668,-1.93769374166279,
7.51860402984325));
#408207=CARTESIAN_POINT('Ctrl Pts',(1.94228729131094,-1.93782551305604,
7.51734760759494));
#408208=CARTESIAN_POINT('Ctrl Pts',(1.94265041783264,-1.93800137376573,
7.51608817408573));
#408209=CARTESIAN_POINT('Ctrl Pts',(1.94294852171252,-1.93823293770863,
7.5148100591312));
#408210=CARTESIAN_POINT('Ctrl Pts',(1.94321855133035,-1.93844269386152,
7.51365231206384));
#408211=CARTESIAN_POINT('Ctrl Pts',(1.94343576286587,-1.93869825356333,
7.51247773061043));
#408212=CARTESIAN_POINT('Ctrl Pts',(1.94356826237055,-1.93901910824856,
7.51129758471022));
#408213=CARTESIAN_POINT('Ctrl Pts',(1.94373294412285,-1.93941789397931,
7.50983079813402));
#408214=CARTESIAN_POINT('Ctrl Pts',(1.94374947141059,-1.93990978941467,
7.50839324291155));
#408215=CARTESIAN_POINT('Ctrl Pts',(1.94353557175022,-1.94050115292895,
7.50715379678855));
#408216=CARTESIAN_POINT('Ctrl Pts',(1.94343675627051,-1.94077434583282,
7.50658120839351));
#408217=CARTESIAN_POINT('Ctrl Pts',(1.94326578097651,-1.94110437188969,
7.50598221009429));
#408218=CARTESIAN_POINT('Ctrl Pts',(1.94300651780458,-1.94147291354816,
7.50545747549611));
#408219=CARTESIAN_POINT('Ctrl Pts',(1.9428681669511,-1.94166957878455,7.50517746087247));
#408220=CARTESIAN_POINT('Ctrl Pts',(1.94270334047091,-1.94187946086699,
7.50491486231392));
#408221=CARTESIAN_POINT('Ctrl Pts',(1.94251509140964,-1.94209597154046,
7.50468370960992));
#408222=CARTESIAN_POINT('Ctrl Pts',(1.94223359968323,-1.94241972329172,
7.50433806340447));
#408223=CARTESIAN_POINT('Ctrl Pts',(1.94189087484744,-1.94276763919195,
7.50405484070984));
#408224=CARTESIAN_POINT('Ctrl Pts',(1.9415094884218,-1.94311578500609,7.50385766036131));
#408225=CARTESIAN_POINT('Ctrl Pts',(1.94146870507166,-1.94315301378951,
7.50383657498791));
#408226=CARTESIAN_POINT('Ctrl Pts',(1.94142750738743,-1.94319023939013,
7.50381643264937));
#408227=CARTESIAN_POINT('Ctrl Pts',(1.94138594320287,-1.94322742863343,
7.50379723213559));
#408228=CARTESIAN_POINT('Ctrl Pts',(1.94110848867435,-1.94347567899792,
7.50366906242519));
#408229=CARTESIAN_POINT('Ctrl Pts',(1.94080818815368,-1.94372717343727,
7.50358235568538));
#408230=CARTESIAN_POINT('Ctrl Pts',(1.94051290838089,-1.94396262527654,
7.5035341175365));
#408231=CARTESIAN_POINT('Ctrl Pts',(1.9400701697808,-1.94431565866151,7.50346178989176));
#408232=CARTESIAN_POINT('Ctrl Pts',(1.93957887322525,-1.94467661751401,
7.50346967198527));
#408233=CARTESIAN_POINT('Ctrl Pts',(1.93908566887044,-1.94501612685798,
7.50354272648692));
#408234=CARTESIAN_POINT('Ctrl Pts',(1.93888280371058,-1.94515577407859,
7.50357277531559));
#408235=CARTESIAN_POINT('Ctrl Pts',(1.93867996572295,-1.94529172362374,
7.50361331098761));
#408236=CARTESIAN_POINT('Ctrl Pts',(1.93848173883116,-1.9454216878516,7.50366116523658));
#408237=CARTESIAN_POINT('',(1.86023191546278,-1.92084218059617,7.57603338622103));
#408238=CARTESIAN_POINT('Origin',(1.8663775697776,-1.92719217450502,7.58486873427627));
#408239=CARTESIAN_POINT('Ctrl Pts',(1.93848173888624,-1.9454216878626,7.50366116529968));
#408240=CARTESIAN_POINT('Ctrl Pts',(1.91244077647096,-1.93724268576655,
7.52783573079709));
#408241=CARTESIAN_POINT('Ctrl Pts',(1.88635872817014,-1.92904992062092,
7.55196141284068));
#408242=CARTESIAN_POINT('Ctrl Pts',(1.86023191671463,-1.92084218061873,
7.57603338728831));
#408243=CARTESIAN_POINT('Ctrl Pts',(1.8611755226901,-1.91265177151731,7.59639677331372));
#408244=CARTESIAN_POINT('Ctrl Pts',(1.84481208014828,-1.9045086969183,7.59959882295463));
#408245=CARTESIAN_POINT('Ctrl Pts',(1.85194244145045,-1.92135704284004,
7.59642833564546));
#408246=CARTESIAN_POINT('Ctrl Pts',(1.85800812538024,-1.91037521746235,
7.58707626057423));
#408247=CARTESIAN_POINT('Ctrl Pts',(1.85132774352081,-1.9115087029048,7.58809943920598));
#408248=CARTESIAN_POINT('Ctrl Pts',(1.84987780277126,-1.91811264662167,
7.58710240504252));
#408249=CARTESIAN_POINT('Ctrl Pts',(1.85891234067499,-1.91638421296595,
7.5801537675693));
#408250=CARTESIAN_POINT('Ctrl Pts',(1.85606317263307,-1.91649151098492,
7.5820588065976));
#408251=CARTESIAN_POINT('Ctrl Pts',(1.85582498577148,-1.91929692397712,
7.58020924244128));
#408252=CARTESIAN_POINT('Ctrl Pts',(1.86023191488719,-1.92084218000155,
7.57603338509286));
#408253=CARTESIAN_POINT('Ctrl Pts',(1.86023191488719,-1.92084218000155,
7.57603338509286));
#408254=CARTESIAN_POINT('Ctrl Pts',(1.86023191488719,-1.92084218000155,
7.57603338509286));
#408255=CARTESIAN_POINT('Origin',(1.86638166893217,-1.9271882046956,7.58486873427621));
#408256=CARTESIAN_POINT('Ctrl Pts',(1.87676178653315,-2.0112667340225,7.51098857897448));
#408257=CARTESIAN_POINT('Ctrl Pts',(1.87518608698743,-2.00559419641456,
7.50433767179956));
#408258=CARTESIAN_POINT('Ctrl Pts',(1.88274964256493,-2.0014831529815,7.50214974420965));
#408259=CARTESIAN_POINT('Ctrl Pts',(1.86833068520011,-1.98091466625817,
7.53887321589171));
#408260=CARTESIAN_POINT('Ctrl Pts',(1.86677386533131,-1.97531009571771,
7.53220407452065));
#408261=CARTESIAN_POINT('Ctrl Pts',(1.87428431468889,-1.97116328123316,
7.53003438070911));
#408262=CARTESIAN_POINT('Ctrl Pts',(1.85988339304239,-1.95050431132724,
7.56669465659232));
#408263=CARTESIAN_POINT('Ctrl Pts',(1.85833577368955,-1.94493286275669,
7.56004085833297));
#408264=CARTESIAN_POINT('Ctrl Pts',(1.86580194876566,-1.94078643298402,
7.55785582193789));
#408265=CARTESIAN_POINT('Ctrl Pts',(1.85142029209724,-1.92003704456848,
7.59443891967696));
#408266=CARTESIAN_POINT('Ctrl Pts',(1.84987042888904,-1.91445751809117,
7.58783901202978));
#408267=CARTESIAN_POINT('Ctrl Pts',(1.85730288403347,-1.9103541306473,7.58560008491213));
#408268=CARTESIAN_POINT('',(1.88229076388123,-1.99983961245518,7.50366116523517));
#408269=CARTESIAN_POINT('Ctrl Pts',(1.88229076388149,-1.99983961245545,
7.50366116523554));
#408270=CARTESIAN_POINT('Ctrl Pts',(1.88185507294513,-2.0004595406164,7.50350835821027));
#408271=CARTESIAN_POINT('Ctrl Pts',(1.88143439851296,-2.00101523030791,
7.50345484956));
#408272=CARTESIAN_POINT('Ctrl Pts',(1.88101671237273,-2.001523565088,7.50349758195598));
#408273=CARTESIAN_POINT('Ctrl Pts',(1.88080240840638,-2.00178437852927,
7.50351950684424));
#408274=CARTESIAN_POINT('Ctrl Pts',(1.8805678684454,-2.00205851502273,7.50357029184312));
#408275=CARTESIAN_POINT('Ctrl Pts',(1.88033443789261,-2.0023166448891,7.50365515313923));
#408276=CARTESIAN_POINT('Ctrl Pts',(1.87997532717706,-2.00271375315068,
7.50378570417639));
#408277=CARTESIAN_POINT('Ctrl Pts',(1.87960855821356,-2.00308486823549,
7.50400001621911));
#408278=CARTESIAN_POINT('Ctrl Pts',(1.87926043259258,-2.00340014695398,
7.50428903009634));
#408279=CARTESIAN_POINT('Ctrl Pts',(1.87922179332696,-2.00343514046613,
7.50432110841318));
#408280=CARTESIAN_POINT('Ctrl Pts',(1.87918337678663,-2.00346947562229,
7.50435406373354));
#408281=CARTESIAN_POINT('Ctrl Pts',(1.87914521351089,-2.00350313332715,
7.50438785222352));
#408282=CARTESIAN_POINT('Ctrl Pts',(1.87891220836886,-2.00370862979324,
7.50459414719561));
#408283=CARTESIAN_POINT('Ctrl Pts',(1.8786845933235,-2.00389175788385,7.50483629897752));
#408284=CARTESIAN_POINT('Ctrl Pts',(1.87847191320126,-2.00404652738305,
7.5050991045531));
#408285=CARTESIAN_POINT('Ctrl Pts',(1.8780027194899,-2.0043879644434,7.50567888004914));
#408286=CARTESIAN_POINT('Ctrl Pts',(1.87758802946555,-2.00460525892003,
7.50637912803145));
#408287=CARTESIAN_POINT('Ctrl Pts',(1.87723454422321,-2.00472858553219,
7.50710440483569));
#408288=CARTESIAN_POINT('Ctrl Pts',(1.87714786262412,-2.00475882766586,
7.50728225710685));
#408289=CARTESIAN_POINT('Ctrl Pts',(1.87706318394926,-2.00478415908271,
7.50746498566954));
#408290=CARTESIAN_POINT('Ctrl Pts',(1.87698260426796,-2.0048043875829,7.50764697238949));
#408291=CARTESIAN_POINT('Ctrl Pts',(1.87654943007741,-2.00491313043287,
7.50862528291181));
#408292=CARTESIAN_POINT('Ctrl Pts',(1.87619639556211,-2.00488829293659,
7.5096585683742));
#408293=CARTESIAN_POINT('Ctrl Pts',(1.87590124787002,-2.00479232672667,
7.510679598732));
#408294=CARTESIAN_POINT('Ctrl Pts',(1.87573882772278,-2.00473951640031,
7.51124147302577));
#408295=CARTESIAN_POINT('Ctrl Pts',(1.87559403221404,-2.00466474005354,
7.51180065547252));
#408296=CARTESIAN_POINT('Ctrl Pts',(1.87546408647931,-2.00457585463505,
7.51235175716501));
#408297=CARTESIAN_POINT('Ctrl Pts',(1.87501507220157,-2.0042687201064,7.51425603304536));
#408298=CARTESIAN_POINT('Ctrl Pts',(1.87469324828193,-2.00375150081788,
7.51626900505181));
#408299=CARTESIAN_POINT('Ctrl Pts',(1.8744902304368,-2.0030839660859,7.51827788969245));
#408300=CARTESIAN_POINT('Ctrl Pts',(1.87447924272737,-2.00304783784474,
7.51838661432546));
#408301=CARTESIAN_POINT('Ctrl Pts',(1.87446860714959,-2.00301126023611,
7.51849533314857));
#408302=CARTESIAN_POINT('Ctrl Pts',(1.87445832375787,-2.00297423990031,
7.51860402984325));
#408303=CARTESIAN_POINT('Ctrl Pts',(1.86023191544585,-1.92084218184913,
7.57603338728984));
#408304=CARTESIAN_POINT('Ctrl Pts',(1.86759803292184,-1.94721864079347,
7.55196141284921));
#408305=CARTESIAN_POINT('Ctrl Pts',(1.87495061796935,-1.97354987962968,
7.52783573083105));
#408306=CARTESIAN_POINT('Ctrl Pts',(1.88229076389185,-1.9998396125134,7.50366116530176));
#408307=CARTESIAN_POINT('Origin',(6.42796117143052E-16,-6.6373976549288E-16,
7.49482233047033));
#408308=CARTESIAN_POINT('Origin',(1.93224291659625,-1.93916053003964,7.49482233047033));
#408309=CARTESIAN_POINT('Origin',(0.,0.,7.50366116523517));
#408310=CARTESIAN_POINT('Origin',(1.87623278704651,-1.9934033156418,7.49482233047033));
#408311=CARTESIAN_POINT('Ctrl Pts',(1.9418647882945,-1.93769342600927,7.51860402984325));
#408312=CARTESIAN_POINT('Ctrl Pts',(1.9491269287305,-1.93996446152595,7.51860402984325));
#408313=CARTESIAN_POINT('Ctrl Pts',(1.95447964353083,-1.93455662181897,
7.51860402984325));
#408314=CARTESIAN_POINT('Ctrl Pts',(1.9445612709771,-1.93853667578216,7.51041458714365));
#408315=CARTESIAN_POINT('Ctrl Pts',(1.95039504114,-1.93868327539489,7.51004642900441));
#408316=CARTESIAN_POINT('Ctrl Pts',(1.95448111974601,-1.93455513040099,
7.50729136483009));
#408317=CARTESIAN_POINT('Ctrl Pts',(1.94469947306817,-1.94134819447875,
7.50215815450138));
#408318=CARTESIAN_POINT('Ctrl Pts',(1.9478131375204,-1.94129199696614,7.49877163671531));
#408319=CARTESIAN_POINT('Ctrl Pts',(1.95025716865164,-1.9388567073686,7.49481588533172));
#408320=CARTESIAN_POINT('Ctrl Pts',(1.93848135025099,-1.94542129788096,
7.50366171572174));
#408321=CARTESIAN_POINT('Ctrl Pts',(1.9410659436124,-1.94801514433233,7.50000045605858));
#408322=CARTESIAN_POINT('Ctrl Pts',(1.94106594361249,-1.94801514433224,
7.49482233047317));
#408323=CARTESIAN_POINT('Origin',(1.94559564515114,-1.92576318262889,7.51860402984325));
#408324=CARTESIAN_POINT('Origin',(1.94559564515114,-1.92576318262889,9.));
#408325=CARTESIAN_POINT('Origin',(1.94559564515114,-1.92576318262889,8.75721825406948));
#408326=CARTESIAN_POINT('Ctrl Pts',(1.9259264261929,-1.9327105887171,8.78942910404912));
#408327=CARTESIAN_POINT('Ctrl Pts',(1.93123897640997,-1.93439262287037,
8.79672699501691));
#408328=CARTESIAN_POINT('Ctrl Pts',(1.93545014613629,-1.92652245543134,
8.79893251111267));
#408329=CARTESIAN_POINT('Ctrl Pts',(1.93641991058458,-1.93599116855337,
8.78111911759582));
#408330=CARTESIAN_POINT('Ctrl Pts',(1.94272024732633,-1.93797814290299,
8.78644465894813));
#408331=CARTESIAN_POINT('Ctrl Pts',(1.94798872487631,-1.93181708324732,
8.78817647674132));
#408332=CARTESIAN_POINT('Ctrl Pts',(1.94295970036019,-1.93803570412616,
8.76780923932029));
#408333=CARTESIAN_POINT('Ctrl Pts',(1.95039851453346,-1.94037638361425,
8.76988516158373));
#408334=CARTESIAN_POINT('Ctrl Pts',(1.95582445196924,-1.93511372427326,
8.77093053738833));
#408335=CARTESIAN_POINT('Ctrl Pts',(1.94168453085778,-1.93763704766925,
8.75371302330492));
#408336=CARTESIAN_POINT('Ctrl Pts',(1.94894054439862,-1.93992100670192,
8.75300828287559));
#408337=CARTESIAN_POINT('Ctrl Pts',(1.95429634438096,-1.93447032363614,
8.75267964240738));
#408338=CARTESIAN_POINT('Origin',(1.93221186659145,-1.92157901568046,8.78727029226991));
#408339=CARTESIAN_POINT('Ctrl Pts',(1.86024642503786,-1.91217709997533,
8.85049129520029));
#408340=CARTESIAN_POINT('Ctrl Pts',(1.86582001548255,-1.91391956999743,
8.85711686593484));
#408341=CARTESIAN_POINT('Ctrl Pts',(1.87016576301195,-1.90655647007113,
8.85933012996512));
#408342=CARTESIAN_POINT('Ctrl Pts',(1.88302471602833,-1.91929827071787,
8.82945683644723));
#408343=CARTESIAN_POINT('Ctrl Pts',(1.88864457064357,-1.92105520429467,
8.83607469902389));
#408344=CARTESIAN_POINT('Ctrl Pts',(1.89297078040509,-1.91365142474655,
8.8382956714852));
#408345=CARTESIAN_POINT('Ctrl Pts',(1.90576905413923,-1.92640882678116,
8.80838214965003));
#408346=CARTESIAN_POINT('Ctrl Pts',(1.91141108732463,-1.92817269403816,
8.81501364461988));
#408347=CARTESIAN_POINT('Ctrl Pts',(1.91574100516642,-1.92073625510015,
8.81722098428721));
#408348=CARTESIAN_POINT('Ctrl Pts',(1.92848201925699,-1.93350957471437,
8.78727029226991));
#408349=CARTESIAN_POINT('Ctrl Pts',(1.93412498960265,-1.93527373495551,
8.79393457792714));
#408350=CARTESIAN_POINT('Ctrl Pts',(1.93847908687937,-1.92781174781514,
8.79610912703474));
#408351=CARTESIAN_POINT('Origin',(1.86397627237232,-1.90024654094142,8.85049129520029));
#408352=CARTESIAN_POINT('Ctrl Pts',(1.85157082176548,-1.92057895321252,
8.85049129520029));
#408353=CARTESIAN_POINT('Ctrl Pts',(1.85313375416823,-1.92620552894981,
8.85711686593484));
#408354=CARTESIAN_POINT('Ctrl Pts',(1.84563514921934,-1.93031304473608,
8.85933012996512));
#408355=CARTESIAN_POINT('Ctrl Pts',(1.85018811802994,-1.91560120287821,
8.86332496987231));
#408356=CARTESIAN_POINT('Ctrl Pts',(1.84707133638469,-1.91901259065336,
8.86648636486738));
#408357=CARTESIAN_POINT('Ctrl Pts',(1.8417834867551,-1.91638299977497,8.87206031107458));
#408358=CARTESIAN_POINT('Ctrl Pts',(1.85528204317687,-1.91062508666239,
8.86341338519876));
#408359=CARTESIAN_POINT('Ctrl Pts',(1.85878222246585,-1.90758827656308,
8.86654584966059));
#408360=CARTESIAN_POINT('Ctrl Pts',(1.85626083386738,-1.90222481198104,
8.87215952290713));
#408361=CARTESIAN_POINT('Ctrl Pts',(1.86024642503786,-1.91217709997533,
8.85049129520029));
#408362=CARTESIAN_POINT('Ctrl Pts',(1.86582001548255,-1.91391956999743,
8.85711686593484));
#408363=CARTESIAN_POINT('Ctrl Pts',(1.87016576301195,-1.90655647007113,
8.85933012996512));
#408364=CARTESIAN_POINT('Origin',(1.83952684496835,-1.92392449097349,8.85049129520029));
#408365=CARTESIAN_POINT('Ctrl Pts',(1.87070527778335,-1.98946322855769,
8.78727029226991));
#408366=CARTESIAN_POINT('Ctrl Pts',(1.87228766552577,-1.99515984375543,
8.79393457792714));
#408367=CARTESIAN_POINT('Ctrl Pts',(1.86468995654688,-1.99927253550784,
8.79610912703474));
#408368=CARTESIAN_POINT('Ctrl Pts',(1.86433616446273,-1.96653434282024,
8.80838214965002));
#408369=CARTESIAN_POINT('Ctrl Pts',(1.865918289409,-1.97223001194861,8.81501364461986));
#408370=CARTESIAN_POINT('Ctrl Pts',(1.85834689049528,-1.97631935554928,
8.81722098428721));
#408371=CARTESIAN_POINT('Ctrl Pts',(1.85795825360523,-1.94357378584256,
8.82945683644723));
#408372=CARTESIAN_POINT('Ctrl Pts',(1.85953415929191,-1.94924706556034,
8.83607469902388));
#408373=CARTESIAN_POINT('Ctrl Pts',(1.851995521838,-1.95333374977088,8.8382956714852));
#408374=CARTESIAN_POINT('Ctrl Pts',(1.85157082176548,-1.92057895321252,
8.85049129520029));
#408375=CARTESIAN_POINT('Ctrl Pts',(1.85313375416823,-1.92620552894981,
8.85711686593484));
#408376=CARTESIAN_POINT('Ctrl Pts',(1.84563514921934,-1.93031304473608,
8.85933012996512));
#408377=CARTESIAN_POINT('Origin',(1.85866130098622,-1.99280876631867,8.78727029226991));
#408378=CARTESIAN_POINT('Ctrl Pts',(1.87440874889962,-2.00279583872934,
8.75374538247847));
#408379=CARTESIAN_POINT('Ctrl Pts',(1.87645520159847,-2.01011406322296,
8.75304829418601));
#408380=CARTESIAN_POINT('Ctrl Pts',(1.87084545367739,-2.01529106732485,
8.75272238421917));
#408381=CARTESIAN_POINT('Ctrl Pts',(1.87476203373011,-2.00406766683984,
8.76769408445023));
#408382=CARTESIAN_POINT('Ctrl Pts',(1.87685931964825,-2.01157023618304,
8.76974318093971));
#408383=CARTESIAN_POINT('Ctrl Pts',(1.87143335527491,-2.0168216424613,8.7707786988043));
#408384=CARTESIAN_POINT('Ctrl Pts',(1.87295129695636,-1.99754900045418,
8.78108014887986));
#408385=CARTESIAN_POINT('Ctrl Pts',(1.87473233033614,-2.00390613482436,
8.78639403366322));
#408386=CARTESIAN_POINT('Ctrl Pts',(1.86842728617051,-2.00898240252794,
8.78812224174741));
#408387=CARTESIAN_POINT('Ctrl Pts',(1.86998389907454,-1.98686634526786,
8.78944554828686));
#408388=CARTESIAN_POINT('Ctrl Pts',(1.8714902781559,-1.99222239228784,8.79673892988687));
#408389=CARTESIAN_POINT('Ctrl Pts',(1.86349886841125,-1.99617725317157,
8.79894799272499));
#408390=CARTESIAN_POINT('Origin',(1.86241434696074,-2.00631977766128,8.75721825406948));
#408391=CARTESIAN_POINT('Origin',(1.86241434696074,-2.00631977766128,9.));
#408392=CARTESIAN_POINT('Origin',(1.86241434696074,-2.00631977766128,7.51860402984325));
#408393=CARTESIAN_POINT('Ctrl Pts',(1.88229022471614,-1.99983903961936,
7.50366195182966));
#408394=CARTESIAN_POINT('Ctrl Pts',(1.88480006004662,-2.00250561388683,
7.50000065167735));
#408395=CARTESIAN_POINT('Ctrl Pts',(1.88480006004653,-2.00250561388691,
7.49482233047108));
#408396=CARTESIAN_POINT('Ctrl Pts',(1.87801537607976,-2.00592833093631,
7.50215800491337));
#408397=CARTESIAN_POINT('Ctrl Pts',(1.87785800363692,-2.00903958969902,
7.49877273257263));
#408398=CARTESIAN_POINT('Ctrl Pts',(1.87534423927866,-2.01140562966089,
7.49481816995647));
#408399=CARTESIAN_POINT('Ctrl Pts',(1.87521302519499,-2.00568990723634,
7.51043025814042));
#408400=CARTESIAN_POINT('Ctrl Pts',(1.87517626445681,-2.0115286918389,7.51006209594516));
#408401=CARTESIAN_POINT('Ctrl Pts',(1.870916666451,-2.01548277769926,7.50731281821699));
#408402=CARTESIAN_POINT('Ctrl Pts',(1.87445791915217,-2.00297278365627,
7.51860402984325));
#408403=CARTESIAN_POINT('Ctrl Pts',(1.87649537412108,-2.01030420880015,
7.51860402984324));
#408404=CARTESIAN_POINT('Ctrl Pts',(1.87091852206101,-2.01548105518485,
7.51860402984325));
#408405=CARTESIAN_POINT('Origin',(0.,0.,7.5));
#408406=CARTESIAN_POINT('Origin',(1.97081848695447,-1.79800236791131,7.5));
#408407=CARTESIAN_POINT('',(1.97081848695447,-1.79800236791131,7.59394543036555));
#408408=CARTESIAN_POINT('',(1.97081848695447,-1.79800236791131,8.85049129520029));
#408409=CARTESIAN_POINT('',(1.97081848695447,-1.79800236791131,7.5));
#408410=CARTESIAN_POINT('',(1.99432705985486,-1.8655191643187,8.78727029226991));
#408411=CARTESIAN_POINT('Ctrl Pts',(1.97081848695447,-1.79800236791131,
8.85049129520029));
#408412=CARTESIAN_POINT('Ctrl Pts',(1.97866606858373,-1.82054068078118,
8.82945686509571));
#408413=CARTESIAN_POINT('Ctrl Pts',(1.98650198383398,-1.84304548772368,
8.80838212259895));
#408414=CARTESIAN_POINT('Ctrl Pts',(1.99432705985486,-1.8655191643187,8.78727029226991));
#408415=CARTESIAN_POINT('',(1.9989380482628,-1.87876195735827,8.75721825406948));
#408416=CARTESIAN_POINT('Origin',(1.98506217516105,-1.83890973278876,8.75937679713163));
#408417=CARTESIAN_POINT('',(1.9989380482628,-1.87876195735827,7.51860402984325));
#408418=CARTESIAN_POINT('',(1.9989380482628,-1.87876195735827,7.5));
#408419=CARTESIAN_POINT('Ctrl Pts',(1.9989380482628,-1.87876195735827,7.51860402984325));
#408420=CARTESIAN_POINT('Ctrl Pts',(1.99531683401271,-1.86836180306959,
7.52834476460825));
#408421=CARTESIAN_POINT('Ctrl Pts',(1.99169326892259,-1.85795489715082,
7.53807742314407));
#408422=CARTESIAN_POINT('Ctrl Pts',(1.98806727405985,-1.84754101290699,
7.54780169004674));
#408423=CARTESIAN_POINT('Ctrl Pts',(1.98232389416557,-1.83104598308719,
7.5632044032688));
#408424=CARTESIAN_POINT('Ctrl Pts',(1.97657441098223,-1.81453342457585,
7.57858609112103));
#408425=CARTESIAN_POINT('Ctrl Pts',(1.97081848695447,-1.79800236791131,
7.59394543036555));
#408426=CARTESIAN_POINT('Origin',(2.24612836500519,-1.85413331864099,7.5));
#408427=CARTESIAN_POINT('',(2.0620244905542,-1.80929677321441,8.75721825406948));
#408428=CARTESIAN_POINT('',(2.04840012990614,-1.80597870472223,8.78727029226991));
#408429=CARTESIAN_POINT('Origin',(2.01381642095027,-1.79755620931172,8.75658640621115));
#408430=CARTESIAN_POINT('',(1.97893795668432,-1.78906192937257,8.85049129520029));
#408431=CARTESIAN_POINT('Ctrl Pts',(2.04840012990614,-1.80597870472223,
8.78727029226991));
#408432=CARTESIAN_POINT('Ctrl Pts',(2.02527891415481,-1.80034777792373,
8.80838212259896));
#408433=CARTESIAN_POINT('Ctrl Pts',(2.0021256710902,-1.79470905121288,8.82945686509571));
#408434=CARTESIAN_POINT('Ctrl Pts',(1.97893795668432,-1.78906192937257,
8.85049129520029));
#408435=CARTESIAN_POINT('',(1.97893795668432,-1.78906192937257,7.59394543036555));
#408436=CARTESIAN_POINT('',(1.97893795668432,-1.78906192937257,7.5));
#408437=CARTESIAN_POINT('',(2.0620244905542,-1.80929677321441,7.51860402984325));
#408438=CARTESIAN_POINT('Ctrl Pts',(1.97893795668431,-1.78906192937257,
7.59394543036555));
#408439=CARTESIAN_POINT('Ctrl Pts',(1.99594532644522,-1.79320389384314,
7.57858609112103));
#408440=CARTESIAN_POINT('Ctrl Pts',(2.01293366506122,-1.7973412234803,7.56320440326857));
#408441=CARTESIAN_POINT('Ctrl Pts',(2.02990396992771,-1.80147416118906,
7.54780169004651));
#408442=CARTESIAN_POINT('Ctrl Pts',(2.04061791178733,-1.80408342806256,
7.53807742314383));
#408443=CARTESIAN_POINT('Ctrl Pts',(2.05132467425404,-1.80669094647106,
7.52834476460825));
#408444=CARTESIAN_POINT('Ctrl Pts',(2.0620244905542,-1.80929677321441,7.51860402984325));
#408445=CARTESIAN_POINT('',(2.0620244905542,-1.80929677321441,7.5));
#408446=CARTESIAN_POINT('Origin',(1.97731117195261,-1.79574168958059,7.5));
#408447=CARTESIAN_POINT('Ctrl Pts',(1.97893795668432,-1.78906192937257,
8.85049129520029));
#408448=CARTESIAN_POINT('Ctrl Pts',(1.97874979487762,-1.78901610456079,
8.85097269580138));
#408449=CARTESIAN_POINT('Ctrl Pts',(1.97856201674473,-1.78897903045468,
8.85143669361005));
#408450=CARTESIAN_POINT('Ctrl Pts',(1.9783658063634,-1.78894985763937,8.8519052845931));
#408451=CARTESIAN_POINT('Ctrl Pts',(1.97798203130075,-1.78889279746269,
8.85282181883899));
#408452=CARTESIAN_POINT('Ctrl Pts',(1.97757584056464,-1.78886762770679,
8.85372622499635));
#408453=CARTESIAN_POINT('Ctrl Pts',(1.97713990672663,-1.78888934263685,
8.85462257735071));
#408454=CARTESIAN_POINT('Ctrl Pts',(1.97677800993722,-1.78890736960054,
8.85536669723986));
#408455=CARTESIAN_POINT('Ctrl Pts',(1.97639553091104,-1.78895768077186,
8.85610498449051));
#408456=CARTESIAN_POINT('Ctrl Pts',(1.97598928856819,-1.7890567933604,8.85681338218371));
#408457=CARTESIAN_POINT('Ctrl Pts',(1.97562062300403,-1.78914673819017,
8.85745625420284));
#408458=CARTESIAN_POINT('Ctrl Pts',(1.97522762055869,-1.78927742070007,
8.85808743050665));
#408459=CARTESIAN_POINT('Ctrl Pts',(1.97480670587177,-1.78947721452131,
8.8586680450841));
#408460=CARTESIAN_POINT('Ctrl Pts',(1.97461250495954,-1.78956939505943,
8.85893592806395));
#408461=CARTESIAN_POINT('Ctrl Pts',(1.97441236097825,-1.78967652968199,
8.85919241173848));
#408462=CARTESIAN_POINT('Ctrl Pts',(1.97420613659522,-1.78980298681162,
8.85943017985534));
#408463=CARTESIAN_POINT('Ctrl Pts',(1.97392767262918,-1.78997374137194,
8.8597512372));
#408464=CARTESIAN_POINT('Ctrl Pts',(1.97363136948359,-1.7901846188583,8.86004599534706));
#408465=CARTESIAN_POINT('Ctrl Pts',(1.97332682621396,-1.7904415711516,8.86026130871722));
#408466=CARTESIAN_POINT('Ctrl Pts',(1.97321532433697,-1.79053564863043,
8.86034014101236));
#408467=CARTESIAN_POINT('Ctrl Pts',(1.97310103504486,-1.79063730615675,
8.86040910639693));
#408468=CARTESIAN_POINT('Ctrl Pts',(1.97298729564543,-1.79074402546768,
8.86046313645507));
#408469=CARTESIAN_POINT('Ctrl Pts',(1.97280980626519,-1.79091056005861,
8.8605474499083));
#408470=CARTESIAN_POINT('Ctrl Pts',(1.9726289116331,-1.79109407389667,8.86059655985669));
#408471=CARTESIAN_POINT('Ctrl Pts',(1.97245600443692,-1.79128259202279,
8.86059725258816));
#408472=CARTESIAN_POINT('Ctrl Pts',(1.97228269775604,-1.7914715457011,8.86059794692012));
#408473=CARTESIAN_POINT('Ctrl Pts',(1.97211745140938,-1.79166941813832,
8.86056369958366));
#408474=CARTESIAN_POINT('Ctrl Pts',(1.97196638965372,-1.79186300516204,
8.86048590497774));
#408475=CARTESIAN_POINT('Ctrl Pts',(1.97192696703314,-1.79191352561145,
8.86046560290182));
#408476=CARTESIAN_POINT('Ctrl Pts',(1.97188806900511,-1.7919644671666,8.86044257503091));
#408477=CARTESIAN_POINT('Ctrl Pts',(1.97185087146102,-1.79201423576954,
8.86041778462583));
#408478=CARTESIAN_POINT('Ctrl Pts',(1.97160057814758,-1.79234911670961,
8.86025097596201));
#408479=CARTESIAN_POINT('Ctrl Pts',(1.9713939560763,-1.79267602610359,8.8599848982295));
#408480=CARTESIAN_POINT('Ctrl Pts',(1.97122987412083,-1.79298089568,8.85968173251461));
#408481=CARTESIAN_POINT('Ctrl Pts',(1.97114308416717,-1.79314215421898,
8.85952137522076));
#408482=CARTESIAN_POINT('Ctrl Pts',(1.97106635501148,-1.79330026432412,
8.85934740853961));
#408483=CARTESIAN_POINT('Ctrl Pts',(1.97099937013856,-1.79345231758423,
8.8591675900182));
#408484=CARTESIAN_POINT('Ctrl Pts',(1.97073039105572,-1.79406289045929,
8.85844552518695));
#408485=CARTESIAN_POINT('Ctrl Pts',(1.97060056149349,-1.79460908862718,
8.85759444184124));
#408486=CARTESIAN_POINT('Ctrl Pts',(1.97053470628905,-1.79506393733561,
8.85683498915138));
#408487=CARTESIAN_POINT('Ctrl Pts',(1.9705278147173,-1.79511153604159,8.85675551444998));
#408488=CARTESIAN_POINT('Ctrl Pts',(1.97052164367322,-1.79515813331054,
8.85667699793651));
#408489=CARTESIAN_POINT('Ctrl Pts',(1.97051612006802,-1.79520369685433,
8.85659965593547));
#408490=CARTESIAN_POINT('Ctrl Pts',(1.97044156216318,-1.79581871589338,
8.85555568965886));
#408491=CARTESIAN_POINT('Ctrl Pts',(1.9704587283161,-1.79642055493027,8.85434650606346));
#408492=CARTESIAN_POINT('Ctrl Pts',(1.97056149117541,-1.79701236630734,
8.85297329937117));
#408493=CARTESIAN_POINT('Ctrl Pts',(1.97061928902234,-1.79734522414734,
8.85220095427747));
#408494=CARTESIAN_POINT('Ctrl Pts',(1.97070449840186,-1.79767499193948,
8.85137579139183));
#408495=CARTESIAN_POINT('Ctrl Pts',(1.97081848695447,-1.79800236791131,
8.85049129520029));
#408496=CARTESIAN_POINT('Origin',(1.97731117195261,-1.79574168958059,7.59394543036555));
#408497=CARTESIAN_POINT('Ctrl Pts',(1.97839165948369,-1.78892888448513,
7.59443877723642));
#408498=CARTESIAN_POINT('Ctrl Pts',(1.97276532395028,-1.78755865015692,
7.58783886950016));
#408499=CARTESIAN_POINT('Ctrl Pts',(1.96890226666508,-1.79511880689789,
7.58559994247159));
#408500=CARTESIAN_POINT('Ctrl Pts',(2.0091056600909,-1.79640895348185,7.56670252222136));
#408501=CARTESIAN_POINT('Ctrl Pts',(2.00348745620967,-1.7950406995313,7.56004874999026));
#408502=CARTESIAN_POINT('Ctrl Pts',(1.99958248326974,-1.80263593116663,
7.55786368756704));
#408503=CARTESIAN_POINT('Ctrl Pts',(2.03976230537068,-1.80387505419708,
7.53888913333559));
#408504=CARTESIAN_POINT('Ctrl Pts',(2.03411071222872,-1.80249866864629,
7.53222002137279));
#408505=CARTESIAN_POINT('Ctrl Pts',(2.03020677218686,-1.81013815140818,
7.53005029815326));
#408506=CARTESIAN_POINT('Ctrl Pts',(2.07036020808908,-1.81132684878468,
7.51101258149734));
#408507=CARTESIAN_POINT('Ctrl Pts',(2.06464010736904,-1.80993377894005,
7.5043616886572));
#408508=CARTESIAN_POINT('Ctrl Pts',(2.06077360068109,-1.81762517722493,
7.50217374673251));
#408509=CARTESIAN_POINT('',(2.05914251569205,-1.81722565891164,7.50366116523517));
#408510=CARTESIAN_POINT('Ctrl Pts',(2.0620244905542,-1.80929677321441,7.51860402984325));
#408511=CARTESIAN_POINT('Ctrl Pts',(2.06245356066702,-1.80940126868829,
7.51734760759494));
#408512=CARTESIAN_POINT('Ctrl Pts',(2.06282720854069,-1.80955350247717,
7.51608817408573));
#408513=CARTESIAN_POINT('Ctrl Pts',(2.06313953628695,-1.80976549106596,
7.5148100591312));
#408514=CARTESIAN_POINT('Ctrl Pts',(2.06342245022282,-1.80995751539531,
7.51365231206384));
#408515=CARTESIAN_POINT('Ctrl Pts',(2.06365558924025,-1.81019863323145,
7.51247773061043));
#408516=CARTESIAN_POINT('Ctrl Pts',(2.06380837374076,-1.8105103394139,7.51129758471022));
#408517=CARTESIAN_POINT('Ctrl Pts',(2.06399826742623,-1.8108977546005,7.50983079813402));
#408518=CARTESIAN_POINT('Ctrl Pts',(2.06404627660563,-1.81138758047697,
7.50839324291155));
#408519=CARTESIAN_POINT('Ctrl Pts',(2.06387070521551,-1.81199143356978,
7.50715379678855));
#408520=CARTESIAN_POINT('Ctrl Pts',(2.06378959629224,-1.81227039629905,
7.50658120839351));
#408521=CARTESIAN_POINT('Ctrl Pts',(2.06364011712739,-1.8126106987067,7.50598221009429));
#408522=CARTESIAN_POINT('Ctrl Pts',(2.06340499918458,-1.81299509420526,
7.50545747549612));
#408523=CARTESIAN_POINT('Ctrl Pts',(2.06327953297272,-1.81320021954144,
7.50517746087247));
#408524=CARTESIAN_POINT('Ctrl Pts',(2.06312849233741,-1.81342023086748,
7.50491486231392));
#408525=CARTESIAN_POINT('Ctrl Pts',(2.0629545019405,-1.81364835785532,7.50468370960992));
#408526=CARTESIAN_POINT('Ctrl Pts',(2.06269433141495,-1.81398947966072,
7.50433806340446));
#408527=CARTESIAN_POINT('Ctrl Pts',(2.06237460179235,-1.81435863918605,
7.50405484070983));
#408528=CARTESIAN_POINT('Ctrl Pts',(2.06201630474492,-1.81473050520947,
7.5038576603613));
#408529=CARTESIAN_POINT('Ctrl Pts',(2.0619779904449,-1.81477027050056,7.50383657498791));
#408530=CARTESIAN_POINT('Ctrl Pts',(2.06193926245815,-1.81481005916188,
7.50381643264937));
#408531=CARTESIAN_POINT('Ctrl Pts',(2.06190016639467,-1.81484983502234,
7.50379723213559));
#408532=CARTESIAN_POINT('Ctrl Pts',(2.06163918738169,-1.81511535190252,
7.50366906242519));
#408533=CARTESIAN_POINT('Ctrl Pts',(2.06135561716471,-1.81538556993998,
7.50358235568538));
#408534=CARTESIAN_POINT('Ctrl Pts',(2.06107602952701,-1.81563945665819,
7.5035341175365));
#408535=CARTESIAN_POINT('Ctrl Pts',(2.0606568195075,-1.81602013105772,7.50346178989176));
#408536=CARTESIAN_POINT('Ctrl Pts',(2.0601896590865,-1.81641182575993,7.50346967198527));
#408537=CARTESIAN_POINT('Ctrl Pts',(2.05971922051128,-1.81678223725705,
7.50354272648692));
#408538=CARTESIAN_POINT('Ctrl Pts',(2.05952571938779,-1.81693459517288,
7.50357277531559));
#408539=CARTESIAN_POINT('Ctrl Pts',(2.05933200846983,-1.8170832612696,7.50361331098761));
#408540=CARTESIAN_POINT('Ctrl Pts',(2.05914251569312,-1.81722565891258,
7.50366116523659));
#408541=CARTESIAN_POINT('',(1.97947865054224,-1.79771013628761,7.57603338622103));
#408542=CARTESIAN_POINT('Origin',(1.98601852345805,-1.80365333002949,7.58486873427628));
#408543=CARTESIAN_POINT('Ctrl Pts',(2.05914251574879,-1.81722565892002,
7.50366116529968));
#408544=CARTESIAN_POINT('Ctrl Pts',(2.03263102682017,-1.81073191165143,
7.52783573079709));
#408545=CARTESIAN_POINT('Ctrl Pts',(2.00607765461974,-1.80422706199264,
7.55196141284068));
#408546=CARTESIAN_POINT('Ctrl Pts',(1.97947865179297,-1.79771013622992,
7.57603338728831));
#408547=CARTESIAN_POINT('Ctrl Pts',(1.97989555771598,-1.78947609816003,
7.5963967733137));
#408548=CARTESIAN_POINT('Ctrl Pts',(1.96304400704071,-1.78239816374406,
7.5995988229547));
#408549=CARTESIAN_POINT('Ctrl Pts',(1.97123919548054,-1.79875504911528,
7.59642833564546));
#408550=CARTESIAN_POINT('Ctrl Pts',(1.9765888088445,-1.78740715737189,7.58707626057421));
#408551=CARTESIAN_POINT('Ctrl Pts',(1.96999477520764,-1.78896632748219,
7.58809943920599));
#408552=CARTESIAN_POINT('Ctrl Pts',(1.96897092964353,-1.79564960071125,
7.58710240504253));
#408553=CARTESIAN_POINT('Ctrl Pts',(1.97787616399563,-1.79334587347696,
7.58015376756929));
#408554=CARTESIAN_POINT('Ctrl Pts',(1.9750397244827,-1.79363549786383,7.58205880659761));
#408555=CARTESIAN_POINT('Ctrl Pts',(1.9749817704291,-1.79645040751884,7.58020924244126));
#408556=CARTESIAN_POINT('Ctrl Pts',(1.97947864992974,-1.79771013573109,
7.57603338509286));
#408557=CARTESIAN_POINT('Ctrl Pts',(1.97947864992974,-1.79771013573109,
7.57603338509286));
#408558=CARTESIAN_POINT('Ctrl Pts',(1.97947864992974,-1.79771013573109,
7.57603338509286));
#408559=CARTESIAN_POINT('Origin',(1.98602235984358,-1.80364910574229,7.58486873427622));
#408560=CARTESIAN_POINT('Ctrl Pts',(2.00176808024936,-1.8868898302952,7.51098857897448));
#408561=CARTESIAN_POINT('Ctrl Pts',(1.99983217741496,-1.88132990294067,
7.50433767179956));
#408562=CARTESIAN_POINT('Ctrl Pts',(2.00711679739923,-1.87674270741756,
7.50214974420965));
#408563=CARTESIAN_POINT('Ctrl Pts',(1.99140963785971,-1.85714030662641,
7.53887321589171));
#408564=CARTESIAN_POINT('Ctrl Pts',(1.98949693057689,-1.85164699706867,
7.53220407452065));
#408565=CARTESIAN_POINT('Ctrl Pts',(1.99672626159454,-1.84702750651672,
7.53003438070911));
#408566=CARTESIAN_POINT('Ctrl Pts',(1.98103130343959,-1.82733365289799,
7.56669465659232));
#408567=CARTESIAN_POINT('Ctrl Pts',(1.97912989990116,-1.82187280777845,
7.56004085833298));
#408568=CARTESIAN_POINT('Ctrl Pts',(1.98631507225217,-1.8172565378109,7.55785582193788));
#408569=CARTESIAN_POINT('Ctrl Pts',(1.97063354635954,-1.79747121714566,
7.59443891967696));
#408570=CARTESIAN_POINT('Ctrl Pts',(1.96872938602274,-1.79200245448059,
7.58783901202978));
#408571=CARTESIAN_POINT('Ctrl Pts',(1.97588366545475,-1.78743129885021,
7.58560008491213));
#408572=CARTESIAN_POINT('',(2.00655355952794,-1.87513194417972,7.50366116523517));
#408573=CARTESIAN_POINT('Ctrl Pts',(2.00655355952821,-1.87513194417998,
7.50366116523554));
#408574=CARTESIAN_POINT('Ctrl Pts',(2.00615848269925,-1.87577851344617,
7.50350835821027));
#408575=CARTESIAN_POINT('Ctrl Pts',(2.00577427574859,-1.87636001411703,
7.50345484956));
#408576=CARTESIAN_POINT('Ctrl Pts',(2.00539001691052,-1.87689406571167,
7.50349758195598));
#408577=CARTESIAN_POINT('Ctrl Pts',(2.00519286362921,-1.87716807378603,
7.50351950684424));
#408578=CARTESIAN_POINT('Ctrl Pts',(2.00497636954117,-1.87745667406356,
7.50357029184312));
#408579=CARTESIAN_POINT('Ctrl Pts',(2.00475995703381,-1.8777292295213,7.50365515313924));
#408580=CARTESIAN_POINT('Ctrl Pts',(2.00442702696342,-1.8781485301839,7.50378570417639));
#408581=CARTESIAN_POINT('Ctrl Pts',(2.00408478899121,-1.87854238174115,
7.50400001621911));
#408582=CARTESIAN_POINT('Ctrl Pts',(2.0037575786085,-1.87887931717082,7.50428903009634));
#408583=CARTESIAN_POINT('Ctrl Pts',(2.00372126077342,-1.87891671441129,
7.50432110841318));
#408584=CARTESIAN_POINT('Ctrl Pts',(2.003685123025,-1.87895344037837,7.50435406373354));
#408585=CARTESIAN_POINT('Ctrl Pts',(2.00364919461635,-1.87898947405934,
7.50438785222352));
#408586=CARTESIAN_POINT('Ctrl Pts',(2.00342983441216,-1.87920947700161,
7.50459414719561));
#408587=CARTESIAN_POINT('Ctrl Pts',(2.00321442008338,-1.87940681218195,
7.50483629897752));
#408588=CARTESIAN_POINT('Ctrl Pts',(2.00301209305112,-1.87957489015283,
7.5050991045531));
#408589=CARTESIAN_POINT('Ctrl Pts',(2.00256573929613,-1.87994568703842,
7.50567888004914));
#408590=CARTESIAN_POINT('Ctrl Pts',(2.00216582340183,-1.88018910434133,
7.50637912803144));
#408591=CARTESIAN_POINT('Ctrl Pts',(2.001820965996,-1.88033482544297,7.50710440483569));
#408592=CARTESIAN_POINT('Ctrl Pts',(2.00173640011371,-1.88037055915006,
7.50728225710685));
#408593=CARTESIAN_POINT('Ctrl Pts',(2.00165351840972,-1.88040126390212,
7.50746498566954));
#408594=CARTESIAN_POINT('Ctrl Pts',(2.00157440033248,-1.88042661359859,
7.50764697238949));
#408595=CARTESIAN_POINT('Ctrl Pts',(2.00114908332307,-1.8805628865904,7.50862528291181));
#408596=CARTESIAN_POINT('Ctrl Pts',(2.00079518281119,-1.88056071912447,
7.50965856837421));
#408597=CARTESIAN_POINT('Ctrl Pts',(2.00049449295551,-1.88048386026498,
7.51067959873202));
#408598=CARTESIAN_POINT('Ctrl Pts',(2.00032902294865,-1.88044156473766,
7.51124147302578));
#408599=CARTESIAN_POINT('Ctrl Pts',(2.00017973400084,-1.88037621910702,
7.51180065547253));
#408600=CARTESIAN_POINT('Ctrl Pts',(2.00004436034524,-1.88029584196496,
7.51235175716501));
#408601=CARTESIAN_POINT('Ctrl Pts',(1.99957659043867,-1.88001810692069,
7.51425603304536));
#408602=CARTESIAN_POINT('Ctrl Pts',(1.9992222893872,-1.879522569644,7.5162690050518));
#408603=CARTESIAN_POINT('Ctrl Pts',(1.99897691956688,-1.87886941383172,
7.51827788969243));
#408604=CARTESIAN_POINT('Ctrl Pts',(1.99896363968852,-1.87883406380486,
7.51838661432545));
#408605=CARTESIAN_POINT('Ctrl Pts',(1.99895068242725,-1.87879824277265,
7.51849533314856));
#408606=CARTESIAN_POINT('Ctrl Pts',(1.99893804826279,-1.87876195735827,
7.51860402984325));
#408607=CARTESIAN_POINT('Ctrl Pts',(1.97947865060564,-1.79771013753908,
7.57603338728984));
#408608=CARTESIAN_POINT('Ctrl Pts',(1.98851957913015,-1.82356045445255,
7.55196141284921));
#408609=CARTESIAN_POINT('Ctrl Pts',(1.99754410576772,-1.84936651119314,
7.52783573083104));
#408610=CARTESIAN_POINT('Ctrl Pts',(2.00655355954226,-1.87513194423715,
7.50366116530176));
#408611=CARTESIAN_POINT('Origin',(6.8400137636579E-16,-6.21191952330704E-16,
7.49482233047033));
#408612=CARTESIAN_POINT('Origin',(2.05251535802926,-1.81137708803386,7.49482233047033));
#408613=CARTESIAN_POINT('Origin',(0.,0.,7.50366116523517));
#408614=CARTESIAN_POINT('Origin',(2.00009565450364,-1.86909700733688,7.49482233047033));
#408615=CARTESIAN_POINT('Ctrl Pts',(2.0620234628822,-1.80929652288974,7.51860402984325));
#408616=CARTESIAN_POINT('Ctrl Pts',(2.06941618821694,-1.81109760538512,
7.51860402984325));
#408617=CARTESIAN_POINT('Ctrl Pts',(2.07441142381099,-1.80535792705005,
7.51860402984325));
#408618=CARTESIAN_POINT('Ctrl Pts',(2.06476843255037,-1.80996527587688,
7.51041458714366));
#408619=CARTESIAN_POINT('Ctrl Pts',(2.07059960927626,-1.80973780334733,
7.51004642900442));
#408620=CARTESIAN_POINT('Ctrl Pts',(2.07441280143767,-1.80535634411491,
7.50729136483009));
#408621=CARTESIAN_POINT('Ctrl Pts',(2.0650864853118,-1.8127621633684,7.50215815450138));
#408622=CARTESIAN_POINT('Ctrl Pts',(2.06819015181947,-1.81250658815321,
7.4987716367153));
#408623=CARTESIAN_POINT('Ctrl Pts',(2.07047313188641,-1.80991971250712,
7.49481588533171));
#408624=CARTESIAN_POINT('Ctrl Pts',(2.05914210292583,-1.81722529463959,
7.50366171572174));
#408625=CARTESIAN_POINT('Ctrl Pts',(2.06188757427571,-1.81964821629001,
7.50000045605858));
#408626=CARTESIAN_POINT('Ctrl Pts',(2.0618875742758,-1.81964821628992,7.49482233047317));
#408627=CARTESIAN_POINT('Origin',(2.06498228097549,-1.79715175465437,7.51860402984325));
#408628=CARTESIAN_POINT('Origin',(2.06498228097549,-1.79715175465437,9.));
#408629=CARTESIAN_POINT('Origin',(2.06498228097549,-1.79715175465437,8.75721825406948));
#408630=CARTESIAN_POINT('Ctrl Pts',(2.04579859637349,-1.80534509773718,
8.78942910404913));
#408631=CARTESIAN_POINT('Ctrl Pts',(2.05120799968458,-1.80668329970981,
8.7967269950169));
#408632=CARTESIAN_POINT('Ctrl Pts',(2.05490627375195,-1.79855949180312,
8.79893251111266));
#408633=CARTESIAN_POINT('Ctrl Pts',(2.05648070824781,-1.80794661741698,
8.78111911759577));
#408634=CARTESIAN_POINT('Ctrl Pts',(2.0628954061557,-1.80952584535372,8.78644465894812));
#408635=CARTESIAN_POINT('Ctrl Pts',(2.06775831860606,-1.80303989174028,
8.78817647674132));
#408636=CARTESIAN_POINT('Ctrl Pts',(2.06313805516787,-1.80956794650262,
8.76780923932035));
#408637=CARTESIAN_POINT('Ctrl Pts',(2.07071155334932,-1.81142721035319,
8.76988516158375));
#408638=CARTESIAN_POINT('Ctrl Pts',(2.07578916287304,-1.8058277227051,8.77093053738833));
#408639=CARTESIAN_POINT('Ctrl Pts',(2.06183996363106,-1.80925180951868,
8.75371302330491));
#408640=CARTESIAN_POINT('Ctrl Pts',(2.06922740267153,-1.81106618152883,
8.75300828287558));
#408641=CARTESIAN_POINT('Ctrl Pts',(2.07422297212532,-1.80528355019295,
8.75267964240738));
#408642=CARTESIAN_POINT('Origin',(2.05135792032744,-1.79383368616219,8.78727029226991));
#408643=CARTESIAN_POINT('Ctrl Pts',(1.97893795668432,-1.78906192937257,
8.85049129520029));
#408644=CARTESIAN_POINT('Ctrl Pts',(1.9846117360273,-1.79044371813726,8.85711686593484));
#408645=CARTESIAN_POINT('Ctrl Pts',(1.9884767993203,-1.78281731348926,8.85933012996512));
#408646=CARTESIAN_POINT('Ctrl Pts',(2.00212570220898,-1.79470905879152,
8.82945683644723));
#408647=CARTESIAN_POINT('Ctrl Pts',(2.00784657735092,-1.79610231723841,
8.83607469902389));
#408648=CARTESIAN_POINT('Ctrl Pts',(2.01168953666617,-1.78843656833835,
8.83829567148519));
#408649=CARTESIAN_POINT('Ctrl Pts',(2.02527888452907,-1.8003477707087,8.80838214965003));
#408650=CARTESIAN_POINT('Ctrl Pts',(2.03102233691534,-1.80174652760393,
8.81501364461986));
#408651=CARTESIAN_POINT('Ctrl Pts',(2.03486690419791,-1.79404794883865,
8.81722098428721));
#408652=CARTESIAN_POINT('Ctrl Pts',(2.04840012990614,-1.80597870472223,
8.78727029226991));
#408653=CARTESIAN_POINT('Ctrl Pts',(2.05414453629875,-1.80737769395556,
8.79393457792714));
#408654=CARTESIAN_POINT('Ctrl Pts',(2.05801159645807,-1.79965207029772,
8.79610912703474));
#408655=CARTESIAN_POINT('Origin',(1.98189574710561,-1.77691691081253,8.85049129520029));
#408656=CARTESIAN_POINT('Ctrl Pts',(1.97081848695447,-1.79800236791131,
8.85049129520029));
#408657=CARTESIAN_POINT('Ctrl Pts',(1.9727387040902,-1.80351724582245,8.85711686593484));
#408658=CARTESIAN_POINT('Ctrl Pts',(1.9655186752694,-1.80809675954562,8.85933012996512));
#408659=CARTESIAN_POINT('Ctrl Pts',(1.96911969857312,-1.79312343503143,
8.86332496987233));
#408660=CARTESIAN_POINT('Ctrl Pts',(1.96622788905522,-1.79672750663017,
8.86648636486738));
#408661=CARTESIAN_POINT('Ctrl Pts',(1.9607824254138,-1.79444211221725,8.87206031107456));
#408662=CARTESIAN_POINT('Ctrl Pts',(1.97388433684392,-1.78783117387533,
8.86341338519875));
#408663=CARTESIAN_POINT('Ctrl Pts',(1.97718275554805,-1.78457634597106,
8.86654584966058));
#408664=CARTESIAN_POINT('Ctrl Pts',(1.97432290905723,-1.77938544712438,
8.87215952290715));
#408665=CARTESIAN_POINT('Ctrl Pts',(1.97893795668432,-1.78906192937257,
8.85049129520029));
#408666=CARTESIAN_POINT('Ctrl Pts',(1.9846117360273,-1.79044371813726,8.85711686593484));
#408667=CARTESIAN_POINT('Ctrl Pts',(1.9884767993203,-1.78281731348926,8.85933012996512));
#408668=CARTESIAN_POINT('Origin',(1.95901360513968,-1.80211269214899,8.85049129520029));
#408669=CARTESIAN_POINT('Ctrl Pts',(1.99432705985486,-1.8655191643187,8.78727029226991));
#408670=CARTESIAN_POINT('Ctrl Pts',(1.99627117980082,-1.8711026912788,8.79393457792714));
#408671=CARTESIAN_POINT('Ctrl Pts',(1.98895258219517,-1.87569371995055,
8.79610912703474));
#408672=CARTESIAN_POINT('Ctrl Pts',(1.98650197380754,-1.84304545892765,
8.80838214965002));
#408673=CARTESIAN_POINT('Ctrl Pts',(1.98844577088239,-1.84862805859965,
8.81501364461993));
#408674=CARTESIAN_POINT('Ctrl Pts',(1.98115193336384,-1.85319410139922,
8.81722098428721));
#408675=CARTESIAN_POINT('Ctrl Pts',(1.97866607911547,-1.82054071102842,
8.82945683644721));
#408676=CARTESIAN_POINT('Ctrl Pts',(1.9806022352144,-1.82610136576058,8.83607469902388));
#408677=CARTESIAN_POINT('Ctrl Pts',(1.97334092145606,-1.83066265560013,
8.83829567148519));
#408678=CARTESIAN_POINT('Ctrl Pts',(1.97081848695447,-1.79800236791131,
8.85049129520029));
#408679=CARTESIAN_POINT('Ctrl Pts',(1.9727387040902,-1.80351724582245,8.85711686593484));
#408680=CARTESIAN_POINT('Ctrl Pts',(1.9655186752694,-1.80809675954562,8.85933012996512));
#408681=CARTESIAN_POINT('Origin',(1.98252217804007,-1.86962948855638,8.78727029226991));
#408682=CARTESIAN_POINT('Ctrl Pts',(1.99887714505915,-1.87858709900373,
8.75374538247848));
#408683=CARTESIAN_POINT('Ctrl Pts',(2.00138827335462,-1.88575917074565,
8.75304829418601));
#408684=CARTESIAN_POINT('Ctrl Pts',(1.99612174305393,-1.89128495592071,
8.75272238421917));
#408685=CARTESIAN_POINT('Ctrl Pts',(1.99931119033488,-1.87983367897014,
8.76769408445018));
#408686=CARTESIAN_POINT('Ctrl Pts',(2.00188485842239,-1.88718645990986,
8.76974318093969));
#408687=CARTESIAN_POINT('Ctrl Pts',(1.99680650103025,-1.89277471934172,
8.77077869880429));
#408688=CARTESIAN_POINT('Ctrl Pts',(1.99708652152473,-1.87344442018716,
8.78108014887992));
#408689=CARTESIAN_POINT('Ctrl Pts',(1.99927119857793,-1.87967438194253,
8.78639403366325));
#408690=CARTESIAN_POINT('Ctrl Pts',(1.9933043463902,-1.88514418547636,8.78812224174742));
#408691=CARTESIAN_POINT('Ctrl Pts',(1.99344078041233,-1.86297383549666,
8.78944554828685));
#408692=CARTESIAN_POINT('Ctrl Pts',(1.99528722758711,-1.86822236390449,
8.79673892988686));
#408693=CARTESIAN_POINT('Ctrl Pts',(1.98756562585767,-1.87268111048267,
8.79894799272499));
#408694=CARTESIAN_POINT('Origin',(1.98713316644801,-1.88287228159595,8.75721825406948));
#408695=CARTESIAN_POINT('Origin',(1.98713316644801,-1.88287228159595,9.));
#408696=CARTESIAN_POINT('Origin',(1.98713316644801,-1.88287228159595,7.51860402984325));
#408697=CARTESIAN_POINT('Ctrl Pts',(2.0065529847689,-1.87513140706529,7.50366195182966));
#408698=CARTESIAN_POINT('Ctrl Pts',(2.00922851137342,-1.8776316968682,7.50000065167735));
#408699=CARTESIAN_POINT('Ctrl Pts',(2.00922851137334,-1.87763169686828,
7.49482233047108));
#408700=CARTESIAN_POINT('Ctrl Pts',(2.00267706150172,-1.88148207777267,
7.50215800491337));
#408701=CARTESIAN_POINT('Ctrl Pts',(2.0027193514308,-1.88459702700761,7.49877273257264));
#408702=CARTESIAN_POINT('Ctrl Pts',(2.00036234457185,-1.88711926312202,
7.49481816995647));
#408703=CARTESIAN_POINT('Ctrl Pts',(1.99986519248849,-1.88142369117742,
7.51043025814041));
#408704=CARTESIAN_POINT('Ctrl Pts',(2.00020259949308,-1.88725283463937,
7.51006209594515));
#408705=CARTESIAN_POINT('Ctrl Pts',(1.99620509243912,-1.89147170978753,
7.50731281821699));
#408706=CARTESIAN_POINT('Ctrl Pts',(1.99893755118653,-1.87876053002942,
7.51860402984325));
#408707=CARTESIAN_POINT('Ctrl Pts',(2.00144054600743,-1.885946351786,7.51860402984325));
#408708=CARTESIAN_POINT('Ctrl Pts',(1.99620683387471,-1.89146987192287,
7.51860402984325));
#408709=CARTESIAN_POINT('Origin',(0.,0.,7.5));
#408710=CARTESIAN_POINT('Origin',(2.08196763624133,-1.66803740521006,7.5));
#408711=CARTESIAN_POINT('',(2.08196763624133,-1.66803740521006,7.59394543036555));
#408712=CARTESIAN_POINT('',(2.08196763624133,-1.66803740521006,8.85049129520029));
#408713=CARTESIAN_POINT('',(2.08196763624133,-1.66803740521006,7.5));
#408714=CARTESIAN_POINT('',(2.10975372425562,-1.73390928168091,8.78727029226991));
#408715=CARTESIAN_POINT('Ctrl Pts',(2.08196763624133,-1.66803740521006,
8.85049129520029));
#408716=CARTESIAN_POINT('Ctrl Pts',(2.09124312883604,-1.69002661441761,
8.82945686509571));
#408717=CARTESIAN_POINT('Ctrl Pts',(2.10050483228945,-1.71198313400677,
8.80838212259895));
#408718=CARTESIAN_POINT('Ctrl Pts',(2.10975372425562,-1.73390928168091,
8.78727029226991));
#408719=CARTESIAN_POINT('',(2.11520370755655,-1.74682943894027,8.75721825406948));
#408720=CARTESIAN_POINT('Origin',(2.09880300312937,-1.70794812528232,8.75937679713171));
#408721=CARTESIAN_POINT('',(2.11520370755655,-1.74682943894027,7.51860402984325));
#408722=CARTESIAN_POINT('',(2.11520370755655,-1.74682943894027,7.5));
#408723=CARTESIAN_POINT('Ctrl Pts',(2.11520370755655,-1.74682943894027,
7.51860402984325));
#408724=CARTESIAN_POINT('Ctrl Pts',(2.1109235933064,-1.73668266487759,7.52834476460825));
#408725=CARTESIAN_POINT('Ctrl Pts',(2.10664070046786,-1.7265293036756,7.53807742314407));
#408726=CARTESIAN_POINT('Ctrl Pts',(2.10235493574609,-1.71636913416235,
7.54780169004674));
#408727=CARTESIAN_POINT('Ctrl Pts',(2.09556651605263,-1.70027597476365,
7.5632044032688));
#408728=CARTESIAN_POINT('Ctrl Pts',(2.08877088254286,-1.68416571372708,
7.57858609112103));
#408729=CARTESIAN_POINT('Ctrl Pts',(2.08196763624133,-1.66803740521006,
7.59394543036555));
#408730=CARTESIAN_POINT('Origin',(2.36030818298168,-1.70641386443187,7.5));
#408731=CARTESIAN_POINT('',(2.17370988235716,-1.67346501623194,8.75721825406948));
#408732=CARTESIAN_POINT('',(2.15990092504106,-1.67102668085116,8.78727029226991));
#408733=CARTESIAN_POINT('Origin',(2.12484864088931,-1.6648372762011,8.75658640621081));
#408734=CARTESIAN_POINT('',(2.0894976077859,-1.65859511954943,8.85049129520029));
#408735=CARTESIAN_POINT('Ctrl Pts',(2.15990092504106,-1.67102668085116,
8.78727029226991));
#408736=CARTESIAN_POINT('Ctrl Pts',(2.13646643958855,-1.66688870477509,
8.80838212259895));
#408737=CARTESIAN_POINT('Ctrl Pts',(2.11299949288423,-1.66274499680943,
8.82945686509571));
#408738=CARTESIAN_POINT('Ctrl Pts',(2.0894976077859,-1.65859511954943,8.85049129520029));
#408739=CARTESIAN_POINT('',(2.0894976077859,-1.65859511954943,7.59394543036555));
#408740=CARTESIAN_POINT('',(2.0894976077859,-1.65859511954943,7.5));
#408741=CARTESIAN_POINT('',(2.17370988235716,-1.67346501623194,7.51860402984325));
#408742=CARTESIAN_POINT('Ctrl Pts',(2.0894976077859,-1.65859511954943,7.59394543036555));
#408743=CARTESIAN_POINT('Ctrl Pts',(2.10673541065637,-1.6616389079879,7.57858609112103));
#408744=CARTESIAN_POINT('Ctrl Pts',(2.12395392452868,-1.66467929044536,
7.56320440326857));
#408745=CARTESIAN_POINT('Ctrl Pts',(2.14115416031193,-1.66771644542441,
7.54780169004651));
#408746=CARTESIAN_POINT('Ctrl Pts',(2.15201326553151,-1.66963390666746,
7.53807742314383));
#408747=CARTESIAN_POINT('Ctrl Pts',(2.16286509408447,-1.67155008302322,
7.52834476460825));
#408748=CARTESIAN_POINT('Ctrl Pts',(2.17370988235716,-1.67346501623194,
7.51860402984325));
#408749=CARTESIAN_POINT('',(2.17370988235716,-1.67346501623194,7.5));
#408750=CARTESIAN_POINT('Origin',(2.08830213916384,-1.66536538392933,7.5));
#408751=CARTESIAN_POINT('Ctrl Pts',(2.0894976077859,-1.65859511954943,8.85049129520029));
#408752=CARTESIAN_POINT('Ctrl Pts',(2.08930689657204,-1.658561444458,8.85097269580138));
#408753=CARTESIAN_POINT('Ctrl Pts',(2.08911712890333,-1.65853647751089,
8.85143669361005));
#408754=CARTESIAN_POINT('Ctrl Pts',(2.08891945254858,-1.65851993587655,
8.8519052845931));
#408755=CARTESIAN_POINT('Ctrl Pts',(2.08853281013488,-1.65848758148882,
8.85282181883899));
#408756=CARTESIAN_POINT('Ctrl Pts',(2.08812584132941,-1.65848848817669,
8.85372622499636));
#408757=CARTESIAN_POINT('Ctrl Pts',(2.08769219444457,-1.658538088868,8.85462257735071));
#408758=CARTESIAN_POINT('Ctrl Pts',(2.08733219620246,-1.65857926560027,
8.85536669723987));
#408759=CARTESIAN_POINT('Ctrl Pts',(2.08695372646827,-1.65865397891724,
8.85610498449051));
#408760=CARTESIAN_POINT('Ctrl Pts',(2.08655466895923,-1.65877891590461,
8.85681338218371));
#408761=CARTESIAN_POINT('Ctrl Pts',(2.08619252364304,-1.65889229641687,
8.85745625420285));
#408762=CARTESIAN_POINT('Ctrl Pts',(2.08580870152052,-1.65904789017867,
8.85808743050667));
#408763=CARTESIAN_POINT('Ctrl Pts',(2.08540145248205,-1.65927424159866,
8.85866804508412));
#408764=CARTESIAN_POINT('Ctrl Pts',(2.08521355660378,-1.65937867523714,
8.85893592806396));
#408765=CARTESIAN_POINT('Ctrl Pts',(2.0850206879786,-1.65949841300904,8.85919241173849));
#408766=CARTESIAN_POINT('Ctrl Pts',(2.0848229894418,-1.65963782316052,8.85943017985534));
#408767=CARTESIAN_POINT('Ctrl Pts',(2.08455603789209,-1.65982606813484,
8.8597512372));
#408768=CARTESIAN_POINT('Ctrl Pts',(2.08427385450003,-1.66005549655851,
8.86004599534705));
#408769=CARTESIAN_POINT('Ctrl Pts',(2.08398639993717,-1.66033143307005,
8.86026130871721));
#408770=CARTESIAN_POINT('Ctrl Pts',(2.0838811547175,-1.66043246120639,8.86034014101235));
#408771=CARTESIAN_POINT('Ctrl Pts',(2.08377361346507,-1.66054123240651,
8.86040910639692));
#408772=CARTESIAN_POINT('Ctrl Pts',(2.08366694528517,-1.66065501975951,
8.86046313645506));
#408773=CARTESIAN_POINT('Ctrl Pts',(2.08350049048377,-1.66083258397089,
8.86054744990829));
#408774=CARTESIAN_POINT('Ctrl Pts',(2.08333172529108,-1.66102731071897,
8.86059655985668));
#408775=CARTESIAN_POINT('Ctrl Pts',(2.08317125174908,-1.66122651971647,
8.86059725258816));
#408776=CARTESIAN_POINT('Ctrl Pts',(2.0830104074491,-1.66142618896635,8.86059794692011));
#408777=CARTESIAN_POINT('Ctrl Pts',(2.08285817834937,-1.66163424222321,
8.86056369958365));
#408778=CARTESIAN_POINT('Ctrl Pts',(2.08271983012948,-1.66183711006154,
8.86048590497774));
#408779=CARTESIAN_POINT('Ctrl Pts',(2.08268372536321,-1.66189005252724,
8.86046560290182));
#408780=CARTESIAN_POINT('Ctrl Pts',(2.082648171092,-1.66194338162272,8.86044257503091));
#408781=CARTESIAN_POINT('Ctrl Pts',(2.08261423865959,-1.66199543122556,
8.86041778462583));
#408782=CARTESIAN_POINT('Ctrl Pts',(2.0823859154961,-1.66234566046448,8.86025097596201));
#408783=CARTESIAN_POINT('Ctrl Pts',(2.08220066310881,-1.6626851365096,8.8599848982295));
#408784=CARTESIAN_POINT('Ctrl Pts',(2.08205645133815,-1.66299989246576,
8.85968173251461));
#408785=CARTESIAN_POINT('Ctrl Pts',(2.08198017157382,-1.66316638033319,
8.85952137522076));
#408786=CARTESIAN_POINT('Ctrl Pts',(2.08191373021563,-1.66332908163805,
8.85934740853961));
#408787=CARTESIAN_POINT('Ctrl Pts',(2.08185662505613,-1.66348511422397,
8.8591675900182));
#408788=CARTESIAN_POINT('Ctrl Pts',(2.08162731815808,-1.66411166616059,
8.85844552518695));
#408789=CARTESIAN_POINT('Ctrl Pts',(2.08153275038139,-1.66466506031438,
8.85759444184123));
#408790=CARTESIAN_POINT('Ctrl Pts',(2.08149617274034,-1.6651231938448,8.85683498915137));
#408791=CARTESIAN_POINT('Ctrl Pts',(2.08149234498762,-1.66517113629864,
8.85675551444997));
#408792=CARTESIAN_POINT('Ctrl Pts',(2.08148917211988,-1.66521803320865,
8.85667699793651));
#408793=CARTESIAN_POINT('Ctrl Pts',(2.0814865791298,-1.66526385703585,8.85659965593547));
#408794=CARTESIAN_POINT('Ctrl Pts',(2.08145157881729,-1.66588238939369,
8.85555568965886));
#408795=CARTESIAN_POINT('Ctrl Pts',(2.08150726966,-1.66648189204854,8.85434650606346));
#408796=CARTESIAN_POINT('Ctrl Pts',(2.08164773886711,-1.66706590344665,
8.85297329937117));
#408797=CARTESIAN_POINT('Ctrl Pts',(2.08172674423719,-1.66739437427376,
8.85220095427747));
#408798=CARTESIAN_POINT('Ctrl Pts',(2.08183290683989,-1.66771800513891,
8.85137579139183));
#408799=CARTESIAN_POINT('Ctrl Pts',(2.08196763624133,-1.66803740521006,
8.85049129520029));
#408800=CARTESIAN_POINT('Origin',(2.08830213916384,-1.66536538392933,7.59394543036555));
#408801=CARTESIAN_POINT('Ctrl Pts',(2.08894390879625,-1.65849734939881,
7.59443877723642));
#408802=CARTESIAN_POINT('Ctrl Pts',(2.08324134195779,-1.6574904109193,7.58783886950016));
#408803=CARTESIAN_POINT('Ctrl Pts',(2.07987060264358,-1.66528254143747,
7.58559994247159));
#408804=CARTESIAN_POINT('Ctrl Pts',(2.12007405386126,-1.66399419701615,
7.56670252222138));
#408805=CARTESIAN_POINT('Ctrl Pts',(2.11437972885085,-1.66298871384865,
7.56004874999029));
#408806=CARTESIAN_POINT('Ctrl Pts',(2.1109694072583,-1.67081853274127,7.55786368756705));
#408807=CARTESIAN_POINT('Ctrl Pts',(2.15114606649061,-1.66948077981977,
7.5388891333356));
#408808=CARTESIAN_POINT('Ctrl Pts',(2.14541789982785,-1.66846932101654,
7.53222002137277));
#408809=CARTESIAN_POINT('Ctrl Pts',(2.14201144419061,-1.67634323393906,
7.53005029815326));
#408810=CARTESIAN_POINT('Ctrl Pts',(2.18215854065473,-1.67495684953808,
7.51101258149734));
#408811=CARTESIAN_POINT('Ctrl Pts',(2.1763609382037,-1.67393313001629,7.5043616886572));
#408812=CARTESIAN_POINT('Ctrl Pts',(2.1729951652485,-1.68185645343255,7.50217374673251));
#408813=CARTESIAN_POINT('',(2.17134183427229,-1.68156225994654,7.50366116523517));
#408814=CARTESIAN_POINT('Ctrl Pts',(2.17370988235716,-1.67346501623194,
7.51860402984325));
#408815=CARTESIAN_POINT('Ctrl Pts',(2.17414476594742,-1.67354180639215,
7.51734760759493));
#408816=CARTESIAN_POINT('Ctrl Pts',(2.1745273997738,-1.67366978769892,7.51608817408573));
#408817=CARTESIAN_POINT('Ctrl Pts',(2.17485266796472,-1.67386132982701,
7.5148100591312));
#408818=CARTESIAN_POINT('Ctrl Pts',(2.17514730366459,-1.67403483326368,
7.51365231206384));
#408819=CARTESIAN_POINT('Ctrl Pts',(2.17539541214572,-1.67426051842923,
7.51247773061043));
#408820=CARTESIAN_POINT('Ctrl Pts',(2.17556785381776,-1.67456179524134,
7.51129758471022));
#408821=CARTESIAN_POINT('Ctrl Pts',(2.17578217912252,-1.67493624791169,
7.50983079813401));
#408822=CARTESIAN_POINT('Ctrl Pts',(2.17586147291357,-1.67542199142967,
7.50839324291155));
#408823=CARTESIAN_POINT('Ctrl Pts',(2.17572495125419,-1.67603585273913,
7.50715379678855));
#408824=CARTESIAN_POINT('Ctrl Pts',(2.17566188218133,-1.67631943897611,
7.50658120839351));
#408825=CARTESIAN_POINT('Ctrl Pts',(2.17553451338757,-1.67666861935894,
7.50598221009429));
#408826=CARTESIAN_POINT('Ctrl Pts',(2.17532450682395,-1.67706728913404,
7.50545747549611));
#408827=CARTESIAN_POINT('Ctrl Pts',(2.17521244082129,-1.67728003166601,
7.50517746087247));
#408828=CARTESIAN_POINT('Ctrl Pts',(2.17507580668922,-1.67750926816192,
7.50491486231392));
#408829=CARTESIAN_POINT('Ctrl Pts',(2.17491678992053,-1.6777480740414,7.50468370960992));
#408830=CARTESIAN_POINT('Ctrl Pts',(2.17467900969235,-1.67810516415827,
7.50433806340446));
#408831=CARTESIAN_POINT('Ctrl Pts',(2.17438358912055,-1.67849405035301,
7.50405484070983));
#408832=CARTESIAN_POINT('Ctrl Pts',(2.17404985377076,-1.67888810850845,
7.50385766036131));
#408833=CARTESIAN_POINT('Ctrl Pts',(2.17401416596252,-1.67893024690312,
7.50383657498791));
#408834=CARTESIAN_POINT('Ctrl Pts',(2.17397806681485,-1.678972435125,7.50381643264937));
#408835=CARTESIAN_POINT('Ctrl Pts',(2.17394159952656,-1.67901463415508,
7.50379723213559));
#408836=CARTESIAN_POINT('Ctrl Pts',(2.17369816844787,-1.67929632648512,
7.50366906242519));
#408837=CARTESIAN_POINT('Ctrl Pts',(2.17343249378542,-1.67958415773683,
7.50358235568538));
#408838=CARTESIAN_POINT('Ctrl Pts',(2.17316974716839,-1.679855436059,7.5035341175365));
#408839=CARTESIAN_POINT('Ctrl Pts',(2.17277578835334,-1.68026218720031,
7.50346178989176));
#408840=CARTESIAN_POINT('Ctrl Pts',(2.17233468372927,-1.68068300819468,
7.50346967198527));
#408841=CARTESIAN_POINT('Ctrl Pts',(2.17188894406666,-1.68108279974466,
7.50354272648692));
#408842=CARTESIAN_POINT('Ctrl Pts',(2.17170560211717,-1.68124724228436,
7.50357277531559));
#408843=CARTESIAN_POINT('Ctrl Pts',(2.17152181426858,-1.68140801403177,
7.50361331098761));
#408844=CARTESIAN_POINT('Ctrl Pts',(2.17134183427341,-1.68156225994741,
7.50366116523659));
#408845=CARTESIAN_POINT('',(2.09059128324979,-1.66719091542144,7.57603338622103));
#408846=CARTESIAN_POINT('Origin',(2.09749850102558,-1.67270288713781,7.58486873427625));
#408847=CARTESIAN_POINT('Ctrl Pts',(2.17134183432944,-1.68156225995127,
7.50366116529969));
#408848=CARTESIAN_POINT('Ctrl Pts',(2.14446876028218,-1.67678045171056,
7.52783573079709));
#408849=CARTESIAN_POINT('Ctrl Pts',(2.1175531776842,-1.67199024736115,7.55196141284068));
#408850=CARTESIAN_POINT('Ctrl Pts',(2.09059128449425,-1.66719091528372,
7.57603338728831));
#408851=CARTESIAN_POINT('Ctrl Pts',(2.09047977720881,-1.65894708367393,
7.59639677331371));
#408852=CARTESIAN_POINT('Ctrl Pts',(2.07320936503687,-1.65296337419233,
7.59959882295466));
#408853=CARTESIAN_POINT('Ctrl Pts',(2.08243570482692,-1.66876158506196,
7.59642833564546));
#408854=CARTESIAN_POINT('Ctrl Pts',(2.0870472649161,-1.65709425787419,7.58707626057422));
#408855=CARTESIAN_POINT('Ctrl Pts',(2.08056667580056,-1.65907270568797,
7.58809943920599));
#408856=CARTESIAN_POINT('Ctrl Pts',(2.07997313262296,-1.66580784542589,
7.58710240504252));
#408857=CARTESIAN_POINT('Ctrl Pts',(2.08871246990533,-1.66293829112234,
7.58015376756929));
#408858=CARTESIAN_POINT('Ctrl Pts',(2.08590041445979,-1.66340905174838,
7.5820588065976));
#408859=CARTESIAN_POINT('Ctrl Pts',(2.08602293135981,-1.66622189099856,
7.58020924244128));
#408860=CARTESIAN_POINT('Ctrl Pts',(2.09059128260289,-1.6671909149053,7.57603338509286));
#408861=CARTESIAN_POINT('Ctrl Pts',(2.09059128260289,-1.6671909149053,7.57603338509286));
#408862=CARTESIAN_POINT('Ctrl Pts',(2.09059128260289,-1.6671909149053,7.57603338509286));
#408863=CARTESIAN_POINT('Origin',(2.09750205887835,-1.67269842573215,7.58486873427623));
#408864=CARTESIAN_POINT('Ctrl Pts',(2.11854867954592,-1.75475929151861,
7.51098857897448));
#408865=CARTESIAN_POINT('Ctrl Pts',(2.11626052846283,-1.74933482135159,
7.50433767179956));
#408866=CARTESIAN_POINT('Ctrl Pts',(2.12323627878781,-1.74429032350879,
7.50214974420965));
#408867=CARTESIAN_POINT('Ctrl Pts',(2.10630546116131,-1.72573455911936,
7.53887321589167));
#408868=CARTESIAN_POINT('Ctrl Pts',(2.10404472618893,-1.72037508373164,
7.53220407452062));
#408869=CARTESIAN_POINT('Ctrl Pts',(2.11096323199481,-1.71530189958989,
7.53003438070911));
#408870=CARTESIAN_POINT('Ctrl Pts',(2.09403873128106,-1.69665408852713,
7.56669465659231));
#408871=CARTESIAN_POINT('Ctrl Pts',(2.09179135683201,-1.69132628664256,
7.56004085833298));
#408872=CARTESIAN_POINT('Ctrl Pts',(2.0986660010435,-1.68625914572364,7.5578558219379));
#408873=CARTESIAN_POINT('Ctrl Pts',(2.08174904468028,-1.66751919493522,
7.59443891967696));
#408874=CARTESIAN_POINT('Ctrl Pts',(2.07949841181814,-1.66218366840122,
7.58783901202978));
#408875=CARTESIAN_POINT('Ctrl Pts',(2.08634511706896,-1.65716352844334,
7.58560008491213));
#408876=CARTESIAN_POINT('',(2.12257099619415,-1.7427189565311,7.50366116523517));
#408877=CARTESIAN_POINT('Ctrl Pts',(2.12257099619444,-1.74271895653134,
7.50366116523554));
#408878=CARTESIAN_POINT('Ctrl Pts',(2.12221815692832,-1.74338951001097,
7.50350835821027));
#408879=CARTESIAN_POINT('Ctrl Pts',(2.12187199624794,-1.74399443215018,
7.50345484956));
#408880=CARTESIAN_POINT('Ctrl Pts',(2.12152274371401,-1.74455200602683,
7.50349758195598));
#408881=CARTESIAN_POINT('Ctrl Pts',(2.12134355126286,-1.74483808277631,
7.50351950684424));
#408882=CARTESIAN_POINT('Ctrl Pts',(2.12114599266842,-1.74513996091746,
7.50357029184312));
#408883=CARTESIAN_POINT('Ctrl Pts',(2.1209474874919,-1.74542582197774,7.50365515313924));
#408884=CARTESIAN_POINT('Ctrl Pts',(2.12064210614773,-1.74586559204501,
7.50378570417639));
#408885=CARTESIAN_POINT('Ctrl Pts',(2.12032580549606,-1.74628056165416,
7.50400001621911));
#408886=CARTESIAN_POINT('Ctrl Pts',(2.12002085492926,-1.74663776925505,
7.50428903009635));
#408887=CARTESIAN_POINT('Ctrl Pts',(2.1199870077625,-1.74667741655056,7.50432110841318));
#408888=CARTESIAN_POINT('Ctrl Pts',(2.11995329730375,-1.7467163824137,7.50435406373354));
#408889=CARTESIAN_POINT('Ctrl Pts',(2.11991975139974,-1.74675464400065,
7.50438785222352));
#408890=CARTESIAN_POINT('Ctrl Pts',(2.11971493753152,-1.74698824937982,
7.50459414719561));
#408891=CARTESIAN_POINT('Ctrl Pts',(2.119512609103,-1.74719898075729,7.50483629897752));
#408892=CARTESIAN_POINT('Ctrl Pts',(2.11932146656589,-1.74737967653142,
7.5050991045531));
#408893=CARTESIAN_POINT('Ctrl Pts',(2.11889978693059,-1.74777830955832,
7.50567888004914));
#408894=CARTESIAN_POINT('Ctrl Pts',(2.11851628850652,-1.74804684943359,
7.50637912803144));
#408895=CARTESIAN_POINT('Ctrl Pts',(2.11818147603026,-1.74821436622545,
7.50710440483569));
#408896=CARTESIAN_POINT('Ctrl Pts',(2.11809937336412,-1.74825544466849,
7.50728225710685));
#408897=CARTESIAN_POINT('Ctrl Pts',(2.1180186292097,-1.74829139658335,7.50746498566954));
#408898=CARTESIAN_POINT('Ctrl Pts',(2.11794129784966,-1.74832176330876,
7.50764697238949));
#408899=CARTESIAN_POINT('Ctrl Pts',(2.11752558574023,-1.74848500646745,
7.50862528291181));
#408900=CARTESIAN_POINT('Ctrl Pts',(2.11717227348489,-1.74850551793846,
7.50965856837421));
#408901=CARTESIAN_POINT('Ctrl Pts',(2.11686727706473,-1.74844808225894,
7.51067959873201));
#408902=CARTESIAN_POINT('Ctrl Pts',(2.11669943715001,-1.74841647533206,
7.51124147302578));
#408903=CARTESIAN_POINT('Ctrl Pts',(2.11654626822342,-1.74836082893675,
7.51180065547252));
#408904=CARTESIAN_POINT('Ctrl Pts',(2.11640602292634,-1.74828929035804,
7.512351757165));
#408905=CARTESIAN_POINT('Ctrl Pts',(2.11592141955783,-1.74804209607102,
7.51425603304536));
#408906=CARTESIAN_POINT('Ctrl Pts',(2.11553609727354,-1.74757027707511,
7.5162690050518));
#408907=CARTESIAN_POINT('Ctrl Pts',(2.11524938375526,-1.74693418413987,
7.51827788969244));
#408908=CARTESIAN_POINT('Ctrl Pts',(2.11523386627784,-1.74689975758816,
7.51838661432545));
#408909=CARTESIAN_POINT('Ctrl Pts',(2.11521864057724,-1.74686484032868,
7.51849533314856));
#408910=CARTESIAN_POINT('Ctrl Pts',(2.11520370755655,-1.74682943894028,
7.51860402984325));
#408911=CARTESIAN_POINT('Ctrl Pts',(2.09059128339322,-1.66719091666627,
7.57603338728985));
#408912=CARTESIAN_POINT('Ctrl Pts',(2.10126987185163,-1.69240886705183,
7.55196141284922));
#408913=CARTESIAN_POINT('Ctrl Pts',(2.11192925636358,-1.71758369907425,
7.52783573083104));
#408914=CARTESIAN_POINT('Ctrl Pts',(2.12257099621212,-1.74271895658749,
7.50366116530176));
#408915=CARTESIAN_POINT('Origin',(7.22395927215206E-16,-5.76091528191146E-16,
7.49482233047033));
#408916=CARTESIAN_POINT('Origin',(2.16435357359296,-1.67615030903418,7.49482233047033));
#408917=CARTESIAN_POINT('Origin',(0.,0.,7.50366116523517));
#408918=CARTESIAN_POINT('Origin',(2.11573969989724,-1.73711017850876,7.49482233047033));
#408919=CARTESIAN_POINT('Ctrl Pts',(2.17370884075828,-1.67346483226476,
7.51860402984325));
#408920=CARTESIAN_POINT('Ctrl Pts',(2.18120177269763,-1.67478856070453,
7.51860402984325));
#408921=CARTESIAN_POINT('Ctrl Pts',(2.18581900259087,-1.66874062931082,
7.51860402984325));
#408922=CARTESIAN_POINT('Ctrl Pts',(2.17649101774286,-1.67395634041669,
7.51041458714365));
#408923=CARTESIAN_POINT('Ctrl Pts',(2.18229563947575,-1.67335573047827,
7.51004642900441));
#408924=CARTESIAN_POINT('Ctrl Pts',(2.18582027596805,-1.66873896136315,
7.50729136483009));
#408925=CARTESIAN_POINT('Ctrl Pts',(2.17698761422762,-1.6767271036925,7.50215815450138));
#408926=CARTESIAN_POINT('Ctrl Pts',(2.18006852915933,-1.67627320098811,
7.49877163671531));
#408927=CARTESIAN_POINT('Ctrl Pts',(2.18218107690716,-1.67354536932037,
7.49481588533172));
#408928=CARTESIAN_POINT('Ctrl Pts',(2.17134139901514,-1.68156192286894,
7.50366171572174));
#408929=CARTESIAN_POINT('Ctrl Pts',(2.17423646662283,-1.68380396341364,
7.50000045605858));
#408930=CARTESIAN_POINT('Ctrl Pts',(2.17423646662291,-1.68380396341354,
7.49482233047317));
#408931=CARTESIAN_POINT('Origin',(2.17588346167,-1.66115544463214,7.51860402984325));
#408932=CARTESIAN_POINT('Origin',(2.17588346167,-1.66115544463214,9.));
#408933=CARTESIAN_POINT('Origin',(2.17588346167,-1.66115544463214,8.75721825406948));
#408934=CARTESIAN_POINT('Ctrl Pts',(2.15726414129915,-1.67056105650534,
8.78942910404913));
#408935=CARTESIAN_POINT('Ctrl Pts',(2.16274816930576,-1.6715499273384,8.79672699501691));
#408936=CARTESIAN_POINT('Ctrl Pts',(2.16591835071274,-1.66320586143327,
8.79893251111267));
#408937=CARTESIAN_POINT('Ctrl Pts',(2.16809098556714,-1.6724728258263,8.78111911759577));
#408938=CARTESIAN_POINT('Ctrl Pts',(2.17459368527149,-1.67363781796379,
8.7864446589481));
#408939=CARTESIAN_POINT('Ctrl Pts',(2.1790310498719,-1.66685362256725,8.78817647674132));
#408940=CARTESIAN_POINT('Ctrl Pts',(2.17483853316514,-1.67366428603579,
8.76780923932034));
#408941=CARTESIAN_POINT('Ctrl Pts',(2.18251559422625,-1.67503449413487,
8.76988516158376));
#408942=CARTESIAN_POINT('Ctrl Pts',(2.18722401085122,-1.66912118767553,
8.77093053738833));
#408943=CARTESIAN_POINT('Ctrl Pts',(2.1735228537305,-1.67343196759951,8.75371302330491));
#408944=CARTESIAN_POINT('Ctrl Pts',(2.18101136169898,-1.67476929694335,
8.75300828287558));
#408945=CARTESIAN_POINT('Ctrl Pts',(2.1856261727578,-1.66867847940991,8.75267964240738));
#408946=CARTESIAN_POINT('Origin',(2.1620745043539,-1.65871710925135,8.78727029226991));
#408947=CARTESIAN_POINT('Ctrl Pts',(2.0894976077859,-1.65859511954943,8.85049129520029));
#408948=CARTESIAN_POINT('Ctrl Pts',(2.09524826125083,-1.65961054899028,
8.85711686593484));
#408949=CARTESIAN_POINT('Ctrl Pts',(2.09861675793331,-1.65175217815314,
8.85933012996512));
#408950=CARTESIAN_POINT('Ctrl Pts',(2.11299952442464,-1.66274500237873,
8.82945683644724));
#408951=CARTESIAN_POINT('Ctrl Pts',(2.11879791179024,-1.66376886049788,
8.83607469902391));
#408952=CARTESIAN_POINT('Ctrl Pts',(2.12214182911506,-1.65587264245236,
8.83829567148519));
#408953=CARTESIAN_POINT('Ctrl Pts',(2.13646640956141,-1.66688869947301,
8.80838214965002));
#408954=CARTESIAN_POINT('Ctrl Pts',(2.14228768007077,-1.66791659821434,
8.81501364461988));
#408955=CARTESIAN_POINT('Ctrl Pts',(2.14563109864249,-1.65998751473328,
8.81722098428721));
#408956=CARTESIAN_POINT('Ctrl Pts',(2.15990092504106,-1.67102668085116,
8.78727029226991));
#408957=CARTESIAN_POINT('Ctrl Pts',(2.16572316248258,-1.67205475032983,
8.79393457792714));
#408958=CARTESIAN_POINT('Ctrl Pts',(2.16908729494481,-1.66409723639929,
8.79610912703474));
#408959=CARTESIAN_POINT('Origin',(2.09167118709874,-1.64628554794962,8.85049129520029));
#408960=CARTESIAN_POINT('Ctrl Pts',(2.08196763624133,-1.66803740521006,
8.85049129520029));
#408961=CARTESIAN_POINT('Ctrl Pts',(2.08423724752594,-1.67341792347876,
8.85711686593484));
#408962=CARTESIAN_POINT('Ctrl Pts',(2.07732546348034,-1.67845061693465,
8.85933012996512));
#408963=CARTESIAN_POINT('Ctrl Pts',(2.07995974390002,-1.66327733836634,
8.86332496987231));
#408964=CARTESIAN_POINT('Ctrl Pts',(2.07730478957507,-1.66705928388541,
8.86648636486738));
#408965=CARTESIAN_POINT('Ctrl Pts',(2.07172408849994,-1.66512747711382,
8.87206031107456));
#408966=CARTESIAN_POINT('Ctrl Pts',(2.08437551637402,-1.65769067930624,
8.86341338519877));
#408967=CARTESIAN_POINT('Ctrl Pts',(2.08745862058335,-1.654231208383,8.86654584966059));
#408968=CARTESIAN_POINT('Ctrl Pts',(2.08427206792285,-1.6492342057885,8.87215952290715));
#408969=CARTESIAN_POINT('Ctrl Pts',(2.0894976077859,-1.65859511954943,8.85049129520029));
#408970=CARTESIAN_POINT('Ctrl Pts',(2.09524826125083,-1.65961054899028,
8.85711686593484));
#408971=CARTESIAN_POINT('Ctrl Pts',(2.09861675793331,-1.65175217815314,
8.85933012996512));
#408972=CARTESIAN_POINT('Origin',(2.07045035820039,-1.67289562572048,8.85049129520029));
#408973=CARTESIAN_POINT('Ctrl Pts',(2.10975372425562,-1.73390928168091,
8.78727029226991));
#408974=CARTESIAN_POINT('Ctrl Pts',(2.11205158759924,-1.73935677649344,
8.79393457792714));
#408975=CARTESIAN_POINT('Ctrl Pts',(2.10504217505423,-1.74440727656294,
8.79610912703474));
#408976=CARTESIAN_POINT('Ctrl Pts',(2.10050482043863,-1.7119831059123,8.80838214965002));
#408977=CARTESIAN_POINT('Ctrl Pts',(2.10280230216297,-1.7174296960283,8.81501364461987));
#408978=CARTESIAN_POINT('Ctrl Pts',(2.09581599798248,-1.72245367517762,
8.81722098428721));
#408979=CARTESIAN_POINT('Ctrl Pts',(2.0912431412841,-1.69002664392795,8.82945683644722));
#408980=CARTESIAN_POINT('Ctrl Pts',(2.09353159171462,-1.69545182375141,
8.8360746990239));
#408981=CARTESIAN_POINT('Ctrl Pts',(2.08657743994755,-1.70046897590161,
8.8382956714852));
#408982=CARTESIAN_POINT('Ctrl Pts',(2.08196763624133,-1.66803740521006,
8.85049129520029));
#408983=CARTESIAN_POINT('Ctrl Pts',(2.08423724752594,-1.67341792347876,
8.85711686593484));
#408984=CARTESIAN_POINT('Ctrl Pts',(2.07732546348034,-1.67845061693465,
8.85933012996512));
#408985=CARTESIAN_POINT('Origin',(2.09823644621469,-1.73876750219133,8.78727029226991));
#408986=CARTESIAN_POINT('Ctrl Pts',(2.11513172627182,-1.74665884193262,
8.75374538247848));
#408987=CARTESIAN_POINT('Ctrl Pts',(2.11809721139911,-1.75365528934166,
8.75304829418601));
#408988=CARTESIAN_POINT('Ctrl Pts',(2.1131955400215,-1.75950714895335,8.75272238421917));
#408989=CARTESIAN_POINT('Ctrl Pts',(2.11564474840766,-1.74787505129053,
8.7676940844502));
#408990=CARTESIAN_POINT('Ctrl Pts',(2.11868422291036,-1.75504782967268,
8.76974318093972));
#408991=CARTESIAN_POINT('Ctrl Pts',(2.11397434055922,-1.76094997890145,
8.7707786988043));
#408992=CARTESIAN_POINT('Ctrl Pts',(2.11301528920241,-1.74164145494495,
8.78108014887988));
#408993=CARTESIAN_POINT('Ctrl Pts',(2.11559463262245,-1.74771864383637,
8.78639403366322));
#408994=CARTESIAN_POINT('Ctrl Pts',(2.10999049148817,-1.75355950660447,
8.78812224174741));
#408995=CARTESIAN_POINT('Ctrl Pts',(2.10870618599171,-1.73142596662878,
8.78944554828685));
#408996=CARTESIAN_POINT('Ctrl Pts',(2.11088511381241,-1.73654540909541,
8.79673892988686));
#408997=CARTESIAN_POINT('Ctrl Pts',(2.10346504981595,-1.74148971942196,
8.79894799272499));
#408998=CARTESIAN_POINT('Origin',(2.10368642951562,-1.75168765945069,8.75721825406948));
#408999=CARTESIAN_POINT('Origin',(2.10368642951562,-1.75168765945069,9.));
#409000=CARTESIAN_POINT('Origin',(2.10368642951562,-1.75168765945069,7.51860402984325));
#409001=CARTESIAN_POINT('Ctrl Pts',(2.12257038820298,-1.74271845734516,
7.50366195182966));
#409002=CARTESIAN_POINT('Ctrl Pts',(2.12540061176883,-1.7450421884564,7.50000065167736));
#409003=CARTESIAN_POINT('Ctrl Pts',(2.12540061176876,-1.74504218845649,
7.49482233047108));
#409004=CARTESIAN_POINT('Ctrl Pts',(2.11910931730509,-1.74930441117483,
7.50215800491336));
#409005=CARTESIAN_POINT('Ctrl Pts',(2.11935109582767,-1.75241025088743,
7.49877273257264));
#409006=CARTESIAN_POINT('Ctrl Pts',(2.11716053191481,-1.75507831874518,
7.49481816995647));
#409007=CARTESIAN_POINT('Ctrl Pts',(2.11629948473631,-1.74942630160732,
7.51043025814042));
#409008=CARTESIAN_POINT('Ctrl Pts',(2.11700967300596,-1.75522185072786,
7.51006209594515));
#409009=CARTESIAN_POINT('Ctrl Pts',(2.11329068351776,-1.75968817890087,
7.50731281821699));
#409010=CARTESIAN_POINT('Ctrl Pts',(2.11520312005231,-1.74682804639181,
7.51860402984325));
#409011=CARTESIAN_POINT('Ctrl Pts',(2.11816136938258,-1.75383873667812,
7.51860402984324));
#409012=CARTESIAN_POINT('Ctrl Pts',(2.11329230362299,-1.75968623323814,
7.51860402984325));
#409013=CARTESIAN_POINT('Origin',(0.,0.,7.5));
#409014=CARTESIAN_POINT('Origin',(2.1845615339302,-1.5312181190179,7.5));
#409015=CARTESIAN_POINT('',(2.1845615339302,-1.5312181190179,7.59394543036555));
#409016=CARTESIAN_POINT('',(2.1845615339302,-1.5312181190179,8.85049129520029));
#409017=CARTESIAN_POINT('',(2.1845615339302,-1.5312181190179,7.5));
#409018=CARTESIAN_POINT('',(2.21651095806265,-1.59517439388233,8.78727029226991));
#409019=CARTESIAN_POINT('Ctrl Pts',(2.1845615339302,-1.5312181190179,8.85049129520029));
#409020=CARTESIAN_POINT('Ctrl Pts',(2.19522682250172,-1.55256786618582,
8.82945686509571));
#409021=CARTESIAN_POINT('Ctrl Pts',(2.20587625583215,-1.573885874373,8.80838212259895));
#409022=CARTESIAN_POINT('Ctrl Pts',(2.21651095806265,-1.59517439388233,
8.78727029226991));
#409023=CARTESIAN_POINT('',(2.22277754110618,-1.60771882366393,8.75721825406948));
#409024=CARTESIAN_POINT('Origin',(2.20391939936576,-1.56996819257488,8.75937679713147));
#409025=CARTESIAN_POINT('',(2.22277754110618,-1.60771882366393,7.51860402984325));
#409026=CARTESIAN_POINT('',(2.22277754110618,-1.60771882366393,7.5));
#409027=CARTESIAN_POINT('Ctrl Pts',(2.22277754110618,-1.60771882366393,
7.51860402984325));
#409028=CARTESIAN_POINT('Ctrl Pts',(2.21785611476351,-1.59786712509835,
7.52834476460825));
#409029=CARTESIAN_POINT('Ctrl Pts',(2.21293149350188,-1.58800903095222,
7.53807742314407));
#409030=CARTESIAN_POINT('Ctrl Pts',(2.20800357004763,-1.57814432648541,
7.54780169004674));
#409031=CARTESIAN_POINT('Ctrl Pts',(2.20019800562762,-1.56251916775177,
7.5632044032688));
#409032=CARTESIAN_POINT('Ctrl Pts',(2.19238414650717,-1.54687740470819,
7.57858609112103));
#409033=CARTESIAN_POINT('Ctrl Pts',(2.1845615339302,-1.5312181190179,7.59394543036555));
#409034=CARTESIAN_POINT('Origin',(2.46478898834977,-1.55168238962917,7.5));
#409035=CARTESIAN_POINT('',(2.27646303399421,-1.53075663254066,8.75721825406948));
#409036=CARTESIAN_POINT('',(2.26252622397769,-1.52920804991437,8.78727029226991));
#409037=CARTESIAN_POINT('Origin',(2.22714940198636,-1.5252771696165,8.75658640621103));
#409038=CARTESIAN_POINT('',(2.19147106502126,-1.52131278661253,8.85049129520029));
#409039=CARTESIAN_POINT('Ctrl Pts',(2.26252622397769,-1.52920804991437,
8.78727029226991));
#409040=CARTESIAN_POINT('Ctrl Pts',(2.23887476615141,-1.52658002839203,
8.80838212259895));
#409041=CARTESIAN_POINT('Ctrl Pts',(2.21519054652502,-1.52394836655642,
8.82945686509571));
#409042=CARTESIAN_POINT('Ctrl Pts',(2.19147106502126,-1.52131278661253,
8.85049129520029));
#409043=CARTESIAN_POINT('',(2.19147106502126,-1.52131278661253,7.59394543036555));
#409044=CARTESIAN_POINT('',(2.19147106502126,-1.52131278661253,7.5));
#409045=CARTESIAN_POINT('',(2.27646303399421,-1.53075663254066,7.51860402984325));
#409046=CARTESIAN_POINT('Ctrl Pts',(2.19147106502125,-1.52131278661253,
7.59394543036555));
#409047=CARTESIAN_POINT('Ctrl Pts',(2.20886846717181,-1.52324589143932,
7.57858609112103));
#409048=CARTESIAN_POINT('Ctrl Pts',(2.22624640173356,-1.5251768331334,7.56320440326857));
#409049=CARTESIAN_POINT('Ctrl Pts',(2.2436058889753,-1.52710572506146,7.54780169004651));
#409050=CARTESIAN_POINT('Ctrl Pts',(2.25456553516222,-1.52832350141452,
7.53807742314383));
#409051=CARTESIAN_POINT('Ctrl Pts',(2.26551783731019,-1.52954046173787,
7.52834476460825));
#409052=CARTESIAN_POINT('Ctrl Pts',(2.27646303399421,-1.53075663254066,
7.51860402984325));
#409053=CARTESIAN_POINT('',(2.27646303399421,-1.53075663254066,7.5));
#409054=CARTESIAN_POINT('Origin',(2.19071182494584,-1.52814573469575,7.5));
#409055=CARTESIAN_POINT('Ctrl Pts',(2.19147106502126,-1.52131278661253,
8.85049129520029));
#409056=CARTESIAN_POINT('Ctrl Pts',(2.19127858807353,-1.52129139961961,
8.85097269580138));
#409057=CARTESIAN_POINT('Ctrl Pts',(2.19108761066505,-1.52127864242605,
8.85143669361005));
#409058=CARTESIAN_POINT('Ctrl Pts',(2.19088928063142,-1.52127479994581,
8.8519052845931));
#409059=CARTESIAN_POINT('Ctrl Pts',(2.19050135966329,-1.52126728429814,
8.85282181883899));
#409060=CARTESIAN_POINT('Ctrl Pts',(2.19009528511056,-1.52129426370401,
8.85372622499636));
#409061=CARTESIAN_POINT('Ctrl Pts',(2.18966570712696,-1.52137154633668,
8.85462257735071));
#409062=CARTESIAN_POINT('Ctrl Pts',(2.18930908674214,-1.52143570363351,
8.85536669723986));
#409063=CARTESIAN_POINT('Ctrl Pts',(2.18893618151326,-1.52153451208308,
8.85610498449051));
#409064=CARTESIAN_POINT('Ctrl Pts',(2.18854594865094,-1.5216847600764,8.85681338218371));
#409065=CARTESIAN_POINT('Ctrl Pts',(2.18819181171551,-1.52182111036631,
8.85745625420284));
#409066=CARTESIAN_POINT('Ctrl Pts',(2.18781874712326,-1.52200097601186,
8.85808743050666));
#409067=CARTESIAN_POINT('Ctrl Pts',(2.18742683720688,-1.52225295490406,
8.85866804508411));
#409068=CARTESIAN_POINT('Ctrl Pts',(2.18724601846703,-1.52236921250269,
8.85893592806396));
#409069=CARTESIAN_POINT('Ctrl Pts',(2.18706121773651,-1.52250106139574,
8.85919241173848));
#409070=CARTESIAN_POINT('Ctrl Pts',(2.18687285743163,-1.52265285170285,
8.85943017985534));
#409071=CARTESIAN_POINT('Ctrl Pts',(2.18661851525943,-1.5228578135522,8.8597512372));
#409072=CARTESIAN_POINT('Ctrl Pts',(2.18635161117299,-1.52310485014257,
8.86004599534706));
#409073=CARTESIAN_POINT('Ctrl Pts',(2.18608242652935,-1.52339863699003,
8.86026130871721));
#409074=CARTESIAN_POINT('Ctrl Pts',(2.18598387044219,-1.52350620063761,
8.86034014101235));
#409075=CARTESIAN_POINT('Ctrl Pts',(2.18588351913952,-1.52362163854733,
8.86040910639692));
#409076=CARTESIAN_POINT('Ctrl Pts',(2.18578436050157,-1.52374202636576,
8.86046313645506));
#409077=CARTESIAN_POINT('Ctrl Pts',(2.1856296242775,-1.52392989054817,8.86054744990829));
#409078=CARTESIAN_POINT('Ctrl Pts',(2.18547368201657,-1.52413503003227,
8.86059655985668));
#409079=CARTESIAN_POINT('Ctrl Pts',(2.18532630154898,-1.52434411130867,
8.86059725258815));
#409080=CARTESIAN_POINT('Ctrl Pts',(2.18517858057362,-1.52455367564634,
8.86059794692011));
#409081=CARTESIAN_POINT('Ctrl Pts',(2.18503999426283,-1.52477105478738,
8.86056369958366));
#409082=CARTESIAN_POINT('Ctrl Pts',(2.18491492808123,-1.52498236981286,
8.86048590497774));
#409083=CARTESIAN_POINT('Ctrl Pts',(2.1848822895315,-1.5250375167429,8.86046560290182));
#409084=CARTESIAN_POINT('Ctrl Pts',(2.18485022511723,-1.52509301423802,
8.86044257503091));
#409085=CARTESIAN_POINT('Ctrl Pts',(2.18481969723215,-1.52514713095777,
8.86041778462583));
#409086=CARTESIAN_POINT('Ctrl Pts',(2.18461428244747,-1.52551126932846,
8.86025097596201));
#409087=CARTESIAN_POINT('Ctrl Pts',(2.18445116098596,-1.52586191704486,
8.8599848982295));
#409088=CARTESIAN_POINT('Ctrl Pts',(2.1843274119972,-1.52618526598101,8.85968173251462));
#409089=CARTESIAN_POINT('Ctrl Pts',(2.18426195587212,-1.52635629904255,
8.85952137522077));
#409090=CARTESIAN_POINT('Ctrl Pts',(2.18420607533322,-1.52652292297255,
8.85934740853961));
#409091=CARTESIAN_POINT('Ctrl Pts',(2.1841590845445,-1.52668229371293,8.8591675900182));
#409092=CARTESIAN_POINT('Ctrl Pts',(2.18397039210248,-1.52732225007479,
8.85844552518694));
#409093=CARTESIAN_POINT('Ctrl Pts',(2.18391147471059,-1.52788056619921,
8.85759444184122));
#409094=CARTESIAN_POINT('Ctrl Pts',(2.1839043249383,-1.52834010198266,8.85683498915136));
#409095=CARTESIAN_POINT('Ctrl Pts',(2.18390357673367,-1.52838819117855,
8.85675551444997));
#409096=CARTESIAN_POINT('Ctrl Pts',(2.18390341508028,-1.52843519502016,
8.8566769979365));
#409097=CARTESIAN_POINT('Ctrl Pts',(2.18390376336045,-1.52848109083083,
8.85659965593547));
#409098=CARTESIAN_POINT('Ctrl Pts',(2.18390846446408,-1.52910059482533,
8.85555568965886));
#409099=CARTESIAN_POINT('Ctrl Pts',(2.18400245115095,-1.52969529761313,
8.85434650606346));
#409100=CARTESIAN_POINT('Ctrl Pts',(2.18418004948776,-1.5302691092042,8.85297329937117));
#409101=CARTESIAN_POINT('Ctrl Pts',(2.18427993773099,-1.53059184326132,
8.85220095427747));
#409102=CARTESIAN_POINT('Ctrl Pts',(2.18440661731195,-1.53090800733084,
8.85137579139183));
#409103=CARTESIAN_POINT('Ctrl Pts',(2.1845615339302,-1.5312181190179,8.85049129520029));
#409104=CARTESIAN_POINT('Origin',(2.19071182494584,-1.52814573469575,7.59394543036555));
#409105=CARTESIAN_POINT('Ctrl Pts',(2.19091223951051,-1.52125069295724,
7.59443877723642));
#409106=CARTESIAN_POINT('Ctrl Pts',(2.18515687443732,-1.52061118805262,
7.58783886950016));
#409107=CARTESIAN_POINT('Ctrl Pts',(2.18229230418496,-1.5286032728123,7.58559994247159));
#409108=CARTESIAN_POINT('Ctrl Pts',(2.22233060858982,-1.52474173146927,
7.56670252222138));
#409109=CARTESIAN_POINT('Ctrl Pts',(2.21658356165311,-1.52410315083086,
7.56004874999025));
#409110=CARTESIAN_POINT('Ctrl Pts',(2.21368190515091,-1.53213538257544,
7.55786368756704));
#409111=CARTESIAN_POINT('Ctrl Pts',(2.25369030700393,-1.52822625081568,
7.53888913333558));
#409112=CARTESIAN_POINT('Ctrl Pts',(2.24790910508592,-1.52758387506119,
7.53222002137278));
#409113=CARTESIAN_POINT('Ctrl Pts',(2.24501413171017,-1.53565986254719,
7.53005029815327));
#409114=CARTESIAN_POINT('Ctrl Pts',(2.28498991570529,-1.5317040933196,7.51101258149734));
#409115=CARTESIAN_POINT('Ctrl Pts',(2.27913863511533,-1.53105393080376,
7.5043616886572));
#409116=CARTESIAN_POINT('Ctrl Pts',(2.2762874265759,-1.53917662071594,7.50217374673251));
#409117=CARTESIAN_POINT('',(2.27461864350413,-1.53898896096134,7.50366116523517));
#409118=CARTESIAN_POINT('Ctrl Pts',(2.27646303399421,-1.53075663254066,
7.51860402984325));
#409119=CARTESIAN_POINT('Ctrl Pts',(2.27690194403195,-1.53080540183996,
7.51734760759493));
#409120=CARTESIAN_POINT('Ctrl Pts',(2.27729199148658,-1.53090860476198,
7.51608817408573));
#409121=CARTESIAN_POINT('Ctrl Pts',(2.2776288635254,-1.53107891334168,7.51481005913119));
#409122=CARTESIAN_POINT('Ctrl Pts',(2.27793401026798,-1.53123318292282,
7.51365231206383));
#409123=CARTESIAN_POINT('Ctrl Pts',(2.27819606868182,-1.53144250802903,
7.51247773061042));
#409124=CARTESIAN_POINT('Ctrl Pts',(2.27838745892558,-1.53173211745976,
7.51129758471022));
#409125=CARTESIAN_POINT('Ctrl Pts',(2.27862533514098,-1.53209206890751,
7.50983079813402));
#409126=CARTESIAN_POINT('Ctrl Pts',(2.27873558770848,-1.53257173404271,
7.50839324291155));
#409127=CARTESIAN_POINT('Ctrl Pts',(2.27863867677663,-1.53319308108102,
7.50715379678855));
#409128=CARTESIAN_POINT('Ctrl Pts',(2.27859390671853,-1.53348012550903,
7.50658120839351));
#409129=CARTESIAN_POINT('Ctrl Pts',(2.27848917168156,-1.53383674900995,
7.50598221009429));
#409130=CARTESIAN_POINT('Ctrl Pts',(2.27830513945914,-1.53424805484197,
7.50545747549611));
#409131=CARTESIAN_POINT('Ctrl Pts',(2.27820693416892,-1.53446754036504,
7.50517746087247));
#409132=CARTESIAN_POINT('Ctrl Pts',(2.27808526799905,-1.53470506004887,
7.50491486231392));
#409133=CARTESIAN_POINT('Ctrl Pts',(2.2779418782926,-1.53495356351541,7.50468370960992));
#409134=CARTESIAN_POINT('Ctrl Pts',(2.27772746545173,-1.53532515458387,
7.50433806340446));
#409135=CARTESIAN_POINT('Ctrl Pts',(2.27745756787722,-1.53573216943124,
7.50405484070983));
#409136=CARTESIAN_POINT('Ctrl Pts',(2.2771497656152,-1.53614680044922,7.5038576603613));
#409137=CARTESIAN_POINT('Ctrl Pts',(2.27711685094761,-1.53619113879176,
7.5038365749879));
#409138=CARTESIAN_POINT('Ctrl Pts',(2.27708352897818,-1.53623555321374,
7.50381643264937));
#409139=CARTESIAN_POINT('Ctrl Pts',(2.27704984031698,-1.53628000200856,
7.50379723213559));
#409140=CARTESIAN_POINT('Ctrl Pts',(2.2768249574831,-1.53657671225426,7.50366906242519));
#409141=CARTESIAN_POINT('Ctrl Pts',(2.27657827008935,-1.53688097395986,
7.50358235568538));
#409142=CARTESIAN_POINT('Ctrl Pts',(2.27633344417521,-1.53716852914518,
7.5035341175365));
#409143=CARTESIAN_POINT('Ctrl Pts',(2.2759663554259,-1.53759968560059,7.50346178989176));
#409144=CARTESIAN_POINT('Ctrl Pts',(2.27555311919226,-1.53804790364339,
7.50346967198527));
#409145=CARTESIAN_POINT('Ctrl Pts',(2.27513391008215,-1.53847543241699,
7.50354272648692));
#409146=CARTESIAN_POINT('Ctrl Pts',(2.27496148069805,-1.53865128385089,
7.50357277531559));
#409147=CARTESIAN_POINT('Ctrl Pts',(2.27478837114253,-1.53882350060339,
7.50361331098761));
#409148=CARTESIAN_POINT('Ctrl Pts',(2.27461864350531,-1.53898896096214,
7.50366116523659));
#409149=CARTESIAN_POINT('',(2.19311322794403,-1.52982084947247,7.57603338622103));
#409150=CARTESIAN_POINT('Origin',(2.20035940734052,-1.53487894928946,7.58486873427628));
#409151=CARTESIAN_POINT('Ctrl Pts',(2.27461864356147,-1.5389889609624,7.50366116529968));
#409152=CARTESIAN_POINT('Ctrl Pts',(2.24749441162108,-1.53593874122534,
7.52783573079709));
#409153=CARTESIAN_POINT('Ctrl Pts',(2.22032722052781,-1.53288286616248,
7.55196141284068));
#409154=CARTESIAN_POINT('Ctrl Pts',(2.19311322917711,-1.5298208492553,7.57603338728831));
#409155=CARTESIAN_POINT('Ctrl Pts',(2.19247376689065,-1.52160109977801,
7.59639677331371));
#409156=CARTESIAN_POINT('Ctrl Pts',(2.1748554610499,-1.51673620357623,7.59959882295466));
#409157=CARTESIAN_POINT('Ctrl Pts',(2.1850750391811,-1.53191082170738,7.59642833564546));
#409158=CARTESIAN_POINT('Ctrl Pts',(2.18892959610601,-1.51997200262526,
7.58707626057423));
#409159=CARTESIAN_POINT('Ctrl Pts',(2.18258908164249,-1.52236159827603,
7.58809943920599));
#409160=CARTESIAN_POINT('Ctrl Pts',(2.1824282798476,-1.529120928389,7.58710240504253));
#409161=CARTESIAN_POINT('Ctrl Pts',(2.19096580824876,-1.52569733863037,
7.5801537675693));
#409162=CARTESIAN_POINT('Ctrl Pts',(2.18818969220951,-1.5263473010393,7.58205880659762));
#409163=CARTESIAN_POINT('Ctrl Pts',(2.18849217661503,-1.52914651132475,
7.58020924244127));
#409164=CARTESIAN_POINT('Ctrl Pts',(2.1931132272654,-1.52982084899883,7.57603338509286));
#409165=CARTESIAN_POINT('Ctrl Pts',(2.1931132272654,-1.52982084899883,7.57603338509286));
#409166=CARTESIAN_POINT('Ctrl Pts',(2.1931132272654,-1.52982084899883,7.57603338509286));
#409167=CARTESIAN_POINT('Origin',(2.20036267204003,-1.5348742690978,7.58486873427622));
#409168=CARTESIAN_POINT('Ctrl Pts',(2.22662370789095,-1.61541807041848,
7.51098857897448));
#409169=CARTESIAN_POINT('Ctrl Pts',(2.22399271106279,-1.61015134775044,
7.50433767179956));
#409170=CARTESIAN_POINT('Ctrl Pts',(2.2306309268741,-1.60467027651163,7.50214974420965));
#409171=CARTESIAN_POINT('Ctrl Pts',(2.21254602352189,-1.58723739814,7.53887321589165));
#409172=CARTESIAN_POINT('Ctrl Pts',(2.20994655070493,-1.58203378015628,
7.53220407452062));
#409173=CARTESIAN_POINT('Ctrl Pts',(2.21652580167462,-1.57652774922653,
7.53003438070912));
#409174=CARTESIAN_POINT('Ctrl Pts',(2.19844130480581,-1.55900260857537,
7.56669465659232));
#409175=CARTESIAN_POINT('Ctrl Pts',(2.19585719438983,-1.55382974300651,
7.56004085833299));
#409176=CARTESIAN_POINT('Ctrl Pts',(2.20239306107413,-1.54833255310514,
7.55785582193789));
#409177=CARTESIAN_POINT('Ctrl Pts',(2.18431018964266,-1.53071497867105,
7.59443891967696));
#409178=CARTESIAN_POINT('Ctrl Pts',(2.18172233258837,-1.52553461309112,
7.58783901202978));
#409179=CARTESIAN_POINT('Ctrl Pts',(2.1882333290775,-1.52008611763762,7.58560008491213));
#409180=CARTESIAN_POINT('',(2.22986633334695,-1.60314476287804,7.50366116523517));
#409181=CARTESIAN_POINT('Ctrl Pts',(2.22986633334725,-1.60314476287826,
7.50366116523554));
#409182=CARTESIAN_POINT('Ctrl Pts',(2.22955718153619,-1.60383654512325,
7.50350835821027));
#409183=CARTESIAN_POINT('Ctrl Pts',(2.22925048957459,-1.60446240297599,
7.50345484956));
#409184=CARTESIAN_POINT('Ctrl Pts',(2.22893767849838,-1.60504120794399,
7.50349758195598));
#409185=CARTESIAN_POINT('Ctrl Pts',(2.22877718321761,-1.60533817781787,
7.50351950684424));
#409186=CARTESIAN_POINT('Ctrl Pts',(2.2285993719274,-1.60565209334061,7.50357029184312));
#409187=CARTESIAN_POINT('Ctrl Pts',(2.22841958978207,-1.605950085339,7.50365515313924));
#409188=CARTESIAN_POINT('Ctrl Pts',(2.22814301204158,-1.60640851770141,
7.50378570417639));
#409189=CARTESIAN_POINT('Ctrl Pts',(2.22785394845766,-1.60684290016333,
7.50400001621911));
#409190=CARTESIAN_POINT('Ctrl Pts',(2.22757251081408,-1.60721891209279,
7.50428903009635));
#409191=CARTESIAN_POINT('Ctrl Pts',(2.2275412734009,-1.6072606465241,7.50432110841318));
#409192=CARTESIAN_POINT('Ctrl Pts',(2.22751012875532,-1.6073016921642,7.50435406373354));
#409193=CARTESIAN_POINT('Ctrl Pts',(2.22747910320326,-1.60734202443206,
7.50438785222352));
#409194=CARTESIAN_POINT('Ctrl Pts',(2.22728967729514,-1.60758827231352,
7.50459414719561));
#409195=CARTESIAN_POINT('Ctrl Pts',(2.22710126617778,-1.6078115339477,7.50483629897752));
#409196=CARTESIAN_POINT('Ctrl Pts',(2.22692209358151,-1.60800410500738,
7.5050991045531));
#409197=CARTESIAN_POINT('Ctrl Pts',(2.22652682083797,-1.60842893610696,
7.50567888004914));
#409198=CARTESIAN_POINT('Ctrl Pts',(2.22616131576143,-1.60872149506665,
7.50637912803144));
#409199=CARTESIAN_POINT('Ctrl Pts',(2.22583792403101,-1.60891011918631,
7.50710440483569));
#409200=CARTESIAN_POINT('Ctrl Pts',(2.22575862195849,-1.60895637356516,
7.50728225710685));
#409201=CARTESIAN_POINT('Ctrl Pts',(2.22568034714869,-1.60899742490869,
7.50746498566954));
#409202=CARTESIAN_POINT('Ctrl Pts',(2.225605120277,-1.60903268387966,7.50764697238949));
#409203=CARTESIAN_POINT('Ctrl Pts',(2.22520072131776,-1.60922222640407,
7.50862528291182));
#409204=CARTESIAN_POINT('Ctrl Pts',(2.22484944915481,-1.60926533252598,
7.50965856837421));
#409205=CARTESIAN_POINT('Ctrl Pts',(2.22454139946588,-1.60922755604196,
7.51067959873202));
#409206=CARTESIAN_POINT('Ctrl Pts',(2.22437187933351,-1.60920676759516,
7.51124147302578));
#409207=CARTESIAN_POINT('Ctrl Pts',(2.22421545983212,-1.60916104909815,
7.51180065547253));
#409208=CARTESIAN_POINT('Ctrl Pts',(2.22407091919156,-1.60909864305016,
7.512351757165));
#409209=CARTESIAN_POINT('Ctrl Pts',(2.2235714737003,-1.60888300529474,7.51425603304536));
#409210=CARTESIAN_POINT('Ctrl Pts',(2.22315671355512,-1.60843684338508,
7.51626900505181));
#409211=CARTESIAN_POINT('Ctrl Pts',(2.22282983450622,-1.60782042716918,
7.51827788969244));
#409212=CARTESIAN_POINT('Ctrl Pts',(2.22281214319438,-1.60778706555871,
7.51838661432546));
#409213=CARTESIAN_POINT('Ctrl Pts',(2.22279471162011,-1.60775319555448,
7.51849533314857));
#409214=CARTESIAN_POINT('Ctrl Pts',(2.22277754110617,-1.60771882366394,
7.51860402984325));
#409215=CARTESIAN_POINT('Ctrl Pts',(2.19311322816693,-1.52982085070556,
7.57603338728985));
#409216=CARTESIAN_POINT('Ctrl Pts',(2.20538559594874,-1.55430280859582,
7.55196141284922));
#409217=CARTESIAN_POINT('Ctrl Pts',(2.21763603663764,-1.57874296711532,
7.52783573083105));
#409218=CARTESIAN_POINT('Ctrl Pts',(2.2298663333685,-1.60314476293316,7.50366116530176));
#409219=CARTESIAN_POINT('Origin',(7.57821998246254E-16,-5.28623820391005E-16,
7.49482233047033));
#409220=CARTESIAN_POINT('Origin',(2.26729799607038,-1.53403586888157,7.49482233047033));
#409221=CARTESIAN_POINT('Origin',(0.,0.,7.50366116523517));
#409222=CARTESIAN_POINT('Origin',(2.22268971703922,-1.59798519134819,7.49482233047033));
#409223=CARTESIAN_POINT('Ctrl Pts',(2.27646198274858,-1.53075651568693,
7.51860402984325));
#409224=CARTESIAN_POINT('Ctrl Pts',(2.28402433122799,-1.531597450587,7.51860402984325));
#409225=CARTESIAN_POINT('Ctrl Pts',(2.28824458223239,-1.52526611838201,
7.51860402984325));
#409226=CARTESIAN_POINT('Ctrl Pts',(2.27926993448757,-1.53106875929122,
7.51041458714366));
#409227=CARTESIAN_POINT('Ctrl Pts',(2.2850241487917,-1.53009747997901,7.51004642900442));
#409228=CARTESIAN_POINT('Ctrl Pts',(2.28824574612751,-1.52526437227577,
7.5072913648301));
#409229=CARTESIAN_POINT('Ctrl Pts',(2.27994303407421,-1.5338020126907,7.50215815450137));
#409230=CARTESIAN_POINT('Ctrl Pts',(2.28298853728965,-1.53315164768067,
7.4987716367153));
#409231=CARTESIAN_POINT('Ctrl Pts',(2.28492197180653,-1.53029406923673,
7.4948158853317));
#409232=CARTESIAN_POINT('Ctrl Pts',(2.27461818754463,-1.53898865246333,
7.50366171572174));
#409233=CARTESIAN_POINT('Ctrl Pts',(2.27765095495633,-1.54104059887679,
7.50000045605858));
#409234=CARTESIAN_POINT('Ctrl Pts',(2.2776509549564,-1.54104059887668,7.49482233047317));
#409235=CARTESIAN_POINT('Origin',(2.27784347049497,-1.51833309057118,7.51860402984325));
#409236=CARTESIAN_POINT('Origin',(2.27784347049497,-1.51833309057118,9.));
#409237=CARTESIAN_POINT('Origin',(2.27784347049497,-1.51833309057118,8.75721825406948));
#409238=CARTESIAN_POINT('Ctrl Pts',(2.2598650251365,-1.5289123215581,8.78942910404912));
#409239=CARTESIAN_POINT('Ctrl Pts',(2.26540114279122,-1.5295477977692,8.79672699501691));
#409240=CARTESIAN_POINT('Ctrl Pts',(2.26803020458243,-1.52101776142226,
8.79893251111267));
#409241=CARTESIAN_POINT('Ctrl Pts',(2.27079211197274,-1.53012648465001,
8.78111911759582));
#409242=CARTESIAN_POINT('Ctrl Pts',(2.27735609248566,-1.53087245378568,
8.78644465894813));
#409243=CARTESIAN_POINT('Ctrl Pts',(2.28134967515313,-1.52381789432009,
8.78817647674132));
#409244=CARTESIAN_POINT('Ctrl Pts',(2.27760213312822,-1.53088318001778,
8.76780923932029));
#409245=CARTESIAN_POINT('Ctrl Pts',(2.28535121037834,-1.53175870188637,
8.76988516158373));
#409246=CARTESIAN_POINT('Ctrl Pts',(2.28967108621072,-1.52555587566044,
8.77093053738833));
#409247=CARTESIAN_POINT('Ctrl Pts',(2.27627427220479,-1.53073563477544,
8.75371302330492));
#409248=CARTESIAN_POINT('Ctrl Pts',(2.28383307721574,-1.53159042607985,
8.75300828287559));
#409249=CARTESIAN_POINT('Ctrl Pts',(2.28804816663108,-1.52521645082456,
8.75267964240738));
#409250=CARTESIAN_POINT('Origin',(2.26390666047845,-1.5167845079449,8.78727029226991));
#409251=CARTESIAN_POINT('Ctrl Pts',(2.19147106502126,-1.52131278661253,
8.85049129520029));
#409252=CARTESIAN_POINT('Ctrl Pts',(2.19727496193954,-1.52195768411216,
8.85711686593484));
#409253=CARTESIAN_POINT('Ctrl Pts',(2.20013305013608,-1.51389963881726,
8.85933012996512));
#409254=CARTESIAN_POINT('Ctrl Pts',(2.21519057835743,-1.52394837009347,
8.82945683644721));
#409255=CARTESIAN_POINT('Ctrl Pts',(2.22104265112921,-1.52459862063228,
8.83607469902385));
#409256=CARTESIAN_POINT('Ctrl Pts',(2.2238737855901,-1.516504380695,8.83829567148519));
#409257=CARTESIAN_POINT('Ctrl Pts',(2.23887473584627,-1.52658002502469,
8.80838214965001));
#409258=CARTESIAN_POINT('Ctrl Pts',(2.24474990362954,-1.5272328417557,8.81501364461993));
#409259=CARTESIAN_POINT('Ctrl Pts',(2.24757843466632,-1.51910583586367,
8.81722098428721));
#409260=CARTESIAN_POINT('Ctrl Pts',(2.26252622397769,-1.52920804991437,
8.78727029226991));
#409261=CARTESIAN_POINT('Ctrl Pts',(2.26840236764561,-1.52986097508039,
8.79393457792714));
#409262=CARTESIAN_POINT('Ctrl Pts',(2.27124974846887,-1.52170427000876,
8.79610912703474));
#409263=CARTESIAN_POINT('Origin',(2.19285150152201,-1.50888924464306,8.85049129520029));
#409264=CARTESIAN_POINT('Ctrl Pts',(2.1845615339302,-1.5312181190179,8.85049129520029));
#409265=CARTESIAN_POINT('Ctrl Pts',(2.1871712130441,-1.53644216794048,8.85711686593484));
#409266=CARTESIAN_POINT('Ctrl Pts',(2.18059607577693,-1.54190736071218,
8.85933012996512));
#409267=CARTESIAN_POINT('Ctrl Pts',(2.18225278848926,-1.52659647834603,
8.86332496987231));
#409268=CARTESIAN_POINT('Ctrl Pts',(2.1798455991341,-1.53054075696004,8.86648636486738));
#409269=CARTESIAN_POINT('Ctrl Pts',(2.17415259292302,-1.52897047603819,
8.87206031107456));
#409270=CARTESIAN_POINT('Ctrl Pts',(2.18630154981017,-1.52073837816234,
8.86341338519876));
#409271=CARTESIAN_POINT('Ctrl Pts',(2.18915667038817,-1.51708847992823,
8.86654584966059));
#409272=CARTESIAN_POINT('Ctrl Pts',(2.18565650578641,-1.51230590734143,
8.87215952290715));
#409273=CARTESIAN_POINT('Ctrl Pts',(2.19147106502126,-1.52131278661253,
8.85049129520029));
#409274=CARTESIAN_POINT('Ctrl Pts',(2.19727496193954,-1.52195768411216,
8.85711686593484));
#409275=CARTESIAN_POINT('Ctrl Pts',(2.20013305013608,-1.51389963881726,
8.85933012996512));
#409276=CARTESIAN_POINT('Origin',(2.17337918662905,-1.5368042723309,8.85049129520029));
#409277=CARTESIAN_POINT('Ctrl Pts',(2.21651095806265,-1.59517439388233,
8.78727029226991));
#409278=CARTESIAN_POINT('Ctrl Pts',(2.21915312239058,-1.6004634716226,8.79393457792714));
#409279=CARTESIAN_POINT('Ctrl Pts',(2.21248169808586,-1.60595268950174,
8.79610912703474));
#409280=CARTESIAN_POINT('Ctrl Pts',(2.20587624220566,-1.57388584709553,
8.80838214965002));
#409281=CARTESIAN_POINT('Ctrl Pts',(2.20851796773431,-1.57917404644858,
8.81501364461994));
#409282=CARTESIAN_POINT('Ctrl Pts',(2.20186790511426,-1.58463531733956,
8.81722098428722));
#409283=CARTESIAN_POINT('Ctrl Pts',(2.19522683681494,-1.55256789483797,
8.8294568364472));
#409284=CARTESIAN_POINT('Ctrl Pts',(2.19785817784332,-1.55783530652512,
8.83607469902386));
#409285=CARTESIAN_POINT('Ctrl Pts',(2.19123976416885,-1.56328770443167,
8.83829567148519));
#409286=CARTESIAN_POINT('Ctrl Pts',(2.1845615339302,-1.5312181190179,8.85049129520029));
#409287=CARTESIAN_POINT('Ctrl Pts',(2.1871712130441,-1.53644216794048,8.85711686593484));
#409288=CARTESIAN_POINT('Ctrl Pts',(2.18059607577693,-1.54190736071218,
8.85933012996512));
#409289=CARTESIAN_POINT('Origin',(2.2053286107615,-1.60076054719533,8.78727029226991));
#409290=CARTESIAN_POINT('Ctrl Pts',(2.22269477752691,-1.60755318902288,
8.75374538247849));
#409291=CARTESIAN_POINT('Ctrl Pts',(2.22610243367153,-1.61434526219589,
8.75304829418602));
#409292=CARTESIAN_POINT('Ctrl Pts',(2.22158576323609,-1.62049914969784,
8.75272238421917));
#409293=CARTESIAN_POINT('Ctrl Pts',(2.22328466840486,-1.60873403010713,
8.76769408445016));
#409294=CARTESIAN_POINT('Ctrl Pts',(2.22677745947003,-1.61569733144681,
8.76974318093967));
#409295=CARTESIAN_POINT('Ctrl Pts',(2.22245540607675,-1.6218891172753,8.77077869880429));
#409296=CARTESIAN_POINT('Ctrl Pts',(2.22026122381642,-1.60268171138352,
8.78108014887993));
#409297=CARTESIAN_POINT('Ctrl Pts',(2.22322463452794,-1.60858115493823,
8.78639403366327));
#409298=CARTESIAN_POINT('Ctrl Pts',(2.21800623306506,-1.61476907558262,
8.78812224174741));
#409299=CARTESIAN_POINT('Ctrl Pts',(2.21530646553678,-1.59276329707431,
8.78944554828684));
#409300=CARTESIAN_POINT('Ctrl Pts',(2.21780892032158,-1.59773261671255,
8.79673892988686));
#409301=CARTESIAN_POINT('Ctrl Pts',(2.2107208846927,-1.60314217355577,8.79894799272499));
#409302=CARTESIAN_POINT('Origin',(2.21159519380502,-1.61330497697693,8.75721825406948));
#409303=CARTESIAN_POINT('Origin',(2.21159519380502,-1.61330497697693,9.));
#409304=CARTESIAN_POINT('Origin',(2.21159519380502,-1.61330497697693,7.51860402984325));
#409305=CARTESIAN_POINT('Ctrl Pts',(2.22986569462201,-1.60314430367187,
7.50366195182966));
#409306=CARTESIAN_POINT('Ctrl Pts',(2.23283898515348,-1.60528192738186,
7.50000065167735));
#409307=CARTESIAN_POINT('Ctrl Pts',(2.23283898515341,-1.60528192738195,
7.49482233047108));
#409308=CARTESIAN_POINT('Ctrl Pts',(2.22683369837613,-1.60993847752684,
7.50215800491337));
#409309=CARTESIAN_POINT('Ctrl Pts',(2.22727397197242,-1.61302244515553,
7.49877273257266));
#409310=CARTESIAN_POINT('Ctrl Pts',(2.22525885250261,-1.6158253810935,7.49481816995647));
#409311=CARTESIAN_POINT('Ctrl Pts',(2.22403744845654,-1.61024014411316,
7.51043025814042));
#409312=CARTESIAN_POINT('Ctrl Pts',(2.22511749967528,-1.6159782837378,7.51006209594513));
#409313=CARTESIAN_POINT('Ctrl Pts',(2.2216923098784,-1.62067371183517,7.50731281821699));
#409314=CARTESIAN_POINT('Ctrl Pts',(2.22277686558814,-1.60771747161814,
7.51860402984325));
#409315=CARTESIAN_POINT('Ctrl Pts',(2.22617821334675,-1.61452422200402,
7.51860402984324));
#409316=CARTESIAN_POINT('Ctrl Pts',(2.22169380199591,-1.62067166636953,
7.51860402984325));
#409317=CARTESIAN_POINT('Origin',(0.,0.,7.5));
#409318=CARTESIAN_POINT('Origin',(2.27817859968918,-1.38810672912943,7.5));
#409319=CARTESIAN_POINT('',(2.27817859968918,-1.38810672912943,7.59394543036555));
#409320=CARTESIAN_POINT('',(2.27817859968918,-1.38810672912943,8.85049129520029));
#409321=CARTESIAN_POINT('',(2.27817859968918,-1.38810672912943,7.5));
#409322=CARTESIAN_POINT('',(2.3141600729029,-1.44988459233544,8.78727029226991));
#409323=CARTESIAN_POINT('Ctrl Pts',(2.27817859968918,-1.38810672912943,
8.85049129520029));
#409324=CARTESIAN_POINT('Ctrl Pts',(2.29018985827907,-1.40872928356711,
8.82945686509571));
#409325=CARTESIAN_POINT('Ctrl Pts',(2.30218326068068,-1.42932118008398,
8.80838212259896));
#409326=CARTESIAN_POINT('Ctrl Pts',(2.3141600729029,-1.44988459233544,8.78727029226991));
#409327=CARTESIAN_POINT('',(2.32121750495511,-1.46200174688655,8.75721825406948));
#409328=CARTESIAN_POINT('Origin',(2.29997941805042,-1.42553692380631,8.75937679713093));
#409329=CARTESIAN_POINT('',(2.32121750495511,-1.46200174688655,7.51860402984325));
#409330=CARTESIAN_POINT('',(2.32121750495511,-1.46200174688655,7.5));
#409331=CARTESIAN_POINT('Ctrl Pts',(2.32121750495511,-1.46200174688655,
7.51860402984325));
#409332=CARTESIAN_POINT('Ctrl Pts',(2.3156749897164,-1.45248560656066,7.52834476460825));
#409333=CARTESIAN_POINT('Ctrl Pts',(2.31012887635679,-1.44296328849378,
7.53807742314407));
#409334=CARTESIAN_POINT('Ctrl Pts',(2.30457904406456,-1.43343458526004,
7.54780169004674));
#409335=CARTESIAN_POINT('Ctrl Pts',(2.2957884096565,-1.41834163432028,7.5632044032688));
#409336=CARTESIAN_POINT('Ctrl Pts',(2.28698843374856,-1.4032326446292,7.57858609112103));
#409337=CARTESIAN_POINT('Ctrl Pts',(2.27817859968918,-1.38810672912943,
7.59394543036555));
#409338=CARTESIAN_POINT('Origin',(2.55914144706916,-1.39057471905265,7.5));
#409339=CARTESIAN_POINT('',(2.36986171072479,-1.3817580415,8.75721825406948));
#409340=CARTESIAN_POINT('',(2.35585431734964,-1.38110557508639,8.78727029226991));
#409341=CARTESIAN_POINT('Origin',(2.32029832846392,-1.3794493719707,8.7565864062096));
#409342=CARTESIAN_POINT('',(2.28443929758137,-1.37777905311488,8.85049129520029));
#409343=CARTESIAN_POINT('Ctrl Pts',(2.35585431734964,-1.38110557508639,
8.78727029226991));
#409344=CARTESIAN_POINT('Ctrl Pts',(2.33208307606304,-1.37999830722192,
8.80838212259897));
#409345=CARTESIAN_POINT('Ctrl Pts',(2.30827890705326,-1.37888950557933,
8.82945686509571));
#409346=CARTESIAN_POINT('Ctrl Pts',(2.28443929758137,-1.37777905311488,
8.85049129520029));
#409347=CARTESIAN_POINT('',(2.28443929758137,-1.37777905311488,7.59394543036555));
#409348=CARTESIAN_POINT('',(2.28443929758137,-1.37777905311488,7.5));
#409349=CARTESIAN_POINT('',(2.36986171072479,-1.3817580415,7.51860402984325));
#409350=CARTESIAN_POINT('Ctrl Pts',(2.28443929758137,-1.37777905311488,
7.59394543036555));
#409351=CARTESIAN_POINT('Ctrl Pts',(2.30192480935484,-1.37859353078759,
7.57858609112103));
#409352=CARTESIAN_POINT('Ctrl Pts',(2.31939075494536,-1.37940709706468,
7.56320440326856));
#409353=CARTESIAN_POINT('Ctrl Pts',(2.33683815978891,-1.38021979971107,
7.54780169004651));
#409354=CARTESIAN_POINT('Ctrl Pts',(2.34785331140615,-1.38073288706991,
7.53807742314383));
#409355=CARTESIAN_POINT('Ctrl Pts',(2.35886108179036,-1.38124563060984,
7.52834476460825));
#409356=CARTESIAN_POINT('Ctrl Pts',(2.36986171072479,-1.3817580415,7.51860402984325));
#409357=CARTESIAN_POINT('',(2.36986171072479,-1.3817580415,7.5));
#409358=CARTESIAN_POINT('Origin',(2.28411940593293,-1.38464660685207,7.5));
#409359=CARTESIAN_POINT('Ctrl Pts',(2.28443929758137,-1.37777905311488,
8.85049129520029));
#409360=CARTESIAN_POINT('Ctrl Pts',(2.28424584582883,-1.3777700421042,8.85097269580138));
#409361=CARTESIAN_POINT('Ctrl Pts',(2.28405444344772,-1.37776954708624,
8.85143669361005));
#409362=CARTESIAN_POINT('Ctrl Pts',(2.28385627471587,-1.37777841954967,
8.8519052845931));
#409363=CARTESIAN_POINT('Ctrl Pts',(2.28346866924377,-1.37779577352546,
8.85282181883899));
#409364=CARTESIAN_POINT('Ctrl Pts',(2.28306515759124,-1.37784871478518,
8.85372622499635));
#409365=CARTESIAN_POINT('Ctrl Pts',(2.28264141373695,-1.3779533617883,8.8546225773507));
#409366=CARTESIAN_POINT('Ctrl Pts',(2.28228963663908,-1.37804023601358,
8.85536669723986));
#409367=CARTESIAN_POINT('Ctrl Pts',(2.28192382826309,-1.37816273357065,
8.85610498449051));
#409368=CARTESIAN_POINT('Ctrl Pts',(2.28154402359801,-1.37833767516868,
8.85681338218371));
#409369=CARTESIAN_POINT('Ctrl Pts',(2.28119935026796,-1.37849643494365,
8.85745625420285));
#409370=CARTESIAN_POINT('Ctrl Pts',(2.28083857620841,-1.37869983336644,
8.85808743050666));
#409371=CARTESIAN_POINT('Ctrl Pts',(2.28046361585604,-1.37897640429554,
8.85866804508411));
#409372=CARTESIAN_POINT('Ctrl Pts',(2.2802906172776,-1.3791040081269,8.85893592806396));
#409373=CARTESIAN_POINT('Ctrl Pts',(2.28011464382758,-1.37924742634571,
8.85919241173848));
#409374=CARTESIAN_POINT('Ctrl Pts',(2.27993639576752,-1.37941097306953,
8.85943017985534));
#409375=CARTESIAN_POINT('Ctrl Pts',(2.27969570811936,-1.3796318095617,8.8597512372));
#409376=CARTESIAN_POINT('Ctrl Pts',(2.27944518010468,-1.37989543919243,
8.86004599534705));
#409377=CARTESIAN_POINT('Ctrl Pts',(2.2791953715177,-1.38020586914263,8.86026130871721));
#409378=CARTESIAN_POINT('Ctrl Pts',(2.27910390955116,-1.38031952629935,
8.86034014101235));
#409379=CARTESIAN_POINT('Ctrl Pts',(2.27901116056327,-1.38044115655954,
8.86040910639692));
#409380=CARTESIAN_POINT('Ctrl Pts',(2.27891991893139,-1.38056765014403,
8.86046313645506));
#409381=CARTESIAN_POINT('Ctrl Pts',(2.27877753712898,-1.38076504232325,
8.86054744990829));
#409382=CARTESIAN_POINT('Ctrl Pts',(2.27863505860003,-1.38097975158124,
8.86059655985668));
#409383=CARTESIAN_POINT('Ctrl Pts',(2.27850137682478,-1.38119784597671,
8.86059725258816));
#409384=CARTESIAN_POINT('Ctrl Pts',(2.27836738619123,-1.38141644425736,
8.86059794692011));
#409385=CARTESIAN_POINT('Ctrl Pts',(2.27824301215027,-1.38164225602506,
8.86056369958366));
#409386=CARTESIAN_POINT('Ctrl Pts',(2.27813174193072,-1.38186114989892,
8.86048590497774));
#409387=CARTESIAN_POINT('Ctrl Pts',(2.27810270371633,-1.38191827468275,
8.86046560290182));
#409388=CARTESIAN_POINT('Ctrl Pts',(2.27807426091855,-1.38197571252638,
8.86044257503091));
#409389=CARTESIAN_POINT('Ctrl Pts',(2.27804726302642,-1.38203167398584,
8.86041778462583));
#409390=CARTESIAN_POINT('Ctrl Pts',(2.27786560071396,-1.38240822516564,
8.86025097596201));
#409391=CARTESIAN_POINT('Ctrl Pts',(2.27772528047932,-1.38276860366661,
8.8599848982295));
#409392=CARTESIAN_POINT('Ctrl Pts',(2.2776225027836,-1.38309921687263,8.85968173251461));
#409393=CARTESIAN_POINT('Ctrl Pts',(2.27756813927102,-1.38327409231674,
8.85952137522076));
#409394=CARTESIAN_POINT('Ctrl Pts',(2.27752304917653,-1.38344395417843,
8.85934740853961));
#409395=CARTESIAN_POINT('Ctrl Pts',(2.27748636585382,-1.38360600818469,
8.8591675900182));
#409396=CARTESIAN_POINT('Ctrl Pts',(2.27733906324554,-1.38425673925384,
8.85844552518695));
#409397=CARTESIAN_POINT('Ctrl Pts',(2.27731603834266,-1.38481768310816,
8.85759444184124));
#409398=CARTESIAN_POINT('Ctrl Pts',(2.27733834581908,-1.38527673281353,
8.85683498915138));
#409399=CARTESIAN_POINT('Ctrl Pts',(2.27734068023708,-1.38532477114265,
8.85675551444998));
#409400=CARTESIAN_POINT('Ctrl Pts',(2.27734353046229,-1.385371688767,8.85667699793651));
#409401=CARTESIAN_POINT('Ctrl Pts',(2.27734681858158,-1.38541746796543,
8.85659965593547));
#409402=CARTESIAN_POINT('Ctrl Pts',(2.27739120178349,-1.38603539792178,
8.85555568965886));
#409403=CARTESIAN_POINT('Ctrl Pts',(2.27752309810307,-1.38662285708122,
8.85434650606346));
#409404=CARTESIAN_POINT('Ctrl Pts',(2.27773709577991,-1.38718411095032,
8.85297329937117));
#409405=CARTESIAN_POINT('Ctrl Pts',(2.27785745643407,-1.38749978205399,
8.85220095427747));
#409406=CARTESIAN_POINT('Ctrl Pts',(2.27800413243973,-1.38780718014191,
8.85137579139183));
#409407=CARTESIAN_POINT('Ctrl Pts',(2.27817859968918,-1.38810672912943,
8.85049129520029));
#409408=CARTESIAN_POINT('Origin',(2.28411940593293,-1.38464660685207,7.59394543036555));
#409409=CARTESIAN_POINT('Ctrl Pts',(2.28387764188342,-1.37775289111106,
7.59443877723642));
#409410=CARTESIAN_POINT('Ctrl Pts',(2.27809312860512,-1.37748344764416,
7.58783886950016));
#409411=CARTESIAN_POINT('Ctrl Pts',(2.27574649854822,-1.38564264545478,
7.58559994247159));
#409412=CARTESIAN_POINT('Ctrl Pts',(2.31545513015925,-1.37922377509171,
7.56670252222136));
#409413=CARTESIAN_POINT('Ctrl Pts',(2.30967897714493,-1.37895472104715,
7.5600487499903));
#409414=CARTESIAN_POINT('Ctrl Pts',(2.30729790926198,-1.38715635948058,
7.55786368756705));
#409415=CARTESIAN_POINT('Ctrl Pts',(2.34697365063072,-1.38069191234348,
7.53888913333557));
#409416=CARTESIAN_POINT('Ctrl Pts',(2.34116316965616,-1.38042125929753,
7.53222002137276));
#409417=CARTESIAN_POINT('Ctrl Pts',(2.33879157460851,-1.38866613538211,
7.53005029815326));
#409418=CARTESIAN_POINT('Ctrl Pts',(2.37843177706342,-1.38215723643218,
7.51101258149734));
#409419=CARTESIAN_POINT('Ctrl Pts',(2.37255086250157,-1.38188330257953,
7.5043616886572));
#409420=CARTESIAN_POINT('Ctrl Pts',(2.37022593460538,-1.39017198111245,
7.50217374673251));
#409421=CARTESIAN_POINT('',(2.36854855682565,-1.39009162622346,7.50366116523517));
#409422=CARTESIAN_POINT('Ctrl Pts',(2.36986171072479,-1.3817580415,7.51860402984325));
#409423=CARTESIAN_POINT('Ctrl Pts',(2.37030284363452,-1.38177858953488,
7.51734760759493));
#409424=CARTESIAN_POINT('Ctrl Pts',(2.37069870192874,-1.3818565899892,7.51608817408572));
#409425=CARTESIAN_POINT('Ctrl Pts',(2.37104579353599,-1.38200496518603,
7.51481005913119));
#409426=CARTESIAN_POINT('Ctrl Pts',(2.37136019740786,-1.38213936698485,
7.51365231206383));
#409427=CARTESIAN_POINT('Ctrl Pts',(2.37163512890018,-1.38233147186995,
7.51247773061042));
#409428=CARTESIAN_POINT('Ctrl Pts',(2.37184468125209,-1.38260822385203,
7.51129758471022));
#409429=CARTESIAN_POINT('Ctrl Pts',(2.37210513089374,-1.38295219495948,
7.50983079813402));
#409430=CARTESIAN_POINT('Ctrl Pts',(2.37224588918625,-1.38342381066495,
7.50839324291155));
#409431=CARTESIAN_POINT('Ctrl Pts',(2.37218898720973,-1.38405009018386,
7.50715379678855));
#409432=CARTESIAN_POINT('Ctrl Pts',(2.37216270013616,-1.38433941327578,
7.50658120839351));
#409433=CARTESIAN_POINT('Ctrl Pts',(2.37208102923471,-1.38470201445232,
7.50598221009429));
#409434=CARTESIAN_POINT('Ctrl Pts',(2.37192372758136,-1.38512426619737,
7.50545747549611));
#409435=CARTESIAN_POINT('Ctrl Pts',(2.37183978655019,-1.38534959279844,
7.50517746087247));
#409436=CARTESIAN_POINT('Ctrl Pts',(2.37173358829491,-1.38559441965088,
7.50491486231392));
#409437=CARTESIAN_POINT('Ctrl Pts',(2.37160641486976,-1.38585159955043,
7.50468370960993));
#409438=CARTESIAN_POINT('Ctrl Pts',(2.37141625048457,-1.38623616462306,
7.50433806340447));
#409439=CARTESIAN_POINT('Ctrl Pts',(2.37117298497438,-1.38665963561174,
7.50405484070984));
#409440=CARTESIAN_POINT('Ctrl Pts',(2.37089238062566,-1.38709313568445,
7.50385766036131));
#409441=CARTESIAN_POINT('Ctrl Pts',(2.37086237435214,-1.38713949177911,
7.50383657498791));
#409442=CARTESIAN_POINT('Ctrl Pts',(2.37083196648805,-1.38718594989282,
7.50381643264937));
#409443=CARTESIAN_POINT('Ctrl Pts',(2.37080119488787,-1.38723246580277,
7.50379723213559));
#409444=CARTESIAN_POINT('Ctrl Pts',(2.37059578439061,-1.38754297471808,
7.50366906242519));
#409445=CARTESIAN_POINT('Ctrl Pts',(2.37036909795698,-1.38786241660096,
7.50358235568538));
#409446=CARTESIAN_POINT('Ctrl Pts',(2.37014319878791,-1.38816506702348,
7.5035341175365));
#409447=CARTESIAN_POINT('Ctrl Pts',(2.36980448855075,-1.38861885707863,
7.50346178989176));
#409448=CARTESIAN_POINT('Ctrl Pts',(2.36942081878388,-1.38909263034579,
7.50346967198527));
#409449=CARTESIAN_POINT('Ctrl Pts',(2.36902986284642,-1.38954613953558,
7.50354272648692));
#409450=CARTESIAN_POINT('Ctrl Pts',(2.36886905457703,-1.38973267725242,
7.50357277531559));
#409451=CARTESIAN_POINT('Ctrl Pts',(2.36870733465888,-1.38991563133443,
7.50361331098761));
#409452=CARTESIAN_POINT('Ctrl Pts',(2.36854855682688,-1.39009162622418,
7.50366116523659));
#409453=CARTESIAN_POINT('',(2.28662319996335,-1.38616442150747,7.57603338622103));
#409454=CARTESIAN_POINT('Origin',(2.294178564875,-1.39074786460788,7.58486873427628));
#409455=CARTESIAN_POINT('Ctrl Pts',(2.36854855688294,-1.39009162622084,
7.50366116529968));
#409456=CARTESIAN_POINT('Ctrl Pts',(2.34128462633659,-1.3887855289946,7.52783573079709));
#409457=CARTESIAN_POINT('Ctrl Pts',(2.31397746256358,-1.38747654046439,
7.55196141284068));
#409458=CARTESIAN_POINT('Ctrl Pts',(2.28662320117998,-1.38616442121175,
7.57603338728831));
#409459=CARTESIAN_POINT('Ctrl Pts',(2.28545841158025,-1.3780025305807,7.5963967733137));
#409460=CARTESIAN_POINT('Ctrl Pts',(2.26756460946825,-1.3742764385605,7.59959882295475));
#409461=CARTESIAN_POINT('Ctrl Pts',(2.27873543150217,-1.38876510819256,
7.59642833564546));
#409462=CARTESIAN_POINT('Ctrl Pts',(2.28181714606166,-1.37660385638453,
7.58707626057419));
#409463=CARTESIAN_POINT('Ctrl Pts',(2.27564276078405,-1.3793947805112,7.58809943920599));
#409464=CARTESIAN_POINT('Ctrl Pts',(2.27591536114095,-1.38615052546194,
7.58710240504253));
#409465=CARTESIAN_POINT('Ctrl Pts',(2.28421599812538,-1.38218696851294,
7.58015376756929));
#409466=CARTESIAN_POINT('Ctrl Pts',(2.28148722914879,-1.3830134618697,7.58205880659763));
#409467=CARTESIAN_POINT('Ctrl Pts',(2.28196843808642,-1.38578754063506,
7.58020924244125));
#409468=CARTESIAN_POINT('Ctrl Pts',(2.28662319925576,-1.38616442107829,
7.57603338509286));
#409469=CARTESIAN_POINT('Ctrl Pts',(2.28662319925576,-1.38616442107829,
7.57603338509286));
#409470=CARTESIAN_POINT('Ctrl Pts',(2.28662319925576,-1.38616442107829,
7.57603338509286));
#409471=CARTESIAN_POINT('Origin',(2.29418152300587,-1.3907429848622,7.58486873427622));
#409472=CARTESIAN_POINT('Ctrl Pts',(2.32554906181098,-1.46943874996092,
7.51098857897448));
#409473=CARTESIAN_POINT('Ctrl Pts',(2.32258603056805,-1.464351416885,7.50433767179956));
#409474=CARTESIAN_POINT('Ctrl Pts',(2.32885943401303,-1.45845629514758,
7.50214974420965));
#409475=CARTESIAN_POINT('Ctrl Pts',(2.30969475968219,-1.44221793823036,
7.53887321589167));
#409476=CARTESIAN_POINT('Ctrl Pts',(2.30676723081195,-1.43719156043309,
7.5322040745206));
#409477=CARTESIAN_POINT('Ctrl Pts',(2.31298019139209,-1.43127530817745,
7.53003438070911));
#409478=CARTESIAN_POINT('Ctrl Pts',(2.29381001144492,-1.41494485249995,
7.56669465659232));
#409479=CARTESIAN_POINT('Ctrl Pts',(2.29089978372603,-1.40994817966098,
7.56004085833297));
#409480=CARTESIAN_POINT('Ctrl Pts',(2.297070015605,-1.4040435299096,7.55785582193789));
#409481=CARTESIAN_POINT('Ctrl Pts',(2.27789553550273,-1.38762072622218,
7.59443891967696));
#409482=CARTESIAN_POINT('Ctrl Pts',(2.27498108831602,-1.38261680882968,
7.58783901202978));
#409483=CARTESIAN_POINT('Ctrl Pts',(2.2811296209623,-1.37676234691709,7.58560008491213));
#409484=CARTESIAN_POINT('',(2.3279986714312,-1.45698290352085,7.50366116523517));
#409485=CARTESIAN_POINT('Ctrl Pts',(2.32799867143151,-1.45698290352105,
7.50366116523554));
#409486=CARTESIAN_POINT('Ctrl Pts',(2.32773447744662,-1.45769307184976,
7.50350835821027));
#409487=CARTESIAN_POINT('Ctrl Pts',(2.32746851446685,-1.45833729363187,
7.50345484956));
#409488=CARTESIAN_POINT('Ctrl Pts',(2.32719343025617,-1.45893495125745,
7.50349758195598));
#409489=CARTESIAN_POINT('Ctrl Pts',(2.32705229165532,-1.45924159394282,
7.50351950684424));
#409490=CARTESIAN_POINT('Ctrl Pts',(2.32689495833407,-1.45956625690093,
7.50357029184312));
#409491=CARTESIAN_POINT('Ctrl Pts',(2.32673463798333,-1.4598751553244,7.50365515313923));
#409492=CARTESIAN_POINT('Ctrl Pts',(2.32648800036377,-1.46035036618503,
7.50378570417639));
#409493=CARTESIAN_POINT('Ctrl Pts',(2.32622736167188,-1.460802376529,7.50400001621911));
#409494=CARTESIAN_POINT('Ctrl Pts',(2.32597059343916,-1.46119564767336,
7.50428903009635));
#409495=CARTESIAN_POINT('Ctrl Pts',(2.32594209414078,-1.46123929774474,
7.50432110841318));
#409496=CARTESIAN_POINT('Ctrl Pts',(2.32591364328842,-1.46128225449646,
7.50435406373354));
#409497=CARTESIAN_POINT('Ctrl Pts',(2.32588526557895,-1.4613244917113,7.50438785222352));
#409498=CARTESIAN_POINT('Ctrl Pts',(2.32571200602261,-1.46158237020968,
7.50459414719561));
#409499=CARTESIAN_POINT('Ctrl Pts',(2.32553828643811,-1.46181724467062,
7.50483629897752));
#409500=CARTESIAN_POINT('Ctrl Pts',(2.32537182004132,-1.46202089970006,
7.5050991045531));
#409501=CARTESIAN_POINT('Ctrl Pts',(2.32500457845002,-1.46247018315022,
7.50567888004914));
#409502=CARTESIAN_POINT('Ctrl Pts',(2.32465856865977,-1.46278555900681,
7.50637912803144));
#409503=CARTESIAN_POINT('Ctrl Pts',(2.32434792656118,-1.46299451535729,
7.50710440483569));
#409504=CARTESIAN_POINT('Ctrl Pts',(2.3242717509515,-1.46304575560279,7.50728225710685));
#409505=CARTESIAN_POINT('Ctrl Pts',(2.3241962671343,-1.46309173768622,7.50746498566954));
#409506=CARTESIAN_POINT('Ctrl Pts',(2.32412345387431,-1.46313174401607,
7.50764697238949));
#409507=CARTESIAN_POINT('Ctrl Pts',(2.32373202982735,-1.46334680703531,
7.50862528291182));
#409508=CARTESIAN_POINT('Ctrl Pts',(2.32338424120944,-1.46341233067583,
7.50965856837422));
#409509=CARTESIAN_POINT('Ctrl Pts',(2.32307440409399,-1.46339436861898,
7.51067959873203));
#409510=CARTESIAN_POINT('Ctrl Pts',(2.32290390033856,-1.46338448407644,
7.51124147302579));
#409511=CARTESIAN_POINT('Ctrl Pts',(2.32274487302364,-1.46334888134486,
7.51180065547253));
#409512=CARTESIAN_POINT('Ctrl Pts',(2.32259663098812,-1.46329586426742,
7.51235175716501));
#409513=CARTESIAN_POINT('Ctrl Pts',(2.32208439570276,-1.46311266914538,
7.51425603304536));
#409514=CARTESIAN_POINT('Ctrl Pts',(2.32164190203507,-1.46269399769696,
7.51626900505181));
#409515=CARTESIAN_POINT('Ctrl Pts',(2.32127620067169,-1.46209979118686,
7.51827788969245));
#409516=CARTESIAN_POINT('Ctrl Pts',(2.32125640822282,-1.46206763160763,
7.51838661432546));
#409517=CARTESIAN_POINT('Ctrl Pts',(2.32123684240497,-1.46203494803775,
7.51849533314857));
#409518=CARTESIAN_POINT('Ctrl Pts',(2.32121750495511,-1.46200174688656,
7.51860402984325));
#409519=CARTESIAN_POINT('Ctrl Pts',(2.2866232002648,-1.38616442272374,7.57603338728985));
#409520=CARTESIAN_POINT('Ctrl Pts',(2.30043891757839,-1.40980978650236,
7.55196141284922));
#409521=CARTESIAN_POINT('Ctrl Pts',(2.31423007475575,-1.43341484166519,
7.52783573083105));
#409522=CARTESIAN_POINT('Ctrl Pts',(2.32799867145623,-1.45698290357448,
7.50366116530176));
#409523=CARTESIAN_POINT('Origin',(7.90134016134199E-16,-4.78983883923424E-16,
7.49482233047033));
#409524=CARTESIAN_POINT('Origin',(2.36092560474805,-1.38561774629407,7.49482233047033));
#409525=CARTESIAN_POINT('Origin',(0.,0.,7.50366116523517));
#409526=CARTESIAN_POINT('Origin',(2.32050622536844,-1.45229374026962,7.49482233047033));
#409527=CARTESIAN_POINT('Ctrl Pts',(2.36986065415221,-1.3817579922399,7.51860402984325));
#409528=CARTESIAN_POINT('Ctrl Pts',(2.37746134385964,-1.38211267801838,
7.51860402984325));
#409529=CARTESIAN_POINT('Ctrl Pts',(2.38126727405859,-1.37552396180421,
7.51860402984325));
#409530=CARTESIAN_POINT('Ctrl Pts',(2.37268284216962,-1.3818896882206,7.51041458714366));
#409531=CARTESIAN_POINT('Ctrl Pts',(2.37836300374412,-1.38055173072963,
7.51004642900443));
#409532=CARTESIAN_POINT('Ctrl Pts',(2.38126832368895,-1.37552214471451,
7.5072913648301));
#409533=CARTESIAN_POINT('Ctrl Pts',(2.37352967894753,-1.38457420021925,
7.50215815450137));
#409534=CARTESIAN_POINT('Ctrl Pts',(2.37652725582072,-1.38373004539292,
7.49877163671529));
#409535=CARTESIAN_POINT('Ctrl Pts',(2.37827363220952,-1.38075446257555,
7.4948158853317));
#409536=CARTESIAN_POINT('Ctrl Pts',(2.36854808203743,-1.39009134757271,
7.50366171572174));
#409537=CARTESIAN_POINT('Ctrl Pts',(2.37170608696132,-1.39194476796698,
7.50000045605858));
#409538=CARTESIAN_POINT('Ctrl Pts',(2.37170608696138,-1.39194476796687,
7.49482233047317));
#409539=CARTESIAN_POINT('Origin',(2.37044333190378,-1.36927158015965,7.51860402984325));
#409540=CARTESIAN_POINT('Origin',(2.37044333190378,-1.36927158015965,9.));
#409541=CARTESIAN_POINT('Origin',(2.37044333190378,-1.36927158015965,8.75721825406948));
#409542=CARTESIAN_POINT('Ctrl Pts',(2.35317963884605,-1.38098095793091,
8.78942910404912));
#409543=CARTESIAN_POINT('Ctrl Pts',(2.35874509705393,-1.38126042821201,
8.7967269950169));
#409544=CARTESIAN_POINT('Ctrl Pts',(2.36082223585053,-1.37257947317229,
8.79893251111266));
#409545=CARTESIAN_POINT('Ctrl Pts',(2.36416206650685,-1.38149252553718,
8.78111911759584));
#409546=CARTESIAN_POINT('Ctrl Pts',(2.37076035502444,-1.38181640632384,
8.78644465894815));
#409547=CARTESIAN_POINT('Ctrl Pts',(2.37429374527117,-1.37452047148726,
8.78817647674132));
#409548=CARTESIAN_POINT('Ctrl Pts',(2.37100657738217,-1.38181134663966,
8.76780923932029));
#409549=CARTESIAN_POINT('Ctrl Pts',(2.37879582820069,-1.38218858457061,
8.76988516158373));
#409550=CARTESIAN_POINT('Ctrl Pts',(2.38270941194408,-1.37572172732154,
8.77093053738833));
#409551=CARTESIAN_POINT('Ctrl Pts',(2.36967199143527,-1.38174918088632,
8.75371302330492));
#409552=CARTESIAN_POINT('Ctrl Pts',(2.37727003273756,-1.38211792163047,
8.75300828287559));
#409553=CARTESIAN_POINT('Ctrl Pts',(2.38106807980287,-1.37548698068487,
8.75267964240738));
#409554=CARTESIAN_POINT('Origin',(2.35643593852863,-1.36861911374604,8.78727029226991));
#409555=CARTESIAN_POINT('Ctrl Pts',(2.28443929758137,-1.37777905311488,
8.85049129520029));
#409556=CARTESIAN_POINT('Ctrl Pts',(2.29027258849564,-1.37805076865112,
8.85711686593484));
#409557=CARTESIAN_POINT('Ctrl Pts',(2.29260852370879,-1.36982616113503,
8.85933012996512));
#409558=CARTESIAN_POINT('Ctrl Pts',(2.3082789390469,-1.3788895070696,8.82945683644722));
#409559=CARTESIAN_POINT('Ctrl Pts',(2.31416064980263,-1.37916347800908,
8.83607469902389));
#409560=CARTESIAN_POINT('Ctrl Pts',(2.31646736766074,-1.37090447714816,
8.8382956714852));
#409561=CARTESIAN_POINT('Ctrl Pts',(2.33208304560441,-1.37999830580315,
8.80838214965003));
#409562=CARTESIAN_POINT('Ctrl Pts',(2.33798796833692,-1.38027335795988,
8.81501364461991));
#409563=CARTESIAN_POINT('Ctrl Pts',(2.34028998879804,-1.37198182526731,
8.81722098428721));
#409564=CARTESIAN_POINT('Ctrl Pts',(2.35585431734964,-1.38110557508639,
8.78727029226991));
#409565=CARTESIAN_POINT('Ctrl Pts',(2.3617602209092,-1.38138067293018,8.79393457792714));
#409566=CARTESIAN_POINT('Ctrl Pts',(2.36407914959491,-1.37305829436821,
8.79610912703474));
#409567=CARTESIAN_POINT('Origin',(2.28502091876036,-1.36529259177452,8.85049129520029));
#409568=CARTESIAN_POINT('Ctrl Pts',(2.27817859968918,-1.38810672912943,
8.85049129520029));
#409569=CARTESIAN_POINT('Ctrl Pts',(2.28111762290111,-1.39315284196833,
8.85711686593484));
#409570=CARTESIAN_POINT('Ctrl Pts',(2.27490615106176,-1.39902807640644,
8.85933012996512));
#409571=CARTESIAN_POINT('Ctrl Pts',(2.27557848827884,-1.38364250594227,
8.86332496987233));
#409572=CARTESIAN_POINT('Ctrl Pts',(2.27342895555082,-1.38773290976438,
8.86648636486737));
#409573=CARTESIAN_POINT('Ctrl Pts',(2.2676470379875,-1.38653060731339,8.87206031107456));
#409574=CARTESIAN_POINT('Ctrl Pts',(2.27924360121797,-1.37753703682522,
8.86341338519876));
#409575=CARTESIAN_POINT('Ctrl Pts',(2.28185900586176,-1.37371170949497,
8.86654584966059));
#409576=CARTESIAN_POINT('Ctrl Pts',(2.27805961224584,-1.36916321953248,
8.87215952290715));
#409577=CARTESIAN_POINT('Ctrl Pts',(2.28443929758137,-1.37777905311488,
8.85049129520029));
#409578=CARTESIAN_POINT('Ctrl Pts',(2.29027258849564,-1.37805076865112,
8.85711686593484));
#409579=CARTESIAN_POINT('Ctrl Pts',(2.29260852370879,-1.36982616113503,
8.85933012996512));
#409580=CARTESIAN_POINT('Origin',(2.26737713379147,-1.39439786054282,8.85049129520029));
#409581=CARTESIAN_POINT('Ctrl Pts',(2.3141600729029,-1.44988459233544,8.78727029226991));
#409582=CARTESIAN_POINT('Ctrl Pts',(2.31713568099515,-1.45499351904854,
8.79393457792714));
#409583=CARTESIAN_POINT('Ctrl Pts',(2.31082965924422,-1.46089889836361,
8.79610912703474));
#409584=CARTESIAN_POINT('Ctrl Pts',(2.30218324533452,-1.42932115373562,
8.80838214965003));
#409585=CARTESIAN_POINT('Ctrl Pts',(2.30515835925059,-1.43442923198012,
8.81501364461989));
#409586=CARTESIAN_POINT('Ctrl Pts',(2.29887186472478,-1.44030535307933,
8.81722098428721));
#409587=CARTESIAN_POINT('Ctrl Pts',(2.29018987439862,-1.40872931124334,
8.82945683644721));
#409588=CARTESIAN_POINT('Ctrl Pts',(2.29315329328017,-1.41381730986973,
8.83607469902388));
#409589=CARTESIAN_POINT('Ctrl Pts',(2.2868978141797,-1.41968254846006,8.8382956714852));
#409590=CARTESIAN_POINT('Ctrl Pts',(2.27817859968918,-1.38810672912943,
8.85049129520029));
#409591=CARTESIAN_POINT('Ctrl Pts',(2.28111762290111,-1.39315284196833,
8.85711686593484));
#409592=CARTESIAN_POINT('Ctrl Pts',(2.27490615106176,-1.39902807640644,
8.85933012996512));
#409593=CARTESIAN_POINT('Origin',(2.30335860700519,-1.45617572374883,8.78727029226991));
#409594=CARTESIAN_POINT('Ctrl Pts',(2.32112429917461,-1.46184175524037,
8.75374538247849));
#409595=CARTESIAN_POINT('Ctrl Pts',(2.32496012354654,-1.46840154409179,
8.75304829418602));
#409596=CARTESIAN_POINT('Ctrl Pts',(2.32084701402089,-1.47483217184024,
8.75272238421917));
#409597=CARTESIAN_POINT('Ctrl Pts',(2.32178863480649,-1.46298237572162,
8.76769408445018));
#409598=CARTESIAN_POINT('Ctrl Pts',(2.32572038980644,-1.46970758632,8.76974318093968));
#409599=CARTESIAN_POINT('Ctrl Pts',(2.32180392561553,-1.47616356537213,
8.77077869880429));
#409600=CARTESIAN_POINT('Ctrl Pts',(2.31838362881724,-1.45713620489586,
8.78108014887992));
#409601=CARTESIAN_POINT('Ctrl Pts',(2.32171892952992,-1.4628336610349,8.78639403366326));
#409602=CARTESIAN_POINT('Ctrl Pts',(2.31690771126943,-1.46934321206233,
8.78812224174742));
#409603=CARTESIAN_POINT('Ctrl Pts',(2.31280357563322,-1.4475556214855,8.78944554828685));
#409604=CARTESIAN_POINT('Ctrl Pts',(2.31561927425866,-1.45235439829503,
8.79673892988685));
#409605=CARTESIAN_POINT('Ctrl Pts',(2.3088923932561,-1.45820697262553,8.79894799272499));
#409606=CARTESIAN_POINT('Origin',(2.3104160390574,-1.46829287829994,8.75721825406948));
#409607=CARTESIAN_POINT('Origin',(2.3104160390574,-1.46829287829994,9.));
#409608=CARTESIAN_POINT('Origin',(2.3104160390574,-1.46829287829994,7.51860402984325));
#409609=CARTESIAN_POINT('Ctrl Pts',(2.32799800459714,-1.45698248618141,
7.50366195182966));
#409610=CARTESIAN_POINT('Ctrl Pts',(2.33110214420567,-1.45892521853581,
7.50000065167735));
#409611=CARTESIAN_POINT('Ctrl Pts',(2.3311021442056,-1.45892521853591,7.49482233047108));
#409612=CARTESIAN_POINT('Ctrl Pts',(2.32540754212621,-1.46395696134398,
7.50215800491337));
#409613=CARTESIAN_POINT('Ctrl Pts',(2.32604450161756,-1.46700638420423,
7.49877273257267));
#409614=CARTESIAN_POINT('Ctrl Pts',(2.32421310714897,-1.46993267035743,
7.49481816995649));
#409615=CARTESIAN_POINT('Ctrl Pts',(2.32263636524652,-1.46443716447142,
7.51043025814042));
#409616=CARTESIAN_POINT('Ctrl Pts',(2.32408184125221,-1.47009431535362,
7.51006209594513));
#409617=CARTESIAN_POINT('Ctrl Pts',(2.32096452598623,-1.47499954885414,
7.50731281821698));
#409618=CARTESIAN_POINT('Ctrl Pts',(2.32121674419913,-1.46200044089927,
7.51860402984325));
#409619=CARTESIAN_POINT('Ctrl Pts',(2.32504721351855,-1.46857528098733,
7.51860402984325));
#409620=CARTESIAN_POINT('Ctrl Pts',(2.3209658839846,-1.47499741199082,7.51860402984325));
#409621=CARTESIAN_POINT('Origin',(0.,0.,7.5));
#409622=CARTESIAN_POINT('',(0.,0.,0.));
#409623=CARTESIAN_POINT('Origin',(0.,-1.11022302462516E-14,-14.21875));
#409624=CARTESIAN_POINT('',(-8.32001735975286E-31,-1.17524047358087,-13.9375));
#409625=CARTESIAN_POINT('',(-1.43925448419923E-16,-1.17524047358087,-14.));
#409626=CARTESIAN_POINT('',(1.43925448419925E-16,-1.1752404735809,-14.21875));
#409627=CARTESIAN_POINT('',(-0.823407874165272,-0.838564036615699,-14.));
#409628=CARTESIAN_POINT('Ctrl Pts',(-0.823407874165272,-0.838564036615699,
-14.));
#409629=CARTESIAN_POINT('Ctrl Pts',(-0.480534359260996,-1.17524047358087,
-13.9670084971875));
#409630=CARTESIAN_POINT('Ctrl Pts',(-1.43925448419923E-16,-1.17524047358087,
-13.9375));
#409631=CARTESIAN_POINT('Origin',(0.,2.54061283442571E-15,-14.));
#409632=CARTESIAN_POINT('Origin',(0.,-1.11022302462516E-14,-14.21875));
#409633=CARTESIAN_POINT('',(-8.32001735975286E-31,-1.17524047358087,-13.4375));
#409634=CARTESIAN_POINT('',(-8.32001735975286E-31,-1.17524047358087,-13.5));
#409635=CARTESIAN_POINT('',(1.43925448419925E-16,-1.1752404735809,-14.21875));
#409636=CARTESIAN_POINT('Ctrl Pts',(-1.43925448419923E-16,-1.17524047358087,
-13.9375));
#409637=CARTESIAN_POINT('Ctrl Pts',(0.678525403784459,-1.17524047358087,
-13.8958333333333));
#409638=CARTESIAN_POINT('Ctrl Pts',(1.01778810567669,-0.587620236790434,
-13.8541666666667));
#409639=CARTESIAN_POINT('Ctrl Pts',(1.35705080756892,2.29132664526027E-15,
-13.8125));
#409640=CARTESIAN_POINT('Ctrl Pts',(1.01778810567669,0.587620236790438,
-13.7708333333333));
#409641=CARTESIAN_POINT('Ctrl Pts',(0.67852540378446,1.17524047358087,-13.7291666666667));
#409642=CARTESIAN_POINT('Ctrl Pts',(0.,1.17524047358087,-13.6875));
#409643=CARTESIAN_POINT('Ctrl Pts',(-0.678525403784459,1.17524047358087,
-13.6458333333333));
#409644=CARTESIAN_POINT('Ctrl Pts',(-1.01778810567669,0.587620236790438,
-13.6041666666667));
#409645=CARTESIAN_POINT('Ctrl Pts',(-1.35705080756892,2.62370823081419E-15,
-13.5625));
#409646=CARTESIAN_POINT('Ctrl Pts',(-1.01778810567669,-0.587620236790433,
-13.5208333333333));
#409647=CARTESIAN_POINT('Ctrl Pts',(-0.67852540378446,-1.17524047358087,
-13.4791666666667));
#409648=CARTESIAN_POINT('Ctrl Pts',(-1.43925448419923E-16,-1.17524047358087,
-13.4375));
#409649=CARTESIAN_POINT('Ctrl Pts',(-1.43925448419923E-16,-1.17524047358087,
-14.));
#409650=CARTESIAN_POINT('Ctrl Pts',(0.67852540378446,-1.17524047358087,
-13.9583333333333));
#409651=CARTESIAN_POINT('Ctrl Pts',(1.01778810567669,-0.587620236790434,
-13.9166666666667));
#409652=CARTESIAN_POINT('Ctrl Pts',(1.35705080756892,2.29132664526027E-15,
-13.875));
#409653=CARTESIAN_POINT('Ctrl Pts',(1.01778810567669,0.587620236790438,
-13.8333333333333));
#409654=CARTESIAN_POINT('Ctrl Pts',(0.67852540378446,1.17524047358087,-13.7916666666667));
#409655=CARTESIAN_POINT('Ctrl Pts',(0.,1.17524047358087,-13.75));
#409656=CARTESIAN_POINT('Ctrl Pts',(-0.678525403784459,1.17524047358087,
-13.7083333333333));
#409657=CARTESIAN_POINT('Ctrl Pts',(-1.01778810567669,0.587620236790438,
-13.6666666666667));
#409658=CARTESIAN_POINT('Ctrl Pts',(-1.35705080756892,2.62370823081419E-15,
-13.625));
#409659=CARTESIAN_POINT('Ctrl Pts',(-1.01778810567669,-0.587620236790433,
-13.5833333333333));
#409660=CARTESIAN_POINT('Ctrl Pts',(-0.67852540378446,-1.17524047358087,
-13.5416666666667));
#409661=CARTESIAN_POINT('Ctrl Pts',(-1.43925448419923E-16,-1.17524047358087,
-13.5));
#409662=CARTESIAN_POINT('Origin',(0.,-1.11022302462516E-14,-14.21875));
#409663=CARTESIAN_POINT('',(-8.32001735975286E-31,-1.17524047358087,-12.9375));
#409664=CARTESIAN_POINT('',(-8.32001735975286E-31,-1.17524047358087,-13.));
#409665=CARTESIAN_POINT('',(1.43925448419925E-16,-1.1752404735809,-14.21875));
#409666=CARTESIAN_POINT('Ctrl Pts',(-1.43925448419923E-16,-1.17524047358087,
-13.4375));
#409667=CARTESIAN_POINT('Ctrl Pts',(0.678525403784459,-1.17524047358087,
-13.3958333333333));
#409668=CARTESIAN_POINT('Ctrl Pts',(1.01778810567669,-0.587620236790434,
-13.3541666666667));
#409669=CARTESIAN_POINT('Ctrl Pts',(1.35705080756892,2.29132664526027E-15,
-13.3125));
#409670=CARTESIAN_POINT('Ctrl Pts',(1.01778810567669,0.587620236790438,
-13.2708333333333));
#409671=CARTESIAN_POINT('Ctrl Pts',(0.67852540378446,1.17524047358087,-13.2291666666667));
#409672=CARTESIAN_POINT('Ctrl Pts',(0.,1.17524047358087,-13.1875));
#409673=CARTESIAN_POINT('Ctrl Pts',(-0.678525403784459,1.17524047358087,
-13.1458333333333));
#409674=CARTESIAN_POINT('Ctrl Pts',(-1.01778810567669,0.587620236790438,
-13.1041666666667));
#409675=CARTESIAN_POINT('Ctrl Pts',(-1.35705080756892,2.62370823081419E-15,
-13.0625));
#409676=CARTESIAN_POINT('Ctrl Pts',(-1.01778810567669,-0.587620236790433,
-13.0208333333333));
#409677=CARTESIAN_POINT('Ctrl Pts',(-0.67852540378446,-1.17524047358087,
-12.9791666666667));
#409678=CARTESIAN_POINT('Ctrl Pts',(-1.43925448419923E-16,-1.17524047358087,
-12.9375));
#409679=CARTESIAN_POINT('Ctrl Pts',(-1.43925448419923E-16,-1.17524047358087,
-13.5));
#409680=CARTESIAN_POINT('Ctrl Pts',(0.678525403784459,-1.17524047358087,
-13.4583333333333));
#409681=CARTESIAN_POINT('Ctrl Pts',(1.01778810567669,-0.587620236790434,
-13.4166666666667));
#409682=CARTESIAN_POINT('Ctrl Pts',(1.35705080756892,2.29132664526027E-15,
-13.375));
#409683=CARTESIAN_POINT('Ctrl Pts',(1.01778810567669,0.587620236790438,
-13.3333333333333));
#409684=CARTESIAN_POINT('Ctrl Pts',(0.67852540378446,1.17524047358087,-13.2916666666667));
#409685=CARTESIAN_POINT('Ctrl Pts',(0.,1.17524047358087,-13.25));
#409686=CARTESIAN_POINT('Ctrl Pts',(-0.678525403784459,1.17524047358087,
-13.2083333333333));
#409687=CARTESIAN_POINT('Ctrl Pts',(-1.01778810567669,0.587620236790438,
-13.1666666666667));
#409688=CARTESIAN_POINT('Ctrl Pts',(-1.35705080756892,2.62370823081419E-15,
-13.125));
#409689=CARTESIAN_POINT('Ctrl Pts',(-1.01778810567669,-0.587620236790433,
-13.0833333333333));
#409690=CARTESIAN_POINT('Ctrl Pts',(-0.67852540378446,-1.17524047358087,
-13.0416666666667));
#409691=CARTESIAN_POINT('Ctrl Pts',(-1.43925448419923E-16,-1.17524047358087,
-13.));
#409692=CARTESIAN_POINT('Origin',(0.,-1.11022302462516E-14,-14.21875));
#409693=CARTESIAN_POINT('',(-8.32001735975286E-31,-1.17524047358087,-12.4375));
#409694=CARTESIAN_POINT('',(-8.32001735975286E-31,-1.17524047358087,-12.5));
#409695=CARTESIAN_POINT('',(1.43925448419925E-16,-1.1752404735809,-14.21875));
#409696=CARTESIAN_POINT('Ctrl Pts',(-1.43925448419923E-16,-1.17524047358087,
-12.9375));
#409697=CARTESIAN_POINT('Ctrl Pts',(0.678525403784459,-1.17524047358087,
-12.8958333333333));
#409698=CARTESIAN_POINT('Ctrl Pts',(1.01778810567669,-0.587620236790434,
-12.8541666666667));
#409699=CARTESIAN_POINT('Ctrl Pts',(1.35705080756892,2.29132664526027E-15,
-12.8125));
#409700=CARTESIAN_POINT('Ctrl Pts',(1.01778810567669,0.587620236790438,
-12.7708333333333));
#409701=CARTESIAN_POINT('Ctrl Pts',(0.67852540378446,1.17524047358087,-12.7291666666667));
#409702=CARTESIAN_POINT('Ctrl Pts',(0.,1.17524047358087,-12.6875));
#409703=CARTESIAN_POINT('Ctrl Pts',(-0.678525403784459,1.17524047358087,
-12.6458333333333));
#409704=CARTESIAN_POINT('Ctrl Pts',(-1.01778810567669,0.587620236790438,
-12.6041666666667));
#409705=CARTESIAN_POINT('Ctrl Pts',(-1.35705080756892,2.62370823081419E-15,
-12.5625));
#409706=CARTESIAN_POINT('Ctrl Pts',(-1.01778810567669,-0.587620236790433,
-12.5208333333333));
#409707=CARTESIAN_POINT('Ctrl Pts',(-0.67852540378446,-1.17524047358087,
-12.4791666666667));
#409708=CARTESIAN_POINT('Ctrl Pts',(-1.43925448419923E-16,-1.17524047358087,
-12.4375));
#409709=CARTESIAN_POINT('Ctrl Pts',(-1.43925448419923E-16,-1.17524047358087,
-13.));
#409710=CARTESIAN_POINT('Ctrl Pts',(0.678525403784459,-1.17524047358087,
-12.9583333333333));
#409711=CARTESIAN_POINT('Ctrl Pts',(1.01778810567669,-0.587620236790434,
-12.9166666666667));
#409712=CARTESIAN_POINT('Ctrl Pts',(1.35705080756892,2.29132664526027E-15,
-12.875));
#409713=CARTESIAN_POINT('Ctrl Pts',(1.01778810567669,0.587620236790438,
-12.8333333333333));
#409714=CARTESIAN_POINT('Ctrl Pts',(0.67852540378446,1.17524047358087,-12.7916666666667));
#409715=CARTESIAN_POINT('Ctrl Pts',(0.,1.17524047358087,-12.75));
#409716=CARTESIAN_POINT('Ctrl Pts',(-0.678525403784459,1.17524047358087,
-12.7083333333333));
#409717=CARTESIAN_POINT('Ctrl Pts',(-1.01778810567669,0.587620236790438,
-12.6666666666667));
#409718=CARTESIAN_POINT('Ctrl Pts',(-1.35705080756892,2.62370823081419E-15,
-12.625));
#409719=CARTESIAN_POINT('Ctrl Pts',(-1.01778810567669,-0.587620236790433,
-12.5833333333333));
#409720=CARTESIAN_POINT('Ctrl Pts',(-0.67852540378446,-1.17524047358087,
-12.5416666666667));
#409721=CARTESIAN_POINT('Ctrl Pts',(-1.43925448419923E-16,-1.17524047358087,
-12.5));
#409722=CARTESIAN_POINT('Origin',(0.,-1.11022302462516E-14,-14.21875));
#409723=CARTESIAN_POINT('',(-8.32001735975286E-31,-1.17524047358087,-11.9375));
#409724=CARTESIAN_POINT('',(-8.32001735975286E-31,-1.17524047358087,-12.));
#409725=CARTESIAN_POINT('',(1.43925448419925E-16,-1.1752404735809,-14.21875));
#409726=CARTESIAN_POINT('Ctrl Pts',(-1.43925448419923E-16,-1.17524047358087,
-12.4375));
#409727=CARTESIAN_POINT('Ctrl Pts',(0.678525403784459,-1.17524047358087,
-12.3958333333333));
#409728=CARTESIAN_POINT('Ctrl Pts',(1.01778810567669,-0.587620236790434,
-12.3541666666667));
#409729=CARTESIAN_POINT('Ctrl Pts',(1.35705080756892,2.29132664526027E-15,
-12.3125));
#409730=CARTESIAN_POINT('Ctrl Pts',(1.01778810567669,0.587620236790438,
-12.2708333333333));
#409731=CARTESIAN_POINT('Ctrl Pts',(0.67852540378446,1.17524047358087,-12.2291666666667));
#409732=CARTESIAN_POINT('Ctrl Pts',(0.,1.17524047358087,-12.1875));
#409733=CARTESIAN_POINT('Ctrl Pts',(-0.678525403784459,1.17524047358087,
-12.1458333333333));
#409734=CARTESIAN_POINT('Ctrl Pts',(-1.01778810567669,0.587620236790438,
-12.1041666666667));
#409735=CARTESIAN_POINT('Ctrl Pts',(-1.35705080756892,2.62370823081419E-15,
-12.0625));
#409736=CARTESIAN_POINT('Ctrl Pts',(-1.01778810567669,-0.587620236790433,
-12.0208333333333));
#409737=CARTESIAN_POINT('Ctrl Pts',(-0.67852540378446,-1.17524047358087,
-11.9791666666667));
#409738=CARTESIAN_POINT('Ctrl Pts',(-1.43925448419923E-16,-1.17524047358087,
-11.9375));
#409739=CARTESIAN_POINT('Ctrl Pts',(-1.43925448419923E-16,-1.17524047358087,
-12.5));
#409740=CARTESIAN_POINT('Ctrl Pts',(0.678525403784459,-1.17524047358087,
-12.4583333333333));
#409741=CARTESIAN_POINT('Ctrl Pts',(1.01778810567669,-0.587620236790434,
-12.4166666666667));
#409742=CARTESIAN_POINT('Ctrl Pts',(1.35705080756892,2.29132664526027E-15,
-12.375));
#409743=CARTESIAN_POINT('Ctrl Pts',(1.01778810567669,0.587620236790438,
-12.3333333333333));
#409744=CARTESIAN_POINT('Ctrl Pts',(0.67852540378446,1.17524047358087,-12.2916666666667));
#409745=CARTESIAN_POINT('Ctrl Pts',(0.,1.17524047358087,-12.25));
#409746=CARTESIAN_POINT('Ctrl Pts',(-0.678525403784459,1.17524047358087,
-12.2083333333333));
#409747=CARTESIAN_POINT('Ctrl Pts',(-1.01778810567669,0.587620236790438,
-12.1666666666667));
#409748=CARTESIAN_POINT('Ctrl Pts',(-1.35705080756892,2.62370823081419E-15,
-12.125));
#409749=CARTESIAN_POINT('Ctrl Pts',(-1.01778810567669,-0.587620236790433,
-12.0833333333333));
#409750=CARTESIAN_POINT('Ctrl Pts',(-0.67852540378446,-1.17524047358087,
-12.0416666666667));
#409751=CARTESIAN_POINT('Ctrl Pts',(-1.43925448419923E-16,-1.17524047358087,
-12.));
#409752=CARTESIAN_POINT('Origin',(0.,-1.11022302462516E-14,-14.21875));
#409753=CARTESIAN_POINT('',(-8.32001735975286E-31,-1.17524047358087,-11.4375));
#409754=CARTESIAN_POINT('',(-8.32001735975286E-31,-1.17524047358087,-11.5));
#409755=CARTESIAN_POINT('',(1.43925448419925E-16,-1.1752404735809,-14.21875));
#409756=CARTESIAN_POINT('Ctrl Pts',(-1.43925448419923E-16,-1.17524047358087,
-11.9375));
#409757=CARTESIAN_POINT('Ctrl Pts',(0.678525403784459,-1.17524047358087,
-11.8958333333333));
#409758=CARTESIAN_POINT('Ctrl Pts',(1.01778810567669,-0.587620236790434,
-11.8541666666667));
#409759=CARTESIAN_POINT('Ctrl Pts',(1.35705080756892,2.29132664526027E-15,
-11.8125));
#409760=CARTESIAN_POINT('Ctrl Pts',(1.01778810567669,0.587620236790438,
-11.7708333333333));
#409761=CARTESIAN_POINT('Ctrl Pts',(0.67852540378446,1.17524047358087,-11.7291666666667));
#409762=CARTESIAN_POINT('Ctrl Pts',(0.,1.17524047358087,-11.6875));
#409763=CARTESIAN_POINT('Ctrl Pts',(-0.678525403784459,1.17524047358087,
-11.6458333333333));
#409764=CARTESIAN_POINT('Ctrl Pts',(-1.01778810567669,0.587620236790438,
-11.6041666666667));
#409765=CARTESIAN_POINT('Ctrl Pts',(-1.35705080756892,2.62370823081419E-15,
-11.5625));
#409766=CARTESIAN_POINT('Ctrl Pts',(-1.01778810567669,-0.587620236790433,
-11.5208333333333));
#409767=CARTESIAN_POINT('Ctrl Pts',(-0.67852540378446,-1.17524047358087,
-11.4791666666667));
#409768=CARTESIAN_POINT('Ctrl Pts',(-1.43925448419923E-16,-1.17524047358087,
-11.4375));
#409769=CARTESIAN_POINT('Ctrl Pts',(-1.43925448419923E-16,-1.17524047358087,
-12.));
#409770=CARTESIAN_POINT('Ctrl Pts',(0.678525403784459,-1.17524047358087,
-11.9583333333333));
#409771=CARTESIAN_POINT('Ctrl Pts',(1.01778810567669,-0.587620236790434,
-11.9166666666667));
#409772=CARTESIAN_POINT('Ctrl Pts',(1.35705080756892,2.29132664526027E-15,
-11.875));
#409773=CARTESIAN_POINT('Ctrl Pts',(1.01778810567669,0.587620236790438,
-11.8333333333333));
#409774=CARTESIAN_POINT('Ctrl Pts',(0.67852540378446,1.17524047358087,-11.7916666666667));
#409775=CARTESIAN_POINT('Ctrl Pts',(0.,1.17524047358087,-11.75));
#409776=CARTESIAN_POINT('Ctrl Pts',(-0.678525403784459,1.17524047358087,
-11.7083333333333));
#409777=CARTESIAN_POINT('Ctrl Pts',(-1.01778810567669,0.587620236790438,
-11.6666666666667));
#409778=CARTESIAN_POINT('Ctrl Pts',(-1.35705080756892,2.62370823081419E-15,
-11.625));
#409779=CARTESIAN_POINT('Ctrl Pts',(-1.01778810567669,-0.587620236790433,
-11.5833333333333));
#409780=CARTESIAN_POINT('Ctrl Pts',(-0.67852540378446,-1.17524047358087,
-11.5416666666667));
#409781=CARTESIAN_POINT('Ctrl Pts',(-1.43925448419923E-16,-1.17524047358087,
-11.5));
#409782=CARTESIAN_POINT('Origin',(0.,-1.11022302462516E-14,-14.21875));
#409783=CARTESIAN_POINT('',(-8.32001735975286E-31,-1.17524047358087,-10.9375));
#409784=CARTESIAN_POINT('',(-8.32001735975286E-31,-1.17524047358087,-11.));
#409785=CARTESIAN_POINT('',(1.43925448419925E-16,-1.1752404735809,-14.21875));
#409786=CARTESIAN_POINT('Ctrl Pts',(-1.43925448419923E-16,-1.17524047358087,
-11.4375));
#409787=CARTESIAN_POINT('Ctrl Pts',(0.678525403784459,-1.17524047358087,
-11.3958333333333));
#409788=CARTESIAN_POINT('Ctrl Pts',(1.01778810567669,-0.587620236790434,
-11.3541666666667));
#409789=CARTESIAN_POINT('Ctrl Pts',(1.35705080756892,2.29132664526027E-15,
-11.3125));
#409790=CARTESIAN_POINT('Ctrl Pts',(1.01778810567669,0.587620236790438,
-11.2708333333333));
#409791=CARTESIAN_POINT('Ctrl Pts',(0.67852540378446,1.17524047358087,-11.2291666666667));
#409792=CARTESIAN_POINT('Ctrl Pts',(0.,1.17524047358087,-11.1875));
#409793=CARTESIAN_POINT('Ctrl Pts',(-0.678525403784459,1.17524047358087,
-11.1458333333333));
#409794=CARTESIAN_POINT('Ctrl Pts',(-1.01778810567669,0.587620236790438,
-11.1041666666667));
#409795=CARTESIAN_POINT('Ctrl Pts',(-1.35705080756892,2.62370823081419E-15,
-11.0625));
#409796=CARTESIAN_POINT('Ctrl Pts',(-1.01778810567669,-0.587620236790433,
-11.0208333333333));
#409797=CARTESIAN_POINT('Ctrl Pts',(-0.67852540378446,-1.17524047358087,
-10.9791666666667));
#409798=CARTESIAN_POINT('Ctrl Pts',(-1.43925448419923E-16,-1.17524047358087,
-10.9375));
#409799=CARTESIAN_POINT('Ctrl Pts',(-1.43925448419923E-16,-1.17524047358087,
-11.5));
#409800=CARTESIAN_POINT('Ctrl Pts',(0.678525403784459,-1.17524047358087,
-11.4583333333333));
#409801=CARTESIAN_POINT('Ctrl Pts',(1.01778810567669,-0.587620236790434,
-11.4166666666667));
#409802=CARTESIAN_POINT('Ctrl Pts',(1.35705080756892,2.29132664526027E-15,
-11.375));
#409803=CARTESIAN_POINT('Ctrl Pts',(1.01778810567669,0.587620236790438,
-11.3333333333333));
#409804=CARTESIAN_POINT('Ctrl Pts',(0.67852540378446,1.17524047358087,-11.2916666666667));
#409805=CARTESIAN_POINT('Ctrl Pts',(0.,1.17524047358087,-11.25));
#409806=CARTESIAN_POINT('Ctrl Pts',(-0.678525403784459,1.17524047358087,
-11.2083333333333));
#409807=CARTESIAN_POINT('Ctrl Pts',(-1.01778810567669,0.587620236790438,
-11.1666666666667));
#409808=CARTESIAN_POINT('Ctrl Pts',(-1.35705080756892,2.62370823081419E-15,
-11.125));
#409809=CARTESIAN_POINT('Ctrl Pts',(-1.01778810567669,-0.587620236790433,
-11.0833333333333));
#409810=CARTESIAN_POINT('Ctrl Pts',(-0.67852540378446,-1.17524047358087,
-11.0416666666667));
#409811=CARTESIAN_POINT('Ctrl Pts',(-1.43925448419923E-16,-1.17524047358087,
-11.));
#409812=CARTESIAN_POINT('Origin',(0.,-1.11022302462516E-14,-14.21875));
#409813=CARTESIAN_POINT('',(-8.32001735975286E-31,-1.17524047358087,-10.4375));
#409814=CARTESIAN_POINT('',(-8.32001735975286E-31,-1.17524047358087,-10.5));
#409815=CARTESIAN_POINT('',(1.43925448419925E-16,-1.1752404735809,-14.21875));
#409816=CARTESIAN_POINT('Ctrl Pts',(-1.43925448419923E-16,-1.17524047358087,
-10.9375));
#409817=CARTESIAN_POINT('Ctrl Pts',(0.678525403784459,-1.17524047358087,
-10.8958333333333));
#409818=CARTESIAN_POINT('Ctrl Pts',(1.01778810567669,-0.587620236790434,
-10.8541666666667));
#409819=CARTESIAN_POINT('Ctrl Pts',(1.35705080756892,2.29132664526027E-15,
-10.8125));
#409820=CARTESIAN_POINT('Ctrl Pts',(1.01778810567669,0.587620236790438,
-10.7708333333333));
#409821=CARTESIAN_POINT('Ctrl Pts',(0.67852540378446,1.17524047358087,-10.7291666666667));
#409822=CARTESIAN_POINT('Ctrl Pts',(0.,1.17524047358087,-10.6875));
#409823=CARTESIAN_POINT('Ctrl Pts',(-0.678525403784459,1.17524047358087,
-10.6458333333333));
#409824=CARTESIAN_POINT('Ctrl Pts',(-1.01778810567669,0.587620236790438,
-10.6041666666667));
#409825=CARTESIAN_POINT('Ctrl Pts',(-1.35705080756892,2.62370823081419E-15,
-10.5625));
#409826=CARTESIAN_POINT('Ctrl Pts',(-1.01778810567669,-0.587620236790433,
-10.5208333333333));
#409827=CARTESIAN_POINT('Ctrl Pts',(-0.67852540378446,-1.17524047358087,
-10.4791666666667));
#409828=CARTESIAN_POINT('Ctrl Pts',(-1.43925448419923E-16,-1.17524047358087,
-10.4375));
#409829=CARTESIAN_POINT('Ctrl Pts',(-1.43925448419923E-16,-1.17524047358087,
-11.));
#409830=CARTESIAN_POINT('Ctrl Pts',(0.678525403784459,-1.17524047358087,
-10.9583333333333));
#409831=CARTESIAN_POINT('Ctrl Pts',(1.01778810567669,-0.587620236790434,
-10.9166666666667));
#409832=CARTESIAN_POINT('Ctrl Pts',(1.35705080756892,2.29132664526027E-15,
-10.875));
#409833=CARTESIAN_POINT('Ctrl Pts',(1.01778810567669,0.587620236790438,
-10.8333333333333));
#409834=CARTESIAN_POINT('Ctrl Pts',(0.67852540378446,1.17524047358087,-10.7916666666667));
#409835=CARTESIAN_POINT('Ctrl Pts',(0.,1.17524047358087,-10.75));
#409836=CARTESIAN_POINT('Ctrl Pts',(-0.678525403784459,1.17524047358087,
-10.7083333333333));
#409837=CARTESIAN_POINT('Ctrl Pts',(-1.01778810567669,0.587620236790438,
-10.6666666666667));
#409838=CARTESIAN_POINT('Ctrl Pts',(-1.35705080756892,2.62370823081419E-15,
-10.625));
#409839=CARTESIAN_POINT('Ctrl Pts',(-1.01778810567669,-0.587620236790433,
-10.5833333333333));
#409840=CARTESIAN_POINT('Ctrl Pts',(-0.67852540378446,-1.17524047358087,
-10.5416666666667));
#409841=CARTESIAN_POINT('Ctrl Pts',(-1.43925448419923E-16,-1.17524047358087,
-10.5));
#409842=CARTESIAN_POINT('Origin',(0.,-1.11022302462516E-14,-14.21875));
#409843=CARTESIAN_POINT('',(-8.32001735975286E-31,-1.17524047358087,-9.93749999999999));
#409844=CARTESIAN_POINT('',(-8.32001735975286E-31,-1.17524047358087,-9.99999999999999));
#409845=CARTESIAN_POINT('',(1.43925448419925E-16,-1.1752404735809,-14.21875));
#409846=CARTESIAN_POINT('Ctrl Pts',(-1.43925448419923E-16,-1.17524047358087,
-10.4375));
#409847=CARTESIAN_POINT('Ctrl Pts',(0.678525403784459,-1.17524047358087,
-10.3958333333333));
#409848=CARTESIAN_POINT('Ctrl Pts',(1.01778810567669,-0.587620236790434,
-10.3541666666667));
#409849=CARTESIAN_POINT('Ctrl Pts',(1.35705080756892,2.29132664526027E-15,
-10.3125));
#409850=CARTESIAN_POINT('Ctrl Pts',(1.01778810567669,0.587620236790438,
-10.2708333333333));
#409851=CARTESIAN_POINT('Ctrl Pts',(0.67852540378446,1.17524047358087,-10.2291666666667));
#409852=CARTESIAN_POINT('Ctrl Pts',(0.,1.17524047358087,-10.1875));
#409853=CARTESIAN_POINT('Ctrl Pts',(-0.678525403784459,1.17524047358087,
-10.1458333333333));
#409854=CARTESIAN_POINT('Ctrl Pts',(-1.01778810567669,0.587620236790438,
-10.1041666666667));
#409855=CARTESIAN_POINT('Ctrl Pts',(-1.35705080756892,2.62370823081419E-15,
-10.0625));
#409856=CARTESIAN_POINT('Ctrl Pts',(-1.01778810567669,-0.587620236790433,
-10.0208333333333));
#409857=CARTESIAN_POINT('Ctrl Pts',(-0.67852540378446,-1.17524047358087,
-9.97916666666666));
#409858=CARTESIAN_POINT('Ctrl Pts',(-1.43925448419923E-16,-1.17524047358087,
-9.93749999999999));
#409859=CARTESIAN_POINT('Ctrl Pts',(-1.43925448419923E-16,-1.17524047358087,
-10.5));
#409860=CARTESIAN_POINT('Ctrl Pts',(0.678525403784459,-1.17524047358087,
-10.4583333333333));
#409861=CARTESIAN_POINT('Ctrl Pts',(1.01778810567669,-0.587620236790434,
-10.4166666666667));
#409862=CARTESIAN_POINT('Ctrl Pts',(1.35705080756892,2.29132664526027E-15,
-10.375));
#409863=CARTESIAN_POINT('Ctrl Pts',(1.01778810567669,0.587620236790438,
-10.3333333333333));
#409864=CARTESIAN_POINT('Ctrl Pts',(0.67852540378446,1.17524047358087,-10.2916666666667));
#409865=CARTESIAN_POINT('Ctrl Pts',(0.,1.17524047358087,-10.25));
#409866=CARTESIAN_POINT('Ctrl Pts',(-0.678525403784459,1.17524047358087,
-10.2083333333333));
#409867=CARTESIAN_POINT('Ctrl Pts',(-1.01778810567669,0.587620236790438,
-10.1666666666667));
#409868=CARTESIAN_POINT('Ctrl Pts',(-1.35705080756892,2.62370823081419E-15,
-10.125));
#409869=CARTESIAN_POINT('Ctrl Pts',(-1.01778810567669,-0.587620236790433,
-10.0833333333333));
#409870=CARTESIAN_POINT('Ctrl Pts',(-0.67852540378446,-1.17524047358087,
-10.0416666666667));
#409871=CARTESIAN_POINT('Ctrl Pts',(-1.43925448419923E-16,-1.17524047358087,
-9.99999999999999));
#409872=CARTESIAN_POINT('Origin',(0.,-1.11022302462516E-14,-14.21875));
#409873=CARTESIAN_POINT('',(-8.32001735975286E-31,-1.17524047358087,-9.43749999999999));
#409874=CARTESIAN_POINT('',(-8.32001735975286E-31,-1.17524047358087,-9.49999999999999));
#409875=CARTESIAN_POINT('',(1.43925448419925E-16,-1.1752404735809,-14.21875));
#409876=CARTESIAN_POINT('Ctrl Pts',(-1.43925448419923E-16,-1.17524047358087,
-9.93749999999999));
#409877=CARTESIAN_POINT('Ctrl Pts',(0.678525403784459,-1.17524047358087,
-9.89583333333332));
#409878=CARTESIAN_POINT('Ctrl Pts',(1.01778810567669,-0.587620236790434,
-9.85416666666666));
#409879=CARTESIAN_POINT('Ctrl Pts',(1.35705080756892,2.29132664526027E-15,
-9.81249999999999));
#409880=CARTESIAN_POINT('Ctrl Pts',(1.01778810567669,0.587620236790438,
-9.77083333333332));
#409881=CARTESIAN_POINT('Ctrl Pts',(0.67852540378446,1.17524047358087,-9.72916666666666));
#409882=CARTESIAN_POINT('Ctrl Pts',(0.,1.17524047358087,-9.68749999999999));
#409883=CARTESIAN_POINT('Ctrl Pts',(-0.678525403784459,1.17524047358087,
-9.64583333333332));
#409884=CARTESIAN_POINT('Ctrl Pts',(-1.01778810567669,0.587620236790438,
-9.60416666666666));
#409885=CARTESIAN_POINT('Ctrl Pts',(-1.35705080756892,2.62370823081419E-15,
-9.56249999999999));
#409886=CARTESIAN_POINT('Ctrl Pts',(-1.01778810567669,-0.587620236790433,
-9.52083333333332));
#409887=CARTESIAN_POINT('Ctrl Pts',(-0.67852540378446,-1.17524047358087,
-9.47916666666666));
#409888=CARTESIAN_POINT('Ctrl Pts',(-1.43925448419923E-16,-1.17524047358087,
-9.43749999999999));
#409889=CARTESIAN_POINT('Ctrl Pts',(-1.43925448419923E-16,-1.17524047358087,
-9.99999999999999));
#409890=CARTESIAN_POINT('Ctrl Pts',(0.678525403784459,-1.17524047358087,
-9.95833333333332));
#409891=CARTESIAN_POINT('Ctrl Pts',(1.01778810567669,-0.587620236790434,
-9.91666666666666));
#409892=CARTESIAN_POINT('Ctrl Pts',(1.35705080756892,2.29132664526027E-15,
-9.87499999999999));
#409893=CARTESIAN_POINT('Ctrl Pts',(1.01778810567669,0.587620236790438,
-9.83333333333332));
#409894=CARTESIAN_POINT('Ctrl Pts',(0.67852540378446,1.17524047358087,-9.79166666666666));
#409895=CARTESIAN_POINT('Ctrl Pts',(0.,1.17524047358087,-9.74999999999999));
#409896=CARTESIAN_POINT('Ctrl Pts',(-0.678525403784459,1.17524047358087,
-9.70833333333332));
#409897=CARTESIAN_POINT('Ctrl Pts',(-1.01778810567669,0.587620236790438,
-9.66666666666666));
#409898=CARTESIAN_POINT('Ctrl Pts',(-1.35705080756892,2.62370823081419E-15,
-9.62499999999999));
#409899=CARTESIAN_POINT('Ctrl Pts',(-1.01778810567669,-0.587620236790433,
-9.58333333333332));
#409900=CARTESIAN_POINT('Ctrl Pts',(-0.67852540378446,-1.17524047358087,
-9.54166666666666));
#409901=CARTESIAN_POINT('Ctrl Pts',(-1.43925448419923E-16,-1.17524047358087,
-9.49999999999999));
#409902=CARTESIAN_POINT('Origin',(0.,-1.11022302462516E-14,-14.21875));
#409903=CARTESIAN_POINT('',(-8.32001735975286E-31,-1.17524047358087,-8.93749999999999));
#409904=CARTESIAN_POINT('',(-8.32001735975286E-31,-1.17524047358087,-8.99999999999999));
#409905=CARTESIAN_POINT('',(1.43925448419925E-16,-1.1752404735809,-14.21875));
#409906=CARTESIAN_POINT('Ctrl Pts',(-1.43925448419923E-16,-1.17524047358087,
-9.43749999999999));
#409907=CARTESIAN_POINT('Ctrl Pts',(0.678525403784459,-1.17524047358087,
-9.39583333333332));
#409908=CARTESIAN_POINT('Ctrl Pts',(1.01778810567669,-0.587620236790434,
-9.35416666666666));
#409909=CARTESIAN_POINT('Ctrl Pts',(1.35705080756892,2.29132664526027E-15,
-9.31249999999999));
#409910=CARTESIAN_POINT('Ctrl Pts',(1.01778810567669,0.587620236790438,
-9.27083333333332));
#409911=CARTESIAN_POINT('Ctrl Pts',(0.67852540378446,1.17524047358087,-9.22916666666666));
#409912=CARTESIAN_POINT('Ctrl Pts',(0.,1.17524047358087,-9.18749999999999));
#409913=CARTESIAN_POINT('Ctrl Pts',(-0.678525403784459,1.17524047358087,
-9.14583333333333));
#409914=CARTESIAN_POINT('Ctrl Pts',(-1.01778810567669,0.587620236790438,
-9.10416666666666));
#409915=CARTESIAN_POINT('Ctrl Pts',(-1.35705080756892,2.62370823081419E-15,
-9.06249999999999));
#409916=CARTESIAN_POINT('Ctrl Pts',(-1.01778810567669,-0.587620236790433,
-9.02083333333332));
#409917=CARTESIAN_POINT('Ctrl Pts',(-0.67852540378446,-1.17524047358087,
-8.97916666666666));
#409918=CARTESIAN_POINT('Ctrl Pts',(-1.43925448419923E-16,-1.17524047358087,
-8.93749999999999));
#409919=CARTESIAN_POINT('Ctrl Pts',(-1.43925448419923E-16,-1.17524047358087,
-9.49999999999999));
#409920=CARTESIAN_POINT('Ctrl Pts',(0.678525403784459,-1.17524047358087,
-9.45833333333333));
#409921=CARTESIAN_POINT('Ctrl Pts',(1.01778810567669,-0.587620236790434,
-9.41666666666666));
#409922=CARTESIAN_POINT('Ctrl Pts',(1.35705080756892,2.29132664526027E-15,
-9.37499999999999));
#409923=CARTESIAN_POINT('Ctrl Pts',(1.01778810567669,0.587620236790438,
-9.33333333333332));
#409924=CARTESIAN_POINT('Ctrl Pts',(0.67852540378446,1.17524047358087,-9.29166666666666));
#409925=CARTESIAN_POINT('Ctrl Pts',(0.,1.17524047358087,-9.24999999999999));
#409926=CARTESIAN_POINT('Ctrl Pts',(-0.678525403784459,1.17524047358087,
-9.20833333333332));
#409927=CARTESIAN_POINT('Ctrl Pts',(-1.01778810567669,0.587620236790438,
-9.16666666666666));
#409928=CARTESIAN_POINT('Ctrl Pts',(-1.35705080756892,2.62370823081419E-15,
-9.12499999999999));
#409929=CARTESIAN_POINT('Ctrl Pts',(-1.01778810567669,-0.587620236790433,
-9.08333333333332));
#409930=CARTESIAN_POINT('Ctrl Pts',(-0.67852540378446,-1.17524047358087,
-9.04166666666666));
#409931=CARTESIAN_POINT('Ctrl Pts',(-1.43925448419923E-16,-1.17524047358087,
-8.99999999999999));
#409932=CARTESIAN_POINT('Origin',(0.,-1.11022302462516E-14,-14.21875));
#409933=CARTESIAN_POINT('',(-8.32001735975286E-31,-1.17524047358087,-8.43749999999999));
#409934=CARTESIAN_POINT('',(-8.32001735975286E-31,-1.17524047358087,-8.49999999999999));
#409935=CARTESIAN_POINT('',(1.43925448419925E-16,-1.1752404735809,-14.21875));
#409936=CARTESIAN_POINT('Ctrl Pts',(-1.43925448419923E-16,-1.17524047358087,
-8.93749999999999));
#409937=CARTESIAN_POINT('Ctrl Pts',(0.678525403784459,-1.17524047358087,
-8.89583333333332));
#409938=CARTESIAN_POINT('Ctrl Pts',(1.01778810567669,-0.587620236790434,
-8.85416666666666));
#409939=CARTESIAN_POINT('Ctrl Pts',(1.35705080756892,2.29132664526027E-15,
-8.81249999999999));
#409940=CARTESIAN_POINT('Ctrl Pts',(1.01778810567669,0.587620236790438,
-8.77083333333332));
#409941=CARTESIAN_POINT('Ctrl Pts',(0.67852540378446,1.17524047358087,-8.72916666666666));
#409942=CARTESIAN_POINT('Ctrl Pts',(0.,1.17524047358087,-8.68749999999999));
#409943=CARTESIAN_POINT('Ctrl Pts',(-0.678525403784459,1.17524047358087,
-8.64583333333333));
#409944=CARTESIAN_POINT('Ctrl Pts',(-1.01778810567669,0.587620236790438,
-8.60416666666666));
#409945=CARTESIAN_POINT('Ctrl Pts',(-1.35705080756892,2.62370823081419E-15,
-8.56249999999999));
#409946=CARTESIAN_POINT('Ctrl Pts',(-1.01778810567669,-0.587620236790433,
-8.52083333333333));
#409947=CARTESIAN_POINT('Ctrl Pts',(-0.67852540378446,-1.17524047358087,
-8.47916666666666));
#409948=CARTESIAN_POINT('Ctrl Pts',(-1.43925448419923E-16,-1.17524047358087,
-8.43749999999999));
#409949=CARTESIAN_POINT('Ctrl Pts',(-1.43925448419923E-16,-1.17524047358087,
-8.99999999999999));
#409950=CARTESIAN_POINT('Ctrl Pts',(0.678525403784459,-1.17524047358087,
-8.95833333333332));
#409951=CARTESIAN_POINT('Ctrl Pts',(1.01778810567669,-0.587620236790434,
-8.91666666666666));
#409952=CARTESIAN_POINT('Ctrl Pts',(1.35705080756892,2.29132664526027E-15,
-8.87499999999999));
#409953=CARTESIAN_POINT('Ctrl Pts',(1.01778810567669,0.587620236790438,
-8.83333333333333));
#409954=CARTESIAN_POINT('Ctrl Pts',(0.67852540378446,1.17524047358087,-8.79166666666666));
#409955=CARTESIAN_POINT('Ctrl Pts',(0.,1.17524047358087,-8.74999999999999));
#409956=CARTESIAN_POINT('Ctrl Pts',(-0.678525403784459,1.17524047358087,
-8.70833333333333));
#409957=CARTESIAN_POINT('Ctrl Pts',(-1.01778810567669,0.587620236790438,
-8.66666666666666));
#409958=CARTESIAN_POINT('Ctrl Pts',(-1.35705080756892,2.62370823081419E-15,
-8.62499999999999));
#409959=CARTESIAN_POINT('Ctrl Pts',(-1.01778810567669,-0.587620236790433,
-8.58333333333333));
#409960=CARTESIAN_POINT('Ctrl Pts',(-0.67852540378446,-1.17524047358087,
-8.54166666666666));
#409961=CARTESIAN_POINT('Ctrl Pts',(-1.43925448419923E-16,-1.17524047358087,
-8.49999999999999));
#409962=CARTESIAN_POINT('Origin',(0.,-1.11022302462516E-14,-14.21875));
#409963=CARTESIAN_POINT('',(-8.32001735975286E-31,-1.17524047358087,-7.93749999999999));
#409964=CARTESIAN_POINT('',(-8.32001735975286E-31,-1.17524047358087,-7.99999999999999));
#409965=CARTESIAN_POINT('',(1.43925448419925E-16,-1.1752404735809,-14.21875));
#409966=CARTESIAN_POINT('Ctrl Pts',(-1.43925448419923E-16,-1.17524047358087,
-8.43749999999999));
#409967=CARTESIAN_POINT('Ctrl Pts',(0.678525403784459,-1.17524047358087,
-8.39583333333333));
#409968=CARTESIAN_POINT('Ctrl Pts',(1.01778810567669,-0.587620236790434,
-8.35416666666666));
#409969=CARTESIAN_POINT('Ctrl Pts',(1.35705080756892,2.29132664526027E-15,
-8.31249999999999));
#409970=CARTESIAN_POINT('Ctrl Pts',(1.01778810567669,0.587620236790438,
-8.27083333333333));
#409971=CARTESIAN_POINT('Ctrl Pts',(0.67852540378446,1.17524047358087,-8.22916666666666));
#409972=CARTESIAN_POINT('Ctrl Pts',(0.,1.17524047358087,-8.18749999999999));
#409973=CARTESIAN_POINT('Ctrl Pts',(-0.678525403784459,1.17524047358087,
-8.14583333333333));
#409974=CARTESIAN_POINT('Ctrl Pts',(-1.01778810567669,0.587620236790438,
-8.10416666666666));
#409975=CARTESIAN_POINT('Ctrl Pts',(-1.35705080756892,2.62370823081419E-15,
-8.06249999999999));
#409976=CARTESIAN_POINT('Ctrl Pts',(-1.01778810567669,-0.587620236790433,
-8.02083333333333));
#409977=CARTESIAN_POINT('Ctrl Pts',(-0.67852540378446,-1.17524047358087,
-7.97916666666666));
#409978=CARTESIAN_POINT('Ctrl Pts',(-1.43925448419923E-16,-1.17524047358087,
-7.93749999999999));
#409979=CARTESIAN_POINT('Ctrl Pts',(-1.43925448419923E-16,-1.17524047358087,
-8.49999999999999));
#409980=CARTESIAN_POINT('Ctrl Pts',(0.678525403784459,-1.17524047358087,
-8.45833333333333));
#409981=CARTESIAN_POINT('Ctrl Pts',(1.01778810567669,-0.587620236790434,
-8.41666666666666));
#409982=CARTESIAN_POINT('Ctrl Pts',(1.35705080756892,2.29132664526027E-15,
-8.37499999999999));
#409983=CARTESIAN_POINT('Ctrl Pts',(1.01778810567669,0.587620236790438,
-8.33333333333333));
#409984=CARTESIAN_POINT('Ctrl Pts',(0.67852540378446,1.17524047358087,-8.29166666666666));
#409985=CARTESIAN_POINT('Ctrl Pts',(0.,1.17524047358087,-8.24999999999999));
#409986=CARTESIAN_POINT('Ctrl Pts',(-0.678525403784459,1.17524047358087,
-8.20833333333333));
#409987=CARTESIAN_POINT('Ctrl Pts',(-1.01778810567669,0.587620236790438,
-8.16666666666666));
#409988=CARTESIAN_POINT('Ctrl Pts',(-1.35705080756892,2.62370823081419E-15,
-8.12499999999999));
#409989=CARTESIAN_POINT('Ctrl Pts',(-1.01778810567669,-0.587620236790433,
-8.08333333333333));
#409990=CARTESIAN_POINT('Ctrl Pts',(-0.67852540378446,-1.17524047358087,
-8.04166666666666));
#409991=CARTESIAN_POINT('Ctrl Pts',(-1.43925448419923E-16,-1.17524047358087,
-7.99999999999999));
#409992=CARTESIAN_POINT('Origin',(0.,-1.11022302462516E-14,-14.21875));
#409993=CARTESIAN_POINT('',(-8.32001735975286E-31,-1.17524047358087,-7.43749999999999));
#409994=CARTESIAN_POINT('',(-8.32001735975286E-31,-1.17524047358087,-7.49999999999999));
#409995=CARTESIAN_POINT('',(1.43925448419925E-16,-1.1752404735809,-14.21875));
#409996=CARTESIAN_POINT('Ctrl Pts',(-1.43925448419923E-16,-1.17524047358087,
-7.93749999999999));
#409997=CARTESIAN_POINT('Ctrl Pts',(0.678525403784459,-1.17524047358087,
-7.89583333333332));
#409998=CARTESIAN_POINT('Ctrl Pts',(1.01778810567669,-0.587620236790434,
-7.85416666666666));
#409999=CARTESIAN_POINT('Ctrl Pts',(1.35705080756892,2.29132664526027E-15,
-7.81249999999999));
#410000=CARTESIAN_POINT('Ctrl Pts',(1.01778810567669,0.587620236790438,
-7.77083333333332));
#410001=CARTESIAN_POINT('Ctrl Pts',(0.67852540378446,1.17524047358087,-7.72916666666666));
#410002=CARTESIAN_POINT('Ctrl Pts',(0.,1.17524047358087,-7.68749999999999));
#410003=CARTESIAN_POINT('Ctrl Pts',(-0.678525403784459,1.17524047358087,
-7.64583333333333));
#410004=CARTESIAN_POINT('Ctrl Pts',(-1.01778810567669,0.587620236790438,
-7.60416666666666));
#410005=CARTESIAN_POINT('Ctrl Pts',(-1.35705080756892,2.62370823081419E-15,
-7.56249999999999));
#410006=CARTESIAN_POINT('Ctrl Pts',(-1.01778810567669,-0.587620236790433,
-7.52083333333332));
#410007=CARTESIAN_POINT('Ctrl Pts',(-0.67852540378446,-1.17524047358087,
-7.47916666666666));
#410008=CARTESIAN_POINT('Ctrl Pts',(-1.43925448419923E-16,-1.17524047358087,
-7.43749999999999));
#410009=CARTESIAN_POINT('Ctrl Pts',(-1.43925448419923E-16,-1.17524047358087,
-7.99999999999999));
#410010=CARTESIAN_POINT('Ctrl Pts',(0.678525403784459,-1.17524047358087,
-7.95833333333333));
#410011=CARTESIAN_POINT('Ctrl Pts',(1.01778810567669,-0.587620236790434,
-7.91666666666666));
#410012=CARTESIAN_POINT('Ctrl Pts',(1.35705080756892,2.29132664526027E-15,
-7.87499999999999));
#410013=CARTESIAN_POINT('Ctrl Pts',(1.01778810567669,0.587620236790438,
-7.83333333333332));
#410014=CARTESIAN_POINT('Ctrl Pts',(0.67852540378446,1.17524047358087,-7.79166666666666));
#410015=CARTESIAN_POINT('Ctrl Pts',(0.,1.17524047358087,-7.74999999999999));
#410016=CARTESIAN_POINT('Ctrl Pts',(-0.678525403784459,1.17524047358087,
-7.70833333333332));
#410017=CARTESIAN_POINT('Ctrl Pts',(-1.01778810567669,0.587620236790438,
-7.66666666666666));
#410018=CARTESIAN_POINT('Ctrl Pts',(-1.35705080756892,2.62370823081419E-15,
-7.62499999999999));
#410019=CARTESIAN_POINT('Ctrl Pts',(-1.01778810567669,-0.587620236790433,
-7.58333333333332));
#410020=CARTESIAN_POINT('Ctrl Pts',(-0.67852540378446,-1.17524047358087,
-7.54166666666666));
#410021=CARTESIAN_POINT('Ctrl Pts',(-1.43925448419923E-16,-1.17524047358087,
-7.49999999999999));
#410022=CARTESIAN_POINT('Origin',(0.,-1.11022302462516E-14,-14.21875));
#410023=CARTESIAN_POINT('',(-8.32001735975286E-31,-1.17524047358087,-6.93749999999999));
#410024=CARTESIAN_POINT('',(-8.32001735975286E-31,-1.17524047358087,-6.99999999999999));
#410025=CARTESIAN_POINT('',(1.43925448419925E-16,-1.1752404735809,-14.21875));
#410026=CARTESIAN_POINT('Ctrl Pts',(-1.43925448419923E-16,-1.17524047358087,
-7.43749999999999));
#410027=CARTESIAN_POINT('Ctrl Pts',(0.678525403784459,-1.17524047358087,
-7.39583333333332));
#410028=CARTESIAN_POINT('Ctrl Pts',(1.01778810567669,-0.587620236790434,
-7.35416666666666));
#410029=CARTESIAN_POINT('Ctrl Pts',(1.35705080756892,2.29132664526027E-15,
-7.31249999999999));
#410030=CARTESIAN_POINT('Ctrl Pts',(1.01778810567669,0.587620236790438,
-7.27083333333332));
#410031=CARTESIAN_POINT('Ctrl Pts',(0.67852540378446,1.17524047358087,-7.22916666666666));
#410032=CARTESIAN_POINT('Ctrl Pts',(0.,1.17524047358087,-7.18749999999999));
#410033=CARTESIAN_POINT('Ctrl Pts',(-0.678525403784459,1.17524047358087,
-7.14583333333332));
#410034=CARTESIAN_POINT('Ctrl Pts',(-1.01778810567669,0.587620236790438,
-7.10416666666666));
#410035=CARTESIAN_POINT('Ctrl Pts',(-1.35705080756892,2.62370823081419E-15,
-7.06249999999999));
#410036=CARTESIAN_POINT('Ctrl Pts',(-1.01778810567669,-0.587620236790433,
-7.02083333333332));
#410037=CARTESIAN_POINT('Ctrl Pts',(-0.67852540378446,-1.17524047358087,
-6.97916666666666));
#410038=CARTESIAN_POINT('Ctrl Pts',(-1.43925448419923E-16,-1.17524047358087,
-6.93749999999999));
#410039=CARTESIAN_POINT('Ctrl Pts',(-1.43925448419923E-16,-1.17524047358087,
-7.49999999999999));
#410040=CARTESIAN_POINT('Ctrl Pts',(0.678525403784459,-1.17524047358087,
-7.45833333333332));
#410041=CARTESIAN_POINT('Ctrl Pts',(1.01778810567669,-0.587620236790434,
-7.41666666666666));
#410042=CARTESIAN_POINT('Ctrl Pts',(1.35705080756892,2.29132664526027E-15,
-7.37499999999999));
#410043=CARTESIAN_POINT('Ctrl Pts',(1.01778810567669,0.587620236790438,
-7.33333333333332));
#410044=CARTESIAN_POINT('Ctrl Pts',(0.67852540378446,1.17524047358087,-7.29166666666666));
#410045=CARTESIAN_POINT('Ctrl Pts',(0.,1.17524047358087,-7.24999999999999));
#410046=CARTESIAN_POINT('Ctrl Pts',(-0.678525403784459,1.17524047358087,
-7.20833333333332));
#410047=CARTESIAN_POINT('Ctrl Pts',(-1.01778810567669,0.587620236790438,
-7.16666666666666));
#410048=CARTESIAN_POINT('Ctrl Pts',(-1.35705080756892,2.62370823081419E-15,
-7.12499999999999));
#410049=CARTESIAN_POINT('Ctrl Pts',(-1.01778810567669,-0.587620236790433,
-7.08333333333332));
#410050=CARTESIAN_POINT('Ctrl Pts',(-0.67852540378446,-1.17524047358087,
-7.04166666666666));
#410051=CARTESIAN_POINT('Ctrl Pts',(-1.43925448419923E-16,-1.17524047358087,
-6.99999999999999));
#410052=CARTESIAN_POINT('Origin',(0.,-1.11022302462516E-14,-14.21875));
#410053=CARTESIAN_POINT('',(-8.32001735975286E-31,-1.17524047358087,-6.43749999999999));
#410054=CARTESIAN_POINT('',(-8.32001735975286E-31,-1.17524047358087,-6.49999999999999));
#410055=CARTESIAN_POINT('',(1.43925448419925E-16,-1.1752404735809,-14.21875));
#410056=CARTESIAN_POINT('Ctrl Pts',(-1.43925448419923E-16,-1.17524047358087,
-6.93749999999999));
#410057=CARTESIAN_POINT('Ctrl Pts',(0.678525403784459,-1.17524047358087,
-6.89583333333332));
#410058=CARTESIAN_POINT('Ctrl Pts',(1.01778810567669,-0.587620236790434,
-6.85416666666666));
#410059=CARTESIAN_POINT('Ctrl Pts',(1.35705080756892,2.29132664526027E-15,
-6.81249999999999));
#410060=CARTESIAN_POINT('Ctrl Pts',(1.01778810567669,0.587620236790438,
-6.77083333333333));
#410061=CARTESIAN_POINT('Ctrl Pts',(0.67852540378446,1.17524047358087,-6.72916666666666));
#410062=CARTESIAN_POINT('Ctrl Pts',(0.,1.17524047358087,-6.68749999999999));
#410063=CARTESIAN_POINT('Ctrl Pts',(-0.678525403784459,1.17524047358087,
-6.64583333333332));
#410064=CARTESIAN_POINT('Ctrl Pts',(-1.01778810567669,0.587620236790438,
-6.60416666666666));
#410065=CARTESIAN_POINT('Ctrl Pts',(-1.35705080756892,2.62370823081419E-15,
-6.56249999999999));
#410066=CARTESIAN_POINT('Ctrl Pts',(-1.01778810567669,-0.587620236790433,
-6.52083333333333));
#410067=CARTESIAN_POINT('Ctrl Pts',(-0.67852540378446,-1.17524047358087,
-6.47916666666666));
#410068=CARTESIAN_POINT('Ctrl Pts',(-1.43925448419923E-16,-1.17524047358087,
-6.43749999999999));
#410069=CARTESIAN_POINT('Ctrl Pts',(-1.43925448419923E-16,-1.17524047358087,
-6.99999999999999));
#410070=CARTESIAN_POINT('Ctrl Pts',(0.678525403784459,-1.17524047358087,
-6.95833333333332));
#410071=CARTESIAN_POINT('Ctrl Pts',(1.01778810567669,-0.587620236790434,
-6.91666666666666));
#410072=CARTESIAN_POINT('Ctrl Pts',(1.35705080756892,2.29132664526027E-15,
-6.87499999999999));
#410073=CARTESIAN_POINT('Ctrl Pts',(1.01778810567669,0.587620236790438,
-6.83333333333333));
#410074=CARTESIAN_POINT('Ctrl Pts',(0.67852540378446,1.17524047358087,-6.79166666666666));
#410075=CARTESIAN_POINT('Ctrl Pts',(0.,1.17524047358087,-6.74999999999999));
#410076=CARTESIAN_POINT('Ctrl Pts',(-0.678525403784459,1.17524047358087,
-6.70833333333333));
#410077=CARTESIAN_POINT('Ctrl Pts',(-1.01778810567669,0.587620236790438,
-6.66666666666666));
#410078=CARTESIAN_POINT('Ctrl Pts',(-1.35705080756892,2.62370823081419E-15,
-6.62499999999999));
#410079=CARTESIAN_POINT('Ctrl Pts',(-1.01778810567669,-0.587620236790433,
-6.58333333333332));
#410080=CARTESIAN_POINT('Ctrl Pts',(-0.67852540378446,-1.17524047358087,
-6.54166666666666));
#410081=CARTESIAN_POINT('Ctrl Pts',(-1.43925448419923E-16,-1.17524047358087,
-6.49999999999999));
#410082=CARTESIAN_POINT('Origin',(0.,-1.11022302462516E-14,-14.21875));
#410083=CARTESIAN_POINT('',(-8.32001735975286E-31,-1.17524047358087,-5.93749999999999));
#410084=CARTESIAN_POINT('',(-8.32001735975286E-31,-1.17524047358087,-5.99999999999999));
#410085=CARTESIAN_POINT('',(1.43925448419925E-16,-1.1752404735809,-14.21875));
#410086=CARTESIAN_POINT('Ctrl Pts',(-1.43925448419923E-16,-1.17524047358087,
-6.43749999999999));
#410087=CARTESIAN_POINT('Ctrl Pts',(0.678525403784459,-1.17524047358087,
-6.39583333333333));
#410088=CARTESIAN_POINT('Ctrl Pts',(1.01778810567669,-0.587620236790434,
-6.35416666666666));
#410089=CARTESIAN_POINT('Ctrl Pts',(1.35705080756892,2.29132664526027E-15,
-6.31249999999999));
#410090=CARTESIAN_POINT('Ctrl Pts',(1.01778810567669,0.587620236790438,
-6.27083333333332));
#410091=CARTESIAN_POINT('Ctrl Pts',(0.67852540378446,1.17524047358087,-6.22916666666666));
#410092=CARTESIAN_POINT('Ctrl Pts',(0.,1.17524047358087,-6.18749999999999));
#410093=CARTESIAN_POINT('Ctrl Pts',(-0.678525403784459,1.17524047358087,
-6.14583333333333));
#410094=CARTESIAN_POINT('Ctrl Pts',(-1.01778810567669,0.587620236790438,
-6.10416666666666));
#410095=CARTESIAN_POINT('Ctrl Pts',(-1.35705080756892,2.62370823081419E-15,
-6.06249999999999));
#410096=CARTESIAN_POINT('Ctrl Pts',(-1.01778810567669,-0.587620236790433,
-6.02083333333332));
#410097=CARTESIAN_POINT('Ctrl Pts',(-0.67852540378446,-1.17524047358087,
-5.97916666666666));
#410098=CARTESIAN_POINT('Ctrl Pts',(-1.43925448419923E-16,-1.17524047358087,
-5.93749999999999));
#410099=CARTESIAN_POINT('Ctrl Pts',(-1.43925448419923E-16,-1.17524047358087,
-6.49999999999999));
#410100=CARTESIAN_POINT('Ctrl Pts',(0.678525403784459,-1.17524047358087,
-6.45833333333333));
#410101=CARTESIAN_POINT('Ctrl Pts',(1.01778810567669,-0.587620236790434,
-6.41666666666666));
#410102=CARTESIAN_POINT('Ctrl Pts',(1.35705080756892,2.29132664526027E-15,
-6.37499999999999));
#410103=CARTESIAN_POINT('Ctrl Pts',(1.01778810567669,0.587620236790438,
-6.33333333333332));
#410104=CARTESIAN_POINT('Ctrl Pts',(0.67852540378446,1.17524047358087,-6.29166666666666));
#410105=CARTESIAN_POINT('Ctrl Pts',(0.,1.17524047358087,-6.24999999999999));
#410106=CARTESIAN_POINT('Ctrl Pts',(-0.678525403784459,1.17524047358087,
-6.20833333333333));
#410107=CARTESIAN_POINT('Ctrl Pts',(-1.01778810567669,0.587620236790438,
-6.16666666666666));
#410108=CARTESIAN_POINT('Ctrl Pts',(-1.35705080756892,2.62370823081419E-15,
-6.12499999999999));
#410109=CARTESIAN_POINT('Ctrl Pts',(-1.01778810567669,-0.587620236790433,
-6.08333333333333));
#410110=CARTESIAN_POINT('Ctrl Pts',(-0.67852540378446,-1.17524047358087,
-6.04166666666666));
#410111=CARTESIAN_POINT('Ctrl Pts',(-1.43925448419923E-16,-1.17524047358087,
-5.99999999999999));
#410112=CARTESIAN_POINT('Origin',(0.,-1.11022302462516E-14,-14.21875));
#410113=CARTESIAN_POINT('',(-8.32001735975286E-31,-1.17524047358087,-5.43749999999999));
#410114=CARTESIAN_POINT('',(-8.32001735975286E-31,-1.17524047358087,-5.49999999999999));
#410115=CARTESIAN_POINT('',(1.43925448419925E-16,-1.1752404735809,-14.21875));
#410116=CARTESIAN_POINT('Ctrl Pts',(-1.43925448419923E-16,-1.17524047358087,
-5.93749999999999));
#410117=CARTESIAN_POINT('Ctrl Pts',(0.678525403784459,-1.17524047358087,
-5.89583333333333));
#410118=CARTESIAN_POINT('Ctrl Pts',(1.01778810567669,-0.587620236790434,
-5.85416666666666));
#410119=CARTESIAN_POINT('Ctrl Pts',(1.35705080756892,2.29132664526027E-15,
-5.81249999999999));
#410120=CARTESIAN_POINT('Ctrl Pts',(1.01778810567669,0.587620236790438,
-5.77083333333332));
#410121=CARTESIAN_POINT('Ctrl Pts',(0.67852540378446,1.17524047358087,-5.72916666666666));
#410122=CARTESIAN_POINT('Ctrl Pts',(0.,1.17524047358087,-5.68749999999999));
#410123=CARTESIAN_POINT('Ctrl Pts',(-0.678525403784459,1.17524047358087,
-5.64583333333332));
#410124=CARTESIAN_POINT('Ctrl Pts',(-1.01778810567669,0.587620236790438,
-5.60416666666666));
#410125=CARTESIAN_POINT('Ctrl Pts',(-1.35705080756892,2.62370823081419E-15,
-5.56249999999999));
#410126=CARTESIAN_POINT('Ctrl Pts',(-1.01778810567669,-0.587620236790433,
-5.52083333333333));
#410127=CARTESIAN_POINT('Ctrl Pts',(-0.67852540378446,-1.17524047358087,
-5.47916666666666));
#410128=CARTESIAN_POINT('Ctrl Pts',(-1.43925448419923E-16,-1.17524047358087,
-5.43749999999999));
#410129=CARTESIAN_POINT('Ctrl Pts',(-1.43925448419923E-16,-1.17524047358087,
-5.99999999999999));
#410130=CARTESIAN_POINT('Ctrl Pts',(0.678525403784459,-1.17524047358087,
-5.95833333333332));
#410131=CARTESIAN_POINT('Ctrl Pts',(1.01778810567669,-0.587620236790434,
-5.91666666666666));
#410132=CARTESIAN_POINT('Ctrl Pts',(1.35705080756892,2.29132664526027E-15,
-5.87499999999999));
#410133=CARTESIAN_POINT('Ctrl Pts',(1.01778810567669,0.587620236790438,
-5.83333333333333));
#410134=CARTESIAN_POINT('Ctrl Pts',(0.67852540378446,1.17524047358087,-5.79166666666666));
#410135=CARTESIAN_POINT('Ctrl Pts',(0.,1.17524047358087,-5.74999999999999));
#410136=CARTESIAN_POINT('Ctrl Pts',(-0.678525403784459,1.17524047358087,
-5.70833333333332));
#410137=CARTESIAN_POINT('Ctrl Pts',(-1.01778810567669,0.587620236790438,
-5.66666666666666));
#410138=CARTESIAN_POINT('Ctrl Pts',(-1.35705080756892,2.62370823081419E-15,
-5.62499999999999));
#410139=CARTESIAN_POINT('Ctrl Pts',(-1.01778810567669,-0.587620236790433,
-5.58333333333333));
#410140=CARTESIAN_POINT('Ctrl Pts',(-0.67852540378446,-1.17524047358087,
-5.54166666666666));
#410141=CARTESIAN_POINT('Ctrl Pts',(-1.43925448419923E-16,-1.17524047358087,
-5.49999999999999));
#410142=CARTESIAN_POINT('Origin',(0.,-1.11022302462516E-14,-14.21875));
#410143=CARTESIAN_POINT('',(-8.32001735975286E-31,-1.17524047358087,-4.93749999999999));
#410144=CARTESIAN_POINT('',(-8.32001735975286E-31,-1.17524047358087,-4.99999999999999));
#410145=CARTESIAN_POINT('',(1.43925448419925E-16,-1.1752404735809,-14.21875));
#410146=CARTESIAN_POINT('Ctrl Pts',(-1.43925448419923E-16,-1.17524047358087,
-5.43749999999999));
#410147=CARTESIAN_POINT('Ctrl Pts',(0.678525403784459,-1.17524047358087,
-5.39583333333332));
#410148=CARTESIAN_POINT('Ctrl Pts',(1.01778810567669,-0.587620236790434,
-5.35416666666666));
#410149=CARTESIAN_POINT('Ctrl Pts',(1.35705080756892,2.29132664526027E-15,
-5.31249999999999));
#410150=CARTESIAN_POINT('Ctrl Pts',(1.01778810567669,0.587620236790438,
-5.27083333333332));
#410151=CARTESIAN_POINT('Ctrl Pts',(0.67852540378446,1.17524047358087,-5.22916666666666));
#410152=CARTESIAN_POINT('Ctrl Pts',(0.,1.17524047358087,-5.18749999999999));
#410153=CARTESIAN_POINT('Ctrl Pts',(-0.678525403784459,1.17524047358087,
-5.14583333333332));
#410154=CARTESIAN_POINT('Ctrl Pts',(-1.01778810567669,0.587620236790438,
-5.10416666666666));
#410155=CARTESIAN_POINT('Ctrl Pts',(-1.35705080756892,2.62370823081419E-15,
-5.06249999999999));
#410156=CARTESIAN_POINT('Ctrl Pts',(-1.01778810567669,-0.587620236790433,
-5.02083333333332));
#410157=CARTESIAN_POINT('Ctrl Pts',(-0.67852540378446,-1.17524047358087,
-4.97916666666666));
#410158=CARTESIAN_POINT('Ctrl Pts',(-1.43925448419923E-16,-1.17524047358087,
-4.93749999999999));
#410159=CARTESIAN_POINT('Ctrl Pts',(-1.43925448419923E-16,-1.17524047358087,
-5.49999999999999));
#410160=CARTESIAN_POINT('Ctrl Pts',(0.678525403784459,-1.17524047358087,
-5.45833333333332));
#410161=CARTESIAN_POINT('Ctrl Pts',(1.01778810567669,-0.587620236790434,
-5.41666666666666));
#410162=CARTESIAN_POINT('Ctrl Pts',(1.35705080756892,2.29132664526027E-15,
-5.37499999999999));
#410163=CARTESIAN_POINT('Ctrl Pts',(1.01778810567669,0.587620236790438,
-5.33333333333332));
#410164=CARTESIAN_POINT('Ctrl Pts',(0.67852540378446,1.17524047358087,-5.29166666666666));
#410165=CARTESIAN_POINT('Ctrl Pts',(0.,1.17524047358087,-5.24999999999999));
#410166=CARTESIAN_POINT('Ctrl Pts',(-0.678525403784459,1.17524047358087,
-5.20833333333332));
#410167=CARTESIAN_POINT('Ctrl Pts',(-1.01778810567669,0.587620236790438,
-5.16666666666666));
#410168=CARTESIAN_POINT('Ctrl Pts',(-1.35705080756892,2.62370823081419E-15,
-5.12499999999999));
#410169=CARTESIAN_POINT('Ctrl Pts',(-1.01778810567669,-0.587620236790433,
-5.08333333333332));
#410170=CARTESIAN_POINT('Ctrl Pts',(-0.67852540378446,-1.17524047358087,
-5.04166666666666));
#410171=CARTESIAN_POINT('Ctrl Pts',(-1.43925448419923E-16,-1.17524047358087,
-4.99999999999999));
#410172=CARTESIAN_POINT('Origin',(0.,-1.11022302462516E-14,-14.21875));
#410173=CARTESIAN_POINT('',(-8.32001735975286E-31,-1.17524047358087,-4.43749999999999));
#410174=CARTESIAN_POINT('',(-8.32001735975286E-31,-1.17524047358087,-4.49999999999999));
#410175=CARTESIAN_POINT('',(1.43925448419925E-16,-1.1752404735809,-14.21875));
#410176=CARTESIAN_POINT('Ctrl Pts',(-1.43925448419923E-16,-1.17524047358087,
-4.93749999999999));
#410177=CARTESIAN_POINT('Ctrl Pts',(0.678525403784459,-1.17524047358087,
-4.89583333333332));
#410178=CARTESIAN_POINT('Ctrl Pts',(1.01778810567669,-0.587620236790434,
-4.85416666666666));
#410179=CARTESIAN_POINT('Ctrl Pts',(1.35705080756892,2.29132664526027E-15,
-4.81249999999999));
#410180=CARTESIAN_POINT('Ctrl Pts',(1.01778810567669,0.587620236790438,
-4.77083333333332));
#410181=CARTESIAN_POINT('Ctrl Pts',(0.67852540378446,1.17524047358087,-4.72916666666666));
#410182=CARTESIAN_POINT('Ctrl Pts',(0.,1.17524047358087,-4.68749999999999));
#410183=CARTESIAN_POINT('Ctrl Pts',(-0.678525403784459,1.17524047358087,
-4.64583333333332));
#410184=CARTESIAN_POINT('Ctrl Pts',(-1.01778810567669,0.587620236790438,
-4.60416666666666));
#410185=CARTESIAN_POINT('Ctrl Pts',(-1.35705080756892,2.62370823081419E-15,
-4.56249999999999));
#410186=CARTESIAN_POINT('Ctrl Pts',(-1.01778810567669,-0.587620236790433,
-4.52083333333332));
#410187=CARTESIAN_POINT('Ctrl Pts',(-0.67852540378446,-1.17524047358087,
-4.47916666666666));
#410188=CARTESIAN_POINT('Ctrl Pts',(-1.43925448419923E-16,-1.17524047358087,
-4.43749999999999));
#410189=CARTESIAN_POINT('Ctrl Pts',(-1.43925448419923E-16,-1.17524047358087,
-4.99999999999999));
#410190=CARTESIAN_POINT('Ctrl Pts',(0.678525403784459,-1.17524047358087,
-4.95833333333332));
#410191=CARTESIAN_POINT('Ctrl Pts',(1.01778810567669,-0.587620236790434,
-4.91666666666666));
#410192=CARTESIAN_POINT('Ctrl Pts',(1.35705080756892,2.29132664526027E-15,
-4.87499999999999));
#410193=CARTESIAN_POINT('Ctrl Pts',(1.01778810567669,0.587620236790438,
-4.83333333333332));
#410194=CARTESIAN_POINT('Ctrl Pts',(0.67852540378446,1.17524047358087,-4.79166666666666));
#410195=CARTESIAN_POINT('Ctrl Pts',(0.,1.17524047358087,-4.74999999999999));
#410196=CARTESIAN_POINT('Ctrl Pts',(-0.678525403784459,1.17524047358087,
-4.70833333333332));
#410197=CARTESIAN_POINT('Ctrl Pts',(-1.01778810567669,0.587620236790438,
-4.66666666666666));
#410198=CARTESIAN_POINT('Ctrl Pts',(-1.35705080756892,2.62370823081419E-15,
-4.62499999999999));
#410199=CARTESIAN_POINT('Ctrl Pts',(-1.01778810567669,-0.587620236790433,
-4.58333333333332));
#410200=CARTESIAN_POINT('Ctrl Pts',(-0.67852540378446,-1.17524047358087,
-4.54166666666666));
#410201=CARTESIAN_POINT('Ctrl Pts',(-1.43925448419923E-16,-1.17524047358087,
-4.49999999999999));
#410202=CARTESIAN_POINT('Origin',(0.,-1.11022302462516E-14,-14.21875));
#410203=CARTESIAN_POINT('',(-8.32001735975286E-31,-1.17524047358087,-3.93749999999999));
#410204=CARTESIAN_POINT('',(-8.32001735975286E-31,-1.17524047358087,-3.99999999999999));
#410205=CARTESIAN_POINT('',(1.43925448419925E-16,-1.1752404735809,-14.21875));
#410206=CARTESIAN_POINT('Ctrl Pts',(-1.43925448419923E-16,-1.17524047358087,
-4.43749999999999));
#410207=CARTESIAN_POINT('Ctrl Pts',(0.678525403784459,-1.17524047358087,
-4.39583333333332));
#410208=CARTESIAN_POINT('Ctrl Pts',(1.01778810567669,-0.587620236790434,
-4.35416666666666));
#410209=CARTESIAN_POINT('Ctrl Pts',(1.35705080756892,2.29132664526027E-15,
-4.31249999999999));
#410210=CARTESIAN_POINT('Ctrl Pts',(1.01778810567669,0.587620236790438,
-4.27083333333332));
#410211=CARTESIAN_POINT('Ctrl Pts',(0.67852540378446,1.17524047358087,-4.22916666666666));
#410212=CARTESIAN_POINT('Ctrl Pts',(0.,1.17524047358087,-4.18749999999999));
#410213=CARTESIAN_POINT('Ctrl Pts',(-0.678525403784459,1.17524047358087,
-4.14583333333332));
#410214=CARTESIAN_POINT('Ctrl Pts',(-1.01778810567669,0.587620236790438,
-4.10416666666666));
#410215=CARTESIAN_POINT('Ctrl Pts',(-1.35705080756892,2.62370823081419E-15,
-4.06249999999999));
#410216=CARTESIAN_POINT('Ctrl Pts',(-1.01778810567669,-0.587620236790433,
-4.02083333333333));
#410217=CARTESIAN_POINT('Ctrl Pts',(-0.67852540378446,-1.17524047358087,
-3.97916666666666));
#410218=CARTESIAN_POINT('Ctrl Pts',(-1.43925448419923E-16,-1.17524047358087,
-3.93749999999999));
#410219=CARTESIAN_POINT('Ctrl Pts',(-1.43925448419923E-16,-1.17524047358087,
-4.49999999999999));
#410220=CARTESIAN_POINT('Ctrl Pts',(0.678525403784459,-1.17524047358087,
-4.45833333333332));
#410221=CARTESIAN_POINT('Ctrl Pts',(1.01778810567669,-0.587620236790434,
-4.41666666666666));
#410222=CARTESIAN_POINT('Ctrl Pts',(1.35705080756892,2.29132664526027E-15,
-4.37499999999999));
#410223=CARTESIAN_POINT('Ctrl Pts',(1.01778810567669,0.587620236790438,
-4.33333333333333));
#410224=CARTESIAN_POINT('Ctrl Pts',(0.67852540378446,1.17524047358087,-4.29166666666666));
#410225=CARTESIAN_POINT('Ctrl Pts',(0.,1.17524047358087,-4.24999999999999));
#410226=CARTESIAN_POINT('Ctrl Pts',(-0.678525403784459,1.17524047358087,
-4.20833333333332));
#410227=CARTESIAN_POINT('Ctrl Pts',(-1.01778810567669,0.587620236790438,
-4.16666666666666));
#410228=CARTESIAN_POINT('Ctrl Pts',(-1.35705080756892,2.62370823081419E-15,
-4.12499999999999));
#410229=CARTESIAN_POINT('Ctrl Pts',(-1.01778810567669,-0.587620236790433,
-4.08333333333332));
#410230=CARTESIAN_POINT('Ctrl Pts',(-0.67852540378446,-1.17524047358087,
-4.04166666666666));
#410231=CARTESIAN_POINT('Ctrl Pts',(-1.43925448419923E-16,-1.17524047358087,
-3.99999999999999));
#410232=CARTESIAN_POINT('Origin',(0.,-1.11022302462516E-14,-14.21875));
#410233=CARTESIAN_POINT('',(-8.32001735975286E-31,-1.17524047358087,-3.43749999999999));
#410234=CARTESIAN_POINT('',(-8.32001735975286E-31,-1.17524047358087,-3.49999999999999));
#410235=CARTESIAN_POINT('',(1.43925448419925E-16,-1.1752404735809,-14.21875));
#410236=CARTESIAN_POINT('Ctrl Pts',(-1.43925448419923E-16,-1.17524047358087,
-3.93749999999999));
#410237=CARTESIAN_POINT('Ctrl Pts',(0.678525403784459,-1.17524047358087,
-3.89583333333332));
#410238=CARTESIAN_POINT('Ctrl Pts',(1.01778810567669,-0.587620236790434,
-3.85416666666666));
#410239=CARTESIAN_POINT('Ctrl Pts',(1.35705080756892,2.29132664526027E-15,
-3.81249999999999));
#410240=CARTESIAN_POINT('Ctrl Pts',(1.01778810567669,0.587620236790438,
-3.77083333333332));
#410241=CARTESIAN_POINT('Ctrl Pts',(0.67852540378446,1.17524047358087,-3.72916666666666));
#410242=CARTESIAN_POINT('Ctrl Pts',(0.,1.17524047358087,-3.68749999999999));
#410243=CARTESIAN_POINT('Ctrl Pts',(-0.678525403784459,1.17524047358087,
-3.64583333333332));
#410244=CARTESIAN_POINT('Ctrl Pts',(-1.01778810567669,0.587620236790438,
-3.60416666666666));
#410245=CARTESIAN_POINT('Ctrl Pts',(-1.35705080756892,2.62370823081419E-15,
-3.56249999999999));
#410246=CARTESIAN_POINT('Ctrl Pts',(-1.01778810567669,-0.587620236790433,
-3.52083333333332));
#410247=CARTESIAN_POINT('Ctrl Pts',(-0.67852540378446,-1.17524047358087,
-3.47916666666666));
#410248=CARTESIAN_POINT('Ctrl Pts',(-1.43925448419923E-16,-1.17524047358087,
-3.43749999999999));
#410249=CARTESIAN_POINT('Ctrl Pts',(-1.43925448419923E-16,-1.17524047358087,
-3.99999999999999));
#410250=CARTESIAN_POINT('Ctrl Pts',(0.678525403784459,-1.17524047358087,
-3.95833333333332));
#410251=CARTESIAN_POINT('Ctrl Pts',(1.01778810567669,-0.587620236790434,
-3.91666666666666));
#410252=CARTESIAN_POINT('Ctrl Pts',(1.35705080756892,2.29132664526027E-15,
-3.87499999999999));
#410253=CARTESIAN_POINT('Ctrl Pts',(1.01778810567669,0.587620236790438,
-3.83333333333332));
#410254=CARTESIAN_POINT('Ctrl Pts',(0.67852540378446,1.17524047358087,-3.79166666666666));
#410255=CARTESIAN_POINT('Ctrl Pts',(0.,1.17524047358087,-3.74999999999999));
#410256=CARTESIAN_POINT('Ctrl Pts',(-0.678525403784459,1.17524047358087,
-3.70833333333332));
#410257=CARTESIAN_POINT('Ctrl Pts',(-1.01778810567669,0.587620236790438,
-3.66666666666666));
#410258=CARTESIAN_POINT('Ctrl Pts',(-1.35705080756892,2.62370823081419E-15,
-3.62499999999999));
#410259=CARTESIAN_POINT('Ctrl Pts',(-1.01778810567669,-0.587620236790433,
-3.58333333333332));
#410260=CARTESIAN_POINT('Ctrl Pts',(-0.67852540378446,-1.17524047358087,
-3.54166666666666));
#410261=CARTESIAN_POINT('Ctrl Pts',(-1.43925448419923E-16,-1.17524047358087,
-3.49999999999999));
#410262=CARTESIAN_POINT('Origin',(0.,-1.11022302462516E-14,-14.21875));
#410263=CARTESIAN_POINT('',(-8.32001735975286E-31,-1.17524047358087,-2.93749999999999));
#410264=CARTESIAN_POINT('',(-8.32001735975286E-31,-1.17524047358087,-2.99999999999999));
#410265=CARTESIAN_POINT('',(1.43925448419925E-16,-1.1752404735809,-14.21875));
#410266=CARTESIAN_POINT('Ctrl Pts',(-1.43925448419923E-16,-1.17524047358087,
-3.43749999999999));
#410267=CARTESIAN_POINT('Ctrl Pts',(0.678525403784459,-1.17524047358087,
-3.39583333333332));
#410268=CARTESIAN_POINT('Ctrl Pts',(1.01778810567669,-0.587620236790434,
-3.35416666666666));
#410269=CARTESIAN_POINT('Ctrl Pts',(1.35705080756892,2.29132664526027E-15,
-3.31249999999999));
#410270=CARTESIAN_POINT('Ctrl Pts',(1.01778810567669,0.587620236790438,
-3.27083333333332));
#410271=CARTESIAN_POINT('Ctrl Pts',(0.67852540378446,1.17524047358087,-3.22916666666666));
#410272=CARTESIAN_POINT('Ctrl Pts',(0.,1.17524047358087,-3.18749999999999));
#410273=CARTESIAN_POINT('Ctrl Pts',(-0.678525403784459,1.17524047358087,
-3.14583333333332));
#410274=CARTESIAN_POINT('Ctrl Pts',(-1.01778810567669,0.587620236790438,
-3.10416666666666));
#410275=CARTESIAN_POINT('Ctrl Pts',(-1.35705080756892,2.62370823081419E-15,
-3.06249999999999));
#410276=CARTESIAN_POINT('Ctrl Pts',(-1.01778810567669,-0.587620236790433,
-3.02083333333332));
#410277=CARTESIAN_POINT('Ctrl Pts',(-0.67852540378446,-1.17524047358087,
-2.97916666666666));
#410278=CARTESIAN_POINT('Ctrl Pts',(-1.43925448419923E-16,-1.17524047358087,
-2.93749999999999));
#410279=CARTESIAN_POINT('Ctrl Pts',(-1.43925448419923E-16,-1.17524047358087,
-3.49999999999999));
#410280=CARTESIAN_POINT('Ctrl Pts',(0.678525403784459,-1.17524047358087,
-3.45833333333333));
#410281=CARTESIAN_POINT('Ctrl Pts',(1.01778810567669,-0.587620236790434,
-3.41666666666666));
#410282=CARTESIAN_POINT('Ctrl Pts',(1.35705080756892,2.29132664526027E-15,
-3.37499999999999));
#410283=CARTESIAN_POINT('Ctrl Pts',(1.01778810567669,0.587620236790438,
-3.33333333333332));
#410284=CARTESIAN_POINT('Ctrl Pts',(0.67852540378446,1.17524047358087,-3.29166666666666));
#410285=CARTESIAN_POINT('Ctrl Pts',(0.,1.17524047358087,-3.24999999999999));
#410286=CARTESIAN_POINT('Ctrl Pts',(-0.678525403784459,1.17524047358087,
-3.20833333333332));
#410287=CARTESIAN_POINT('Ctrl Pts',(-1.01778810567669,0.587620236790438,
-3.16666666666666));
#410288=CARTESIAN_POINT('Ctrl Pts',(-1.35705080756892,2.62370823081419E-15,
-3.12499999999999));
#410289=CARTESIAN_POINT('Ctrl Pts',(-1.01778810567669,-0.587620236790433,
-3.08333333333332));
#410290=CARTESIAN_POINT('Ctrl Pts',(-0.67852540378446,-1.17524047358087,
-3.04166666666666));
#410291=CARTESIAN_POINT('Ctrl Pts',(-1.43925448419923E-16,-1.17524047358087,
-2.99999999999999));
#410292=CARTESIAN_POINT('Origin',(0.,-1.11022302462516E-14,-14.21875));
#410293=CARTESIAN_POINT('',(-8.32001735975286E-31,-1.17524047358087,-2.43749999999999));
#410294=CARTESIAN_POINT('',(-8.32001735975286E-31,-1.17524047358087,-2.49999999999999));
#410295=CARTESIAN_POINT('',(1.43925448419925E-16,-1.1752404735809,-14.21875));
#410296=CARTESIAN_POINT('Ctrl Pts',(-1.43925448419923E-16,-1.17524047358087,
-2.93749999999999));
#410297=CARTESIAN_POINT('Ctrl Pts',(0.678525403784459,-1.17524047358087,
-2.89583333333332));
#410298=CARTESIAN_POINT('Ctrl Pts',(1.01778810567669,-0.587620236790434,
-2.85416666666666));
#410299=CARTESIAN_POINT('Ctrl Pts',(1.35705080756892,2.29132664526027E-15,
-2.81249999999999));
#410300=CARTESIAN_POINT('Ctrl Pts',(1.01778810567669,0.587620236790438,
-2.77083333333332));
#410301=CARTESIAN_POINT('Ctrl Pts',(0.67852540378446,1.17524047358087,-2.72916666666666));
#410302=CARTESIAN_POINT('Ctrl Pts',(0.,1.17524047358087,-2.68749999999999));
#410303=CARTESIAN_POINT('Ctrl Pts',(-0.678525403784459,1.17524047358087,
-2.64583333333332));
#410304=CARTESIAN_POINT('Ctrl Pts',(-1.01778810567669,0.587620236790438,
-2.60416666666666));
#410305=CARTESIAN_POINT('Ctrl Pts',(-1.35705080756892,2.62370823081419E-15,
-2.56249999999999));
#410306=CARTESIAN_POINT('Ctrl Pts',(-1.01778810567669,-0.587620236790433,
-2.52083333333333));
#410307=CARTESIAN_POINT('Ctrl Pts',(-0.67852540378446,-1.17524047358087,
-2.47916666666666));
#410308=CARTESIAN_POINT('Ctrl Pts',(-1.43925448419923E-16,-1.17524047358087,
-2.43749999999999));
#410309=CARTESIAN_POINT('Ctrl Pts',(-1.43925448419923E-16,-1.17524047358087,
-2.99999999999999));
#410310=CARTESIAN_POINT('Ctrl Pts',(0.678525403784459,-1.17524047358087,
-2.95833333333332));
#410311=CARTESIAN_POINT('Ctrl Pts',(1.01778810567669,-0.587620236790434,
-2.91666666666666));
#410312=CARTESIAN_POINT('Ctrl Pts',(1.35705080756892,2.29132664526027E-15,
-2.87499999999999));
#410313=CARTESIAN_POINT('Ctrl Pts',(1.01778810567669,0.587620236790438,
-2.83333333333332));
#410314=CARTESIAN_POINT('Ctrl Pts',(0.67852540378446,1.17524047358087,-2.79166666666666));
#410315=CARTESIAN_POINT('Ctrl Pts',(0.,1.17524047358087,-2.74999999999999));
#410316=CARTESIAN_POINT('Ctrl Pts',(-0.678525403784459,1.17524047358087,
-2.70833333333332));
#410317=CARTESIAN_POINT('Ctrl Pts',(-1.01778810567669,0.587620236790438,
-2.66666666666666));
#410318=CARTESIAN_POINT('Ctrl Pts',(-1.35705080756892,2.62370823081419E-15,
-2.62499999999999));
#410319=CARTESIAN_POINT('Ctrl Pts',(-1.01778810567669,-0.587620236790433,
-2.58333333333332));
#410320=CARTESIAN_POINT('Ctrl Pts',(-0.67852540378446,-1.17524047358087,
-2.54166666666666));
#410321=CARTESIAN_POINT('Ctrl Pts',(-1.43925448419923E-16,-1.17524047358087,
-2.49999999999999));
#410322=CARTESIAN_POINT('Origin',(0.,-1.11022302462516E-14,-14.21875));
#410323=CARTESIAN_POINT('',(-8.32001735975286E-31,-1.17524047358087,-1.93749999999999));
#410324=CARTESIAN_POINT('',(-8.32001735975286E-31,-1.17524047358087,-1.99999999999999));
#410325=CARTESIAN_POINT('',(1.43925448419925E-16,-1.1752404735809,-14.21875));
#410326=CARTESIAN_POINT('Ctrl Pts',(-1.43925448419923E-16,-1.17524047358087,
-2.43749999999999));
#410327=CARTESIAN_POINT('Ctrl Pts',(0.678525403784459,-1.17524047358087,
-2.39583333333333));
#410328=CARTESIAN_POINT('Ctrl Pts',(1.01778810567669,-0.587620236790434,
-2.35416666666666));
#410329=CARTESIAN_POINT('Ctrl Pts',(1.35705080756892,2.29132664526027E-15,
-2.31249999999999));
#410330=CARTESIAN_POINT('Ctrl Pts',(1.01778810567669,0.587620236790438,
-2.27083333333332));
#410331=CARTESIAN_POINT('Ctrl Pts',(0.67852540378446,1.17524047358087,-2.22916666666666));
#410332=CARTESIAN_POINT('Ctrl Pts',(0.,1.17524047358087,-2.18749999999999));
#410333=CARTESIAN_POINT('Ctrl Pts',(-0.678525403784459,1.17524047358087,
-2.14583333333332));
#410334=CARTESIAN_POINT('Ctrl Pts',(-1.01778810567669,0.587620236790438,
-2.10416666666666));
#410335=CARTESIAN_POINT('Ctrl Pts',(-1.35705080756892,2.62370823081419E-15,
-2.06249999999999));
#410336=CARTESIAN_POINT('Ctrl Pts',(-1.01778810567669,-0.587620236790433,
-2.02083333333332));
#410337=CARTESIAN_POINT('Ctrl Pts',(-0.67852540378446,-1.17524047358087,
-1.97916666666666));
#410338=CARTESIAN_POINT('Ctrl Pts',(-1.43925448419923E-16,-1.17524047358087,
-1.93749999999999));
#410339=CARTESIAN_POINT('Ctrl Pts',(-1.43925448419923E-16,-1.17524047358087,
-2.49999999999999));
#410340=CARTESIAN_POINT('Ctrl Pts',(0.678525403784459,-1.17524047358087,
-2.45833333333332));
#410341=CARTESIAN_POINT('Ctrl Pts',(1.01778810567669,-0.587620236790434,
-2.41666666666666));
#410342=CARTESIAN_POINT('Ctrl Pts',(1.35705080756892,2.29132664526027E-15,
-2.37499999999999));
#410343=CARTESIAN_POINT('Ctrl Pts',(1.01778810567669,0.587620236790438,
-2.33333333333332));
#410344=CARTESIAN_POINT('Ctrl Pts',(0.67852540378446,1.17524047358087,-2.29166666666666));
#410345=CARTESIAN_POINT('Ctrl Pts',(0.,1.17524047358087,-2.24999999999999));
#410346=CARTESIAN_POINT('Ctrl Pts',(-0.678525403784459,1.17524047358087,
-2.20833333333332));
#410347=CARTESIAN_POINT('Ctrl Pts',(-1.01778810567669,0.587620236790438,
-2.16666666666666));
#410348=CARTESIAN_POINT('Ctrl Pts',(-1.35705080756892,2.62370823081419E-15,
-2.12499999999999));
#410349=CARTESIAN_POINT('Ctrl Pts',(-1.01778810567669,-0.587620236790433,
-2.08333333333332));
#410350=CARTESIAN_POINT('Ctrl Pts',(-0.67852540378446,-1.17524047358087,
-2.04166666666666));
#410351=CARTESIAN_POINT('Ctrl Pts',(-1.43925448419923E-16,-1.17524047358087,
-1.99999999999999));
#410352=CARTESIAN_POINT('Origin',(0.,-1.11022302462516E-14,-14.21875));
#410353=CARTESIAN_POINT('',(-8.32001735975286E-31,-1.17524047358087,-1.43749999999999));
#410354=CARTESIAN_POINT('',(-8.32001735975286E-31,-1.17524047358087,-1.49999999999999));
#410355=CARTESIAN_POINT('',(1.43925448419925E-16,-1.1752404735809,-14.21875));
#410356=CARTESIAN_POINT('Ctrl Pts',(-1.43925448419923E-16,-1.17524047358087,
-1.93749999999999));
#410357=CARTESIAN_POINT('Ctrl Pts',(0.678525403784459,-1.17524047358087,
-1.89583333333332));
#410358=CARTESIAN_POINT('Ctrl Pts',(1.01778810567669,-0.587620236790434,
-1.85416666666666));
#410359=CARTESIAN_POINT('Ctrl Pts',(1.35705080756892,2.29132664526027E-15,
-1.81249999999999));
#410360=CARTESIAN_POINT('Ctrl Pts',(1.01778810567669,0.587620236790438,
-1.77083333333332));
#410361=CARTESIAN_POINT('Ctrl Pts',(0.67852540378446,1.17524047358087,-1.72916666666666));
#410362=CARTESIAN_POINT('Ctrl Pts',(0.,1.17524047358087,-1.68749999999999));
#410363=CARTESIAN_POINT('Ctrl Pts',(-0.678525403784459,1.17524047358087,
-1.64583333333332));
#410364=CARTESIAN_POINT('Ctrl Pts',(-1.01778810567669,0.587620236790438,
-1.60416666666666));
#410365=CARTESIAN_POINT('Ctrl Pts',(-1.35705080756892,2.62370823081419E-15,
-1.56249999999999));
#410366=CARTESIAN_POINT('Ctrl Pts',(-1.01778810567669,-0.587620236790433,
-1.52083333333332));
#410367=CARTESIAN_POINT('Ctrl Pts',(-0.67852540378446,-1.17524047358087,
-1.47916666666666));
#410368=CARTESIAN_POINT('Ctrl Pts',(-1.43925448419923E-16,-1.17524047358087,
-1.43749999999999));
#410369=CARTESIAN_POINT('Ctrl Pts',(-1.43925448419923E-16,-1.17524047358087,
-1.99999999999999));
#410370=CARTESIAN_POINT('Ctrl Pts',(0.678525403784459,-1.17524047358087,
-1.95833333333332));
#410371=CARTESIAN_POINT('Ctrl Pts',(1.01778810567669,-0.587620236790434,
-1.91666666666666));
#410372=CARTESIAN_POINT('Ctrl Pts',(1.35705080756892,2.29132664526027E-15,
-1.87499999999999));
#410373=CARTESIAN_POINT('Ctrl Pts',(1.01778810567669,0.587620236790438,
-1.83333333333332));
#410374=CARTESIAN_POINT('Ctrl Pts',(0.67852540378446,1.17524047358087,-1.79166666666666));
#410375=CARTESIAN_POINT('Ctrl Pts',(0.,1.17524047358087,-1.74999999999999));
#410376=CARTESIAN_POINT('Ctrl Pts',(-0.678525403784459,1.17524047358087,
-1.70833333333332));
#410377=CARTESIAN_POINT('Ctrl Pts',(-1.01778810567669,0.587620236790438,
-1.66666666666666));
#410378=CARTESIAN_POINT('Ctrl Pts',(-1.35705080756892,2.62370823081419E-15,
-1.62499999999999));
#410379=CARTESIAN_POINT('Ctrl Pts',(-1.01778810567669,-0.587620236790433,
-1.58333333333332));
#410380=CARTESIAN_POINT('Ctrl Pts',(-0.67852540378446,-1.17524047358087,
-1.54166666666666));
#410381=CARTESIAN_POINT('Ctrl Pts',(-1.43925448419923E-16,-1.17524047358087,
-1.49999999999999));
#410382=CARTESIAN_POINT('Origin',(0.,-1.11022302462516E-14,-14.21875));
#410383=CARTESIAN_POINT('',(-8.32001735975286E-31,-1.17524047358087,-0.937499999999991));
#410384=CARTESIAN_POINT('',(-8.32001735975286E-31,-1.17524047358087,-0.99999999999999));
#410385=CARTESIAN_POINT('',(1.43925448419925E-16,-1.1752404735809,-14.21875));
#410386=CARTESIAN_POINT('Ctrl Pts',(-1.43925448419923E-16,-1.17524047358087,
-1.43749999999999));
#410387=CARTESIAN_POINT('Ctrl Pts',(0.678525403784459,-1.17524047358087,
-1.39583333333332));
#410388=CARTESIAN_POINT('Ctrl Pts',(1.01778810567669,-0.587620236790434,
-1.35416666666666));
#410389=CARTESIAN_POINT('Ctrl Pts',(1.35705080756892,2.29132664526027E-15,
-1.31249999999999));
#410390=CARTESIAN_POINT('Ctrl Pts',(1.01778810567669,0.587620236790438,
-1.27083333333332));
#410391=CARTESIAN_POINT('Ctrl Pts',(0.67852540378446,1.17524047358087,-1.22916666666666));
#410392=CARTESIAN_POINT('Ctrl Pts',(0.,1.17524047358087,-1.18749999999999));
#410393=CARTESIAN_POINT('Ctrl Pts',(-0.678525403784459,1.17524047358087,
-1.14583333333332));
#410394=CARTESIAN_POINT('Ctrl Pts',(-1.01778810567669,0.587620236790438,
-1.10416666666666));
#410395=CARTESIAN_POINT('Ctrl Pts',(-1.35705080756892,2.62370823081419E-15,
-1.06249999999999));
#410396=CARTESIAN_POINT('Ctrl Pts',(-1.01778810567669,-0.587620236790433,
-1.02083333333332));
#410397=CARTESIAN_POINT('Ctrl Pts',(-0.67852540378446,-1.17524047358087,
-0.979166666666658));
#410398=CARTESIAN_POINT('Ctrl Pts',(-1.43925448419923E-16,-1.17524047358087,
-0.937499999999991));
#410399=CARTESIAN_POINT('Ctrl Pts',(-1.43925448419923E-16,-1.17524047358087,
-1.49999999999999));
#410400=CARTESIAN_POINT('Ctrl Pts',(0.678525403784459,-1.17524047358087,
-1.45833333333332));
#410401=CARTESIAN_POINT('Ctrl Pts',(1.01778810567669,-0.587620236790434,
-1.41666666666666));
#410402=CARTESIAN_POINT('Ctrl Pts',(1.35705080756892,2.29132664526027E-15,
-1.37499999999999));
#410403=CARTESIAN_POINT('Ctrl Pts',(1.01778810567669,0.587620236790438,
-1.33333333333332));
#410404=CARTESIAN_POINT('Ctrl Pts',(0.67852540378446,1.17524047358087,-1.29166666666666));
#410405=CARTESIAN_POINT('Ctrl Pts',(0.,1.17524047358087,-1.24999999999999));
#410406=CARTESIAN_POINT('Ctrl Pts',(-0.678525403784459,1.17524047358087,
-1.20833333333332));
#410407=CARTESIAN_POINT('Ctrl Pts',(-1.01778810567669,0.587620236790438,
-1.16666666666666));
#410408=CARTESIAN_POINT('Ctrl Pts',(-1.35705080756892,2.62370823081419E-15,
-1.12499999999999));
#410409=CARTESIAN_POINT('Ctrl Pts',(-1.01778810567669,-0.587620236790433,
-1.08333333333332));
#410410=CARTESIAN_POINT('Ctrl Pts',(-0.67852540378446,-1.17524047358087,
-1.04166666666666));
#410411=CARTESIAN_POINT('Ctrl Pts',(-1.43925448419923E-16,-1.17524047358087,
-0.99999999999999));
#410412=CARTESIAN_POINT('Origin',(0.,-1.11022302462516E-14,-14.21875));
#410413=CARTESIAN_POINT('',(-8.32001735975286E-31,-1.17524047358087,-0.43749999999999));
#410414=CARTESIAN_POINT('',(-8.32001735975286E-31,-1.17524047358087,-0.49999999999999));
#410415=CARTESIAN_POINT('',(1.43925448419925E-16,-1.1752404735809,-14.21875));
#410416=CARTESIAN_POINT('Ctrl Pts',(-1.43925448419923E-16,-1.17524047358087,
-0.937499999999991));
#410417=CARTESIAN_POINT('Ctrl Pts',(0.678525403784459,-1.17524047358087,
-0.895833333333323));
#410418=CARTESIAN_POINT('Ctrl Pts',(1.01778810567669,-0.587620236790434,
-0.854166666666658));
#410419=CARTESIAN_POINT('Ctrl Pts',(1.35705080756892,2.29132664526027E-15,
-0.81249999999999));
#410420=CARTESIAN_POINT('Ctrl Pts',(1.01778810567669,0.587620236790438,
-0.770833333333323));
#410421=CARTESIAN_POINT('Ctrl Pts',(0.67852540378446,1.17524047358087,-0.729166666666658));
#410422=CARTESIAN_POINT('Ctrl Pts',(0.,1.17524047358087,-0.68749999999999));
#410423=CARTESIAN_POINT('Ctrl Pts',(-0.678525403784459,1.17524047358087,
-0.645833333333325));
#410424=CARTESIAN_POINT('Ctrl Pts',(-1.01778810567669,0.587620236790438,
-0.604166666666657));
#410425=CARTESIAN_POINT('Ctrl Pts',(-1.35705080756892,2.62370823081419E-15,
-0.56249999999999));
#410426=CARTESIAN_POINT('Ctrl Pts',(-1.01778810567669,-0.587620236790433,
-0.520833333333325));
#410427=CARTESIAN_POINT('Ctrl Pts',(-0.67852540378446,-1.17524047358087,
-0.479166666666657));
#410428=CARTESIAN_POINT('Ctrl Pts',(-1.43925448419923E-16,-1.17524047358087,
-0.43749999999999));
#410429=CARTESIAN_POINT('Ctrl Pts',(-1.43925448419923E-16,-1.17524047358087,
-0.99999999999999));
#410430=CARTESIAN_POINT('Ctrl Pts',(0.678525403784459,-1.17524047358087,
-0.958333333333323));
#410431=CARTESIAN_POINT('Ctrl Pts',(1.01778810567669,-0.587620236790434,
-0.916666666666658));
#410432=CARTESIAN_POINT('Ctrl Pts',(1.35705080756892,2.29132664526027E-15,
-0.87499999999999));
#410433=CARTESIAN_POINT('Ctrl Pts',(1.01778810567669,0.587620236790438,
-0.833333333333323));
#410434=CARTESIAN_POINT('Ctrl Pts',(0.67852540378446,1.17524047358087,-0.791666666666657));
#410435=CARTESIAN_POINT('Ctrl Pts',(0.,1.17524047358087,-0.74999999999999));
#410436=CARTESIAN_POINT('Ctrl Pts',(-0.678525403784459,1.17524047358087,
-0.708333333333325));
#410437=CARTESIAN_POINT('Ctrl Pts',(-1.01778810567669,0.587620236790438,
-0.666666666666658));
#410438=CARTESIAN_POINT('Ctrl Pts',(-1.35705080756892,2.62370823081419E-15,
-0.62499999999999));
#410439=CARTESIAN_POINT('Ctrl Pts',(-1.01778810567669,-0.587620236790433,
-0.583333333333325));
#410440=CARTESIAN_POINT('Ctrl Pts',(-0.67852540378446,-1.17524047358087,
-0.541666666666657));
#410441=CARTESIAN_POINT('Ctrl Pts',(-1.43925448419923E-16,-1.17524047358087,
-0.49999999999999));
#410442=CARTESIAN_POINT('Origin',(0.,-1.11022302462516E-14,-14.21875));
#410443=CARTESIAN_POINT('',(-8.32001735975286E-31,-1.17524047358087,0.0625000000000087));
#410444=CARTESIAN_POINT('',(-8.32001735975286E-31,-1.17524047358087,8.67361737988404E-15));
#410445=CARTESIAN_POINT('',(1.43925448419925E-16,-1.1752404735809,-14.21875));
#410446=CARTESIAN_POINT('Ctrl Pts',(-1.43925448419923E-16,-1.17524047358087,
-0.43749999999999));
#410447=CARTESIAN_POINT('Ctrl Pts',(0.678525403784459,-1.17524047358087,
-0.395833333333324));
#410448=CARTESIAN_POINT('Ctrl Pts',(1.01778810567669,-0.587620236790434,
-0.354166666666657));
#410449=CARTESIAN_POINT('Ctrl Pts',(1.35705080756892,2.29132664526027E-15,
-0.31249999999999));
#410450=CARTESIAN_POINT('Ctrl Pts',(1.01778810567669,0.587620236790438,
-0.270833333333324));
#410451=CARTESIAN_POINT('Ctrl Pts',(0.67852540378446,1.17524047358087,-0.229166666666657));
#410452=CARTESIAN_POINT('Ctrl Pts',(0.,1.17524047358087,-0.18749999999999));
#410453=CARTESIAN_POINT('Ctrl Pts',(-0.678525403784459,1.17524047358087,
-0.145833333333324));
#410454=CARTESIAN_POINT('Ctrl Pts',(-1.01778810567669,0.587620236790438,
-0.104166666666657));
#410455=CARTESIAN_POINT('Ctrl Pts',(-1.35705080756892,2.62370823081419E-15,
-0.0624999999999914));
#410456=CARTESIAN_POINT('Ctrl Pts',(-1.01778810567669,-0.587620236790433,
-0.0208333333333241));
#410457=CARTESIAN_POINT('Ctrl Pts',(-0.67852540378446,-1.17524047358087,
0.0208333333333432));
#410458=CARTESIAN_POINT('Ctrl Pts',(-1.43925448419923E-16,-1.17524047358087,
0.0625000000000087));
#410459=CARTESIAN_POINT('Ctrl Pts',(-1.43925448419923E-16,-1.17524047358087,
-0.49999999999999));
#410460=CARTESIAN_POINT('Ctrl Pts',(0.678525403784459,-1.17524047358087,
-0.458333333333324));
#410461=CARTESIAN_POINT('Ctrl Pts',(1.01778810567669,-0.587620236790434,
-0.416666666666657));
#410462=CARTESIAN_POINT('Ctrl Pts',(1.35705080756892,2.29132664526027E-15,
-0.37499999999999));
#410463=CARTESIAN_POINT('Ctrl Pts',(1.01778810567669,0.587620236790438,
-0.333333333333324));
#410464=CARTESIAN_POINT('Ctrl Pts',(0.67852540378446,1.17524047358087,-0.291666666666657));
#410465=CARTESIAN_POINT('Ctrl Pts',(0.,1.17524047358087,-0.24999999999999));
#410466=CARTESIAN_POINT('Ctrl Pts',(-0.678525403784459,1.17524047358087,
-0.208333333333324));
#410467=CARTESIAN_POINT('Ctrl Pts',(-1.01778810567669,0.587620236790438,
-0.166666666666657));
#410468=CARTESIAN_POINT('Ctrl Pts',(-1.35705080756892,2.62370823081419E-15,
-0.124999999999991));
#410469=CARTESIAN_POINT('Ctrl Pts',(-1.01778810567669,-0.587620236790433,
-0.0833333333333242));
#410470=CARTESIAN_POINT('Ctrl Pts',(-0.67852540378446,-1.17524047358087,
-0.0416666666666569));
#410471=CARTESIAN_POINT('Ctrl Pts',(-1.43925448419923E-16,-1.17524047358087,
8.67361737988404E-15));
#410472=CARTESIAN_POINT('Origin',(0.,-1.11022302462516E-14,-14.21875));
#410473=CARTESIAN_POINT('',(-8.32001735975286E-31,-1.17524047358087,0.562500000000009));
#410474=CARTESIAN_POINT('',(-8.32001735975286E-31,-1.17524047358087,0.500000000000009));
#410475=CARTESIAN_POINT('',(1.43925448419925E-16,-1.1752404735809,-14.21875));
#410476=CARTESIAN_POINT('Ctrl Pts',(-1.43925448419923E-16,-1.17524047358087,
0.0625000000000087));
#410477=CARTESIAN_POINT('Ctrl Pts',(0.678525403784459,-1.17524047358087,
0.104166666666676));
#410478=CARTESIAN_POINT('Ctrl Pts',(1.01778810567669,-0.587620236790434,
0.145833333333343));
#410479=CARTESIAN_POINT('Ctrl Pts',(1.35705080756892,2.29132664526027E-15,
0.187500000000009));
#410480=CARTESIAN_POINT('Ctrl Pts',(1.01778810567669,0.587620236790438,
0.229166666666676));
#410481=CARTESIAN_POINT('Ctrl Pts',(0.67852540378446,1.17524047358087,0.270833333333343));
#410482=CARTESIAN_POINT('Ctrl Pts',(0.,1.17524047358087,0.312500000000009));
#410483=CARTESIAN_POINT('Ctrl Pts',(-0.678525403784459,1.17524047358087,
0.354166666666676));
#410484=CARTESIAN_POINT('Ctrl Pts',(-1.01778810567669,0.587620236790438,
0.395833333333344));
#410485=CARTESIAN_POINT('Ctrl Pts',(-1.35705080756892,2.62370823081419E-15,
0.437500000000009));
#410486=CARTESIAN_POINT('Ctrl Pts',(-1.01778810567669,-0.587620236790433,
0.479166666666676));
#410487=CARTESIAN_POINT('Ctrl Pts',(-0.67852540378446,-1.17524047358087,
0.520833333333344));
#410488=CARTESIAN_POINT('Ctrl Pts',(-1.43925448419923E-16,-1.17524047358087,
0.562500000000009));
#410489=CARTESIAN_POINT('Ctrl Pts',(-1.43925448419923E-16,-1.17524047358087,
8.67361737988404E-15));
#410490=CARTESIAN_POINT('Ctrl Pts',(0.678525403784459,-1.17524047358087,
0.041666666666676));
#410491=CARTESIAN_POINT('Ctrl Pts',(1.01778810567669,-0.587620236790434,
0.0833333333333432));
#410492=CARTESIAN_POINT('Ctrl Pts',(1.35705080756892,2.29132664526027E-15,
0.125000000000009));
#410493=CARTESIAN_POINT('Ctrl Pts',(1.01778810567669,0.587620236790438,
0.166666666666676));
#410494=CARTESIAN_POINT('Ctrl Pts',(0.67852540378446,1.17524047358087,0.208333333333343));
#410495=CARTESIAN_POINT('Ctrl Pts',(0.,1.17524047358087,0.250000000000009));
#410496=CARTESIAN_POINT('Ctrl Pts',(-0.678525403784459,1.17524047358087,
0.291666666666676));
#410497=CARTESIAN_POINT('Ctrl Pts',(-1.01778810567669,0.587620236790438,
0.333333333333343));
#410498=CARTESIAN_POINT('Ctrl Pts',(-1.35705080756892,2.62370823081419E-15,
0.375000000000009));
#410499=CARTESIAN_POINT('Ctrl Pts',(-1.01778810567669,-0.587620236790433,
0.416666666666676));
#410500=CARTESIAN_POINT('Ctrl Pts',(-0.67852540378446,-1.17524047358087,
0.458333333333344));
#410501=CARTESIAN_POINT('Ctrl Pts',(-1.43925448419923E-16,-1.17524047358087,
0.500000000000009));
#410502=CARTESIAN_POINT('Origin',(0.,-1.11022302462516E-14,-14.21875));
#410503=CARTESIAN_POINT('',(-8.32001735975286E-31,-1.17524047358087,1.06250000000001));
#410504=CARTESIAN_POINT('',(-8.32001735975286E-31,-1.17524047358087,1.00000000000001));
#410505=CARTESIAN_POINT('',(1.43925448419925E-16,-1.1752404735809,-14.21875));
#410506=CARTESIAN_POINT('Ctrl Pts',(-1.43925448419923E-16,-1.17524047358087,
0.562500000000009));
#410507=CARTESIAN_POINT('Ctrl Pts',(0.678525403784459,-1.17524047358087,
0.604166666666677));
#410508=CARTESIAN_POINT('Ctrl Pts',(1.01778810567669,-0.587620236790434,
0.645833333333342));
#410509=CARTESIAN_POINT('Ctrl Pts',(1.35705080756892,2.29132664526027E-15,
0.687500000000009));
#410510=CARTESIAN_POINT('Ctrl Pts',(1.01778810567669,0.587620236790438,
0.729166666666677));
#410511=CARTESIAN_POINT('Ctrl Pts',(0.67852540378446,1.17524047358087,0.770833333333342));
#410512=CARTESIAN_POINT('Ctrl Pts',(0.,1.17524047358087,0.812500000000009));
#410513=CARTESIAN_POINT('Ctrl Pts',(-0.678525403784459,1.17524047358087,
0.854166666666677));
#410514=CARTESIAN_POINT('Ctrl Pts',(-1.01778810567669,0.587620236790438,
0.895833333333342));
#410515=CARTESIAN_POINT('Ctrl Pts',(-1.35705080756892,2.62370823081419E-15,
0.93750000000001));
#410516=CARTESIAN_POINT('Ctrl Pts',(-1.01778810567669,-0.587620236790433,
0.979166666666677));
#410517=CARTESIAN_POINT('Ctrl Pts',(-0.67852540378446,-1.17524047358087,
1.02083333333334));
#410518=CARTESIAN_POINT('Ctrl Pts',(-1.43925448419923E-16,-1.17524047358087,
1.06250000000001));
#410519=CARTESIAN_POINT('Ctrl Pts',(-1.43925448419923E-16,-1.17524047358087,
0.500000000000009));
#410520=CARTESIAN_POINT('Ctrl Pts',(0.678525403784459,-1.17524047358087,
0.541666666666676));
#410521=CARTESIAN_POINT('Ctrl Pts',(1.01778810567669,-0.587620236790434,
0.583333333333342));
#410522=CARTESIAN_POINT('Ctrl Pts',(1.35705080756892,2.29132664526027E-15,
0.625000000000009));
#410523=CARTESIAN_POINT('Ctrl Pts',(1.01778810567669,0.587620236790438,
0.666666666666677));
#410524=CARTESIAN_POINT('Ctrl Pts',(0.67852540378446,1.17524047358087,0.708333333333342));
#410525=CARTESIAN_POINT('Ctrl Pts',(0.,1.17524047358087,0.750000000000009));
#410526=CARTESIAN_POINT('Ctrl Pts',(-0.678525403784459,1.17524047358087,
0.791666666666677));
#410527=CARTESIAN_POINT('Ctrl Pts',(-1.01778810567669,0.587620236790438,
0.833333333333342));
#410528=CARTESIAN_POINT('Ctrl Pts',(-1.35705080756892,2.62370823081419E-15,
0.87500000000001));
#410529=CARTESIAN_POINT('Ctrl Pts',(-1.01778810567669,-0.587620236790433,
0.916666666666677));
#410530=CARTESIAN_POINT('Ctrl Pts',(-0.67852540378446,-1.17524047358087,
0.958333333333342));
#410531=CARTESIAN_POINT('Ctrl Pts',(-1.43925448419923E-16,-1.17524047358087,
1.00000000000001));
#410532=CARTESIAN_POINT('Origin',(0.,-1.11022302462516E-14,-14.21875));
#410533=CARTESIAN_POINT('',(-8.32001735975286E-31,-1.17524047358087,1.56250000000001));
#410534=CARTESIAN_POINT('',(-8.32001735975286E-31,-1.17524047358087,1.50000000000001));
#410535=CARTESIAN_POINT('',(1.43925448419925E-16,-1.1752404735809,-14.21875));
#410536=CARTESIAN_POINT('Ctrl Pts',(-1.43925448419923E-16,-1.17524047358087,
1.06250000000001));
#410537=CARTESIAN_POINT('Ctrl Pts',(0.678525403784459,-1.17524047358087,
1.10416666666668));
#410538=CARTESIAN_POINT('Ctrl Pts',(1.01778810567669,-0.587620236790434,
1.14583333333334));
#410539=CARTESIAN_POINT('Ctrl Pts',(1.35705080756892,2.29132664526027E-15,
1.18750000000001));
#410540=CARTESIAN_POINT('Ctrl Pts',(1.01778810567669,0.587620236790438,
1.22916666666668));
#410541=CARTESIAN_POINT('Ctrl Pts',(0.67852540378446,1.17524047358087,1.27083333333334));
#410542=CARTESIAN_POINT('Ctrl Pts',(0.,1.17524047358087,1.31250000000001));
#410543=CARTESIAN_POINT('Ctrl Pts',(-0.678525403784459,1.17524047358087,
1.35416666666668));
#410544=CARTESIAN_POINT('Ctrl Pts',(-1.01778810567669,0.587620236790438,
1.39583333333334));
#410545=CARTESIAN_POINT('Ctrl Pts',(-1.35705080756892,2.62370823081419E-15,
1.43750000000001));
#410546=CARTESIAN_POINT('Ctrl Pts',(-1.01778810567669,-0.587620236790433,
1.47916666666668));
#410547=CARTESIAN_POINT('Ctrl Pts',(-0.67852540378446,-1.17524047358087,
1.52083333333334));
#410548=CARTESIAN_POINT('Ctrl Pts',(-1.43925448419923E-16,-1.17524047358087,
1.56250000000001));
#410549=CARTESIAN_POINT('Ctrl Pts',(-1.43925448419923E-16,-1.17524047358087,
1.00000000000001));
#410550=CARTESIAN_POINT('Ctrl Pts',(0.678525403784459,-1.17524047358087,
1.04166666666668));
#410551=CARTESIAN_POINT('Ctrl Pts',(1.01778810567669,-0.587620236790434,
1.08333333333334));
#410552=CARTESIAN_POINT('Ctrl Pts',(1.35705080756892,2.29132664526027E-15,
1.12500000000001));
#410553=CARTESIAN_POINT('Ctrl Pts',(1.01778810567669,0.587620236790438,
1.16666666666668));
#410554=CARTESIAN_POINT('Ctrl Pts',(0.67852540378446,1.17524047358087,1.20833333333334));
#410555=CARTESIAN_POINT('Ctrl Pts',(0.,1.17524047358087,1.25000000000001));
#410556=CARTESIAN_POINT('Ctrl Pts',(-0.678525403784459,1.17524047358087,
1.29166666666668));
#410557=CARTESIAN_POINT('Ctrl Pts',(-1.01778810567669,0.587620236790438,
1.33333333333334));
#410558=CARTESIAN_POINT('Ctrl Pts',(-1.35705080756892,2.62370823081419E-15,
1.37500000000001));
#410559=CARTESIAN_POINT('Ctrl Pts',(-1.01778810567669,-0.587620236790433,
1.41666666666668));
#410560=CARTESIAN_POINT('Ctrl Pts',(-0.67852540378446,-1.17524047358087,
1.45833333333334));
#410561=CARTESIAN_POINT('Ctrl Pts',(-1.43925448419923E-16,-1.17524047358087,
1.50000000000001));
#410562=CARTESIAN_POINT('Origin',(0.,-1.11022302462516E-14,-14.21875));
#410563=CARTESIAN_POINT('',(-8.32001735975286E-31,-1.17524047358087,2.06250000000001));
#410564=CARTESIAN_POINT('',(-8.32001735975286E-31,-1.17524047358087,2.00000000000001));
#410565=CARTESIAN_POINT('',(1.43925448419925E-16,-1.1752404735809,-14.21875));
#410566=CARTESIAN_POINT('Ctrl Pts',(-1.43925448419923E-16,-1.17524047358087,
1.56250000000001));
#410567=CARTESIAN_POINT('Ctrl Pts',(0.678525403784459,-1.17524047358087,
1.60416666666668));
#410568=CARTESIAN_POINT('Ctrl Pts',(1.01778810567669,-0.587620236790434,
1.64583333333334));
#410569=CARTESIAN_POINT('Ctrl Pts',(1.35705080756892,2.29132664526027E-15,
1.68750000000001));
#410570=CARTESIAN_POINT('Ctrl Pts',(1.01778810567669,0.587620236790438,
1.72916666666668));
#410571=CARTESIAN_POINT('Ctrl Pts',(0.67852540378446,1.17524047358087,1.77083333333334));
#410572=CARTESIAN_POINT('Ctrl Pts',(0.,1.17524047358087,1.81250000000001));
#410573=CARTESIAN_POINT('Ctrl Pts',(-0.678525403784459,1.17524047358087,
1.85416666666668));
#410574=CARTESIAN_POINT('Ctrl Pts',(-1.01778810567669,0.587620236790438,
1.89583333333334));
#410575=CARTESIAN_POINT('Ctrl Pts',(-1.35705080756892,2.62370823081419E-15,
1.93750000000001));
#410576=CARTESIAN_POINT('Ctrl Pts',(-1.01778810567669,-0.587620236790433,
1.97916666666668));
#410577=CARTESIAN_POINT('Ctrl Pts',(-0.67852540378446,-1.17524047358087,
2.02083333333334));
#410578=CARTESIAN_POINT('Ctrl Pts',(-1.43925448419923E-16,-1.17524047358087,
2.06250000000001));
#410579=CARTESIAN_POINT('Ctrl Pts',(-1.43925448419923E-16,-1.17524047358087,
1.50000000000001));
#410580=CARTESIAN_POINT('Ctrl Pts',(0.678525403784459,-1.17524047358087,
1.54166666666668));
#410581=CARTESIAN_POINT('Ctrl Pts',(1.01778810567669,-0.587620236790434,
1.58333333333334));
#410582=CARTESIAN_POINT('Ctrl Pts',(1.35705080756892,2.29132664526027E-15,
1.62500000000001));
#410583=CARTESIAN_POINT('Ctrl Pts',(1.01778810567669,0.587620236790438,
1.66666666666668));
#410584=CARTESIAN_POINT('Ctrl Pts',(0.67852540378446,1.17524047358087,1.70833333333334));
#410585=CARTESIAN_POINT('Ctrl Pts',(0.,1.17524047358087,1.75000000000001));
#410586=CARTESIAN_POINT('Ctrl Pts',(-0.678525403784459,1.17524047358087,
1.79166666666668));
#410587=CARTESIAN_POINT('Ctrl Pts',(-1.01778810567669,0.587620236790438,
1.83333333333334));
#410588=CARTESIAN_POINT('Ctrl Pts',(-1.35705080756892,2.62370823081419E-15,
1.87500000000001));
#410589=CARTESIAN_POINT('Ctrl Pts',(-1.01778810567669,-0.587620236790433,
1.91666666666668));
#410590=CARTESIAN_POINT('Ctrl Pts',(-0.67852540378446,-1.17524047358087,
1.95833333333334));
#410591=CARTESIAN_POINT('Ctrl Pts',(-1.43925448419923E-16,-1.17524047358087,
2.00000000000001));
#410592=CARTESIAN_POINT('Origin',(0.,-1.11022302462516E-14,-14.21875));
#410593=CARTESIAN_POINT('',(-8.32001735975286E-31,-1.17524047358087,2.56250000000001));
#410594=CARTESIAN_POINT('',(-8.32001735975286E-31,-1.17524047358087,2.50000000000001));
#410595=CARTESIAN_POINT('',(1.43925448419925E-16,-1.1752404735809,-14.21875));
#410596=CARTESIAN_POINT('Ctrl Pts',(-1.43925448419923E-16,-1.17524047358087,
2.06250000000001));
#410597=CARTESIAN_POINT('Ctrl Pts',(0.678525403784459,-1.17524047358087,
2.10416666666668));
#410598=CARTESIAN_POINT('Ctrl Pts',(1.01778810567669,-0.587620236790434,
2.14583333333334));
#410599=CARTESIAN_POINT('Ctrl Pts',(1.35705080756892,2.29132664526027E-15,
2.18750000000001));
#410600=CARTESIAN_POINT('Ctrl Pts',(1.01778810567669,0.587620236790438,
2.22916666666668));
#410601=CARTESIAN_POINT('Ctrl Pts',(0.67852540378446,1.17524047358087,2.27083333333334));
#410602=CARTESIAN_POINT('Ctrl Pts',(0.,1.17524047358087,2.31250000000001));
#410603=CARTESIAN_POINT('Ctrl Pts',(-0.678525403784459,1.17524047358087,
2.35416666666668));
#410604=CARTESIAN_POINT('Ctrl Pts',(-1.01778810567669,0.587620236790438,
2.39583333333334));
#410605=CARTESIAN_POINT('Ctrl Pts',(-1.35705080756892,2.62370823081419E-15,
2.43750000000001));
#410606=CARTESIAN_POINT('Ctrl Pts',(-1.01778810567669,-0.587620236790433,
2.47916666666668));
#410607=CARTESIAN_POINT('Ctrl Pts',(-0.67852540378446,-1.17524047358087,
2.52083333333334));
#410608=CARTESIAN_POINT('Ctrl Pts',(-1.43925448419923E-16,-1.17524047358087,
2.56250000000001));
#410609=CARTESIAN_POINT('Ctrl Pts',(-1.43925448419923E-16,-1.17524047358087,
2.00000000000001));
#410610=CARTESIAN_POINT('Ctrl Pts',(0.678525403784459,-1.17524047358087,
2.04166666666668));
#410611=CARTESIAN_POINT('Ctrl Pts',(1.01778810567669,-0.587620236790434,
2.08333333333334));
#410612=CARTESIAN_POINT('Ctrl Pts',(1.35705080756892,2.29132664526027E-15,
2.12500000000001));
#410613=CARTESIAN_POINT('Ctrl Pts',(1.01778810567669,0.587620236790438,
2.16666666666668));
#410614=CARTESIAN_POINT('Ctrl Pts',(0.67852540378446,1.17524047358087,2.20833333333334));
#410615=CARTESIAN_POINT('Ctrl Pts',(0.,1.17524047358087,2.25000000000001));
#410616=CARTESIAN_POINT('Ctrl Pts',(-0.678525403784459,1.17524047358087,
2.29166666666668));
#410617=CARTESIAN_POINT('Ctrl Pts',(-1.01778810567669,0.587620236790438,
2.33333333333334));
#410618=CARTESIAN_POINT('Ctrl Pts',(-1.35705080756892,2.62370823081419E-15,
2.37500000000001));
#410619=CARTESIAN_POINT('Ctrl Pts',(-1.01778810567669,-0.587620236790433,
2.41666666666668));
#410620=CARTESIAN_POINT('Ctrl Pts',(-0.67852540378446,-1.17524047358087,
2.45833333333334));
#410621=CARTESIAN_POINT('Ctrl Pts',(-1.43925448419923E-16,-1.17524047358087,
2.50000000000001));
#410622=CARTESIAN_POINT('Origin',(0.,-1.11022302462516E-14,-14.21875));
#410623=CARTESIAN_POINT('',(-8.32001735975286E-31,-1.17524047358087,3.06250000000001));
#410624=CARTESIAN_POINT('',(-8.32001735975286E-31,-1.17524047358087,3.00000000000001));
#410625=CARTESIAN_POINT('',(1.43925448419925E-16,-1.1752404735809,-14.21875));
#410626=CARTESIAN_POINT('Ctrl Pts',(-1.43925448419923E-16,-1.17524047358087,
2.56250000000001));
#410627=CARTESIAN_POINT('Ctrl Pts',(0.678525403784459,-1.17524047358087,
2.60416666666668));
#410628=CARTESIAN_POINT('Ctrl Pts',(1.01778810567669,-0.587620236790434,
2.64583333333334));
#410629=CARTESIAN_POINT('Ctrl Pts',(1.35705080756892,2.29132664526027E-15,
2.68750000000001));
#410630=CARTESIAN_POINT('Ctrl Pts',(1.01778810567669,0.587620236790438,
2.72916666666668));
#410631=CARTESIAN_POINT('Ctrl Pts',(0.67852540378446,1.17524047358087,2.77083333333334));
#410632=CARTESIAN_POINT('Ctrl Pts',(0.,1.17524047358087,2.81250000000001));
#410633=CARTESIAN_POINT('Ctrl Pts',(-0.678525403784459,1.17524047358087,
2.85416666666668));
#410634=CARTESIAN_POINT('Ctrl Pts',(-1.01778810567669,0.587620236790438,
2.89583333333334));
#410635=CARTESIAN_POINT('Ctrl Pts',(-1.35705080756892,2.62370823081419E-15,
2.93750000000001));
#410636=CARTESIAN_POINT('Ctrl Pts',(-1.01778810567669,-0.587620236790433,
2.97916666666668));
#410637=CARTESIAN_POINT('Ctrl Pts',(-0.67852540378446,-1.17524047358087,
3.02083333333334));
#410638=CARTESIAN_POINT('Ctrl Pts',(-1.43925448419923E-16,-1.17524047358087,
3.06250000000001));
#410639=CARTESIAN_POINT('Ctrl Pts',(-1.43925448419923E-16,-1.17524047358087,
2.50000000000001));
#410640=CARTESIAN_POINT('Ctrl Pts',(0.678525403784459,-1.17524047358087,
2.54166666666668));
#410641=CARTESIAN_POINT('Ctrl Pts',(1.01778810567669,-0.587620236790434,
2.58333333333334));
#410642=CARTESIAN_POINT('Ctrl Pts',(1.35705080756892,2.29132664526027E-15,
2.62500000000001));
#410643=CARTESIAN_POINT('Ctrl Pts',(1.01778810567669,0.587620236790438,
2.66666666666668));
#410644=CARTESIAN_POINT('Ctrl Pts',(0.67852540378446,1.17524047358087,2.70833333333334));
#410645=CARTESIAN_POINT('Ctrl Pts',(0.,1.17524047358087,2.75000000000001));
#410646=CARTESIAN_POINT('Ctrl Pts',(-0.678525403784459,1.17524047358087,
2.79166666666668));
#410647=CARTESIAN_POINT('Ctrl Pts',(-1.01778810567669,0.587620236790438,
2.83333333333334));
#410648=CARTESIAN_POINT('Ctrl Pts',(-1.35705080756892,2.62370823081419E-15,
2.87500000000001));
#410649=CARTESIAN_POINT('Ctrl Pts',(-1.01778810567669,-0.587620236790433,
2.91666666666668));
#410650=CARTESIAN_POINT('Ctrl Pts',(-0.67852540378446,-1.17524047358087,
2.95833333333334));
#410651=CARTESIAN_POINT('Ctrl Pts',(-1.43925448419923E-16,-1.17524047358087,
3.00000000000001));
#410652=CARTESIAN_POINT('Origin',(0.,-1.11022302462516E-14,-14.21875));
#410653=CARTESIAN_POINT('',(-8.32001735975286E-31,-1.17524047358087,3.56250000000001));
#410654=CARTESIAN_POINT('',(-8.32001735975286E-31,-1.17524047358087,3.50000000000001));
#410655=CARTESIAN_POINT('',(1.43925448419925E-16,-1.1752404735809,-14.21875));
#410656=CARTESIAN_POINT('Ctrl Pts',(-1.43925448419923E-16,-1.17524047358087,
3.06250000000001));
#410657=CARTESIAN_POINT('Ctrl Pts',(0.678525403784459,-1.17524047358087,
3.10416666666668));
#410658=CARTESIAN_POINT('Ctrl Pts',(1.01778810567669,-0.587620236790434,
3.14583333333334));
#410659=CARTESIAN_POINT('Ctrl Pts',(1.35705080756892,2.29132664526027E-15,
3.18750000000001));
#410660=CARTESIAN_POINT('Ctrl Pts',(1.01778810567669,0.587620236790438,
3.22916666666668));
#410661=CARTESIAN_POINT('Ctrl Pts',(0.67852540378446,1.17524047358087,3.27083333333334));
#410662=CARTESIAN_POINT('Ctrl Pts',(0.,1.17524047358087,3.31250000000001));
#410663=CARTESIAN_POINT('Ctrl Pts',(-0.678525403784459,1.17524047358087,
3.35416666666668));
#410664=CARTESIAN_POINT('Ctrl Pts',(-1.01778810567669,0.587620236790438,
3.39583333333334));
#410665=CARTESIAN_POINT('Ctrl Pts',(-1.35705080756892,2.62370823081419E-15,
3.43750000000001));
#410666=CARTESIAN_POINT('Ctrl Pts',(-1.01778810567669,-0.587620236790433,
3.47916666666668));
#410667=CARTESIAN_POINT('Ctrl Pts',(-0.67852540378446,-1.17524047358087,
3.52083333333334));
#410668=CARTESIAN_POINT('Ctrl Pts',(-1.43925448419923E-16,-1.17524047358087,
3.56250000000001));
#410669=CARTESIAN_POINT('Ctrl Pts',(-1.43925448419923E-16,-1.17524047358087,
3.00000000000001));
#410670=CARTESIAN_POINT('Ctrl Pts',(0.678525403784459,-1.17524047358087,
3.04166666666668));
#410671=CARTESIAN_POINT('Ctrl Pts',(1.01778810567669,-0.587620236790434,
3.08333333333334));
#410672=CARTESIAN_POINT('Ctrl Pts',(1.35705080756892,2.29132664526027E-15,
3.12500000000001));
#410673=CARTESIAN_POINT('Ctrl Pts',(1.01778810567669,0.587620236790438,
3.16666666666668));
#410674=CARTESIAN_POINT('Ctrl Pts',(0.67852540378446,1.17524047358087,3.20833333333334));
#410675=CARTESIAN_POINT('Ctrl Pts',(0.,1.17524047358087,3.25000000000001));
#410676=CARTESIAN_POINT('Ctrl Pts',(-0.678525403784459,1.17524047358087,
3.29166666666668));
#410677=CARTESIAN_POINT('Ctrl Pts',(-1.01778810567669,0.587620236790438,
3.33333333333334));
#410678=CARTESIAN_POINT('Ctrl Pts',(-1.35705080756892,2.62370823081419E-15,
3.37500000000001));
#410679=CARTESIAN_POINT('Ctrl Pts',(-1.01778810567669,-0.587620236790433,
3.41666666666668));
#410680=CARTESIAN_POINT('Ctrl Pts',(-0.67852540378446,-1.17524047358087,
3.45833333333334));
#410681=CARTESIAN_POINT('Ctrl Pts',(-1.43925448419923E-16,-1.17524047358087,
3.50000000000001));
#410682=CARTESIAN_POINT('Origin',(0.,-1.19311743680736E-13,1002.5));
#410683=CARTESIAN_POINT('',(0.,1.50000000000006,4.00000000000002));
#410684=CARTESIAN_POINT('',(2.65829355574649E-12,1.22263611415551,3.72263611415551));
#410685=CARTESIAN_POINT('',(-1.22464679914734E-13,999.999999999989,1002.5));
#410686=CARTESIAN_POINT('',(1.16245326511943,-0.172894699617312,3.67524047358081));
#410687=CARTESIAN_POINT('Ctrl Pts',(5.09848710616739E-14,1.5000000000003,
4.00000000000016));
#410688=CARTESIAN_POINT('Ctrl Pts',(0.0614459419740359,1.49300527352564,
3.9930052735255));
#410689=CARTESIAN_POINT('Ctrl Pts',(0.176619180984774,1.47627277954793,
3.97963189845153));
#410690=CARTESIAN_POINT('Ctrl Pts',(0.407741104272866,1.39313746098645,
3.94828274522662));
#410691=CARTESIAN_POINT('Ctrl Pts',(0.496650592209766,1.35004412327267,
3.93518797642063));
#410692=CARTESIAN_POINT('Ctrl Pts',(0.73463717654934,1.20168003430334,3.89686512472376));
#410693=CARTESIAN_POINT('Ctrl Pts',(0.868548220680461,1.07608400562327,
3.87108844075398));
#410694=CARTESIAN_POINT('Ctrl Pts',(1.05190674105084,0.820029611618427,
3.82725385858292));
#410695=CARTESIAN_POINT('Ctrl Pts',(1.14450211555196,0.659211935335112,
3.80455972666058));
#410696=CARTESIAN_POINT('Ctrl Pts',(1.21470849431358,0.34856178753037,3.75902940895801));
#410697=CARTESIAN_POINT('Ctrl Pts',(1.22403973629944,0.238553492192828,
3.74234909593137));
#410698=CARTESIAN_POINT('Ctrl Pts',(1.21272207332383,0.0262843883317015,
3.70875263493674));
#410699=CARTESIAN_POINT('Ctrl Pts',(1.19398876028483,-0.0751524073185166,
3.69205355609417));
#410700=CARTESIAN_POINT('Ctrl Pts',(1.16245326511929,-0.172894699617247,
3.67524047358073));
#410701=CARTESIAN_POINT('',(0.943477955796025,0.700742119234707,3.67524047358081));
#410702=CARTESIAN_POINT('Origin',(-5.55111512312578E-16,5.58580959264532E-15,
3.67524047358089));
#410703=CARTESIAN_POINT('Ctrl Pts',(0.943477955795997,0.700742119234686,
3.67524047358083));
#410704=CARTESIAN_POINT('Ctrl Pts',(0.894463001055356,0.772758356925599,
3.67883146777442));
#410705=CARTESIAN_POINT('Ctrl Pts',(0.837726504812894,0.839196987658124,
3.68256694202216));
#410706=CARTESIAN_POINT('Ctrl Pts',(0.712851122357575,0.956652840655983,
3.69006027251154));
#410707=CARTESIAN_POINT('Ctrl Pts',(0.645482378604126,1.00776531764839,
3.69379267345778));
#410708=CARTESIAN_POINT('Ctrl Pts',(0.447490290696521,1.12733650300416,
3.70398399106719));
#410709=CARTESIAN_POINT('Ctrl Pts',(0.308736215403076,1.17946143006525,
3.71032040612255));
#410710=CARTESIAN_POINT('Ctrl Pts',(0.108169821062047,1.21501394733954,
3.71850309831));
#410711=CARTESIAN_POINT('Ctrl Pts',(0.0533501263262607,1.22063965939443,
3.72063965939443));
#410712=CARTESIAN_POINT('Ctrl Pts',(5.31673684123335E-12,1.22263611415551,
3.72263611415551));
#410713=CARTESIAN_POINT('Origin',(0.,2.54061283442571E-15,-14.));
#410714=CARTESIAN_POINT('',(1.4102143475861E-12,1.33373412263468,-13.8415063509462));
#410715=CARTESIAN_POINT('',(-1.43925448419923E-16,1.17524047358087,-14.));
#410716=CARTESIAN_POINT('',(-1.43925448419923E-16,1.17524047358087,-14.));
#410717=CARTESIAN_POINT('Ctrl Pts',(2.82059203049461E-12,1.33373412263468,
-13.8415063509462));
#410718=CARTESIAN_POINT('Ctrl Pts',(0.0503707035999144,1.33200617731085,
-13.84323429627));
#410719=CARTESIAN_POINT('Ctrl Pts',(0.101566648626412,1.32733503529964,
-13.8450537305792));
#410720=CARTESIAN_POINT('Ctrl Pts',(0.311597220248351,1.29512418775187,
-13.8528065966954));
#410721=CARTESIAN_POINT('Ctrl Pts',(0.464060849169011,1.2419652779919,-13.8590957478521));
#410722=CARTESIAN_POINT('Ctrl Pts',(0.752305458718201,1.07737853149812,
-13.8724606339434));
#410723=CARTESIAN_POINT('Ctrl Pts',(0.883244570548725,0.963577263216904,
-13.8794314317899));
#410724=CARTESIAN_POINT('Ctrl Pts',(1.05897345549616,0.736523802329364,
-13.8904755074827));
#410725=CARTESIAN_POINT('Ctrl Pts',(1.15669334597624,0.586782768129815,
-13.8964531882757));
#410726=CARTESIAN_POINT('Ctrl Pts',(1.25343072844487,0.22591559097259,-13.9112797109474));
#410727=CARTESIAN_POINT('Ctrl Pts',(1.26526290710797,0.0682549586007996,
-13.9178507152948));
#410728=CARTESIAN_POINT('Ctrl Pts',(1.22916289389683,-0.252389992813634,
-13.9314343166522));
#410729=CARTESIAN_POINT('Ctrl Pts',(1.1780317000175,-0.411978763297157,
-13.9383169357496));
#410730=CARTESIAN_POINT('Ctrl Pts',(0.998487821188208,-0.73449306440248,
-13.9524375659778));
#410731=CARTESIAN_POINT('Ctrl Pts',(0.881213268978223,-0.845390401721151,
-13.9587809847204));
#410732=CARTESIAN_POINT('Ctrl Pts',(0.688202236191876,-1.00009299759695,
-13.9693507574149));
#410733=CARTESIAN_POINT('Ctrl Pts',(0.564231790739783,-1.06795850550759,
-13.9755497402544));
#410734=CARTESIAN_POINT('Ctrl Pts',(0.292597606675929,-1.15980721556296,
-13.9880801320964));
#410735=CARTESIAN_POINT('Ctrl Pts',(0.146401631267334,-1.18094002160998,
-13.9943004519709));
#410736=CARTESIAN_POINT('Ctrl Pts',(-2.42861286636753E-16,-1.17524047358088,
-14.));
#410737=CARTESIAN_POINT('Origin',(0.,2.54061283442571E-15,-14.));
#410738=CARTESIAN_POINT('Origin',(0.,2.5406128344257E-15,14.));
#410739=CARTESIAN_POINT('',(-1.2271251213284E-13,1.50000000000006,-13.4375));
#410740=CARTESIAN_POINT('',(-1.76090861703506E-14,1.50000000000006,-13.5));
#410741=CARTESIAN_POINT('',(-1.8369701987211E-16,1.50000000000006,14.));
#410742=CARTESIAN_POINT('',(0.2433378840056,-1.48013062741362,-13.6752404735808));
#410743=CARTESIAN_POINT('Ctrl Pts',(-2.45289899503121E-13,1.50000000000006,
-13.4375));
#410744=CARTESIAN_POINT('Ctrl Pts',(0.154099018422491,1.50000000000008,
-13.4449140924807));
#410745=CARTESIAN_POINT('Ctrl Pts',(0.3075139555236,1.47625956742878,-13.4529547285437));
#410746=CARTESIAN_POINT('Ctrl Pts',(0.642809422800748,1.36956233159267,
-13.4720504513412));
#410747=CARTESIAN_POINT('Ctrl Pts',(0.817133592085943,1.27326193964589,
-13.4831126377338));
#410748=CARTESIAN_POINT('Ctrl Pts',(1.11308167833158,1.02332674485026,-13.5042940909721));
#410749=CARTESIAN_POINT('Ctrl Pts',(1.23365593605882,0.874188091054278,
-13.5139339949414));
#410750=CARTESIAN_POINT('Ctrl Pts',(1.41682962140902,0.531160231905482,
-13.5329910982275));
#410751=CARTESIAN_POINT('Ctrl Pts',(1.47467131896198,0.338905698544985,
-13.5436719056364));
#410752=CARTESIAN_POINT('Ctrl Pts',(1.51168174079155,-0.053055686762387,
-13.5654475381535));
#410753=CARTESIAN_POINT('Ctrl Pts',(1.49200417916322,-0.248854522257683,
-13.5763252512365));
#410754=CARTESIAN_POINT('Ctrl Pts',(1.38003397123258,-0.617986951620019,
-13.5968326084233));
#410755=CARTESIAN_POINT('Ctrl Pts',(1.29034581469085,-0.788293050011382,
-13.6056485705454));
#410756=CARTESIAN_POINT('Ctrl Pts',(1.05637903511238,-1.08064599775905,
-13.6250262176915));
#410757=CARTESIAN_POINT('Ctrl Pts',(0.916265143532659,-1.20173932499309,
-13.6351311539775));
#410758=CARTESIAN_POINT('Ctrl Pts',(0.599147008227846,-1.38737752273559,
-13.6555451239801));
#410759=CARTESIAN_POINT('Ctrl Pts',(0.424766445511276,-1.45030323148159,
-13.6656829490696));
#410760=CARTESIAN_POINT('Ctrl Pts',(0.243337884005714,-1.4801306274136,
-13.6752404735808));
#410761=CARTESIAN_POINT('',(1.20419349529495,-0.894381364905089,-13.6752404735808));
#410762=CARTESIAN_POINT('Origin',(0.,2.54061283442571E-15,-13.6752404735808));
#410763=CARTESIAN_POINT('Ctrl Pts',(1.20419349529495,-0.894381364905085,
-13.6752404735808));
#410764=CARTESIAN_POINT('Ctrl Pts',(1.26487937350023,-0.812674005317148,
-13.6700510740269));
#410765=CARTESIAN_POINT('Ctrl Pts',(1.3170709609443,-0.725038800233257,
-13.6652799333463));
#410766=CARTESIAN_POINT('Ctrl Pts',(1.40415555674086,-0.537868414461984,
-13.6548815785812));
#410767=CARTESIAN_POINT('Ctrl Pts',(1.43825077374835,-0.438617967969369,
-13.6493676648871));
#410768=CARTESIAN_POINT('Ctrl Pts',(1.50578641792733,-0.145369370312591,
-13.6330760761284));
#410769=CARTESIAN_POINT('Ctrl Pts',(1.51186815437617,0.052697405544391,
-13.6220723663586));
#410770=CARTESIAN_POINT('Ctrl Pts',(1.44677677093112,0.443724946936882,
-13.600348614059));
#410771=CARTESIAN_POINT('Ctrl Pts',(1.37474540067206,0.632529457136806,
-13.5902388728971));
#410772=CARTESIAN_POINT('Ctrl Pts',(1.16558432059299,0.963340423632484,
-13.570986412226));
#410773=CARTESIAN_POINT('Ctrl Pts',(1.03334003549703,1.10399171713937,-13.5607168257176));
#410774=CARTESIAN_POINT('Ctrl Pts',(0.717145150131488,1.33236982232222,
-13.5391600559473));
#410775=CARTESIAN_POINT('Ctrl Pts',(0.534471089831185,1.41557611950021,
-13.5280598600906));
#410776=CARTESIAN_POINT('Ctrl Pts',(0.228875537835284,1.48689143938017,
-13.5113759061321));
#410777=CARTESIAN_POINT('Ctrl Pts',(0.114507097818563,1.50000000000006,
-13.5055092253125));
#410778=CARTESIAN_POINT('Ctrl Pts',(-3.33413852082742E-14,1.50000000000006,
-13.5));
#410779=CARTESIAN_POINT('Origin',(0.,2.5406128344257E-15,14.));
#410780=CARTESIAN_POINT('',(-1.4424133868457E-14,1.50000000000006,-12.9375));
#410781=CARTESIAN_POINT('',(-1.17935083679999E-13,1.50000000000006,-13.));
#410782=CARTESIAN_POINT('',(-1.8369701987211E-16,1.50000000000006,14.));
#410783=CARTESIAN_POINT('Ctrl Pts',(-2.86576318231369E-14,1.50000000000006,
-12.9375));
#410784=CARTESIAN_POINT('Ctrl Pts',(0.184852825957988,1.50000000000006,
-12.9463937357356));
#410785=CARTESIAN_POINT('Ctrl Pts',(0.368282906907539,1.4658328779758,-12.956168106343));
#410786=CARTESIAN_POINT('Ctrl Pts',(0.72389141137937,1.32831699878958,-12.9770972140245));
#410787=CARTESIAN_POINT('Ctrl Pts',(0.891143524743268,1.22242037256957,
-12.9880857080312));
#410788=CARTESIAN_POINT('Ctrl Pts',(1.17101075554248,0.956468513672169,
-13.0089383780871));
#410789=CARTESIAN_POINT('Ctrl Pts',(1.28259586684403,0.800644978114965,
-13.0180197234381));
#410790=CARTESIAN_POINT('Ctrl Pts',(1.44543345949742,0.447528023135354,
-13.037637332048));
#410791=CARTESIAN_POINT('Ctrl Pts',(1.49196279374196,0.252162578720567,
-13.0484909678489));
#410792=CARTESIAN_POINT('Ctrl Pts',(1.50595370549604,-0.140261693065969,
-13.0702923162814));
#410793=CARTESIAN_POINT('Ctrl Pts',(1.47524935824808,-0.333499915715787,
-13.0810277730953));
#410794=CARTESIAN_POINT('Ctrl Pts',(1.34246640649021,-0.69629608957844,
-13.1011831160877));
#410795=CARTESIAN_POINT('Ctrl Pts',(1.24216320762647,-0.862598601288366,
-13.1100308003996));
#410796=CARTESIAN_POINT('Ctrl Pts',(0.979665680373286,-1.15321907962225,
-13.1307330096329));
#410797=CARTESIAN_POINT('Ctrl Pts',(0.818085798325511,-1.2729432454608,
-13.1418326966058));
#410798=CARTESIAN_POINT('Ctrl Pts',(0.4644476501586,-1.43909739126499,-13.1634625128815));
#410799=CARTESIAN_POINT('Ctrl Pts',(0.276987275447283,-1.48661095844317,
-13.1738015256755));
#410800=CARTESIAN_POINT('Ctrl Pts',(-0.112827305776877,-1.50890274072842,
-13.1931757046337));
#410801=CARTESIAN_POINT('Ctrl Pts',(-0.311602660346058,-1.48069201022844,
-13.2030283230351));
#410802=CARTESIAN_POINT('Ctrl Pts',(-0.684567164515238,-1.34908723753913,
-13.2246282742387));
#410803=CARTESIAN_POINT('Ctrl Pts',(-0.855341639053257,-1.24782221144681,
-13.2356575823673));
#410804=CARTESIAN_POINT('Ctrl Pts',(-1.14309366854786,-0.989654320961702,
-13.2566733886326));
#410805=CARTESIAN_POINT('Ctrl Pts',(-1.25906862022969,-0.837139245306665,
-13.2659922641496));
#410806=CARTESIAN_POINT('Ctrl Pts',(-1.43195153850576,-0.488941921447512,
-13.2853365599196));
#410807=CARTESIAN_POINT('Ctrl Pts',(-1.48407800628601,-0.29502430488665,
-13.2961097608396));
#410808=CARTESIAN_POINT('Ctrl Pts',(-1.50940514181516,0.0973417379654638,
-13.3179078743314));
#410809=CARTESIAN_POINT('Ctrl Pts',(-1.48410708479636,0.291918192051283,
-13.3287176773362));
#410810=CARTESIAN_POINT('Ctrl Pts',(-1.36157410946492,0.657874819395,-13.3490486010775));
#410811=CARTESIAN_POINT('Ctrl Pts',(-1.26655798730886,0.826143729909582,
-13.3578444706988));
#410812=CARTESIAN_POINT('Ctrl Pts',(-1.01301440814474,1.12414268541646,
-13.3783208406031));
#410813=CARTESIAN_POINT('Ctrl Pts',(-0.854503038877091,1.24888216839119,
-13.3894122080509));
#410814=CARTESIAN_POINT('Ctrl Pts',(-0.504746456989134,1.42553331513728,
-13.4111468557414));
#410815=CARTESIAN_POINT('Ctrl Pts',(-0.318170363476253,1.4784117155096,
-13.4215923466807));
#410816=CARTESIAN_POINT('Ctrl Pts',(-0.0844779885570294,1.49821791269636,
-13.4333860484554));
#410817=CARTESIAN_POINT('Ctrl Pts',(-0.0422157010777418,1.50000000000005,
-13.4354688961349));
#410818=CARTESIAN_POINT('Ctrl Pts',(-2.45241327245807E-13,1.50000000000006,
-13.4375));
#410819=CARTESIAN_POINT('Ctrl Pts',(-3.5034475320829E-14,1.50000000000006,
-13.5));
#410820=CARTESIAN_POINT('Ctrl Pts',(-0.0777857544300243,1.50000000000006,
-13.496257531145));
#410821=CARTESIAN_POINT('Ctrl Pts',(-0.155619149278412,1.4939502636561,
-13.4923447219576));
#410822=CARTESIAN_POINT('Ctrl Pts',(-0.423998845455286,1.45178591133617,
-13.4782610657959));
#410823=CARTESIAN_POINT('Ctrl Pts',(-0.60756485963818,1.38502997963198,
-13.4675749103845));
#410824=CARTESIAN_POINT('Ctrl Pts',(-0.94375800148565,1.18273677189161,
-13.4457805545352));
#410825=CARTESIAN_POINT('Ctrl Pts',(-1.09209305825346,1.04732852804349,
-13.434882440682));
#410826=CARTESIAN_POINT('Ctrl Pts',(-1.3221095209703,0.733599132438725,
-13.4151010630262));
#410827=CARTESIAN_POINT('Ctrl Pts',(-1.40434608742343,0.560323983928858,
-13.4061291102182));
#410828=CARTESIAN_POINT('Ctrl Pts',(-1.50114237669675,0.186782615875113,
-13.385376811993));
#410829=CARTESIAN_POINT('Ctrl Pts',(-1.51268012037893,-0.0104892337438368,
-13.3744172647919));
#410830=CARTESIAN_POINT('Ctrl Pts',(-1.45891178653008,-0.401398254268275,
-13.352700096985));
#410831=CARTESIAN_POINT('Ctrl Pts',(-1.39291869469351,-0.590987184595628,
-13.3422671879284));
#410832=CARTESIAN_POINT('Ctrl Pts',(-1.19502793232843,-0.926443398889491,
-13.3234279360101));
#410833=CARTESIAN_POINT('Ctrl Pts',(-1.06766380281429,-1.07072827672343,
-13.3132922131986));
#410834=CARTESIAN_POINT('Ctrl Pts',(-0.759913809545176,-1.30835035009972,
-13.2918849715945));
#410835=CARTESIAN_POINT('Ctrl Pts',(-0.580652095742315,-1.3971751572685,
-13.2807928826132));
#410836=CARTESIAN_POINT('Ctrl Pts',(-0.201378097004742,-1.49910542573291,
-13.2597136574947));
#410837=CARTESIAN_POINT('Ctrl Pts',(-0.00544640710581742,-1.51255858965364,
-13.2506108900966));
#410838=CARTESIAN_POINT('Ctrl Pts',(0.379052846273133,-1.46408732054578,
-13.2307652370012));
#410839=CARTESIAN_POINT('Ctrl Pts',(0.564029572780868,-1.4032415620624,
-13.2201753801398));
#410840=CARTESIAN_POINT('Ctrl Pts',(0.907438980410449,-1.21111096966877,
-13.1983161264118));
#410841=CARTESIAN_POINT('Ctrl Pts',(1.06109936088841,-1.07903671034705,
-13.1872544084835));
#410842=CARTESIAN_POINT('Ctrl Pts',(1.30116498830284,-0.770235999508398,
-13.167126448076));
#410843=CARTESIAN_POINT('Ctrl Pts',(1.38836336564338,-0.598954100754246,
-13.1582752278196));
#410844=CARTESIAN_POINT('Ctrl Pts',(1.4953150158834,-0.228343295009018,
-13.1376857386115));
#410845=CARTESIAN_POINT('Ctrl Pts',(1.51230785211533,-0.0320201587424078,
-13.1267788977078));
#410846=CARTESIAN_POINT('Ctrl Pts',(1.46975295761758,0.359626694949958,
-13.1050207391693));
#410847=CARTESIAN_POINT('Ctrl Pts',(1.40921800047594,0.551031376972371,
-13.0943871457237));
#410848=CARTESIAN_POINT('Ctrl Pts',(1.2211769228825,0.891569478800854,-13.0754683622887));
#410849=CARTESIAN_POINT('Ctrl Pts',(1.09838808096619,1.03911396724531,-13.0656486109837));
#410850=CARTESIAN_POINT('Ctrl Pts',(0.798522165802527,1.28505980419314,
-13.0443894766095));
#410851=CARTESIAN_POINT('Ctrl Pts',(0.622543558908819,1.37893394517422,
-13.0333150869105));
#410852=CARTESIAN_POINT('Ctrl Pts',(0.292600113075803,1.47852197007691,
-13.0146743414463));
#410853=CARTESIAN_POINT('Ctrl Pts',(0.146573787712378,1.50000000000008,
-13.0070520346493));
#410854=CARTESIAN_POINT('Ctrl Pts',(-2.35471364629092E-13,1.50000000000006,
-13.));
#410855=CARTESIAN_POINT('Origin',(0.,2.5406128344257E-15,14.));
#410856=CARTESIAN_POINT('',(9.46300839574452E-15,1.50000000000006,-12.4375));
#410857=CARTESIAN_POINT('',(-3.99037522836055E-14,1.50000000000006,-12.5));
#410858=CARTESIAN_POINT('',(-1.8369701987211E-16,1.50000000000006,14.));
#410859=CARTESIAN_POINT('Ctrl Pts',(1.91097138113612E-14,1.50000000000006,
-12.4375));
#410860=CARTESIAN_POINT('Ctrl Pts',(0.0144712148980006,1.50000000000006,
-12.4381962466514));
#410861=CARTESIAN_POINT('Ctrl Pts',(0.0289506003252937,1.49979058477179,
-12.4388987034969));
#410862=CARTESIAN_POINT('Ctrl Pts',(0.242185688672286,1.49361360589839,
-12.4493295642149));
#410863=CARTESIAN_POINT('Ctrl Pts',(0.437789212302859,1.44839601290101,
-12.4599965873837));
#410864=CARTESIAN_POINT('Ctrl Pts',(0.796491878951723,1.28593468629028,
-12.4817674921075));
#410865=CARTESIAN_POINT('Ctrl Pts',(0.95675559810253,1.17160325035686,-12.4926540571106));
#410866=CARTESIAN_POINT('Ctrl Pts',(1.2215744375202,0.891136897701778,-12.5131858914808));
#410867=CARTESIAN_POINT('Ctrl Pts',(1.32484055345982,0.728809131594151,
-12.5220106038003));
#410868=CARTESIAN_POINT('Ctrl Pts',(1.46863560718626,0.36507643645482,-12.5422179757525));
#410869=CARTESIAN_POINT('Ctrl Pts',(1.50421453234514,0.165813395109599,
-12.5532881447161));
#410870=CARTESIAN_POINT('Ctrl Pts',(1.49516690833387,-0.227209539152673,
-12.5751227521751));
#410871=CARTESIAN_POINT('Ctrl Pts',(1.45363347765981,-0.417271052511157,
-12.5856817251395));
#410872=CARTESIAN_POINT('Ctrl Pts',(1.29997176929002,-0.773385643877929,
-12.6054658691043));
#410873=CARTESIAN_POINT('Ctrl Pts',(1.18850487773847,-0.93569056662924,
-12.6146427703706));
#410874=CARTESIAN_POINT('Ctrl Pts',(0.907589738804474,-1.21056091538983,
-12.6357935937598));
#410875=CARTESIAN_POINT('Ctrl Pts',(0.740111695936488,-1.31962373145034,
-12.6468809075226));
#410876=CARTESIAN_POINT('Ctrl Pts',(0.379276311980173,-1.46372383810901,
-12.6682443887681));
#410877=CARTESIAN_POINT('Ctrl Pts',(0.190452331770557,-1.50000248438981,
-12.6783367889045));
#410878=CARTESIAN_POINT('Ctrl Pts',(-0.198819746662407,-1.49999740672085,
-12.6970657915568));
#410879=CARTESIAN_POINT('Ctrl Pts',(-0.39561299924559,-1.46047412053578,
-12.707631880397));
#410880=CARTESIAN_POINT('Ctrl Pts',(-0.759347989869126,-1.30829369300126,
-12.729359322391));
#410881=CARTESIAN_POINT('Ctrl Pts',(-0.923268236624447,-1.19825844329666,
-12.7403024736542));
#410882=CARTESIAN_POINT('Ctrl Pts',(-1.1958717752218,-0.925246685340456,
-12.7610017774634));
#410883=CARTESIAN_POINT('Ctrl Pts',(-1.30343461885677,-0.76631653272979,
-12.7699268592928));
#410884=CARTESIAN_POINT('Ctrl Pts',(-1.45688562510155,-0.408718687921794,
-12.7897934062266));
#410885=CARTESIAN_POINT('Ctrl Pts',(-1.4981782275804,-0.212156984428337,
-12.8007135008651));
#410886=CARTESIAN_POINT('Ctrl Pts',(-1.50165481736864,0.18002650253877,
-12.8225014723633));
#410887=CARTESIAN_POINT('Ctrl Pts',(-1.46597742543479,0.371889550365959,
-12.8331605305759));
#410888=CARTESIAN_POINT('Ctrl Pts',(-1.32367068114965,0.731678966310704,
-12.8531488314617));
#410889=CARTESIAN_POINT('Ctrl Pts',(-1.21834364925858,0.896159005203687,
-12.862109052878));
#410890=CARTESIAN_POINT('Ctrl Pts',(-0.947471792132494,1.17971885604868,
-12.8830180437038));
#410891=CARTESIAN_POINT('Ctrl Pts',(-0.783139322974793,1.29465224984847,
-12.8941170875847));
#410892=CARTESIAN_POINT('Ctrl Pts',(-0.426123079502387,1.45084226121507,
-12.9156326510344));
#410893=CARTESIAN_POINT('Ctrl Pts',(-0.237968535444941,1.49329096691863,
-12.9258643714701));
#410894=CARTESIAN_POINT('Ctrl Pts',(-0.0312538598267095,1.49975594898516,
-12.9359895187731));
#410895=CARTESIAN_POINT('Ctrl Pts',(-0.0156221697085717,1.50000000000006,
-12.9367483780095));
#410896=CARTESIAN_POINT('Ctrl Pts',(-2.86645707170419E-14,1.50000000000006,
-12.9375));
#410897=CARTESIAN_POINT('Ctrl Pts',(-2.35686470340126E-13,1.50000000000006,
-13.));
#410898=CARTESIAN_POINT('Ctrl Pts',(-0.0488561908367927,1.50000000000005,
-12.9976494054224));
#410899=CARTESIAN_POINT('Ctrl Pts',(-0.0977668133780745,1.49761321556351,
-12.9952298924304));
#410900=CARTESIAN_POINT('Ctrl Pts',(-0.338072805258772,1.47402088263108,
-12.9830128224239));
#410901=CARTESIAN_POINT('Ctrl Pts',(-0.52416483036909,1.41854276041394,
-12.9725184067408));
#410902=CARTESIAN_POINT('Ctrl Pts',(-0.871927326752233,1.2368262397146,
-12.9507389947019));
#410903=CARTESIAN_POINT('Ctrl Pts',(-1.0288946842114,1.10967845678737,-12.9396550163359));
#410904=CARTESIAN_POINT('Ctrl Pts',(-1.27806597055699,0.808135776262727,
-12.9192905716619));
#410905=CARTESIAN_POINT('Ctrl Pts',(-1.37052783126929,0.638898595859914,
-12.9104943664366));
#410906=CARTESIAN_POINT('Ctrl Pts',(-1.48802713407293,0.271417741405987,
-12.8900787634113));
#410907=CARTESIAN_POINT('Ctrl Pts',(-1.51065228263555,0.0762387495105381,
-12.8792354860838));
#410908=CARTESIAN_POINT('Ctrl Pts',(-1.47975611674998,-0.315978046570199,
-12.8574456640793));
#410909=CARTESIAN_POINT('Ctrl Pts',(-1.4248986350945,-0.50912454103883,
-12.8467153032755));
#410910=CARTESIAN_POINT('Ctrl Pts',(-1.24710381956909,-0.854870564928091,
-12.8275071908372));
#410911=CARTESIAN_POINT('Ctrl Pts',(-1.12894714535878,-1.0057727497918,
-12.8180450295841));
#410912=CARTESIAN_POINT('Ctrl Pts',(-0.837297925413553,-1.26004460532475,
-12.7969499428489));
#410913=CARTESIAN_POINT('Ctrl Pts',(-0.664820905826346,-1.35896785705792,
-12.7859037702712));
#410914=CARTESIAN_POINT('Ctrl Pts',(-0.290553549488137,-1.48484308526585,
-12.7644002895768));
#410915=CARTESIAN_POINT('Ctrl Pts',(-0.0923424899387176,-1.51017590176458,
-12.7547254940565));
#410916=CARTESIAN_POINT('Ctrl Pts',(0.296492136046974,-1.48287582776257,
-12.7352593440023));
#410917=CARTESIAN_POINT('Ctrl Pts',(0.483553291929648,-1.43282385304763,
-12.7248690273126));
#410918=CARTESIAN_POINT('Ctrl Pts',(0.835393916110487,-1.26169561153856,
-12.7031875251249));
#410919=CARTESIAN_POINT('Ctrl Pts',(0.995541605556879,-1.13959079644599,
-12.6920906154047));
#410920=CARTESIAN_POINT('Ctrl Pts',(1.25381344303546,-0.8454676424949,-12.6714944182206));
#410921=CARTESIAN_POINT('Ctrl Pts',(1.35161198790032,-0.678239112822272,
-12.6626799507123));
#410922=CARTESIAN_POINT('Ctrl Pts',(1.47956707389454,-0.313945143036675,
-12.6424413968353));
#410923=CARTESIAN_POINT('Ctrl Pts',(1.50773153685902,-0.120058126980392,
-12.6316698959433));
#410924=CARTESIAN_POINT('Ctrl Pts',(1.48840274776665,0.272379766589699,
-12.6098677907449));
#410925=CARTESIAN_POINT('Ctrl Pts',(1.43923156534188,0.467083856763257,
-12.5990508968464));
#410926=CARTESIAN_POINT('Ctrl Pts',(1.2716553361612,0.817895896734298,-12.5795613390702));
#410927=CARTESIAN_POINT('Ctrl Pts',(1.15801103262477,0.972156887553523,
-12.5703771404632));
#410928=CARTESIAN_POINT('Ctrl Pts',(0.874438668330924,1.23446705149296,
-12.5494473652821));
#410929=CARTESIAN_POINT('Ctrl Pts',(0.705518706497666,1.33820509943847,
-12.5384385873862));
#410930=CARTESIAN_POINT('Ctrl Pts',(0.354347959586764,1.46839643927147,
-12.5179264508413));
#410931=CARTESIAN_POINT('Ctrl Pts',(0.177787084102027,1.50000000000007,
-12.508553785072));
#410932=CARTESIAN_POINT('Ctrl Pts',(-7.95891130778159E-14,1.50000000000006,
-12.5));
#410933=CARTESIAN_POINT('Origin',(0.,2.5406128344257E-15,14.));
#410934=CARTESIAN_POINT('',(1.24121291263909E-13,1.50000000000006,-11.9375));
#410935=CARTESIAN_POINT('',(7.83583777527795E-15,1.50000000000006,-12.));
#410936=CARTESIAN_POINT('',(-1.8369701987211E-16,1.50000000000006,14.));
#410937=CARTESIAN_POINT('Ctrl Pts',(2.4842627954769E-13,1.50000000000006,
-11.9375));
#410938=CARTESIAN_POINT('Ctrl Pts',(0.0429770385529035,1.50000000000006,
-11.9395677337315));
#410939=CARTESIAN_POINT('Ctrl Pts',(0.0860016566600157,1.49815305830009,
-11.9416890605714));
#410940=CARTESIAN_POINT('Ctrl Pts',(0.320455096552336,1.47792193396156,
-11.9535311826337));
#410941=CARTESIAN_POINT('Ctrl Pts',(0.506977512895046,1.42474532959968,
-11.963982374473));
#410942=CARTESIAN_POINT('Ctrl Pts',(0.856509125031369,1.24751244453871,
-11.9857223576989));
#410943=CARTESIAN_POINT('Ctrl Pts',(1.01484528553922,1.12249598149265,-11.9968129893023));
#410944=CARTESIAN_POINT('Ctrl Pts',(1.26788852442334,0.824089509044983,
-12.0172766064886));
#410945=CARTESIAN_POINT('Ctrl Pts',(1.3626114035016,0.65571019094691,-12.0260716560585));
#410946=CARTESIAN_POINT('Ctrl Pts',(1.48456931942257,0.289578440662951,
-12.0464123088521));
#410947=CARTESIAN_POINT('Ctrl Pts',(1.50956256359297,0.0949313160154064,
-12.0572260379991));
#410948=CARTESIAN_POINT('Ctrl Pts',(1.48359916209213,-0.29742169655306,
-12.0790234275863));
#410949=CARTESIAN_POINT('Ctrl Pts',(1.4311600520702,-0.491253205265574,
-12.089791844737));
#410950=CARTESIAN_POINT('Ctrl Pts',(1.25771526043269,-0.839171630783029,
-12.1091206461546));
#410951=CARTESIAN_POINT('Ctrl Pts',(1.1414919566941,-0.991502066499563,
-12.1184550000298));
#410952=CARTESIAN_POINT('Ctrl Pts',(0.853295509986717,-1.24922733560828,
-12.13947989329));
#410953=CARTESIAN_POINT('Ctrl Pts',(0.682325569135146,-1.35022705898739,
-12.1505112362762));
#410954=CARTESIAN_POINT('Ctrl Pts',(0.309210501082249,-1.48117904653476,
-12.1721002985674));
#410955=CARTESIAN_POINT('Ctrl Pts',(0.110499711440047,-1.50906111074809,
-12.1819318826338));
#410956=CARTESIAN_POINT('Ctrl Pts',(-0.279204309035193,-1.48619976188739,
-12.2013165635293));
#410957=CARTESIAN_POINT('Ctrl Pts',(-0.466621070585969,-1.43839788599238,
-12.2116614865596));
#410958=CARTESIAN_POINT('Ctrl Pts',(-0.820058580331773,-1.27167812486944,
-12.2332973611513));
#410959=CARTESIAN_POINT('Ctrl Pts',(-0.98147757103943,-1.15168288128523,
-12.2443968371735));
#410960=CARTESIAN_POINT('Ctrl Pts',(-1.24349615035991,-0.860663422680281,
-12.2650870857989));
#410961=CARTESIAN_POINT('Ctrl Pts',(-1.34351447886236,-0.694256212190225,
-12.2739302104339));
#410962=CARTESIAN_POINT('Ctrl Pts',(-1.47575101472088,-0.331289623800945,
-12.2940950208999));
#410963=CARTESIAN_POINT('Ctrl Pts',(-1.50616850407291,-0.137976327667566,
-12.3048346484629));
#410964=CARTESIAN_POINT('Ctrl Pts',(-1.49157364495768,0.254453151885936,
-12.3266362862159));
#410965=CARTESIAN_POINT('Ctrl Pts',(-1.44474483714684,0.449745590823751,
-12.3374858661569));
#410966=CARTESIAN_POINT('Ctrl Pts',(-1.28137026340723,0.802602783636924,
-12.3570890435354));
#410967=CARTESIAN_POINT('Ctrl Pts',(-1.16955280914026,0.958249070463121,
-12.3661812273027));
#410968=CARTESIAN_POINT('Ctrl Pts',(-0.8892670011538,1.22379091712043,-12.3870426469341));
#410969=CARTESIAN_POINT('Ctrl Pts',(-0.721825367529755,1.32944528069627,
-12.3980335297206));
#410970=CARTESIAN_POINT('Ctrl Pts',(-0.366722866655218,1.46612261404421,
-12.4189149993528));
#410971=CARTESIAN_POINT('Ctrl Pts',(-0.184066879677061,1.50000000000006,
-12.4286440781225));
#410972=CARTESIAN_POINT('Ctrl Pts',(1.85962356624714E-14,1.50000000000006,
-12.4375));
#410973=CARTESIAN_POINT('Ctrl Pts',(-7.96238075473389E-14,1.50000000000006,
-12.5));
#410974=CARTESIAN_POINT('Ctrl Pts',(-0.021657246306187,1.50000000000006,
-12.4989580152512));
#410975=CARTESIAN_POINT('Ctrl Pts',(-0.0433314544011003,1.49953096835747,
-12.4979021857713));
#410976=CARTESIAN_POINT('Ctrl Pts',(-0.256228705129635,1.49029566327074,
-12.4874026257674));
#410977=CARTESIAN_POINT('Ctrl Pts',(-0.444075622041309,1.44547885186977,
-12.4771199253358));
#410978=CARTESIAN_POINT('Ctrl Pts',(-0.799546902645559,1.28462353593294,
-12.4555491021532));
#410979=CARTESIAN_POINT('Ctrl Pts',(-0.962609755641049,1.16744345672824,
-12.4444487347804));
#410980=CARTESIAN_POINT('Ctrl Pts',(-1.22957527214838,0.880569908863771,
-12.4236356407158));
#410981=CARTESIAN_POINT('Ctrl Pts',(-1.33254855999195,0.715241436593647,
-12.4147356353662));
#410982=CARTESIAN_POINT('Ctrl Pts',(-1.47041968409356,0.354043071868654,
-12.3946690595482));
#410983=CARTESIAN_POINT('Ctrl Pts',(-1.50378740274652,0.161523925225723,
-12.3839735514014));
#410984=CARTESIAN_POINT('Ctrl Pts',(-1.4954171406393,-0.230806974685007,
-12.3621773902952));
#410985=CARTESIAN_POINT('Ctrl Pts',(-1.45168177601164,-0.42682950454516,
-12.3512872497474));
#410986=CARTESIAN_POINT('Ctrl Pts',(-1.293852642627,-0.782351512525683,
-12.3315360270818));
#410987=CARTESIAN_POINT('Ctrl Pts',(-1.18442272180316,-0.93983065716822,
-12.3225458242953));
#410988=CARTESIAN_POINT('Ctrl Pts',(-0.908443732773366,-1.20957450506437,
-12.301774894331));
#410989=CARTESIAN_POINT('Ctrl Pts',(-0.742965177194812,-1.31770197949868,
-12.2908097626571));
#410990=CARTESIAN_POINT('Ctrl Pts',(-0.376990871830196,-1.46540920331455,
-12.2690988372412));
#410991=CARTESIAN_POINT('Ctrl Pts',(-0.179674896831448,-1.50240134587015,
-12.2587113165562));
#410992=CARTESIAN_POINT('Ctrl Pts',(0.209843827240239,-1.49745737468072,
-12.2398332556734));
#410993=CARTESIAN_POINT('Ctrl Pts',(0.398413433063471,-1.45864864120757,
-12.2296826759089));
#410994=CARTESIAN_POINT('Ctrl Pts',(0.757686743020997,-1.3096518332869,
-12.2082583305042));
#410995=CARTESIAN_POINT('Ctrl Pts',(0.923911465244628,-1.19819476089986,
-12.1971648100389));
#410996=CARTESIAN_POINT('Ctrl Pts',(1.20075829432931,-0.919774214948045,
-12.17611110671));
#410997=CARTESIAN_POINT('Ctrl Pts',(1.30972221446346,-0.756588576841831,
-12.1670326987134));
#410998=CARTESIAN_POINT('Ctrl Pts',(1.45879219593834,-0.398976183610319,
-12.1471653435339));
#410999=CARTESIAN_POINT('Ctrl Pts',(1.49796783200108,-0.208165256817152,
-12.1365647364898));
#411000=CARTESIAN_POINT('Ctrl Pts',(1.50195600485459,0.185450445196111,
-12.1146971974891));
#411001=CARTESIAN_POINT('Ctrl Pts',(1.46370705882602,0.38450287225785,-12.103638729319));
#411002=CARTESIAN_POINT('Ctrl Pts',(1.31503358379335,0.746295760438966,
-12.08353912442));
#411003=CARTESIAN_POINT('Ctrl Pts',(1.20977572079829,0.907038528106464,
-12.0746765135022));
#411004=CARTESIAN_POINT('Ctrl Pts',(0.941346093386267,1.18406121176143,
-12.0540666124858));
#411005=CARTESIAN_POINT('Ctrl Pts',(0.779375800537106,1.29641804195596,
-12.0431527900767));
#411006=CARTESIAN_POINT('Ctrl Pts',(0.418306890734359,1.45413978895109,
-12.0213996944154));
#411007=CARTESIAN_POINT('Ctrl Pts',(0.222131420495649,1.49672539385334,
-12.0107782642334));
#411008=CARTESIAN_POINT('Ctrl Pts',(0.0155552563317659,1.49993952719833,
-12.0007500824192));
#411009=CARTESIAN_POINT('Ctrl Pts',(0.00777642948193762,1.50000000000006,
-12.0003741436379));
#411010=CARTESIAN_POINT('Ctrl Pts',(1.91097138113612E-14,1.50000000000006,
-12.));
#411011=CARTESIAN_POINT('Origin',(0.,2.5406128344257E-15,14.));
#411012=CARTESIAN_POINT('',(0.,1.50000000000006,-11.4375));
#411013=CARTESIAN_POINT('',(9.54567205468683E-14,1.50000000000006,-11.5));
#411014=CARTESIAN_POINT('',(-1.8369701987211E-16,1.50000000000006,14.));
#411015=CARTESIAN_POINT('Ctrl Pts',(-9.19750386962903E-13,1.50000000000006,
-11.4375));
#411016=CARTESIAN_POINT('Ctrl Pts',(0.130329120553406,1.50000000000014,
-11.4437704627362));
#411017=CARTESIAN_POINT('Ctrl Pts',(0.26015361750193,1.48301567758715,-11.4504884334916));
#411018=CARTESIAN_POINT('Ctrl Pts',(0.516680461991447,1.41466440933564,
-11.464729233392));
#411019=CARTESIAN_POINT('Ctrl Pts',(0.641864718321054,1.36243900991012,
-11.4722028692724));
#411020=CARTESIAN_POINT('Ctrl Pts',(0.929939979719385,1.19363353633602,
-11.4907519376813));
#411021=CARTESIAN_POINT('Ctrl Pts',(1.07984591957781,1.0599528663692,-11.501677642519));
#411022=CARTESIAN_POINT('Ctrl Pts',(1.31358155055579,0.748798092663026,
-11.5215664414662));
#411023=CARTESIAN_POINT('Ctrl Pts',(1.39786282863566,0.576352382580591,
-11.53048042319));
#411024=CARTESIAN_POINT('Ctrl Pts',(1.49886862959217,0.204015777895458,
-11.5511657901169));
#411025=CARTESIAN_POINT('Ctrl Pts',(1.51267080067798,0.00711890021125362,
-11.5621045055438));
#411026=CARTESIAN_POINT('Ctrl Pts',(1.46355675398347,-0.384053847316768,
-11.5838363248509));
#411027=CARTESIAN_POINT('Ctrl Pts',(1.39985149987318,-0.574402771986881,
-11.5944112651104));
#411028=CARTESIAN_POINT('Ctrl Pts',(1.20606174238502,-0.911964039249115,
-11.6131646688472));
#411029=CARTESIAN_POINT('Ctrl Pts',(1.08062285433907,-1.05762666739877,
-11.6232203605518));
#411030=CARTESIAN_POINT('Ctrl Pts',(0.77609634100543,-1.29877885517542,
-11.6445705711385));
#411031=CARTESIAN_POINT('Ctrl Pts',(0.598186717455987,-1.3897227112928,
-11.6556564701179));
#411032=CARTESIAN_POINT('Ctrl Pts',(0.219887652524674,-1.49658312679679,
-11.6768257372407));
#411033=CARTESIAN_POINT('Ctrl Pts',(0.0234993071507874,-1.51246494816405,
-11.6860231404975));
#411034=CARTESIAN_POINT('Ctrl Pts',(-0.361925055423086,-1.46838628355445,
-11.7057912861381));
#411035=CARTESIAN_POINT('Ctrl Pts',(-0.547387505842392,-1.4097863714055,
-11.7163421277817));
#411036=CARTESIAN_POINT('Ctrl Pts',(-0.892657118595693,-1.22200577535338,
-11.7381700474387));
#411037=CARTESIAN_POINT('Ctrl Pts',(-1.04772076955362,-1.09198521825952,
-11.7492422329653));
#411038=CARTESIAN_POINT('Ctrl Pts',(-1.29160959565064,-0.786212353699829,
-11.7694700302642));
#411039=CARTESIAN_POINT('Ctrl Pts',(-1.38100924390979,-0.6157939870204,
-11.7782892229433));
#411040=CARTESIAN_POINT('Ctrl Pts',(-1.49240059316123,-0.24649002818514,
-11.7988061095453));
#411041=CARTESIAN_POINT('Ctrl Pts',(-1.5117689175907,-0.0506288538669847,
-11.8096872858963));
#411042=CARTESIAN_POINT('Ctrl Pts',(-1.47411867367302,0.341300262638134,
-11.8314611257021));
#411043=CARTESIAN_POINT('Ctrl Pts',(-1.41596555384023,0.533458715529244,
-11.8421365953072));
#411044=CARTESIAN_POINT('Ctrl Pts',(-1.23222972897185,0.876200481622434,
-11.8611778045346));
#411045=CARTESIAN_POINT('Ctrl Pts',(-1.11140103543713,1.02515495807662,
-11.8708375526976));
#411046=CARTESIAN_POINT('Ctrl Pts',(-0.815001814868391,1.27463261018898,
-11.8920280016271));
#411047=CARTESIAN_POINT('Ctrl Pts',(-0.640485714472906,1.37065535694332,
-11.9030917099432));
#411048=CARTESIAN_POINT('Ctrl Pts',(-0.305798716040215,1.47652567288713,
-11.9221351877727));
#411049=CARTESIAN_POINT('Ctrl Pts',(-0.153233117418503,1.50000000000006,
-11.9301275682008));
#411050=CARTESIAN_POINT('Ctrl Pts',(2.49522624784504E-13,1.50000000000006,
-11.9375));
#411051=CARTESIAN_POINT('Ctrl Pts',(1.96370697480575E-14,1.50000000000006,
-12.));
#411052=CARTESIAN_POINT('Ctrl Pts',(-0.182328550940932,1.50000000000006,
-11.9912277135028));
#411053=CARTESIAN_POINT('Ctrl Pts',(-0.363251579039296,1.46675784955459,
-11.9815996571869));
#411054=CARTESIAN_POINT('Ctrl Pts',(-0.718522420562673,1.33145425339341,
-11.9607482476278));
#411055=CARTESIAN_POINT('Ctrl Pts',(-0.887482234234511,1.22532586195463,
-11.949671153929));
#411056=CARTESIAN_POINT('Ctrl Pts',(-1.17333378627438,0.954820941023825,
-11.9284040891377));
#411057=CARTESIAN_POINT('Ctrl Pts',(-1.28786816289331,0.793586004890666,
-11.9190881113828));
#411058=CARTESIAN_POINT('Ctrl Pts',(-1.44708864380716,0.439306103519968,
-11.89940589464));
#411059=CARTESIAN_POINT('Ctrl Pts',(-1.49145651876931,0.250189188814036,
-11.8888993993785));
#411060=CARTESIAN_POINT('Ctrl Pts',(-1.50660286706077,-0.142032459715299,
-11.8671093077936));
#411061=CARTESIAN_POINT('Ctrl Pts',(-1.47425057730889,-0.341504197234316,
-11.8560275445981));
#411062=CARTESIAN_POINT('Ctrl Pts',(-1.3363660810813,-0.707550522178523,
-11.8356916376567));
#411063=CARTESIAN_POINT('Ctrl Pts',(-1.23549743422695,-0.871808664519378,
-11.8268926573384));
#411064=CARTESIAN_POINT('Ctrl Pts',(-0.975027265118679,-1.15639102726546,
-11.8064557148523));
#411065=CARTESIAN_POINT('Ctrl Pts',(-0.816841961747075,-1.27305859663344,
-11.7956042550796));
#411066=CARTESIAN_POINT('Ctrl Pts',(-0.461060686783883,-1.44115980884466,
-11.7738172423899));
#411067=CARTESIAN_POINT('Ctrl Pts',(-0.266191369136677,-1.48952496009485,
-11.7630981115496));
#411068=CARTESIAN_POINT('Ctrl Pts',(0.122211266267834,-1.50703124582293,
-11.7439247953262));
#411069=CARTESIAN_POINT('Ctrl Pts',(0.311899438227977,-1.4794688418196,
-11.7344234213321));
#411070=CARTESIAN_POINT('Ctrl Pts',(0.677562252474723,-1.35267066814931,
-11.7133082894881));
#411071=CARTESIAN_POINT('Ctrl Pts',(0.849164217990212,-1.25208995182803,
-11.7022581772861));
#411072=CARTESIAN_POINT('Ctrl Pts',(1.14420642225097,-0.989889976456594,
-11.6807796199659));
#411073=CARTESIAN_POINT('Ctrl Pts',(1.26454579811548,-0.830658622661461,
-11.671147701259));
#411074=CARTESIAN_POINT('Ctrl Pts',(1.43408482697798,-0.479847056524478,
-11.6516581698069));
#411075=CARTESIAN_POINT('Ctrl Pts',(1.48365214893905,-0.292589613456167,
-11.6412549785253));
#411076=CARTESIAN_POINT('Ctrl Pts',(1.51003368203839,0.0979048979622877,
-11.6195608390021));
#411077=CARTESIAN_POINT('Ctrl Pts',(1.48364921311269,0.297630447443781,
-11.608464975142));
#411078=CARTESIAN_POINT('Ctrl Pts',(1.35675031906872,0.667868610533521,
-11.5878961883037));
#411079=CARTESIAN_POINT('Ctrl Pts',(1.26029844307481,0.835743730818598,
-11.5790877001469));
#411080=CARTESIAN_POINT('Ctrl Pts',(1.00783525764039,1.12781802743597,-11.5588278845682));
#411081=CARTESIAN_POINT('Ctrl Pts',(0.853538474200204,1.24866561166777,
-11.5480473997739));
#411082=CARTESIAN_POINT('Ctrl Pts',(0.503332749649789,1.42695064705156,
-11.5262457569015));
#411083=CARTESIAN_POINT('Ctrl Pts',(0.309941789457643,1.48104345618317,
-11.5154386519596));
#411084=CARTESIAN_POINT('Ctrl Pts',(0.074421646781362,1.49861678005269,
-11.5036190359265));
#411085=CARTESIAN_POINT('Ctrl Pts',(0.0371922855396213,1.50000000000006,
-11.5017894146723));
#411086=CARTESIAN_POINT('Ctrl Pts',(1.91097138113609E-13,1.50000000000006,
-11.5));
#411087=CARTESIAN_POINT('Origin',(0.,2.5406128344257E-15,14.));
#411088=CARTESIAN_POINT('',(-1.27489940585681E-13,1.50000000000006,-10.9375));
#411089=CARTESIAN_POINT('',(5.40523406222535E-14,1.50000000000006,-11.));
#411090=CARTESIAN_POINT('',(-1.8369701987211E-16,1.50000000000006,14.));
#411091=CARTESIAN_POINT('Ctrl Pts',(-2.56114573993216E-13,1.50000000000006,
-10.9375));
#411092=CARTESIAN_POINT('Ctrl Pts',(0.15246223475462,1.50000000000008,-10.9448353426897));
#411093=CARTESIAN_POINT('Ctrl Pts',(0.304271509779819,1.47676131292171,
-10.9527847889253));
#411094=CARTESIAN_POINT('Ctrl Pts',(0.638415184845918,1.37162524087191,
-10.9717817304334));
#411095=CARTESIAN_POINT('Ctrl Pts',(0.813101815135945,1.27585000938268,
-10.9828467679488));
#411096=CARTESIAN_POINT('Ctrl Pts',(1.1099025941224,1.02678001623993,-11.0040452130064));
#411097=CARTESIAN_POINT('Ctrl Pts',(1.23095788496071,0.877989340494405,
-11.013722814417));
#411098=CARTESIAN_POINT('Ctrl Pts',(1.41519370737247,0.535502360679354,
-11.0327498688511));
#411099=CARTESIAN_POINT('Ctrl Pts',(1.47362374455104,0.343429821589083,
-11.0434205654673));
#411100=CARTESIAN_POINT('Ctrl Pts',(1.51184320099172,-0.0484697043042123,
-11.0651927613502));
#411101=CARTESIAN_POINT('Ctrl Pts',(1.49275011288303,-0.244385935541777,
-11.076076996419));
#411102=CARTESIAN_POINT('Ctrl Pts',(1.38187379427068,-0.613842289581186,
-11.0966023494212));
#411103=CARTESIAN_POINT('Ctrl Pts',(1.29273054755267,-0.784360605764299,
-11.1054246004696));
#411104=CARTESIAN_POINT('Ctrl Pts',(1.04928595722263,-1.09048672473935,
-11.1256408370878));
#411105=CARTESIAN_POINT('Ctrl Pts',(0.894384273913469,-1.22074701582039,
-11.1367118892198));
#411106=CARTESIAN_POINT('Ctrl Pts',(0.549328415459523,-1.40903475174676,
-11.1585436118369));
#411107=CARTESIAN_POINT('Ctrl Pts',(0.363921115990155,-1.46789621378336,
-11.1690990653039));
#411108=CARTESIAN_POINT('Ctrl Pts',(-0.0213961478304139,-1.51248668470138,
-11.1888762749953));
#411109=CARTESIAN_POINT('Ctrl Pts',(-0.217730804231609,-1.49688877070679,
-11.1980620012388));
#411110=CARTESIAN_POINT('Ctrl Pts',(-0.596145126370211,-1.39060384306678,
-11.2192208279025));
#411111=CARTESIAN_POINT('Ctrl Pts',(-0.774213802494401,-1.29990630406645,
-11.2303075371604));
#411112=CARTESIAN_POINT('Ctrl Pts',(-1.07912867173849,-1.05915598008962,
-11.2516652696463));
#411113=CARTESIAN_POINT('Ctrl Pts',(-1.20478920020793,-0.913649509470577,
-11.2617416939183));
#411114=CARTESIAN_POINT('Ctrl Pts',(-1.39905600226516,-0.576337019190607,
-11.2804812767116));
#411115=CARTESIAN_POINT('Ctrl Pts',(-1.46302376087178,-0.386078227174812,
-11.2910512096014));
#411116=CARTESIAN_POINT('Ctrl Pts',(-1.51268251626141,0.00505016793965425,
-11.3127805648855));
#411117=CARTESIAN_POINT('Ctrl Pts',(-1.49914603176655,0.201992420713084,
-11.3237218011507));
#411118=CARTESIAN_POINT('Ctrl Pts',(-1.39863454333612,0.574471234174373,
-11.3444150685652));
#411119=CARTESIAN_POINT('Ctrl Pts',(-1.31459423506811,0.747014100127693,
-11.3533352803792));
#411120=CARTESIAN_POINT('Ctrl Pts',(-1.08129627686726,1.05847310449937,
-11.3732114726369));
#411121=CARTESIAN_POINT('Ctrl Pts',(-0.931574318326271,1.19235826159576,
-11.3841340058674));
#411122=CARTESIAN_POINT('Ctrl Pts',(-0.643429812963329,1.36173533849175,
-11.4027022836482));
#411123=CARTESIAN_POINT('Ctrl Pts',(-0.517971561185671,1.41422566649052,
-11.4101964612678));
#411124=CARTESIAN_POINT('Ctrl Pts',(-0.260825662036353,1.48292743037495,
-11.4244767814392));
#411125=CARTESIAN_POINT('Ctrl Pts',(-0.130667240233891,1.50000000000014,
-11.4312132694731));
#411126=CARTESIAN_POINT('Ctrl Pts',(9.27764809421916E-13,1.50000000000006,
-11.4375));
#411127=CARTESIAN_POINT('Ctrl Pts',(1.91097138113609E-13,1.50000000000006,
-11.5));
#411128=CARTESIAN_POINT('Ctrl Pts',(-0.152179298203859,1.50000000000006,
-11.4926782701014));
#411129=CARTESIAN_POINT('Ctrl Pts',(-0.303676254544889,1.47684734021558,
-11.4847462399525));
#411130=CARTESIAN_POINT('Ctrl Pts',(-0.636699084008757,1.37229479658189,
-11.4658194342763));
#411131=CARTESIAN_POINT('Ctrl Pts',(-0.810725317540163,1.27722399917584,
-11.4548057377282));
#411132=CARTESIAN_POINT('Ctrl Pts',(-1.11472321897743,1.023353851667,-11.4331276833339));
#411133=CARTESIAN_POINT('Ctrl Pts',(-1.24084474511904,0.866101820708982,
-11.4231167678172));
#411134=CARTESIAN_POINT('Ctrl Pts',(-1.42041058582733,0.518739623571149,
-11.4038188679762));
#411135=CARTESIAN_POINT('Ctrl Pts',(-1.47494686773213,0.333417035429076,
-11.3935231686349));
#411136=CARTESIAN_POINT('Ctrl Pts',(-1.51212516926065,-0.0551064641573005,
-11.371938529769));
#411137=CARTESIAN_POINT('Ctrl Pts',(-1.49150504579564,-0.254913980230995,
-11.3608381122094));
#411138=CARTESIAN_POINT('Ctrl Pts',(-1.37529802672603,-0.629097571714455,
-11.3400501349048));
#411139=CARTESIAN_POINT('Ctrl Pts',(-1.28310967384223,-0.800522046839755,
-11.3311635861094));
#411140=CARTESIAN_POINT('Ctrl Pts',(-1.03834424508844,-1.09970222827409,
-11.3110767433324));
#411141=CARTESIAN_POINT('Ctrl Pts',(-0.887855420222202,-1.22441934816545,
-11.3003719819287));
#411142=CARTESIAN_POINT('Ctrl Pts',(-0.543238920911026,-1.41224451967927,
-11.2785742469997));
#411143=CARTESIAN_POINT('Ctrl Pts',(-0.351419082558947,-1.47175647476156,
-11.2676922008605));
#411144=CARTESIAN_POINT('Ctrl Pts',(0.0354848897897921,-1.51157456061957,
-11.2479712168712));
#411145=CARTESIAN_POINT('Ctrl Pts',(0.226498491371865,-1.49493353218255,
-11.2389618510358));
#411146=CARTESIAN_POINT('Ctrl Pts',(0.597791346128348,-1.38960800183643,
-11.218172306056));
#411147=CARTESIAN_POINT('Ctrl Pts',(0.773938384141673,-1.29976144194085,
-11.2072016899633));
#411148=CARTESIAN_POINT('Ctrl Pts',(1.08409107868713,-1.0556017091574,-11.18549724669));
#411149=CARTESIAN_POINT('Ctrl Pts',(1.2142845463122,-0.902779300458576,
-11.175154405581));
#411150=CARTESIAN_POINT('Ctrl Pts',(1.40366694131897,-0.562277595161398,
-11.1562376441756));
#411151=CARTESIAN_POINT('Ctrl Pts',(1.46374313140388,-0.379301091450682,
-11.1460722828584));
#411152=CARTESIAN_POINT('Ctrl Pts',(1.51303027236692,0.00664128631009762,
-11.1246310396494));
#411153=CARTESIAN_POINT('Ctrl Pts',(1.49891009334133,0.206348046807697,
-11.1135362196218));
#411154=CARTESIAN_POINT('Ctrl Pts',(1.39487942862602,0.584852432951371,
-11.0925081981694));
#411155=CARTESIAN_POINT('Ctrl Pts',(1.30751165546829,0.760360591944268,
-11.0834532229671));
#411156=CARTESIAN_POINT('Ctrl Pts',(1.07140318405049,1.06741553266847,-11.0635641449305));
#411157=CARTESIAN_POINT('Ctrl Pts',(0.925266340380091,1.19630551001658,
-11.0529528556127));
#411158=CARTESIAN_POINT('Ctrl Pts',(0.585586951813232,1.39548565578919,
-11.0310772415834));
#411159=CARTESIAN_POINT('Ctrl Pts',(0.393779769791798,1.46124850900595,
-11.020022168313));
#411160=CARTESIAN_POINT('Ctrl Pts',(0.130016188590412,1.49577813346715,
-11.0063726808605));
#411161=CARTESIAN_POINT('Ctrl Pts',(0.0649794055432486,1.50000000000006,
-11.0031263231068));
#411162=CARTESIAN_POINT('Ctrl Pts',(1.08288378264379E-13,1.50000000000006,
-11.));
#411163=CARTESIAN_POINT('Origin',(0.,2.5406128344257E-15,14.));
#411164=CARTESIAN_POINT('',(-1.92015623212974E-14,1.50000000000006,-10.4375));
#411165=CARTESIAN_POINT('',(6.27805609385103E-15,1.50000000000006,-10.5));
#411166=CARTESIAN_POINT('',(-1.8369701987211E-16,1.50000000000006,14.));
#411167=CARTESIAN_POINT('Ctrl Pts',(-3.67067487516692E-14,1.50000000000006,
-10.4375));
#411168=CARTESIAN_POINT('Ctrl Pts',(0.183341851414791,1.50000000000006,
-10.446321038939));
#411169=CARTESIAN_POINT('Ctrl Pts',(0.365304389821094,1.46638951329501,
-10.4560093402806));
#411170=CARTESIAN_POINT('Ctrl Pts',(0.719975731075,1.33045184597326,-10.4768495194574));
#411171=CARTESIAN_POINT('Ctrl Pts',(0.887586608293778,1.22501447146067,
-10.4878425175062));
#411172=CARTESIAN_POINT('Ctrl Pts',(1.16824672940074,0.959839578059451,
-10.50871175314));
#411173=CARTESIAN_POINT('Ctrl Pts',(1.28027201600136,0.804351637745947,
-10.517813797903));
#411174=CARTESIAN_POINT('Ctrl Pts',(1.44412642835151,0.451726875043387,
-10.5374040624976));
#411175=CARTESIAN_POINT('Ctrl Pts',(1.49122282301231,0.256500091922007,
-10.5482499948932));
#411176=CARTESIAN_POINT('Ctrl Pts',(1.50635756973098,-0.135933250839795,
-10.5700518472689));
#411177=CARTESIAN_POINT('Ctrl Pts',(1.47619662265256,-0.32931329751153,
-10.5807951831951));
#411178=CARTESIAN_POINT('Ctrl Pts',(1.34444850226405,-0.69243201844072,
-10.6009684454689));
#411179=CARTESIAN_POINT('Ctrl Pts',(1.24468450252906,-0.85893283475972,
-10.6098076676941));
#411180=CARTESIAN_POINT('Ctrl Pts',(0.983093886227757,-1.15030836951905,
-10.6304872169434));
#411181=CARTESIAN_POINT('Ctrl Pts',(0.821818972027301,-1.27054556457984,
-10.6415864819557));
#411182=CARTESIAN_POINT('Ctrl Pts',(0.468561415029391,-1.4377703342,-10.6632277265806));
#411183=CARTESIAN_POINT('Ctrl Pts',(0.281183978764755,-1.48582969927626,
-10.6735779100495));
#411184=CARTESIAN_POINT('Ctrl Pts',(-0.108421139476547,-1.50919956519595,
-10.6929719579829));
#411185=CARTESIAN_POINT('Ctrl Pts',(-0.307074366045606,-1.48161063819315,
-10.7027849379306));
#411186=CARTESIAN_POINT('Ctrl Pts',(-0.680323335747035,-1.35124120973445,
-10.7243642603709));
#411187=CARTESIAN_POINT('Ctrl Pts',(-0.851467393385639,-1.25047857568158,
-10.7353973947403));
#411188=CARTESIAN_POINT('Ctrl Pts',(-1.14006036034653,-0.993148583284006,
-10.7564303856814));
#411189=CARTESIAN_POINT('Ctrl Pts',(-1.25650534277258,-0.840982730153672,
-10.7657787372137));
#411190=CARTESIAN_POINT('Ctrl Pts',(-1.43045107049838,-0.493313284731216,
-10.7850937064038));
#411191=CARTESIAN_POINT('Ctrl Pts',(-1.48316886680921,-0.299559002937378,
-10.7958578331701));
#411192=CARTESIAN_POINT('Ctrl Pts',(-1.50969970494823,0.0927815138316741,
-10.8176545285462));
#411193=CARTESIAN_POINT('Ctrl Pts',(-1.48497842356764,0.287491265907305,
-10.8284717369948));
#411194=CARTESIAN_POINT('Ctrl Pts',(-1.36353336161468,0.653778980238932,
-10.8488210544577));
#411195=CARTESIAN_POINT('Ctrl Pts',(-1.26907168900137,0.822256806340053,
-10.8576155600706));
#411196=CARTESIAN_POINT('Ctrl Pts',(-1.01647448726449,1.12102612866584,
-10.8780677964479));
#411197=CARTESIAN_POINT('Ctrl Pts',(-0.858294843992598,1.24628920901697,
-10.889157748093));
#411198=CARTESIAN_POINT('Ctrl Pts',(-0.508964490595935,1.42404024301286,
-10.9109024412792));
#411199=CARTESIAN_POINT('Ctrl Pts',(-0.322490301199188,1.47748253414703,
-10.9213586929867));
#411200=CARTESIAN_POINT('Ctrl Pts',(-0.0873593104501269,1.49809429307222,
-10.9332439869127));
#411201=CARTESIAN_POINT('Ctrl Pts',(-0.0436554318174992,1.50000000000005,
-10.9353996270574));
#411202=CARTESIAN_POINT('Ctrl Pts',(-2.54796184151489E-13,1.50000000000006,
-10.9375));
#411203=CARTESIAN_POINT('Ctrl Pts',(1.08628384065668E-13,1.50000000000006,
-11.));
#411204=CARTESIAN_POINT('Ctrl Pts',(-0.124646908673343,1.50000000000006,
-10.9940029228103));
#411205=CARTESIAN_POINT('Ctrl Pts',(-0.249040797105659,1.48446746031111,
-10.9875865596269));
#411206=CARTESIAN_POINT('Ctrl Pts',(-0.559623546914417,1.40534011798786,
-10.9704456583784));
#411207=CARTESIAN_POINT('Ctrl Pts',(-0.737680680456972,1.32059828077476,
-10.9595249406239));
#411208=CARTESIAN_POINT('Ctrl Pts',(-1.05402417833964,1.08560316763031,
-10.9377772149539));
#411209=CARTESIAN_POINT('Ctrl Pts',(-1.18846144249417,0.936529206524611,
-10.9271681557025));
#411210=CARTESIAN_POINT('Ctrl Pts',(-1.38704353413505,0.601926838882839,
-10.9083193601514));
#411211=CARTESIAN_POINT('Ctrl Pts',(-1.45217349406124,0.421245189850194,
-10.8984025105472));
#411212=CARTESIAN_POINT('Ctrl Pts',(-1.51249416857681,0.0378826690716671,
-10.8771045927262));
#411213=CARTESIAN_POINT('Ctrl Pts',(-1.50431993816539,-0.161551377855926,
-10.8660249234525));
#411214=CARTESIAN_POINT('Ctrl Pts',(-1.41156072865313,-0.543887259640766,
-10.8447840411311));
#411215=CARTESIAN_POINT('Ctrl Pts',(-1.32863515419284,-0.723211201647225,
-10.8355014552816));
#411216=CARTESIAN_POINT('Ctrl Pts',(-1.10043927435011,-1.03735898530839,
-10.8157960485697));
#411217=CARTESIAN_POINT('Ctrl Pts',(-0.95833502546804,-1.16989583252076,
-10.8052774756184));
#411218=CARTESIAN_POINT('Ctrl Pts',(-0.625381252791918,-1.37802505171501,
-10.7834768625617));
#411219=CARTESIAN_POINT('Ctrl Pts',(-0.436129666690129,-1.44908952748857,
-10.7723974781641));
#411220=CARTESIAN_POINT('Ctrl Pts',(-0.0499634214048842,-1.51128177490525,
-10.7520904835969));
#411221=CARTESIAN_POINT('Ctrl Pts',(0.14261394883706,-1.50536798104238,
-10.7432875937719));
#411222=CARTESIAN_POINT('Ctrl Pts',(0.518993104954484,-1.42077123144426,
-10.7228291334691));
#411223=CARTESIAN_POINT('Ctrl Pts',(0.698905132383966,-1.3414422246146,
-10.7119695284904));
#411224=CARTESIAN_POINT('Ctrl Pts',(1.02161140091051,-1.11616616552023,
-10.6901856475987));
#411225=CARTESIAN_POINT('Ctrl Pts',(1.16040271940615,-0.971085200685996,
-10.6794780203732));
#411226=CARTESIAN_POINT('Ctrl Pts',(1.36858524807366,-0.642698786671831,
-10.6603399889589));
#411227=CARTESIAN_POINT('Ctrl Pts',(1.43891951287201,-0.464360061117776,
-10.6507977811732));
#411228=CARTESIAN_POINT('Ctrl Pts',(1.51056087056471,-0.0839233962982022,
-10.6296624109055));
#411229=CARTESIAN_POINT('Ctrl Pts',(1.50850992412876,0.115047782240133,
-10.6186084565422));
#411230=CARTESIAN_POINT('Ctrl Pts',(1.42751338067791,0.501204863537782,
-10.597155285359));
#411231=CARTESIAN_POINT('Ctrl Pts',(1.34921578399448,0.684542255947699,
-10.5875657786751));
#411232=CARTESIAN_POINT('Ctrl Pts',(1.12917766884718,1.00590001882789,-10.5680525853997));
#411233=CARTESIAN_POINT('Ctrl Pts',(0.991275930217928,1.14202854718277,
-10.5576364368965));
#411234=CARTESIAN_POINT('Ctrl Pts',(0.665412928738204,1.35905904241428,
-10.5359297210604));
#411235=CARTESIAN_POINT('Ctrl Pts',(0.478910239367815,1.43543475483331,
-10.5248350586672));
#411236=CARTESIAN_POINT('Ctrl Pts',(0.189462195571091,1.49102689087079,
-10.5093647571659));
#411237=CARTESIAN_POINT('Ctrl Pts',(0.0947355526073646,1.50000000000006,
-10.5045579664));
#411238=CARTESIAN_POINT('Ctrl Pts',(1.27398092075742E-14,1.50000000000006,
-10.5));
#411239=CARTESIAN_POINT('Origin',(0.,2.5406128344257E-15,14.));
#411240=CARTESIAN_POINT('',(6.27805609385103E-15,1.50000000000006,-9.93750000000001));
#411241=CARTESIAN_POINT('',(-5.74209899440205E-14,1.50000000000006,-9.99999999999997));
#411242=CARTESIAN_POINT('',(-1.8369701987211E-16,1.50000000000006,14.));
#411243=CARTESIAN_POINT('Ctrl Pts',(1.27398092075742E-14,1.50000000000006,
-9.93750000000001));
#411244=CARTESIAN_POINT('Ctrl Pts',(0.0130597123856812,1.50000000000006,
-9.93812833570512));
#411245=CARTESIAN_POINT('Ctrl Pts',(0.0261258122046185,1.49982944441199,
-9.93876171638113));
#411246=CARTESIAN_POINT('Ctrl Pts',(0.237959275893557,1.49429234528671,
-9.94910736696385));
#411247=CARTESIAN_POINT('Ctrl Pts',(0.433686462421857,1.4496292512905,-9.95976493711623));
#411248=CARTESIAN_POINT('Ctrl Pts',(0.792893421544092,1.28816466813327,
-9.98153241730482));
#411249=CARTESIAN_POINT('Ctrl Pts',(0.953519043999357,1.17424763864805,
-9.99242488309857));
#411250=CARTESIAN_POINT('Ctrl Pts',(1.21910047056181,0.894506588847375,
-10.0129732601584));
#411251=CARTESIAN_POINT('Ctrl Pts',(1.32278711632104,0.73251490178467,-10.0218047276788));
#411252=CARTESIAN_POINT('Ctrl Pts',(1.46761467127421,0.36919049735013,-10.041989416814));
#411253=CARTESIAN_POINT('Ctrl Pts',(1.50375821813677,0.169969130532061,
-10.0530572705261));
#411254=CARTESIAN_POINT('Ctrl Pts',(1.49577953643009,-0.22318446197286,
-10.0748991367764));
#411255=CARTESIAN_POINT('Ctrl Pts',(1.454743772956,-0.413406885805721,-10.0854670492116));
#411256=CARTESIAN_POINT('Ctrl Pts',(1.30205361502608,-0.769839727586497,
-10.1052688737549));
#411257=CARTESIAN_POINT('Ctrl Pts',(1.19111863148761,-0.932331192165051,
-10.1144237001276));
#411258=CARTESIAN_POINT('Ctrl Pts',(0.911065034014979,-1.20795688997008,
-10.1355540545017));
#411259=CARTESIAN_POINT('Ctrl Pts',(0.743850001404811,-1.31752856339574,
-10.1466428491044));
#411260=CARTESIAN_POINT('Ctrl Pts',(0.383419024228178,-1.4626367917708,
-10.1680148767007));
#411261=CARTESIAN_POINT('Ctrl Pts',(0.194654648445902,-1.49948343696352,
-10.178120324887));
#411262=CARTESIAN_POINT('Ctrl Pts',(-0.194671049551621,-1.50052739221325,
-10.1968807650223));
#411263=CARTESIAN_POINT('Ctrl Pts',(-0.391587058361149,-1.46157443191237,
-10.2074076180211));
#411264=CARTESIAN_POINT('Ctrl Pts',(-0.755882702683686,-1.31030645551807,
-10.2291366886138));
#411265=CARTESIAN_POINT('Ctrl Pts',(-0.92013529308169,-1.20067408870343,
-10.2400846385766));
#411266=CARTESIAN_POINT('Ctrl Pts',(-1.19345565040318,-0.92835447691962,
-10.2607992040601));
#411267=CARTESIAN_POINT('Ctrl Pts',(-1.30141473190726,-0.769733557604032,
-10.2697370245777));
#411268=CARTESIAN_POINT('Ctrl Pts',(-1.45579786117595,-0.412575577740146,
-10.2895791345702));
#411269=CARTESIAN_POINT('Ctrl Pts',(-1.4976105257064,-0.216125919194418,
-10.3004930044894));
#411270=CARTESIAN_POINT('Ctrl Pts',(-1.50212738741465,0.176094060945907,
-10.322283003386));
#411271=CARTESIAN_POINT('Ctrl Pts',(-1.46694025700791,0.368098920177736,
-10.33294994001));
#411272=CARTESIAN_POINT('Ctrl Pts',(-1.32557692878723,0.728189256860354,
-10.3529549587146));
#411273=CARTESIAN_POINT('Ctrl Pts',(-1.22075258050671,0.89284974055885,
-10.3619012291016));
#411274=CARTESIAN_POINT('Ctrl Pts',(-0.950712416699731,1.1771181175009,
-10.3827898863443));
#411275=CARTESIAN_POINT('Ctrl Pts',(-0.786648129094687,1.29253158841395,
-10.3938893628095));
#411276=CARTESIAN_POINT('Ctrl Pts',(-0.429956265913086,1.44971739568654,
-10.4154169805026));
#411277=CARTESIAN_POINT('Ctrl Pts',(-0.241864830797446,1.49267108033264,
-10.4256596918008));
#411278=CARTESIAN_POINT('Ctrl Pts',(-0.0338291921616082,1.49971408378776,
-10.4358644501162));
#411279=CARTESIAN_POINT('Ctrl Pts',(-0.0169091055322462,1.50000000000006,
-10.4366864602808));
#411280=CARTESIAN_POINT('Ctrl Pts',(-3.82194276227227E-14,1.50000000000006,
-10.4375));
#411281=CARTESIAN_POINT('Ctrl Pts',(1.27398092075742E-14,1.50000000000006,
-10.5));
#411282=CARTESIAN_POINT('Ctrl Pts',(-0.0961640021789709,1.50000000000006,
-10.4953733072879));
#411283=CARTESIAN_POINT('Ctrl Pts',(-0.192312189894884,1.49075428983337,
-10.4904905501673));
#411284=CARTESIAN_POINT('Ctrl Pts',(-0.477782555963758,1.43508007583453,
-10.4752093448316));
#411285=CARTESIAN_POINT('Ctrl Pts',(-0.659394616266541,1.36121942857362,
-10.4644198458601));
#411286=CARTESIAN_POINT('Ctrl Pts',(-0.988185935655053,1.14587042885574,
-10.4426189494716));
#411287=CARTESIAN_POINT('Ctrl Pts',(-1.13122500556002,1.00492903946411,
-10.4318219404179));
#411288=CARTESIAN_POINT('Ctrl Pts',(-1.34897707229762,0.682873836252697,
-10.4123993613552));
#411289=CARTESIAN_POINT('Ctrl Pts',(-1.42451113759172,0.506797536541834,
-10.4031554186968));
#411290=CARTESIAN_POINT('Ctrl Pts',(-1.5072744310769,0.129344161205523,
-10.3821857867337));
#411291=CARTESIAN_POINT('Ctrl Pts',(-1.51123947488267,-0.0689901135617249,
-10.3711672159133));
#411292=CARTESIAN_POINT('Ctrl Pts',(-1.44197477365096,-0.458773265628078,
-10.349512596354));
#411293=CARTESIAN_POINT('Ctrl Pts',(-1.36829696590876,-0.646139569010169,
-10.3395505637719));
#411294=CARTESIAN_POINT('Ctrl Pts',(-1.15629839165518,-0.974502057759996,
-10.3202295973694));
#411295=CARTESIAN_POINT('Ctrl Pts',(-1.02257339529214,-1.11400279948846,
-10.3099207298785));
#411296=CARTESIAN_POINT('Ctrl Pts',(-0.703835080463324,-1.33947840127368,
-10.2883222143955));
#411297=CARTESIAN_POINT('Ctrl Pts',(-0.520145363547979,-1.42093085883445,
-10.2772218705043));
#411298=CARTESIAN_POINT('Ctrl Pts',(-0.137752926488043,-1.50604856638516,
-10.2564596250329));
#411299=CARTESIAN_POINT('Ctrl Pts',(0.0566843765573322,-1.51127194686497,
-10.2475858812965));
#411300=CARTESIAN_POINT('Ctrl Pts',(0.437895743281651,-1.44767912219312,
-10.2274783735115));
#411301=CARTESIAN_POINT('Ctrl Pts',(0.62098502059929,-1.37909085880787,
-10.2167642570109));
#411302=CARTESIAN_POINT('Ctrl Pts',(0.955323109226357,-1.17341366981076,
-10.1949651529719));
#411303=CARTESIAN_POINT('Ctrl Pts',(1.10231620339654,-1.03656187644939,
-10.1840915057267));
#411304=CARTESIAN_POINT('Ctrl Pts',(1.32918637441208,-0.720672929449274,
-10.1644015165622));
#411305=CARTESIAN_POINT('Ctrl Pts',(1.40969808132489,-0.546689096092594,
-10.1553716164496));
#411306=CARTESIAN_POINT('Ctrl Pts',(1.50291696629879,-0.172135111132355,
-10.1345630617296));
#411307=CARTESIAN_POINT('Ctrl Pts',(1.5125272829466,0.0254350087036306,
-10.1235869439609));
#411308=CARTESIAN_POINT('Ctrl Pts',(1.45482028604201,0.415991217406076,
-10.1018893768108));
#411309=CARTESIAN_POINT('Ctrl Pts',(1.38692473639455,0.604931293171288,
-10.0915914671261));
#411310=CARTESIAN_POINT('Ctrl Pts',(1.18555560683619,0.938573083172626,
-10.072635262863));
#411311=CARTESIAN_POINT('Ctrl Pts',(1.05658959252395,1.08169148113985,-10.0624548715517));
#411312=CARTESIAN_POINT('Ctrl Pts',(0.746057306961948,1.31633259720232,
-10.0409965712171));
#411313=CARTESIAN_POINT('Ctrl Pts',(0.565664761564748,1.40333993984853,
-10.0299005602009));
#411314=CARTESIAN_POINT('Ctrl Pts',(0.251256457537897,1.4841902328274,-10.0125277421489));
#411315=CARTESIAN_POINT('Ctrl Pts',(0.12575413515895,1.50000000000007,-10.0060503486488));
#411316=CARTESIAN_POINT('Ctrl Pts',(-1.14248888127833E-13,1.50000000000006,
-9.99999999999997));
#411317=CARTESIAN_POINT('Origin',(0.,2.5406128344257E-15,14.));
#411318=CARTESIAN_POINT('',(1.01826625150655E-13,1.50000000000006,-9.43750000000001));
#411319=CARTESIAN_POINT('',(-1.21120035981893E-13,1.50000000000006,-9.49999999999997));
#411320=CARTESIAN_POINT('',(-1.8369701987211E-16,1.50000000000006,14.));
#411321=CARTESIAN_POINT('Ctrl Pts',(2.03836947321181E-13,1.50000000000006,
-9.43750000000001));
#411322=CARTESIAN_POINT('Ctrl Pts',(0.0423644631912906,1.50000000000006,
-9.43953826118564));
#411323=CARTESIAN_POINT('Ctrl Pts',(0.0847727287843001,1.49820533233011,
-9.44162848169512));
#411324=CARTESIAN_POINT('Ctrl Pts',(0.32528689345542,1.4777501628067,-9.45376842399161));
#411325=CARTESIAN_POINT('Ctrl Pts',(0.518115985397973,1.42165119715189,
-9.46460422260485));
#411326=CARTESIAN_POINT('Ctrl Pts',(0.866288558520853,1.23982356349243,
-9.48640645094125));
#411327=CARTESIAN_POINT('Ctrl Pts',(1.0191904154483,1.11753375322258,-9.49715988413679));
#411328=CARTESIAN_POINT('Ctrl Pts',(1.26881896757184,0.822831198353581,
-9.51735632553032));
#411329=CARTESIAN_POINT('Ctrl Pts',(1.36370261923566,0.653658070164938,
-9.52618566276873));
#411330=CARTESIAN_POINT('Ctrl Pts',(1.48667902345296,0.281956269164541,
-9.5468357628243));
#411331=CARTESIAN_POINT('Ctrl Pts',(1.5109431375262,0.0821818978378209,
-9.55793433900912));
#411332=CARTESIAN_POINT('Ctrl Pts',(1.48058378314258,-0.307622245431263,
-9.57959012474629));
#411333=CARTESIAN_POINT('Ctrl Pts',(1.42918258544925,-0.494183852189728,
-9.58995465845509));
#411334=CARTESIAN_POINT('Ctrl Pts',(1.2559630345297,-0.843738403721386,
-9.6093743557624));
#411335=CARTESIAN_POINT('Ctrl Pts',(1.13351755852915,-1.00224760565162,
-9.61913715563922));
#411336=CARTESIAN_POINT('Ctrl Pts',(0.835190258339646,-1.26142024596133,
-9.6406896745704));
#411337=CARTESIAN_POINT('Ctrl Pts',(0.662681532840596,-1.35999168419044,
-9.65172760000214));
#411338=CARTESIAN_POINT('Ctrl Pts',(0.295926946589629,-1.48273874308817,
-9.67278272878528));
#411339=CARTESIAN_POINT('Ctrl Pts',(0.106010913449538,-1.50825160362181,
-9.68217033633698));
#411340=CARTESIAN_POINT('Ctrl Pts',(-0.282146492696278,-1.48658672961012,
-9.70144737030338));
#411341=CARTESIAN_POINT('Ctrl Pts',(-0.476497757838591,-1.43613145389777,
-9.71219963534377));
#411342=CARTESIAN_POINT('Ctrl Pts',(-0.830283464242,-1.26430209867626,-9.73399419572443));
#411343=CARTESIAN_POINT('Ctrl Pts',(-0.987065796433557,-1.14609850085419,
-9.74482082247184));
#411344=CARTESIAN_POINT('Ctrl Pts',(-1.24462862356872,-0.858783093545962,
-9.76519380330649));
#411345=CARTESIAN_POINT('Ctrl Pts',(-1.34389439900638,-0.693221006526352,
-9.77398772185978));
#411346=CARTESIAN_POINT('Ctrl Pts',(-1.47780558639996,-0.325642226491207,
-9.79440876519507));
#411347=CARTESIAN_POINT('Ctrl Pts',(-1.50799467343637,-0.126058655085577,
-9.80549674138427));
#411348=CARTESIAN_POINT('Ctrl Pts',(-1.48876910511602,0.265573728760382,
-9.82725409604237));
#411349=CARTESIAN_POINT('Ctrl Pts',(-1.44251008882995,0.454033490561692,
-9.83772408280911));
#411350=CARTESIAN_POINT('Ctrl Pts',(-1.27955557689145,0.807067726692858,
-9.85733709592751));
#411351=CARTESIAN_POINT('Ctrl Pts',(-1.16293731341604,0.967580676555588,
-9.86675872676962));
#411352=CARTESIAN_POINT('Ctrl Pts',(-0.873763612333058,1.23511086436131,
-9.88810299705557));
#411353=CARTESIAN_POINT('Ctrl Pts',(-0.703831043145741,1.33924652554451,
-9.89917153885769));
#411354=CARTESIAN_POINT('Ctrl Pts',(-0.352421064611548,1.46873171212293,
-9.9196755700712));
#411355=CARTESIAN_POINT('Ctrl Pts',(-0.176837209122336,1.50000000000006,
-9.92899191580921));
#411356=CARTESIAN_POINT('Ctrl Pts',(1.196959198424E-14,1.50000000000006,
-9.9375));
#411357=CARTESIAN_POINT('Ctrl Pts',(-1.14658282868169E-13,1.50000000000006,
-9.99999999999997));
#411358=CARTESIAN_POINT('Ctrl Pts',(-0.0675188942384693,1.50000000000005,
-9.99675149568631));
#411359=CARTESIAN_POINT('Ctrl Pts',(-0.135098082697613,1.49544172065095,
-9.99337347159485));
#411360=CARTESIAN_POINT('Ctrl Pts',(-0.393664768377399,1.46025115578112,
-9.97995566043897));
#411361=CARTESIAN_POINT('Ctrl Pts',(-0.578204640568276,1.39748667206119,
-9.96933352381739));
#411362=CARTESIAN_POINT('Ctrl Pts',(-0.919980234621133,1.20164805513356,
-9.94744987630033));
#411363=CARTESIAN_POINT('Ctrl Pts',(-1.07241923289505,1.06782789335319,
-9.93639842486017));
#411364=CARTESIAN_POINT('Ctrl Pts',(-1.30920251764387,0.756449592440474,
-9.91635678651348));
#411365=CARTESIAN_POINT('Ctrl Pts',(-1.39452034595421,0.584420019403402,
-9.90746777885578));
#411366=CARTESIAN_POINT('Ctrl Pts',(-1.49764701025264,0.212695779101129,
-9.88681643217232));
#411367=CARTESIAN_POINT('Ctrl Pts',(-1.51258840311147,0.0159976360466687,
-9.87588875755818));
#411368=CARTESIAN_POINT('Ctrl Pts',(-1.46581254175606,-0.375356815859686,
-9.85414684356338));
#411369=CARTESIAN_POINT('Ctrl Pts',(-1.40323545031248,-0.56608835829669,
-9.84355064676133));
#411370=CARTESIAN_POINT('Ctrl Pts',(-1.21149399001615,-0.904714767481383,
-9.82473806847329));
#411371=CARTESIAN_POINT('Ctrl Pts',(-1.08700372010449,-1.05104787787605,
-9.81476938314896));
#411372=CARTESIAN_POINT('Ctrl Pts',(-0.78414191969591,-1.29391841961372,
-9.79345153404571));
#411373=CARTESIAN_POINT('Ctrl Pts',(-0.606917337671277,-1.38591440254458,
-9.78236936839716));
#411374=CARTESIAN_POINT('Ctrl Pts',(-0.229116448644826,-1.49524029577133,
-9.76115558428146));
#411375=CARTESIAN_POINT('Ctrl Pts',(-0.0324969925423966,-1.51233971487207,
-9.75190628214028));
#411376=CARTESIAN_POINT('Ctrl Pts',(0.353383565241518,-1.47045095097361,
-9.73217701837269));
#411377=CARTESIAN_POINT('Ctrl Pts',(0.539077702549313,-1.41296972338044,
-9.72164610425942));
#411378=CARTESIAN_POINT('Ctrl Pts',(0.885253015832435,-1.22735984233263,
-9.69983490670441));
#411379=CARTESIAN_POINT('Ctrl Pts',(1.04100510498355,-1.09836632522092,
-9.68875812756812));
#411380=CARTESIAN_POINT('Ctrl Pts',(1.28679104961533,-0.794106348618159,
-9.66848107977669));
#411381=CARTESIAN_POINT('Ctrl Pts',(1.37728758213822,-0.62411371477506,
-9.65967298415421));
#411382=CARTESIAN_POINT('Ctrl Pts',(1.49087595034938,-0.255462173952587,
-9.63919234299741));
#411383=CARTESIAN_POINT('Ctrl Pts',(1.51141733568497,-0.0598401750380719,
-9.62832445416882));
#411384=CARTESIAN_POINT('Ctrl Pts',(1.4761958376045,0.332205859839538,-9.60654411889785));
#411385=CARTESIAN_POINT('Ctrl Pts',(1.41922573178766,0.524726274931734,
-9.59584854028161));
#411386=CARTESIAN_POINT('Ctrl Pts',(1.23762446457936,0.868552370279251,
-9.57674709054008));
#411387=CARTESIAN_POINT('Ctrl Pts',(1.11776010832914,1.0182063201762,-9.56716141605903));
#411388=CARTESIAN_POINT('Ctrl Pts',(0.823072067791609,1.26941697957466,
-9.54600515722591));
#411389=CARTESIAN_POINT('Ctrl Pts',(0.649285913538544,1.36649044792844,
-9.53494738174891));
#411390=CARTESIAN_POINT('Ctrl Pts',(0.312301830568179,1.4755086268206,-9.51570594475061));
#411391=CARTESIAN_POINT('Ctrl Pts',(0.156516666443393,1.50000000000008,
-9.50753041162529));
#411392=CARTESIAN_POINT('Ctrl Pts',(-2.41993924898765E-13,1.50000000000006,
-9.49999999999997));
#411393=CARTESIAN_POINT('Origin',(0.,2.5406128344257E-15,14.));
#411394=CARTESIAN_POINT('',(3.81275791127862E-14,1.50000000000006,-8.93750000000001));
#411395=CARTESIAN_POINT('',(-9.18485099360549E-17,1.50000000000006,-8.99999999999998));
#411396=CARTESIAN_POINT('',(-1.8369701987211E-16,1.50000000000006,14.));
#411397=CARTESIAN_POINT('Ctrl Pts',(7.64388552454446E-14,1.50000000000006,
-8.93750000000001));
#411398=CARTESIAN_POINT('Ctrl Pts',(0.0701697277412552,1.50000000000006,
-8.94087604260004));
#411399=CARTESIAN_POINT('Ctrl Pts',(0.140393881454839,1.49507682204823,
-8.94439145871407));
#411400=CARTESIAN_POINT('Ctrl Pts',(0.408745304662783,1.457103970486,-8.95835732401523));
#411401=CARTESIAN_POINT('Ctrl Pts',(0.599667970056199,1.3894626792969,-8.96942201979208));
#411402=CARTESIAN_POINT('Ctrl Pts',(0.937003600546002,1.18710465492744,
-8.99127314411378));
#411403=CARTESIAN_POINT('Ctrl Pts',(1.08172971331996,1.05691568366112,-9.00185264277413));
#411404=CARTESIAN_POINT('Ctrl Pts',(1.31505937341547,0.747358543121225,
-9.02167753073908));
#411405=CARTESIAN_POINT('Ctrl Pts',(1.4008716427756,0.570519225809976,-9.03080448745509));
#411406=CARTESIAN_POINT('Ctrl Pts',(1.50095938264119,0.190655899122854,
-9.05190800560437));
#411407=CARTESIAN_POINT('Ctrl Pts',(1.5129913597143,-0.00897481519057823,
-9.062998600844));
#411408=CARTESIAN_POINT('Ctrl Pts',(1.45982897099295,-0.394006866340737,
-9.08438927035234));
#411409=CARTESIAN_POINT('Ctrl Pts',(1.39798730795961,-0.576192500279294,
-9.09451069446004));
#411410=CARTESIAN_POINT('Ctrl Pts',(1.20537929923835,-0.91462821674284,
-9.11331267870802));
#411411=CARTESIAN_POINT('Ctrl Pts',(1.0737122353804,-1.06615396931563,-9.12378971735921));
#411412=CARTESIAN_POINT('Ctrl Pts',(0.761347951035123,-1.30714841853425,
-9.14551264125295));
#411413=CARTESIAN_POINT('Ctrl Pts',(0.584517842961423,-1.39521749262844,
-9.15646674696366));
#411414=CARTESIAN_POINT('Ctrl Pts',(0.212337725831777,-1.49702241144052,
-9.17720118560942));
#411415=CARTESIAN_POINT('Ctrl Pts',(0.0210784953152501,-1.51185650475691,
-9.18615651306704));
#411416=CARTESIAN_POINT('Ctrl Pts',(-0.365530383982027,-1.46831626746077,
-9.20596669248082));
#411417=CARTESIAN_POINT('Ctrl Pts',(-0.55677754231025,-1.40696314389929,
-9.21687232910829));
#411418=CARTESIAN_POINT('Ctrl Pts',(-0.899424319695077,-1.21591800100396,
-9.2386647393965));
#411419=CARTESIAN_POINT('Ctrl Pts',(-1.04859030674976,-1.08990528801022,
-9.24934184443354));
#411420=CARTESIAN_POINT('Ctrl Pts',(-1.29070978850643,-0.788305324551741,
-9.26936860019363));
#411421=CARTESIAN_POINT('Ctrl Pts',(-1.38142829751791,-0.615642971931764,
-9.27829761267055));
#411422=CARTESIAN_POINT('Ctrl Pts',(-1.49393087063595,-0.240125194098544,
-9.29915971143906));
#411423=CARTESIAN_POINT('Ctrl Pts',(-1.51256570660118,-0.0403266795942435,
-9.31025962891152));
#411424=CARTESIAN_POINT('Ctrl Pts',(-1.4716815678648,0.347448886442948,
-9.33180271591359));
#411425=CARTESIAN_POINT('Ctrl Pts',(-1.4154460993233,0.532073427304002,
-9.34205963485031));
#411426=CARTESIAN_POINT('Ctrl Pts',(-1.23241032036788,0.878223448450719,
-9.36129019158068));
#411427=CARTESIAN_POINT('Ctrl Pts',(-1.10425483612739,1.03478069252725,
-9.37144875588485));
#411428=CARTESIAN_POINT('Ctrl Pts',(-0.797154057907381,1.28570667084145,
-9.39319431503027));
#411429=CARTESIAN_POINT('Ctrl Pts',(-0.622323356335188,1.37884474301256,
-9.40419302975296));
#411430=CARTESIAN_POINT('Ctrl Pts',(-0.293385231348153,1.4784011982189,
-9.42278452975936));
#411431=CARTESIAN_POINT('Ctrl Pts',(-0.146985099260076,1.50000000000006,
-9.4304281761146));
#411432=CARTESIAN_POINT('Ctrl Pts',(2.02581007524572E-13,1.50000000000006,
-9.43750000000001));
#411433=CARTESIAN_POINT('Ctrl Pts',(-2.42056374943915E-13,1.50000000000006,
-9.49999999999997));
#411434=CARTESIAN_POINT('Ctrl Pts',(-0.0400937591764138,1.50000000000005,
-9.4980709881122));
#411435=CARTESIAN_POINT('Ctrl Pts',(-0.0802312376367462,1.4983925534736,
-9.49609522148706));
#411436=CARTESIAN_POINT('Ctrl Pts',(-0.311798731012663,1.47975813117801,
-9.48443630242584));
#411437=CARTESIAN_POINT('Ctrl Pts',(-0.49852193792271,1.4277110365756,-9.47400682531687));
#411438=CARTESIAN_POINT('Ctrl Pts',(-0.848900532454104,1.25268257467032,
-9.45228732560803));
#411439=CARTESIAN_POINT('Ctrl Pts',(-1.00789774150321,1.12871623256175,
-9.44119405931794));
#411440=CARTESIAN_POINT('Ctrl Pts',(-1.26283453615189,0.831854778879047,
-9.42068225557535));
#411441=CARTESIAN_POINT('Ctrl Pts',(-1.35866853382425,0.663892795229351,
-9.41188293306834));
#411442=CARTESIAN_POINT('Ctrl Pts',(-1.48280150205461,0.298424756848632,
-9.3915791531583));
#411443=CARTESIAN_POINT('Ctrl Pts',(-1.50894686669985,0.104047412402745,
-9.3807804118002));
#411444=CARTESIAN_POINT('Ctrl Pts',(-1.48539000906149,-0.288349426218138,
-9.35898058743237));
#411445=CARTESIAN_POINT('Ctrl Pts',(-1.43413424677483,-0.482503912567459,
-9.34819422707963));
#411446=CARTESIAN_POINT('Ctrl Pts',(-1.26281562140763,-0.831475645725152,
-9.32880690857087));
#411447=CARTESIAN_POINT('Ctrl Pts',(-1.14753048075311,-0.984504981270521,
-9.31952989207304));
#411448=CARTESIAN_POINT('Ctrl Pts',(-0.861013851284105,-1.24390106010667,
-9.2985394076761));
#411449=CARTESIAN_POINT('Ctrl Pts',(-0.690784490420879,-1.34590121332312,
-9.28751590614356));
#411450=CARTESIAN_POINT('Ctrl Pts',(-0.318241244180354,-1.47931981507511,
-9.26588583858086));
#411451=CARTESIAN_POINT('Ctrl Pts',(-0.119286155130846,-1.50844485536951,
-9.25597373713049));
#411452=CARTESIAN_POINT('Ctrl Pts',(0.270834169652757,-1.48773429007375,
-9.23662877077254));
#411453=CARTESIAN_POINT('Ctrl Pts',(0.458413226153797,-1.44102059205357,
-9.22630626648598));
#411454=CARTESIAN_POINT('Ctrl Pts',(0.812603298748567,-1.27643655127287,
-9.20469350976234));
#411455=CARTESIAN_POINT('Ctrl Pts',(0.974627172716593,-1.15746537014635,
-9.19359337746016));
#411456=CARTESIAN_POINT('Ctrl Pts',(1.23845215928419,-0.867953395363224,
-9.17285809257615));
#411457=CARTESIAN_POINT('Ctrl Pts',(1.33954625945943,-0.701940758562861,
-9.1639967088091));
#411458=CARTESIAN_POINT('Ctrl Pts',(1.47384264903161,-0.339617780380702,
-9.14386765446565));
#411459=CARTESIAN_POINT('Ctrl Pts',(1.50534068747472,-0.146589673115085,
-9.13314387072867));
#411460=CARTESIAN_POINT('Ctrl Pts',(1.49302224351914,0.245815292223104,
-9.11134359487654));
#411461=CARTESIAN_POINT('Ctrl Pts',(1.44732297201183,0.441380475807474,
-9.10047886245519));
#411462=CARTESIAN_POINT('Ctrl Pts',(1.28597357042616,0.795215414898501,
-9.08082136583902));
#411463=CARTESIAN_POINT('Ctrl Pts',(1.17503106654397,0.95153043233265,-9.07176897431654));
#411464=CARTESIAN_POINT('Ctrl Pts',(0.896322161173119,1.21861508181268,
-9.05094056781364));
#411465=CARTESIAN_POINT('Ctrl Pts',(0.729595943825354,1.32517998985375,
-9.03995881260694));
#411466=CARTESIAN_POINT('Ctrl Pts',(0.372645820190216,1.4650059210476,-9.01890098813199));
#411467=CARTESIAN_POINT('Ctrl Pts',(0.187073537795138,1.50000000000006,
-9.00900057978367));
#411468=CARTESIAN_POINT('Ctrl Pts',(-2.77555756156289E-16,1.50000000000006,
-8.99999999999998));
#411469=CARTESIAN_POINT('Origin',(0.,2.5406128344257E-15,14.));
#411470=CARTESIAN_POINT('',(-3.69404266092344E-16,1.50000000000006,-8.4375));
#411471=CARTESIAN_POINT('',(1.90178653014251E-14,1.50000000000006,-8.49999999999998));
#411472=CARTESIAN_POINT('',(-1.8369701987211E-16,1.50000000000006,14.));
#411473=CARTESIAN_POINT('Ctrl Pts',(6.93889390390723E-16,1.50000000000006,
-8.4375));
#411474=CARTESIAN_POINT('Ctrl Pts',(0.100048703118938,1.50000000000006,
-8.44231359547315));
#411475=CARTESIAN_POINT('Ctrl Pts',(0.200061577253575,1.48999234904905,
-8.44740345742775));
#411476=CARTESIAN_POINT('Ctrl Pts',(0.49392690742635,1.43030749600499,-8.46319997230237));
#411477=CARTESIAN_POINT('Ctrl Pts',(0.679423997631909,1.35207810285786,
-8.47429774391457));
#411478=CARTESIAN_POINT('Ctrl Pts',(1.00272579266332,1.13195669206866,-8.49596709241351));
#411479=CARTESIAN_POINT('Ctrl Pts',(1.1391209973992,0.994589792123244,-8.50634515698175));
#411480=CARTESIAN_POINT('Ctrl Pts',(1.35625249336917,0.670688029442479,
-8.52578917213798));
#411481=CARTESIAN_POINT('Ctrl Pts',(1.43288715691681,0.48590213439737,-8.535505436978));
#411482=CARTESIAN_POINT('Ctrl Pts',(1.50965805252362,0.0984174505511938,
-8.55703236385833));
#411483=CARTESIAN_POINT('Ctrl Pts',(1.50953122939287,-0.1003441745013,-8.56807467636125));
#411484=CARTESIAN_POINT('Ctrl Pts',(1.43386485159747,-0.479713406126239,
-8.58915074478486));
#411485=CARTESIAN_POINT('Ctrl Pts',(1.36165936049534,-0.657228892664954,
-8.59857682493578));
#411486=CARTESIAN_POINT('Ctrl Pts',(1.15002925545568,-0.983350391502387,
-8.61781781363514));
#411487=CARTESIAN_POINT('Ctrl Pts',(1.00969655551726,-1.12695819727209,
-8.62855867952476));
#411488=CARTESIAN_POINT('Ctrl Pts',(0.684767734231053,-1.34868488435149,
-8.65035089936894));
#411489=CARTESIAN_POINT('Ctrl Pts',(0.504225856506111,-1.42605189050979,
-8.66118630801538));
#411490=CARTESIAN_POINT('Ctrl Pts',(0.126938974991646,-1.50680375704638,
-8.68158163896951));
#411491=CARTESIAN_POINT('Ctrl Pts',(-0.0659595355830271,-1.51070142737475,
-8.69037621776393));
#411492=CARTESIAN_POINT('Ctrl Pts',(-0.451479814049411,-1.44435062852565,
-8.71076764855562));
#411493=CARTESIAN_POINT('Ctrl Pts',(-0.639764629794639,-1.37137527640744,
-8.72185359909125));
#411494=CARTESIAN_POINT('Ctrl Pts',(-0.970208871646639,-1.16003599972617,
-8.7436226405534));
#411495=CARTESIAN_POINT('Ctrl Pts',(-1.11082029581379,-1.02619964802706,
-8.75410548728899));
#411496=CARTESIAN_POINT('Ctrl Pts',(-1.3361091699828,-0.709470730845153,
-8.7737427287785));
#411497=CARTESIAN_POINT('Ctrl Pts',(-1.41739177297902,-0.528725606616922,
-8.78312635518803));
#411498=CARTESIAN_POINT('Ctrl Pts',(-1.50597586053692,-0.145012426518024,
-8.80444375408241));
#411499=CARTESIAN_POINT('Ctrl Pts',(-1.51196665413278,0.0542778614058951,
-8.81551543674485));
#411500=CARTESIAN_POINT('Ctrl Pts',(-1.44760783648443,0.436609821339279,
-8.83675610118559));
#411501=CARTESIAN_POINT('Ctrl Pts',(-1.38063092643955,0.616451079174067,
-8.8465313380023));
#411502=CARTESIAN_POINT('Ctrl Pts',(-1.17864065284233,0.948861810065223,
-8.86548323098553));
#411503=CARTESIAN_POINT('Ctrl Pts',(-1.04264761307,1.09653677036197,-8.8761282813927));
#411504=CARTESIAN_POINT('Ctrl Pts',(-0.724016606612002,1.32810974829059,
-8.89789100555883));
#411505=CARTESIAN_POINT('Ctrl Pts',(-0.545284169269985,1.41093880861734,
-8.90879108119116));
#411506=CARTESIAN_POINT('Ctrl Pts',(-0.239013467161963,1.48569846285508,
-8.9256031942789));
#411507=CARTESIAN_POINT('Ctrl Pts',(-0.119605100351261,1.50000000000006,
-8.93174549692631));
#411508=CARTESIAN_POINT('Ctrl Pts',(7.60502771868232E-14,1.50000000000006,
-8.93750000000001));
#411509=CARTESIAN_POINT('Ctrl Pts',(0.,1.50000000000006,-8.99999999999998));
#411510=CARTESIAN_POINT('Ctrl Pts',(-0.0114925749065063,1.50000000000006,
-8.99944706323198));
#411511=CARTESIAN_POINT('Ctrl Pts',(-0.0229904684161551,1.49986792103453,
-8.99889020171249));
#411512=CARTESIAN_POINT('Ctrl Pts',(-0.225457336202678,1.49521110800026,
-8.98901965407667));
#411513=CARTESIAN_POINT('Ctrl Pts',(-0.413805280348288,1.45438274491613,
-8.97882363819207));
#411514=CARTESIAN_POINT('Ctrl Pts',(-0.77184384434294,1.30139148024828,
-8.9573477423983));
#411515=CARTESIAN_POINT('Ctrl Pts',(-0.937027506192782,1.18800214473311,
-8.94625063599776));
#411516=CARTESIAN_POINT('Ctrl Pts',(-1.21056341325082,0.90672298017732,
-8.9252768234068));
#411517=CARTESIAN_POINT('Ctrl Pts',(-1.31750640773443,0.742820403229874,
-8.91626780017949));
#411518=CARTESIAN_POINT('Ctrl Pts',(-1.46283170239402,0.383998346248297,
-8.89633324145829));
#411519=CARTESIAN_POINT('Ctrl Pts',(-1.50007403509498,0.192597208439964,
-8.88569984491338));
#411520=CARTESIAN_POINT('Ctrl Pts',(-1.49992278590957,-0.201455252188196,
-8.86380804154515));
#411521=CARTESIAN_POINT('Ctrl Pts',(-1.45949387408537,-0.400310244540207,
-8.85276054197004));
#411522=CARTESIAN_POINT('Ctrl Pts',(-1.30684443782229,-0.760502260741033,
-8.83274987440333));
#411523=CARTESIAN_POINT('Ctrl Pts',(-1.19995386392689,-0.919958659763558,
-8.82384506664718));
#411524=CARTESIAN_POINT('Ctrl Pts',(-0.928567014099058,-1.19414298736089,
-8.80317172942481));
#411525=CARTESIAN_POINT('Ctrl Pts',(-0.765212590437898,-1.3048592710734,
-8.79223688372662));
#411526=CARTESIAN_POINT('Ctrl Pts',(-0.402246980449423,-1.45866182365666,
-8.77050139954652));
#411527=CARTESIAN_POINT('Ctrl Pts',(-0.205628964604913,-1.49907990593575,
-8.75991888634082));
#411528=CARTESIAN_POINT('Ctrl Pts',(0.183567016707029,-1.50085076540667,
-8.74114449541847));
#411529=CARTESIAN_POINT('Ctrl Pts',(0.372471377496952,-1.46545895758719,
-8.73111998909442));
#411530=CARTESIAN_POINT('Ctrl Pts',(0.733811676972188,-1.32312328078896,
-8.70978122703021));
#411531=CARTESIAN_POINT('Ctrl Pts',(0.901728634164142,-1.21491752126138,
-8.69869660311809));
#411532=CARTESIAN_POINT('Ctrl Pts',(1.18409112004873,-0.941320453907733,
-8.67751151314428));
#411533=CARTESIAN_POINT('Ctrl Pts',(1.29645387603392,-0.779329009794782,
-8.66829605609977));
#411534=CARTESIAN_POINT('Ctrl Pts',(1.45174678002209,-0.423750361571602,
-8.64854168675403));
#411535=CARTESIAN_POINT('Ctrl Pts',(1.49411427757351,-0.233961822461871,
-8.63799787902571));
#411536=CARTESIAN_POINT('Ctrl Pts',(1.50495464048548,0.158835443777422,
-8.61617580867909));
#411537=CARTESIAN_POINT('Ctrl Pts',(1.4703232657174,0.358164972608317,-8.60510194596626));
#411538=CARTESIAN_POINT('Ctrl Pts',(1.32826209597344,0.722580561232961,
-8.58485663548711));
#411539=CARTESIAN_POINT('Ctrl Pts',(1.22570099624627,0.88547346159937,-8.5760417482997));
#411540=CARTESIAN_POINT('Ctrl Pts',(0.962160812325709,1.16715358642565,
-8.55553771737712));
#411541=CARTESIAN_POINT('Ctrl Pts',(0.802505651928995,1.282176705519,-8.54466121824959));
#411542=CARTESIAN_POINT('Ctrl Pts',(0.444653951517676,1.44630416088315,
-8.52288497430371));
#411543=CARTESIAN_POINT('Ctrl Pts',(0.249261200892981,1.49244982176182,
-8.51220231229284));
#411544=CARTESIAN_POINT('Ctrl Pts',(0.0336834707125518,1.49971652858077,
-8.5016284709464));
#411545=CARTESIAN_POINT('Ctrl Pts',(0.0168366541021336,1.50000000000006,
-8.50081005389816));
#411546=CARTESIAN_POINT('Ctrl Pts',(3.82194276227224E-14,1.50000000000006,
-8.49999999999998));
#411547=CARTESIAN_POINT('Origin',(0.,2.5406128344257E-15,14.));
#411548=CARTESIAN_POINT('',(-7.65307037553809E-14,1.50000000000006,-7.93749999999999));
#411549=CARTESIAN_POINT('',(1.08196529754441E-13,1.50000000000006,-7.99999999999999));
#411550=CARTESIAN_POINT('',(-1.8369701987211E-16,1.50000000000006,14.));
#411551=CARTESIAN_POINT('Ctrl Pts',(-1.52933221642115E-13,1.50000000000006,
-7.93749999999999));
#411552=CARTESIAN_POINT('Ctrl Pts',(0.131087257000726,1.50000000000007,
-7.94380693859306));
#411553=CARTESIAN_POINT('Ctrl Pts',(0.261858013506839,1.48282092882581,
-7.95057584597053));
#411554=CARTESIAN_POINT('Ctrl Pts',(0.580344486051787,1.39730357656786,
-7.96827451553245));
#411555=CARTESIAN_POINT('Ctrl Pts',(0.759629638709708,1.30851601444969,
-7.97936669763146));
#411556=CARTESIAN_POINT('Ctrl Pts',(1.06743714486741,1.07095493849033,-8.00077501195301));
#411557=CARTESIAN_POINT('Ctrl Pts',(1.19483432966657,0.926693877796609,
-8.01091166355043));
#411558=CARTESIAN_POINT('Ctrl Pts',(1.39279680522045,0.591274626156194,
-8.02975333903075));
#411559=CARTESIAN_POINT('Ctrl Pts',(1.45882908968199,0.401698859921977,
-8.04018339667106));
#411560=CARTESIAN_POINT('Ctrl Pts',(1.51267846314344,0.0107967219430277,
-8.06190018211433));
#411561=CARTESIAN_POINT('Ctrl Pts',(1.50118032369557,-0.186481449343415,
-8.07286008051913));
#411562=CARTESIAN_POINT('Ctrl Pts',(1.40445759093839,-0.560043742577229,
-8.09361354125434));
#411563=CARTESIAN_POINT('Ctrl Pts',(1.32225660699352,-0.733333426955382,
-8.10258660563892));
#411564=CARTESIAN_POINT('Ctrl Pts',(1.09230497047696,-1.04710748744377,
-8.12236610503389));
#411565=CARTESIAN_POINT('Ctrl Pts',(0.94399744391964,-1.18254564038123,
-8.13326372514721));
#411566=CARTESIAN_POINT('Ctrl Pts',(0.607842213005839,-1.38490880839251,
-8.15505820034676));
#411567=CARTESIAN_POINT('Ctrl Pts',(0.424285848828745,-1.45170255815611,
-8.16574494197373));
#411568=CARTESIAN_POINT('Ctrl Pts',(0.0422983906788046,-1.51179188388456,
-8.18579247005979));
#411569=CARTESIAN_POINT('Ctrl Pts',(-0.152473772750104,-1.50467891416419,
-8.19470592797397));
#411570=CARTESIAN_POINT('Ctrl Pts',(-0.534175449206377,-1.41568829505058,
-8.21554252008703));
#411571=CARTESIAN_POINT('Ctrl Pts',(-0.716870672388642,-1.33251813997508,
-8.22664273019612));
#411572=CARTESIAN_POINT('Ctrl Pts',(-1.03311840696601,-1.10419976822846,
-8.24820038341315));
#411573=CARTESIAN_POINT('Ctrl Pts',(-1.16539340622638,-0.963572107969621,
-8.2584707911784));
#411574=CARTESIAN_POINT('Ctrl Pts',(-1.37461328749515,-0.632811755228003,
-8.27772467498541));
#411575=CARTESIAN_POINT('Ctrl Pts',(-1.446678866683,-0.444037130716313,
-8.28783127051582));
#411576=CARTESIAN_POINT('Ctrl Pts',(-1.51185690464234,-0.0530351822067093,
-8.30955360098858));
#411577=CARTESIAN_POINT('Ctrl Pts',(-1.50581899066547,0.145037362305904,
-8.32055763123928));
#411578=CARTESIAN_POINT('Ctrl Pts',(-1.41921969677474,0.521437507459838,
-8.34146875041449));
#411579=CARTESIAN_POINT('Ctrl Pts',(-1.34187002821176,0.696742341984953,
-8.35062653544363));
#411580=CARTESIAN_POINT('Ctrl Pts',(-1.12078621757607,1.01655997572849,
-8.37014725840183));
#411581=CARTESIAN_POINT('Ctrl Pts',(-0.97629141006827,1.15602332206968,
-8.38097324991224));
#411582=CARTESIAN_POINT('Ctrl Pts',(-0.645444276829998,1.36786188068275,
-8.4027755444378));
#411583=CARTESIAN_POINT('Ctrl Pts',(-0.463276097361062,1.43980272374935,
-8.41353847181083));
#411584=CARTESIAN_POINT('Ctrl Pts',(-0.182373624965341,1.49168715610955,
-8.42849463254753));
#411585=CARTESIAN_POINT('Ctrl Pts',(-0.0911831684366718,1.50000000000006,
-8.43311294776313));
#411586=CARTESIAN_POINT('Ctrl Pts',(0.,1.50000000000006,-8.4375));
#411587=CARTESIAN_POINT('Ctrl Pts',(3.84067777581265E-14,1.50000000000006,
-8.49999999999998));
#411588=CARTESIAN_POINT('Ctrl Pts',(-0.172932034887872,1.50000000000006,
-8.49167980359215));
#411589=CARTESIAN_POINT('Ctrl Pts',(-0.344713320132888,1.47009849013323,
-8.48258437515609));
#411590=CARTESIAN_POINT('Ctrl Pts',(-0.693324755588895,1.34469310157241,
-8.46232831663192));
#411591=CARTESIAN_POINT('Ctrl Pts',(-0.863935655426715,1.2419804931837,
-8.45126666787545));
#411592=CARTESIAN_POINT('Ctrl Pts',(-1.1554673236908,0.976580224102157,
-8.42986811424961));
#411593=CARTESIAN_POINT('Ctrl Pts',(-1.27357449666595,0.816581108131254,
-8.42036561711846));
#411594=CARTESIAN_POINT('Ctrl Pts',(-1.43917631272028,0.46443648140315,
-8.40080202674468));
#411595=CARTESIAN_POINT('Ctrl Pts',(-1.48676957695217,0.27645348818368,
-8.39035852712137));
#411596=CARTESIAN_POINT('Ctrl Pts',(-1.50887809365703,-0.114736495199806,
-8.36862575026674));
#411597=CARTESIAN_POINT('Ctrl Pts',(-1.48022027472746,-0.314385601088563,
-8.35753413327291));
#411598=CARTESIAN_POINT('Ctrl Pts',(-1.34912750600613,-0.683040129192743,
-8.33705332615602));
#411599=CARTESIAN_POINT('Ctrl Pts',(-1.25099477475441,-0.849530229743552,
-8.32825711889268));
#411600=CARTESIAN_POINT('Ctrl Pts',(-0.995486464685214,-1.1387680659669,
-8.30792958525325));
#411601=CARTESIAN_POINT('Ctrl Pts',(-0.839701779031076,-1.25804455982313,
-8.29712115512963));
#411602=CARTESIAN_POINT('Ctrl Pts',(-0.487346278273407,-1.43248760100607,
-8.27532280316236));
#411603=CARTESIAN_POINT('Ctrl Pts',(-0.293374043358508,-1.48441277650396,
-8.26454794367269));
#411604=CARTESIAN_POINT('Ctrl Pts',(0.0946013444325994,-1.50900837485635,
-8.245198258059));
#411605=CARTESIAN_POINT('Ctrl Pts',(0.284683234072073,-1.48493563279221,
-8.23588471686996));
#411606=CARTESIAN_POINT('Ctrl Pts',(0.652195181345535,-1.36502991310751,
-8.21487207562688));
#411607=CARTESIAN_POINT('Ctrl Pts',(0.825326317838232,-1.26787247932391,
-8.20384348233351));
#411608=CARTESIAN_POINT('Ctrl Pts',(1.12595209051725,-1.0108371779097,-8.18223974861799));
#411609=CARTESIAN_POINT('Ctrl Pts',(1.24988129516094,-0.852835770679252,
-8.1723797650378));
#411610=CARTESIAN_POINT('Ctrl Pts',(1.42567411081573,-0.50416634860906,
-8.15300924158945));
#411611=CARTESIAN_POINT('Ctrl Pts',(1.47835070174964,-0.3181012037514,-8.14267228909736));
#411612=CARTESIAN_POINT('Ctrl Pts',(1.51148122317105,0.0711973638489506,
-8.12104459089734));
#411613=CARTESIAN_POINT('Ctrl Pts',(1.48869659189733,0.270992937052696,
-8.10994483683046));
#411614=CARTESIAN_POINT('Ctrl Pts',(1.36846410711534,0.643707485225511,
-8.08923847304309));
#411615=CARTESIAN_POINT('Ctrl Pts',(1.27467455985319,0.813791482789087,
-8.0803891560554));
#411616=CARTESIAN_POINT('Ctrl Pts',(1.02702162401374,1.11031780191357,-8.06023710642645));
#411617=CARTESIAN_POINT('Ctrl Pts',(0.875097098422878,1.23360087097202,
-8.04950310458486));
#411618=CARTESIAN_POINT('Ctrl Pts',(0.528358954668116,1.41787727470082,
-8.02770186887279));
#411619=CARTESIAN_POINT('Ctrl Pts',(0.335933026065815,1.47536720299694,
-8.01684682961366));
#411620=CARTESIAN_POINT('Ctrl Pts',(0.0919672531652487,1.49788782491748,
-8.00448344806109));
#411621=CARTESIAN_POINT('Ctrl Pts',(0.0459596310377224,1.50000000000006,
-8.00221123377927));
#411622=CARTESIAN_POINT('Ctrl Pts',(2.16576756528755E-13,1.50000000000006,
-7.99999999999999));
#411623=CARTESIAN_POINT('Origin',(0.,2.5406128344257E-15,14.));
#411624=CARTESIAN_POINT('',(-1.02010322170531E-13,1.50000000000006,-7.43749999999999));
#411625=CARTESIAN_POINT('',(2.53877699052118E-14,1.50000000000006,-7.49999999999998));
#411626=CARTESIAN_POINT('',(-1.8369701987211E-16,1.50000000000006,14.));
#411627=CARTESIAN_POINT('Ctrl Pts',(-2.05148398269017E-13,1.50000000000006,
-7.43749999999999));
#411628=CARTESIAN_POINT('Ctrl Pts',(0.162224039161413,1.50000000000008,
-7.44530500772324));
#411629=CARTESIAN_POINT('Ctrl Pts',(0.323597657554839,1.47368937335663,
-7.45379995029834));
#411630=CARTESIAN_POINT('Ctrl Pts',(0.664507480107818,1.3591217960283,-7.47338441448693));
#411631=CARTESIAN_POINT('Ctrl Pts',(0.837011173684796,1.26023580039065,
-7.48443083552599));
#411632=CARTESIAN_POINT('Ctrl Pts',(1.12872193618759,1.00602573548763,-7.50552716682245));
#411633=CARTESIAN_POINT('Ctrl Pts',(1.24691313573543,0.855148909639087,
-7.51499172724232));
#411634=CARTESIAN_POINT('Ctrl Pts',(1.42478524268694,0.509441695054457,
-7.53419768360813));
#411635=CARTESIAN_POINT('Ctrl Pts',(1.47968565726979,0.316307665969748,
-7.54492735189061));
#411636=CARTESIAN_POINT('Ctrl Pts',(1.51066957180406,-0.0759061424649054,
-7.56671700791476));
#411637=CARTESIAN_POINT('Ctrl Pts',(1.48808662914522,-0.271094338745857,
-7.57756079659703));
#411638=CARTESIAN_POINT('Ctrl Pts',(1.37066665142521,-0.638599056246443,
-7.59797772534707));
#411639=CARTESIAN_POINT('Ctrl Pts',(1.27824481809212,-0.807851530565787,
-7.60677407114223));
#411640=CARTESIAN_POINT('Ctrl Pts',(1.02914229971986,-1.10944963628426,
-7.62713674680424));
#411641=CARTESIAN_POINT('Ctrl Pts',(0.872199458171957,-1.23663507764676,
-7.63822059171557));
#411642=CARTESIAN_POINT('Ctrl Pts',(0.52446883006992,-1.41843093624381,
-7.66000067432161));
#411643=CARTESIAN_POINT('Ctrl Pts',(0.338384687929842,-1.47394983452341,
-7.67049584340353));
#411644=CARTESIAN_POINT('Ctrl Pts',(-0.0482888071570643,-1.51199353587383,
-7.6901564500919));
#411645=CARTESIAN_POINT('Ctrl Pts',(-0.24531930706965,-1.49274497385977,
-7.69950445916845));
#411646=CARTESIAN_POINT('Ctrl Pts',(-0.622225557029383,-1.37907811866395,
-7.7207957822189));
#411647=CARTESIAN_POINT('Ctrl Pts',(-0.79822977627011,-1.28524213549069,
-7.73187034425347));
#411648=CARTESIAN_POINT('Ctrl Pts',(-1.09815687256819,-1.03935888441861,
-7.75313068370978));
#411649=CARTESIAN_POINT('Ctrl Pts',(-1.22098038921394,-0.891839198321561,
-7.76295337787107));
#411650=CARTESIAN_POINT('Ctrl Pts',(-1.40909722008401,-0.551340069333862,
-7.78186999614817));
#411651=CARTESIAN_POINT('Ctrl Pts',(-1.46967403244992,-0.35994893374625,
-7.79250283701415));
#411652=CARTESIAN_POINT('Ctrl Pts',(-1.51231529169579,0.0316923961372904,
-7.81426068867434));
#411653=CARTESIAN_POINT('Ctrl Pts',(-1.49536436400893,0.228023414670104,
-7.82516796748172));
#411654=CARTESIAN_POINT('Ctrl Pts',(-1.38849093405516,0.598657105883578,
-7.84575872810469));
#411655=CARTESIAN_POINT('Ctrl Pts',(-1.30133115946933,0.769954259128152,
-7.85461062704046));
#411656=CARTESIAN_POINT('Ctrl Pts',(-1.06133276307849,1.07880796692926,
-7.87473682493171));
#411657=CARTESIAN_POINT('Ctrl Pts',(-0.907697246875946,1.21091814756384,
-7.88579834439128));
#411658=CARTESIAN_POINT('Ctrl Pts',(-0.564320965471289,1.40312493807049,
-7.90765812094721));
#411659=CARTESIAN_POINT('Ctrl Pts',(-0.379353003860085,1.46401008524602,
-7.91824865023773));
#411660=CARTESIAN_POINT('Ctrl Pts',(-0.125455029964037,1.49606952593216,
-7.93135486222142));
#411661=CARTESIAN_POINT('Ctrl Pts',(-0.0626966099648303,1.50000000000005,
-7.93448350794663));
#411662=CARTESIAN_POINT('Ctrl Pts',(-1.5287771049089E-13,1.50000000000006,
-7.93749999999999));
#411663=CARTESIAN_POINT('Ctrl Pts',(2.16576756528755E-13,1.50000000000006,
-7.99999999999999));
#411664=CARTESIAN_POINT('Ctrl Pts',(-0.143393401176053,1.50000000000006,
-7.99310098176924));
#411665=CARTESIAN_POINT('Ctrl Pts',(-0.28626462010078,1.47944402194318,
-7.98565608765337));
#411666=CARTESIAN_POINT('Ctrl Pts',(-0.612336793066801,1.38328881735224,
-7.96729695501164));
#411667=CARTESIAN_POINT('Ctrl Pts',(-0.787711874190217,1.29149167000941,
-7.95630929672747));
#411668=CARTESIAN_POINT('Ctrl Pts',(-1.09695406145413,1.0426157800093,-7.934517655889));
#411669=CARTESIAN_POINT('Ctrl Pts',(-1.22652279206843,0.886541324990798,
-7.92425229583289));
#411670=CARTESIAN_POINT('Ctrl Pts',(-1.41195258880116,0.541233233830744,
-7.90506851299066));
#411671=CARTESIAN_POINT('Ctrl Pts',(-1.46935403187863,0.357098637279686,
-7.89483881318227));
#411672=CARTESIAN_POINT('Ctrl Pts',(-1.51278524446635,-0.0301414675088971,
-7.87332547402735));
#411673=CARTESIAN_POINT('Ctrl Pts',(-1.49551695163616,-0.229922671981429,
-7.86222651822332));
#411674=CARTESIAN_POINT('Ctrl Pts',(-1.38557150881023,-0.606351438922552,
-7.84131380894881));
#411675=CARTESIAN_POINT('Ctrl Pts',(-1.29586581063539,-0.779870624372747,
-7.83235096665115));
#411676=CARTESIAN_POINT('Ctrl Pts',(-1.05556652732417,-1.08312857069952,
-7.81236573014992));
#411677=CARTESIAN_POINT('Ctrl Pts',(-0.907314389496485,-1.21002224796578,
-7.80170812147452));
#411678=CARTESIAN_POINT('Ctrl Pts',(-0.566036474274492,-1.40326457176951,
-7.77992053779481));
#411679=CARTESIAN_POINT('Ctrl Pts',(-0.375192730029538,-1.46587763026472,
-7.76899931224386));
#411680=CARTESIAN_POINT('Ctrl Pts',(0.0112058963216531,-1.51197211392253,
-7.74912829734184));
#411681=CARTESIAN_POINT('Ctrl Pts',(0.202637680581194,-1.49837613065379,
-7.7402054825656));
#411682=CARTESIAN_POINT('Ctrl Pts',(0.575418572063417,-1.39897726956634,
-7.71950897408711));
#411683=CARTESIAN_POINT('Ctrl Pts',(0.752705296176225,-1.31212531947842,
-7.70856670842715));
#411684=CARTESIAN_POINT('Ctrl Pts',(1.06647525919953,-1.07337091032947,
-7.68683837712175));
#411685=CARTESIAN_POINT('Ctrl Pts',(1.19917431145225,-0.922769058598675,
-7.67627050622317));
#411686=CARTESIAN_POINT('Ctrl Pts',(1.39397565077775,-0.585754321668215,
-7.65753660194471));
#411687=CARTESIAN_POINT('Ctrl Pts',(1.45705662752588,-0.404129060630502,
-7.64745161447954));
#411688=CARTESIAN_POINT('Ctrl Pts',(1.51287229333397,-0.0196343197293993,
-7.62609079554058));
#411689=CARTESIAN_POINT('Ctrl Pts',(1.50226400674775,0.179932317560216,
-7.61500376013561));
#411690=CARTESIAN_POINT('Ctrl Pts',(1.40487393979614,0.560713900206558,
-7.59384922776636));
#411691=CARTESIAN_POINT('Ctrl Pts',(1.32012483986009,0.738466283954311,
-7.5846682503061));
#411692=CARTESIAN_POINT('Ctrl Pts',(1.08868961728264,1.04972226780596,-7.56488731841674));
#411693=CARTESIAN_POINT('Ctrl Pts',(0.944928743537071,1.18078550033665,
-7.55432997480567));
#411694=CARTESIAN_POINT('Ctrl Pts',(0.609202422940334,1.38528831244161,
-7.5324967010052));
#411695=CARTESIAN_POINT('Ctrl Pts',(0.418890910224135,1.45419997592632,
-7.52142612120591));
#411696=CARTESIAN_POINT('Ctrl Pts',(0.147445685704055,1.49456941122877,
-7.50724483354916));
#411697=CARTESIAN_POINT('Ctrl Pts',(0.0736975207194608,1.50000000000006,
-7.50354577361881));
#411698=CARTESIAN_POINT('Ctrl Pts',(5.09592368302956E-14,1.50000000000006,
-7.49999999999998));
#411699=CARTESIAN_POINT('Origin',(0.,2.5406128344257E-15,14.));
#411700=CARTESIAN_POINT('',(-4.77560189507343E-15,1.50000000000006,-6.9375));
#411701=CARTESIAN_POINT('',(-9.18485099360549E-17,1.50000000000006,-6.99999999999998));
#411702=CARTESIAN_POINT('',(-1.8369701987211E-16,1.50000000000006,14.));
#411703=CARTESIAN_POINT('Ctrl Pts',(-2.70616862252382E-15,1.50000000000006,
-6.9375));
#411704=CARTESIAN_POINT('Ctrl Pts',(0.192169407202027,1.50000000000006,
-6.94674575491484));
#411705=CARTESIAN_POINT('Ctrl Pts',(0.382677420613757,1.46307171491065,
-6.95693736168064));
#411706=CARTESIAN_POINT('Ctrl Pts',(0.742699722204964,1.31785219373169,
-6.97829281833044));
#411707=CARTESIAN_POINT('Ctrl Pts',(0.908203259366283,1.20975569530316,
-6.98925829148667));
#411708=CARTESIAN_POINT('Ctrl Pts',(1.18423666452601,0.940064710726509,
-7.01003037112276));
#411709=CARTESIAN_POINT('Ctrl Pts',(1.29369671188414,0.782608851879287,
-7.01902173045118));
#411710=CARTESIAN_POINT('Ctrl Pts',(1.45159619429717,0.42712040202094,-7.03877108877665));
#411711=CARTESIAN_POINT('Ctrl Pts',(1.49537080935378,0.231106803664808,
-7.04966073312977));
#411712=CARTESIAN_POINT('Ctrl Pts',(1.50381985831375,-0.161225965822973,
-7.07145699810131));
#411713=CARTESIAN_POINT('Ctrl Pts',(1.47048939491555,-0.353755446754854,
-7.0821530803753));
#411714=CARTESIAN_POINT('Ctrl Pts',(1.33268963618317,-0.714976358151295,
-7.10222090878621));
#411715=CARTESIAN_POINT('Ctrl Pts',(1.22975401776601,-0.88031848372283,
-7.11112005678171));
#411716=CARTESIAN_POINT('Ctrl Pts',(0.962851266472294,-1.16724498350365,
-7.13193160194008));
#411717=CARTESIAN_POINT('Ctrl Pts',(0.79980901962617,-1.28446099149317,
-7.14303197592083));
#411718=CARTESIAN_POINT('Ctrl Pts',(0.444363004845952,-1.44539102120805,
-7.16460365888367));
#411719=CARTESIAN_POINT('Ctrl Pts',(0.256521262648118,-1.49024580454317,
-7.17488716512267));
#411720=CARTESIAN_POINT('Ctrl Pts',(-0.134304007193784,-1.50727538523723,
-7.19416379859328));
#411721=CARTESIAN_POINT('Ctrl Pts',(-0.333680125512914,-1.47601109531253,
-7.20422055098758));
#411722=CARTESIAN_POINT('Ctrl Pts',(-0.705223902700816,-1.33836110897974,
-7.22592007003365));
#411723=CARTESIAN_POINT('Ctrl Pts',(-0.874170307055552,-1.23465777401047,
-7.23692915589664));
#411724=CARTESIAN_POINT('Ctrl Pts',(-1.15780181295661,-0.972405967335528,
-7.2578601554945));
#411725=CARTESIAN_POINT('Ctrl Pts',(-1.27147903464108,-0.818169802504755,
-7.26704612208311));
#411726=CARTESIAN_POINT('Ctrl Pts',(-1.43913063758303,-0.467394654101727,
-7.28653363032772));
#411727=CARTESIAN_POINT('Ctrl Pts',(-1.48834382299317,-0.27270139551403,
-7.29734992247148));
#411728=CARTESIAN_POINT('Ctrl Pts',(-1.50775766368768,0.119736123770694,
-7.31915200687619));
#411729=CARTESIAN_POINT('Ctrl Pts',(-1.47963375324009,0.313633208613137,
-7.32992406714521));
#411730=CARTESIAN_POINT('Ctrl Pts',(-1.35175556934947,0.677950891998563,
-7.3501639384444));
#411731=CARTESIAN_POINT('Ctrl Pts',(-1.25399669761929,0.845194191670035,
-7.3589780055242));
#411732=CARTESIAN_POINT('Ctrl Pts',(-0.995792057819326,1.13937273054366,
-7.37957250812857));
#411733=CARTESIAN_POINT('Ctrl Pts',(-0.835667372739517,1.2615152013883,
-7.39066935704381));
#411734=CARTESIAN_POINT('Ctrl Pts',(-0.483855828346957,1.43272224383282,
-7.41235164904442));
#411735=CARTESIAN_POINT('Ctrl Pts',(-0.296801282743105,1.48281448701481,
-7.42274276626538));
#411736=CARTESIAN_POINT('Ctrl Pts',(-0.0702489658411354,1.49876759045962,
-7.4340859114568));
#411737=CARTESIAN_POINT('Ctrl Pts',(-0.0351062050691992,1.50000000000005,
-7.43581095192109));
#411738=CARTESIAN_POINT('Ctrl Pts',(-2.03836947321191E-13,1.50000000000006,
-7.43749999999999));
#411739=CARTESIAN_POINT('Ctrl Pts',(5.14172038279526E-14,1.50000000000006,
-7.49999999999998));
#411740=CARTESIAN_POINT('Ctrl Pts',(-0.116196176765652,1.50000000000006,
-7.49440950883878));
#411741=CARTESIAN_POINT('Ctrl Pts',(-0.2322300038428,1.48650197062597,-7.4884518834703));
#411742=CARTESIAN_POINT('Ctrl Pts',(-0.535551554263825,1.41464350471122,
-7.47186225007378));
#411743=CARTESIAN_POINT('Ctrl Pts',(-0.714729433285352,1.33311116898231,
-7.46097676324637));
#411744=CARTESIAN_POINT('Ctrl Pts',(-1.03488686131942,1.10386586919407,
-7.43920525681404));
#411745=CARTESIAN_POINT('Ctrl Pts',(-1.17192391894225,0.957146838268963,
-7.42853652966828));
#411746=CARTESIAN_POINT('Ctrl Pts',(-1.37621483367608,0.626224824630856,
-7.40951530029378));
#411747=CARTESIAN_POINT('Ctrl Pts',(-1.4444387423633,0.446945444846318,
-7.39983030249153));
#411748=CARTESIAN_POINT('Ctrl Pts',(-1.51151136657269,0.0653142775771098,
-7.37862857097657));
#411749=CARTESIAN_POINT('Ctrl Pts',(-1.50698852864842,-0.133866114778471,
-7.36756299362348));
#411750=CARTESIAN_POINT('Ctrl Pts',(-1.42122317854349,-0.518496140675042,
-7.34619465885145));
#411751=CARTESIAN_POINT('Ctrl Pts',(-1.34104949567623,-0.700202904909598,
-7.33673785991857));
#411752=CARTESIAN_POINT('Ctrl Pts',(-1.11771606063643,-1.01866065302193,
-7.31714667645662));
#411753=CARTESIAN_POINT('Ctrl Pts',(-0.978111849779189,-1.15335892026023,
-7.30668834719569));
#411754=CARTESIAN_POINT('Ctrl Pts',(-0.649366617591477,-1.36683379620112,
-7.28494172717246));
#411755=CARTESIAN_POINT('Ctrl Pts',(-0.46174017790655,-1.44108321246924,
-7.27385206209897));
#411756=CARTESIAN_POINT('Ctrl Pts',(-0.0766622937430506,-1.51022042322309,
-7.25340451568241));
#411757=CARTESIAN_POINT('Ctrl Pts',(0.116456016918941,-1.50767431930412,
-7.24461018280988));
#411758=CARTESIAN_POINT('Ctrl Pts',(0.494342973444443,-1.42948992987289,
-7.2242572995418));
#411759=CARTESIAN_POINT('Ctrl Pts',(0.675293422908971,-1.35343442244846,
-7.21343866399876));
#411760=CARTESIAN_POINT('Ctrl Pts',(1.00168332648149,-1.13408805910721,
-7.19164226790414));
#411761=CARTESIAN_POINT('Ctrl Pts',(1.14303552835425,-0.99147254996331,
-7.18087991499999));
#411762=CARTESIAN_POINT('Ctrl Pts',(1.35696120970833,-0.666869061643454,
-7.16157064729252));
#411763=CARTESIAN_POINT('Ctrl Pts',(1.43041383923171,-0.48989658305268,
-7.15221647683633));
#411764=CARTESIAN_POINT('Ctrl Pts',(1.50874884321075,-0.111242738002618,
-7.13118015211132));
#411765=CARTESIAN_POINT('Ctrl Pts',(1.51031929183533,0.0873668471844137,
-7.1201462862676));
#411766=CARTESIAN_POINT('Ctrl Pts',(1.43636261111108,0.475722293543195,
-7.09857098369211));
#411767=CARTESIAN_POINT('Ctrl Pts',(1.36083598674517,0.661474591233649,
-7.08876562440499));
#411768=CARTESIAN_POINT('Ctrl Pts',(1.14563340563647,0.987057425931803,
-7.06936771776336));
#411769=CARTESIAN_POINT('Ctrl Pts',(1.0102402743431,1.1252341506302,-7.05901537034408));
#411770=CARTESIAN_POINT('Ctrl Pts',(0.688647512609778,1.34738325925165,
-7.03737192280824));
#411771=CARTESIAN_POINT('Ctrl Pts',(0.503824987368593,1.42683143991068,
-7.02627275100935));
#411772=CARTESIAN_POINT('Ctrl Pts',(0.207068836892841,1.48927712163816,
-7.01026046179241));
#411773=CARTESIAN_POINT('Ctrl Pts',(0.103562773678466,1.50000000000006,
-7.00498266627175));
#411774=CARTESIAN_POINT('Ctrl Pts',(2.16840434497101E-15,1.50000000000006,
-6.99999999999998));
#411775=CARTESIAN_POINT('Origin',(0.,2.5406128344257E-15,14.));
#411776=CARTESIAN_POINT('',(3.81275791127862E-14,1.50000000000006,-6.43750000000001));
#411777=CARTESIAN_POINT('',(-8.92705129629568E-14,1.50000000000006,-6.49999999999997));
#411778=CARTESIAN_POINT('',(-1.8369701987211E-16,1.50000000000006,14.));
#411779=CARTESIAN_POINT('Ctrl Pts',(7.64388552454446E-14,1.50000000000006,
-6.43750000000001));
#411780=CARTESIAN_POINT('Ctrl Pts',(0.0223909192234641,1.50000000000006,
-6.43857728360342));
#411781=CARTESIAN_POINT('Ctrl Pts',(0.0447986082402546,1.49949865191963,
-6.43966930037949));
#411782=CARTESIAN_POINT('Ctrl Pts',(0.265859390180722,1.48958421860951,
-6.45058049313482));
#411783=CARTESIAN_POINT('Ctrl Pts',(0.460739231284261,1.44126257265004,
-6.46129892180487));
#411784=CARTESIAN_POINT('Ctrl Pts',(0.816561570005715,1.27323910504439,
-6.48308575060318));
#411785=CARTESIAN_POINT('Ctrl Pts',(0.974775881668512,1.1566036373632,-6.49393771432445));
#411786=CARTESIAN_POINT('Ctrl Pts',(1.2353063956038,0.872078159699014,-6.51437598001117));
#411787=CARTESIAN_POINT('Ctrl Pts',(1.3362083087437,0.707846967653049,-6.52317516846374));
#411788=CARTESIAN_POINT('Ctrl Pts',(1.47417508943286,0.341832574128559,
-6.54350930143733));
#411789=CARTESIAN_POINT('Ctrl Pts',(1.50657223000472,0.142363393853101,
-6.55459092256374));
#411790=CARTESIAN_POINT('Ctrl Pts',(1.49151053899438,-0.249870029880412,
-6.57638166832671));
#411791=CARTESIAN_POINT('Ctrl Pts',(1.44718195164507,-0.439000366867817,
-6.58688890927046));
#411792=CARTESIAN_POINT('Ctrl Pts',(1.28803882385816,-0.793305960409002,
-6.60657255335608));
#411793=CARTESIAN_POINT('Ctrl Pts',(1.17354741695466,-0.954555822388696,
-6.61588644642036));
#411794=CARTESIAN_POINT('Ctrl Pts',(0.887764635743559,-1.22512200487875,
-6.63715190418358));
#411795=CARTESIAN_POINT('Ctrl Pts',(0.718825168003851,-1.33129149568386,
-6.6482291606373));
#411796=CARTESIAN_POINT('Ctrl Pts',(0.356301293923391,-1.46945047798051,
-6.66950884816954));
#411797=CARTESIAN_POINT('Ctrl Pts',(0.167199836508386,-1.5027415271631,
-6.679379440583));
#411798=CARTESIAN_POINT('Ctrl Pts',(-0.22180495506119,-1.49677377368313,
-6.69826121327373));
#411799=CARTESIAN_POINT('Ctrl Pts',(-0.417989425653454,-1.45423103388989,
-6.70888188578804));
#411800=CARTESIAN_POINT('Ctrl Pts',(-0.779096298556415,-1.29658665327939,
-6.73063465888362));
#411801=CARTESIAN_POINT('Ctrl Pts',(-0.941094149902954,-1.18426214075912,
-6.74154890948832));
#411802=CARTESIAN_POINT('Ctrl Pts',(-1.20958239972972,-0.907295564462036,
-6.76216007243922));
#411803=CARTESIAN_POINT('Ctrl Pts',(-1.31487261361647,-0.746578398793373,
-6.77102342228929));
#411804=CARTESIAN_POINT('Ctrl Pts',(-1.46362507518425,-0.384817140320505,
-6.79112126998222));
#411805=CARTESIAN_POINT('Ctrl Pts',(-1.50191729668966,-0.185768409758887,
-6.8021795327912));
#411806=CARTESIAN_POINT('Ctrl Pts',(-1.49801122233021,0.207856375514794,
-6.82404757641751));
#411807=CARTESIAN_POINT('Ctrl Pts',(-1.45887389293651,0.398679208278765,
-6.8346488449044));
#411808=CARTESIAN_POINT('Ctrl Pts',(-1.30987828284513,0.756315729510975,
-6.85451754052841));
#411809=CARTESIAN_POINT('Ctrl Pts',(-1.20095467590628,0.919515615594141,
-6.86359447498162));
#411810=CARTESIAN_POINT('Ctrl Pts',(-0.924173665643548,1.19799325378724,
-6.88464659749657));
#411811=CARTESIAN_POINT('Ctrl Pts',(-0.757969455871104,1.30948888087906,
-6.89574020202017));
#411812=CARTESIAN_POINT('Ctrl Pts',(-0.39872030251172,1.45856529901397,
-6.91716559658487));
#411813=CARTESIAN_POINT('Ctrl Pts',(-0.21015490020429,1.49741424319437,
-6.92731709107172));
#411814=CARTESIAN_POINT('Ctrl Pts',(-0.0128951306502747,1.49995844027621,
-6.93687842830057));
#411815=CARTESIAN_POINT('Ctrl Pts',(-0.00644668529117233,1.50000000000006,
-6.93718983370931));
#411816=CARTESIAN_POINT('Ctrl Pts',(0.,1.50000000000006,-6.9375));
#411817=CARTESIAN_POINT('Ctrl Pts',(0.,1.50000000000006,-6.99999999999998));
#411818=CARTESIAN_POINT('Ctrl Pts',(-0.0879059832725243,1.50000000000006,
-6.99577062140783));
#411819=CARTESIAN_POINT('Ctrl Pts',(-0.175831940964182,1.49227389480438,
-6.99132566776287));
#411820=CARTESIAN_POINT('Ctrl Pts',(-0.453702387718148,1.44283121748057,
-6.97658321195666));
#411821=CARTESIAN_POINT('Ctrl Pts',(-0.636225722901142,1.37215593521782,
-6.96583835161314));
#411822=CARTESIAN_POINT('Ctrl Pts',(-0.968405417509316,1.16263860615119,
-6.94403642279729));
#411823=CARTESIAN_POINT('Ctrl Pts',(-1.1138498412067,1.02415656188315,-6.93319200124758));
#411824=CARTESIAN_POINT('Ctrl Pts',(-1.33712258522154,0.70581867676277,
-6.91360706731149));
#411825=CARTESIAN_POINT('Ctrl Pts',(-1.41566700697667,0.531016324411727,
-6.90450090691183));
#411826=CARTESIAN_POINT('Ctrl Pts',(-1.5047766983895,0.155312068231135,
-6.88362844823513));
#411827=CARTESIAN_POINT('Ctrl Pts',(-1.51217018903453,-0.0425775048008003,
-6.87263458306669));
#411828=CARTESIAN_POINT('Ctrl Pts',(-1.44967773118986,-0.434367760739349,
-6.85086845773677));
#411829=CARTESIAN_POINT('Ctrl Pts',(-1.37867283939756,-0.624069013339944,
-6.84066284420873));
#411830=CARTESIAN_POINT('Ctrl Pts',(-1.17127304608703,-0.956393555802605,
-6.82145307970996));
#411831=CARTESIAN_POINT('Ctrl Pts',(-1.03994928531237,-1.09774863442188,
-6.81120823236212));
#411832=CARTESIAN_POINT('Ctrl Pts',(-0.72534010093098,-1.32790780096646,
-6.78967828073932));
#411833=CARTESIAN_POINT('Ctrl Pts',(-0.543302158706279,-1.41219268449493,
-6.77857872939579));
#411834=CARTESIAN_POINT('Ctrl Pts',(-0.162060018073507,-1.50371055676201,
-6.75769404523386));
#411835=CARTESIAN_POINT('Ctrl Pts',(0.0329338251145361,-1.51205838946905,
-6.74875042586349));
#411836=CARTESIAN_POINT('Ctrl Pts',(0.415421593607736,-1.45424864437687,
-6.72874214826915));
#411837=CARTESIAN_POINT('Ctrl Pts',(0.599272213566833,-1.38862246315805,
-6.71807368171384));
#411838=CARTESIAN_POINT('Ctrl Pts',(0.936590590215381,-1.1884214702369,
-6.6962833050582));
#411839=CARTESIAN_POINT('Ctrl Pts',(1.08574482652843,-1.05390894243789,
-6.68537065941216));
#411840=CARTESIAN_POINT('Ctrl Pts',(1.31769575376748,-0.741515702901603,
-6.66553332523502));
#411841=CARTESIAN_POINT('Ctrl Pts',(1.40099501903001,-0.568673068221014,
-6.65659294823457));
#411842=CARTESIAN_POINT('Ctrl Pts',(1.4999833846104,-0.195757297541112,
-6.63587540541902));
#411843=CARTESIAN_POINT('Ctrl Pts',(1.51270083303394,0.00132252290894246,
-6.62492652650512));
#411844=CARTESIAN_POINT('Ctrl Pts',(1.4613485562752,0.392429527145843,-6.60319835960307));
#411845=CARTESIAN_POINT('Ctrl Pts',(1.39652484251627,0.582407371418841,
-6.59267901694039));
#411846=CARTESIAN_POINT('Ctrl Pts',(1.20077481135644,0.91895845751198,-6.57391234789469));
#411847=CARTESIAN_POINT('Ctrl Pts',(1.07439799867235,1.06394985203442,-6.56380450192274));
#411848=CARTESIAN_POINT('Ctrl Pts',(0.768367751834957,1.30338393543321,
-6.54242966804569));
#411849=CARTESIAN_POINT('Ctrl Pts',(0.58980812046137,1.39331623132376,-6.5313405944454));
#411850=CARTESIAN_POINT('Ctrl Pts',(0.268717188983998,1.48190412985531,
-6.51343132484262));
#411851=CARTESIAN_POINT('Ctrl Pts',(0.134539763376071,1.50000000000007,
-6.50647304738347));
#411852=CARTESIAN_POINT('Ctrl Pts',(-1.76178516220205E-13,1.50000000000006,
-6.49999999999997));
#411853=CARTESIAN_POINT('Origin',(0.,2.5406128344257E-15,14.));
#411854=CARTESIAN_POINT('',(1.01826625150654E-13,1.50000000000006,-5.93750000000001));
#411855=CARTESIAN_POINT('',(-7.65307037553822E-14,1.50000000000006,-5.99999999999997));
#411856=CARTESIAN_POINT('',(-1.8369701987211E-16,1.50000000000006,14.));
#411857=CARTESIAN_POINT('Ctrl Pts',(2.0383694732118E-13,1.50000000000006,
-5.93750000000001));
#411858=CARTESIAN_POINT('Ctrl Pts',(0.0510987733573682,1.50000000000006,
-5.93995849087943));
#411859=CARTESIAN_POINT('Ctrl Pts',(0.102250512115221,1.49738908990297,
-5.94249205533837));
#411860=CARTESIAN_POINT('Ctrl Pts',(0.351120582172001,1.47182769766712,
-5.95517586083996));
#411861=CARTESIAN_POINT('Ctrl Pts',(0.542952324057759,1.41235470339066,
-5.96605739744349));
#411862=CARTESIAN_POINT('Ctrl Pts',(0.8876101135387,1.22459778685675,-5.98785522297513));
#411863=CARTESIAN_POINT('Ctrl Pts',(1.03812677018933,1.09990818804658,-5.99856055896165));
#411864=CARTESIAN_POINT('Ctrl Pts',(1.28294801490704,0.800779175428834,
-6.01864866582945));
#411865=CARTESIAN_POINT('Ctrl Pts',(1.37516734553438,0.629380715071977,
-6.02753440471824));
#411866=CARTESIAN_POINT('Ctrl Pts',(1.4914523471381,0.255225392585798,-6.04832081152303));
#411867=CARTESIAN_POINT('Ctrl Pts',(1.51211433236649,0.0554178923829198,
-6.05942122820097));
#411868=CARTESIAN_POINT('Ctrl Pts',(1.47501424209642,-0.333120996333186,
-6.08100672201853));
#411869=CARTESIAN_POINT('Ctrl Pts',(1.42051385648069,-0.518458128546809,
-6.09130322936373));
#411870=CARTESIAN_POINT('Ctrl Pts',(1.2410210843566,-0.865845748277928,
-6.11060254157101));
#411871=CARTESIAN_POINT('Ctrl Pts',(1.11494220537351,-1.02311234989756,
-6.12061043896357));
#411872=CARTESIAN_POINT('Ctrl Pts',(0.811009628192773,-1.27704415020625,
-6.14228706302082));
#411873=CARTESIAN_POINT('Ctrl Pts',(0.637000529064983,-1.37215550622816,
-6.15330106181778));
#411874=CARTESIAN_POINT('Ctrl Pts',(0.268408148724571,-1.48796287055158,
-6.17425184221655));
#411875=CARTESIAN_POINT('Ctrl Pts',(0.078078111214819,-1.5099541291653,
-6.18346696153479));
#411876=CARTESIAN_POINT('Ctrl Pts',(-0.309619763643558,-1.48111078536281,
-6.20292128823044));
#411877=CARTESIAN_POINT('Ctrl Pts',(-0.503022272435722,-1.42706009226701,
-6.21372777891475));
#411878=CARTESIAN_POINT('Ctrl Pts',(-0.853270230066218,-1.24884956416789,
-6.23552938408037));
#411879=CARTESIAN_POINT('Ctrl Pts',(-1.00759611314103,-1.12803237920182,
-6.24631042450745));
#411880=CARTESIAN_POINT('Ctrl Pts',(-1.26011862523612,-0.836013236021564,
-6.26657156240144));
#411881=CARTESIAN_POINT('Ctrl Pts',(-1.35660330600879,-0.668165169819857,
-6.27537971278781));
#411882=CARTESIAN_POINT('Ctrl Pts',(-1.48358411268202,-0.29795776991751,
-6.29594679056016));
#411883=CARTESIAN_POINT('Ctrl Pts',(-1.51001292576806,-0.0982334731576826,
-6.3070425848246));
#411884=CARTESIAN_POINT('Ctrl Pts',(-1.48371466166908,0.292275046451878,
-6.32873750258068));
#411885=CARTESIAN_POINT('Ctrl Pts',(-1.43418576814065,0.479546844896079,
-6.33914149138313));
#411886=CARTESIAN_POINT('Ctrl Pts',(-1.26472362376772,0.830384557303938,
-6.35863247540579));
#411887=CARTESIAN_POINT('Ctrl Pts',(-1.14442804264367,0.989630948410885,
-6.36826176202628));
#411888=CARTESIAN_POINT('Ctrl Pts',(-0.849454429133955,1.25189379400266,
-6.38973876566747));
#411889=CARTESIAN_POINT('Ctrl Pts',(-0.677871610264382,1.35251631573508,
-6.40078911793748));
#411890=CARTESIAN_POINT('Ctrl Pts',(-0.333431466914826,1.47204231443247,
-6.42068116869151));
#411891=CARTESIAN_POINT('Ctrl Pts',(-0.167220233864083,1.50000000000006,
-6.42945461274705));
#411892=CARTESIAN_POINT('Ctrl Pts',(7.42461647718073E-14,1.50000000000006,
-6.43750000000001));
#411893=CARTESIAN_POINT('Ctrl Pts',(-1.78357328906041E-13,1.50000000000006,
-6.49999999999997));
#411894=CARTESIAN_POINT('Ctrl Pts',(-0.0595903002411327,1.50000000000005,
-6.49713296034287));
#411895=CARTESIAN_POINT('Ctrl Pts',(-0.119242125513032,1.49644931569961,
-6.49416433044197));
#411896=CARTESIAN_POINT('Ctrl Pts',(-0.370113691097197,1.46635750255132,
-6.48125838291657));
#411897=CARTESIAN_POINT('Ctrl Pts',(-0.555347452026265,1.40668430766311,
-6.47068873069172));
#411898=CARTESIAN_POINT('Ctrl Pts',(-0.899735077112571,1.21682354738176,
-6.44884546334648));
#411899=CARTESIAN_POINT('Ctrl Pts',(-1.05413164380482,1.08582017118329,
-6.43777807239582));
#411900=CARTESIAN_POINT('Ctrl Pts',(-1.29619584274994,0.778598789967767,
-6.41759782593799));
#411901=CARTESIAN_POINT('Ctrl Pts',(-1.38454342506231,0.607769253882239,
-6.40876495854908));
#411902=CARTESIAN_POINT('Ctrl Pts',(-1.4938179707455,0.237840271712374,
-6.38821334842853));
#411903=CARTESIAN_POINT('Ctrl Pts',(-1.51205448725794,0.0417552688562912,
-6.37731973715875));
#411904=CARTESIAN_POINT('Ctrl Pts',(-1.47206513533382,-0.350046935975517,
-6.35555294800142));
#411905=CARTESIAN_POINT('Ctrl Pts',(-1.41277488246974,-0.541849710410891,
-6.34489723831057));
#411906=CARTESIAN_POINT('Ctrl Pts',(-1.22698498723903,-0.883542857306007,
-6.32591428570529));
#411907=CARTESIAN_POINT('Ctrl Pts',(-1.10522364937168,-1.03182450512569,
-6.31617997248098));
#411908=CARTESIAN_POINT('Ctrl Pts',(-0.807172993588271,-1.27962322772243,
-6.29495670576867));
#411909=CARTESIAN_POINT('Ctrl Pts',(-0.63195745332706,-1.37462575956,-6.28388768493963));
#411910=CARTESIAN_POINT('Ctrl Pts',(-0.255634334161712,-1.49106465969635,
-6.26254741653425));
#411911=CARTESIAN_POINT('Ctrl Pts',(-0.0583387744756356,-1.51168935334255,
-6.25313152985522));
#411912=CARTESIAN_POINT('Ctrl Pts',(0.328834283097292,-1.47609403814029,
-6.23351489868188));
#411913=CARTESIAN_POINT('Ctrl Pts',(0.515155646496236,-1.42182325827318,
-6.22304298624273));
#411914=CARTESIAN_POINT('Ctrl Pts',(0.863853447184978,-1.24245742104462,
-6.20128387111747));
#411915=CARTESIAN_POINT('Ctrl Pts',(1.02154251735958,-1.1164262843335,-6.1901961872827));
#411916=CARTESIAN_POINT('Ctrl Pts',(1.2727472828134,-0.816526860684084,
-6.16977955282384));
#411917=CARTESIAN_POINT('Ctrl Pts',(1.36639478227305,-0.647740995638743,
-6.16098561086889));
#411918=CARTESIAN_POINT('Ctrl Pts',(1.48623755001811,-0.280967317389404,
-6.14060929541059));
#411919=CARTESIAN_POINT('Ctrl Pts',(1.51010841709342,-0.0860643245424332,
-6.12978135136354));
#411920=CARTESIAN_POINT('Ctrl Pts',(1.48180480103135,0.306231837685586,
-6.10798712012865));
#411921=CARTESIAN_POINT('Ctrl Pts',(1.42821715856248,0.499742212899848,
-6.09723654373264));
#411922=CARTESIAN_POINT('Ctrl Pts',(1.24863114595614,0.854688722499666,
-6.07751729319949));
#411923=CARTESIAN_POINT('Ctrl Pts',(1.12439779350244,1.01258611140633,-6.06763688874604));
#411924=CARTESIAN_POINT('Ctrl Pts',(0.823302480797979,1.26918280696206,
-6.04602274777158));
#411925=CARTESIAN_POINT('Ctrl Pts',(0.650045418940008,1.36605055780344,
-6.03499614263965));
#411926=CARTESIAN_POINT('Ctrl Pts',(0.313274881536552,1.4753481073596,-6.015757219561));
#411927=CARTESIAN_POINT('Ctrl Pts',(0.157027605796477,1.50000000000007,
-6.00755499420638));
#411928=CARTESIAN_POINT('Ctrl Pts',(-1.55535306856081E-13,1.50000000000006,
-5.99999999999997));
#411929=CARTESIAN_POINT('Origin',(0.,2.5406128344257E-15,14.));
#411930=CARTESIAN_POINT('',(1.26479606976381E-14,1.50000000000006,-5.4375));
#411931=CARTESIAN_POINT('',(3.43726226250065E-8,1.50000000000006,-5.50000000330749));
#411932=CARTESIAN_POINT('',(-1.8369701987211E-16,1.50000000000006,14.));
#411933=CARTESIAN_POINT('Ctrl Pts',(2.54796184151483E-14,1.50000000000006,
-5.4375));
#411934=CARTESIAN_POINT('Ctrl Pts',(0.0795944837401856,1.50000000000006,
-5.44132949138445));
#411935=CARTESIAN_POINT('Ctrl Pts',(0.15922969186804,1.49366568974591,-5.44533689518454));
#411936=CARTESIAN_POINT('Ctrl Pts',(0.435800272974986,1.44918926665121,
-5.45987885966928));
#411937=CARTESIAN_POINT('Ctrl Pts',(0.625072366798754,1.37816585861796,
-5.47095808997459));
#411938=CARTESIAN_POINT('Ctrl Pts',(0.958079568685715,1.17010572017913,
-5.49275935473552));
#411939=CARTESIAN_POINT('Ctrl Pts',(1.10021566829197,1.03759688973605,-5.50327868186193));
#411940=CARTESIAN_POINT('Ctrl Pts',(1.32847369204001,0.723504427834313,
-5.52298554175827));
#411941=CARTESIAN_POINT('Ctrl Pts',(1.41143431922926,0.544210755578284,
-5.53226606913455));
#411942=CARTESIAN_POINT('Ctrl Pts',(1.5042825817161,0.161904499934741,-5.55350530555919));
#411943=CARTESIAN_POINT('Ctrl Pts',(1.51250349955024,-0.0375323642426384,
-5.56458513134683));
#411944=CARTESIAN_POINT('Ctrl Pts',(1.45226919806415,-0.420916767003066,
-5.58588426483352));
#411945=CARTESIAN_POINT('Ctrl Pts',(1.38717863442111,-0.601616447661832,
-5.59580423815753));
#411946=CARTESIAN_POINT('Ctrl Pts',(1.18866924285327,-0.936265388385543,
-5.61465082962138));
#411947=CARTESIAN_POINT('Ctrl Pts',(1.05426528172485,-1.08536896823951,
-5.62525910932324));
#411948=CARTESIAN_POINT('Ctrl Pts',(0.73797091627172,-1.32043673692573,
-5.64700648931765));
#411949=CARTESIAN_POINT('Ctrl Pts',(0.559928386797814,-1.40521926727854,
-5.65792763479848));
#411950=CARTESIAN_POINT('Ctrl Pts',(0.186138296614603,-1.5005351890038,
-5.67855928338982));
#411951=CARTESIAN_POINT('Ctrl Pts',(-0.00559503723360701,-1.51202380497154,
-5.68743519677188));
#411952=CARTESIAN_POINT('Ctrl Pts',(-0.393461389634301,-1.46133488882452,
-5.70750445080109));
#411953=CARTESIAN_POINT('Ctrl Pts',(-0.585287170187141,-1.39561205665681,
-5.71855930719795));
#411954=CARTESIAN_POINT('Ctrl Pts',(-0.925016032529776,-1.19649970050167,
-5.74043541849045));
#411955=CARTESIAN_POINT('Ctrl Pts',(-1.07118271998264,-1.06763747941812,
-5.75104737266061));
#411956=CARTESIAN_POINT('Ctrl Pts',(-1.30735011096432,-0.760635726307789,
-5.77093780803232));
#411957=CARTESIAN_POINT('Ctrl Pts',(-1.39475081741657,-0.585155686287264,
-5.77999135076184));
#411958=CARTESIAN_POINT('Ctrl Pts',(-1.49886490316819,-0.2066802660096,
-5.80101776299948));
#411959=CARTESIAN_POINT('Ctrl Pts',(-1.51302935444535,-0.00697212379655653,
-5.81211265978909));
#411960=CARTESIAN_POINT('Ctrl Pts',(-1.46382445182473,0.378989125746192,
-5.83355495143036));
#411961=CARTESIAN_POINT('Ctrl Pts',(-1.40378576732709,0.561982200655421,
-5.84372123336976));
#411962=CARTESIAN_POINT('Ctrl Pts',(-1.21447194321652,0.902527345162545,
-5.8626404080646));
#411963=CARTESIAN_POINT('Ctrl Pts',(-1.08430982587707,1.05537707770781,
-5.87298048244842));
#411964=CARTESIAN_POINT('Ctrl Pts',(-0.774204305694343,1.29960365670428,
-5.89468451288344));
#411965=CARTESIAN_POINT('Ctrl Pts',(-0.598071925790781,1.38948781563103,
-5.90565546815504));
#411966=CARTESIAN_POINT('Ctrl Pts',(-0.276132584520466,1.48088242042997,
-5.92368352095599));
#411967=CARTESIAN_POINT('Ctrl Pts',(-0.138285900790439,1.50000000000006,
-5.93084671649612));
#411968=CARTESIAN_POINT('Ctrl Pts',(2.02650396463611E-13,1.50000000000006,
-5.93750000000001));
#411969=CARTESIAN_POINT('Ctrl Pts',(-1.52877710490892E-13,1.50000000000006,
-5.99999999999997));
#411970=CARTESIAN_POINT('Ctrl Pts',(-0.0323929666453449,1.50000000000005,
-5.9984414926656));
#411971=CARTESIAN_POINT('Ctrl Pts',(-0.0648163575003628,1.49895072128399,
-5.99685237491475));
#411972=CARTESIAN_POINT('Ctrl Pts',(-0.295674150388503,1.48395653246627,
-5.98532871893077));
#411973=CARTESIAN_POINT('Ctrl Pts',(-0.489567254683016,1.43173032325572,
-5.97454930456728));
#411974=CARTESIAN_POINT('Ctrl Pts',(-0.841627107281658,1.25675283670217,
-5.95275033127395));
#411975=CARTESIAN_POINT('Ctrl Pts',(-0.997206350427106,1.13725736378339,
-5.94194570275591));
#411976=CARTESIAN_POINT('Ctrl Pts',(-1.25229285749514,0.847625748925076,
-5.92162752482742));
#411977=CARTESIAN_POINT('Ctrl Pts',(-1.35019291269777,0.680944445183578,
-5.91283024695462));
#411978=CARTESIAN_POINT('Ctrl Pts',(-1.48070595156035,0.312069812220314,
-5.89233721178999));
#411979=CARTESIAN_POINT('Ctrl Pts',(-1.5090491438535,0.112408640779034,
-5.8812449244877));
#411980=CARTESIAN_POINT('Ctrl Pts',(-1.48634874747747,-0.278687847272671,
-5.85951734181816));
#411981=CARTESIAN_POINT('Ctrl Pts',(-1.43848179378996,-0.466571689567029,
-5.84907935057959));
#411982=CARTESIAN_POINT('Ctrl Pts',(-1.27233558890935,-0.818532709912457,
-5.8295259605604));
#411983=CARTESIAN_POINT('Ctrl Pts',(-1.1539210474878,-0.978425934983905,
-5.8200062207552));
#411984=CARTESIAN_POINT('Ctrl Pts',(-0.861904234968412,-1.24338603709022,
-5.79859655247592));
#411985=CARTESIAN_POINT('Ctrl Pts',(-0.691155026874305,-1.34580496779026,
-5.78753640707394));
#411986=CARTESIAN_POINT('Ctrl Pts',(-0.32650762138883,-1.47632419313749,
-5.76636676656016));
#411987=CARTESIAN_POINT('Ctrl Pts',(-0.137019981631298,-1.50576570776158,
-5.75675253548884));
#411988=CARTESIAN_POINT('Ctrl Pts',(0.251593498909031,-1.49205864866609,
-5.73767460904724));
#411989=CARTESIAN_POINT('Ctrl Pts',(0.44691574301208,-1.44560713225594,
-5.72698684329599));
#411990=CARTESIAN_POINT('Ctrl Pts',(0.804485093324531,-1.28093116860153,
-5.70520894758419));
#411991=CARTESIAN_POINT('Ctrl Pts',(0.963938915732993,-1.16568062196933,
-5.69433581790351));
#411992=CARTESIAN_POINT('Ctrl Pts',(1.22705706108838,-0.883600522245535,
-5.67384098190704));
#411993=CARTESIAN_POINT('Ctrl Pts',(1.32938548142279,-0.720520643564737,
-5.66502892464246));
#411994=CARTESIAN_POINT('Ctrl Pts',(1.47087362554104,-0.355880128331265,
-5.6447711182406));
#411995=CARTESIAN_POINT('Ctrl Pts',(1.50519202463025,-0.156529588792126,
-5.63369608826621));
#411996=CARTESIAN_POINT('Ctrl Pts',(1.4937598411501,0.236191378066057,-5.61187825677409));
#411997=CARTESIAN_POINT('Ctrl Pts',(1.45111716001254,0.425888946128527,
-5.60133950299284));
#411998=CARTESIAN_POINT('Ctrl Pts',(1.2952852599377,0.781290057897524,-5.58159499678345));
#411999=CARTESIAN_POINT('Ctrl Pts',(1.18262570593498,0.943177834697634,
-5.5723663881755));
#412000=CARTESIAN_POINT('Ctrl Pts',(0.8997847440267,1.21635276615106,-5.55117000351049));
#412001=CARTESIAN_POINT('Ctrl Pts',(0.731723497799739,1.32427458714632,
-5.54008632467039));
#412002=CARTESIAN_POINT('Ctrl Pts',(0.373037218568292,1.46492065660309,
-5.51892218775196));
#412003=CARTESIAN_POINT('Ctrl Pts',(0.187294198304379,1.49999999569822,
-5.50901119643687));
#412004=CARTESIAN_POINT('Ctrl Pts',(3.44525195872247E-8,1.50000000000006,
-5.50000000165758));
#412005=CARTESIAN_POINT('Origin',(0.,2.5406128344257E-15,14.));
#412006=CARTESIAN_POINT('',(-1.28316577175103E-14,1.50000000000006,-4.9375));
#412007=CARTESIAN_POINT('',(5.08673883203602E-14,1.50000000000006,-4.99999999999998));
#412008=CARTESIAN_POINT('',(-1.8369701987211E-16,1.50000000000006,14.));
#412009=CARTESIAN_POINT('Ctrl Pts',(-2.76167977375508E-14,1.50000000000006,
-4.9375));
#412010=CARTESIAN_POINT('Ctrl Pts',(0.109269337069246,1.50000000000006,
-4.94275722343093));
#412011=CARTESIAN_POINT('Ctrl Pts',(0.218442531916599,1.48806306207715,
-4.94834140282602));
#412012=CARTESIAN_POINT('Ctrl Pts',(0.519839210729197,1.4210434978429,-4.96470401185852));
#412013=CARTESIAN_POINT('Ctrl Pts',(0.703550414914408,1.33962857731798,
-4.97580434686111));
#412014=CARTESIAN_POINT('Ctrl Pts',(1.02234269722919,1.11421518287066,-4.99740373087437));
#412015=CARTESIAN_POINT('Ctrl Pts',(1.15609916907398,0.974739148629399,
-5.00771342641097));
#412016=CARTESIAN_POINT('Ctrl Pts',(1.36815812327421,0.64642889660756,-5.02703584682477));
#412017=CARTESIAN_POINT('Ctrl Pts',(1.44187087134556,0.459093108451167,
-5.03699482730827));
#412018=CARTESIAN_POINT('Ctrl Pts',(1.51122419412768,0.0693366424525717,
-5.0586479643082));
#412019=CARTESIAN_POINT('Ctrl Pts',(1.5073042347895,-0.129003083014963,
-5.06966683794528));
#412020=CARTESIAN_POINT('Ctrl Pts',(1.42462434211619,-0.506479220501661,
-5.09063773447232));
#412021=CARTESIAN_POINT('Ctrl Pts',(1.3491296193332,-0.682572342742748,
-5.09988364711283));
#412022=CARTESIAN_POINT('Ctrl Pts',(1.13144981391291,-1.00467588146163,
-5.11930409215418));
#412023=CARTESIAN_POINT('Ctrl Pts',(0.988442453312266,-1.14564911851928,
-5.13010046025069));
#412024=CARTESIAN_POINT('Ctrl Pts',(0.659696086921869,-1.36107394947,-5.1519013002602));
#412025=CARTESIAN_POINT('Ctrl Pts',(0.478096294840362,-1.4349761464713,
-5.16269136313604));
#412026=CARTESIAN_POINT('Ctrl Pts',(0.0992354215259686,-1.50894882765366,
-5.18297411210168));
#412027=CARTESIAN_POINT('Ctrl Pts',(-0.0942526461744661,-1.50926821554021,
-5.19177728212173));
#412028=CARTESIAN_POINT('Ctrl Pts',(-0.478585218942584,-1.43554379017561,
-5.21231639235513));
#412029=CARTESIAN_POINT('Ctrl Pts',(-0.665109437551782,-1.35920826021576,
-5.22341097439494));
#412030=CARTESIAN_POINT('Ctrl Pts',(-0.991027454802751,-1.14224485890758,
-5.24511847345852));
#412031=CARTESIAN_POINT('Ctrl Pts',(-1.12896161876897,-1.00614326332682,
-5.25553543389379));
#412032=CARTESIAN_POINT('Ctrl Pts',(-1.34906238708656,-0.684840480971374,
-5.27505011433453));
#412033=CARTESIAN_POINT('Ctrl Pts',(-1.42739574278363,-0.501534207257007,
-5.28463698848573));
#412034=CARTESIAN_POINT('Ctrl Pts',(-1.50848317223173,-0.115405944629524,
-5.3060885586317));
#412035=CARTESIAN_POINT('Ctrl Pts',(-1.5105810897978,0.0835694927427195,
-5.31714274959683));
#412036=CARTESIAN_POINT('Ctrl Pts',(-1.43902654246891,0.464029024789088,
-5.33827939026607));
#412037=CARTESIAN_POINT('Ctrl Pts',(-1.36873250934293,0.642385562050137,
-5.34782420316381));
#412038=CARTESIAN_POINT('Ctrl Pts',(-1.16062414028608,0.970820501985276,
-5.36696001451442));
#412039=CARTESIAN_POINT('Ctrl Pts',(-1.02186611078168,1.11593292892111,
-5.37766691406986));
#412040=CARTESIAN_POINT('Ctrl Pts',(-0.69920801948096,1.34128499831296,
-5.39945058843091));
#412041=CARTESIAN_POINT('Ctrl Pts',(-0.519309753398982,1.42065610626999,
-5.41031070079215));
#412042=CARTESIAN_POINT('Ctrl Pts',(-0.220948667218012,1.48778609346505,
-5.42653032711053));
#412043=CARTESIAN_POINT('Ctrl Pts',(-0.110530101937365,1.50000000000006,
-5.43218211799108));
#412044=CARTESIAN_POINT('Ctrl Pts',(2.47371567674293E-14,1.50000000000006,
-5.4375));
#412045=CARTESIAN_POINT('Ctrl Pts',(3.445252073021E-8,1.50000000000006,
-5.50000000165758));
#412046=CARTESIAN_POINT('Ctrl Pts',(-0.0030264165990009,1.50000000006957,
-5.4998543914654));
#412047=CARTESIAN_POINT('Ctrl Pts',(-0.00605324838429755,1.49999084073414,
-5.49970850852725));
#412048=CARTESIAN_POINT('Ctrl Pts',(-0.20788471157704,1.49876900874675,
-5.48996394794938));
#412049=CARTESIAN_POINT('Ctrl Pts',(-0.404443727576196,1.45805455571796,
-5.47937604085424));
#412050=CARTESIAN_POINT('Ctrl Pts',(-0.767152755435887,1.30371527062883,
-5.45763799225129));
#412051=CARTESIAN_POINT('Ctrl Pts',(-0.930319052752223,1.19277390477609,
-5.44670594550442));
#412052=CARTESIAN_POINT('Ctrl Pts',(-1.20130239453414,0.918201320588246,
-5.42604123716667));
#412053=CARTESIAN_POINT('Ctrl Pts',(-1.30797008719554,0.758570011130649,
-5.41714277839612));
#412054=CARTESIAN_POINT('Ctrl Pts',(-1.46007803199233,0.398158926653063,
-5.39711994036959));
#412055=CARTESIAN_POINT('Ctrl Pts',(-1.50020986801038,0.199275680323789,
-5.38607087112908));
#412056=CARTESIAN_POINT('Ctrl Pts',(-1.49979656184853,-0.194719759397786,
-5.36418223558899));
#412057=CARTESIAN_POINT('Ctrl Pts',(-1.46229033066513,-0.386041612060154,
-5.35355324377441));
#412058=CARTESIAN_POINT('Ctrl Pts',(-1.31645491820166,-0.744699508638727,
-5.33362780507561));
#412059=CARTESIAN_POINT('Ctrl Pts',(-1.20923768704089,-0.908504467636363,
-5.32460990679846));
#412060=CARTESIAN_POINT('Ctrl Pts',(-0.935251135154752,-1.18939613626271,
-5.30362517632391));
#412061=CARTESIAN_POINT('Ctrl Pts',(-0.769924675502597,-1.30252333730794,
-5.29252848107396));
#412062=CARTESIAN_POINT('Ctrl Pts',(-0.411715710282321,-1.45497215413585,
-5.27105945484296));
#412063=CARTESIAN_POINT('Ctrl Pts',(-0.223336374296281,-1.49552600518349,
-5.26086955395209));
#412064=CARTESIAN_POINT('Ctrl Pts',(0.16632152960155,-1.50394222476273,
-5.24188834543261));
#412065=CARTESIAN_POINT('Ctrl Pts',(0.363977751682049,-1.46869754317824,
-5.23161859956776));
#412066=CARTESIAN_POINT('Ctrl Pts',(0.731417505948437,-1.32417154059065,
-5.20992553496505));
#412067=CARTESIAN_POINT('Ctrl Pts',(0.897974983620369,-1.21739343234583,
-5.19894597602191));
#412068=CARTESIAN_POINT('Ctrl Pts',(1.17631320393585,-0.949946835432454,
-5.17812535001668));
#412069=CARTESIAN_POINT('Ctrl Pts',(1.28705016781589,-0.793474227452975,
-5.16908190152514));
#412070=CARTESIAN_POINT('Ctrl Pts',(1.44792263388295,-0.439409787751528,
-5.14941165487506));
#412071=CARTESIAN_POINT('Ctrl Pts',(1.49335585960036,-0.243781396431966,
-5.13854341091286));
#412072=CARTESIAN_POINT('Ctrl Pts',(1.50513872685418,0.148615868687943,
-5.11674356285065));
#412073=CARTESIAN_POINT('Ctrl Pts',(1.47338673581346,0.34157600081826,-5.10602355551008));
#412074=CARTESIAN_POINT('Ctrl Pts',(1.33860559942787,0.703747047495497,
-5.08590294180578));
#412075=CARTESIAN_POINT('Ctrl Pts',(1.23725759045547,0.869666870875445,
-5.0770368371623));
#412076=CARTESIAN_POINT('Ctrl Pts',(0.973007151132674,1.15882272906179,
-5.05629097480075));
#412077=CARTESIAN_POINT('Ctrl Pts',(0.810841581687545,1.27755206180981,
-5.04519074318227));
#412078=CARTESIAN_POINT('Ctrl Pts',(0.456475916524015,1.4416321264999,-5.02358353759307));
#412079=CARTESIAN_POINT('Ctrl Pts',(0.268859507157415,1.48808922179552,
-5.0132663640194));
#412080=CARTESIAN_POINT('Ctrl Pts',(0.0516984644742341,1.49933241652207,
-5.00250588751722));
#412081=CARTESIAN_POINT('Ctrl Pts',(0.0258378280804302,1.50000000000006,
-5.0012431230831));
#412082=CARTESIAN_POINT('Ctrl Pts',(1.01918473660593E-13,1.50000000000006,
-4.99999999999998));
#412083=CARTESIAN_POINT('Origin',(0.,2.5406128344257E-15,14.));
#412084=CARTESIAN_POINT('',(-1.14750131378106E-13,1.50000000000006,-4.43749999999999));
#412085=CARTESIAN_POINT('',(1.14566434358229E-13,1.50000000000006,-4.49999999999999));
#412086=CARTESIAN_POINT('',(-1.8369701987211E-16,1.50000000000006,14.));
#412087=CARTESIAN_POINT('Ctrl Pts',(-2.29122276707017E-13,1.50000000000006,
-4.43749999999999));
#412088=CARTESIAN_POINT('Ctrl Pts',(0.140686638566558,1.50000000000008,
-4.44426878905398));
#412089=CARTESIAN_POINT('Ctrl Pts',(0.28092139039079,1.48021278852266,-4.4515654814602));
#412090=CARTESIAN_POINT('Ctrl Pts',(0.606578491376407,1.38606342884529,
-4.4698489260277));
#412091=CARTESIAN_POINT('Ctrl Pts',(0.783829808490253,1.29410824334802,
-4.48093124470678));
#412092=CARTESIAN_POINT('Ctrl Pts',(1.0867563390801,1.05130438926325,-4.50225035570753));
#412093=CARTESIAN_POINT('Ctrl Pts',(1.21128345120294,0.904997383834726,
-4.51222236756474));
#412094=CARTESIAN_POINT('Ctrl Pts',(1.40310466101198,0.566412353089952,
-4.53103264705056));
#412095=CARTESIAN_POINT('Ctrl Pts',(1.46572570783402,0.375695574426209,
-4.54162802364299));
#412096=CARTESIAN_POINT('Ctrl Pts',(1.51259258447563,-0.0156520677943056,
-4.56336955932191));
#412097=CARTESIAN_POINT('Ctrl Pts',(1.49769549865608,-0.21235806681055,
-4.57429767037837));
#412098=CARTESIAN_POINT('Ctrl Pts',(1.39465136130354,-0.584106202407536,
-4.5949503445782));
#412099=CARTESIAN_POINT('Ctrl Pts',(1.30937394853824,-0.75615194678466,
-4.60384027060582));
#412100=CARTESIAN_POINT('Ctrl Pts',(1.07266136335201,-1.06758554856354,
-4.62388004355339));
#412101=CARTESIAN_POINT('Ctrl Pts',(0.920248839321891,-1.20144313925951,
-4.634931260943));
#412102=CARTESIAN_POINT('Ctrl Pts',(0.578508805863792,-1.39736135123195,
-4.65681540852361));
#412103=CARTESIAN_POINT('Ctrl Pts',(0.393978543135256,-1.4601670655122,
-4.66743822810306));
#412104=CARTESIAN_POINT('Ctrl Pts',(0.0102969179095393,-1.51246850181074,
-4.68735093657861));
#412105=CARTESIAN_POINT('Ctrl Pts',(-0.185244500910995,-1.50111857634093,
-4.69638150864055));
#412106=CARTESIAN_POINT('Ctrl Pts',(-0.565342644764746,-1.40347038284783,
-4.71738143893251));
#412107=CARTESIAN_POINT('Ctrl Pts',(-0.745759245698529,-1.31650216516527,
-4.72847752051664));
#412108=CARTESIAN_POINT('Ctrl Pts',(-1.05635088702636,-1.08192531971329,
-4.74993689131214));
#412109=CARTESIAN_POINT('Ctrl Pts',(-1.18535113736414,-0.938832127839702,
-4.76011822963568));
#412110=CARTESIAN_POINT('Ctrl Pts',(-1.38679467642429,-0.605229638034621,
-4.77907692225551));
#412111=CARTESIAN_POINT('Ctrl Pts',(-1.45473095668339,-0.416303676317022,
-4.78937201798239));
#412112=CARTESIAN_POINT('Ctrl Pts',(-1.512522389727,-0.0257554426009429,
-4.81106914207773));
#412113=CARTESIAN_POINT('Ctrl Pts',(-1.5029534509004,0.171820870721142,
-4.82204560392896));
#412114=CARTESIAN_POINT('Ctrl Pts',(-1.40981131471766,0.546396466236992,
-4.84285535923539));
#412115=CARTESIAN_POINT('Ctrl Pts',(-1.32933648675551,0.72039554288347,
-4.85188658909633));
#412116=CARTESIAN_POINT('Ctrl Pts',(-1.10253366911848,1.03633053760265,
-4.87157461682318));
#412117=CARTESIAN_POINT('Ctrl Pts',(-0.955569431244047,1.17321305285376,
-4.88244772910499));
#412118=CARTESIAN_POINT('Ctrl Pts',(-0.621271389160603,1.3789624257096,
-4.90424691151096));
#412119=CARTESIAN_POINT('Ctrl Pts',(-0.438192504050617,1.4475898433492,
-4.91496161563439));
#412120=CARTESIAN_POINT('Ctrl Pts',(-0.165262371926965,1.49317620308316,
-4.92935926050907));
#412121=CARTESIAN_POINT('Ctrl Pts',(-0.0826129292005308,1.50000000000006,
-4.93352528359063));
#412122=CARTESIAN_POINT('Ctrl Pts',(-2.54796184151484E-14,1.50000000000006,
-4.9375));
#412123=CARTESIAN_POINT('Ctrl Pts',(1.00544572667616E-13,1.50000000000006,
-4.99999999999998));
#412124=CARTESIAN_POINT('Ctrl Pts',(-0.17292231118257,1.50000000000006,
-4.99168027142414));
#412125=CARTESIAN_POINT('Ctrl Pts',(-0.344744171988474,1.47010316998468,
-4.98258302079129));
#412126=CARTESIAN_POINT('Ctrl Pts',(-0.692778521710343,1.34487169787487,
-4.96235955832998));
#412127=CARTESIAN_POINT('Ctrl Pts',(-0.862832126126676,1.242635998465,-4.95133796993361));
#412128=CARTESIAN_POINT('Ctrl Pts',(-1.14895166932908,0.982845840631448,
-4.93035564371977));
#412129=CARTESIAN_POINT('Ctrl Pts',(-1.2640152602166,0.829650895874937,
-4.92109171643747));
#412130=CARTESIAN_POINT('Ctrl Pts',(-1.43483033665852,0.480430526065497,
-4.90169058478139));
#412131=CARTESIAN_POINT('Ctrl Pts',(-1.48580573172146,0.286200686399114,
-4.89090003813326));
#412132=CARTESIAN_POINT('Ctrl Pts',(-1.50879309595032,-0.106204351893178,
-4.86909975822813));
#412133=CARTESIAN_POINT('Ctrl Pts',(-1.48237539572975,-0.300516866633261,
-4.85830461852035));
#412134=CARTESIAN_POINT('Ctrl Pts',(-1.35772770294869,-0.665827304141286,
-4.83800959421435));
#412135=CARTESIAN_POINT('Ctrl Pts',(-1.26162996716907,-0.833690626640661,
-4.8292087938013));
#412136=CARTESIAN_POINT('Ctrl Pts',(-1.00624462373624,-1.13018499056488,
-4.80868560618301));
#412137=CARTESIAN_POINT('Ctrl Pts',(-0.847091637501807,-1.25390183086628,
-4.79759177566535));
#412138=CARTESIAN_POINT('Ctrl Pts',(-0.496514174446316,-1.42840698812214,
-4.77587724413045));
#412139=CARTESIAN_POINT('Ctrl Pts',(-0.309744342612185,-1.48018614779825,
-4.76545296641562));
#412140=CARTESIAN_POINT('Ctrl Pts',(0.0784150369271338,-1.5108862399228,
-4.74592485922336));
#412141=CARTESIAN_POINT('Ctrl Pts',(0.276247764099956,-1.48749184875031,
-4.73636157460697));
#412142=CARTESIAN_POINT('Ctrl Pts',(0.651372897503971,-1.36549254627417,
-4.71492448869786));
#412143=CARTESIAN_POINT('Ctrl Pts',(0.824984713488039,-1.2681702002274,
-4.70386818780549));
#412144=CARTESIAN_POINT('Ctrl Pts',(1.11926587085391,-1.01654845378523,
-4.68272008606354));
#412145=CARTESIAN_POINT('Ctrl Pts',(1.23890122426214,-0.866727828361343,
-4.67315154602005));
#412146=CARTESIAN_POINT('Ctrl Pts',(1.41999400300323,-0.522644239024955,
-4.65403579105691));
#412147=CARTESIAN_POINT('Ctrl Pts',(1.47668210722216,-0.330038749918022,
-4.64333548610653));
#412148=CARTESIAN_POINT('Ctrl Pts',(1.51132536145765,0.0620328913360232,
-4.62155372825908));
#412149=CARTESIAN_POINT('Ctrl Pts',(1.49050500756459,0.257596930718835,
-4.61068905940448));
#412150=CARTESIAN_POINT('Ctrl Pts',(1.37639368179086,0.626092620808326,
-4.59021707662173));
#412151=CARTESIAN_POINT('Ctrl Pts',(1.28563530462021,0.795984064244105,
-4.58141115564893));
#412152=CARTESIAN_POINT('Ctrl Pts',(1.03939729146344,1.09988249420353,-4.56112240066277));
#412153=CARTESIAN_POINT('Ctrl Pts',(0.883481933791372,1.22863050053394,
-4.55004458601002));
#412154=CARTESIAN_POINT('Ctrl Pts',(0.537092514099401,1.41372193594228,
-4.52823748852338));
#412155=CARTESIAN_POINT('Ctrl Pts',(0.351344087889412,1.470936179403,-4.51771137865998));
#412156=CARTESIAN_POINT('Ctrl Pts',(0.106649080622681,1.49715980908738,
-4.50521005047585));
#412157=CARTESIAN_POINT('Ctrl Pts',(0.0532953547121679,1.50000000000006,
-4.50256417394911));
#412158=CARTESIAN_POINT('Ctrl Pts',(2.29316565736331E-13,1.50000000000006,
-4.49999999999999));
#412159=CARTESIAN_POINT('Origin',(0.,2.5406128344257E-15,14.));
#412160=CARTESIAN_POINT('',(-6.37908945478066E-14,1.50000000000006,-3.9375));
#412161=CARTESIAN_POINT('',(1.26479606976381E-14,1.50000000000006,-3.99999999999998));
#412162=CARTESIAN_POINT('',(-1.8369701987211E-16,1.50000000000006,14.));
#412163=CARTESIAN_POINT('Ctrl Pts',(-1.28994037673635E-13,1.50000000000006,
-3.9375));
#412164=CARTESIAN_POINT('Ctrl Pts',(0.172039702205682,1.50000000000007,
-3.94577726403165));
#412165=CARTESIAN_POINT('Ctrl Pts',(0.343000950453755,1.47040772692418,
-3.95482464850851));
#412166=CARTESIAN_POINT('Ctrl Pts',(0.690459276951828,1.34606876560196,
-3.97499560507322));
#412167=CARTESIAN_POINT('Ctrl Pts',(0.860717259763783,1.24410703881113,
-3.9860194162792));
#412168=CARTESIAN_POINT('Ctrl Pts',(1.14729861126686,0.984775223523742,
-4.00701122951788));
#412169=CARTESIAN_POINT('Ctrl Pts',(1.26261987063918,0.831772866439156,
-4.01629039630894));
#412170=CARTESIAN_POINT('Ctrl Pts',(1.43402053602185,0.482841671967244,
-4.03567546266849));
#412171=CARTESIAN_POINT('Ctrl Pts',(1.48532197293877,0.288699503772824,
-4.04646113867929));
#412172=CARTESIAN_POINT('Ctrl Pts',(1.50897163146507,-0.103695919934746,
-4.06826088444082));
#412173=CARTESIAN_POINT('Ctrl Pts',(1.482870655935,-0.298083792777715,-4.07906021070988));
#412174=CARTESIAN_POINT('Ctrl Pts',(1.35882156308033,-0.663577493177654,
-4.09936541628765));
#412175=CARTESIAN_POINT('Ctrl Pts',(1.26303051316353,-0.831555557395231,
-4.10816451491907));
#412176=CARTESIAN_POINT('Ctrl Pts',(1.00816679456882,-1.12847677588431,
-4.12867446292187));
#412177=CARTESIAN_POINT('Ctrl Pts',(0.84919499381207,-1.25248373891458,
-4.13976763511386));
#412178=CARTESIAN_POINT('Ctrl Pts',(0.498848862514922,-1.42759741543611,
-4.16148794000729));
#412179=CARTESIAN_POINT('Ctrl Pts',(0.31213328570595,-1.47968814757021,
-4.1719182621665));
#412180=CARTESIAN_POINT('Ctrl Pts',(-0.0759035487285916,-1.51100097165255,
-4.19145749373681));
#412181=CARTESIAN_POINT('Ctrl Pts',(-0.273668536656642,-1.48795461836484,
-4.20100147754327));
#412182=CARTESIAN_POINT('Ctrl Pts',(-0.648945994403652,-1.36665261103511,
-4.22242652285112));
#412183=CARTESIAN_POINT('Ctrl Pts',(-0.822760499348426,-1.26961968984822,
-4.23348453604122));
#412184=CARTESIAN_POINT('Ctrl Pts',(-1.11751477203434,-1.01847598257923,
-4.2546421216887));
#412185=CARTESIAN_POINT('Ctrl Pts',(-1.2374164158246,-0.868849150927716,
-4.26423060272624));
#412186=CARTESIAN_POINT('Ctrl Pts',(-1.41910042027154,-0.525064982580511,
-4.28332972318997));
#412187=CARTESIAN_POINT('Ctrl Pts',(-1.47611640453722,-0.332558451995796,
-4.29402453044468));
#412188=CARTESIAN_POINT('Ctrl Pts',(-1.51143200208983,0.0594833347478576,
-4.31580462970822));
#412189=CARTESIAN_POINT('Ctrl Pts',(-1.4909360257503,0.255114728648251,
-4.32667304048046));
#412190=CARTESIAN_POINT('Ctrl Pts',(-1.37743276400524,0.623791612541792,
-4.34715508958566));
#412191=CARTESIAN_POINT('Ctrl Pts',(-1.28697881671843,0.793800719434514,
-4.35596355612815));
#412192=CARTESIAN_POINT('Ctrl Pts',(-1.04126642406067,1.09811948207782,
-4.37623869809415));
#412193=CARTESIAN_POINT('Ctrl Pts',(-0.885540927381995,1.22715291585369,
-4.38731530659574));
#412194=CARTESIAN_POINT('Ctrl Pts',(-0.539400512018695,1.41284710562235,
-4.40912716703271));
#412195=CARTESIAN_POINT('Ctrl Pts',(-0.353715241139075,1.47037175692501,
-4.41965886077391));
#412196=CARTESIAN_POINT('Ctrl Pts',(-0.108237918196274,1.49707454363554,
-4.43221113805595));
#412197=CARTESIAN_POINT('Ctrl Pts',(-0.054089489701269,1.50000000000005,
-4.43489761821339));
#412198=CARTESIAN_POINT('Ctrl Pts',(-2.2931656573634E-13,1.50000000000006,
-4.43749999999999));
#412199=CARTESIAN_POINT('Ctrl Pts',(2.29781471627888E-13,1.50000000000006,
-4.49999999999999));
#412200=CARTESIAN_POINT('Ctrl Pts',(-0.141577531670121,1.50000000000006,
-4.49318834783158));
#412201=CARTESIAN_POINT('Ctrl Pts',(-0.282689337369424,1.47996137754507,
-4.48584247451284));
#412202=CARTESIAN_POINT('Ctrl Pts',(-0.609000595035613,1.38499600125823,
-4.46750488968933));
#412203=CARTESIAN_POINT('Ctrl Pts',(-0.786060544261131,1.29274925770904,
-4.45642367936729));
#412204=CARTESIAN_POINT('Ctrl Pts',(-1.08852416186224,1.04946871871112,
-4.43511359903051));
#412205=CARTESIAN_POINT('Ctrl Pts',(-1.21278787608726,0.902974963502137,
-4.42516527575009));
#412206=CARTESIAN_POINT('Ctrl Pts',(-1.40403857665283,0.564094086222278,
-4.40633856034565));
#412207=CARTESIAN_POINT('Ctrl Pts',(-1.46634512329181,0.373271928921311,
-4.39573732938449));
#412208=CARTESIAN_POINT('Ctrl Pts',(-1.51256093779731,-0.0181239560558907,
-4.37399311355242));
#412209=CARTESIAN_POINT('Ctrl Pts',(-1.49734697663919,-0.214773544814063,
-4.36306813639919));
#412210=CARTESIAN_POINT('Ctrl Pts',(-1.39371254638348,-0.586350644688788,
-4.34242496418393));
#412211=CARTESIAN_POINT('Ctrl Pts',(-1.30814590608173,-0.758280757418019,
-4.33354151154521));
#412212=CARTESIAN_POINT('Ctrl Pts',(-1.07092751429217,-1.06931851797489,
-4.3134883985556));
#412213=CARTESIAN_POINT('Ctrl Pts',(-0.918325738887209,-1.2029081661107,
-4.30243551865386));
#412214=CARTESIAN_POINT('Ctrl Pts',(-0.576331635108706,-1.39825667542624,
-4.28055497218306));
#412215=CARTESIAN_POINT('Ctrl Pts',(-0.391732808216006,-1.46076732220635,
-4.26993705012818));
#412216=CARTESIAN_POINT('Ctrl Pts',(-0.00792746944280439,-1.51249229130345,
-4.25003440245961));
#412217=CARTESIAN_POINT('Ctrl Pts',(0.18767220073635,-1.50082665512782,
-4.24099357967453));
#412218=CARTESIAN_POINT('Ctrl Pts',(0.567647827130084,-1.40253498937952,
-4.2199816697773));
#412219=CARTESIAN_POINT('Ctrl Pts',(0.747892048125426,-1.31528683774872,
-4.20888610588382));
#412220=CARTESIAN_POINT('Ctrl Pts',(1.05805850941218,-1.08025023573789,
-4.18743442055706));
#412221=CARTESIAN_POINT('Ctrl Pts',(1.18681357666561,-0.936976785220399,
-4.17725987142561));
#412222=CARTESIAN_POINT('Ctrl Pts',(1.38772429140754,-0.603093330689266,
-4.15831900975202));
#412223=CARTESIAN_POINT('Ctrl Pts',(1.45536894277558,-0.414066520732329,
-4.14800369559621));
#412224=CARTESIAN_POINT('Ctrl Pts',(1.51255592246496,-0.023461578934196,
-4.12630342105187));
#412225=CARTESIAN_POINT('Ctrl Pts',(1.50269082588817,0.174070211172446,
-4.11532943271261));
#412226=CARTESIAN_POINT('Ctrl Pts',(1.40899932305871,0.548491012942113,
-4.09452827705874));
#412227=CARTESIAN_POINT('Ctrl Pts',(1.32826040088197,0.722381015149212,
-4.08550648569052));
#412228=CARTESIAN_POINT('Ctrl Pts',(1.10097533275185,1.03798614056905,-4.06580441871211));
#412229=CARTESIAN_POINT('Ctrl Pts',(0.953804601754212,1.17464851975854,
-4.05492748641587));
#412230=CARTESIAN_POINT('Ctrl Pts',(0.619220134669781,1.379880816514,-4.03312888660562));
#412231=CARTESIAN_POINT('Ctrl Pts',(0.436067013375301,1.44822782335987,
-4.02241839998083));
#412232=CARTESIAN_POINT('Ctrl Pts',(0.163816553264131,1.49329524616321,
-4.00806787075583));
#412233=CARTESIAN_POINT('Ctrl Pts',(0.0818890695196856,1.50000000000006,
-4.00393988969422));
#412234=CARTESIAN_POINT('Ctrl Pts',(2.54796184151483E-14,1.50000000000006,
-3.99999999999998));
#412235=CARTESIAN_POINT('Origin',(0.,2.5406128344257E-15,14.));
#412236=CARTESIAN_POINT('',(-9.18485099360549E-17,1.50000000000006,-3.4375));
#412237=CARTESIAN_POINT('',(-1.28316577175101E-14,1.50000000000006,-3.49999999999998));
#412238=CARTESIAN_POINT('',(-1.8369701987211E-16,1.50000000000006,14.));
#412239=CARTESIAN_POINT('Ctrl Pts',(0.,1.50000000000006,-3.4375));
#412240=CARTESIAN_POINT('Ctrl Pts',(0.00383837813561547,1.50000000000006,
-3.43768467405416));
#412241=CARTESIAN_POINT('Ctrl Pts',(0.00767739578047216,1.49998526685652,
-3.4378697881307));
#412242=CARTESIAN_POINT('Ctrl Pts',(0.202238742844605,1.49849138480775,
-3.44727212202939));
#412243=CARTESIAN_POINT('Ctrl Pts',(0.390908433348299,1.46066537786935,
-3.45740021916103));
#412244=CARTESIAN_POINT('Ctrl Pts',(0.750766726921418,1.31361521777901,
-3.47879863605226));
#412245=CARTESIAN_POINT('Ctrl Pts',(0.917490048972587,1.20310145349813,
-3.48988994241004));
#412246=CARTESIAN_POINT('Ctrl Pts',(1.19594419717257,0.926078500633437,
-3.51098215588574));
#412247=CARTESIAN_POINT('Ctrl Pts',(1.30589435374069,0.763240789073974,
-3.52009773394034));
#412248=CARTESIAN_POINT('Ctrl Pts',(1.45677965863356,0.406218634455983,
-3.53993229808578));
#412249=CARTESIAN_POINT('Ctrl Pts',(1.49688916537199,0.215700620374207,
-3.55051663220144));
#412250=CARTESIAN_POINT('Ctrl Pts',(1.50287980214477,-0.177688244323054,
-3.57237156912906));
#412251=CARTESIAN_POINT('Ctrl Pts',(1.46568688458079,-0.376828077812292,
-3.58343489316959));
#412252=CARTESIAN_POINT('Ctrl Pts',(1.31767783831337,-0.742513459048994,
-3.60375074768186));
#412253=CARTESIAN_POINT('Ctrl Pts',(1.21077959263397,-0.906431974948015,
-3.61275833899274));
#412254=CARTESIAN_POINT('Ctrl Pts',(0.937317259507124,-1.18777435698962,
-3.63373036779756));
#412255=CARTESIAN_POINT('Ctrl Pts',(0.772156944208706,-1.30120646379647,
-3.64482753902805));
#412256=CARTESIAN_POINT('Ctrl Pts',(0.414146270442482,-1.45428625375279,
-3.66630455198837));
#412257=CARTESIAN_POINT('Ctrl Pts',(0.225803487910649,-1.49515942344655,
-3.67650156416275));
#412258=CARTESIAN_POINT('Ctrl Pts',(-0.163876543756407,-1.5042113469918,
-3.69550149574852));
#412259=CARTESIAN_POINT('Ctrl Pts',(-0.36159342079996,-1.46928677785985,
-3.70575031662912));
#412260=CARTESIAN_POINT('Ctrl Pts',(-0.729298491551781,-1.3253443539406,
-3.72743993575863));
#412261=CARTESIAN_POINT('Ctrl Pts',(-0.896052225884826,-1.21881426941551,
-3.73842204755701));
#412262=CARTESIAN_POINT('Ctrl Pts',(-1.17482162487293,-0.951788713600149,
-3.75925172306973));
#412263=CARTESIAN_POINT('Ctrl Pts',(-1.28579767645339,-0.795499399800528,
-3.76830558889997));
#412264=CARTESIAN_POINT('Ctrl Pts',(-1.44722487940157,-0.441701926218901,
-3.78796100409895));
#412265=CARTESIAN_POINT('Ctrl Pts',(-1.4929675491793,-0.246147090610459,
-3.79882516163276));
#412266=CARTESIAN_POINT('Ctrl Pts',(-1.5053733798314,0.146259061249358,
-3.82062550340274));
#412267=CARTESIAN_POINT('Ctrl Pts',(-1.47391678701098,0.339298227844982,
-3.83134990154694));
#412268=CARTESIAN_POINT('Ctrl Pts',(-1.3396994859131,0.701645977298669,
-3.85148033207215));
#412269=CARTESIAN_POINT('Ctrl Pts',(-1.23864678493202,0.867673758381413,
-3.86034096095132));
#412270=CARTESIAN_POINT('Ctrl Pts',(-0.974891200229205,1.15724378580217,
-3.88107451930982));
#412271=CARTESIAN_POINT('Ctrl Pts',(-0.812890468197538,1.27625439466436,
-3.89217463340994));
#412272=CARTESIAN_POINT('Ctrl Pts',(-0.458729099058795,1.44092061171477,
-3.91378829181207));
#412273=CARTESIAN_POINT('Ctrl Pts',(-0.271156167309856,1.48767615682011,
-3.92411166384038));
#412274=CARTESIAN_POINT('Ctrl Pts',(-0.053221028040331,1.4992925278947,
-3.93491975009161));
#412275=CARTESIAN_POINT('Ctrl Pts',(-0.0265985578625327,1.50000000000006,
-3.93622027628817));
#412276=CARTESIAN_POINT('Ctrl Pts',(-1.27398092075741E-13,1.50000000000006,
-3.9375));
#412277=CARTESIAN_POINT('Ctrl Pts',(2.36963226818432E-14,1.50000000000006,
-3.99999999999998));
#412278=CARTESIAN_POINT('Ctrl Pts',(-0.110052726427567,1.50000000000006,
-3.99470508573098));
#412279=CARTESIAN_POINT('Ctrl Pts',(-0.220003344823943,1.48789131581819,
-3.98907873179852));
#412280=CARTESIAN_POINT('Ctrl Pts',(-0.522031754807368,1.42023516921341,
-3.97266804574226));
#412281=CARTESIAN_POINT('Ctrl Pts',(-0.705588874943954,1.33855147507351,
-3.96156765817816));
#412282=CARTESIAN_POINT('Ctrl Pts',(-1.02399430683489,1.11269274086527,
-3.93997451596569));
#412283=CARTESIAN_POINT('Ctrl Pts',(-1.15752520872903,0.973039871272125,
-3.92967076107529));
#412284=CARTESIAN_POINT('Ctrl Pts',(-1.36915150890351,0.644355439731411,
-3.91035876286249));
#412285=CARTESIAN_POINT('Ctrl Pts',(-1.44261380520885,0.456800911229985,
-3.90037782840163));
#412286=CARTESIAN_POINT('Ctrl Pts',(-1.5113319384233,0.0668534138670467,
-3.87871407854813));
#412287=CARTESIAN_POINT('Ctrl Pts',(-1.50708896300539,-0.131447031997297,
-3.86769738711122));
#412288=CARTESIAN_POINT('Ctrl Pts',(-1.42381150292164,-0.508759949520183,
-3.84673555835995));
#412289=CARTESIAN_POINT('Ctrl Pts',(-1.34803476855501,-0.684732585148491,
-3.83750367012102));
#412290=CARTESIAN_POINT('Ctrl Pts',(-1.12983704425607,-1.00648950719521,
-3.8180679349369));
#412291=CARTESIAN_POINT('Ctrl Pts',(-0.986602540188378,-1.14723428560259,
-3.80726698446885));
#412292=CARTESIAN_POINT('Ctrl Pts',(-0.657534322830927,-1.3621153227703,
-3.78546576478033));
#412293=CARTESIAN_POINT('Ctrl Pts',(-0.47584679406526,-1.43571963639234,
-3.77467975520961));
#412294=CARTESIAN_POINT('Ctrl Pts',(-0.0968522807454996,-1.50910999280203,
-3.75440675217435));
#412295=CARTESIAN_POINT('Ctrl Pts',(0.096687802629267,-1.50912053837361,
-3.74560145421517));
#412296=CARTESIAN_POINT('Ctrl Pts',(0.480915377804278,-1.43476027526918,
-3.72504973352138));
#412297=CARTESIAN_POINT('Ctrl Pts',(0.667285027080797,-1.35813672393646,
-3.71395458760836));
#412298=CARTESIAN_POINT('Ctrl Pts',(0.992808230103471,-1.14069248982998,
-3.69225272758658));
#412299=CARTESIAN_POINT('Ctrl Pts',(1.13050975804057,-1.00439792698175,
-3.6818415996556));
#412300=CARTESIAN_POINT('Ctrl Pts',(1.35016111046359,-0.682700899589308,
-3.66233759049615));
#412301=CARTESIAN_POINT('Ctrl Pts',(1.4282378851341,-0.499171310846436,
-3.65273173949143));
#412302=CARTESIAN_POINT('Ctrl Pts',(1.50867319600023,-0.112836516586951,
-3.6312686953659));
#412303=CARTESIAN_POINT('Ctrl Pts',(1.51043421116519,0.0861081306614081,
-3.62021621496322));
#412304=CARTESIAN_POINT('Ctrl Pts',(1.43825701295304,0.466403501236634,
-3.5990886943757));
#412305=CARTESIAN_POINT('Ctrl Pts',(1.36767430010884,0.644632336067039,
-3.58956247333128));
#412306=CARTESIAN_POINT('Ctrl Pts',(1.15903383410136,0.972718921660573,
-3.57041073796369));
#412307=CARTESIAN_POINT('Ctrl Pts',(1.02003707809547,1.11760539553946,-3.5596986291479));
#412308=CARTESIAN_POINT('Ctrl Pts',(0.697033656120665,1.34241177158974,
-3.53791349820543));
#412309=CARTESIAN_POINT('Ctrl Pts',(0.517036849960877,1.42148070619577,
-3.52705703853668));
#412310=CARTESIAN_POINT('Ctrl Pts',(0.21937372040268,1.48796019164546,-3.51088906216489));
#412311=CARTESIAN_POINT('Ctrl Pts',(0.109739389385378,1.50000000000006,
-3.50527983883351));
#412312=CARTESIAN_POINT('Ctrl Pts',(-2.51534904016637E-14,1.50000000000006,
-3.49999999999998));
#412313=CARTESIAN_POINT('Origin',(0.,2.5406128344257E-15,14.));
#412314=CARTESIAN_POINT('',(1.01826625150656E-13,1.50000000000006,-2.93750000000001));
#412315=CARTESIAN_POINT('',(-1.02010322170531E-13,1.50000000000006,-2.99999999999997));
#412316=CARTESIAN_POINT('',(-1.8369701987211E-16,1.50000000000006,14.));
#412317=CARTESIAN_POINT('Ctrl Pts',(2.03836947321183E-13,1.50000000000006,
-2.93750000000001));
#412318=CARTESIAN_POINT('Ctrl Pts',(0.0324756869089283,1.50000000000006,
-2.93906248721492));
#412319=CARTESIAN_POINT('Ctrl Pts',(0.0649840153771657,1.49894535575732,
-2.940655840571));
#412320=CARTESIAN_POINT('Ctrl Pts',(0.288880046979268,1.48436511741472,
-2.95183305003462));
#412321=CARTESIAN_POINT('Ctrl Pts',(0.476101178240112,1.43530432034879,
-2.96220353083074));
#412322=CARTESIAN_POINT('Ctrl Pts',(0.828652016994215,1.26611675306727,
-2.98386529561559));
#412323=CARTESIAN_POINT('Ctrl Pts',(0.989363137339907,1.14493989035571,
-2.99496353696258));
#412324=CARTESIAN_POINT('Ctrl Pts',(1.24928737459687,0.852181743983836,
-3.0156013183909));
#412325=CARTESIAN_POINT('Ctrl Pts',(1.34806301023252,0.685315955484659,
-3.02442689136197));
#412326=CARTESIAN_POINT('Ctrl Pts',(1.47790784661234,0.321606136235137,
-3.04463299243138));
#412327=CARTESIAN_POINT('Ctrl Pts',(1.50706790262235,0.127969168176114,
-3.055390601768));
#412328=CARTESIAN_POINT('Ctrl Pts',(1.48982890756442,-0.26447209595403,
-3.07719289421967));
#412329=CARTESIAN_POINT('Ctrl Pts',(1.44169067460576,-0.459439433716649,
-3.08802441298426));
#412330=CARTESIAN_POINT('Ctrl Pts',(1.27596769337458,-0.811156292291829,
-3.10756423846066));
#412331=CARTESIAN_POINT('Ctrl Pts',(1.16313112751449,-0.966027961343561,
-3.11670627090622));
#412332=CARTESIAN_POINT('Ctrl Pts',(0.881010866199492,-1.22976870676216,
-3.13760592012457));
#412333=CARTESIAN_POINT('Ctrl Pts',(0.712741931599012,-1.33435652805513,
-3.14860698027336));
#412334=CARTESIAN_POINT('Ctrl Pts',(0.341730513984731,-1.47422035071018,
-3.17034238161089));
#412335=CARTESIAN_POINT('Ctrl Pts',(0.142133268152913,-1.50660749914951,
-3.18047806830456));
#412336=CARTESIAN_POINT('Ctrl Pts',(-0.249056218867613,-1.49149956395815,
-3.1997188461406));
#412337=CARTESIAN_POINT('Ctrl Pts',(-0.437027570806907,-1.44761338497599,
-3.20998168255473));
#412338=CARTESIAN_POINT('Ctrl Pts',(-0.793113212309265,-1.28859010546988,
-3.231531174289));
#412339=CARTESIAN_POINT('Ctrl Pts',(-0.956678639165735,-1.17229153401868,
-3.24263123543145));
#412340=CARTESIAN_POINT('Ctrl Pts',(-1.22518115568791,-0.886717531374876,
-3.26348217996535));
#412341=CARTESIAN_POINT('Ctrl Pts',(-1.32907835748031,-0.721723178031133,
-3.27240426788716));
#412342=CARTESIAN_POINT('Ctrl Pts',(-1.46869612189956,-0.361077840727507,
-3.29244011995959));
#412343=CARTESIAN_POINT('Ctrl Pts',(-1.50297472700881,-0.168813816207088,
-3.30312145465516));
#412344=CARTESIAN_POINT('Ctrl Pts',(-1.49653225858235,0.22346636602509,
-3.32491479811251));
#412345=CARTESIAN_POINT('Ctrl Pts',(-1.45375805612543,0.419704959757398,
-3.33581694220875));
#412346=CARTESIAN_POINT('Ctrl Pts',(-1.29765159028516,0.77604672184972,
-3.35561370676943));
#412347=CARTESIAN_POINT('Ctrl Pts',(-1.18895813516421,0.934096362618708,
-3.36457667956784));
#412348=CARTESIAN_POINT('Ctrl Pts',(-0.914309896105459,1.20513119150952,
-3.38531944437755));
#412349=CARTESIAN_POINT('Ctrl Pts',(-0.749443660648884,1.31401401265434,
-3.39627609763889));
#412350=CARTESIAN_POINT('Ctrl Pts',(-0.387862014064975,1.46205087779341,
-3.41778483786408));
#412351=CARTESIAN_POINT('Ctrl Pts',(-0.194804848327324,1.50000000000006,
-3.4281274473649));
#412352=CARTESIAN_POINT('Ctrl Pts',(-2.08166817117217E-16,1.50000000000006,
-3.4375));
#412353=CARTESIAN_POINT('Ctrl Pts',(-2.5479618415148E-14,1.50000000000006,
-3.49999999999998));
#412354=CARTESIAN_POINT('Ctrl Pts',(-0.0804207493428627,1.50000000000006,
-3.49613075489319));
#412355=CARTESIAN_POINT('Ctrl Pts',(-0.160880446843173,1.49353351058198,
-3.49208001118622));
#412356=CARTESIAN_POINT('Ctrl Pts',(-0.438164433049878,1.44847159565109,
-3.47748745932049));
#412357=CARTESIAN_POINT('Ctrl Pts',(-0.627289115656694,1.37715349031037,
-3.46640713530435));
#412358=CARTESIAN_POINT('Ctrl Pts',(-0.959912447691088,1.1685977213517,
-3.44461057197587));
#412359=CARTESIAN_POINT('Ctrl Pts',(-1.10181977458662,1.03588792780666,
-3.43409666937325));
#412360=CARTESIAN_POINT('Ctrl Pts',(-1.32963155482614,0.721398345008406,
-3.4144002482417));
#412361=CARTESIAN_POINT('Ctrl Pts',(-1.4123404120215,0.541887207449783,
-3.40510484485828));
#412362=CARTESIAN_POINT('Ctrl Pts',(-1.50454901637742,0.159368380791001,
-3.38385379893279));
#412363=CARTESIAN_POINT('Ctrl Pts',(-1.5124346897935,-0.0400480155845899,
-3.37277511024526));
#412364=CARTESIAN_POINT('Ctrl Pts',(-1.45158020500728,-0.423275149142189,
-3.3514847139365));
#412365=CARTESIAN_POINT('Ctrl Pts',(-1.38620666532733,-0.603845409694176,
-3.3415870823456));
#412366=CARTESIAN_POINT('Ctrl Pts',(-1.18717508162013,-0.938159660953878,
-3.32272466383028));
#412367=CARTESIAN_POINT('Ctrl Pts',(-1.05253201765593,-1.08705028686621,
-3.31211079567514));
#412368=CARTESIAN_POINT('Ctrl Pts',(-0.73588505348936,-1.32159586462227,
-3.29036095657084));
#412369=CARTESIAN_POINT('Ctrl Pts',(-0.557737809492486,-1.40608600177566,
-3.2794428950435));
#412370=CARTESIAN_POINT('Ctrl Pts',(-0.183806347653259,-1.50082579247428,
-3.25882044834481));
#412371=CARTESIAN_POINT('Ctrl Pts',(0.00797042321779684,-1.51201637084181,
-3.24995031091303));
#412372=CARTESIAN_POINT('Ctrl Pts',(0.395749055373477,-1.46071256652466,
-3.22986819709913));
#412373=CARTESIAN_POINT('Ctrl Pts',(0.587440997207792,-1.39470222434833,
-3.2188117936315));
#412374=CARTESIAN_POINT('Ctrl Pts',(0.926814016028979,-1.19510294647768,
-3.19693927726519));
#412375=CARTESIAN_POINT('Ctrl Pts',(1.07276611057427,-1.06604139951997,
-3.18633211087127));
#412376=CARTESIAN_POINT('Ctrl Pts',(1.30850996460848,-0.758657436181772,
-3.16645143597967));
#412377=CARTESIAN_POINT('Ctrl Pts',(1.39567389041817,-0.582975167886414,
-3.15738750932697));
#412378=CARTESIAN_POINT('Ctrl Pts',(1.49918814551487,-0.204291668769085,
-3.13634953715379));
#412379=CARTESIAN_POINT('Ctrl Pts',(1.51303434523764,-0.00459367178653105,
-3.12525520398809));
#412380=CARTESIAN_POINT('Ctrl Pts',(1.46323834401043,0.381231522641316,
-3.10382047096433));
#412381=CARTESIAN_POINT('Ctrl Pts',(1.40293011990794,0.564105294316241,
-3.09366081698239));
#412382=CARTESIAN_POINT('Ctrl Pts',(1.21312354373214,0.904337840515582,
-3.0747590088602));
#412383=CARTESIAN_POINT('Ctrl Pts',(1.08273616549221,1.05699100076919,-3.06439897358483));
#412384=CARTESIAN_POINT('Ctrl Pts',(0.772291797635089,1.30073681401173,
-3.04269199493775));
#412385=CARTESIAN_POINT('Ctrl Pts',(0.596054210534769,1.39035061333762,
-3.03172348787145));
#412386=CARTESIAN_POINT('Ctrl Pts',(0.274703075377376,1.48108107196493,
-3.01374218365507));
#412387=CARTESIAN_POINT('Ctrl Pts',(0.137565591228464,1.50000000000008,
-3.00661862759389));
#412388=CARTESIAN_POINT('Ctrl Pts',(-2.01123839804751E-13,1.50000000000006,
-2.99999999999997));
#412389=CARTESIAN_POINT('Origin',(0.,2.5406128344257E-15,14.));
#412390=CARTESIAN_POINT('',(8.90868159430818E-14,1.50000000000006,-2.43750000000001));
#412391=CARTESIAN_POINT('',(-3.83112761326589E-14,1.50000000000006,-2.49999999999998));
#412392=CARTESIAN_POINT('',(-1.8369701987211E-16,1.50000000000006,14.));
#412393=CARTESIAN_POINT('Ctrl Pts',(1.78357328906036E-13,1.50000000000006,
-2.43750000000001));
#412394=CARTESIAN_POINT('Ctrl Pts',(0.0600879399513488,1.50000000000006,
-2.44039098235884));
#412395=CARTESIAN_POINT('Ctrl Pts',(0.120237511888765,1.49638976980839,
-2.44338521415997));
#412396=CARTESIAN_POINT('Ctrl Pts',(0.371594894559314,1.46598534480668,
-2.45632321923343));
#412397=CARTESIAN_POINT('Ctrl Pts',(0.556786599151176,1.40611792381491,
-2.46689624319135));
#412398=CARTESIAN_POINT('Ctrl Pts',(0.90101324791975,1.21588098464547,-2.48874221497345));
#412399=CARTESIAN_POINT('Ctrl Pts',(1.05528840530818,1.0847000191656,-2.49980869765185));
#412400=CARTESIAN_POINT('Ctrl Pts',(1.29702193219735,0.777216808900992,
-2.51998030767211));
#412401=CARTESIAN_POINT('Ctrl Pts',(1.38517914898652,0.606312573661868,
-2.5288159681299));
#412402=CARTESIAN_POINT('Ctrl Pts',(1.49406967424139,0.23627057962875,-2.5493738566873));
#412403=CARTESIAN_POINT('Ctrl Pts',(1.51210070438813,0.040145667640204,
-2.5602696851311));
#412404=CARTESIAN_POINT('Ctrl Pts',(1.47168711793412,-0.351632015056332,
-2.58203511194758));
#412405=CARTESIAN_POINT('Ctrl Pts',(1.41219086138491,-0.543369537820228,
-2.59268719654557));
#412406=CARTESIAN_POINT('Ctrl Pts',(1.22602859424387,-0.884872044443282,
-2.61165955802463));
#412407=CARTESIAN_POINT('Ctrl Pts',(1.10409768497012,-1.03303174243462,
-2.62140773487632));
#412408=CARTESIAN_POINT('Ctrl Pts',(0.805747149264772,-1.28052490725735,
-2.64263694185214));
#412409=CARTESIAN_POINT('Ctrl Pts',(0.63040513309612,-1.37534153192259,
-2.653706883668));
#412410=CARTESIAN_POINT('Ctrl Pts',(0.253988236008872,-1.49133760693743,
-2.67503936326793));
#412411=CARTESIAN_POINT('Ctrl Pts',(0.056735146934851,-1.51174226604393,
-2.68444415491362));
#412412=CARTESIAN_POINT('Ctrl Pts',(-0.330358459802904,-1.47575618930825,
-2.70406781799391));
#412413=CARTESIAN_POINT('Ctrl Pts',(-0.516642541644576,-1.42128629030263,
-2.71454346781048));
#412414=CARTESIAN_POINT('Ctrl Pts',(-0.86518719180043,-1.24153256240151,
-2.73630598921819));
#412415=CARTESIAN_POINT('Ctrl Pts',(-1.02275779116148,-1.11531704960142,
-2.74739309468131));
#412416=CARTESIAN_POINT('Ctrl Pts',(-1.27362754231302,-0.815146322030976,
-2.76780114697707));
#412417=CARTESIAN_POINT('Ctrl Pts',(-1.36707943671908,-0.646286224586017,
-2.77659520974523));
#412418=CARTESIAN_POINT('Ctrl Pts',(-1.48653640943523,-0.279395834257768,
-2.79697800920791));
#412419=CARTESIAN_POINT('Ctrl Pts',(-1.51020235437782,-0.0844468628666044,
-2.80780850761853));
#412420=CARTESIAN_POINT('Ctrl Pts',(-1.48147191155196,0.307837417286106,
-2.82960207873812));
#412421=CARTESIAN_POINT('Ctrl Pts',(-1.42767502471587,0.501288471586699,
-2.8403493595326));
#412422=CARTESIAN_POINT('Ctrl Pts',(-1.25178881578139,0.847990517851818,
-2.8596105843251));
#412423=CARTESIAN_POINT('Ctrl Pts',(-1.1344827645406,0.999519102451551,
-2.86901492538767));
#412424=CARTESIAN_POINT('Ctrl Pts',(-0.844351111619898,1.25531200884321,
-2.89007924955807));
#412425=CARTESIAN_POINT('Ctrl Pts',(-0.672533943798328,1.35515124245936,
-2.90111911894406));
#412426=CARTESIAN_POINT('Ctrl Pts',(-0.329578927356474,1.47269892284544,
-2.92088476321));
#412427=CARTESIAN_POINT('Ctrl Pts',(-0.165248197152967,1.50000000000006,
-2.92954949240754));
#412428=CARTESIAN_POINT('Ctrl Pts',(2.06536177049799E-13,1.50000000000006,
-2.93750000000001));
#412429=CARTESIAN_POINT('Ctrl Pts',(-2.03836947321191E-13,1.50000000000006,
-2.99999999999997));
#412430=CARTESIAN_POINT('Ctrl Pts',(-0.0518260929528506,1.50000000000005,
-2.9975065159402));
#412431=CARTESIAN_POINT('Ctrl Pts',(-0.103705738237255,1.49731424103594,
-2.99493585092696));
#412432=CARTESIAN_POINT('Ctrl Pts',(-0.353266974646312,1.47131413802241,
-2.98220660525825));
#412433=CARTESIAN_POINT('Ctrl Pts',(-0.54501292939842,1.41156100563729,
-2.97132141447598));
#412434=CARTESIAN_POINT('Ctrl Pts',(-0.889373472362353,1.22331342656655,
-2.94952426070914));
#412435=CARTESIAN_POINT('Ctrl Pts',(-1.03968986359049,1.09842604100824,
-2.93882306592093));
#412436=CARTESIAN_POINT('Ctrl Pts',(-1.2841096181562,0.798929079940786,
-2.91874405496679));
#412437=CARTESIAN_POINT('Ctrl Pts',(-1.37610609764512,0.627343402167794,
-2.90985241123149));
#412438=CARTESIAN_POINT('Ctrl Pts',(-1.49183001336424,0.25298485137627,
-2.88905471396529));
#412439=CARTESIAN_POINT('Ctrl Pts',(-1.51219086513934,0.0531774261397621,
-2.87795430145215));
#412440=CARTESIAN_POINT('Ctrl Pts',(-1.47452822492152,-0.335250409489197,
-2.85637497725055));
#412441=CARTESIAN_POINT('Ctrl Pts',(-1.41976968043836,-0.520482757750941,
-2.84608429123601));
#412442=CARTESIAN_POINT('Ctrl Pts',(-1.23975119921595,-0.867687374307577,
-2.82679514587175));
#412443=CARTESIAN_POINT('Ctrl Pts',(-1.11336531714322,-1.02484909043133,
-2.81676545017344));
#412444=CARTESIAN_POINT('Ctrl Pts',(-0.808962734118458,-1.27833699989068,
-2.79507854325084));
#412445=CARTESIAN_POINT('Ctrl Pts',(-0.634830535031274,-1.37315641783766,
-2.7840667311953));
#412446=CARTESIAN_POINT('Ctrl Pts',(-0.266085452798857,-1.48838022607664,
-2.76312481381456));
#412447=CARTESIAN_POINT('Ctrl Pts',(-0.0757192170299246,-1.51007466876446,
-2.75392289443798));
#412448=CARTESIAN_POINT('Ctrl Pts',(0.311937677340601,-1.48062452446617,
-2.73445368384764));
#412449=CARTESIAN_POINT('Ctrl Pts',(0.505256838331555,-1.42627069813305,
-2.72364278286858));
#412450=CARTESIAN_POINT('Ctrl Pts',(0.855200408835475,-1.24752402307782,
-2.70184092956442));
#412451=CARTESIAN_POINT('Ctrl Pts',(1.00931667627001,-1.1264881489645,-2.69106389957601));
#412452=CARTESIAN_POINT('Ctrl Pts',(1.26141201577951,-0.834072016097783,
-2.67081228654133));
#412453=CARTESIAN_POINT('Ctrl Pts',(1.357660476778,-0.666029048452036,-2.66200161380283));
#412454=CARTESIAN_POINT('Ctrl Pts',(1.4840513178019,-0.295600261189045,
-2.64142223673266));
#412455=CARTESIAN_POINT('Ctrl Pts',(1.51016080587006,-0.0958671553656366,
-2.63032595307581));
#412456=CARTESIAN_POINT('Ctrl Pts',(1.48326298845563,0.294540097335906,
-2.60863666125906));
#412457=CARTESIAN_POINT('Ctrl Pts',(1.43345743851258,0.481708341663057,
-2.5982384254631));
#412458=CARTESIAN_POINT('Ctrl Pts',(1.26344156569277,0.832357644120056,
-2.57875790865994));
#412459=CARTESIAN_POINT('Ctrl Pts',(1.14283038815684,0.991495693057255,
-2.56910957232394));
#412460=CARTESIAN_POINT('Ctrl Pts',(0.847362746460884,1.2533054056592,-2.54762138676805));
#412461=CARTESIAN_POINT('Ctrl Pts',(0.675642217353411,1.35362668747019,
-2.53657277668673));
#412462=CARTESIAN_POINT('Ctrl Pts',(0.331809149845769,1.47231630234661,
-2.51673316676667));
#412463=CARTESIAN_POINT('Ctrl Pts',(0.166399292541067,1.50000000000007,
-2.50800588969511));
#412464=CARTESIAN_POINT('Ctrl Pts',(-7.5842110369706E-14,1.50000000000006,
-2.49999999999998));
#412465=CARTESIAN_POINT('Origin',(0.,2.5406128344257E-15,14.));
#412466=CARTESIAN_POINT('',(-9.18485099360549E-17,1.50000000000006,-1.9375));
#412467=CARTESIAN_POINT('',(-9.18485099360549E-17,1.50000000000006,-1.99999999999998));
#412468=CARTESIAN_POINT('',(-1.8369701987211E-16,1.50000000000006,14.));
#412469=CARTESIAN_POINT('Ctrl Pts',(0.,1.50000000000006,-1.9375));
#412470=CARTESIAN_POINT('Ctrl Pts',(0.0884346922698931,1.50000000000006,
-1.94175481611565));
#412471=CARTESIAN_POINT('Ctrl Pts',(0.176887442546984,1.49218068882933,
-1.94622770413565));
#412472=CARTESIAN_POINT('Ctrl Pts',(0.455248451650143,1.4423468729858,-1.96100462709277));
#412473=CARTESIAN_POINT('Ctrl Pts',(0.637715067491748,1.37146729159052,
-1.9717524335016));
#412474=CARTESIAN_POINT('Ctrl Pts',(0.9696808619442,1.16157486684138,-1.99355449036593));
#412475=CARTESIAN_POINT('Ctrl Pts',(1.11497252727397,1.02293403844781,-2.0043959729954));
#412476=CARTESIAN_POINT('Ctrl Pts',(1.33789230088642,0.70435701525361,-2.02397056735937));
#412477=CARTESIAN_POINT('Ctrl Pts',(1.41624395528717,0.529473866680497,
-2.03308478518443));
#412478=CARTESIAN_POINT('Ctrl Pts',(1.50494935985186,0.153657189248088,
-2.05396348948623));
#412479=CARTESIAN_POINT('Ctrl Pts',(1.51212460110494,-0.0442624750681964,
-2.06495902639269));
#412480=CARTESIAN_POINT('Ctrl Pts',(1.44919905003476,-0.435926284301219,
-2.08671812690563));
#412481=CARTESIAN_POINT('Ctrl Pts',(1.37802303447125,-0.625478046433682,
-2.0969075593536));
#412482=CARTESIAN_POINT('Ctrl Pts',(1.17033003825317,-0.957550954397508,
-2.11612444073665));
#412483=CARTESIAN_POINT('Ctrl Pts',(1.03885296706329,-1.09878942465052,
-2.12637342511399));
#412484=CARTESIAN_POINT('Ctrl Pts',(0.723979451729282,-1.32865319096229,
-2.14790788880366));
#412485=CARTESIAN_POINT('Ctrl Pts',(0.541835318178859,-1.41275905719967,
-2.15900757657719));
#412486=CARTESIAN_POINT('Ctrl Pts',(0.160518770808986,-1.5038703194419,
-2.17988454591201));
#412487=CARTESIAN_POINT('Ctrl Pts',(-0.0344392415867986,-1.5120193721805,
-2.18882308733395));
#412488=CARTESIAN_POINT('Ctrl Pts',(-0.416846838764254,-1.45384321412457,
-2.20883768582194));
#412489=CARTESIAN_POINT('Ctrl Pts',(-0.600650674242951,-1.38802936907984,
-2.21950911434194));
#412490=CARTESIAN_POINT('Ctrl Pts',(-0.937783113429846,-1.18748053264542,
-2.24130020739709));
#412491=CARTESIAN_POINT('Ctrl Pts',(-1.08680170895694,-1.05281891773745,
-2.25221046833136));
#412492=CARTESIAN_POINT('Ctrl Pts',(-1.31843158101191,-0.740203475262216,
-2.27203852803761));
#412493=CARTESIAN_POINT('Ctrl Pts',(-1.40155435336872,-0.567289223907575,
-2.28098393200514));
#412494=CARTESIAN_POINT('Ctrl Pts',(-1.50017929656928,-0.194269468680472,
-2.30170725173998));
#412495=CARTESIAN_POINT('Ctrl Pts',(-1.51270123839612,0.00284267445957186,
-2.31265792635887));
#412496=CARTESIAN_POINT('Ctrl Pts',(-1.46094827900459,0.393917806733193,
-2.33438432259629));
#412497=CARTESIAN_POINT('Ctrl Pts',(-1.39593051208723,0.583831626159538,
-2.34488914042747));
#412498=CARTESIAN_POINT('Ctrl Pts',(-1.19982509667869,0.920202086774228,
-2.36366789053141));
#412499=CARTESIAN_POINT('Ctrl Pts',(-1.07328430176859,1.06507678699389,
-2.37378038459347));
#412500=CARTESIAN_POINT('Ctrl Pts',(-0.766968168801068,1.30421123790918,
-2.39516065004883));
#412501=CARTESIAN_POINT('Ctrl Pts',(-0.588291662986361,1.39396025608546,
-2.40625025572567));
#412502=CARTESIAN_POINT('Ctrl Pts',(-0.267616746180307,1.48205285089828,
-2.42412575137661));
#412503=CARTESIAN_POINT('Ctrl Pts',(-0.133985757708595,1.50000000000006,
-2.43105360722661));
#412504=CARTESIAN_POINT('Ctrl Pts',(1.80827575135822E-13,1.50000000000006,
-2.43750000000001));
#412505=CARTESIAN_POINT('Ctrl Pts',(-7.64388552454456E-14,1.50000000000006,
-2.49999999999998));
#412506=CARTESIAN_POINT('Ctrl Pts',(-0.0231921828888836,1.50000000000006,
-2.49888416558048));
#412507=CARTESIAN_POINT('Ctrl Pts',(-0.0464021685713373,1.49946212869069,
-2.49775253375393));
#412508=CARTESIAN_POINT('Ctrl Pts',(-0.268251541006387,1.48915550948133,
-2.48679250586798));
#412509=CARTESIAN_POINT('Ctrl Pts',(-0.463055320247125,1.44052039061579,
-2.47606902914529));
#412510=CARTESIAN_POINT('Ctrl Pts',(-0.818581347624592,1.27193687377749,
-2.45428089971003));
#412511=CARTESIAN_POINT('Ctrl Pts',(-0.976586466450202,1.15507021883168,
-2.44343257891537));
#412512=CARTESIAN_POINT('Ctrl Pts',(-1.23668201868617,0.87013486144992,
-2.42300385478546));
#412513=CARTESIAN_POINT('Ctrl Pts',(-1.33734414935178,0.705709309724037,
-2.41420607276238));
#412514=CARTESIAN_POINT('Ctrl Pts',(-1.47471766045293,0.339464868050829,
-2.39385915933609));
#412515=CARTESIAN_POINT('Ctrl Pts',(-1.50679147360988,0.13997746957944,
-2.38277652608768));
#412516=CARTESIAN_POINT('Ctrl Pts',(-1.49111956561788,-0.252170665171258,
-2.36099051860153));
#412517=CARTESIAN_POINT('Ctrl Pts',(-1.44650782625784,-0.441204057198859,
-2.35048866348889));
#412518=CARTESIAN_POINT('Ctrl Pts',(-1.28680700536982,-0.795324315558441,
-2.33081531580225));
#412519=CARTESIAN_POINT('Ctrl Pts',(-1.17200561889551,-0.956466540493105,
-2.32148629828299));
#412520=CARTESIAN_POINT('Ctrl Pts',(-0.885726973651313,-1.22659071766639,
-2.30020926117582));
#412521=CARTESIAN_POINT('Ctrl Pts',(-0.716640993231907,-1.3324637283606,
-2.28913319118615));
#412522=CARTESIAN_POINT('Ctrl Pts',(-0.353946633413566,-1.47001633807981,
-2.26786214483773));
#412523=CARTESIAN_POINT('Ctrl Pts',(-0.164815750605185,-1.50300220280088,
-2.25801309602039));
#412524=CARTESIAN_POINT('Ctrl Pts',(0.224159970903297,-1.49642314518495,
-2.23911574129319));
#412525=CARTESIAN_POINT('Ctrl Pts',(0.42027929336073,-1.45357120372873,
-2.2284896142849));
#412526=CARTESIAN_POINT('Ctrl Pts',(0.781111913268854,-1.29536887785472,
-2.20673453771315));
#412527=CARTESIAN_POINT('Ctrl Pts',(0.942910806682508,-1.18281136012676,
-2.19582338710957));
#412528=CARTESIAN_POINT('Ctrl Pts',(1.21097606234339,-0.905440080178825,
-2.17522133370689));
#412529=CARTESIAN_POINT('Ctrl Pts',(1.31603285800529,-0.744538088387238,
-2.16636322713255));
#412530=CARTESIAN_POINT('Ctrl Pts',(1.46421523239754,-0.382548700011401,
-2.14625270555612));
#412531=CARTESIAN_POINT('Ctrl Pts',(1.5021951427484,-0.183473494950709,
-2.13519297194164));
#412532=CARTESIAN_POINT('Ctrl Pts',(1.49769664685549,0.21008536290726,-2.11332859094953));
#412533=CARTESIAN_POINT('Ctrl Pts',(1.45828293090147,0.400822100376607,
-2.10273210553457));
#412534=CARTESIAN_POINT('Ctrl Pts',(1.30875056254787,0.758284389247239,
-2.0828730894862));
#412535=CARTESIAN_POINT('Ctrl Pts',(1.1995358429708,0.921381433655664,-2.07378543310742));
#412536=CARTESIAN_POINT('Ctrl Pts',(0.922279745513901,1.19944673044089,
-2.05272190687718));
#412537=CARTESIAN_POINT('Ctrl Pts',(0.755927642276091,1.31066393616686,
-2.04162892075274));
#412538=CARTESIAN_POINT('Ctrl Pts',(0.396504479944567,1.45916553552777,
-2.02021112136562));
#412539=CARTESIAN_POINT('Ctrl Pts',(0.207908921595368,1.49772417893426,
-2.01006623990592));
#412540=CARTESIAN_POINT('Ctrl Pts',(0.0114144356045565,1.4999674356079,
-2.00055008185546));
#412541=CARTESIAN_POINT('Ctrl Pts',(0.00570652334405782,1.50000000000006,
-2.00027455523238));
#412542=CARTESIAN_POINT('Ctrl Pts',(0.,1.50000000000006,-1.99999999999998));
#412543=CARTESIAN_POINT('Origin',(0.,2.5406128344257E-15,14.));
#412544=CARTESIAN_POINT('',(-2.5584277190752E-14,1.50000000000006,-1.4375));
#412545=CARTESIAN_POINT('',(1.01826625150654E-13,1.50000000000006,-1.49999999999999));
#412546=CARTESIAN_POINT('',(-1.8369701987211E-16,1.50000000000006,14.));
#412547=CARTESIAN_POINT('Ctrl Pts',(-4.93702301262999E-14,1.50000000000006,
-1.4375));
#412548=CARTESIAN_POINT('Ctrl Pts',(0.116751179473137,1.50000000000006,
-1.44311719374142));
#412549=CARTESIAN_POINT('Ctrl Pts',(0.233334609588104,1.48637273636851,
-1.44910485173897));
#412550=CARTESIAN_POINT('Ctrl Pts',(0.537138132706308,1.4140448040146,-1.46573071479211));
#412551=CARTESIAN_POINT('Ctrl Pts',(0.716244104631243,1.33230116510943,
-1.47661861152039));
#412552=CARTESIAN_POINT('Ctrl Pts',(1.03615413605409,1.10267614366661,-1.49838876290145));
#412553=CARTESIAN_POINT('Ctrl Pts',(1.17302165631554,0.955800930784408,
-1.50905367156481));
#412554=CARTESIAN_POINT('Ctrl Pts',(1.37693820904,0.624636156461619,-1.52806363279108));
#412555=CARTESIAN_POINT('Ctrl Pts',(1.44495918238456,0.445265642356491,
-1.5377630198691));
#412556=CARTESIAN_POINT('Ctrl Pts',(1.51159087068747,0.0635201654975268,
-1.55897110191681));
#412557=CARTESIAN_POINT('Ctrl Pts',(1.50682949726965,-0.135678810543036,
-1.57003771169684));
#412558=CARTESIAN_POINT('Ctrl Pts',(1.42060545718522,-0.52016035689412,
-1.59139779760524));
#412559=CARTESIAN_POINT('Ctrl Pts',(1.34025132827086,-0.701710520174848,
-1.60084242013051));
#412560=CARTESIAN_POINT('Ctrl Pts',(1.11660007662252,-1.01988768661049,
-1.6204411006157));
#412561=CARTESIAN_POINT('Ctrl Pts',(0.976832004464489,-1.1544465360711,
-1.6309034409411));
#412562=CARTESIAN_POINT('Ctrl Pts',(0.647810048663878,-1.36757561427195,
-1.65265376934258));
#412563=CARTESIAN_POINT('Ctrl Pts',(0.460076169110209,-1.44161857982056,
-1.66374286887695));
#412564=CARTESIAN_POINT('Ctrl Pts',(0.074925950513314,-1.51030351218679,
-1.68418133219702));
#412565=CARTESIAN_POINT('Ctrl Pts',(-0.118156433969195,-1.5075379825504,
-1.69297541567572));
#412566=CARTESIAN_POINT('Ctrl Pts',(-0.495946428459652,-1.42893732519622,
-1.71333519685357));
#412567=CARTESIAN_POINT('Ctrl Pts',(-0.676831290210769,-1.3526691172112,
-1.72415658515518));
#412568=CARTESIAN_POINT('Ctrl Pts',(-1.00298556684726,-1.13293629016934,
-1.74595237974635));
#412569=CARTESIAN_POINT('Ctrl Pts',(-1.14417301262309,-0.990159439007331,
-1.75671128754181));
#412570=CARTESIAN_POINT('Ctrl Pts',(-1.35772687033861,-0.665309528353912,
-1.77600951094095));
#412571=CARTESIAN_POINT('Ctrl Pts',(-1.43097742256505,-0.488249372379978,
-1.78537503486779));
#412572=CARTESIAN_POINT('Ctrl Pts',(-1.50888079237126,-0.10947940505863,
-1.80641781083008));
#412573=CARTESIAN_POINT('Ctrl Pts',(-1.5102177655482,0.0891554783909032,
-1.81745308213284));
#412574=CARTESIAN_POINT('Ctrl Pts',(-1.43580522297629,0.477370605819653,
-1.83902058921221));
#412575=CARTESIAN_POINT('Ctrl Pts',(-1.36009907443075,0.662966271740376,
-1.84881126587498));
#412576=CARTESIAN_POINT('Ctrl Pts',(-1.14458440528513,0.988277507115257,
-1.86821664343363));
#412577=CARTESIAN_POINT('Ctrl Pts',(-1.00902902661727,1.12632385521272,
-1.87857317541112));
#412578=CARTESIAN_POINT('Ctrl Pts',(-0.687159260872402,1.34814616795105,
-1.90022087264525));
#412579=CARTESIAN_POINT('Ctrl Pts',(-0.502227210977496,1.42739777272394,
-1.91131985351021));
#412580=CARTESIAN_POINT('Ctrl Pts',(-0.205936556405633,1.48939438257698,
-1.9272972723263));
#412581=CARTESIAN_POINT('Ctrl Pts',(-0.102994860314799,1.50000000000006,
-1.93254465747268));
#412582=CARTESIAN_POINT('Ctrl Pts',(-6.41847686111419E-16,1.50000000000006,
-1.9375));
#412583=CARTESIAN_POINT('Ctrl Pts',(-7.63278329429795E-16,1.50000000000006,
-1.99999999999998));
#412584=CARTESIAN_POINT('Ctrl Pts',(-0.192917176739438,1.50000000000006,
-1.99071826800649));
#412585=CARTESIAN_POINT('Ctrl Pts',(-0.384148717671948,1.46278348849279,
-1.98048384421722));
#412586=CARTESIAN_POINT('Ctrl Pts',(-0.744615514215288,1.31676651004499,
-1.95908485020326));
#412587=CARTESIAN_POINT('Ctrl Pts',(-0.909938568354587,1.20844650284776,
-1.94812185196357));
#412588=CARTESIAN_POINT('Ctrl Pts',(-1.18557905621631,0.938373943019263,
-1.92735807725724));
#412589=CARTESIAN_POINT('Ctrl Pts',(-1.29482159251507,0.780749871870283,
-1.91837499288161));
#412590=CARTESIAN_POINT('Ctrl Pts',(-1.4522129484349,0.425019177606191,
-1.8986121765336));
#412591=CARTESIAN_POINT('Ctrl Pts',(-1.49570405827205,0.228941258167677,
-1.88771895878702));
#412592=CARTESIAN_POINT('Ctrl Pts',(-1.50358414165862,-0.163377651610241,
-1.86592346379936));
#412593=CARTESIAN_POINT('Ctrl Pts',(-1.46998468639679,-0.355832339875636,
-1.8552315366735));
#412594=CARTESIAN_POINT('Ctrl Pts',(-1.33166952614332,-0.716890331994617,
-1.83517275933356));
#412595=CARTESIAN_POINT('Ctrl Pts',(-1.22846171708624,-0.882133856646464,
-1.82626734034715));
#412596=CARTESIAN_POINT('Ctrl Pts',(-0.961105613395692,-1.16867768044156,
-1.80544461314991));
#412597=CARTESIAN_POINT('Ctrl Pts',(-0.797914674599878,-1.28563405408433,
-1.79434429728958));
#412598=CARTESIAN_POINT('Ctrl Pts',(-0.442286477948419,-1.44602425107628,
-1.77277884445079));
#412599=CARTESIAN_POINT('Ctrl Pts',(-0.25440752314352,-1.49060470774768,
-1.7625011680045));
#412600=CARTESIAN_POINT('Ctrl Pts',(0.136521115123568,-1.50709030388568,
-1.74323467190033));
#412601=CARTESIAN_POINT('Ctrl Pts',(0.335959743335738,-1.47550857771446,
-1.73315581202657));
#412602=CARTESIAN_POINT('Ctrl Pts',(0.707353561594332,-1.33723222712268,
-1.71144610887566));
#412603=CARTESIAN_POINT('Ctrl Pts',(0.876108720190405,-1.23327818046135,
-1.70043926011485));
#412604=CARTESIAN_POINT('Ctrl Pts',(1.15931277117352,-0.970604750688442,
-1.6795171146986));
#412605=CARTESIAN_POINT('Ctrl Pts',(1.27275210847479,-0.816189071901462,
-1.67034383732778));
#412606=CARTESIAN_POINT('Ctrl Pts',(1.43985875024554,-0.465147354053559,
-1.65084151966956));
#412607=CARTESIAN_POINT('Ctrl Pts',(1.48876823392591,-0.270376001889668,
-1.64002088899379));
#412608=CARTESIAN_POINT('Ctrl Pts',(1.50756724114496,0.122063805581502,
-1.61821867746762));
#412609=CARTESIAN_POINT('Ctrl Pts',(1.4791502374132,0.315887913870442,-1.60745067145156));
#412610=CARTESIAN_POINT('Ctrl Pts',(1.35071611931521,0.680034066690072,
-1.58722032962825));
#412611=CARTESIAN_POINT('Ctrl Pts',(1.25267028978167,0.84717060780074,-1.57840327720084));
#412612=CARTESIAN_POINT('Ctrl Pts',(0.993979789467423,1.14094847596908,
-1.55779652836339));
#412613=CARTESIAN_POINT('Ctrl Pts',(0.833688936219203,1.26281854097953,
-1.54669925150715));
#412614=CARTESIAN_POINT('Ctrl Pts',(0.481667483160786,1.43345561613014,
-1.52502269269598));
#412615=CARTESIAN_POINT('Ctrl Pts',(0.294565327051418,1.48325663576675,
-1.51463737435643));
#412616=CARTESIAN_POINT('Ctrl Pts',(0.0687623041536401,1.49881918806375,
-1.50334112823258));
#412617=CARTESIAN_POINT('Ctrl Pts',(0.0343634242159142,1.50000000000006,
-1.50165331101842));
#412618=CARTESIAN_POINT('Ctrl Pts',(2.0383694732118E-13,1.50000000000006,
-1.49999999999999));
#412619=CARTESIAN_POINT('Origin',(0.,2.5406128344257E-15,14.));
#412620=CARTESIAN_POINT('',(-1.02008187126244E-13,1.50000000000006,-0.937499999999992));
#412621=CARTESIAN_POINT('',(7.63841236998029E-14,1.50000000000006,-0.999999999999987));
#412622=CARTESIAN_POINT('',(-1.8369701987211E-16,1.50000000000006,14.));
#412623=CARTESIAN_POINT('Ctrl Pts',(-2.07854566891541E-13,1.50000000000006,
-0.937499999999992));
#412624=CARTESIAN_POINT('Ctrl Pts',(0.143984182832987,1.50000000000008,
-0.944427442226474));
#412625=CARTESIAN_POINT('Ctrl Pts',(0.287436109780675,1.47927426985385,
-0.951904991006021));
#412626=CARTESIAN_POINT('Ctrl Pts',(0.613981995335455,1.38256263179278,
-0.970302371640589));
#412627=CARTESIAN_POINT('Ctrl Pts',(0.789268204116796,1.29054467388821,
-0.981291887678922));
#412628=CARTESIAN_POINT('Ctrl Pts',(1.09815839824932,1.04133076500178,-1.00307598265347));
#412629=CARTESIAN_POINT('Ctrl Pts',(1.22749428546384,0.885176755556808,
-1.01332351358019));
#412630=CARTESIAN_POINT('Ctrl Pts',(1.41253059674625,0.539729966787636,
-1.03251500184514));
#412631=CARTESIAN_POINT('Ctrl Pts',(1.46974075814148,0.355514378153379,
-1.04274920121371));
#412632=CARTESIAN_POINT('Ctrl Pts',(1.51275388252878,-0.0318148201579883,
-1.06426749000879));
#412633=CARTESIAN_POINT('Ctrl Pts',(1.49526116535058,-0.231599490017907,
-1.07536663833434));
#412634=CARTESIAN_POINT('Ctrl Pts',(1.38489535340168,-0.607879061196219,
-1.09627105895536));
#412635=CARTESIAN_POINT('Ctrl Pts',(1.29502325176767,-0.781257261786077,
-1.10522808868728));
#412636=CARTESIAN_POINT('Ctrl Pts',(1.05442509401626,-1.08424333824674,
-1.12522015285099));
#412637=CARTESIAN_POINT('Ctrl Pts',(0.906022693938836,-1.21099293928177,
-1.13588098890472));
#412638=CARTESIAN_POINT('Ctrl Pts',(0.564519249383978,-1.40387549529209,
-1.15766942981969));
#412639=CARTESIAN_POINT('Ctrl Pts',(0.373608740790731,-1.46628204988311,
-1.16858813135228));
#412640=CARTESIAN_POINT('Ctrl Pts',(-0.0128248159912985,-1.51195748147707,
-1.18844918651034));
#412641=CARTESIAN_POINT('Ctrl Pts',(-0.204228069040268,-1.49815846947414,
-1.19737708117877));
#412642=CARTESIAN_POINT('Ctrl Pts',(-0.576910843083501,-1.39836541638178,
-1.21807981875769));
#412643=CARTESIAN_POINT('Ctrl Pts',(-0.754123327422173,-1.31131393576137,
-1.22902405506964));
#412644=CARTESIAN_POINT('Ctrl Pts',(-1.06773753463044,-1.07213603112307,
-1.25075665633349));
#412645=CARTESIAN_POINT('Ctrl Pts',(-1.20024082815659,-0.921356835669098,
-1.26131350912951));
#412646=CARTESIAN_POINT('Ctrl Pts',(-1.39468136007972,-0.584114630158508,
-1.28004918721343));
#412647=CARTESIAN_POINT('Ctrl Pts',(-1.45752703712634,-0.40238829166349,
-1.2901450949076));
#412648=CARTESIAN_POINT('Ctrl Pts',(-1.51289686949854,-0.0178933003594045,
-1.31150592775782));
#412649=CARTESIAN_POINT('Ctrl Pts',(-1.5020561457567,0.1816844768087,-1.32259358204494));
#412650=CARTESIAN_POINT('Ctrl Pts',(-1.40422510707694,0.562316600134008,
-1.34373981111857));
#412651=CARTESIAN_POINT('Ctrl Pts',(-1.3193022688901,0.739919605343474,
-1.35291169569682));
#412652=CARTESIAN_POINT('Ctrl Pts',(-1.08755774812862,1.0508986120432,-1.37269981489221));
#412653=CARTESIAN_POINT('Ctrl Pts',(-0.943639096864894,1.18181973459741,
-1.38326080207832));
#412654=CARTESIAN_POINT('Ctrl Pts',(-0.607649407629921,1.3859735809312,
-1.40509705371465));
#412655=CARTESIAN_POINT('Ctrl Pts',(-0.417237669683396,1.4546784054474,
-1.41616671007568));
#412656=CARTESIAN_POINT('Ctrl Pts',(-0.146295653475665,1.49465386686708,
-1.43031284339225));
#412657=CARTESIAN_POINT('Ctrl Pts',(-0.0731221438195881,1.50000000000006,
-1.43398190921517));
#412658=CARTESIAN_POINT('Ctrl Pts',(-5.09848573616319E-14,1.50000000000006,
-1.4375));
#412659=CARTESIAN_POINT('Ctrl Pts',(2.01557520673745E-13,1.50000000000006,
-1.49999999999999));
#412660=CARTESIAN_POINT('Ctrl Pts',(-0.163076993215546,1.50000000000006,
-1.49215395450569));
#412661=CARTESIAN_POINT('Ctrl Pts',(-0.325284941199979,1.47341187781026,
-1.48361116201977));
#412662=CARTESIAN_POINT('Ctrl Pts',(-0.666774070055783,1.35800653720901,
-1.46397555474166));
#412663=CARTESIAN_POINT('Ctrl Pts',(-0.839084622063507,1.25885117771763,
-1.45293094390141));
#412664=CARTESIAN_POINT('Ctrl Pts',(-1.13035010986776,1.00419423254928,
-1.43184362255317));
#412665=CARTESIAN_POINT('Ctrl Pts',(-1.24829156360079,0.853133852358968,
-1.42239632513096));
#412666=CARTESIAN_POINT('Ctrl Pts',(-1.425604258413,0.507145912590032,-1.40317477292158));
#412667=CARTESIAN_POINT('Ctrl Pts',(-1.4801939064406,0.313921894434058,
-1.39244010524625));
#412668=CARTESIAN_POINT('Ctrl Pts',(-1.51054280030923,-0.0783130896786427,
-1.37064927279555));
#412669=CARTESIAN_POINT('Ctrl Pts',(-1.48765448455202,-0.273434472762779,
-1.35980919595754));
#412670=CARTESIAN_POINT('Ctrl Pts',(-1.36966045789988,-0.640766391251696,
-1.3394018671526));
#412671=CARTESIAN_POINT('Ctrl Pts',(-1.27694880415301,-0.80990821445398,
-1.33060644425));
#412672=CARTESIAN_POINT('Ctrl Pts',(-1.02734853964785,-1.11110493461528,
-1.31023097036481));
#412673=CARTESIAN_POINT('Ctrl Pts',(-0.870228411340921,-1.23801764817459,
-1.29914617151263));
#412674=CARTESIAN_POINT('Ctrl Pts',(-0.522267470058889,-1.41923902210377,
-1.27737096586599));
#412675=CARTESIAN_POINT('Ctrl Pts',(-0.336126458157626,-1.47446270144526,
-1.26688126116247));
#412676=CARTESIAN_POINT('Ctrl Pts',(0.0506655324405109,-1.5119274905271,
-1.24723103425251));
#412677=CARTESIAN_POINT('Ctrl Pts',(0.247758477655687,-1.49235408951537,
-1.23786732828351));
#412678=CARTESIAN_POINT('Ctrl Pts',(0.624527801942727,-1.37803234427684,
-1.21656440168249));
#412679=CARTESIAN_POINT('Ctrl Pts',(0.80034635329346,-1.28392016920687,
-1.2054911006013));
#412680=CARTESIAN_POINT('Ctrl Pts',(1.09983031217248,-1.03758380842166,
-1.1842394952231));
#412681=CARTESIAN_POINT('Ctrl Pts',(1.22240274388499,-0.889884415739311,
-1.17443802309653));
#412682=CARTESIAN_POINT('Ctrl Pts',(1.40997071439767,-0.549103068721887,
-1.15550572604001));
#412683=CARTESIAN_POINT('Ctrl Pts',(1.47024422577187,-0.357614005740911,
-1.14486744476329));
#412684=CARTESIAN_POINT('Ctrl Pts',(1.51225978779453,0.0340669096270831,
-1.12310739390951));
#412685=CARTESIAN_POINT('Ctrl Pts',(1.49500530224573,0.230340624900049,
-1.11220329861657));
#412686=CARTESIAN_POINT('Ctrl Pts',(1.38756521684153,0.600808416508208,
-1.09162175463834));
#412687=CARTESIAN_POINT('Ctrl Pts',(1.30012565076874,0.771995093330025,
-1.08277468305615));
#412688=CARTESIAN_POINT('Ctrl Pts',(1.05964010826565,1.08046460082033,-1.0626357195675));
#412689=CARTESIAN_POINT('Ctrl Pts',(0.905824574968569,1.21231434941454,
-1.05157277325478));
#412690=CARTESIAN_POINT('Ctrl Pts',(0.562208588186646,1.4039687863011,-1.02971680702462));
#412691=CARTESIAN_POINT('Ctrl Pts',(0.377177291438441,1.46456844624561,
-1.01913116072177));
#412692=CARTESIAN_POINT('Ctrl Pts',(0.123991130493491,1.49616075506402,
-1.00607217173987));
#412693=CARTESIAN_POINT('Ctrl Pts',(0.0619646518964964,1.50000000000006,
-1.00298127570437));
#412694=CARTESIAN_POINT('Ctrl Pts',(1.52951944419478E-13,1.50000000000006,
-0.999999999999987));
#412695=CARTESIAN_POINT('Origin',(0.,2.5406128344257E-15,14.));
#412696=CARTESIAN_POINT('',(-2.5584277190752E-14,1.50000000000006,-0.437499999999999));
#412697=CARTESIAN_POINT('',(-9.18485099360549E-17,1.50000000000006,-0.499999999999979));
#412698=CARTESIAN_POINT('',(-1.8369701987211E-16,1.50000000000006,14.));
#412699=CARTESIAN_POINT('Ctrl Pts',(-6.21377949094892E-14,1.50000000000006,
-0.437499999999998));
#412700=CARTESIAN_POINT('Ctrl Pts',(0.173580596425634,1.50000000000006,
-0.44585140033937));
#412701=CARTESIAN_POINT('Ctrl Pts',(0.345993724196958,1.46987362435102,
-0.454983474584967));
#412702=CARTESIAN_POINT('Ctrl Pts',(0.695072954621779,1.34379403305005,
-0.47528076775896));
#412703=CARTESIAN_POINT('Ctrl Pts',(0.865571975060887,1.24084475054896,
-0.486343607996248));
#412704=CARTESIAN_POINT('Ctrl Pts',(1.15671230200722,0.975089906948394,
-0.507733182496353));
#412705=CARTESIAN_POINT('Ctrl Pts',(1.27457179400174,0.815005418983616,
-0.517221921167599));
#412706=CARTESIAN_POINT('Ctrl Pts',(1.43973441003759,0.462712829251458,
-0.536793731708271));
#412707=CARTESIAN_POINT('Ctrl Pts',(1.48710669693086,0.274650118336476,
-0.547241660092437));
#412708=CARTESIAN_POINT('Ctrl Pts',(1.50873745620068,-0.116614669232582,
-0.56897859273516));
#412709=CARTESIAN_POINT('Ctrl Pts',(1.47982573747034,-0.316253690432183,
-0.58006964946847));
#412710=CARTESIAN_POINT('Ctrl Pts',(1.34826529463441,-0.684730366235242,
-0.600540575901972));
#412711=CARTESIAN_POINT('Ctrl Pts',(1.24994476750033,-0.851066300014426,
-0.609336068223602));
#412712=CARTESIAN_POINT('Ctrl Pts',(0.994095986485352,-1.13998606148232,
-0.629671147369168));
#412713=CARTESIAN_POINT('Ctrl Pts',(0.838145624621811,-1.25908547839775,
-0.640482629789217));
#412714=CARTESIAN_POINT('Ctrl Pts',(0.485551981950049,-1.4330965882011,
-0.662280441270788));
#412715=CARTESIAN_POINT('Ctrl Pts',(0.29151619983436,-1.48477858918177,
-0.673051603328882));
#412716=CARTESIAN_POINT('Ctrl Pts',(-0.0964898530872458,-1.50888896974836,
-0.692389286047522));
#412717=CARTESIAN_POINT('Ctrl Pts',(-0.286543981390868,-1.48457803169005,
-0.701714741741183));
#412718=CARTESIAN_POINT('Ctrl Pts',(-0.653931217369355,-1.36420266800585,
-0.722734428475939));
#412719=CARTESIAN_POINT('Ctrl Pts',(-0.826960249159726,-1.2668112528236,
-0.733764608737817));
#412720=CARTESIAN_POINT('Ctrl Pts',(-1.1272064357018,-1.00942186759203,
-0.755359915268406));
#412721=CARTESIAN_POINT('Ctrl Pts',(-1.25089002162263,-0.851336442437078,
-0.765203530975736));
#412722=CARTESIAN_POINT('Ctrl Pts',(-1.42625796427823,-0.502520518591022,
-0.784582193411627));
#412723=CARTESIAN_POINT('Ctrl Pts',(-1.47872436454764,-0.31637284196314,
-0.794923731002064));
#412724=CARTESIAN_POINT('Ctrl Pts',(-1.51139791543748,0.0730104938014621,
-0.816556138544541));
#412725=CARTESIAN_POINT('Ctrl Pts',(-1.4883691825351,0.27280329776716,-0.827655738764857));
#412726=CARTESIAN_POINT('Ctrl Pts',(-1.36768356350131,0.64535123374593,
-0.848352846319232));
#412727=CARTESIAN_POINT('Ctrl Pts',(-1.27371349050755,0.815284648275066,
-0.857198560234187));
#412728=CARTESIAN_POINT('Ctrl Pts',(-1.02573471227558,1.11151062047477,
-0.877357943992418));
#412729=CARTESIAN_POINT('Ctrl Pts',(-0.873648710432303,1.23463054467116,
-0.88809518306211));
#412730=CARTESIAN_POINT('Ctrl Pts',(-0.52667301189673,1.41850422189462,
-0.909896661286518));
#412731=CARTESIAN_POINT('Ctrl Pts',(-0.334179940101096,1.47576515148728,
-0.920748569898953));
#412732=CARTESIAN_POINT('Ctrl Pts',(-0.0907817741771738,1.49794192209733,
-0.933075091022824));
#412733=CARTESIAN_POINT('Ctrl Pts',(-0.0453672191895883,1.50000000000005,
-0.935317268649044));
#412734=CARTESIAN_POINT('Ctrl Pts',(-2.03832677232616E-13,1.50000000000006,
-0.937499999999992));
#412735=CARTESIAN_POINT('Ctrl Pts',(1.46913731180476E-13,1.50000000000006,
-0.999999999999986));
#412736=CARTESIAN_POINT('Ctrl Pts',(-0.131899581151311,1.50000000000006,
-0.993653978443012));
#412737=CARTESIAN_POINT('Ctrl Pts',(-0.263472160605492,1.48260736580286,
-0.986840561034739));
#412738=CARTESIAN_POINT('Ctrl Pts',(-0.582573966398612,1.39637102289311,
-0.969092314275562));
#412739=CARTESIAN_POINT('Ctrl Pts',(-0.761689021652897,1.30731357265555,
-0.958000819099493));
#412740=CARTESIAN_POINT('Ctrl Pts',(-1.06907929995926,1.06931057908566,
-0.936600303173127));
#412741=CARTESIAN_POINT('Ctrl Pts',(-1.19623673913263,0.924877016116167,
-0.926470394612626));
#412742=CARTESIAN_POINT('Ctrl Pts',(-1.39367914953313,0.589190131513344,
-0.907646306529701));
#412743=CARTESIAN_POINT('Ctrl Pts',(-1.45942723684233,0.399519099757115,
-0.897195505541958));
#412744=CARTESIAN_POINT('Ctrl Pts',(-1.51268906272795,0.00856741889772205,
-0.875475967716439));
#412745=CARTESIAN_POINT('Ctrl Pts',(-1.50090383822517,-0.188664743856311,
-0.864518625341217));
#412746=CARTESIAN_POINT('Ctrl Pts',(-1.40364785614872,-0.562075240715819,
-0.843773597737913));
#412747=CARTESIAN_POINT('Ctrl Pts',(-1.32118880347593,-0.735259580504762,
-0.834808515375079));
#412748=CARTESIAN_POINT('Ctrl Pts',(-1.0907670814543,-1.04870959175978,
-0.815015400348303));
#412749=CARTESIAN_POINT('Ctrl Pts',(-0.942260035311356,-1.18393070164062,
-0.804114209818238));
#412750=CARTESIAN_POINT('Ctrl Pts',(-0.605830191961757,-1.38578633010734,
-0.782320620642388));
#412751=CARTESIAN_POINT('Ctrl Pts',(-0.422204016207854,-1.45230578227655,
-0.771638139581986));
#412752=CARTESIAN_POINT('Ctrl Pts',(-0.0400986940400851,-1.51185958119907,
-0.751599816505332));
#412753=CARTESIAN_POINT('Ctrl Pts',(0.154725281291594,-1.50445690023413,
-0.74267957921716));
#412754=CARTESIAN_POINT('Ctrl Pts',(0.536319722570401,-1.41487308640885,
-0.721831668828105));
#412755=CARTESIAN_POINT('Ctrl Pts',(0.718861257413663,-1.33144084341973,
-0.710731572832847));
#412756=CARTESIAN_POINT('Ctrl Pts',(1.0347253322851,-1.10268938550674,-0.689180348280738));
#412757=CARTESIAN_POINT('Ctrl Pts',(1.16677741219797,-0.961890420146206,
-0.678915907252553));
#412758=CARTESIAN_POINT('Ctrl Pts',(1.37557057361387,-0.630762884694104,
-0.659672354494296));
#412759=CARTESIAN_POINT('Ctrl Pts',(1.4473878108606,-0.441771302548477,
-0.649542850141474));
#412760=CARTESIAN_POINT('Ctrl Pts',(1.51193683368003,-0.0505838155729788,
-0.62781021197617));
#412761=CARTESIAN_POINT('Ctrl Pts',(1.50558094216201,0.147446649609004,
-0.61680851946606));
#412762=CARTESIAN_POINT('Ctrl Pts',(1.41839292597098,0.523684067536241,
-0.595906440692327));
#412763=CARTESIAN_POINT('Ctrl Pts',(1.34076354521001,0.698870895164634,
-0.586761102390866));
#412764=CARTESIAN_POINT('Ctrl Pts',(1.11916700372969,1.01834261045172,-0.567225319504408));
#412765=CARTESIAN_POINT('Ctrl Pts',(0.9744492721012,1.15757682489316,-0.55639496732724));
#412766=CARTESIAN_POINT('Ctrl Pts',(0.643288707878562,1.36887271675508,
-0.534592666922834));
#412767=CARTESIAN_POINT('Ctrl Pts',(0.461036608622036,1.44051741693377,
-0.523833928148471));
#412768=CARTESIAN_POINT('Ctrl Pts',(0.180842166400501,1.49182645708902,
-0.508927815646213));
#412769=CARTESIAN_POINT('Ctrl Pts',(0.0904158668629034,1.50000000000006,
-0.504350135422671));
#412770=CARTESIAN_POINT('Ctrl Pts',(0.,1.50000000000006,-0.499999999999979));
#412771=CARTESIAN_POINT('Origin',(0.,2.5406128344257E-15,14.));
#412772=CARTESIAN_POINT('',(-9.18485099360549E-17,1.50000000000006,0.0624999999999975));
#412773=CARTESIAN_POINT('',(-2.55842840407684E-14,1.50000000000006,2.41061511030425E-14));
#412774=CARTESIAN_POINT('',(-1.8369701987211E-16,1.50000000000006,14.));
#412775=CARTESIAN_POINT('Ctrl Pts',(0.,1.50000000000006,0.0624999999999976));
#412776=CARTESIAN_POINT('Ctrl Pts',(0.012054289146646,1.50000000000006,
0.0619200377430222));
#412777=CARTESIAN_POINT('Ctrl Pts',(0.0241143953777522,1.49985469449604,
0.0613357593474155));
#412778=CARTESIAN_POINT('Ctrl Pts',(0.227159790220428,1.49495612231971,
0.0514306617838963));
#412779=CARTESIAN_POINT('Ctrl Pts',(0.415482244731523,1.45390737684839,
0.0412297505369348));
#412780=CARTESIAN_POINT('Ctrl Pts',(0.773383422037556,1.30048073774713,
0.0197483710290463));
#412781=CARTESIAN_POINT('Ctrl Pts',(0.93845214862749,1.18688107122445,0.00865095192579394));
#412782=CARTESIAN_POINT('Ctrl Pts',(1.2116261284016,0.905291054690885,-0.0123140822077631));
#412783=CARTESIAN_POINT('Ctrl Pts',(1.31834906133297,0.741310066150857,
-0.021316107436091));
#412784=CARTESIAN_POINT('Ctrl Pts',(1.4632645623403,0.382356276828995,-0.0412579846206378));
#412785=CARTESIAN_POINT('Ctrl Pts',(1.50029477690078,0.19089170271958,-0.0518949054044928));
#412786=CARTESIAN_POINT('Ctrl Pts',(1.4996898553524,-0.203205997702154,
-0.0737892220945868));
#412787=CARTESIAN_POINT('Ctrl Pts',(1.45902227025322,-0.402037982209106,
-0.084835443456084));
#412788=CARTESIAN_POINT('Ctrl Pts',(1.30593786665162,-0.762053788740558,
-0.104836321596719));
#412789=CARTESIAN_POINT('Ctrl Pts',(1.19886813597746,-0.921369750070448,
-0.113746367416195));
#412790=CARTESIAN_POINT('Ctrl Pts',(0.927156984189888,-1.19524181015156,
-0.134426633526201));
#412791=CARTESIAN_POINT('Ctrl Pts',(0.763651532865142,-1.30577691246609,
-0.14536371272963));
#412792=CARTESIAN_POINT('Ctrl Pts',(0.400480218338332,-1.45914764262538,
-0.16709709880661));
#412793=CARTESIAN_POINT('Ctrl Pts',(0.203815102558579,-1.4993273908806,
-0.177675257719447));
#412794=CARTESIAN_POINT('Ctrl Pts',(-0.185401401652342,-1.50062783086148,
-0.196437568842183));
#412795=CARTESIAN_POINT('Ctrl Pts',(-0.374284202094425,-1.46499993765963,
-0.20647998102331));
#412796=CARTESIAN_POINT('Ctrl Pts',(-0.735490393930043,-1.3221946159591,
-0.227825336522426));
#412797=CARTESIAN_POINT('Ctrl Pts',(-0.903290925767023,-1.21376054447359,
-0.238910700915876));
#412798=CARTESIAN_POINT('Ctrl Pts',(-1.1852683061334,-0.939824153228578,
-0.26008668815545));
#412799=CARTESIAN_POINT('Ctrl Pts',(-1.2973924118842,-0.77774928530609,
-0.269291706371907));
#412800=CARTESIAN_POINT('Ctrl Pts',(-1.4522514080294,-0.422027875514621,
-0.289054006915876));
#412801=CARTESIAN_POINT('Ctrl Pts',(-1.49439722341846,-0.232166380326087,
-0.299601867759683));
#412802=CARTESIAN_POINT('Ctrl Pts',(-1.50476095174324,0.160691684605172,
-0.321427315811418));
#412803=CARTESIAN_POINT('Ctrl Pts',(-1.46987757693276,0.360003953280259,
-0.3325002196267));
#412804=CARTESIAN_POINT('Ctrl Pts',(-1.32735514008263,0.724238208405123,
-0.352735456022524));
#412805=CARTESIAN_POINT('Ctrl Pts',(-1.22460662669361,0.886980672789432,
-0.361552771557538));
#412806=CARTESIAN_POINT('Ctrl Pts',(-0.960726520483816,1.16833841263676,
-0.382064201860574));
#412807=CARTESIAN_POINT('Ctrl Pts',(-0.800909367067889,1.28317803984535,
-0.392943397884075));
#412808=CARTESIAN_POINT('Ctrl Pts',(-0.442830785125446,1.44686319665528,
-0.414718271601753));
#412809=CARTESIAN_POINT('Ctrl Pts',(-0.247381584421267,1.49276234346049,
-0.425396801955183));
#412810=CARTESIAN_POINT('Ctrl Pts',(-0.0324259740880306,1.49973729413911,
-0.435932607209287));
#412811=CARTESIAN_POINT('Ctrl Pts',(-0.0162082427937986,1.50000000000006,
-0.436720180554994));
#412812=CARTESIAN_POINT('Ctrl Pts',(-5.09848573616319E-14,1.50000000000006,
-0.437499999999999));
#412813=CARTESIAN_POINT('Ctrl Pts',(7.45931094670027E-16,1.50000000000006,
-0.499999999999979));
#412814=CARTESIAN_POINT('Ctrl Pts',(-0.100870160085812,1.50000000000006,
-0.495146882160084));
#412815=CARTESIAN_POINT('Ctrl Pts',(-0.20169983483153,1.48982736637166,
-0.490013139015587));
#412816=CARTESIAN_POINT('Ctrl Pts',(-0.496243158183144,1.42950096301812,
-0.474166183337012));
#412817=CARTESIAN_POINT('Ctrl Pts',(-0.681583232330906,1.3509861438843,
-0.463068037663782));
#412818=CARTESIAN_POINT('Ctrl Pts',(-1.00448658647526,1.13038954226337,
-0.441404659415633));
#412819=CARTESIAN_POINT('Ctrl Pts',(-1.14064794355933,0.992832675357211,
-0.431032568987764));
#412820=CARTESIAN_POINT('Ctrl Pts',(-1.3573289981967,0.668537834146947,
-0.411599306852214));
#412821=CARTESIAN_POINT('Ctrl Pts',(-1.43370523838309,0.48352662619307,
-0.401862590343936));
#412822=CARTESIAN_POINT('Ctrl Pts',(-1.50981966629285,0.095837857719107,
-0.380324325428716));
#412823=CARTESIAN_POINT('Ctrl Pts',(-1.50935560392058,-0.102889185679314,
-0.369283934128803));
#412824=CARTESIAN_POINT('Ctrl Pts',(-1.43306586861821,-0.482091858059621,
-0.348217118996566));
#412825=CARTESIAN_POINT('Ctrl Pts',(-1.36056953424563,-0.659480305237118,
-0.338808201536163));
#412826=CARTESIAN_POINT('Ctrl Pts',(-1.14840390936391,-0.985248392224554,
-0.319551264622214));
#412827=CARTESIAN_POINT('Ctrl Pts',(-1.00783288225427,-1.12862552383915,
-0.308805339826642));
#412828=CARTESIAN_POINT('Ctrl Pts',(-0.682561860333359,-1.34979812671681,
-0.287012047074571));
#412829=CARTESIAN_POINT('Ctrl Pts',(-0.501923892968732,-1.42685954182922,
-0.276180503953351));
#412830=CARTESIAN_POINT('Ctrl Pts',(-0.124496714670119,-1.50701298862099,
-0.255795045737731));
#412831=CARTESIAN_POINT('Ctrl Pts',(0.0684526444356624,-1.51059602506114,
-0.247000904638357));
#412832=CARTESIAN_POINT('Ctrl Pts',(0.453870608993343,-1.44359645502584,
-0.226596375005052));
#412833=CARTESIAN_POINT('Ctrl Pts',(0.642002889011626,-1.37032399989127,
-0.21550951048644));
#412834=CARTESIAN_POINT('Ctrl Pts',(0.972052791411423,-1.15848637848887,
-0.193745598781109));
#412835=CARTESIAN_POINT('Ctrl Pts',(1.11243019608887,-1.02444870831659,
-0.183268419133659));
#412836=CARTESIAN_POINT('Ctrl Pts',(1.33726432612642,-0.707317214958666,
-0.163641873859811));
#412837=CARTESIAN_POINT('Ctrl Pts',(1.41828932336204,-0.526348860670041,
-0.154241603370399));
#412838=CARTESIAN_POINT('Ctrl Pts',(1.50621864088017,-0.142421766452506,
-0.132912320358315));
#412839=CARTESIAN_POINT('Ctrl Pts',(1.51186799289991,0.0568439120604016,
-0.121842004885376));
#412840=CARTESIAN_POINT('Ctrl Pts',(1.44687788961899,0.439013439406849,
-0.100610364477241));
#412841=CARTESIAN_POINT('Ctrl Pts',(1.37961132542521,0.6187237847525,-0.0908564757104214));
#412842=CARTESIAN_POINT('Ctrl Pts',(1.1770866073687,0.950789355903772,-0.0718884570267085));
#412843=CARTESIAN_POINT('Ctrl Pts',(1.040850589036,1.09824308004335,-0.0612378617569129));
#412844=CARTESIAN_POINT('Ctrl Pts',(0.721863706966089,1.32927659203654,
-0.039473000682295));
#412845=CARTESIAN_POINT('Ctrl Pts',(0.543027040436241,1.41180481335541,
-0.0285762669599376));
#412846=CARTESIAN_POINT('Ctrl Pts',(0.237438697047166,1.48588709847123,
-0.0118157996803148));
#412847=CARTESIAN_POINT('Ctrl Pts',(0.118813593213069,1.50000000000006,
-0.00571642166872418));
#412848=CARTESIAN_POINT('Ctrl Pts',(-4.74273398332059E-14,1.50000000000006,
2.38090797077817E-14));
#412849=CARTESIAN_POINT('Origin',(0.,2.5406128344257E-15,14.));
#412850=CARTESIAN_POINT('',(1.27348944451369E-13,1.50000000000006,0.562499999999986));
#412851=CARTESIAN_POINT('',(-1.01921478372424E-13,1.50000000000006,0.50000000000003));
#412852=CARTESIAN_POINT('',(-1.8369701987211E-16,1.50000000000006,14.));
#412853=CARTESIAN_POINT('Ctrl Pts',(2.54881585922611E-13,1.50000000000006,
0.562499999999986));
#412854=CARTESIAN_POINT('Ctrl Pts',(0.0406408989401091,1.50000000000006,
0.560544663838062));
#412855=CARTESIAN_POINT('Ctrl Pts',(0.0813262693164112,1.4983483840002,
0.558541309820913));
#412856=CARTESIAN_POINT('Ctrl Pts',(0.313442176157069,1.47941358982352,
0.546847661541202));
#412857=CARTESIAN_POINT('Ctrl Pts',(0.500127801022325,1.4271521204739,0.536414037745119));
#412858=CARTESIAN_POINT('Ctrl Pts',(0.850346715884616,1.25170506897473,
0.514690593139223));
#412859=CARTESIAN_POINT('Ctrl Pts',(1.00921900268806,1.12753921057511,0.503597795054284));
#412860=CARTESIAN_POINT('Ctrl Pts',(1.26379674107868,0.830384213019557,
0.483095112417506));
#412861=CARTESIAN_POINT('Ctrl Pts',(1.35941976917598,0.662343199038309,
0.474296844390982));
#412862=CARTESIAN_POINT('Ctrl Pts',(1.48314056992831,0.296749108474254,
0.45398606158187));
#412863=CARTESIAN_POINT('Ctrl Pts',(1.5090677735988,0.102320123342678,0.443184451296783));
#412864=CARTESIAN_POINT('Ctrl Pts',(1.4850548862901,-0.290069550070151,
0.421385024996072));
#412865=CARTESIAN_POINT('Ctrl Pts',(1.43357470864608,-0.484163398894276,
0.410602033394734));
#412866=CARTESIAN_POINT('Ctrl Pts',(1.26185297329218,-0.832935861582507,
0.391225785467612));
#412867=CARTESIAN_POINT('Ctrl Pts',(1.14639029827533,-0.985832644872433,
0.381938155473427));
#412868=CARTESIAN_POINT('Ctrl Pts',(0.859555578540014,-1.24491280118131,
0.360941142577173));
#412869=CARTESIAN_POINT('Ctrl Pts',(0.689185616573045,-1.34672400738396,
0.349916124899035));
#412870=CARTESIAN_POINT('Ctrl Pts',(0.316533522162275,-1.47967569734543,
0.328293790148262));
#412871=CARTESIAN_POINT('Ctrl Pts',(0.117624745672662,-1.50856522554025,
0.318397146146432));
#412872=CARTESIAN_POINT('Ctrl Pts',(-0.27241708027596,-1.48744781999047,
0.299044655447275));
#412873=CARTESIAN_POINT('Ctrl Pts',(-0.459965936736015,-1.44052839410447,
0.288717889497935));
#412874=CARTESIAN_POINT('Ctrl Pts',(-0.814014715386158,-1.27554039433401,
0.267100709699319));
#412875=CARTESIAN_POINT('Ctrl Pts',(-0.975924727411788,-1.156375414924,
0.256000672296751));
#412876=CARTESIAN_POINT('Ctrl Pts',(-1.23940847168001,-0.866578105453092,
0.235273879476976));
#412877=CARTESIAN_POINT('Ctrl Pts',(-1.34029906880132,-0.700490994357527,
0.226416166353165));
#412878=CARTESIAN_POINT('Ctrl Pts',(-1.47420654920234,-0.338046251999789,
0.206280347333291));
#412879=CARTESIAN_POINT('Ctrl Pts',(-1.50550075040419,-0.144963845736001,
0.195553546985305));
#412880=CARTESIAN_POINT('Ctrl Pts',(-1.49275257816999,0.247446765567662,
0.173752957468437));
#412881=CARTESIAN_POINT('Ctrl Pts',(-1.44683992264741,0.442960968548592,
0.162891057302831));
#412882=CARTESIAN_POINT('Ctrl Pts',(-1.28510797535013,0.796611616917752,
0.143243799060103));
#412883=CARTESIAN_POINT('Ctrl Pts',(-1.17400046898735,0.952800260806589,
0.134184116655229));
#412884=CARTESIAN_POINT('Ctrl Pts',(-0.894994052729665,1.21959421410027,
0.113349471047183));
#412885=CARTESIAN_POINT('Ctrl Pts',(-0.728132560453016,1.32598777580278,
0.102365967042949));
#412886=CARTESIAN_POINT('Ctrl Pts',(-0.371528935965003,1.46521793089753,
0.0813413628520834));
#412887=CARTESIAN_POINT('Ctrl Pts',(-0.186506457465428,1.50000000000006,
0.0714732961186032));
#412888=CARTESIAN_POINT('Ctrl Pts',(-3.15719672627779E-15,1.50000000000006,
0.0624999999999978));
#412889=CARTESIAN_POINT('Ctrl Pts',(-5.09848710616648E-14,1.50000000000006,
2.38546161990259E-14));
#412890=CARTESIAN_POINT('Ctrl Pts',(-0.0709875012889099,1.50000000000006,
0.00341538774820884));
#412891=CARTESIAN_POINT('Ctrl Pts',(-0.142028686340236,1.49496141470086,
0.00697331906053692));
#412892=CARTESIAN_POINT('Ctrl Pts',(-0.411099076206722,1.45643705631314,
0.0209890952952234));
#412893=CARTESIAN_POINT('Ctrl Pts',(-0.601880785957816,1.38850081793605,
0.0320552023180216));
#412894=CARTESIAN_POINT('Ctrl Pts',(-0.938844531503994,1.18564451242515,
0.0539022754598391));
#412895=CARTESIAN_POINT('Ctrl Pts',(-1.08334734961584,1.05525225377623,
0.0644766777224905));
#412896=CARTESIAN_POINT('Ctrl Pts',(-1.31623827713633,0.74530117362232,
0.0842913999236317));
#412897=CARTESIAN_POINT('Ctrl Pts',(-1.40180453069513,0.568250798011601,
0.0934305112217602));
#412898=CARTESIAN_POINT('Ctrl Pts',(-1.50126820996767,0.188174214398025,
0.114545876978065));
#412899=CARTESIAN_POINT('Ctrl Pts',(-1.51297047242782,-0.0114425435933111,
0.12563569686647));
#412900=CARTESIAN_POINT('Ctrl Pts',(-1.4591968707338,-0.396327239575063,
0.147018179976564));
#412901=CARTESIAN_POINT('Ctrl Pts',(-1.39707708900367,-0.578386341706428,
0.157132574539417));
#412902=CARTESIAN_POINT('Ctrl Pts',(-1.20396132549991,-0.916492801378582,
0.175916266743421));
#412903=CARTESIAN_POINT('Ctrl Pts',(-1.07206249365286,-1.06781241836371,
0.186415158624291));
#412904=CARTESIAN_POINT('Ctrl Pts',(-0.759351410534148,-1.30830487595872,
0.208140823670025));
#412905=CARTESIAN_POINT('Ctrl Pts',(-0.582414938121718,-1.39609256486489,
0.219092230581993));
#412906=CARTESIAN_POINT('Ctrl Pts',(-0.210095445423381,-1.49734090530431,
0.23981791442758));
#412907=CARTESIAN_POINT('Ctrl Pts',(-0.0187966379690382,-1.51188883256379,
0.248765400985086));
#412908=CARTESIAN_POINT('Ctrl Pts',(0.36776423073231,-1.46775849240247,
0.268589662234254));
#412909=CARTESIAN_POINT('Ctrl Pts',(0.558918940856327,-1.40611402825547,
0.279498943739474));
#412910=CARTESIAN_POINT('Ctrl Pts',(0.901250708619873,-1.21456036593823,
0.301290323659713));
#412911=CARTESIAN_POINT('Ctrl Pts',(1.0502060064706,-1.08834353623334,0.31196296181635));
#412912=CARTESIAN_POINT('Ctrl Pts',(1.29190529576069,-0.786360349714089,
0.331980146141988));
#412913=CARTESIAN_POINT('Ctrl Pts',(1.38239012590076,-0.613500578045895,
0.340916634553032));
#412914=CARTESIAN_POINT('Ctrl Pts',(1.49430302141388,-0.237771999146122,
0.361790444491908));
#412915=CARTESIAN_POINT('Ctrl Pts',(1.5126224446182,-0.0379766749085486,
0.372890184727328));
#412916=CARTESIAN_POINT('Ctrl Pts',(1.47115013980118,0.349676795606788,
0.394426488644846));
#412917=CARTESIAN_POINT('Ctrl Pts',(1.41464528846236,0.534188936917993,
0.404677163162135));
#412918=CARTESIAN_POINT('Ctrl Pts',(1.23105735621897,0.880145184501605,
0.423896954694558));
#412919=CARTESIAN_POINT('Ctrl Pts',(1.1025766449906,1.03659133669472,0.434079793564812));
#412920=CARTESIAN_POINT('Ctrl Pts',(0.794982012712315,1.28704585517344,
0.455836017168149));
#412921=CARTESIAN_POINT('Ctrl Pts',(0.620024979142385,1.37987519435246,
0.466832234125473));
#412922=CARTESIAN_POINT('Ctrl Pts',(0.291744411200726,1.47864384033826,
0.485370213814313));
#412923=CARTESIAN_POINT('Ctrl Pts',(0.146157289931562,1.50000000000008,
0.49296800410952));
#412924=CARTESIAN_POINT('Ctrl Pts',(-2.06189232354603E-13,1.50000000000006,
0.50000000000003));
#412925=CARTESIAN_POINT('Origin',(0.,2.5406128344257E-15,14.));
#412926=CARTESIAN_POINT('',(5.08396327447441E-14,1.50000000000006,1.06249999999999));
#412927=CARTESIAN_POINT('',(-9.18485099360549E-17,1.50000000000006,1.00000000000002));
#412928=CARTESIAN_POINT('',(-1.8369701987211E-16,1.50000000000006,14.));
#412929=CARTESIAN_POINT('Ctrl Pts',(1.0186296250936E-13,1.50000000000006,
1.06249999999999));
#412930=CARTESIAN_POINT('Ctrl Pts',(0.0680382842757857,1.50000000000006,
1.05922650652151));
#412931=CARTESIAN_POINT('Ctrl Pts',(0.136136544871693,1.49537132922985,
1.05582155324288));
#412932=CARTESIAN_POINT('Ctrl Pts',(0.395203876533196,1.45983798970958,
1.0423701332279));
#412933=CARTESIAN_POINT('Ctrl Pts',(0.579696520662932,1.39687125311336,
1.03174465073202));
#412934=CARTESIAN_POINT('Ctrl Pts',(0.921297492681591,1.20064222399006,
1.00985855993829));
#412935=CARTESIAN_POINT('Ctrl Pts',(1.07360653158139,1.06663849347069,0.998808262039792));
#412936=CARTESIAN_POINT('Ctrl Pts',(1.31004293758201,0.754988953245441,
0.978775778479312));
#412937=CARTESIAN_POINT('Ctrl Pts',(1.3951625075513,0.582880009906409,0.969882222772534));
#412938=CARTESIAN_POINT('Ctrl Pts',(1.49788420655235,0.211038565719377,
0.949224364762146));
#412939=CARTESIAN_POINT('Ctrl Pts',(1.51260816412702,0.0143019682214694,
0.93829455379004));
#412940=CARTESIAN_POINT('Ctrl Pts',(1.46538570869696,-0.377018865546308,
0.91655450746961));
#412941=CARTESIAN_POINT('Ctrl Pts',(1.40259296866089,-0.567677864245,0.905962340875239));
#412942=CARTESIAN_POINT('Ctrl Pts',(1.21046020806795,-0.906101173453465,
0.887161045919216));
#412943=CARTESIAN_POINT('Ctrl Pts',(1.08578909657305,-1.05230619708041,
0.877175991235747));
#412944=CARTESIAN_POINT('Ctrl Pts',(0.782609624085623,-1.29484936108939,
0.855851951953274));
#412945=CARTESIAN_POINT('Ctrl Pts',(0.605253911944434,-1.38664503724576,
0.844769041381123));
#412946=CARTESIAN_POINT('Ctrl Pts',(0.227357440291247,-1.49550062377031,
0.823563722619211));
#412947=CARTESIAN_POINT('Ctrl Pts',(0.0307822054468046,-1.51236761327203,
0.81432455436315));
#412948=CARTESIAN_POINT('Ctrl Pts',(-0.355011658420151,-1.47006145389006,
0.794587867339601));
#412949=CARTESIAN_POINT('Ctrl Pts',(-0.540662172389121,-1.41236706042891,
0.784053130781083));
#412950=CARTESIAN_POINT('Ctrl Pts',(-0.886665972559036,-1.22634334768617,
0.762238689829726));
#412951=CARTESIAN_POINT('Ctrl Pts',(-1.04228741892642,-1.09715391965502,
0.751162754277315));
#412952=CARTESIAN_POINT('Ctrl Pts',(-1.28771223104499,-0.792605411430979,
0.730895066714778));
#412953=CARTESIAN_POINT('Ctrl Pts',(-1.37799972031613,-0.622531871559214,
0.722085103975474));
#412954=CARTESIAN_POINT('Ctrl Pts',(-1.49117016866574,-0.253755936497839,
0.701597552027621));
#412955=CARTESIAN_POINT('Ctrl Pts',(-1.5114885454466,-0.0580879035252565,
0.690727105751367));
#412956=CARTESIAN_POINT('Ctrl Pts',(-1.47580497889151,0.333937053169343,
0.668947941490558));
#412957=CARTESIAN_POINT('Ctrl Pts',(-1.41860962415413,0.526389181544339,
0.658256156580836));
#412958=CARTESIAN_POINT('Ctrl Pts',(-1.23660211030209,0.87000933239387,
0.639166148200308));
#412959=CARTESIAN_POINT('Ctrl Pts',(-1.11655459910737,1.0195301344132,0.629566643351781));
#412960=CARTESIAN_POINT('Ctrl Pts',(-0.821541279919785,1.270411883044,0.608403870952528));
#412961=CARTESIAN_POINT('Ctrl Pts',(-0.647615965374159,1.36728612241562,
0.597344934261222));
#412962=CARTESIAN_POINT('Ctrl Pts',(-0.311066258152681,1.47570356486116,
0.578141083299403));
#412963=CARTESIAN_POINT('Ctrl Pts',(-0.155892677277793,1.50000000000006,
0.570000389932598));
#412964=CARTESIAN_POINT('Ctrl Pts',(2.56461518688411E-13,1.50000000000006,
0.562499999999986));
#412965=CARTESIAN_POINT('Ctrl Pts',(-2.03659259724975E-13,1.50000000000006,
0.50000000000003));
#412966=CARTESIAN_POINT('Ctrl Pts',(-0.043191708028036,1.50000000000005,
0.502078062021416));
#412967=CARTESIAN_POINT('Ctrl Pts',(-0.0864282246675912,1.49813456320497,
0.504210097586897));
#412968=CARTESIAN_POINT('Ctrl Pts',(-0.327738068046906,1.47720865117899,
0.516401398173714));
#412969=CARTESIAN_POINT('Ctrl Pts',(-0.520475306897241,1.42078936554684,
0.527241675280143));
#412970=CARTESIAN_POINT('Ctrl Pts',(-0.868319352452527,1.23839726903149,
0.549043776850346));
#412971=CARTESIAN_POINT('Ctrl Pts',(-1.02099688329402,1.11587823707962,
0.559792784420996));
#412972=CARTESIAN_POINT('Ctrl Pts',(-1.27017123344605,0.820755811782216,
0.579979036079432));
#412973=CARTESIAN_POINT('Ctrl Pts',(-1.36480343662259,0.651373723038201,
0.588812570942347));
#412974=CARTESIAN_POINT('Ctrl Pts',(-1.48714974026619,0.279438547031942,
0.609475636276026));
#412975=CARTESIAN_POINT('Ctrl Pts',(-1.51107383067189,0.0796583666816162,
0.620574535184376));
#412976=CARTESIAN_POINT('Ctrl Pts',(-1.48007727192697,-0.310031319599864,
0.642223962200013));
#412977=CARTESIAN_POINT('Ctrl Pts',(-1.42838264999849,-0.49647962280372,
0.652582201266895));
#412978=CARTESIAN_POINT('Ctrl Pts',(-1.25457208539778,-0.845831340986355,
0.671990630054817));
#412979=CARTESIAN_POINT('Ctrl Pts',(-1.13178665459598,-1.00422413691273,
0.68177533743958));
#412980=CARTESIAN_POINT('Ctrl Pts',(-0.832931565108941,-1.26290740472686,
0.70333965596475));
#412981=CARTESIAN_POINT('Ctrl Pts',(-0.660279040728227,-1.36115474455317,
0.71437549718999));
#412982=CARTESIAN_POINT('Ctrl Pts',(-0.293350074741007,-1.48324987324057,
0.7354209066496));
#412983=CARTESIAN_POINT('Ctrl Pts',(-0.103396430208456,-1.50843250688356,
0.744791100629857));
#412984=CARTESIAN_POINT('Ctrl Pts',(0.2847199519682,-1.48609621704444,0.764084811269269));
#412985=CARTESIAN_POINT('Ctrl Pts',(0.478985398772131,-1.43530395959292,
0.774842307976797));
#412986=CARTESIAN_POINT('Ctrl Pts',(0.832445184826515,-1.26287480719448,
0.796637848540046));
#412987=CARTESIAN_POINT('Ctrl Pts',(0.988999606252736,-1.14442470702295,
0.807460357213135));
#412988=CARTESIAN_POINT('Ctrl Pts',(1.24609216178188,-0.856668614388136,
0.827822953353661));
#412989=CARTESIAN_POINT('Ctrl Pts',(1.34509862215902,-0.690894590198938,
0.836616967211182));
#412990=CARTESIAN_POINT('Ctrl Pts',(1.47836546238066,-0.323069043266823,
0.857051719818521));
#412991=CARTESIAN_POINT('Ctrl Pts',(1.50820423027976,-0.123469482155708,
0.868140584324693));
#412992=CARTESIAN_POINT('Ctrl Pts',(1.48831877173615,0.268063539597317,
0.889892418866527));
#412993=CARTESIAN_POINT('Ctrl Pts',(1.44175418543378,0.45641507535595,0.90035639307534));
#412994=CARTESIAN_POINT('Ctrl Pts',(1.27819434454985,0.809246369246787,
0.919958131624831));
#412995=CARTESIAN_POINT('Ctrl Pts',(1.16123647414513,0.969641981338816,
0.929397816903269));
#412996=CARTESIAN_POINT('Ctrl Pts',(0.871523790004527,1.23668668522225,
0.950754533359159));
#412997=CARTESIAN_POINT('Ctrl Pts',(0.701435278023972,1.34049769856449,
0.961821559966836));
#412998=CARTESIAN_POINT('Ctrl Pts',(0.350660738991283,1.46904663991433,
0.982269011771168));
#412999=CARTESIAN_POINT('Ctrl Pts',(0.175945122352012,1.50000000000006,
0.991534836353976));
#413000=CARTESIAN_POINT('Ctrl Pts',(3.41740524767431E-15,1.50000000000006,
1.00000000000002));
#413001=CARTESIAN_POINT('Origin',(0.,2.5406128344257E-15,14.));
#413002=CARTESIAN_POINT('',(-9.18485099360549E-17,1.50000000000006,1.5625));
#413003=CARTESIAN_POINT('',(-9.18485099360549E-17,1.50000000000006,1.50000000000002));
#413004=CARTESIAN_POINT('',(-1.8369701987211E-16,1.50000000000006,14.));
#413005=CARTESIAN_POINT('Ctrl Pts',(0.,1.50000000000006,1.5625));
#413006=CARTESIAN_POINT('Ctrl Pts',(0.0966928609426964,1.50000000000006,
1.55784786255883));
#413007=CARTESIAN_POINT('Ctrl Pts',(0.193367170400976,1.49065233465526,
1.55293696030564));
#413008=CARTESIAN_POINT('Ctrl Pts',(0.479319745183868,1.43457013871789,
1.53762122186073));
#413009=CARTESIAN_POINT('Ctrl Pts',(0.660871598557134,1.3605059032998,1.52682896436994));
#413010=CARTESIAN_POINT('Ctrl Pts',(0.989442467783122,1.14478539925305,
1.50502835483013));
#413011=CARTESIAN_POINT('Ctrl Pts',(1.13232608393568,1.00368801786495,1.49423449193753));
#413012=CARTESIAN_POINT('Ctrl Pts',(1.34972401676549,0.681396013205005,
1.47482237333249));
#413013=CARTESIAN_POINT('Ctrl Pts',(1.4250652882199,0.505237233551949,1.46556873519728));
#413014=CARTESIAN_POINT('Ctrl Pts',(1.50741977300721,0.127672340085819,
1.44459290778249));
#413015=CARTESIAN_POINT('Ctrl Pts',(1.51116381860928,-0.0706885550306063,
1.4335728580538));
#413016=CARTESIAN_POINT('Ctrl Pts',(1.44146481134182,-0.460340823710175,
1.41192550979383));
#413017=CARTESIAN_POINT('Ctrl Pts',(1.3676157802519,-0.647557592297102,
1.40197840067584));
#413018=CARTESIAN_POINT('Ctrl Pts',(1.15532125302563,-0.975663988445489,
1.3826503089127));
#413019=CARTESIAN_POINT('Ctrl Pts',(1.02144199305684,-1.11504353664287,
1.37233738589762));
#413020=CARTESIAN_POINT('Ctrl Pts',(0.702439219068069,-1.34021405169521,
1.35073462124883));
#413021=CARTESIAN_POINT('Ctrl Pts',(0.518644232623378,-1.4214824349833,
1.3396343257492));
#413022=CARTESIAN_POINT('Ctrl Pts',(0.136178992505056,-1.50618660754137,
1.31888006462221));
#413023=CARTESIAN_POINT('Ctrl Pts',(-0.058222912169048,-1.51120841051425,
1.31001009356864));
#413024=CARTESIAN_POINT('Ctrl Pts',(-0.439350732684371,-1.44724076227978,
1.28989619363684));
#413025=CARTESIAN_POINT('Ctrl Pts',(-0.622388972984679,-1.37846051901595,
1.27917919988151));
#413026=CARTESIAN_POINT('Ctrl Pts',(-0.956530543513232,-1.17242945138438,
1.25737972086184));
#413027=CARTESIAN_POINT('Ctrl Pts',(-1.10338207804408,-1.0354270734641,
1.24650870150359));
#413028=CARTESIAN_POINT('Ctrl Pts',(-1.32992195461779,-0.719312385456412,
1.22682833305432));
#413029=CARTESIAN_POINT('Ctrl Pts',(-1.41025282826834,-0.54525377106231,
1.21779187617008));
#413030=CARTESIAN_POINT('Ctrl Pts',(-1.50309527717499,-0.170593837017244,
1.1969774353898));
#413031=CARTESIAN_POINT('Ctrl Pts',(-1.51250263433437,0.027006577808505,
1.18599963456615));
#413032=CARTESIAN_POINT('Ctrl Pts',(-1.45438152330554,0.417523507132094,
1.16430424960373));
#413033=CARTESIAN_POINT('Ctrl Pts',(-1.38628623378875,0.60639427834552,
1.15402010867801));
#413034=CARTESIAN_POINT('Ctrl Pts',(-1.18455223017824,0.939843159453667,
1.13505170798423));
#413035=CARTESIAN_POINT('Ctrl Pts',(-1.05541834887102,1.08283785496255,
1.1248666763478));
#413036=CARTESIAN_POINT('Ctrl Pts',(-0.744595072247187,1.31716361140241,
1.10340313568871));
#413037=CARTESIAN_POINT('Ctrl Pts',(-0.564084622698752,1.40397900186252,
1.09230678401163));
#413038=CARTESIAN_POINT('Ctrl Pts',(-0.250118003558327,1.48433383807843,
1.07496897922141));
#413039=CARTESIAN_POINT('Ctrl Pts',(-0.125181652506405,1.50000000000006,
1.06852280506435));
#413040=CARTESIAN_POINT('Ctrl Pts',(1.04569131131882E-13,1.50000000000006,
1.06249999999999));
#413041=CARTESIAN_POINT('Ctrl Pts',(0.,1.50000000000006,1.00000000000002));
#413042=CARTESIAN_POINT('Ctrl Pts',(-0.0139210510018308,1.50000000000006,
1.00066977687863));
#413043=CARTESIAN_POINT('Ctrl Pts',(-0.0278492894904031,1.49980620499738,
1.00134528275986));
#413044=CARTESIAN_POINT('Ctrl Pts',(-0.240537711569285,1.49387972184136,
1.01174288377037));
#413045=CARTESIAN_POINT('Ctrl Pts',(-0.436189653169356,1.44887832885034,
1.02240623089375));
#413046=CARTESIAN_POINT('Ctrl Pts',(-0.795089312113688,1.28680552109984,
1.04417582122323));
#413047=CARTESIAN_POINT('Ctrl Pts',(-0.955494288648501,1.17263556134334,
1.05506469702606));
#413048=CARTESIAN_POINT('Ctrl Pts',(-1.22061058356622,0.892451995158634,
1.07560298755096));
#413049=CARTESIAN_POINT('Ctrl Pts',(-1.32404072569848,0.730255405911734,
1.08443025522714));
#413050=CARTESIAN_POINT('Ctrl Pts',(-1.46823865828982,0.366681879396492,
1.10462878447799));
#413051=CARTESIAN_POINT('Ctrl Pts',(-1.50403786499845,0.167434914266591,
1.11569806031854));
#413052=CARTESIAN_POINT('Ctrl Pts',(-1.49540721658617,-0.225639333643708,
1.13753551853577));
#413053=CARTESIAN_POINT('Ctrl Pts',(-1.45406788653697,-0.415763779928748,
1.14809798777383));
#413054=CARTESIAN_POINT('Ctrl Pts',(-1.30078525664892,-0.772002631184901,
1.16788903506584));
#413055=CARTESIAN_POINT('Ctrl Pts',(-1.18952605275022,-0.934380352713317,
1.17705724423399));
#413056=CARTESIAN_POINT('Ctrl Pts',(-0.90894711489216,-1.20954569071685,
1.19820008628697));
#413057=CARTESIAN_POINT('Ctrl Pts',(-0.741571552574805,-1.31880719574008,
1.20928798858982));
#413058=CARTESIAN_POINT('Ctrl Pts',(-0.380954539113411,-1.46327655339019,
1.23065122045201));
#413059=CARTESIAN_POINT('Ctrl Pts',(-0.192160135790726,-1.49980121533441,
1.24074916935989));
#413060=CARTESIAN_POINT('Ctrl Pts',(0.19713022252603,-1.50020556531808,
1.25949014240114));
#413061=CARTESIAN_POINT('Ctrl Pts',(0.393978862733631,-1.46093121186798,
1.27004056098599));
#413062=CARTESIAN_POINT('Ctrl Pts',(0.757995919010254,-1.30908048418716,
1.29177241554081));
#413063=CARTESIAN_POINT('Ctrl Pts',(0.922046013593202,-1.19920238796898,
1.30271744873588));
#413064=CARTESIAN_POINT('Ctrl Pts',(1.19492942175059,-0.92646074969302,
1.32342271445107));
#413065=CARTESIAN_POINT('Ctrl Pts',(1.30264695433063,-0.767651402828271,
1.3323526998429));
#413066=CARTESIAN_POINT('Ctrl Pts',(1.45646204507119,-0.410225232893653,
1.35220970928371));
#413067=CARTESIAN_POINT('Ctrl Pts',(1.49795778001533,-0.213707117097209,
1.36312738238351));
#413068=CARTESIAN_POINT('Ctrl Pts',(1.50184059064658,0.17849095181665,1.38491616398984));
#413069=CARTESIAN_POINT('Ctrl Pts',(1.46635459727517,0.370409526770628,
1.39557830704284));
#413070=CARTESIAN_POINT('Ctrl Pts',(1.3244162876751,0.730316542399309,1.41557314124443));
#413071=CARTESIAN_POINT('Ctrl Pts',(1.2192857036431,0.894867051655917,1.4245278406668));
#413072=CARTESIAN_POINT('Ctrl Pts',(0.948738703363631,1.17870384636733,
1.44542889469543));
#413073=CARTESIAN_POINT('Ctrl Pts',(0.784510847160999,1.29382486837113,
1.45652811727779));
#413074=CARTESIAN_POINT('Ctrl Pts',(0.427621011032748,1.45040399534779,
1.47804840771823));
#413075=CARTESIAN_POINT('Ctrl Pts',(0.239490962892949,1.49304999447822,
1.48828442996654));
#413076=CARTESIAN_POINT('Ctrl Pts',(0.0322600286735331,1.49973998657262,
1.4984406660516));
#413077=CARTESIAN_POINT('Ctrl Pts',(0.0161249733935312,1.50000000000006,
1.4992241868559));
#413078=CARTESIAN_POINT('Ctrl Pts',(0.,1.50000000000006,1.50000000000002));
#413079=CARTESIAN_POINT('Origin',(0.,2.5406128344257E-15,14.));
#413080=CARTESIAN_POINT('',(-5.10233297646144E-14,1.50000000000006,2.0625));
#413081=CARTESIAN_POINT('',(-1.01921478372424E-13,1.50000000000006,2.00000000000003));
#413082=CARTESIAN_POINT('',(-1.8369701987211E-16,1.50000000000006,14.));
#413083=CARTESIAN_POINT('Ctrl Pts',(-1.04048714089089E-13,1.50000000000006,
2.0625));
#413084=CARTESIAN_POINT('Ctrl Pts',(0.12517267806619,1.50000000000007,2.05647762671861));
#413085=CARTESIAN_POINT('Ctrl Pts',(0.250086085653614,1.4843361608151,2.05003262094985));
#413086=CARTESIAN_POINT('Ctrl Pts',(0.561115034207491,1.40474810468895,
2.03285745434856));
#413087=CARTESIAN_POINT('Ctrl Pts',(0.739100615817919,1.31980715676613,
2.02193464828504));
#413088=CARTESIAN_POINT('Ctrl Pts',(1.05520352380897,1.08445660057722,2.00018862458367));
#413089=CARTESIAN_POINT('Ctrl Pts',(1.18947775543681,0.935237772913789,
1.98958338516728));
#413090=CARTESIAN_POINT('Ctrl Pts',(1.38770404920368,0.600407544068855,
1.97074537847158));
#413091=CARTESIAN_POINT('Ctrl Pts',(1.45264120120664,0.419637605253057,
1.96081320029176));
#413092=CARTESIAN_POINT('Ctrl Pts',(1.51253906744299,0.0361680336928372,
1.93950933520509));
#413093=CARTESIAN_POINT('Ctrl Pts',(1.5041363021745,-0.163279701360834,
1.92842890547989));
#413094=CARTESIAN_POINT('Ctrl Pts',(1.41094126534843,-0.545470493318642,
1.90719608370446));
#413095=CARTESIAN_POINT('Ctrl Pts',(1.32784413751172,-0.724646312094739,
1.8979235332946));
#413096=CARTESIAN_POINT('Ctrl Pts',(1.09934406827611,-1.03852324259145,
1.87821101496277));
#413097=CARTESIAN_POINT('Ctrl Pts',(0.957083938063734,-1.17092285550576,
1.86768875423129));
#413098=CARTESIAN_POINT('Ctrl Pts',(0.623868722042991,-1.37871374742355,
1.84588496045572));
#413099=CARTESIAN_POINT('Ctrl Pts',(0.434516816534613,-1.44957711310134,
1.83480633582993));
#413100=CARTESIAN_POINT('Ctrl Pts',(0.0482837836795281,-1.51133308800197,
1.8145082466253));
#413101=CARTESIAN_POINT('Ctrl Pts',(-0.144260380713892,-1.50520783480527,
1.80570393127465));
#413102=CARTESIAN_POINT('Ctrl Pts',(-0.520543454270307,-1.4202068029843,
1.7852388636844));
#413103=CARTESIAN_POINT('Ctrl Pts',(-0.700388001592572,-1.34067165157295,
1.77437677910558));
#413104=CARTESIAN_POINT('Ctrl Pts',(-1.02285817948285,-1.11502347609753,
1.75259392056372));
#413105=CARTESIAN_POINT('Ctrl Pts',(-1.16148641546404,-0.969788519798059,
1.74188986210865));
#413106=CARTESIAN_POINT('Ctrl Pts',(-1.369305754301,-0.641164531862946,
1.72276270539765));
#413107=CARTESIAN_POINT('Ctrl Pts',(-1.43944299511357,-0.4627385332705,
1.71320769629275));
#413108=CARTESIAN_POINT('Ctrl Pts',(-1.51065911408002,-0.0821899165916949,
1.69206610647726));
#413109=CARTESIAN_POINT('Ctrl Pts',(-1.50837808077227,0.116802018761552,
1.68101099895764));
#413110=CARTESIAN_POINT('Ctrl Pts',(-1.42693643557648,0.502817858674299,
1.65956567451804));
#413111=CARTESIAN_POINT('Ctrl Pts',(-1.34846371621931,0.686002866464551,
1.649989022283));
#413112=CARTESIAN_POINT('Ctrl Pts',(-1.12811871027367,1.00709126310415,
1.63046854611269));
#413113=CARTESIAN_POINT('Ctrl Pts',(-0.990058164560742,1.14308777164135,
1.62004842421734));
#413114=CARTESIAN_POINT('Ctrl Pts',(-0.663925760947525,1.35978943579843,
1.59833788096152));
#413115=CARTESIAN_POINT('Ctrl Pts',(-0.477317675891636,1.43596823386572,
1.58724361755909));
#413116=CARTESIAN_POINT('Ctrl Pts',(-0.188340196669765,1.49113307834988,
1.57180782531633));
#413117=CARTESIAN_POINT('Ctrl Pts',(-0.0941732849861451,1.50000000000006,
1.56703091428643));
#413118=CARTESIAN_POINT('Ctrl Pts',(0.,1.50000000000006,1.5625));
#413119=CARTESIAN_POINT('',(-1.8369701987211E-16,-1.50000000000005,1.75000000000002));
#413120=CARTESIAN_POINT('Ctrl Pts',(-4.1286418728248E-15,1.50000000000006,
1.50000000000002));
#413121=CARTESIAN_POINT('Ctrl Pts',(-0.184262216122471,1.50000000000006,
1.50886532000667));
#413122=CARTESIAN_POINT('Ctrl Pts',(-0.367118755739811,1.46605100166279,
1.51860603710253));
#413123=CARTESIAN_POINT('Ctrl Pts',(-0.722361712575998,1.32915277951315,
1.53950040022534));
#413124=CARTESIAN_POINT('Ctrl Pts',(-0.8897541949698,1.22343551296505,1.55049066552698));
#413125=CARTESIAN_POINT('Ctrl Pts',(-1.16993138802411,0.957787239945069,
1.57134981570788));
#413126=CARTESIAN_POINT('Ctrl Pts',(-1.28168854585672,0.802094977551391,
1.58043916791386));
#413127=CARTESIAN_POINT('Ctrl Pts',(-1.44492382107869,0.449170364453763,
1.60004609086372));
#413128=CARTESIAN_POINT('Ctrl Pts',(-1.49167494434391,0.253858939542195,
1.61089672558103));
#413129=CARTESIAN_POINT('Ctrl Pts',(-1.50611310936441,-0.138569278761815,
1.63269829326459));
#413130=CARTESIAN_POINT('Ctrl Pts',(-1.47562118216477,-0.331863137943603,
1.64343684099692));
#413131=CARTESIAN_POINT('Ctrl Pts',(-1.34324288372284,-0.694785535748963,
1.66359919643055));
#413132=CARTESIAN_POINT('Ctrl Pts',(-1.24315068270372,-0.861165580826581,
1.67244348435894));
#413133=CARTESIAN_POINT('Ctrl Pts',(-0.98100786127297,-1.15208159054694,
1.69313683700554));
#413134=CARTESIAN_POINT('Ctrl Pts',(-0.81954709883969,-1.27200654544351,
1.70423637030721));
#413135=CARTESIAN_POINT('Ctrl Pts',(-0.53802415872237,-1.40466713678027,
1.72146616550488));
#413136=CARTESIAN_POINT('Ctrl Pts',(-0.431603932160252,-1.44093061146929,
1.72759362978394));
#413137=CARTESIAN_POINT('Ctrl Pts',(-0.216284089425334,-1.48827659240416,
1.73926837668476));
#413138=CARTESIAN_POINT('Ctrl Pts',(-0.10828047712643,-1.50000000000005,
1.74479035311528));
#413139=CARTESIAN_POINT('Ctrl Pts',(-6.34908792207511E-15,-1.50000000000005,
1.75000000000002));
#413140=CARTESIAN_POINT('Ctrl Pts',(-4.71844785465692E-15,-1.50000000000005,
1.75000000000002));
#413141=CARTESIAN_POINT('Ctrl Pts',(0.128403685255941,-1.50000000000005,
1.75617782518731));
#413142=CARTESIAN_POINT('Ctrl Pts',(0.256326208420938,-1.48351384584679,
1.76279044917918));
#413143=CARTESIAN_POINT('Ctrl Pts',(0.509319919036628,-1.41714236576765,
1.77680626698088));
#413144=CARTESIAN_POINT('Ctrl Pts',(0.632935497437535,-1.36641436013271,
1.78416283553733));
#413145=CARTESIAN_POINT('Ctrl Pts',(0.922300322214955,-1.19987495267307,
1.80271100181225));
#413146=CARTESIAN_POINT('Ctrl Pts',(1.07451020764395,-1.06573144674092,
1.81376041183752));
#413147=CARTESIAN_POINT('Ctrl Pts',(1.31068226001403,-0.753875344699292,
1.83378591450625));
#413148=CARTESIAN_POINT('Ctrl Pts',(1.39565079861265,-0.581705867170076,
1.84268300737946));
#413149=CARTESIAN_POINT('Ctrl Pts',(1.49806378045915,-0.20977516263816,
1.8633458242979));
#413150=CARTESIAN_POINT('Ctrl Pts',(1.51262195103989,-0.013009410980133,
1.87427725494557));
#413151=CARTESIAN_POINT('Ctrl Pts',(1.46505908465797,0.378285452977615,
1.89601585849878));
#413152=CARTESIAN_POINT('Ctrl Pts',(1.40210202271853,0.568888986002621,
1.90660494366683));
#413153=CARTESIAN_POINT('Ctrl Pts',(1.20967102284127,0.907157376390545,
1.92539763202172));
#413154=CARTESIAN_POINT('Ctrl Pts',(1.08486195850373,1.05326477583204,1.93539524290294));
#413155=CARTESIAN_POINT('Ctrl Pts',(0.781440253264683,1.2955581387605,1.9567239976952));
#413156=CARTESIAN_POINT('Ctrl Pts',(0.603984679494169,1.3872009278219,1.96780746599849));
#413157=CARTESIAN_POINT('Ctrl Pts',(0.279029618057427,1.48048001337916,
1.98603295939133));
#413158=CARTESIAN_POINT('Ctrl Pts',(0.139733470854763,1.50000000000008,
1.99327707024896));
#413159=CARTESIAN_POINT('Ctrl Pts',(-2.07299455379228E-13,1.50000000000006,
2.00000000000003));
#413160=CARTESIAN_POINT('Origin',(0.,2.5406128344257E-15,14.));
#413161=CARTESIAN_POINT('',(-1.02008187126244E-13,1.50000000000006,2.56250000000001));
#413162=CARTESIAN_POINT('',(-5.10753851888394E-14,1.50000000000006,2.50000000000003));
#413163=CARTESIAN_POINT('',(-1.8369701987211E-16,1.50000000000006,14.));
#413164=CARTESIAN_POINT('Ctrl Pts',(-2.03205507975923E-13,1.50000000000006,
2.56250000000001));
#413165=CARTESIAN_POINT('Ctrl Pts',(0.152713236942429,1.50000000000008,
2.55515258096187));
#413166=CARTESIAN_POINT('Ctrl Pts',(0.30473367800193,1.47668454310575,2.54719084250068));
#413167=CARTESIAN_POINT('Ctrl Pts',(0.638172333335415,1.37161328158764,
2.52822962156282));
#413168=CARTESIAN_POINT('Ctrl Pts',(0.812114721878652,1.27634425022348,
2.51721445250974));
#413169=CARTESIAN_POINT('Ctrl Pts',(1.11579326242716,1.02217281916496,2.49554339438594));
#413170=CARTESIAN_POINT('Ctrl Pts',(1.24170636010353,0.864849575481081,
2.48554719863771));
#413171=CARTESIAN_POINT('Ctrl Pts',(1.42091497161675,0.517363128589665,
2.46624239603264));
#413172=CARTESIAN_POINT('Ctrl Pts',(1.47527571320793,0.331969496264806,
2.45594274979237));
#413173=CARTESIAN_POINT('Ctrl Pts',(1.51207157545589,-0.0566290982231031,
2.43435393898749));
#413174=CARTESIAN_POINT('Ctrl Pts',(1.49124677003707,-0.256436455976549,
2.42325353022342));
#413175=CARTESIAN_POINT('Ctrl Pts',(1.37465850715388,-0.630481773494482,
2.40247323480576));
#413176=CARTESIAN_POINT('Ctrl Pts',(1.28231869436786,-0.801779084055222,
2.39359061239114));
#413177=CARTESIAN_POINT('Ctrl Pts',(1.03728034493493,-1.10070901891445,
2.3734975900056));
#413178=CARTESIAN_POINT('Ctrl Pts',(0.886655461639068,-1.22529149545185,
2.36279002258088));
#413179=CARTESIAN_POINT('Ctrl Pts',(0.541837171242186,-1.4127827946624,
2.3409918532043));
#413180=CARTESIAN_POINT('Ctrl Pts',(0.349959198744996,-1.47210419758972,
2.33011230320026));
#413181=CARTESIAN_POINT('Ctrl Pts',(-0.0369745037304581,-1.5115377391189,
2.31040057060645));
#413182=CARTESIAN_POINT('Ctrl Pts',(-0.227963124566986,-1.49470983444342,
2.30138517001216));
#413183=CARTESIAN_POINT('Ctrl Pts',(-0.599163506202012,-1.38901960020766,
2.28058994348392));
#413184=CARTESIAN_POINT('Ctrl Pts',(-0.775238772760863,-1.29898915396473,
2.26961767254284));
#413185=CARTESIAN_POINT('Ctrl Pts',(-1.08516059471296,-1.05450253849513,
2.24791525705771));
#413186=CARTESIAN_POINT('Ctrl Pts',(-1.21520066557894,-0.901546538308134,
2.2375859187948));
#413187=CARTESIAN_POINT('Ctrl Pts',(-1.40424756528659,-0.560832488679741,
2.21865736048212));
#413188=CARTESIAN_POINT('Ctrl Pts',(-1.46414026274044,-0.377775002516861,
2.20848750013974));
#413189=CARTESIAN_POINT('Ctrl Pts',(-1.51302509452222,0.0082595196597254,
2.1870411377966));
#413190=CARTESIAN_POINT('Ctrl Pts',(-1.49868835278631,0.207972947953393,
2.17594594733584));
#413191=CARTESIAN_POINT('Ctrl Pts',(-1.39424969182913,0.586335583316973,
2.15492580092676));
#413192=CARTESIAN_POINT('Ctrl Pts',(-1.30672083828862,0.761706235670994,
2.1458777957653));
#413193=CARTESIAN_POINT('Ctrl Pts',(-1.07032415199273,1.06850094754418,
2.12598207956313));
#413194=CARTESIAN_POINT('Ctrl Pts',(-0.924041350037075,1.19725506618534,
2.11536754167697));
#413195=CARTESIAN_POINT('Ctrl Pts',(-0.584120040911811,1.39610344662897,
2.09348950394298));
#413196=CARTESIAN_POINT('Ctrl Pts',(-0.392221943321926,1.4616704545275,
2.08243549664298));
#413197=CARTESIAN_POINT('Ctrl Pts',(-0.12893753989064,1.49584792717374,
2.0688188456366));
#413198=CARTESIAN_POINT('Ctrl Pts',(-0.064440010018234,1.50000000000005,
2.06560037142755));
#413199=CARTESIAN_POINT('Ctrl Pts',(-1.01862962509357E-13,1.50000000000006,
2.0625));
#413200=CARTESIAN_POINT('Ctrl Pts',(-2.03659259724975E-13,1.50000000000006,
2.00000000000003));
#413201=CARTESIAN_POINT('Ctrl Pts',(-0.0549400060433684,1.50000000000005,
2.00264330227322));
#413202=CARTESIAN_POINT('Ctrl Pts',(-0.10993950796974,1.4969818263819,2.00537330519949));
#413203=CARTESIAN_POINT('Ctrl Pts',(-0.356253708025767,1.46976303075573,
2.0179801803314));
#413204=CARTESIAN_POINT('Ctrl Pts',(-0.5418707719965,1.41190599495831,2.02851782536881));
#413205=CARTESIAN_POINT('Ctrl Pts',(-0.887743372098913,1.2255665984787,
2.05033472294666));
#413206=CARTESIAN_POINT('Ctrl Pts',(-1.04326496929328,1.09622775919434,
2.06141000481609));
#413207=CARTESIAN_POINT('Ctrl Pts',(-1.28841412800607,0.791459185658804,
2.08167054292328));
#413208=CARTESIAN_POINT('Ctrl Pts',(-1.37854213118331,0.621323847434963,
2.09048200847586));
#413209=CARTESIAN_POINT('Ctrl Pts',(-1.49139348533716,0.25245302547749,
2.11097483191794));
#413210=CARTESIAN_POINT('Ctrl Pts',(-1.51154154601725,0.0567500141491085,
2.12184722143618));
#413211=CARTESIAN_POINT('Ctrl Pts',(-1.47550519730677,-0.335258481026087,
2.14362547116814));
#413212=CARTESIAN_POINT('Ctrl Pts',(-1.41813792564057,-0.527658291165775,
2.15431434950923));
#413213=CARTESIAN_POINT('Ctrl Pts',(-1.23582029636045,-0.871121096433655,
2.17339561646856));
#413214=CARTESIAN_POINT('Ctrl Pts',(-1.11563285200374,-1.02054026590828,
2.1830057634346));
#413215=CARTESIAN_POINT('Ctrl Pts',(-0.820371101776589,-1.2711706465811,
2.20417350603454));
#413216=CARTESIAN_POINT('Ctrl Pts',(-0.646339631367295,-1.36789256596225,
2.21523331904138));
#413217=CARTESIAN_POINT('Ctrl Pts',(-0.270899415401483,-1.48844644321116,
2.23664541366655));
#413218=CARTESIAN_POINT('Ctrl Pts',(-0.0732069894380748,-1.51111961532319,
2.24616894887505));
#413219=CARTESIAN_POINT('Ctrl Pts',(0.314698002855619,-1.47914902699323,
2.2657201084165));
#413220=CARTESIAN_POINT('Ctrl Pts',(0.501354739620307,-1.4267237235383,
2.27615689328056));
#413221=CARTESIAN_POINT('Ctrl Pts',(0.851451281918399,-1.25095683228224,
2.29788333467141));
#413222=CARTESIAN_POINT('Ctrl Pts',(1.01022792711823,-1.1266385612444,2.30897576488195));
#413223=CARTESIAN_POINT('Ctrl Pts',(1.26453115601539,-0.82925932324522,
2.32947146907578));
#413224=CARTESIAN_POINT('Ctrl Pts',(1.35999298008976,-0.661157855585676,
2.33826900802304));
#413225=CARTESIAN_POINT('Ctrl Pts',(1.48339858266622,-0.295467457128719,
2.35858514127065));
#413226=CARTESIAN_POINT('Ctrl Pts',(1.50915889939786,-0.100999143947135,
2.3693889364474));
#413227=CARTESIAN_POINT('Ctrl Pts',(1.48479726843207,0.291384690358864,
2.39118803835329));
#413228=CARTESIAN_POINT('Ctrl Pts',(1.43314552716761,0.485431988898048,
2.40196844382769));
#413229=CARTESIAN_POINT('Ctrl Pts',(1.26111558532972,0.834051958767407,
2.42133621993154));
#413230=CARTESIAN_POINT('Ctrl Pts',(1.14551706690535,0.986847410654543,
2.43063204582883));
#413231=CARTESIAN_POINT('Ctrl Pts',(0.858439019841868,1.24568575260506,
2.45163404875111));
#413232=CARTESIAN_POINT('Ctrl Pts',(0.687961617920957,1.3473522652111,2.46266021636987));
#413233=CARTESIAN_POINT('Ctrl Pts',(0.341125347611844,1.47073361724696,
2.48277464398429));
#413234=CARTESIAN_POINT('Ctrl Pts',(0.171090208316003,1.50000000000007,
2.49176841851444));
#413235=CARTESIAN_POINT('Ctrl Pts',(-1.0325074129014E-13,1.50000000000006,
2.50000000000003));
#413236=CARTESIAN_POINT('Origin',(0.,2.5406128344257E-15,14.));
#413237=CARTESIAN_POINT('',(6.67357304637349E-15,1.50000000000006,3.0625));
#413238=CARTESIAN_POINT('',(-9.18485099360549E-17,1.50000000000006,3.00000000000002));
#413239=CARTESIAN_POINT('',(-1.8369701987211E-16,1.50000000000006,14.));
#413240=CARTESIAN_POINT('Ctrl Pts',(3.64291929955129E-15,1.50000000000006,
3.0625));
#413241=CARTESIAN_POINT('Ctrl Pts',(0.182882853306852,1.50000000000006,
3.05370104461776));
#413242=CARTESIAN_POINT('Ctrl Pts',(0.364344307785531,1.46655523112887,
3.04404145496085));
#413243=CARTESIAN_POINT('Ctrl Pts',(0.719999996592976,1.33065906568766,
3.02315506917039));
#413244=CARTESIAN_POINT('Ctrl Pts',(0.888860395184684,1.224330073046,3.01207718632626));
#413245=CARTESIAN_POINT('Ctrl Pts',(1.17437618710092,0.953526175329834,
2.99081797089076));
#413246=CARTESIAN_POINT('Ctrl Pts',(1.28870083644925,0.792218373209365,
2.98151213184482));
#413247=CARTESIAN_POINT('Ctrl Pts',(1.44754363339846,0.437813070668275,
2.96182294837032));
#413248=CARTESIAN_POINT('Ctrl Pts',(1.49171964063901,0.248630694274393,
2.95131281634844));
#413249=CARTESIAN_POINT('Ctrl Pts',(1.50645258404152,-0.143648281191507,
2.92951953993367));
#413250=CARTESIAN_POINT('Ctrl Pts',(1.47388129179558,-0.343107440067577,
2.91843847555167));
#413251=CARTESIAN_POINT('Ctrl Pts',(1.33559504363155,-0.708997785802925,
2.89811123412193));
#413252=CARTESIAN_POINT('Ctrl Pts',(1.23456394643513,-0.873124364491001,
2.88931119766451));
#413253=CARTESIAN_POINT('Ctrl Pts',(0.973799092840822,-1.15742887662232,
2.86886779523715));
#413254=CARTESIAN_POINT('Ctrl Pts',(0.815472175779737,-1.27393959786869,
2.85801387896488));
#413255=CARTESIAN_POINT('Ctrl Pts',(0.459490510962695,-1.44166101725917,
2.83622777481443));
#413256=CARTESIAN_POINT('Ctrl Pts',(0.26456989253311,-1.48981367055675,
2.82551207848497));
#413257=CARTESIAN_POINT('Ctrl Pts',(-0.123856795158379,-1.50689770288092,
2.8063493343066));
#413258=CARTESIAN_POINT('Ctrl Pts',(-0.313522320195767,-1.47912677479024,
2.79683583852498));
#413259=CARTESIAN_POINT('Ctrl Pts',(-0.679073137343345,-1.35191598287377,
2.77571463352598));
#413260=CARTESIAN_POINT('Ctrl Pts',(-0.850581476939661,-1.25113107802357,
2.76466335399951));
#413261=CARTESIAN_POINT('Ctrl Pts',(-1.14528857231865,-0.98862407240659,
2.74319239099495));
#413262=CARTESIAN_POINT('Ctrl Pts',(-1.26541405236657,-0.829319266629043,
2.73357329259036));
#413263=CARTESIAN_POINT('Ctrl Pts',(-1.43457743682025,-0.478379997782074,
2.71407666654331));
#413264=CARTESIAN_POINT('Ctrl Pts',(-1.48395695812464,-0.291052487239219,
2.70366958262427));
#413265=CARTESIAN_POINT('Ctrl Pts',(-1.50993158675046,0.0995103046966565,
2.68197164973895));
#413266=CARTESIAN_POINT('Ctrl Pts',(-1.48333044076327,0.299229642968109,
2.67087613094609));
#413267=CARTESIAN_POINT('Ctrl Pts',(-1.35603134593058,0.669317429512583,
2.65031569836029));
#413268=CARTESIAN_POINT('Ctrl Pts',(-1.25941917298638,0.83706039188798,
2.64150882232628));
#413269=CARTESIAN_POINT('Ctrl Pts',(-1.00666608391223,1.12886512042551,
2.6212425467545));
#413270=CARTESIAN_POINT('Ctrl Pts',(-0.852227140816204,1.24956407323514,
2.61045935095119));
#413271=CARTESIAN_POINT('Ctrl Pts',(-0.501815166956722,1.4274848830235,
2.58865790228193));
#413272=CARTESIAN_POINT('Ctrl Pts',(-0.308367856338849,1.48137183976405,
2.57785380430087));
#413273=CARTESIAN_POINT('Ctrl Pts',(-0.0733611638817185,1.49865591149239,
2.56606692643469));
#413274=CARTESIAN_POINT('Ctrl Pts',(-0.0366624048499707,1.50000000000005,
2.56426392077577));
#413275=CARTESIAN_POINT('Ctrl Pts',(-2.03832677232616E-13,1.50000000000006,
2.56250000000001));
#413276=CARTESIAN_POINT('Ctrl Pts',(-1.01967073357807E-13,1.50000000000006,
2.50000000000003));
#413277=CARTESIAN_POINT('Ctrl Pts',(-0.0274177145351737,1.50000000000006,
2.50131913540564));
#413278=CARTESIAN_POINT('Ctrl Pts',(-0.0548605401926219,1.49924828163703,
2.50266036003634));
#413279=CARTESIAN_POINT('Ctrl Pts',(-0.273628599396303,1.48722738833696,
2.51351975689506));
#413280=CARTESIAN_POINT('Ctrl Pts',(-0.461154186550479,1.4401504841588,
2.5238497776964));
#413281=CARTESIAN_POINT('Ctrl Pts',(-0.815094499336094,1.27485332480795,
2.5454703266948));
#413282=CARTESIAN_POINT('Ctrl Pts',(-0.976917197504026,1.15554005927025,
2.55657028226653));
#413283=CARTESIAN_POINT('Ctrl Pts',(-1.24013964613848,0.865524440878566,
2.57729056763096));
#413284=CARTESIAN_POINT('Ctrl Pts',(-1.34087450658538,0.699380283990824,
2.58614553977831));
#413285=CARTESIAN_POINT('Ctrl Pts',(-1.47448412598132,0.336842361844777,
2.60628653545309));
#413286=CARTESIAN_POINT('Ctrl Pts',(-1.50562215511498,0.143718511421741,
2.61701563825437));
#413287=CARTESIAN_POINT('Ctrl Pts',(-1.49254483650425,-0.248696103796777,
2.63881645021095));
#413288=CARTESIAN_POINT('Ctrl Pts',(-1.44646879082916,-0.444171099187499,
2.6496761721771));
#413289=CARTESIAN_POINT('Ctrl Pts',(-1.28444391432844,-0.797680502985018,
2.66931558349919));
#413290=CARTESIAN_POINT('Ctrl Pts',(-1.17320997448533,-0.953772395014446,
2.67838091975722));
#413291=CARTESIAN_POINT('Ctrl Pts',(-0.893975630318868,-1.2203435216428,
2.6992203419223));
#413292=CARTESIAN_POINT('Ctrl Pts',(-0.727010595442072,-1.32660567225268,
2.71020517731408));
#413293=CARTESIAN_POINT('Ctrl Pts',(-0.359020312185557,-1.46991806658127,
2.73189101791465));
#413294=CARTESIAN_POINT('Ctrl Pts',(-0.161238567423123,-1.50449720087997,
2.74211748356123));
#413295=CARTESIAN_POINT('Ctrl Pts',(0.228464169802661,-1.49475941767255,
2.76113755922599));
#413296=CARTESIAN_POINT('Ctrl Pts',(0.416766918687362,-1.45354179816621,
2.77134221333097));
#413297=CARTESIAN_POINT('Ctrl Pts',(0.774562466398808,-1.29978160830849,
2.79282777603141));
#413298=CARTESIAN_POINT('Ctrl Pts',(0.93954294283116,-1.1860208389091,2.80392542427689));
#413299=CARTESIAN_POINT('Ctrl Pts',(1.21243949942647,-0.904192764779027,
2.82488372359255));
#413300=CARTESIAN_POINT('Ctrl Pts',(1.3189938637598,-0.740151664975824,
2.83388046305692));
#413301=CARTESIAN_POINT('Ctrl Pts',(1.46359518940313,-0.38109696698799,
2.85382794627847));
#413302=CARTESIAN_POINT('Ctrl Pts',(1.50046270778976,-0.189583912945483,
2.86446756039169));
#413303=CARTESIAN_POINT('Ctrl Pts',(1.49952874275399,0.196746644945994,
2.88593036916345));
#413304=CARTESIAN_POINT('Ctrl Pts',(1.46177059901948,0.387992437134483,
2.89655513539638));
#413305=CARTESIAN_POINT('Ctrl Pts',(1.31544793633266,0.746493348129332,
2.91647185267387));
#413306=CARTESIAN_POINT('Ctrl Pts',(1.20796845018551,0.910205053758987,
2.92549839789162));
#413307=CARTESIAN_POINT('Ctrl Pts',(0.933551340114328,1.19072603442544,
2.94649354671873));
#413308=CARTESIAN_POINT('Ctrl Pts',(0.768088770422058,1.30360253054627,
2.95758982654036));
#413309=CARTESIAN_POINT('Ctrl Pts',(0.409717686637218,1.45553271405181,
2.97905224622326));
#413310=CARTESIAN_POINT('Ctrl Pts',(0.221308716892194,1.49582417711568,
2.98923628431392));
#413311=CARTESIAN_POINT('Ctrl Pts',(0.0202523014979187,1.49989750363487,
2.99902276356864));
#413312=CARTESIAN_POINT('Ctrl Pts',(0.010124057874074,1.50000000000006,
2.99951290603844));
#413313=CARTESIAN_POINT('Ctrl Pts',(0.,1.50000000000006,3.00000000000002));
#413314=CARTESIAN_POINT('Origin',(0.,2.5406128344257E-15,14.));
#413315=CARTESIAN_POINT('',(-1.8369701987211E-16,1.50000000000006,10.875));
#413316=CARTESIAN_POINT('Origin',(0.,2.12729453971344E-15,10.875));
#413317=CARTESIAN_POINT('',(-1.8369701987211E-16,1.50000000000006,14.));
#413318=CARTESIAN_POINT('',(1.05094390383309,1.07028823734368,4.));
#413319=CARTESIAN_POINT('Origin',(0.,2.96923921412725E-15,4.));
#413320=CARTESIAN_POINT('',(2.54005801708804E-14,1.50000000000006,3.56249999999999));
#413321=CARTESIAN_POINT('Ctrl Pts',(1.05094390383236,1.0702882373444,4.00000000000005));
#413322=CARTESIAN_POINT('Ctrl Pts',(1.13819986706457,0.98460933381889,3.9934219259693));
#413323=CARTESIAN_POINT('Ctrl Pts',(1.21465675291404,0.888578028464408,
3.98707585607391));
#413324=CARTESIAN_POINT('Ctrl Pts',(1.34189007761835,0.681157619080558,
3.97519266184647));
#413325=CARTESIAN_POINT('Ctrl Pts',(1.3924635746937,0.570707296225168,3.96920596090126));
#413326=CARTESIAN_POINT('Ctrl Pts',(1.48831628150228,0.269842273341566,
3.95249123740774));
#413327=CARTESIAN_POINT('Ctrl Pts',(1.5107358108084,0.0746185298859356,
3.94164547388242));
#413328=CARTESIAN_POINT('Ctrl Pts',(1.47941220484531,-0.317583526733779,
3.91985647073689));
#413329=CARTESIAN_POINT('Ctrl Pts',(1.42434561767773,-0.510669207825729,
3.90912948845401));
#413330=CARTESIAN_POINT('Ctrl Pts',(1.24617432945898,-0.856226129726136,
3.88993188168177));
#413331=CARTESIAN_POINT('Ctrl Pts',(1.12784943062945,-1.00700480087526,
3.88045799211828));
#413332=CARTESIAN_POINT('Ctrl Pts',(0.835900384523997,-1.26097554236673,
3.85935684426919));
#413333=CARTESIAN_POINT('Ctrl Pts',(0.663293475671837,-1.3597172074586,
3.84830946646471));
#413334=CARTESIAN_POINT('Ctrl Pts',(0.288927509018431,-1.48515116315491,
3.82681349894903));
#413335=CARTESIAN_POINT('Ctrl Pts',(0.0907596703675172,-1.51026295578127,
3.81715175878143));
#413336=CARTESIAN_POINT('Ctrl Pts',(-0.297998583554222,-1.4825762872731,
3.79767854444359));
#413337=CARTESIAN_POINT('Ctrl Pts',(-0.485027444519739,-1.43232807704285,
3.78728433055736));
#413338=CARTESIAN_POINT('Ctrl Pts',(-0.836726191001619,-1.26081585576662,
3.765598988359));
#413339=CARTESIAN_POINT('Ctrl Pts',(-0.996761692002802,-1.13852756988451,
3.75450237989703));
#413340=CARTESIAN_POINT('Ctrl Pts',(-1.25470601413975,-0.844134566990372,
3.73391444449817));
#413341=CARTESIAN_POINT('Ctrl Pts',(-1.35231124109025,-0.676834035612717,
3.72510189086725));
#413342=CARTESIAN_POINT('Ctrl Pts',(-1.47989147440158,-0.312424518808318,
3.70485691771146));
#413343=CARTESIAN_POINT('Ctrl Pts',(-1.5078582402593,-0.118488502263773,
3.6940826945701));
#413344=CARTESIAN_POINT('Ctrl Pts',(-1.4881148687202,0.273947391756074,
3.67228070045789));
#413345=CARTESIAN_POINT('Ctrl Pts',(-1.43873897053923,0.46859859659788,
3.66146674463334));
#413346=CARTESIAN_POINT('Ctrl Pts',(-1.27079537012017,0.819230759889241,
3.64198718000605));
#413347=CARTESIAN_POINT('Ctrl Pts',(-1.15699057424196,0.973370756955023,
3.63279432504184));
#413348=CARTESIAN_POINT('Ctrl Pts',(-0.873129892992125,1.23539635915665,
3.61185858269747));
#413349=CARTESIAN_POINT('Ctrl Pts',(-0.704081077148935,1.33896510422339,
3.60084830816784));
#413350=CARTESIAN_POINT('Ctrl Pts',(-0.353261863578898,1.46859190696227,
3.58036876636469));
#413351=CARTESIAN_POINT('Ctrl Pts',(-0.177236729236581,1.50000000000006,
3.57102730611125));
#413352=CARTESIAN_POINT('Ctrl Pts',(4.85722573273506E-14,1.50000000000006,
3.5625));
#413353=CARTESIAN_POINT('',(1.27227548117872E-13,1.50000000000006,3.50000000000001));
#413354=CARTESIAN_POINT('',(-1.8369701987211E-16,1.50000000000006,14.));
#413355=CARTESIAN_POINT('Ctrl Pts',(2.56704379975048E-13,1.50000000000006,
3.50000000000001));
#413356=CARTESIAN_POINT('Ctrl Pts',(-0.158046323335796,1.50000000000006,
3.50760400727687));
#413357=CARTESIAN_POINT('Ctrl Pts',(-0.315330238810465,1.4750274495662,
3.51586501514492));
#413358=CARTESIAN_POINT('Ctrl Pts',(-0.653374864141001,1.36453160991631,
3.53519852364348));
#413359=CARTESIAN_POINT('Ctrl Pts',(-0.826818998759573,1.26697063414261,
3.54625338556592));
#413360=CARTESIAN_POINT('Ctrl Pts',(-1.12070945700276,1.01495450578277,
3.56739364484083));
#413361=CARTESIAN_POINT('Ctrl Pts',(-1.24012502110656,0.864973703597631,
3.57694590535571));
#413362=CARTESIAN_POINT('Ctrl Pts',(-1.42072919648182,0.52064298505673,
3.59607538971909));
#413363=CARTESIAN_POINT('Ctrl Pts',(-1.4771462620762,0.327956166591618,
3.60678021296716));
#413364=CARTESIAN_POINT('Ctrl Pts',(-1.51123400863953,-0.0641392666801464,
3.62856329259336));
#413365=CARTESIAN_POINT('Ctrl Pts',(-1.49014576997854,-0.259647257636294,
3.63942484764648));
#413366=CARTESIAN_POINT('Ctrl Pts',(-1.37553208625951,-0.627993035281357,
3.6598885019601));
#413367=CARTESIAN_POINT('Ctrl Pts',(-1.28452190376951,-0.797787326061387,
3.66869250348051));
#413368=CARTESIAN_POINT('Ctrl Pts',(-1.03784945108146,-1.10133792947263,
3.6889924985998));
#413369=CARTESIAN_POINT('Ctrl Pts',(-0.881777476509032,-1.22984971864792,
3.70007128689903));
#413370=CARTESIAN_POINT('Ctrl Pts',(-0.535182924356041,-1.41444249945224,
3.72187440230903));
#413371=CARTESIAN_POINT('Ctrl Pts',(-0.349382661133372,-1.47140002254497,
3.73239587506053));
#413372=CARTESIAN_POINT('Ctrl Pts',(0.0367104195384525,-1.51226310178053,
3.75210687259969));
#413373=CARTESIAN_POINT('Ctrl Pts',(0.233438879771808,-1.49459180630664,
3.76138156094225));
#413374=CARTESIAN_POINT('Ctrl Pts',(0.611003620457198,-1.3841094382759,
3.7826161076657));
#413375=CARTESIAN_POINT('Ctrl Pts',(0.787904850030921,-1.29162169817824,
3.7936963759335));
#413376=CARTESIAN_POINT('Ctrl Pts',(1.08998526853455,-1.0479469575977,3.81499896963907));
#413377=CARTESIAN_POINT('Ctrl Pts',(1.21403107573361,-0.901298500932676,
3.82492786105932));
#413378=CARTESIAN_POINT('Ctrl Pts',(1.40480917993946,-0.562172842280676,
3.84376817542888));
#413379=CARTESIAN_POINT('Ctrl Pts',(1.46685510831189,-0.371263810872641,
3.85437423272932));
#413380=CARTESIAN_POINT('Ctrl Pts',(1.51253167011941,0.0201712061737881,
3.87612062256523));
#413381=CARTESIAN_POINT('Ctrl Pts',(1.49705537048712,0.216773695591539,
3.88704298308844));
#413382=CARTESIAN_POINT('Ctrl Pts',(1.39293210601042,0.58820894756761,3.90767827486489));
#413383=CARTESIAN_POINT('Ctrl Pts',(1.307125692317,0.760043369025171,3.91655653494596));
#413384=CARTESIAN_POINT('Ctrl Pts',(1.06948823490166,1.07075281541671,3.93662069040197));
#413385=CARTESIAN_POINT('Ctrl Pts',(0.916729933887096,1.2041201811228,3.94767492663366));
#413386=CARTESIAN_POINT('Ctrl Pts',(0.627705282594136,1.36871201538997,
3.96615262704884));
#413387=CARTESIAN_POINT('Ctrl Pts',(0.505012804915808,1.4185740311113,3.9734407276257));
#413388=CARTESIAN_POINT('Ctrl Pts',(0.25408959443158,1.4838014838608,3.98732514990643));
#413389=CARTESIAN_POINT('Ctrl Pts',(0.127278690505086,1.50000000000006,
3.99387630114792));
#413390=CARTESIAN_POINT('Ctrl Pts',(2.56739074444567E-14,1.50000000000006,
4.00000000000002));
#413391=CARTESIAN_POINT('Origin',(1.05441810806075E-15,7.08435492480263E-16,
12.4908873016278));
#413392=CARTESIAN_POINT('',(2.29888601477292,1.49740593435477,12.5064436508139));
#413393=CARTESIAN_POINT('',(2.25522951324155,1.56238320643934,12.5064436508139));
#413394=CARTESIAN_POINT('Origin',(4.27850903389135E-31,-2.27990188045099E-31,
12.5064436508139));
#413395=CARTESIAN_POINT('',(2.30428529106063,1.50092281527121,12.4908873016278));
#413396=CARTESIAN_POINT('Origin',(2.28585100873214,1.48891543274904,12.4908873016278));
#413397=CARTESIAN_POINT('',(2.26052625573157,1.56605269615942,12.4908873016278));
#413398=CARTESIAN_POINT('Origin',(2.10883621612149E-15,1.41687098496053E-15,
12.4908873016278));
#413399=CARTESIAN_POINT('Origin',(2.24244204568572,1.55352427459015,12.4908873016278));
#413400=CARTESIAN_POINT('Origin',(1.10865368822092E-15,6.20133367273767E-16,
12.4908873016278));
#413401=CARTESIAN_POINT('',(2.41328914609189,1.30504288761499,12.5064436508139));
#413402=CARTESIAN_POINT('',(2.37507415886241,1.37336236334895,12.5064436508139));
#413403=CARTESIAN_POINT('Origin',(4.49858057657419E-31,-2.63820513560149E-31,
12.5064436508139));
#413404=CARTESIAN_POINT('',(2.41895711517698,1.30810797525842,12.4908873016278));
#413405=CARTESIAN_POINT('Origin',(2.39960545825556,1.29764311145636,12.4908873016278));
#413406=CARTESIAN_POINT('',(2.38065237435682,1.3765879094592,12.4908873016278));
#413407=CARTESIAN_POINT('Origin',(2.21730737644184E-15,1.24026673454754E-15,
12.4908873016278));
#413408=CARTESIAN_POINT('Origin',(2.36160715536196,1.36557520618352,12.4908873016278));
#413409=CARTESIAN_POINT('Origin',(1.15551136100097E-15,5.27704356822869E-16,
12.4908873016278));
#413410=CARTESIAN_POINT('',(2.5116322363083,1.10399499577506,12.5064436508139));
#413411=CARTESIAN_POINT('',(2.47911307781569,1.17520202031931,12.5064436508139));
#413412=CARTESIAN_POINT('Origin',(4.68871480773348E-31,-3.01325404000159E-31,
12.5064436508139));
#413413=CARTESIAN_POINT('',(2.51753117879165,1.10658789249292,12.4908873016278));
#413414=CARTESIAN_POINT('Origin',(2.49739092936132,1.09773518935297,12.4908873016278));
#413415=CARTESIAN_POINT('',(2.48493564421071,1.17796215734254,12.4908873016278));
#413416=CARTESIAN_POINT('Origin',(2.31102272200194E-15,1.05540871364574E-15,
12.4908873016278));
#413417=CARTESIAN_POINT('Origin',(2.46505615905703,1.1685384600838,12.4908873016278));
#413418=CARTESIAN_POINT('Origin',(1.19467929631951E-15,4.31763560942405E-16,
12.4908873016278));
#413419=CARTESIAN_POINT('',(2.59326082838222,0.895600199384597,12.5064436508139));
#413420=CARTESIAN_POINT('',(2.56665390826098,0.969220901739124,12.5064436508139));
#413421=CARTESIAN_POINT('Origin',(4.8476464154308E-31,-3.40255270507121E-31,
12.5064436508139));
#413422=CARTESIAN_POINT('',(2.59935148777488,0.897703649877022,12.4908873016278));
#413423=CARTESIAN_POINT('Origin',(2.57855667587268,0.890522020678006,12.4908873016278));
#413424=CARTESIAN_POINT('',(2.57268207733791,0.971497261418848,12.4908873016278));
#413425=CARTESIAN_POINT('Origin',(2.38935859263903E-15,8.63527121884811E-16,
12.4908873016278));
#413426=CARTESIAN_POINT('Origin',(2.5521006207192,0.963725283327497,12.4908873016278));
#413427=CARTESIAN_POINT('Origin',(1.22589683802926E-15,3.32949449799843E-16,
12.4908873016278));
#413428=CARTESIAN_POINT('',(2.65763169750119,0.681245331430862,12.5064436508139));
#413429=CARTESIAN_POINT('',(2.63711408041488,0.756789777968061,12.5064436508139));
#413430=CARTESIAN_POINT('Origin',(4.97431773603878E-31,-3.80351041242409E-31,
12.5064436508139));
#413431=CARTESIAN_POINT('',(2.66387354146977,0.682845337581871,12.4908873016278));
#413432=CARTESIAN_POINT('Origin',(2.64256255313801,0.677382574881216,12.4908873016278));
#413433=CARTESIAN_POINT('',(2.64330773570308,0.758567211506177,12.4908873016278));
#413434=CARTESIAN_POINT('Origin',(2.45179367605852E-15,6.65898899599686E-16,
12.4908873016278));
#413435=CARTESIAN_POINT('Origin',(2.62216127381746,0.752498673814127,12.4908873016278));
#413436=CARTESIAN_POINT('Origin',(1.24895623854066E-15,2.31919615001655E-16,
12.4908873016278));
#413437=CARTESIAN_POINT('',(2.70431646615165,0.462356888194023,12.5064436508139));
#413438=CARTESIAN_POINT('',(2.69002469345682,0.539322343086144,12.5064436508139));
#413439=CARTESIAN_POINT('Origin',(5.06788579281809E-31,-4.21345885467116E-31,
12.5064436508139));
#413440=CARTESIAN_POINT('',(2.71066795625438,0.463442802226664,12.4908873016278));
#413441=CARTESIAN_POINT('Origin',(2.68898261260435,0.45973525980885,12.4908873016278));
#413442=CARTESIAN_POINT('',(2.69634261720223,0.540589021955712,12.4908873016278));
#413443=CARTESIAN_POINT('Origin',(2.49791247708132E-15,4.63839230003311E-16,
12.4908873016278));
#413444=CARTESIAN_POINT('Origin',(2.67477187626461,0.536264309780066,12.4908873016278));
#413445=CARTESIAN_POINT('Origin',(1.26370404134785E-15,1.29346393429673E-16,
12.4908873016278));
#413446=CARTESIAN_POINT('',(2.73300445490068,0.240391536149767,12.5064436508139));
#413447=CARTESIAN_POINT('',(2.72503363598663,0.318265806992911,12.5064436508139));
#413448=CARTESIAN_POINT('Origin',(5.12772790578849E-31,-4.62966989256598E-31,
12.5064436508139));
#413449=CARTESIAN_POINT('',(2.73942332301885,0.240956131485315,12.4908873016278));
#413450=CARTESIAN_POINT('Origin',(2.7175079364347,0.239028482433433,12.4908873016278));
#413451=CARTESIAN_POINT('',(2.73143378344912,0.31901330165504,12.4908873016278));
#413452=CARTESIAN_POINT('Origin',(2.5274080826957E-15,2.58692786859347E-16,
12.4908873016278));
#413453=CARTESIAN_POINT('Origin',(2.70958231318152,0.316461195241799,12.4908873016278));
#413454=CARTESIAN_POINT('Origin',(1.27004210225636E-15,2.59123929500705E-17,
12.4908873016278));
#413455=CARTESIAN_POINT('',(2.74350474991634,0.0168264180942478,12.5064436508139));
#413456=CARTESIAN_POINT('',(2.74190792926786,0.0950912644643034,12.5064436508139));
#413457=CARTESIAN_POINT('Origin',(5.15344583556142E-31,-5.04937371032137E-31,
12.5064436508139));
#413458=CARTESIAN_POINT('',(2.74994827954166,0.0168659374438978,12.4908873016278));
#413459=CARTESIAN_POINT('Origin',(2.72794869330533,0.0167310099443466,12.4908873016278));
#413460=CARTESIAN_POINT('',(2.748347708522,0.0953146004653459,12.4908873016278));
#413461=CARTESIAN_POINT('Origin',(2.54008420451272E-15,5.18247859001415E-17,
12.4908873016278));
#413462=CARTESIAN_POINT('Origin',(2.72636092685383,0.0945520836616232,12.4908873016278));
#413463=CARTESIAN_POINT('Origin',(1.26792824251655E-15,-7.76940502293709E-17,
12.4908873016278));
#413464=CARTESIAN_POINT('',(2.73574747346773,-0.206850676997525,12.5064436508139));
#413465=CARTESIAN_POINT('',(2.74053527766277,-0.128716094740359,12.5064436508139));
#413466=CARTESIAN_POINT('Origin',(5.1448684335574E-31,-5.4697772482764E-31,
12.5064436508139));
#413467=CARTESIAN_POINT('',(2.74217278397365,-0.207336496628525,12.4908873016278));
#413468=CARTESIAN_POINT('Origin',(2.72023540170186,-0.205677804655497,12.4908873016278));
#413469=CARTESIAN_POINT('',(2.74697183304013,-0.129018403664643,12.4908873016278));
#413470=CARTESIAN_POINT('Origin',(2.5358564850331E-15,-1.55388100458741E-16,
12.4908873016278));
#413471=CARTESIAN_POINT('Origin',(2.72499605837581,-0.127986256435326,12.4908873016278));
#413472=CARTESIAN_POINT('Origin',(1.25737652951623E-15,-1.80783452323152E-16,
12.4908873016278));
#413473=CARTESIAN_POINT('',(2.70978424894975,-0.429151214961838,12.5064436508139));
#413474=CARTESIAN_POINT('',(2.72092481594134,-0.351666869571186,12.5064436508139));
#413475=CARTESIAN_POINT('Origin',(5.1020527809716E-31,-5.8880827902477E-31,
12.5064436508139));
#413476=CARTESIAN_POINT('',(2.71614858095496,-0.430159140523999,12.4908873016278));
#413477=CARTESIAN_POINT('Origin',(2.69441939230732,-0.426717867399807,12.4908873016278));
#413478=CARTESIAN_POINT('',(2.72731531322782,-0.352492811604782,12.4908873016278));
#413479=CARTESIAN_POINT('Origin',(2.51475305903246E-15,-3.61566904646303E-16,
12.4908873016278));
#413480=CARTESIAN_POINT('Origin',(2.705496790722,-0.349672869111943,12.4908873016278));
#413481=CARTESIAN_POINT('Origin',(1.2384571831645E-15,-2.82669770368892E-16,
12.4908873016278));
#413482=CARTESIAN_POINT('',(2.66578785733794,-0.648595822395547,12.5064436508139));
#413483=CARTESIAN_POINT('',(2.6832070484908,-0.572277359405966,12.5064436508139));
#413484=CARTESIAN_POINT('Origin',(5.02528380890789E-31,-6.30150658186899E-31,
12.5064436508139));
#413485=CARTESIAN_POINT('',(2.67204885726299,-0.650119146310548,12.4908873016278));
#413486=CARTESIAN_POINT('Origin',(2.65067246640489,-0.644918193140064,12.4908873016278));
#413487=CARTESIAN_POINT('',(2.68950895998134,-0.573621438040911,12.4908873016278));
#413488=CARTESIAN_POINT('Origin',(2.476914366329E-15,-5.65339540737784E-16,
12.4908873016278));
#413489=CARTESIAN_POINT('Origin',(2.66799288830148,-0.569032466536583,12.4908873016278));
#413490=CARTESIAN_POINT('Origin',(1.21129610858987E-15,-3.82674967730057E-16,
12.4908873016278));
#413491=CARTESIAN_POINT('',(2.60405108735959,-0.863724131641991,12.5064436508139));
#413492=CARTESIAN_POINT('',(2.62763298083056,-0.789079437833017,12.5064436508139));
#413493=CARTESIAN_POINT('Origin',(4.91507240220936E-31,-6.70729735601718E-31,
12.5064436508139));
#413494=CARTESIAN_POINT('',(2.61016708928296,-0.86575271644051,12.4908873016278));
#413495=CARTESIAN_POINT('Origin',(2.5892857525687,-0.858826694708985,12.4908873016278));
#413496=CARTESIAN_POINT('',(2.63380436834392,-0.790932708447753,12.4908873016278));
#413497=CARTESIAN_POINT('Origin',(2.42259221717973E-15,-7.65349935460113E-16,
12.4908873016278));
#413498=CARTESIAN_POINT('Origin',(2.61273393339717,-0.784605246780171,12.4908873016278));
#413499=CARTESIAN_POINT('Origin',(1.17607405826236E-15,-4.80133526317904E-16,
12.4908873016278));
#413500=CARTESIAN_POINT('',(2.52498478703305,-1.07310449929681,12.5064436508139));
#413501=CARTESIAN_POINT('',(2.55457244921182,-1.00063032279023,12.5064436508139));
#413502=CARTESIAN_POINT('Origin',(4.772151999604E-31,-7.10275464204105E-31,
12.5064436508139));
#413503=CARTESIAN_POINT('',(2.53091508997101,-1.0756248450817,12.4908873016278));
#413504=CARTESIAN_POINT('Origin',(2.51066776925124,-1.06701984632105,12.4908873016278));
#413505=CARTESIAN_POINT('',(2.56057224318231,-1.00298045217459,12.4908873016278));
#413506=CARTESIAN_POINT('Origin',(2.35214811652471E-15,-9.60267052635807E-16,
12.4908873016278));
#413507=CARTESIAN_POINT('Origin',(2.54008766523685,-0.99495660855719,12.4908873016278));
#413508=CARTESIAN_POINT('Origin',(1.13302542911567E-15,-5.74396875504561E-16,
12.4908873016278));
#413509=CARTESIAN_POINT('',(2.42911512954197,-1.27534353355859,12.5064436508139));
#413510=CARTESIAN_POINT('',(2.46451165941837,-1.20552217804166,12.5064436508139));
#413511=CARTESIAN_POINT('Origin',(4.59747371279093E-31,-7.48524673694799E-31,
12.5064436508139));
#413512=CARTESIAN_POINT('',(2.4348202683069,-1.27833886784449,12.4908873016278));
#413513=CARTESIAN_POINT('Origin',(2.41534170616044,-1.26811215690173,12.4908873016278));
#413514=CARTESIAN_POINT('',(2.470299932207,-1.20835352647233,12.4908873016278));
#413515=CARTESIAN_POINT('Origin',(2.26605085823134E-15,-1.14879375100912E-15,
12.4908873016278));
#413516=CARTESIAN_POINT('Origin',(2.45053753274934,-1.19868669826055,12.4908873016278));
#413517=CARTESIAN_POINT('Origin',(1.08243670267426E-15,-6.64837708253549E-16,
12.4908873016278));
#413518=CARTESIAN_POINT('',(2.31708011163957,-1.4690953670214,12.5064436508139));
#413519=CARTESIAN_POINT('',(2.35804995114728,-1.40239148209538,12.5064436508139));
#413520=CARTESIAN_POINT('Origin',(4.39219999694901E-31,-7.85222821895314E-31,
12.5064436508139));
#413521=CARTESIAN_POINT('',(2.32252211947427,-1.47254575635283,12.4908873016278));
#413522=CARTESIAN_POINT('Origin',(2.30394194251848,-1.46076539030201,12.4908873016278));
#413523=CARTESIAN_POINT('',(2.36358818275365,-1.40568520741569,12.4908873016278));
#413524=CARTESIAN_POINT('Origin',(2.16487340534852E-15,-1.3296754165071E-15,
12.4908873016278));
#413525=CARTESIAN_POINT('Origin',(2.34467947729162,-1.39443972575636,12.4908873016278));
#413526=CARTESIAN_POINT('Origin',(1.02464453856604E-15,-7.50854155744611E-16,
12.4908873016278));
#413527=CARTESIAN_POINT('',(2.18962530788552,-1.65307061320037,12.5064436508139));
#413528=CARTESIAN_POINT('',(2.23589580950217,-1.58992810221407,12.5064436508139));
#413529=CARTESIAN_POINT('Origin',(4.15769691478938E-31,-8.20125688684145E-31,
12.5064436508139));
#413530=CARTESIAN_POINT('',(2.19476796912572,-1.6569530958056,12.4908873016278));
#413531=CARTESIAN_POINT('Origin',(2.17720982537272,-1.64369747103915,12.4908873016278));
#413532=CARTESIAN_POINT('',(2.24114714390868,-1.59366228522544,12.4908873016278));
#413533=CARTESIAN_POINT('Origin',(2.04928907713207E-15,-1.50170831148922E-15,
12.4908873016278));
#413534=CARTESIAN_POINT('Origin',(2.22321796675741,-1.58091298694363,12.4908873016278));
#413535=CARTESIAN_POINT('Origin',(9.60033534108104E-16,-8.31873792711407E-16,
12.4908873016278));
#413536=CARTESIAN_POINT('',(2.04759890897023,-1.82604494718594,12.5064436508139));
#413537=CARTESIAN_POINT('',(2.09886215014166,-1.76688401313219,12.5064436508139));
#413538=CARTESIAN_POINT('Origin',(3.89552504563353E-31,-8.53001001241378E-31,
12.5064436508139));
#413539=CARTESIAN_POINT('',(2.05240800005387,-1.83033368578379,12.4908873016278));
#413540=CARTESIAN_POINT('Origin',(2.03598873605344,-1.81569101629752,12.4908873016278));
#413541=CARTESIAN_POINT('',(2.10379164058425,-1.77103380346278,12.4908873016278));
#413542=CARTESIAN_POINT('Origin',(1.92006706821621E-15,-1.66374758542281E-15,
12.4908873016278));
#413543=CARTESIAN_POINT('Origin',(2.08696130745958,-1.75686553303508,12.4908873016278));
#413544=CARTESIAN_POINT('Origin',(8.89033664875066E-16,-9.07357446837224E-16,
12.4908873016278));
#413545=CARTESIAN_POINT('',(1.89194607714579,-1.98686725332419,12.5064436508139));
#413546=CARTESIAN_POINT('',(1.94786090945984,-1.93208160245826,12.5064436508139));
#413547=CARTESIAN_POINT('Origin',(3.60742910001539E-31,-8.83629979785991E-31,
12.5064436508139));
#413548=CARTESIAN_POINT('',(1.89638959436514,-1.9915337070669,12.4908873016278));
#413549=CARTESIAN_POINT('Origin',(1.88121847761022,-1.97560143741037,12.4908873016278));
#413550=CARTESIAN_POINT('',(1.95243575099292,-1.93661938393808,12.4908873016278));
#413551=CARTESIAN_POINT('Origin',(1.77806732975013E-15,-1.81471489367445E-15,
12.4908873016278));
#413552=CARTESIAN_POINT('Origin',(1.93681626498497,-1.92112642886658,12.4908873016278));
#413553=CARTESIAN_POINT('Origin',(8.12117423282514E-16,-9.7680278685778E-16,
12.4908873016278));
#413554=CARTESIAN_POINT('',(1.72370265632708,-2.1344672857016,12.5064436508139));
#413555=CARTESIAN_POINT('',(1.78389697579999,-2.084421507491,12.5064436508139));
#413556=CARTESIAN_POINT('Origin',(3.29532630892054E-31,-9.11808793519194E-31,
12.5064436508139));
#413557=CARTESIAN_POINT('',(1.72775102880817,-2.13948040010941,12.4908873016278));
#413558=CARTESIAN_POINT('Origin',(1.7139290205777,-2.12236455690854,12.4908873016278));
#413559=CARTESIAN_POINT('',(1.78808672360795,-2.08931708193299,12.4908873016278));
#413560=CARTESIAN_POINT('Origin',(1.62423484656503E-15,-1.95360557371556E-15,
12.4908873016278));
#413561=CARTESIAN_POINT('Origin',(1.77378202981909,-2.07260254527753,12.4908873016278));
#413562=CARTESIAN_POINT('Origin',(7.29796674227961E-16,-1.03974766549291E-15,
12.4908873016278));
#413563=CARTESIAN_POINT('',(1.54398827872143,-2.26786279045497,12.5064436508139));
#413564=CARTESIAN_POINT('',(1.60806150208848,-2.22288993129672,12.5064436508139));
#413565=CARTESIAN_POINT('Origin',(2.96129366493041E-31,-9.37349917084771E-31,
12.5064436508139));
#413566=CARTESIAN_POINT('',(1.54761456521333,-2.27318920407861,12.4908873016278));
#413567=CARTESIAN_POINT('Origin',(1.53523364869163,-2.25500369044598,12.4908873016278));
#413568=CARTESIAN_POINT('',(1.61183827409092,-2.22811071946068,12.4908873016278));
#413569=CARTESIAN_POINT('Origin',(1.45959334845592E-15,-2.07949533098583E-15,
12.4908873016278));
#413570=CARTESIAN_POINT('Origin',(1.59894356789819,-2.210285833705,12.4908873016278));
#413571=CARTESIAN_POINT('Origin',(6.42619248714396E-16,-1.09577319496048E-15,
12.4908873016278));
#413572=CARTESIAN_POINT('',(1.35399891386102,-2.38616604250889,12.5064436508139));
#413573=CARTESIAN_POINT('',(1.42152464439204,-2.34656538936069,12.5064436508139));
#413574=CARTESIAN_POINT('Origin',(2.60755410017922E-31,-9.60083378519382E-31,
12.5064436508139));
#413575=CARTESIAN_POINT('',(1.35717898202543,-2.39177030894449,12.4908873016278));
#413576=CARTESIAN_POINT('Origin',(1.34632155016923,-2.37263614647293,12.4908873016278));
#413577=CARTESIAN_POINT('',(1.42486330679441,-2.35207664776276,12.4908873016278));
#413578=CARTESIAN_POINT('Origin',(1.28523849742879E-15,-2.19154638992096E-15,
12.4908873016278));
#413579=CARTESIAN_POINT('Origin',(1.41346440034005,-2.33326003458066,12.4908873016278));
#413580=CARTESIAN_POINT('Origin',(5.5116529812535E-16,-1.14450653460544E-15,
12.4908873016278));
#413581=CARTESIAN_POINT('',(1.15499890962297,-2.4885897532396,12.5064436508139));
#413582=CARTESIAN_POINT('',(1.22552777472223,-2.4546248419145,12.5064436508139));
#413583=CARTESIAN_POINT('Origin',(2.23646169310749E-31,-9.79857890387934E-31,
12.5064436508139));
#413584=CARTESIAN_POINT('',(1.15771159663093,-2.49443457701866,12.4908873016278));
#413585=CARTESIAN_POINT('Origin',(1.14844990385788,-2.47447910040251,12.4908873016278));
#413586=CARTESIAN_POINT('',(1.22840610927708,-2.46038989403931,12.4908873016278));
#413587=CARTESIAN_POINT('Origin',(1.1023305962507E-15,-2.28901306921088E-15,
12.4908873016278));
#413588=CARTESIAN_POINT('Origin',(1.21857886040286,-2.44070677488699,12.4908873016278));
#413589=CARTESIAN_POINT('Origin',(4.56043433413153E-16,-1.18562337209288E-15,
12.4908873016278));
#413590=CARTESIAN_POINT('',(0.948312578202777,-2.57445230975091,12.5064436508139));
#413591=CARTESIAN_POINT('',(1.02137521990949,-2.54634917112996,12.5064436508139));
#413592=CARTESIAN_POINT('Origin',(1.85048600245833E-31,-9.9654185657651E-31,
12.5064436508139));
#413593=CARTESIAN_POINT('',(0.950539831569808,-2.58049879453552,12.4908873016278));
#413594=CARTESIAN_POINT('Origin',(0.942935512917249,-2.55985480417923,12.4908873016278));
#413595=CARTESIAN_POINT('',(1.02377407177525,-2.55232965150678,12.4908873016278));
#413596=CARTESIAN_POINT('Origin',(9.12086866826306E-16,-2.37124674418577E-15,
12.4908873016278));
#413597=CARTESIAN_POINT('Origin',(1.01558387920105,-2.53191101429473,12.4908873016278));
#413598=CARTESIAN_POINT('Origin',(3.57886674893462E-16,-1.21885008165314E-15,
12.4908873016278));
#413599=CARTESIAN_POINT('',(0.735315383035209,-2.64318231089556,12.5064436508139));
#413600=CARTESIAN_POINT('',(0.810425581523304,-2.62112796672959,12.5064436508139));
#413601=CARTESIAN_POINT('Origin',(1.45219563277151E-31,-1.01002424804278E-30,
12.5064436508139));
#413602=CARTESIAN_POINT('',(0.737042380757625,-2.64939021832707,12.4908873016278));
#413603=CARTESIAN_POINT('Origin',(0.731146041711564,-2.62819509658045,12.4908873016278));
#413604=CARTESIAN_POINT('',(0.812328986736591,-2.62728407624823,12.4908873016278));
#413605=CARTESIAN_POINT('Origin',(7.15773349786924E-16,-2.43770016330627E-15,
12.4908873016278));
#413606=CARTESIAN_POINT('Origin',(0.805830354842698,-2.60626580363824,12.4908873016278));
#413607=CARTESIAN_POINT('Origin',(2.573482395995E-16,-1.2439655450161E-15,
12.4908873016278));
#413608=CARTESIAN_POINT('',(0.517424785312041,-2.69432236985558,12.5064436508139));
#413609=CARTESIAN_POINT('',(0.59408269460289,-2.67846358816631,12.5064436508139));
#413610=CARTESIAN_POINT('Origin',(1.04424114074401E-31,-1.02021534169599E-30,
12.5064436508139));
#413611=CARTESIAN_POINT('',(0.518640034504934,-2.70065038733427,12.4908873016278));
#413612=CARTESIAN_POINT('Origin',(0.514490914228895,-2.67904518423559,12.4908873016278));
#413613=CARTESIAN_POINT('',(0.595477986316048,-2.6847543589336,12.4908873016278));
#413614=CARTESIAN_POINT('Origin',(5.14696479198999E-16,-2.48793109003219E-15,
12.4908873016278));
#413615=CARTESIAN_POINT('Origin',(0.59071416242552,-2.66327632406214,12.4908873016278));
#413616=CARTESIAN_POINT('Origin',(1.55097194230474E-16,-1.26080262291684E-15,
12.4908873016278));
#413617=CARTESIAN_POINT('',(0.296090811011702,-2.72753215797611,12.5064436508139));
#413618=CARTESIAN_POINT('',(0.373786285366639,-2.71797447633917,12.5064436508139));
#413619=CARTESIAN_POINT('Origin',(6.29337396212522E-32,-1.02704731748927E-30,
12.5064436508139));
#413620=CARTESIAN_POINT('',(0.296786224392195,-2.73393817358971,12.4908873016278));
#413621=CARTESIAN_POINT('Origin',(0.294411934597058,-2.71206666820099,12.4908873016278));
#413622=CARTESIAN_POINT('',(0.374664178143524,-2.72435804431357,12.4908873016278));
#413623=CARTESIAN_POINT('Origin',(3.10194388460947E-16,-2.52160524583369E-15,
12.4908873016278));
#413624=CARTESIAN_POINT('Origin',(0.371666864718376,-2.70256317995906,12.4908873016278));
#413625=CARTESIAN_POINT('Origin',(5.18140026230798E-17,-1.26924926737987E-15,
12.4908873016278));
#413626=CARTESIAN_POINT('',(0.0727864012156247,-2.74259066959644,12.5064436508139));
#413627=CARTESIAN_POINT('',(0.151002390071669,-2.73939769280622,12.5064436508139));
#413628=CARTESIAN_POINT('Origin',(2.102455151426E-32,-1.03047470975092E-30,
12.5064436508139));
#413629=CARTESIAN_POINT('',(0.0729573509224068,-2.74903205236796,12.4908873016278));
#413630=CARTESIAN_POINT('Origin',(0.0723736921150276,-2.72703979594902,
12.4908873016278));
#413631=CARTESIAN_POINT('',(0.151357041680694,-2.74583157639606,12.4908873016278));
#413632=CARTESIAN_POINT('Origin',(1.0362800524616E-16,-2.53849853475974E-15,
12.4908873016278));
#413633=CARTESIAN_POINT('Origin',(0.150146185347248,-2.72386492378489,12.4908873016278));
#413634=CARTESIAN_POINT('Origin',(-5.18140026230626E-17,-1.26924926737987E-15,
12.4908873016278));
#413635=CARTESIAN_POINT('',(-0.151002390071633,-2.73939769280622,12.5064436508139));
#413636=CARTESIAN_POINT('',(-0.0727864012155879,-2.74259066959644,12.5064436508139));
#413637=CARTESIAN_POINT('Origin',(-2.1024551514253E-32,-1.03047470975092E-30,
12.5064436508139));
#413638=CARTESIAN_POINT('',(-0.151357041680656,-2.74583157639606,12.4908873016278));
#413639=CARTESIAN_POINT('Origin',(-0.150146185347211,-2.72386492378489,
12.4908873016278));
#413640=CARTESIAN_POINT('',(-0.0729573509223692,-2.74903205236796,12.4908873016278));
#413641=CARTESIAN_POINT('Origin',(-1.03628005246125E-16,-2.53849853475974E-15,
12.4908873016278));
#413642=CARTESIAN_POINT('Origin',(-0.0723736921149902,-2.72703979594902,
12.4908873016278));
#413643=CARTESIAN_POINT('Origin',(-1.55097194230457E-16,-1.26080262291685E-15,
12.4908873016278));
#413644=CARTESIAN_POINT('',(-0.373786285366603,-2.71797447633918,12.5064436508139));
#413645=CARTESIAN_POINT('',(-0.296090811011665,-2.72753215797611,12.5064436508139));
#413646=CARTESIAN_POINT('Origin',(-6.29337396212453E-32,-1.02704731748927E-30,
12.5064436508139));
#413647=CARTESIAN_POINT('',(-0.374664178143487,-2.72435804431357,12.4908873016278));
#413648=CARTESIAN_POINT('Origin',(-0.371666864718339,-2.70256317995906,
12.4908873016278));
#413649=CARTESIAN_POINT('',(-0.296786224392158,-2.73393817358971,12.4908873016278));
#413650=CARTESIAN_POINT('Origin',(-3.10194388460913E-16,-2.52160524583369E-15,
12.4908873016278));
#413651=CARTESIAN_POINT('Origin',(-0.294411934597021,-2.71206666820099,
12.4908873016278));
#413652=CARTESIAN_POINT('Origin',(-2.57348239599483E-16,-1.2439655450161E-15,
12.4908873016278));
#413653=CARTESIAN_POINT('',(-0.594082694602854,-2.67846358816632,12.5064436508139));
#413654=CARTESIAN_POINT('',(-0.517424785312005,-2.69432236985558,12.5064436508139));
#413655=CARTESIAN_POINT('Origin',(-1.04424114074394E-31,-1.02021534169599E-30,
12.5064436508139));
#413656=CARTESIAN_POINT('',(-0.595477986316011,-2.68475435893361,12.4908873016278));
#413657=CARTESIAN_POINT('Origin',(-0.590714162425483,-2.66327632406214,
12.4908873016278));
#413658=CARTESIAN_POINT('',(-0.518640034504897,-2.70065038733427,12.4908873016278));
#413659=CARTESIAN_POINT('Origin',(-5.14696479198966E-16,-2.4879310900322E-15,
12.4908873016278));
#413660=CARTESIAN_POINT('Origin',(-0.514490914228858,-2.6790451842356,12.4908873016278));
#413661=CARTESIAN_POINT('Origin',(-3.57886674893445E-16,-1.21885008165314E-15,
12.4908873016278));
#413662=CARTESIAN_POINT('',(-0.810425581523269,-2.6211279667296,12.5064436508139));
#413663=CARTESIAN_POINT('',(-0.735315383035173,-2.64318231089557,12.5064436508139));
#413664=CARTESIAN_POINT('Origin',(-1.45219563277144E-31,-1.01002424804279E-30,
12.5064436508139));
#413665=CARTESIAN_POINT('',(-0.812328986736555,-2.62728407624824,12.4908873016278));
#413666=CARTESIAN_POINT('Origin',(-0.805830354842662,-2.60626580363825,
12.4908873016278));
#413667=CARTESIAN_POINT('',(-0.737042380757589,-2.64939021832708,12.4908873016278));
#413668=CARTESIAN_POINT('Origin',(-7.15773349786891E-16,-2.43770016330628E-15,
12.4908873016278));
#413669=CARTESIAN_POINT('Origin',(-0.731146041711528,-2.62819509658046,
12.4908873016278));
#413670=CARTESIAN_POINT('Origin',(-4.56043433413137E-16,-1.18562337209289E-15,
12.4908873016278));
#413671=CARTESIAN_POINT('',(-1.02137521990946,-2.54634917112997,12.5064436508139));
#413672=CARTESIAN_POINT('',(-0.948312578202743,-2.57445230975092,12.5064436508139));
#413673=CARTESIAN_POINT('Origin',(-1.85048600245827E-31,-9.96541856576512E-31,
12.5064436508139));
#413674=CARTESIAN_POINT('',(-1.02377407177522,-2.5523296515068,12.4908873016278));
#413675=CARTESIAN_POINT('Origin',(-1.01558387920101,-2.53191101429474,12.4908873016278));
#413676=CARTESIAN_POINT('',(-0.950539831569773,-2.58049879453553,12.4908873016278));
#413677=CARTESIAN_POINT('Origin',(-9.12086866826275E-16,-2.37124674418578E-15,
12.4908873016278));
#413678=CARTESIAN_POINT('Origin',(-0.942935512917215,-2.55985480417924,
12.4908873016278));
#413679=CARTESIAN_POINT('Origin',(-5.51165298125335E-16,-1.14450653460545E-15,
12.4908873016278));
#413680=CARTESIAN_POINT('',(-1.22552777472219,-2.45462484191451,12.5064436508139));
#413681=CARTESIAN_POINT('',(-1.15499890962293,-2.48858975323962,12.5064436508139));
#413682=CARTESIAN_POINT('Origin',(-2.23646169310743E-31,-9.79857890387937E-31,
12.5064436508139));
#413683=CARTESIAN_POINT('',(-1.22840610927704,-2.46038989403932,12.4908873016278));
#413684=CARTESIAN_POINT('Origin',(-1.21857886040283,-2.44070677488701,12.4908873016278));
#413685=CARTESIAN_POINT('',(-1.15771159663089,-2.49443457701868,12.4908873016278));
#413686=CARTESIAN_POINT('Origin',(-1.10233059625067E-15,-2.28901306921089E-15,
12.4908873016278));
#413687=CARTESIAN_POINT('Origin',(-1.14844990385785,-2.47447910040253,12.4908873016278));
#413688=CARTESIAN_POINT('Origin',(-6.42619248714382E-16,-1.09577319496049E-15,
12.4908873016278));
#413689=CARTESIAN_POINT('',(-1.42152464439201,-2.34656538936071,12.5064436508139));
#413690=CARTESIAN_POINT('',(-1.35399891386099,-2.38616604250891,12.5064436508139));
#413691=CARTESIAN_POINT('Origin',(-2.60755410017916E-31,-9.60083378519385E-31,
12.5064436508139));
#413692=CARTESIAN_POINT('',(-1.42486330679438,-2.35207664776278,12.4908873016278));
#413693=CARTESIAN_POINT('Origin',(-1.41346440034002,-2.33326003458068,12.4908873016278));
#413694=CARTESIAN_POINT('',(-1.3571789820254,-2.39177030894451,12.4908873016278));
#413695=CARTESIAN_POINT('Origin',(-1.28523849742876E-15,-2.19154638992098E-15,
12.4908873016278));
#413696=CARTESIAN_POINT('Origin',(-1.3463215501692,-2.37263614647295,12.4908873016278));
#413697=CARTESIAN_POINT('Origin',(-7.29796674227947E-16,-1.03974766549292E-15,
12.4908873016278));
#413698=CARTESIAN_POINT('',(-1.60806150208845,-2.22288993129674,12.5064436508139));
#413699=CARTESIAN_POINT('',(-1.5439882787214,-2.26786279045499,12.5064436508139));
#413700=CARTESIAN_POINT('Origin',(-2.96129366493035E-31,-9.37349917084775E-31,
12.5064436508139));
#413701=CARTESIAN_POINT('',(-1.61183827409089,-2.22811071946071,12.4908873016278));
#413702=CARTESIAN_POINT('Origin',(-1.59894356789816,-2.21028583370502,12.4908873016278));
#413703=CARTESIAN_POINT('',(-1.5476145652133,-2.27318920407863,12.4908873016278));
#413704=CARTESIAN_POINT('Origin',(-1.45959334845589E-15,-2.07949533098585E-15,
12.4908873016278));
#413705=CARTESIAN_POINT('Origin',(-1.5352336486916,-2.255003690446,12.4908873016278));
#413706=CARTESIAN_POINT('Origin',(-8.12117423282501E-16,-9.76802786857791E-16,
12.4908873016278));
#413707=CARTESIAN_POINT('',(-1.78389697579996,-2.08442150749102,12.5064436508139));
#413708=CARTESIAN_POINT('',(-1.72370265632705,-2.13446728570162,12.5064436508139));
#413709=CARTESIAN_POINT('Origin',(-3.29532630892049E-31,-9.11808793519199E-31,
12.5064436508139));
#413710=CARTESIAN_POINT('',(-1.78808672360792,-2.08931708193301,12.4908873016278));
#413711=CARTESIAN_POINT('Origin',(-1.77378202981906,-2.07260254527755,12.4908873016278));
#413712=CARTESIAN_POINT('',(-1.72775102880814,-2.13948040010943,12.4908873016278));
#413713=CARTESIAN_POINT('Origin',(-1.624234846565E-15,-1.95360557371558E-15,
12.4908873016278));
#413714=CARTESIAN_POINT('Origin',(-1.71392902057767,-2.12236455690856,12.4908873016278));
#413715=CARTESIAN_POINT('Origin',(-8.89033664875054E-16,-9.07357446837236E-16,
12.4908873016278));
#413716=CARTESIAN_POINT('',(-1.94786090945981,-1.93208160245828,12.5064436508139));
#413717=CARTESIAN_POINT('',(-1.89194607714577,-1.98686725332422,12.5064436508139));
#413718=CARTESIAN_POINT('Origin',(-3.60742910001534E-31,-8.83629979785995E-31,
12.5064436508139));
#413719=CARTESIAN_POINT('',(-1.95243575099289,-1.93661938393811,12.4908873016278));
#413720=CARTESIAN_POINT('Origin',(-1.93681626498495,-1.92112642886661,12.4908873016278));
#413721=CARTESIAN_POINT('',(-1.89638959436511,-1.99153370706693,12.4908873016278));
#413722=CARTESIAN_POINT('Origin',(-1.77806732975011E-15,-1.81471489367447E-15,
12.4908873016278));
#413723=CARTESIAN_POINT('Origin',(-1.88121847761019,-1.97560143741039,12.4908873016278));
#413724=CARTESIAN_POINT('Origin',(-9.60033534108093E-16,-8.3187379271142E-16,
12.4908873016278));
#413725=CARTESIAN_POINT('',(-2.09886215014164,-1.76688401313222,12.5064436508139));
#413726=CARTESIAN_POINT('',(-2.04759890897021,-1.82604494718596,12.5064436508139));
#413727=CARTESIAN_POINT('Origin',(-3.89552504563349E-31,-8.53001001241383E-31,
12.5064436508139));
#413728=CARTESIAN_POINT('',(-2.10379164058423,-1.77103380346281,12.4908873016278));
#413729=CARTESIAN_POINT('Origin',(-2.08696130745955,-1.7568655330351,12.4908873016278));
#413730=CARTESIAN_POINT('',(-2.05240800005384,-1.83033368578382,12.4908873016278));
#413731=CARTESIAN_POINT('Origin',(-1.92006706821618E-15,-1.66374758542284E-15,
12.4908873016278));
#413732=CARTESIAN_POINT('Origin',(-2.03598873605341,-1.81569101629755,12.4908873016278));
#413733=CARTESIAN_POINT('Origin',(-1.02464453856603E-15,-7.50854155744624E-16,
12.4908873016278));
#413734=CARTESIAN_POINT('',(-2.23589580950215,-1.5899281022141,12.5064436508139));
#413735=CARTESIAN_POINT('',(-2.18962530788549,-1.6530706132004,12.5064436508139));
#413736=CARTESIAN_POINT('Origin',(-4.15769691478934E-31,-8.2012568868415E-31,
12.5064436508139));
#413737=CARTESIAN_POINT('',(-2.24114714390866,-1.59366228522547,12.4908873016278));
#413738=CARTESIAN_POINT('Origin',(-2.22321796675739,-1.58091298694366,12.4908873016278));
#413739=CARTESIAN_POINT('',(-2.1947679691257,-1.65695309580563,12.4908873016278));
#413740=CARTESIAN_POINT('Origin',(-2.04928907713205E-15,-1.50170831148925E-15,
12.4908873016278));
#413741=CARTESIAN_POINT('Origin',(-2.1772098253727,-1.64369747103918,12.4908873016278));
#413742=CARTESIAN_POINT('Origin',(-1.08243670267425E-15,-6.64837708253564E-16,
12.4908873016278));
#413743=CARTESIAN_POINT('',(-2.35804995114726,-1.40239148209542,12.5064436508139));
#413744=CARTESIAN_POINT('',(-2.31708011163955,-1.46909536702144,12.5064436508139));
#413745=CARTESIAN_POINT('Origin',(-4.39219999694897E-31,-7.8522282189532E-31,
12.5064436508139));
#413746=CARTESIAN_POINT('',(-2.36358818275363,-1.40568520741572,12.4908873016278));
#413747=CARTESIAN_POINT('Origin',(-2.3446794772916,-1.3944397257564,12.4908873016278));
#413748=CARTESIAN_POINT('',(-2.32252211947425,-1.47254575635286,12.4908873016278));
#413749=CARTESIAN_POINT('Origin',(-2.1648734053485E-15,-1.32967541650713E-15,
12.4908873016278));
#413750=CARTESIAN_POINT('Origin',(-2.30394194251846,-1.46076539030204,12.4908873016278));
#413751=CARTESIAN_POINT('Origin',(-1.13302542911566E-15,-5.74396875504576E-16,
12.4908873016278));
#413752=CARTESIAN_POINT('',(-2.46451165941835,-1.20552217804169,12.5064436508139));
#413753=CARTESIAN_POINT('',(-2.42911512954195,-1.27534353355862,12.5064436508139));
#413754=CARTESIAN_POINT('Origin',(-4.5974737127909E-31,-7.48524673694805E-31,
12.5064436508139));
#413755=CARTESIAN_POINT('',(-2.47029993220698,-1.20835352647236,12.4908873016278));
#413756=CARTESIAN_POINT('Origin',(-2.45053753274933,-1.19868669826058,12.4908873016278));
#413757=CARTESIAN_POINT('',(-2.43482026830688,-1.27833886784452,12.4908873016278));
#413758=CARTESIAN_POINT('Origin',(-2.26605085823133E-15,-1.14879375100915E-15,
12.4908873016278));
#413759=CARTESIAN_POINT('Origin',(-2.41534170616043,-1.26811215690176,12.4908873016278));
#413760=CARTESIAN_POINT('Origin',(-1.17607405826235E-15,-4.8013352631792E-16,
12.4908873016278));
#413761=CARTESIAN_POINT('',(-2.55457244921181,-1.00063032279027,12.5064436508139));
#413762=CARTESIAN_POINT('',(-2.52498478703303,-1.07310449929684,12.5064436508139));
#413763=CARTESIAN_POINT('Origin',(-4.77215199960397E-31,-7.10275464204111E-31,
12.5064436508139));
#413764=CARTESIAN_POINT('',(-2.56057224318229,-1.00298045217462,12.4908873016278));
#413765=CARTESIAN_POINT('Origin',(-2.54008766523683,-0.994956608557225,
12.4908873016278));
#413766=CARTESIAN_POINT('',(-2.530915089971,-1.07562484508174,12.4908873016278));
#413767=CARTESIAN_POINT('Origin',(-2.3521481165247E-15,-9.60267052635839E-16,
12.4908873016278));
#413768=CARTESIAN_POINT('Origin',(-2.51066776925123,-1.06701984632108,12.4908873016278));
#413769=CARTESIAN_POINT('Origin',(-1.21129610858986E-15,-3.82674967730074E-16,
12.4908873016278));
#413770=CARTESIAN_POINT('',(-2.62763298083055,-0.789079437833052,12.5064436508139));
#413771=CARTESIAN_POINT('',(-2.60405108735958,-0.863724131642026,12.5064436508139));
#413772=CARTESIAN_POINT('Origin',(-4.91507240220934E-31,-6.70729735601724E-31,
12.5064436508139));
#413773=CARTESIAN_POINT('',(-2.63380436834391,-0.79093270844779,12.4908873016278));
#413774=CARTESIAN_POINT('Origin',(-2.61273393339716,-0.784605246780207,
12.4908873016278));
#413775=CARTESIAN_POINT('',(-2.61016708928295,-0.865752716440546,12.4908873016278));
#413776=CARTESIAN_POINT('Origin',(-2.42259221717972E-15,-7.65349935460146E-16,
12.4908873016278));
#413777=CARTESIAN_POINT('Origin',(-2.58928575256869,-0.858826694709021,
12.4908873016278));
#413778=CARTESIAN_POINT('Origin',(-1.2384571831645E-15,-2.82669770368909E-16,
12.4908873016278));
#413779=CARTESIAN_POINT('',(-2.68320704849079,-0.572277359406002,12.5064436508139));
#413780=CARTESIAN_POINT('',(-2.66578785733794,-0.648595822395582,12.5064436508139));
#413781=CARTESIAN_POINT('Origin',(-5.02528380890787E-31,-6.30150658186906E-31,
12.5064436508139));
#413782=CARTESIAN_POINT('',(-2.68950895998133,-0.573621438040948,12.4908873016278));
#413783=CARTESIAN_POINT('Origin',(-2.66799288830148,-0.56903246653662,12.4908873016278));
#413784=CARTESIAN_POINT('',(-2.67204885726298,-0.650119146310585,12.4908873016278));
#413785=CARTESIAN_POINT('Origin',(-2.476914366329E-15,-5.65339540737817E-16,
12.4908873016278));
#413786=CARTESIAN_POINT('Origin',(-2.65067246640488,-0.6449181931401,12.4908873016278));
#413787=CARTESIAN_POINT('Origin',(-1.25737652951623E-15,-1.80783452323169E-16,
12.4908873016278));
#413788=CARTESIAN_POINT('',(-2.72092481594133,-0.351666869571222,12.5064436508139));
#413789=CARTESIAN_POINT('',(-2.70978424894974,-0.429151214961874,12.5064436508139));
#413790=CARTESIAN_POINT('Origin',(-5.10205278097159E-31,-5.88808279024776E-31,
12.5064436508139));
#413791=CARTESIAN_POINT('',(-2.72731531322782,-0.352492811604818,12.4908873016278));
#413792=CARTESIAN_POINT('Origin',(-2.70549679072199,-0.34967286911198,12.4908873016278));
#413793=CARTESIAN_POINT('',(-2.71614858095496,-0.430159140524035,12.4908873016278));
#413794=CARTESIAN_POINT('Origin',(-2.51475305903245E-15,-3.61566904646336E-16,
12.4908873016278));
#413795=CARTESIAN_POINT('Origin',(-2.69441939230732,-0.426717867399843,
12.4908873016278));
#413796=CARTESIAN_POINT('Origin',(-1.26792824251655E-15,-7.76940502293878E-17,
12.4908873016278));
#413797=CARTESIAN_POINT('',(-2.74053527766277,-0.128716094740396,12.5064436508139));
#413798=CARTESIAN_POINT('',(-2.73574747346772,-0.206850676997561,12.5064436508139));
#413799=CARTESIAN_POINT('Origin',(-5.1448684335574E-31,-5.46977724827647E-31,
12.5064436508139));
#413800=CARTESIAN_POINT('',(-2.74697183304013,-0.12901840366468,12.4908873016278));
#413801=CARTESIAN_POINT('Origin',(-2.7249960583758,-0.127986256435362,12.4908873016278));
#413802=CARTESIAN_POINT('',(-2.74217278397365,-0.207336496628562,12.4908873016278));
#413803=CARTESIAN_POINT('Origin',(-2.5358564850331E-15,-1.55388100458775E-16,
12.4908873016278));
#413804=CARTESIAN_POINT('Origin',(-2.72023540170186,-0.205677804655533,
12.4908873016278));
#413805=CARTESIAN_POINT('Origin',(-1.27004210225636E-15,2.59123929500539E-17,
12.4908873016278));
#413806=CARTESIAN_POINT('',(-2.74190792926786,0.0950912644642679,12.5064436508139));
#413807=CARTESIAN_POINT('',(-2.74350474991634,0.0168264180942123,12.5064436508139));
#413808=CARTESIAN_POINT('Origin',(-5.15344583556142E-31,-5.04937371032143E-31,
12.5064436508139));
#413809=CARTESIAN_POINT('',(-2.748347708522,0.0953146004653095,12.4908873016278));
#413810=CARTESIAN_POINT('Origin',(-2.72636092685383,0.0945520836615871,
12.4908873016278));
#413811=CARTESIAN_POINT('',(-2.74994827954166,0.0168659374438614,12.4908873016278));
#413812=CARTESIAN_POINT('Origin',(-2.54008420451272E-15,5.18247859001083E-17,
12.4908873016278));
#413813=CARTESIAN_POINT('Origin',(-2.72794869330533,0.0167310099443105,
12.4908873016278));
#413814=CARTESIAN_POINT('Origin',(-1.26370404134785E-15,1.29346393429657E-16,
12.4908873016278));
#413815=CARTESIAN_POINT('',(-2.72503363598664,0.318265806992875,12.5064436508139));
#413816=CARTESIAN_POINT('',(-2.73300445490068,0.240391536149731,12.5064436508139));
#413817=CARTESIAN_POINT('Origin',(-5.12772790578849E-31,-4.62966989256605E-31,
12.5064436508139));
#413818=CARTESIAN_POINT('',(-2.73143378344912,0.319013301655004,12.4908873016278));
#413819=CARTESIAN_POINT('Origin',(-2.70958231318153,0.316461195241764,12.4908873016278));
#413820=CARTESIAN_POINT('',(-2.73942332301885,0.240956131485279,12.4908873016278));
#413821=CARTESIAN_POINT('Origin',(-2.52740808269571E-15,2.58692786859314E-16,
12.4908873016278));
#413822=CARTESIAN_POINT('Origin',(-2.7175079364347,0.239028482433397,12.4908873016278));
#413823=CARTESIAN_POINT('Origin',(-1.24895623854067E-15,2.31919615001638E-16,
12.4908873016278));
#413824=CARTESIAN_POINT('',(-2.69002469345683,0.539322343086108,12.5064436508139));
#413825=CARTESIAN_POINT('',(-2.70431646615165,0.462356888193986,12.5064436508139));
#413826=CARTESIAN_POINT('Origin',(-5.0678857928181E-31,-4.21345885467123E-31,
12.5064436508139));
#413827=CARTESIAN_POINT('',(-2.69634261720224,0.540589021955675,12.4908873016278));
#413828=CARTESIAN_POINT('Origin',(-2.67477187626462,0.536264309780029,12.4908873016278));
#413829=CARTESIAN_POINT('',(-2.71066795625439,0.463442802226626,12.4908873016278));
#413830=CARTESIAN_POINT('Origin',(-2.49791247708133E-15,4.63839230003276E-16,
12.4908873016278));
#413831=CARTESIAN_POINT('Origin',(-2.68898261260435,0.459735259808813,12.4908873016278));
#413832=CARTESIAN_POINT('Origin',(-1.22589683802926E-15,3.32949449799826E-16,
12.4908873016278));
#413833=CARTESIAN_POINT('',(-2.63711408041489,0.756789777968025,12.5064436508139));
#413834=CARTESIAN_POINT('',(-2.6576316975012,0.681245331430826,12.5064436508139));
#413835=CARTESIAN_POINT('Origin',(-4.9743177360388E-31,-3.80351041242416E-31,
12.5064436508139));
#413836=CARTESIAN_POINT('',(-2.64330773570309,0.75856721150614,12.4908873016278));
#413837=CARTESIAN_POINT('Origin',(-2.62216127381747,0.752498673814091,12.4908873016278));
#413838=CARTESIAN_POINT('',(-2.66387354146978,0.682845337581834,12.4908873016278));
#413839=CARTESIAN_POINT('Origin',(-2.45179367605853E-15,6.65898899599653E-16,
12.4908873016278));
#413840=CARTESIAN_POINT('Origin',(-2.64256255313802,0.677382574881179,12.4908873016278));
#413841=CARTESIAN_POINT('Origin',(-1.19467929631952E-15,4.31763560942389E-16,
12.4908873016278));
#413842=CARTESIAN_POINT('',(-2.566653908261,0.969220901739089,12.5064436508139));
#413843=CARTESIAN_POINT('',(-2.59326082838224,0.895600199384562,12.5064436508139));
#413844=CARTESIAN_POINT('Origin',(-4.84764641543082E-31,-3.40255270507128E-31,
12.5064436508139));
#413845=CARTESIAN_POINT('',(-2.57268207733792,0.971497261418813,12.4908873016278));
#413846=CARTESIAN_POINT('Origin',(-2.55210062071922,0.963725283327462,12.4908873016278));
#413847=CARTESIAN_POINT('',(-2.59935148777489,0.897703649876986,12.4908873016278));
#413848=CARTESIAN_POINT('Origin',(-2.38935859263904E-15,8.63527121884779E-16,
12.4908873016278));
#413849=CARTESIAN_POINT('Origin',(-2.57855667587269,0.89052202067797,12.4908873016278));
#413850=CARTESIAN_POINT('Origin',(-1.15551136100098E-15,5.27704356822854E-16,
12.4908873016278));
#413851=CARTESIAN_POINT('',(-2.47911307781571,1.17520202031927,12.5064436508139));
#413852=CARTESIAN_POINT('',(-2.51163223630831,1.10399499577503,12.5064436508139));
#413853=CARTESIAN_POINT('Origin',(-4.68871480773351E-31,-3.01325404000165E-31,
12.5064436508139));
#413854=CARTESIAN_POINT('',(-2.48493564421073,1.17796215734251,12.4908873016278));
#413855=CARTESIAN_POINT('Origin',(-2.46505615905704,1.16853846008377,12.4908873016278));
#413856=CARTESIAN_POINT('',(-2.51753117879167,1.10658789249288,12.4908873016278));
#413857=CARTESIAN_POINT('Origin',(-2.31102272200196E-15,1.05540871364571E-15,
12.4908873016278));
#413858=CARTESIAN_POINT('Origin',(-2.49739092936133,1.09773518935294,12.4908873016278));
#413859=CARTESIAN_POINT('Origin',(-1.10865368822093E-15,6.20133367273753E-16,
12.4908873016278));
#413860=CARTESIAN_POINT('',(-2.37507415886243,1.37336236334892,12.5064436508139));
#413861=CARTESIAN_POINT('',(-2.4132891460919,1.30504288761496,12.5064436508139));
#413862=CARTESIAN_POINT('Origin',(-4.49858057657423E-31,-2.63820513560155E-31,
12.5064436508139));
#413863=CARTESIAN_POINT('',(-2.38065237435684,1.37658790945917,12.4908873016278));
#413864=CARTESIAN_POINT('Origin',(-2.36160715536198,1.36557520618349,12.4908873016278));
#413865=CARTESIAN_POINT('',(-2.41895711517699,1.30810797525839,12.4908873016278));
#413866=CARTESIAN_POINT('Origin',(-2.21730737644186E-15,1.24026673454751E-15,
12.4908873016278));
#413867=CARTESIAN_POINT('Origin',(-2.39960545825558,1.29764311145632,12.4908873016278));
#413868=CARTESIAN_POINT('Origin',(-1.05441810806075E-15,7.08435492480249E-16,
12.4908873016278));
#413869=CARTESIAN_POINT('',(-2.25522951324157,1.56238320643931,12.5064436508139));
#413870=CARTESIAN_POINT('',(-2.29888601477294,1.49740593435474,12.5064436508139));
#413871=CARTESIAN_POINT('Origin',(-4.27850903389139E-31,-2.27990188045105E-31,
12.5064436508139));
#413872=CARTESIAN_POINT('',(-2.2605262557316,1.56605269615939,12.4908873016278));
#413873=CARTESIAN_POINT('Origin',(-2.24244204568574,1.55352427459012,12.4908873016278));
#413874=CARTESIAN_POINT('',(-2.30428529106065,1.50092281527118,12.4908873016278));
#413875=CARTESIAN_POINT('Origin',(-2.10883621612151E-15,1.4168709849605E-15,
12.4908873016278));
#413876=CARTESIAN_POINT('Origin',(-2.28585100873216,1.48891543274901,12.4908873016278));
#413877=CARTESIAN_POINT('Origin',(-9.93165549358178E-16,7.92023096367917E-16,
12.4908873016278));
#413878=CARTESIAN_POINT('',(-2.12037668729676,1.74100664706594,12.5064436508139));
#413879=CARTESIAN_POINT('',(-2.16918417631515,1.67980399165597,12.5064436508139));
#413880=CARTESIAN_POINT('Origin',(-4.0299647194923E-31,-1.9407287235973E-31,
12.5064436508139));
#413881=CARTESIAN_POINT('',(-2.12535670783504,1.74509566054718,12.4908873016278));
#413882=CARTESIAN_POINT('Origin',(-2.10835385417236,1.7311348952628,12.4908873016278));
#413883=CARTESIAN_POINT('',(-2.1742788285126,1.68374926158317,12.4908873016278));
#413884=CARTESIAN_POINT('Origin',(-1.98633109871636E-15,1.58404619273583E-15,
12.4908873016278));
#413885=CARTESIAN_POINT('Origin',(-2.1568845978845,1.6702792674905,12.4908873016278));
#413886=CARTESIAN_POINT('Origin',(-9.25303637785404E-16,8.7033991722387E-16,
12.4908873016278));
#413887=CARTESIAN_POINT('',(-1.97141310433553,1.90804397570222,12.5064436508139));
#413888=CARTESIAN_POINT('',(-2.02504677505419,1.85102323054089,12.5064436508139));
#413889=CARTESIAN_POINT('Origin',(-3.75460165478238E-31,-1.62294280643953E-31,
12.5064436508139));
#413890=CARTESIAN_POINT('',(-1.97604326170702,1.91252530123455,12.4908873016278));
#413891=CARTESIAN_POINT('Origin',(-1.96023491561336,1.89722509882467,12.4908873016278));
#413892=CARTESIAN_POINT('',(-2.02980289909156,1.8553706343584,12.4908873016278));
#413893=CARTESIAN_POINT('Origin',(-1.85060727557081E-15,1.74067983444774E-15,
12.4908873016278));
#413894=CARTESIAN_POINT('Origin',(-2.01356447589883,1.84052766928353,12.4908873016278));
#413895=CARTESIAN_POINT('Origin',(-8.51283983167522E-16,9.42864769526676E-16,
12.4908873016278));
#413896=CARTESIAN_POINT('',(-1.80933009242521,2.0623835864853,12.5064436508139));
#413897=CARTESIAN_POINT('',(-1.86743302161444,2.00992421522389,12.5064436508139));
#413898=CARTESIAN_POINT('Origin',(-3.45425233552554E-31,-1.32865894182544E-31,
12.5064436508139));
#413899=CARTESIAN_POINT('',(-1.81357957369652,2.06722740158666,12.4908873016278));
#413900=CARTESIAN_POINT('Origin',(-1.79907093710695,2.05068958237397,12.4908873016278));
#413901=CARTESIAN_POINT('',(-1.87181896627098,2.01464482167658,12.4908873016278));
#413902=CARTESIAN_POINT('Origin',(-1.70256796633504E-15,1.88572953905335E-15,
12.4908873016278));
#413903=CARTESIAN_POINT('Origin',(-1.85684441454081,1.99852766310317,12.4908873016278));
#413904=CARTESIAN_POINT('Origin',(-7.71599174093631E-16,1.00911501235002E-15,
12.4908873016278));
#413905=CARTESIAN_POINT('',(-1.63520628726825,2.20299837476966,12.5064436508139));
#413906=CARTESIAN_POINT('',(-1.6973918095206,2.15544948586873,12.5064436508139));
#413907=CARTESIAN_POINT('Origin',(-3.1309155368873E-31,-1.05983554032062E-31,
12.5064436508139));
#413908=CARTESIAN_POINT('',(-1.63904681284264,2.20817244464973,12.4908873016278));
#413909=CARTESIAN_POINT('Origin',(-1.6259344383399,2.19050706509254,12.4908873016278));
#413910=CARTESIAN_POINT('',(-1.70137838705825,2.1605118800995,12.4908873016278));
#413911=CARTESIAN_POINT('Origin',(-1.54319834818726E-15,2.01823002470004E-15,
12.4908873016278));
#413912=CARTESIAN_POINT('Origin',(-1.68776735996178,2.14322778505871,12.4908873016278));
#413913=CARTESIAN_POINT('Origin',(-6.86779499821049E-16,1.06864976125843E-15,
12.4908873016278));
#413914=CARTESIAN_POINT('',(-1.45020045405957,2.32895257233908,12.5064436508139));
#413915=CARTESIAN_POINT('',(-1.51605473498434,2.28663059580924,12.5064436508139));
#413916=CARTESIAN_POINT('Origin',(-2.78674301191578E-31,-8.18261577309334E-32,
12.5064436508139));
#413917=CARTESIAN_POINT('',(-1.45360646587299,2.33442246441647,12.4908873016278));
#413918=CARTESIAN_POINT('Origin',(-1.441977614146,2.31574708470114,12.4908873016278));
#413919=CARTESIAN_POINT('',(-1.51961541538732,2.29200108841973,12.4908873016278));
#413920=CARTESIAN_POINT('Origin',(-1.3735589996421E-15,2.13729952251686E-15,
12.4908873016278));
#413921=CARTESIAN_POINT('Origin',(-1.50745849206422,2.27366507971237,12.4908873016278));
#413922=CARTESIAN_POINT('Origin',(-5.97389421287801E-16,1.12107282232047E-15,
12.4908873016278));
#413923=CARTESIAN_POINT('',(-1.25554377609535,2.43940797478971,12.5064436508139));
#413924=CARTESIAN_POINT('',(-1.32462856631819,2.40259455640214,12.5064436508139));
#413925=CARTESIAN_POINT('Origin',(-2.42402517198019E-31,-6.05544687658534E-32,
12.5064436508139));
#413926=CARTESIAN_POINT('',(-1.25849260770113,2.44513728783511,12.4908873016278));
#413927=CARTESIAN_POINT('Origin',(-1.24842466683952,2.42557618953242,12.4908873016278));
#413928=CARTESIAN_POINT('',(-1.32773965384588,2.40823740765009,12.4908873016278));
#413929=CARTESIAN_POINT('Origin',(-1.1947788425756E-15,2.24214564464094E-15,
12.4908873016278));
#413930=CARTESIAN_POINT('Origin',(-1.31711773661511,2.38897150838889,12.4908873016278));
#413931=CARTESIAN_POINT('Origin',(-5.04023814718198E-16,1.16603532871396E-15,
12.4908873016278));
#413932=CARTESIAN_POINT('',(-1.05253166145136,2.53362951964209,12.5064436508139));
#413933=CARTESIAN_POINT('',(-1.12438721309152,2.50256964662238,12.5064436508139));
#413934=CARTESIAN_POINT('Origin',(-2.04517584446108E-31,-4.23100467173029E-32,
12.5064436508139));
#413935=CARTESIAN_POINT('',(-1.05500368886169,2.53958012602246,12.4908873016278));
#413936=CARTESIAN_POINT('Origin',(-1.0465636593508,2.51926348501428,12.4908873016278));
#413937=CARTESIAN_POINT('',(-1.12702800396973,2.50844730426374,12.4908873016278));
#413938=CARTESIAN_POINT('Origin',(-1.0080476294364E-15,2.33207065742792E-15,
12.4908873016278));
#413939=CARTESIAN_POINT('Origin',(-1.11801177993797,2.48837972582963,12.4908873016278));
#413940=CARTESIAN_POINT('Origin',(-4.07304012819722E-16,1.20323806237714E-15,
12.4908873016278));
#413941=CARTESIAN_POINT('',(-0.842515122255916,2.61099017806071,12.5064436508139));
#413942=CARTESIAN_POINT('',(-0.916663248472555,2.58589054873928,12.5064436508139));
#413943=CARTESIAN_POINT('Origin',(-1.65271620912734E-31,-2.72143052038969E-32,
12.5064436508139));
#413944=CARTESIAN_POINT('',(-0.844493894536228,2.61712247747236,12.4908873016278));
#413945=CARTESIAN_POINT('Origin',(-0.837737943379938,2.59618549765258,12.4908873016278));
#413946=CARTESIAN_POINT('',(-0.918816168673682,2.59196389793219,12.4908873016278));
#413947=CARTESIAN_POINT('Origin',(-8.14608025639444E-16,2.40647612475429E-15,
12.4908873016278));
#413948=CARTESIAN_POINT('Origin',(-0.911465639324292,2.57122818674873,12.4908873016278));
#413949=CARTESIAN_POINT('Origin',(-3.07873669916363E-16,1.23243344525552E-15,
12.4908873016278));
#413950=CARTESIAN_POINT('',(-0.626891783927067,2.67097512762739,12.5064436508139));
#413951=CARTESIAN_POINT('',(-0.702839041173797,2.65200277589623,12.5064436508139));
#413952=CARTESIAN_POINT('Origin',(-1.24925802010084E-31,-1.53677038947852E-32,
12.5064436508139));
#413953=CARTESIAN_POINT('',(-0.628364132674314,2.67724831062949,12.4908873016278));
#413954=CARTESIAN_POINT('Origin',(-0.62333721961292,2.65583032414446,12.4908873016278));
#413955=CARTESIAN_POINT('',(-0.704489763369112,2.65823139950384,12.4908873016278));
#413956=CARTESIAN_POINT('Origin',(-6.15747339832725E-16,2.46486689051103E-15,
12.4908873016278));
#413957=CARTESIAN_POINT('Origin',(-0.698853845262159,2.63696554830781,12.4908873016278));
#413958=CARTESIAN_POINT('Origin',(-2.0639447853529E-16,1.25342718689292E-15,
12.4908873016278));
#413959=CARTESIAN_POINT('',(-0.407096584206047,2.71318517839958,12.5064436508139));
#413960=CARTESIAN_POINT('',(-0.484337556016306,2.70046636212924,12.5064436508139));
#413961=CARTESIAN_POINT('Origin',(-8.37486225063633E-32,-6.84907996712842E-33,
12.5064436508139));
#413962=CARTESIAN_POINT('',(-0.408052711182237,2.71955749799427,12.4908873016278));
#413963=CARTESIAN_POINT('Origin',(-0.404788289492779,2.69780103801031,12.4908873016278));
#413964=CARTESIAN_POINT('',(-0.485475094921951,2.7068088096891,12.4908873016278));
#413965=CARTESIAN_POINT('Origin',(-4.1278895707058E-16,2.50685437378584E-15,
12.4908873016278));
#413966=CARTESIAN_POINT('Origin',(-0.481591294162575,2.68515433921159,12.4908873016278));
#413967=CARTESIAN_POINT('Origin',(9.93165549358168E-16,7.9202309636793E-16,
12.4908873016278));
#413968=CARTESIAN_POINT('',(2.16918417631513,1.679803991656,12.5064436508139));
#413969=CARTESIAN_POINT('',(2.12037668729674,1.74100664706597,12.5064436508139));
#413970=CARTESIAN_POINT('Origin',(4.02996471949226E-31,-1.94072872359725E-31,
12.5064436508139));
#413971=CARTESIAN_POINT('',(2.17427882851258,1.6837492615832,12.4908873016278));
#413972=CARTESIAN_POINT('Origin',(2.15688459788448,1.67027926749053,12.4908873016278));
#413973=CARTESIAN_POINT('',(2.12535670783502,1.74509566054721,12.4908873016278));
#413974=CARTESIAN_POINT('Origin',(1.98633109871634E-15,1.58404619273586E-15,
12.4908873016278));
#413975=CARTESIAN_POINT('Origin',(2.10835385417234,1.73113489526283,12.4908873016278));
#413976=CARTESIAN_POINT('Origin',(9.25303637785393E-16,8.70339917223882E-16,
12.4908873016278));
#413977=CARTESIAN_POINT('',(2.02504677505416,1.85102323054091,12.5064436508139));
#413978=CARTESIAN_POINT('',(1.9714131043355,1.90804397570225,12.5064436508139));
#413979=CARTESIAN_POINT('Origin',(3.75460165478233E-31,-1.62294280643948E-31,
12.5064436508139));
#413980=CARTESIAN_POINT('',(2.02980289909154,1.85537063435843,12.4908873016278));
#413981=CARTESIAN_POINT('Origin',(2.01356447589881,1.84052766928356,12.4908873016278));
#413982=CARTESIAN_POINT('',(1.97604326170699,1.91252530123458,12.4908873016278));
#413983=CARTESIAN_POINT('Origin',(1.85060727557078E-15,1.74067983444776E-15,
12.4908873016278));
#413984=CARTESIAN_POINT('Origin',(1.96023491561333,1.8972250988247,12.4908873016278));
#413985=CARTESIAN_POINT('Origin',(8.5128398316751E-16,9.42864769526687E-16,
12.4908873016278));
#413986=CARTESIAN_POINT('',(1.86743302161441,2.00992421522391,12.5064436508139));
#413987=CARTESIAN_POINT('',(1.80933009242518,2.06238358648533,12.5064436508139));
#413988=CARTESIAN_POINT('Origin',(3.45425233552549E-31,-1.3286589418254E-31,
12.5064436508139));
#413989=CARTESIAN_POINT('',(1.87181896627095,2.01464482167661,12.4908873016278));
#413990=CARTESIAN_POINT('Origin',(1.85684441454078,1.99852766310319,12.4908873016278));
#413991=CARTESIAN_POINT('',(1.81357957369649,2.06722740158669,12.4908873016278));
#413992=CARTESIAN_POINT('Origin',(1.70256796633502E-15,1.88572953905338E-15,
12.4908873016278));
#413993=CARTESIAN_POINT('Origin',(1.79907093710692,2.05068958237399,12.4908873016278));
#413994=CARTESIAN_POINT('Origin',(7.71599174093617E-16,1.00911501235003E-15,
12.4908873016278));
#413995=CARTESIAN_POINT('',(1.69739180952057,2.15544948586875,12.5064436508139));
#413996=CARTESIAN_POINT('',(1.63520628726822,2.20299837476969,12.5064436508139));
#413997=CARTESIAN_POINT('Origin',(3.13091553688725E-31,-1.05983554032057E-31,
12.5064436508139));
#413998=CARTESIAN_POINT('',(1.70137838705821,2.16051188009953,12.4908873016278));
#413999=CARTESIAN_POINT('Origin',(1.68776735996175,2.14322778505873,12.4908873016278));
#414000=CARTESIAN_POINT('',(1.63904681284261,2.20817244464976,12.4908873016278));
#414001=CARTESIAN_POINT('Origin',(1.54319834818723E-15,2.01823002470006E-15,
12.4908873016278));
#414002=CARTESIAN_POINT('Origin',(1.62593443833987,2.19050706509256,12.4908873016278));
#414003=CARTESIAN_POINT('Origin',(6.86779499821035E-16,1.06864976125844E-15,
12.4908873016278));
#414004=CARTESIAN_POINT('',(1.51605473498431,2.28663059580926,12.5064436508139));
#414005=CARTESIAN_POINT('',(1.45020045405953,2.3289525723391,12.5064436508139));
#414006=CARTESIAN_POINT('Origin',(2.78674301191572E-31,-8.18261577309295E-32,
12.5064436508139));
#414007=CARTESIAN_POINT('',(1.51961541538728,2.29200108841975,12.4908873016278));
#414008=CARTESIAN_POINT('Origin',(1.50745849206419,2.2736650797124,12.4908873016278));
#414009=CARTESIAN_POINT('',(1.45360646587295,2.33442246441649,12.4908873016278));
#414010=CARTESIAN_POINT('Origin',(1.37355899964207E-15,2.13729952251688E-15,
12.4908873016278));
#414011=CARTESIAN_POINT('Origin',(1.44197761414597,2.31574708470116,12.4908873016278));
#414012=CARTESIAN_POINT('Origin',(5.97389421287786E-16,1.12107282232048E-15,
12.4908873016278));
#414013=CARTESIAN_POINT('',(1.32462856631816,2.40259455640216,12.5064436508139));
#414014=CARTESIAN_POINT('',(1.25554377609532,2.43940797478972,12.5064436508139));
#414015=CARTESIAN_POINT('Origin',(2.42402517198013E-31,-6.05544687658502E-32,
12.5064436508139));
#414016=CARTESIAN_POINT('',(1.32773965384585,2.40823740765011,12.4908873016278));
#414017=CARTESIAN_POINT('Origin',(1.31711773661508,2.38897150838891,12.4908873016278));
#414018=CARTESIAN_POINT('',(1.2584926077011,2.44513728783512,12.4908873016278));
#414019=CARTESIAN_POINT('Origin',(1.19477884257557E-15,2.24214564464095E-15,
12.4908873016278));
#414020=CARTESIAN_POINT('Origin',(1.24842466683949,2.42557618953244,12.4908873016278));
#414021=CARTESIAN_POINT('Origin',(5.04023814718182E-16,1.16603532871397E-15,
12.4908873016278));
#414022=CARTESIAN_POINT('',(1.12438721309149,2.5025696466224,12.5064436508139));
#414023=CARTESIAN_POINT('',(1.05253166145133,2.53362951964211,12.5064436508139));
#414024=CARTESIAN_POINT('Origin',(2.04517584446102E-31,-4.23100467173001E-32,
12.5064436508139));
#414025=CARTESIAN_POINT('',(1.12702800396969,2.50844730426376,12.4908873016278));
#414026=CARTESIAN_POINT('Origin',(1.11801177993793,2.48837972582965,12.4908873016278));
#414027=CARTESIAN_POINT('',(1.05500368886165,2.53958012602247,12.4908873016278));
#414028=CARTESIAN_POINT('Origin',(1.00804762943636E-15,2.33207065742793E-15,
12.4908873016278));
#414029=CARTESIAN_POINT('Origin',(1.04656365935076,2.51926348501429,12.4908873016278));
#414030=CARTESIAN_POINT('Origin',(4.07304012819706E-16,1.20323806237715E-15,
12.4908873016278));
#414031=CARTESIAN_POINT('',(0.916663248472521,2.58589054873929,12.5064436508139));
#414032=CARTESIAN_POINT('',(0.842515122255881,2.61099017806072,12.5064436508139));
#414033=CARTESIAN_POINT('Origin',(1.65271620912728E-31,-2.72143052038947E-32,
12.5064436508139));
#414034=CARTESIAN_POINT('',(0.918816168673646,2.5919638979322,12.4908873016278));
#414035=CARTESIAN_POINT('Origin',(0.911465639324257,2.57122818674874,12.4908873016278));
#414036=CARTESIAN_POINT('',(0.844493894536193,2.61712247747237,12.4908873016278));
#414037=CARTESIAN_POINT('Origin',(8.14608025639412E-16,2.4064761247543E-15,
12.4908873016278));
#414038=CARTESIAN_POINT('Origin',(0.837737943379903,2.59618549765259,12.4908873016278));
#414039=CARTESIAN_POINT('Origin',(3.07873669916346E-16,1.23243344525552E-15,
12.4908873016278));
#414040=CARTESIAN_POINT('',(0.702839041173762,2.65200277589623,12.5064436508139));
#414041=CARTESIAN_POINT('',(0.626891783927031,2.67097512762739,12.5064436508139));
#414042=CARTESIAN_POINT('Origin',(1.24925802010077E-31,-1.53677038947836E-32,
12.5064436508139));
#414043=CARTESIAN_POINT('',(0.704489763369076,2.65823139950385,12.4908873016278));
#414044=CARTESIAN_POINT('Origin',(0.698853845262123,2.63696554830782,12.4908873016278));
#414045=CARTESIAN_POINT('',(0.628364132674278,2.6772483106295,12.4908873016278));
#414046=CARTESIAN_POINT('Origin',(6.15747339832692E-16,2.46486689051104E-15,
12.4908873016278));
#414047=CARTESIAN_POINT('Origin',(0.623337219612883,2.65583032414446,12.4908873016278));
#414048=CARTESIAN_POINT('Origin',(2.06394478535273E-16,1.25342718689292E-15,
12.4908873016278));
#414049=CARTESIAN_POINT('',(0.484337556016271,2.70046636212925,12.5064436508139));
#414050=CARTESIAN_POINT('',(0.407096584206011,2.71318517839958,12.5064436508139));
#414051=CARTESIAN_POINT('Origin',(8.37486225063565E-32,-6.84907996712733E-33,
12.5064436508139));
#414052=CARTESIAN_POINT('',(0.485475094921914,2.70680880968911,12.4908873016278));
#414053=CARTESIAN_POINT('Origin',(0.481591294162539,2.6851543392116,12.4908873016278));
#414054=CARTESIAN_POINT('',(0.408052711182201,2.71955749799427,12.4908873016278));
#414055=CARTESIAN_POINT('Origin',(4.12788957070546E-16,2.50685437378585E-15,
12.4908873016278));
#414056=CARTESIAN_POINT('Origin',(0.404788289492743,2.69780103801032,12.4908873016278));
#414057=CARTESIAN_POINT('Origin',(1.0354176595224E-16,1.26607957740248E-15,
12.4908873016278));
#414058=CARTESIAN_POINT('',(0.262612884333563,2.73095879026788,12.5064436508139));
#414059=CARTESIAN_POINT('',(0.184592223883309,2.73733942945357,12.5064436508139));
#414060=CARTESIAN_POINT('Origin',(4.2014109737406E-32,-1.71512345769042E-33,
12.5064436508139));
#414061=CARTESIAN_POINT('',(0.2632296698158,2.7373728538379,12.4908873016278));
#414062=CARTESIAN_POINT('Origin',(0.261123832457273,2.7154738710072,12.4908873016278));
#414063=CARTESIAN_POINT('',(0.185025766221164,2.7437684789053,12.4908873016278));
#414064=CARTESIAN_POINT('Origin',(2.0708353190448E-16,2.53215915480496E-15,
12.4908873016278));
#414065=CARTESIAN_POINT('Origin',(0.183545560091395,2.72181833107405,12.4908873016278));
#414066=CARTESIAN_POINT('Origin',(-1.03541765952257E-16,1.26607957740248E-15,
12.4908873016278));
#414067=CARTESIAN_POINT('',(-0.184592223883345,2.73733942945357,12.5064436508139));
#414068=CARTESIAN_POINT('',(-0.262612884333599,2.73095879026787,12.5064436508139));
#414069=CARTESIAN_POINT('Origin',(-4.20141097374128E-32,-1.71512345769099E-33,
12.5064436508139));
#414070=CARTESIAN_POINT('',(-0.185025766221201,2.74376847890529,12.4908873016278));
#414071=CARTESIAN_POINT('Origin',(-0.183545560091431,2.72181833107405,12.4908873016278));
#414072=CARTESIAN_POINT('',(-0.263229669815836,2.7373728538379,12.4908873016278));
#414073=CARTESIAN_POINT('Origin',(-2.07083531904513E-16,2.53215915480496E-15,
12.4908873016278));
#414074=CARTESIAN_POINT('Origin',(-0.261123832457309,2.7154738710072,12.4908873016278));
#414075=CARTESIAN_POINT('Origin',(0.,1.27030641721285E-15,12.4908873016278));
#414076=CARTESIAN_POINT('',(0.0391405672337278,2.74327713823376,12.5064436508139));
#414077=CARTESIAN_POINT('',(-0.0391405672337274,2.74327713823376,12.5064436508139));
#414078=CARTESIAN_POINT('Origin',(0.,0.,12.5064436508139));
#414079=CARTESIAN_POINT('',(0.0392324946869353,2.74972013327914,12.4908873016278));
#414080=CARTESIAN_POINT('Origin',(0.0389186347294398,2.72772237221291,12.4908873016278));
#414081=CARTESIAN_POINT('',(-3.36777869765522E-16,2.75,12.4908873016278));
#414082=CARTESIAN_POINT('Origin',(0.,2.5406128344257E-15,12.4908873016278));
#414083=CARTESIAN_POINT('',(-0.0392324946869358,2.74972013327914,12.4908873016278));
#414084=CARTESIAN_POINT('Origin',(0.,2.5406128344257E-15,12.4908873016278));
#414085=CARTESIAN_POINT('Origin',(-0.0389186347294403,2.72772237221291,
12.4908873016278));
#414086=CARTESIAN_POINT('Origin',(0.,2.5406128344257E-15,14.));
#414087=CARTESIAN_POINT('Ctrl Pts',(5.09848573616328E-14,1.50000000000006,
3.56249999999999));
#414088=CARTESIAN_POINT('Ctrl Pts',(0.0221291496324529,1.50000000000006,
3.56143531079189));
#414089=CARTESIAN_POINT('Ctrl Pts',(0.0442758983615595,1.49951030585925,
3.56035617223172));
#414090=CARTESIAN_POINT('Ctrl Pts',(0.257655251405688,1.49005198771531,
3.54982722226221));
#414091=CARTESIAN_POINT('Ctrl Pts',(0.4454768622445,1.44505001124848,3.53954059589557));
#414092=CARTESIAN_POINT('Ctrl Pts',(0.800824790268939,1.28383039135365,
3.51796558796231));
#414093=CARTESIAN_POINT('Ctrl Pts',(0.963787085995833,1.16647513895563,
3.50686519273134));
#414094=CARTESIAN_POINT('Ctrl Pts',(1.23044649741185,0.879343431360836,
3.48605965505124));
#414095=CARTESIAN_POINT('Ctrl Pts',(1.33323611595351,0.713948364951426,
3.47716379805274));
#414096=CARTESIAN_POINT('Ctrl Pts',(1.47075916267875,0.352640067717556,
3.45709111487308));
#414097=CARTESIAN_POINT('Ctrl Pts',(1.50394514491438,0.160070583293647,
3.44639281018286));
#414098=CARTESIAN_POINT('Ctrl Pts',(1.49519059383191,-0.232269284766078,
3.42459615084621));
#414099=CARTESIAN_POINT('Ctrl Pts',(1.45126380539184,-0.428248175400973,
3.41370843469983));
#414100=CARTESIAN_POINT('Ctrl Pts',(1.29309157908641,-0.783606459655687,
3.39396630779679));
#414101=CARTESIAN_POINT('Ctrl Pts',(1.18351469246117,-0.940972047829285,
3.38497043141703));
#414102=CARTESIAN_POINT('Ctrl Pts',(0.907270262029569,-1.21045797416603,
3.36419389488503));
#414103=CARTESIAN_POINT('Ctrl Pts',(0.741669889100236,-1.31843428196421,
3.35322710134436));
#414104=CARTESIAN_POINT('Ctrl Pts',(0.375529554756225,-1.46578458593757,
3.33151810229555));
#414105=CARTESIAN_POINT('Ctrl Pts',(0.178174599457163,-1.50258046483778,
3.32114410899197));
#414106=CARTESIAN_POINT('Ctrl Pts',(-0.211361302901406,-1.49724634791122,
3.30225438423687));
#414107=CARTESIAN_POINT('Ctrl Pts',(-0.399910321477038,-1.45824144824317,
3.29209934591581));
#414108=CARTESIAN_POINT('Ctrl Pts',(-0.75906562043593,-1.30885629638807,
3.27066989098638));
#414109=CARTESIAN_POINT('Ctrl Pts',(-0.925190190968117,-1.19721116860686,
3.25957596531059));
#414110=CARTESIAN_POINT('Ctrl Pts',(-1.20171588727651,-0.918512169742024,
3.23852997768644));
#414111=CARTESIAN_POINT('Ctrl Pts',(-1.31048317138742,-0.755257014255049,
3.22945872301403));
#414112=CARTESIAN_POINT('Ctrl Pts',(-1.45919026539019,-0.397526930631808,
3.20958482947941));
#414113=CARTESIAN_POINT('Ctrl Pts',(-1.49817895313977,-0.206657980265481,
3.1989809989035));
#414114=CARTESIAN_POINT('Ctrl Pts',(-1.50176649068865,0.187001885967594,
3.177111006335));
#414115=CARTESIAN_POINT('Ctrl Pts',(-1.46330637831753,0.386036190213434,
3.16605354498801));
#414116=CARTESIAN_POINT('Ctrl Pts',(-1.31424750513171,0.74767468120116,
3.14596251771092));
#414117=CARTESIAN_POINT('Ctrl Pts',(-1.20883176095049,0.908292547458259,
3.13709626334183));
#414118=CARTESIAN_POINT('Ctrl Pts',(-0.940116049528959,1.18504136043139,
3.11648020562108));
#414119=CARTESIAN_POINT('Ctrl Pts',(-0.778011313664844,1.29724039855353,
3.10556429793257));
#414120=CARTESIAN_POINT('Ctrl Pts',(-0.416757278153209,1.45458446347175,
3.08381278657525));
#414121=CARTESIAN_POINT('Ctrl Pts',(-0.220537971993564,1.49696084199159,
3.07319505918041));
#414122=CARTESIAN_POINT('Ctrl Pts',(-0.0144919151713928,1.4999475112981,
3.06319870061314));
#414123=CARTESIAN_POINT('Ctrl Pts',(-0.00724491145173278,1.50000000000006,
3.06284857096474));
#414124=CARTESIAN_POINT('Ctrl Pts',(0.,1.50000000000006,3.0625));
#414125=CARTESIAN_POINT('Ctrl Pts',(-2.98372437868011E-15,1.50000000000006,
3.00000000000002));
#414126=CARTESIAN_POINT('Ctrl Pts',(-0.188455291586078,1.50000000000006,
3.00906705944397));
#414127=CARTESIAN_POINT('Ctrl Pts',(-0.375366776561344,1.46448662492846,
3.01904632509861));
#414128=CARTESIAN_POINT('Ctrl Pts',(-0.733157320802567,1.32320528790295,
3.04018501226858));
#414129=CARTESIAN_POINT('Ctrl Pts',(-0.899553263327317,1.21622363549137,
3.05116245335296));
#414130=CARTESIAN_POINT('Ctrl Pts',(-1.1775370644247,0.948431228996448,
3.07197563317732));
#414131=CARTESIAN_POINT('Ctrl Pts',(-1.28807755391854,0.791807805127463,
3.08101067749294));
#414132=CARTESIAN_POINT('Ctrl Pts',(-1.44849369979861,0.437524057649878,
3.10069310790836));
#414133=CARTESIAN_POINT('Ctrl Pts',(-1.49367236884049,0.241835556225419,
3.11156469132083));
#414134=CARTESIAN_POINT('Ctrl Pts',(-1.50494300158585,-0.15055365529281,
3.13336409196073));
#414135=CARTESIAN_POINT('Ctrl Pts',(-1.47294822231951,-0.343448461845158,
3.14408047010253));
#414136=CARTESIAN_POINT('Ctrl Pts',(-1.33770341904721,-0.705474016485607,
3.16419300091589));
#414137=CARTESIAN_POINT('Ctrl Pts',(-1.23611227524098,-0.871305075546333,
3.17306377252695));
#414138=CARTESIAN_POINT('Ctrl Pts',(-0.971454761532004,-1.16011981675612,
3.19381974479247));
#414139=CARTESIAN_POINT('Ctrl Pts',(-0.809153893177124,-1.27861751448815,
3.20492005167678));
#414140=CARTESIAN_POINT('Ctrl Pts',(-0.454620812975482,-1.44221503163789,
3.22652190792741));
#414141=CARTESIAN_POINT('Ctrl Pts',(-0.266968976146824,-1.48842649888177,
3.23683396300421));
#414142=CARTESIAN_POINT('Ctrl Pts',(0.123342579191924,-1.50814342958972,
3.25616052898576));
#414143=CARTESIAN_POINT('Ctrl Pts',(0.322410969801838,-1.47844242014425,
3.26611082667975));
#414144=CARTESIAN_POINT('Ctrl Pts',(0.694687026706395,-1.34388282867076,
3.28775973324846));
#414145=CARTESIAN_POINT('Ctrl Pts',(0.86457198998191,-1.24142178853681,
3.29877946735871));
#414146=CARTESIAN_POINT('Ctrl Pts',(1.15031108047358,-0.981254372061885,
3.31975396843968));
#414147=CARTESIAN_POINT('Ctrl Pts',(1.26516247843284,-0.827900610361255,
3.32900552164662));
#414148=CARTESIAN_POINT('Ctrl Pts',(1.43549475582945,-0.478442146227225,
3.34841988076518));
#414149=CARTESIAN_POINT('Ctrl Pts',(1.48620129994845,-0.284140467929323,
3.35921441844839));
#414150=CARTESIAN_POINT('Ctrl Pts',(1.50864280780171,0.10827164962177,3.38101509164567));
#414151=CARTESIAN_POINT('Ctrl Pts',(1.48196418538353,0.302521670583031,
3.39180675947686));
#414152=CARTESIAN_POINT('Ctrl Pts',(1.35682312299937,0.667680854124861,
3.41209338078474));
#414153=CARTESIAN_POINT('Ctrl Pts',(1.26047230423381,0.835449643206916,
3.42089576585393));
#414154=CARTESIAN_POINT('Ctrl Pts',(1.00465686502723,1.13159161946978,3.44142985791863));
#414155=CARTESIAN_POINT('Ctrl Pts',(0.845354804113819,1.25506895416932,
3.45252420786174));
#414156=CARTESIAN_POINT('Ctrl Pts',(0.494587291621475,1.42907193518553,
3.47423393381445));
#414157=CARTESIAN_POINT('Ctrl Pts',(0.307773091644003,1.48059404892646,
3.4846532060277));
#414158=CARTESIAN_POINT('Ctrl Pts',(0.07754992579976,1.49849817898652,3.49622716020497));
#414159=CARTESIAN_POINT('Ctrl Pts',(0.0387540406423458,1.50000000000006,
3.49813544535027));
#414160=CARTESIAN_POINT('Ctrl Pts',(2.54638793255616E-13,1.50000000000006,
3.50000000000001));
#414161=CARTESIAN_POINT('Origin',(0.,2.54061283442571E-15,-14.));
#414162=CARTESIAN_POINT('Origin',(0.,2.54061283442571E-15,-14.));
#414163=CARTESIAN_POINT('Ctrl Pts',(-0.823407874165269,-0.838564036615697,
-14.));
#414164=CARTESIAN_POINT('Ctrl Pts',(-0.756416185228378,-0.929775963188785,
-13.9818543033194));
#414165=CARTESIAN_POINT('Ctrl Pts',(-0.676968561320634,-1.01110546462205,
-13.9635779264192));
#414166=CARTESIAN_POINT('Ctrl Pts',(-0.493123550224768,-1.15288970360126,
-13.9268301874654));
#414167=CARTESIAN_POINT('Ctrl Pts',(-0.388650102107146,-1.21130894798347,
-13.9085879752964));
#414168=CARTESIAN_POINT('Ctrl Pts',(-0.0867303172682547,-1.32599918452642,
-13.8617929132792));
#414169=CARTESIAN_POINT('Ctrl Pts',(0.0922000261171598,-1.33900590687874,
-13.8403605160919));
#414170=CARTESIAN_POINT('Ctrl Pts',(0.415180403822383,-1.32700291925115,
-13.7965652989098));
#414171=CARTESIAN_POINT('Ctrl Pts',(0.594058047496376,-1.2850341936251,
-13.7710785130787));
#414172=CARTESIAN_POINT('Ctrl Pts',(0.927045689042117,-1.1348132370896,
-13.7211832277058));
#414173=CARTESIAN_POINT('Ctrl Pts',(1.07787156833995,-1.02758606827755,
-13.6972272991397));
#414174=CARTESIAN_POINT('Ctrl Pts',(1.20419349529485,-0.894381364905194,
-13.6752404735808));
#414175=CARTESIAN_POINT('Ctrl Pts',(0.2433378840056,-1.48013062741362,-13.6752404735808));
#414176=CARTESIAN_POINT('Ctrl Pts',(0.0878351636314239,-1.50046100868921,
-13.6804058622075));
#414177=CARTESIAN_POINT('Ctrl Pts',(-0.113668939415186,-1.50249934332334,
-13.6862245455364));
#414178=CARTESIAN_POINT('Ctrl Pts',(-0.508346872926709,-1.39607161064129,
-13.7001701627267));
#414179=CARTESIAN_POINT('Ctrl Pts',(-0.670210107973824,-1.31887778576118,
-13.7065578661612));
#414180=CARTESIAN_POINT('Ctrl Pts',(-0.960585995374814,-1.10865683103123,
-13.7194722663245));
#414181=CARTESIAN_POINT('Ctrl Pts',(-1.08605380403871,-0.976577419570047,
-13.7258892843333));
#414182=CARTESIAN_POINT('Ctrl Pts',(-1.28730702605004,-0.666237733335184,
-13.738138899672));
#414183=CARTESIAN_POINT('Ctrl Pts',(-1.35775902821766,-0.490214386563022,
-13.7441298583672));
#414184=CARTESIAN_POINT('Ctrl Pts',(-1.42412756405518,-0.123231367734631,
-13.7576357071516));
#414185=CARTESIAN_POINT('Ctrl Pts',(-1.42122151653519,0.062238330299575,
-13.764557557877));
#414186=CARTESIAN_POINT('Ctrl Pts',(-1.34076312397572,0.439251787203608,
-13.7788380930996));
#414187=CARTESIAN_POINT('Ctrl Pts',(-1.26392881942988,0.592902262433157,
-13.7847532065818));
#414188=CARTESIAN_POINT('Ctrl Pts',(-1.10178307552258,0.850803513425684,
-13.7948280321824));
#414189=CARTESIAN_POINT('Ctrl Pts',(-0.97694301654997,0.982455774393795,
-13.8014111507482));
#414190=CARTESIAN_POINT('Ctrl Pts',(-0.687878136749956,1.18635983250677,
-13.814959411892));
#414191=CARTESIAN_POINT('Ctrl Pts',(-0.527665126931193,1.25844424723993,
-13.8217821937768));
#414192=CARTESIAN_POINT('Ctrl Pts',(-0.246854066918538,1.32456649908357,
-13.8327263387908));
#414193=CARTESIAN_POINT('Ctrl Pts',(-0.126033019444995,1.33805763116345,
-13.8371828424174));
#414194=CARTESIAN_POINT('Ctrl Pts',(2.82071241364257E-12,1.33373412263468,
-13.8415063509462));
#414195=CARTESIAN_POINT('Origin',(0.,2.12729453971344E-15,10.875));
#414196=CARTESIAN_POINT('',(-1.99005104861452E-16,1.62500000000006,11.));
#414197=CARTESIAN_POINT('Origin',(0.,2.1119864547241E-15,11.));
#414198=CARTESIAN_POINT('',(-1.8369701987211E-16,1.50000000000006,10.875));
#414199=CARTESIAN_POINT('Origin',(0.,-1.19311743680736E-13,1002.5));
#414200=CARTESIAN_POINT('Ctrl Pts',(5.31356209032552E-12,1.22263611415557,
3.72263611415548));
#414201=CARTESIAN_POINT('Ctrl Pts',(-0.115140231501621,1.22694486240484,
3.72694486240474));
#414202=CARTESIAN_POINT('Ctrl Pts',(-0.223387617715824,1.21491489606931,
3.73130199756615));
#414203=CARTESIAN_POINT('Ctrl Pts',(-0.477646668670485,1.15783281542956,
3.7420580001785));
#414204=CARTESIAN_POINT('Ctrl Pts',(-0.626800140389253,1.09224861512651,
3.74894844269113));
#414205=CARTESIAN_POINT('Ctrl Pts',(-0.883097504433533,0.913997938980513,
3.76196824108044));
#414206=CARTESIAN_POINT('Ctrl Pts',(-0.990260824443083,0.806192221606663,
3.76801225902082));
#414207=CARTESIAN_POINT('Ctrl Pts',(-1.1594027114994,0.559881561084235,
3.77898658930956));
#414208=CARTESIAN_POINT('Ctrl Pts',(-1.23589039363347,0.402018119962777,
3.78540611680621));
#414209=CARTESIAN_POINT('Ctrl Pts',(-1.30922461006992,0.052236834727649,
3.79979386655726));
#414210=CARTESIAN_POINT('Ctrl Pts',(-1.31196909528878,-0.114702199266043,
3.80655334440203));
#414211=CARTESIAN_POINT('Ctrl Pts',(-1.25359061453279,-0.447247862144007,
3.81982054016495));
#414212=CARTESIAN_POINT('Ctrl Pts',(-1.19080632970482,-0.607717569079429,
3.82575565648249));
#414213=CARTESIAN_POINT('Ctrl Pts',(-1.0090355403278,-0.894191254356796,
3.83788884476785));
#414214=CARTESIAN_POINT('Ctrl Pts',(-0.894427795580347,-1.01729807198153,
3.84429372566382));
#414215=CARTESIAN_POINT('Ctrl Pts',(-0.615801045481274,-1.22339207350308,
3.85780068559773));
#414216=CARTESIAN_POINT('Ctrl Pts',(-0.451389920483652,-1.30044995450671,
3.86478375140228));
#414217=CARTESIAN_POINT('Ctrl Pts',(-0.0544533398554264,-1.39747377486497,
3.87971469241723));
#414218=CARTESIAN_POINT('Ctrl Pts',(0.137352170431063,-1.3850270031156,
3.88569345776851));
#414219=CARTESIAN_POINT('Ctrl Pts',(0.441490712532983,-1.33694519343306,
3.89675172792063));
#414220=CARTESIAN_POINT('Ctrl Pts',(0.609869556531502,-1.27636341835511,
3.90343513599766));
#414221=CARTESIAN_POINT('Ctrl Pts',(0.922667308153377,-1.09142050062308,
3.91702496349085));
#414222=CARTESIAN_POINT('Ctrl Pts',(1.06243642188326,-0.965913476410583,
3.92379303130526));
#414223=CARTESIAN_POINT('Ctrl Pts',(1.28233086394066,-0.671442131958786,
3.93607517114796));
#414224=CARTESIAN_POINT('Ctrl Pts',(1.36257154856445,-0.505299200941526,
3.94189107383887));
#414225=CARTESIAN_POINT('Ctrl Pts',(1.4594463320603,-0.149070381108668,
3.95499431856923));
#414226=CARTESIAN_POINT('Ctrl Pts',(1.4732980264083,0.0398859931747112,
3.96184849000785));
#414227=CARTESIAN_POINT('Ctrl Pts',(1.43253582146537,0.380306004358064,
3.97402788695104));
#414228=CARTESIAN_POINT('Ctrl Pts',(1.38965366882792,0.53041702884642,3.97933564957226));
#414229=CARTESIAN_POINT('Ctrl Pts',(1.25552926384395,0.817304591643929,
3.98938551561423));
#414230=CARTESIAN_POINT('Ctrl Pts',(1.16283360252483,0.952666431224754,
3.99446704079842));
#414231=CARTESIAN_POINT('Ctrl Pts',(1.05094390383308,1.07028823734367,4.));
#414232=CARTESIAN_POINT('Origin',(0.,2.35813972515597E-15,12.5));
#414233=CARTESIAN_POINT('',(0.,2.35813972515597E-15,11.778312163513));
#414234=CARTESIAN_POINT('',(-1.25,2.35813972515597E-15,12.5));
#414235=CARTESIAN_POINT('',(-1.25,2.20505887526255E-15,12.5));
#414236=CARTESIAN_POINT('',(-0.624999999999998,-1.08253175473054,12.5));
#414237=CARTESIAN_POINT('Origin',(0.,2.35813972515597E-15,12.5));
#414238=CARTESIAN_POINT('',(0.624999999999998,-1.08253175473054,12.5));
#414239=CARTESIAN_POINT('Origin',(0.,2.35813972515597E-15,12.5));
#414240=CARTESIAN_POINT('',(1.25,1.79477175062954E-15,12.5));
#414241=CARTESIAN_POINT('Origin',(0.,2.35813972515597E-15,12.5));
#414242=CARTESIAN_POINT('',(0.624999999999999,1.08253175473055,12.5));
#414243=CARTESIAN_POINT('Origin',(0.,2.35813972515597E-15,12.5));
#414244=CARTESIAN_POINT('',(-0.624999999999998,1.08253175473055,12.5));
#414245=CARTESIAN_POINT('Origin',(0.,2.35813972515597E-15,12.5));
#414246=CARTESIAN_POINT('Origin',(0.,2.35813972515597E-15,12.5));
#414247=CARTESIAN_POINT('Origin',(0.,-1.34815096107107E-30,14.));
#414248=CARTESIAN_POINT('',(1.25,0.721687836487035,14.));
#414249=CARTESIAN_POINT('',(1.25,-0.721687836487022,14.));
#414250=CARTESIAN_POINT('Ctrl Pts',(1.25,0.721687836487029,14.));
#414251=CARTESIAN_POINT('Ctrl Pts',(1.25,3.60822483003176E-15,13.6391560817565));
#414252=CARTESIAN_POINT('Ctrl Pts',(1.25,-0.721687836487019,14.));
#414253=CARTESIAN_POINT('Origin',(0.,-1.34815096107107E-30,14.));
#414254=CARTESIAN_POINT('Origin',(0.,2.60208521396521E-15,11.088));
#414255=CARTESIAN_POINT('',(-3.12992118721911E-16,2.55577460325564,11.0257746032556));
#414256=CARTESIAN_POINT('Origin',(0.,2.5406128344257E-15,11.0257746032556));
#414257=CARTESIAN_POINT('',(-3.05371705427039E-16,2.49354920651122,11.));
#414258=CARTESIAN_POINT('Origin',(-3.05371705427039E-16,2.49354920651122,
11.088));
#414259=CARTESIAN_POINT('Origin',(0.,2.5406128344257E-15,11.));
#414260=CARTESIAN_POINT('Origin',(0.,2.5406128344257E-15,11.0257746032556));
#414261=CARTESIAN_POINT('',(-3.33621391227899E-16,2.72422539674443,11.1942253967444));
#414262=CARTESIAN_POINT('Origin',(0.,2.5406128344257E-15,11.1942253967444));
#414263=CARTESIAN_POINT('',(-3.12992118721911E-16,2.55577460325564,11.0257746032556));
#414264=CARTESIAN_POINT('Origin',(0.,2.60208521396521E-15,11.2564507934888));
#414265=CARTESIAN_POINT('',(-3.36777869765522E-16,2.75,11.2564507934888));
#414266=CARTESIAN_POINT('Origin',(0.,2.5406128344257E-15,11.2564507934888));
#414267=CARTESIAN_POINT('Origin',(-3.26000977933025E-16,2.662,11.2564507934888));
#414268=CARTESIAN_POINT('Origin',(0.,2.5406128344257E-15,13.8057746032556));
#414269=CARTESIAN_POINT('',(3.7272661817839E-12,2.65571825406948,13.8742817459305));
#414270=CARTESIAN_POINT('',(-0.0523410482444132,2.69040761867485,13.8390832900376));
#414271=CARTESIAN_POINT('Ctrl Pts',(3.72682759446776E-12,2.65571825406948,
13.8742817459305));
#414272=CARTESIAN_POINT('Ctrl Pts',(-0.000866695601887436,2.65571825406942,
13.8742817459306));
#414273=CARTESIAN_POINT('Ctrl Pts',(-0.00173384839344961,2.65573803419417,
13.8742615387396));
#414274=CARTESIAN_POINT('Ctrl Pts',(-0.00259288537059199,2.65577720866165,
13.8742215255972));
#414275=CARTESIAN_POINT('Ctrl Pts',(-0.00713269347825356,2.65598423649613,
13.8740100655633));
#414276=CARTESIAN_POINT('Ctrl Pts',(-0.0116665345428952,2.65675308215573,
13.8732246156103));
#414277=CARTESIAN_POINT('Ctrl Pts',(-0.0158696469572718,2.65797057625734,
13.8719820486038));
#414278=CARTESIAN_POINT('Ctrl Pts',(-0.0201451887618009,2.6592090506104,
13.8707180692815));
#414279=CARTESIAN_POINT('Ctrl Pts',(-0.0241780317224058,2.66093171307035,
13.868960862563));
#414280=CARTESIAN_POINT('Ctrl Pts',(-0.0277864605543921,2.66294927630088,
13.8669057591701));
#414281=CARTESIAN_POINT('Ctrl Pts',(-0.033342610859648,2.66605585954836,
13.8637413727084));
#414282=CARTESIAN_POINT('Ctrl Pts',(-0.038077514536549,2.66993490073839,
13.8597962563956));
#414283=CARTESIAN_POINT('Ctrl Pts',(-0.041917102398969,2.6741245431149,
13.855546950204));
#414284=CARTESIAN_POINT('Ctrl Pts',(-0.0464962509255301,2.6791211717643,
13.850479165618));
#414285=CARTESIAN_POINT('Ctrl Pts',(-0.0499450320083385,2.68468912462994,
13.8448473071436));
#414286=CARTESIAN_POINT('Ctrl Pts',(-0.0523410482444142,2.69040761867485,
13.8390832900376));
#414287=CARTESIAN_POINT('',(-0.0661728417005766,2.72342159191127,13.8057746032556));
#414288=CARTESIAN_POINT('',(-0.0523410482444132,2.69040761867485,13.8390832900376));
#414289=CARTESIAN_POINT('',(-0.156031485724598,2.71975333214794,13.8057746032556));
#414290=CARTESIAN_POINT('Origin',(0.,2.5406128344257E-15,13.8057746032556));
#414291=CARTESIAN_POINT('',(-0.167126309723535,2.68572179060922,13.8390832900376));
#414292=CARTESIAN_POINT('',(-0.156031485724598,2.71975333214794,13.8057746032556));
#414293=CARTESIAN_POINT('',(-0.27146008517196,2.67718922792421,13.8390832900376));
#414294=CARTESIAN_POINT('Ctrl Pts',(-0.167126309723536,2.68572179060922,
13.8390832900376));
#414295=CARTESIAN_POINT('Ctrl Pts',(-0.169287253635042,2.67909395725023,
13.8455641171218));
#414296=CARTESIAN_POINT('Ctrl Pts',(-0.172798832469115,2.67252844642108,
13.851896480191));
#414297=CARTESIAN_POINT('Ctrl Pts',(-0.17782767861645,2.66662913816789,
13.8574481026913));
#414298=CARTESIAN_POINT('Ctrl Pts',(-0.181226763520718,2.6626416927298,
13.8612005412592));
#414299=CARTESIAN_POINT('Ctrl Pts',(-0.185412613168551,2.6588765980049,
13.8646714234115));
#414300=CARTESIAN_POINT('Ctrl Pts',(-0.190316524340427,2.65572590449234,
13.8674635290331));
#414301=CARTESIAN_POINT('Ctrl Pts',(-0.194268697023493,2.65318668948689,
13.8697137499649));
#414302=CARTESIAN_POINT('Ctrl Pts',(-0.198787314993229,2.65099882204377,
13.8715630732995));
#414303=CARTESIAN_POINT('Ctrl Pts',(-0.203607653128417,2.64944501921187,
13.8727429581918));
#414304=CARTESIAN_POINT('Ctrl Pts',(-0.208483548820085,2.64787330778389,
13.873936442031));
#414305=CARTESIAN_POINT('Ctrl Pts',(-0.213819966241819,2.64691770663781,
13.8744652622107));
#414306=CARTESIAN_POINT('Ctrl Pts',(-0.219073920661324,2.64672829398743,
13.8742206332401));
#414307=CARTESIAN_POINT('Ctrl Pts',(-0.223596332596698,2.64656525450091,
13.8740100655633));
#414308=CARTESIAN_POINT('Ctrl Pts',(-0.228177755399591,2.64696202456949,
13.8732246156103));
#414309=CARTESIAN_POINT('Ctrl Pts',(-0.232466119376086,2.64783287487835,
13.8719820486038));
#414310=CARTESIAN_POINT('Ctrl Pts',(-0.236828381825177,2.6487187319609,
13.8707180692815));
#414311=CARTESIAN_POINT('Ctrl Pts',(-0.24098821881642,2.65010694826325,
13.868960862563));
#414312=CARTESIAN_POINT('Ctrl Pts',(-0.244749091032574,2.65182367776974,
13.8669057591701));
#414313=CARTESIAN_POINT('Ctrl Pts',(-0.25053996908082,2.65446704628708,
13.8637413727084));
#414314=CARTESIAN_POINT('Ctrl Pts',(-0.255575295624587,2.65794724168118,
13.8597962563956));
#414315=CARTESIAN_POINT('Ctrl Pts',(-0.259743602323567,2.66180998131253,
13.855546950204));
#414316=CARTESIAN_POINT('Ctrl Pts',(-0.264714785732522,2.66641674097663,
13.850479165618));
#414317=CARTESIAN_POINT('Ctrl Pts',(-0.268605931129685,2.67168505926326,
13.8448473071436));
#414318=CARTESIAN_POINT('Ctrl Pts',(-0.27146008517196,2.67718922792421,
13.8390832900376));
#414319=CARTESIAN_POINT('',(-0.287936799781984,2.70896593031337,13.8057746032556));
#414320=CARTESIAN_POINT('',(-0.27146008517196,2.67718922792421,13.8390832900376));
#414321=CARTESIAN_POINT('',(-0.377197449355658,2.69798556268688,13.8057746032556));
#414322=CARTESIAN_POINT('Origin',(0.,2.5406128344257E-15,13.8057746032556));
#414323=CARTESIAN_POINT('',(-0.385481469674173,2.66316292713999,13.8390832900376));
#414324=CARTESIAN_POINT('',(-0.377197449355658,2.69798556268688,13.8057746032556));
#414325=CARTESIAN_POINT('',(-0.488772600020449,2.64615458456686,13.8390832900376));
#414326=CARTESIAN_POINT('Ctrl Pts',(-0.385481469674174,2.66316292713999,
13.8390832900376));
#414327=CARTESIAN_POINT('Ctrl Pts',(-0.387094993274519,2.65638101035973,
13.8455641171218));
#414328=CARTESIAN_POINT('Ctrl Pts',(-0.390059737535903,2.64955111945136,
13.851896480191));
#414329=CARTESIAN_POINT('Ctrl Pts',(-0.394591002223392,2.64326154301319,
13.8574481026913));
#414330=CARTESIAN_POINT('Ctrl Pts',(-0.397653763132204,2.6390103084956,
13.8612005412592));
#414331=CARTESIAN_POINT('Ctrl Pts',(-0.401518794537129,2.63491655620696,
13.8646714234115));
#414332=CARTESIAN_POINT('Ctrl Pts',(-0.406149577578239,2.63137663208095,
13.8674635290331));
#414333=CARTESIAN_POINT('Ctrl Pts',(-0.409881630136867,2.62852372734011,
13.8697137499649));
#414334=CARTESIAN_POINT('Ctrl Pts',(-0.414206881270284,2.62597483053209,
13.8715630732995));
#414335=CARTESIAN_POINT('Ctrl Pts',(-0.418884530772376,2.62403329554307,
13.8727429581918));
#414336=CARTESIAN_POINT('Ctrl Pts',(-0.423616093250925,2.62206938309073,
13.873936442031));
#414337=CARTESIAN_POINT('Ctrl Pts',(-0.42885686381914,2.62068199406788,
13.8744652622107));
#414338=CARTESIAN_POINT('Ctrl Pts',(-0.434077897249308,2.62006496561196,
13.8742206332401));
#414339=CARTESIAN_POINT('Ctrl Pts',(-0.438571972000304,2.61953385006912,
13.8740100655633));
#414340=CARTESIAN_POINT('Ctrl Pts',(-0.443170490940781,2.61955587142774,
13.8732246156103));
#414341=CARTESIAN_POINT('Ctrl Pts',(-0.447515568124662,2.62007428257872,
13.8719820486038));
#414342=CARTESIAN_POINT('Ctrl Pts',(-0.451935521081438,2.62060162715804,
13.8707180692815));
#414343=CARTESIAN_POINT('Ctrl Pts',(-0.456194669074472,2.62164615895233,
13.868960862563));
#414344=CARTESIAN_POINT('Ctrl Pts',(-0.460082956690694,2.62305063018316,
13.8669057591701));
#414345=CARTESIAN_POINT('Ctrl Pts',(-0.466070025143948,2.62521319278899,
13.8637413727084));
#414346=CARTESIAN_POINT('Ctrl Pts',(-0.4713722652872,2.62827138226101,13.8597962563956));
#414347=CARTESIAN_POINT('Ctrl Pts',(-0.47584155142938,2.63178151325225,
13.855546950204));
#414348=CARTESIAN_POINT('Ctrl Pts',(-0.48117168731533,2.63596774670555,
13.850479165618));
#414349=CARTESIAN_POINT('Ctrl Pts',(-0.485479302096222,2.6409013706242,
13.8448473071436));
#414350=CARTESIAN_POINT('Ctrl Pts',(-0.488772600020449,2.64615458456686,
13.8390832900376));
#414351=CARTESIAN_POINT('',(-0.50778458596707,2.67648254739715,13.8057746032556));
#414352=CARTESIAN_POINT('',(-0.488772600020449,2.64615458456686,13.8390832900376));
#414353=CARTESIAN_POINT('',(-0.595853226194454,2.65826314444243,13.8057746032556));
#414354=CARTESIAN_POINT('Origin',(0.,2.5406128344257E-15,13.8057746032556));
#414355=CARTESIAN_POINT('',(-0.601271314044095,2.62288115378159,13.8390832900376));
#414356=CARTESIAN_POINT('',(-0.595853226194454,2.65826314444243,13.8057746032556));
#414357=CARTESIAN_POINT('',(-0.702832413857604,2.597510219034,13.8390832900376));
#414358=CARTESIAN_POINT('Ctrl Pts',(-0.601271314044095,2.62288115378159,
13.8390832900376));
#414359=CARTESIAN_POINT('Ctrl Pts',(-0.602326679599933,2.61599028611731,
13.8455641171218));
#414360=CARTESIAN_POINT('Ctrl Pts',(-0.604724859404717,2.60894146692686,
13.851896480191));
#414361=CARTESIAN_POINT('Ctrl Pts',(-0.608728387813473,2.6023034783972,
13.8574481026913));
#414362=CARTESIAN_POINT('Ctrl Pts',(-0.611434442558301,2.5978167460644,
13.8612005412592));
#414363=CARTESIAN_POINT('Ctrl Pts',(-0.614952934574,2.5934215794581,13.8646714234115));
#414364=CARTESIAN_POINT('Ctrl Pts',(-0.619279772387232,2.58951598232965,
13.8674635290331));
#414365=CARTESIAN_POINT('Ctrl Pts',(-0.62276686862739,2.58636837346377,
13.8697137499649));
#414366=CARTESIAN_POINT('Ctrl Pts',(-0.626869969091811,2.58347540977857,
13.8715630732995));
#414367=CARTESIAN_POINT('Ctrl Pts',(-0.631373800975127,2.58115906322746,
13.8727429581918));
#414368=CARTESIAN_POINT('Ctrl Pts',(-0.635929542472916,2.57881601926411,
13.873936442031));
#414369=CARTESIAN_POINT('Ctrl Pts',(-0.641039789724145,2.57700607520953,
13.8744652622107));
#414370=CARTESIAN_POINT('Ctrl Pts',(-0.646193157048908,2.57596553717062,
13.8742206332401));
#414371=CARTESIAN_POINT('Ctrl Pts',(-0.650628987289528,2.57506988005778,
13.8740100655633));
#414372=CARTESIAN_POINT('Ctrl Pts',(-0.655213999982748,2.57471700615793,
13.8732246156103));
#414373=CARTESIAN_POINT('Ctrl Pts',(-0.659586874602242,2.57487952821036,
13.8719820486038));
#414374=CARTESIAN_POINT('Ctrl Pts',(-0.664035104009018,2.57504485089527,
13.8707180692815));
#414375=CARTESIAN_POINT('Ctrl Pts',(-0.668365219076652,2.57573874699475,
13.868960862563));
#414376=CARTESIAN_POINT('Ctrl Pts',(-0.67235504618038,2.5768216134256,13.8669057591701));
#414377=CARTESIAN_POINT('Ctrl Pts',(-0.678498462085881,2.57848897862259,
13.8637413727084));
#414378=CARTESIAN_POINT('Ctrl Pts',(-0.684032330295278,2.58110481042614,
13.8597962563956));
#414379=CARTESIAN_POINT('Ctrl Pts',(-0.688772853518762,2.58423897343466,
13.855546950204));
#414380=CARTESIAN_POINT('Ctrl Pts',(-0.694426470706797,2.58797682198422,
13.850479165618));
#414381=CARTESIAN_POINT('Ctrl Pts',(-0.699121888405755,2.59254291908168,
13.8448473071436));
#414382=CARTESIAN_POINT('Ctrl Pts',(-0.702832413857603,2.597510219034,13.8390832900376));
#414383=CARTESIAN_POINT('',(-0.724253149511105,2.62618761471653,13.8057746032556));
#414384=CARTESIAN_POINT('',(-0.702832413857604,2.597510219034,13.8390832900376));
#414385=CARTESIAN_POINT('',(-0.810543698121789,2.60085042355425,13.8057746032556));
#414386=CARTESIAN_POINT('Origin',(0.,2.5406128344257E-15,13.8057746032556));
#414387=CARTESIAN_POINT('',(-0.813059797021838,2.56514453908971,13.8390832900376));
#414388=CARTESIAN_POINT('',(-0.810543698121789,2.60085042355425,13.8057746032556));
#414389=CARTESIAN_POINT('',(-0.912214993939723,2.53157985155249,13.8390832900376));
#414390=CARTESIAN_POINT('Ctrl Pts',(-0.813059797021838,2.56514453908971,
13.8390832900376));
#414391=CARTESIAN_POINT('Ctrl Pts',(-0.813549981249516,2.55819057812879,
13.8455641171218));
#414392=CARTESIAN_POINT('Ctrl Pts',(-0.81536563710677,2.55096973938501,
13.851896480191));
#414393=CARTESIAN_POINT('Ctrl Pts',(-0.818814786415766,2.54402751348232,
13.8574481026913));
#414394=CARTESIAN_POINT('Ctrl Pts',(-0.821146126648752,2.53933514179775,
13.8612005412592));
#414395=CARTESIAN_POINT('Ctrl Pts',(-0.824294664291374,2.53466780998238,
13.8646714234115));
#414396=CARTESIAN_POINT('Ctrl Pts',(-0.828288762484958,2.53042253095601,
13.8674635290331));
#414397=CARTESIAN_POINT('Ctrl Pts',(-0.831507696356497,2.52700116478278,
13.8697137499649));
#414398=CARTESIAN_POINT('Ctrl Pts',(-0.835361340695299,2.5237833864164,
13.8715630732995));
#414399=CARTESIAN_POINT('Ctrl Pts',(-0.839661382701735,2.52110764320733,
13.8727429581918));
#414400=CARTESIAN_POINT('Ctrl Pts',(-0.844010985510741,2.51840106030397,
13.873936442031));
#414401=CARTESIAN_POINT('Ctrl Pts',(-0.848956701592656,2.51618060609673,
13.8744652622107));
#414402=CARTESIAN_POINT('Ctrl Pts',(-0.854008108002714,2.51472348308381,
13.8742206332401));
#414403=CARTESIAN_POINT('Ctrl Pts',(-0.858356174014567,2.51346924485128,
13.8740100655633));
#414404=CARTESIAN_POINT('Ctrl Pts',(-0.862897167957527,2.51274382401054,
13.8732246156103));
#414405=CARTESIAN_POINT('Ctrl Pts',(-0.867268739253517,2.51254937540697,
13.8719820486038));
#414406=CARTESIAN_POINT('Ctrl Pts',(-0.871715642877495,2.51235157600229,
13.8707180692815));
#414407=CARTESIAN_POINT('Ctrl Pts',(-0.876087908818377,2.5126902186429,
13.868960862563));
#414408=CARTESIAN_POINT('Ctrl Pts',(-0.880152723768509,2.51344427397633,
13.8669057591701));
#414409=CARTESIAN_POINT('Ctrl Pts',(-0.886411603706999,2.51460534572418,
13.8637413727084));
#414410=CARTESIAN_POINT('Ctrl Pts',(-0.892140273002629,2.51676141193022,
13.8597962563956));
#414411=CARTESIAN_POINT('Ctrl Pts',(-0.897120485907497,2.51949874961829,
13.855546950204));
#414412=CARTESIAN_POINT('Ctrl Pts',(-0.903059960508011,2.5227633384987,
13.850479165618));
#414413=CARTESIAN_POINT('Ctrl Pts',(-0.908111933894941,2.52693152215215,
13.8448473071436));
#414414=CARTESIAN_POINT('Ctrl Pts',(-0.912214993939722,2.53157985155249,
13.8390832900376));
#414415=CARTESIAN_POINT('',(-0.935901927838502,2.55841583675044,13.8057746032556));
#414416=CARTESIAN_POINT('',(-0.912214993939723,2.53157985155249,13.8390832900376));
#414417=CARTESIAN_POINT('',(-1.01984013546842,2.52612947220744,13.8057746032556));
#414418=CARTESIAN_POINT('Origin',(0.,2.5406128344257E-15,13.8057746032556));
#414419=CARTESIAN_POINT('',(-1.01943750119583,2.49033731070925,13.8390832900376));
#414420=CARTESIAN_POINT('',(-1.01984013546842,2.52612947220744,13.8057746032556));
#414421=CARTESIAN_POINT('',(-1.11552693374205,2.44880223784017,13.8390832900376));
#414422=CARTESIAN_POINT('Ctrl Pts',(-1.01943750119582,2.49033731070925,
13.8390832900376));
#414423=CARTESIAN_POINT('Ctrl Pts',(-1.01935924200018,2.48336653391456,
13.8455641171218));
#414424=CARTESIAN_POINT('Ctrl Pts',(-1.02058029101974,2.47602172910793,
13.851896480191));
#414425=CARTESIAN_POINT('Ctrl Pts',(-1.02345210770939,2.46882146520022,
13.8574481026913));
#414426=CARTESIAN_POINT('Ctrl Pts',(-1.02539321874593,2.46395468112323,
13.8612005412592));
#414427=CARTESIAN_POINT('Ctrl Pts',(-1.02815084901694,2.45904624442198,
13.8646714234115));
#414428=CARTESIAN_POINT('Ctrl Pts',(-1.03178562752637,2.45448953512919,
13.8674635290331));
#414429=CARTESIAN_POINT('Ctrl Pts',(-1.03471497755547,2.450817180276,13.8697137499649));
#414430=CARTESIAN_POINT('Ctrl Pts',(-1.03829352040138,2.44729600101259,
13.8715630732995));
#414431=CARTESIAN_POINT('Ctrl Pts',(-1.04236115646084,2.44427866777515,
13.8727429581918));
#414432=CARTESIAN_POINT('Ctrl Pts',(-1.046475674692,2.44122655779444,13.873936442031));
#414433=CARTESIAN_POINT('Ctrl Pts',(-1.05122394668006,2.43861037019094,
13.8744652622107));
#414434=CARTESIAN_POINT('Ctrl Pts',(-1.05613977589918,2.43674635911725,
13.8742206332401));
#414435=CARTESIAN_POINT('Ctrl Pts',(-1.06037114202034,2.43514188651353,
13.8740100655633));
#414436=CARTESIAN_POINT('Ctrl Pts',(-1.06483789764756,2.43404874628791,
13.8732246156103));
#414437=CARTESIAN_POINT('Ctrl Pts',(-1.06917907353433,2.43349862105172,
13.8719820486038));
#414438=CARTESIAN_POINT('Ctrl Pts',(-1.07359505796558,2.43293901587984,
13.8707180692815));
#414439=CARTESIAN_POINT('Ctrl Pts',(-1.07798037807125,2.43292015145069,
13.868960862563));
#414440=CARTESIAN_POINT('Ctrl Pts',(-1.08209313019494,2.43334037757286,
13.8669057591701));
#414441=CARTESIAN_POINT('Ctrl Pts',(-1.08842582235307,2.43398742913067,
13.8637413727084));
#414442=CARTESIAN_POINT('Ctrl Pts',(-1.09431116938593,2.43566938147429,
13.8597962563956));
#414443=CARTESIAN_POINT('Ctrl Pts',(-1.09949792947698,2.43799167731123,
13.855546950204));
#414444=CARTESIAN_POINT('Ctrl Pts',(-1.10568373526645,2.44076128122212,
13.850479165618));
#414445=CARTESIAN_POINT('Ctrl Pts',(-1.11105864429198,2.44450381285705,
13.8448473071436));
#414446=CARTESIAN_POINT('Ctrl Pts',(-1.11552693374205,2.44880223784017,
13.8390832900376));
#414447=CARTESIAN_POINT('',(-1.14132243324908,2.47361822349967,13.8057746032556));
#414448=CARTESIAN_POINT('',(-1.11552693374205,2.44880223784017,13.8390832900376));
#414449=CARTESIAN_POINT('',(-1.22234970497529,2.43459754600511,13.8057746032556));
#414450=CARTESIAN_POINT('Origin',(0.,2.5406128344257E-15,13.8057746032556));
#414451=CARTESIAN_POINT('',(-1.2190310169947,2.39895729840275,13.8390832900376));
#414452=CARTESIAN_POINT('',(-1.22234970497529,2.43459754600511,13.8057746032556));
#414453=CARTESIAN_POINT('',(-1.31141522584932,2.34972824925896,13.8390832900376));
#414454=CARTESIAN_POINT('Ctrl Pts',(-1.2190310169947,2.39895729840275,13.8390832900376));
#414455=CARTESIAN_POINT('Ctrl Pts',(-1.21838483517778,2.39201609514376,
13.8455641171218));
#414456=CARTESIAN_POINT('Ctrl Pts',(-1.21900315147987,2.38459620273847,
13.851896480191));
#414457=CARTESIAN_POINT('Ctrl Pts',(-1.22127852408393,2.37718581739407,
13.8574481026913));
#414458=CARTESIAN_POINT('Ctrl Pts',(-1.22281648815033,2.37217700856975,
13.8612005412592));
#414459=CARTESIAN_POINT('Ctrl Pts',(-1.22516485947524,2.36706013181903,
13.8646714234115));
#414460=CARTESIAN_POINT('Ctrl Pts',(-1.22841612944925,2.36222231640835,
13.8674635290331));
#414461=CARTESIAN_POINT('Ctrl Pts',(-1.23103640129476,2.35832341179085,
13.8697137499649));
#414462=CARTESIAN_POINT('Ctrl Pts',(-1.23431602803556,2.35452226449745,
13.8715630732995));
#414463=CARTESIAN_POINT('Ctrl Pts',(-1.23812418870118,2.35118342108651,
13.8727429581918));
#414464=CARTESIAN_POINT('Ctrl Pts',(-1.24197624091452,2.34780609531682,
13.873936442031));
#414465=CARTESIAN_POINT('Ctrl Pts',(-1.24649546984206,2.34481158461392,
13.8744652622107));
#414466=CARTESIAN_POINT('Ctrl Pts',(-1.25124300783784,2.34255309016562,
13.8742206332401));
#414467=CARTESIAN_POINT('Ctrl Pts',(-1.25532951502489,2.34060906069116,
13.8740100655633));
#414468=CARTESIAN_POINT('Ctrl Pts',(-1.25969230681464,2.33915547574851,
13.8732246156103));
#414469=CARTESIAN_POINT('Ctrl Pts',(-1.2639741974829,2.33825333487238,13.8719820486038));
#414470=CARTESIAN_POINT('Ctrl Pts',(-1.26832987507362,2.3373356480134,13.8707180692815));
#414471=CARTESIAN_POINT('Ctrl Pts',(-1.27269906576229,2.33695940205415,
13.868960862563));
#414472=CARTESIAN_POINT('Ctrl Pts',(-1.27683238537272,2.33704300242955,
13.8669057591701));
#414473=CARTESIAN_POINT('Ctrl Pts',(-1.283196746729,2.33717172777594,13.8637413727084));
#414474=CARTESIAN_POINT('Ctrl Pts',(-1.28919960548561,2.33836837314182,
13.8597962563956));
#414475=CARTESIAN_POINT('Ctrl Pts',(-1.29455839573018,2.34026017263199,
13.855546950204));
#414476=CARTESIAN_POINT('Ctrl Pts',(-1.30094936719167,2.34251636031628,
13.850479165618));
#414477=CARTESIAN_POINT('Ctrl Pts',(-1.30661144272303,2.34580833400213,
13.8448473071436));
#414478=CARTESIAN_POINT('Ctrl Pts',(-1.31141522584932,2.34972824925896,
13.8390832900376));
#414479=CARTESIAN_POINT('',(-1.33914762617134,2.37235908908979,13.8057746032556));
#414480=CARTESIAN_POINT('',(-1.31141522584932,2.34972824925896,13.8390832900376));
#414481=CARTESIAN_POINT('',(-1.41672473886905,2.32686377481444,13.8057746032556));
#414482=CARTESIAN_POINT('Origin',(0.,2.5406128344257E-15,13.8057746032556));
#414483=CARTESIAN_POINT('',(-1.41051208250144,2.29161262107548,13.8390832900376));
#414484=CARTESIAN_POINT('',(-1.41672473886905,2.32686377481444,13.8057746032556));
#414485=CARTESIAN_POINT('',(-1.49857626599684,2.2350172068568,13.8390832900376));
#414486=CARTESIAN_POINT('Ctrl Pts',(-1.41051208250144,2.29161262107548,
13.8390832900376));
#414487=CARTESIAN_POINT('Ctrl Pts',(-1.40930227829661,2.28474718391466,
13.8455641171218));
#414488=CARTESIAN_POINT('Ctrl Pts',(-1.40931374708826,2.27730158207046,
13.851896480191));
#414489=CARTESIAN_POINT('Ctrl Pts',(-1.41097753337746,2.26973039018123,
13.8574481026913));
#414490=CARTESIAN_POINT('Ctrl Pts',(-1.4121021155766,2.2646128894059,13.8612005412592));
#414491=CARTESIAN_POINT('Ctrl Pts',(-1.41402559993171,2.25932162457625,
13.8646714234115));
#414492=CARTESIAN_POINT('Ctrl Pts',(-1.41687172470503,2.25423489791106,
13.8674635290331));
#414493=CARTESIAN_POINT('Ctrl Pts',(-1.41916548089014,2.25013539009621,
13.8697137499649));
#414494=CARTESIAN_POINT('Ctrl Pts',(-1.42212436615097,2.24607957078092,
13.8715630732995));
#414495=CARTESIAN_POINT('Ctrl Pts',(-1.42564770874183,2.2424414366485,13.8727429581918));
#414496=CARTESIAN_POINT('Ctrl Pts',(-1.4292116601654,2.23876137063561,13.873936442031));
#414497=CARTESIAN_POINT('Ctrl Pts',(-1.43347177130953,2.23540846480797,
13.8744652622107));
#414498=CARTESIAN_POINT('Ctrl Pts',(-1.4380194239999,2.23277051689298,13.8742206332401));
#414499=CARTESIAN_POINT('Ctrl Pts',(-1.44193387722174,2.2304998677432,13.8740100655633));
#414500=CARTESIAN_POINT('Ctrl Pts',(-1.44616367151446,2.22869551145149,
13.8732246156103));
#414501=CARTESIAN_POINT('Ctrl Pts',(-1.45035778168829,2.22744735853411,
13.8719820486038));
#414502=CARTESIAN_POINT('Ctrl Pts',(-1.45462416612275,2.22617769704267,
13.8707180692815));
#414503=CARTESIAN_POINT('Ctrl Pts',(-1.45894815115126,2.22544657340809,
13.868960862563));
#414504=CARTESIAN_POINT('Ctrl Pts',(-1.46307453168836,2.22519299169003,
13.8669057591701));
#414505=CARTESIAN_POINT('Ctrl Pts',(-1.46942820846801,2.22480253417906,
13.8637413727084));
#414506=CARTESIAN_POINT('Ctrl Pts',(-1.47550863091374,2.22550590908972,
13.8597962563956));
#414507=CARTESIAN_POINT('Ctrl Pts',(-1.4810037894469,2.22695462261963,13.855546950204));
#414508=CARTESIAN_POINT('Ctrl Pts',(-1.48755739571976,2.22868237952053,
13.850479165618));
#414509=CARTESIAN_POINT('Ctrl Pts',(-1.49346895757847,2.23150188771555,
13.8448473071436));
#414510=CARTESIAN_POINT('Ctrl Pts',(-1.49857626599684,2.23501720685679,
13.8390832900376));
#414511=CARTESIAN_POINT('',(-1.52806101258523,2.25531229635372,13.8057746032556));
#414512=CARTESIAN_POINT('',(-1.49857626599684,2.2350172068568,13.8390832900376));
#414513=CARTESIAN_POINT('',(-1.60167170336877,2.20364510910788,13.8057746032556));
#414514=CARTESIAN_POINT('Origin',(0.,2.5406128344257E-15,13.8057746032556));
#414515=CARTESIAN_POINT('',(-1.59260642281724,2.16901763984442,13.8390832900376));
#414516=CARTESIAN_POINT('',(-1.60167170336877,2.20364510910788,13.8057746032556));
#414517=CARTESIAN_POINT('',(-1.67576452834183,2.10543249369488,13.8390832900376));
#414518=CARTESIAN_POINT('Ctrl Pts',(-1.59260642281724,2.16901763984442,
13.8390832900376));
#414519=CARTESIAN_POINT('Ctrl Pts',(-1.59084104727189,2.16227365713336,
13.8455641171218));
#414520=CARTESIAN_POINT('Ctrl Pts',(-1.59024559223018,2.15485189510208,
13.851896480191));
#414521=CARTESIAN_POINT('Ctrl Pts',(-1.59128671998126,2.14717028170087,
13.8574481026913));
#414522=CARTESIAN_POINT('Ctrl Pts',(-1.59199043640417,2.14197814509787,
13.8612005412592));
#414523=CARTESIAN_POINT('Ctrl Pts',(-1.59347623331844,2.13654770468375,
13.8646714234115));
#414524=CARTESIAN_POINT('Ctrl Pts',(-1.59589827240028,2.13124591809075,
13.8674635290331));
#414525=CARTESIAN_POINT('Ctrl Pts',(-1.59785024835603,2.12697308862669,
13.8697137499649));
#414526=CARTESIAN_POINT('Ctrl Pts',(-1.60046870124365,2.12268958809788,
13.8715630732995));
#414527=CARTESIAN_POINT('Ctrl Pts',(-1.60368377849611,2.11877637442639,
13.8727429581918));
#414528=CARTESIAN_POINT('Ctrl Pts',(-1.60693591162122,2.11481805840244,
13.873936442031));
#414529=CARTESIAN_POINT('Ctrl Pts',(-1.61090855464514,2.11112907048516,
13.8744652622107));
#414530=CARTESIAN_POINT('Ctrl Pts',(-1.61522605815175,2.10812922421163,
13.8742206332401));
#414531=CARTESIAN_POINT('Ctrl Pts',(-1.61894240736803,2.10554706618199,
13.8740100655633));
#414532=CARTESIAN_POINT('Ctrl Pts',(-1.62301105558057,2.10340394623464,
13.8732246156103));
#414533=CARTESIAN_POINT('Ctrl Pts',(-1.62708947414873,2.10181808752774,
13.8719820486038));
#414534=CARTESIAN_POINT('Ctrl Pts',(-1.63123817334242,2.10020490079158,
13.8707180692815));
#414535=CARTESIAN_POINT('Ctrl Pts',(-1.63548817730382,2.09912376498884,
13.868960862563));
#414536=CARTESIAN_POINT('Ctrl Pts',(-1.63958015838592,2.0985346887218,13.8669057591701));
#414537=CARTESIAN_POINT('Ctrl Pts',(-1.64588086791825,2.0976276467838,13.8637413727084));
#414538=CARTESIAN_POINT('Ctrl Pts',(-1.65199838984492,2.09783307039525,
13.8597962563956));
#414539=CARTESIAN_POINT('Ctrl Pts',(-1.65759334729327,2.09882905701538,
13.855546950204));
#414540=CARTESIAN_POINT('Ctrl Pts',(-1.66426597520903,2.10001688519578,
13.850479165618));
#414541=CARTESIAN_POINT('Ctrl Pts',(-1.67038768292626,2.10234516453813,
13.8448473071436));
#414542=CARTESIAN_POINT('Ctrl Pts',(-1.67576452834183,2.10543249369488,
13.8390832900376));
#414543=CARTESIAN_POINT('',(-1.70680540507268,2.12325677238575,13.8057746032556));
#414544=CARTESIAN_POINT('',(-1.67576452834183,2.10543249369488,13.8390832900376));
#414545=CARTESIAN_POINT('',(-1.7759598069398,2.06576154877605,13.8057746032556));
#414546=CARTESIAN_POINT('Origin',(0.,2.5406128344257E-15,13.8057746032556));
#414547=CARTESIAN_POINT('',(-1.76410223015076,2.03198820408291,13.8390832900376));
#414548=CARTESIAN_POINT('',(-1.7759598069398,2.06576154877605,13.8057746032556));
#414549=CARTESIAN_POINT('',(-1.84180085423239,1.96183647465934,13.8390832900376));
#414550=CARTESIAN_POINT('Ctrl Pts',(-1.76410223015076,2.03198820408291,
13.8390832900376));
#414551=CARTESIAN_POINT('Ctrl Pts',(-1.76179303154787,2.02541055591388,
13.8455641171218));
#414552=CARTESIAN_POINT('Ctrl Pts',(-1.76059461532786,2.01806202429734,
13.851896480191));
#414553=CARTESIAN_POINT('Ctrl Pts',(-1.76100615600743,2.01032110925397,
13.8574481026913));
#414554=CARTESIAN_POINT('Ctrl Pts',(-1.76128432353739,2.00508888963573,
13.8612005412592));
#414555=CARTESIAN_POINT('Ctrl Pts',(-1.7623225452775,1.99955541232213,13.8646714234115));
#414556=CARTESIAN_POINT('Ctrl Pts',(-1.76430438039739,1.99407384831637,
13.8674635290331));
#414557=CARTESIAN_POINT('Ctrl Pts',(-1.76590158604583,1.98965613217822,
13.8697137499649));
#414558=CARTESIAN_POINT('Ctrl Pts',(-1.76816218118831,1.98517345642518,
13.8715630732995));
#414559=CARTESIAN_POINT('Ctrl Pts',(-1.77104759729371,1.98101120500597,
13.8727429581918));
#414560=CARTESIAN_POINT('Ctrl Pts',(-1.77396626971095,1.97680098091103,
13.873936442031));
#414561=CARTESIAN_POINT('Ctrl Pts',(-1.77762500733078,1.97280046051005,
13.8744652622107));
#414562=CARTESIAN_POINT('Ctrl Pts',(-1.78168362938013,1.96945867935999,
13.8742206332401));
#414563=CARTESIAN_POINT('Ctrl Pts',(-1.78517714289997,1.96658219628615,
13.8740100655633));
#414564=CARTESIAN_POINT('Ctrl Pts',(-1.78905756884977,1.96411457479282,
13.8732246156103));
#414565=CARTESIAN_POINT('Ctrl Pts',(-1.79299315460958,1.96220156392444,
13.8719820486038));
#414566=CARTESIAN_POINT('Ctrl Pts',(-1.79699655965385,1.96025558743515,
13.8707180692815));
#414567=CARTESIAN_POINT('Ctrl Pts',(-1.80114429947297,1.95883163424464,
13.868960862563));
#414568=CARTESIAN_POINT('Ctrl Pts',(-1.80517464964111,1.95791098363399,
13.8669057591701));
#414569=CARTESIAN_POINT('Ctrl Pts',(-1.81138046174373,1.95649339348339,
13.8637413727084));
#414570=CARTESIAN_POINT('Ctrl Pts',(-1.81749437205224,1.95619949873539,
13.8597962563956));
#414571=CARTESIAN_POINT('Ctrl Pts',(-1.82315189489706,1.95673613031912,
13.855546950204));
#414572=CARTESIAN_POINT('Ctrl Pts',(-1.82989913921785,1.95737612497844,
13.850479165618));
#414573=CARTESIAN_POINT('Ctrl Pts',(-1.83619025383874,1.95919768115324,
13.8448473071436));
#414574=CARTESIAN_POINT('Ctrl Pts',(-1.84180085423239,1.96183647465934,
13.8390832900376));
#414575=CARTESIAN_POINT('',(-1.87419128919245,1.97707132491026,13.8057746032556));
#414576=CARTESIAN_POINT('',(-1.84180085423239,1.96183647465934,13.8390832900376));
#414577=CARTESIAN_POINT('',(-1.93842919100838,1.91413068616379,13.8057746032556));
#414578=CARTESIAN_POINT('Origin',(0.,2.5406128344257E-15,13.8057746032556));
#414579=CARTESIAN_POINT('',(-1.92385822819901,1.88143622207769,13.8390832900376));
#414580=CARTESIAN_POINT('',(-1.93842919100838,1.91413068616379,13.8057746032556));
#414581=CARTESIAN_POINT('',(-1.99558029931379,1.80518475756518,13.8390832900376));
#414582=CARTESIAN_POINT('Ctrl Pts',(-1.923858228199,1.88143622207769,13.8390832900376));
#414583=CARTESIAN_POINT('Ctrl Pts',(-1.92102057387428,1.87506868161401,
13.8455641171218));
#414584=CARTESIAN_POINT('Ctrl Pts',(-1.91922717173821,1.8678422836777,13.851896480191));
#414585=CARTESIAN_POINT('Ctrl Pts',(-1.91900638661092,1.86009358150461,
13.8574481026913));
#414586=CARTESIAN_POINT('Ctrl Pts',(-1.91885715408894,1.85485609842945,
13.8612005412592));
#414587=CARTESIAN_POINT('Ctrl Pts',(-1.91944089146049,1.84925640859494,
13.8646714234115));
#414588=CARTESIAN_POINT('Ctrl Pts',(-1.92096933383269,1.84363154608048,
13.8674635290331));
#414589=CARTESIAN_POINT('Ctrl Pts',(-1.92220114003376,1.83909834244026,
13.8697137499649));
#414590=CARTESIAN_POINT('Ctrl Pts',(-1.92408883354338,1.83444632293054,
13.8715630732995));
#414591=CARTESIAN_POINT('Ctrl Pts',(-1.9266253865336,1.83006273286008,13.8727429581918));
#414592=CARTESIAN_POINT('Ctrl Pts',(-1.9291911749596,1.82562861904085,13.873936442031));
#414593=CARTESIAN_POINT('Ctrl Pts',(-1.93251165888012,1.82134318895941,
13.8744652622107));
#414594=CARTESIAN_POINT('Ctrl Pts',(-1.9362843900121,1.81768171193502,13.8742206332401));
#414595=CARTESIAN_POINT('Ctrl Pts',(-1.93953181907942,1.81453004633725,
13.8740100655633));
#414596=CARTESIAN_POINT('Ctrl Pts',(-1.94319819917199,1.81175434491185,
13.8732246156103));
#414597=CARTESIAN_POINT('Ctrl Pts',(-1.94696476144955,1.80952691265371,
13.8719820486038));
#414598=CARTESIAN_POINT('Ctrl Pts',(-1.95079623034435,1.80726109656374,
13.8707180692815));
#414599=CARTESIAN_POINT('Ctrl Pts',(-1.95481410349702,1.805503802159,13.868960862563));
#414600=CARTESIAN_POINT('Ctrl Pts',(-1.95875600143578,1.80425770398267,
13.8669057591701));
#414601=CARTESIAN_POINT('Ctrl Pts',(-1.96482561745304,1.80233899944804,
13.8637413727084));
#414602=CARTESIAN_POINT('Ctrl Pts',(-1.97089522907902,1.80154774216165,
13.8597962563956));
#414603=CARTESIAN_POINT('Ctrl Pts',(-1.9765776674392,1.80162144751432,13.855546950204));
#414604=CARTESIAN_POINT('Ctrl Pts',(-1.98335462636727,1.80170934959371,
13.850479165618));
#414605=CARTESIAN_POINT('Ctrl Pts',(-1.98977328156199,1.80301206044513,
13.8448473071436));
#414606=CARTESIAN_POINT('Ctrl Pts',(-1.99558029931379,1.80518475756518,
13.8390832900376));
#414607=CARTESIAN_POINT('',(-2.02910473950244,1.8177287939613,13.8057746032556));
#414608=CARTESIAN_POINT('',(-1.99558029931379,1.80518475756518,13.8390832900376));
#414609=CARTESIAN_POINT('',(-2.08799864862912,1.74976159964444,13.8057746032556));
#414610=CARTESIAN_POINT('Origin',(0.,2.5406128344257E-15,13.8057746032556));
#414611=CARTESIAN_POINT('',(-2.07081126715285,1.71836359242966,13.8390832900376));
#414612=CARTESIAN_POINT('',(-2.08799864862912,1.74976159964444,13.8057746032556));
#414613=CARTESIAN_POINT('',(-2.13607948675083,1.63651983374394,13.8390832900376));
#414614=CARTESIAN_POINT('Ctrl Pts',(-2.07081126715285,1.71836359242966,
13.8390832900376));
#414615=CARTESIAN_POINT('Ctrl Pts',(-2.06746404122766,1.71224853460256,
13.8455641171218));
#414616=CARTESIAN_POINT('Ctrl Pts',(-2.06508758797082,1.70519236083247,
13.851896480191));
#414617=CARTESIAN_POINT('Ctrl Pts',(-2.06423594632529,1.69748743786418,
13.8574481026913));
#414618=CARTESIAN_POINT('Ctrl Pts',(-2.06366030686916,1.69227954591784,
13.8612005412592));
#414619=CARTESIAN_POINT('Ctrl Pts',(-2.06378567519628,1.68665090857437,
13.8646714234115));
#414620=CARTESIAN_POINT('Ctrl Pts',(-2.06485055328896,1.68092018008321,
13.8674635290331));
#414621=CARTESIAN_POINT('Ctrl Pts',(-2.06570876257563,1.67630165666322,
13.8697137499649));
#414622=CARTESIAN_POINT('Ctrl Pts',(-2.06721099216353,1.67151125181913,
13.8715630732995));
#414623=CARTESIAN_POINT('Ctrl Pts',(-2.06938180169692,1.6669354951661,13.8727429581918));
#414624=CARTESIAN_POINT('Ctrl Pts',(-2.07157763123302,1.66230699991848,
13.873936442031));
#414625=CARTESIAN_POINT('Ctrl Pts',(-2.07453776418159,1.65776517898672,
13.8744652622107));
#414626=CARTESIAN_POINT('Ctrl Pts',(-2.07799949749298,1.65380837261349,
13.8742206332401));
#414627=CARTESIAN_POINT('Ctrl Pts',(-2.08097923100311,1.65040249830636,
13.8740100655633));
#414628=CARTESIAN_POINT('Ctrl Pts',(-2.08440716608385,1.64733718878392,
13.8732246156103));
#414629=CARTESIAN_POINT('Ctrl Pts',(-2.08797963902864,1.64481015833018,
13.8719820486038));
#414630=CARTESIAN_POINT('Ctrl Pts',(-2.09161367398063,1.64223958127179,
13.8707180692815));
#414631=CARTESIAN_POINT('Ctrl Pts',(-2.09547494218393,1.64016064015716,
13.868960862563));
#414632=CARTESIAN_POINT('Ctrl Pts',(-2.0993021552129,1.63859738699291,13.8669057591701));
#414633=CARTESIAN_POINT('Ctrl Pts',(-2.10519518285161,1.63619033673636,
13.8637413727084));
#414634=CARTESIAN_POINT('Ctrl Pts',(-2.11118010353109,1.63490698259828,
13.8597962563956));
#414635=CARTESIAN_POINT('Ctrl Pts',(-2.11684964171689,1.63451727122293,
13.855546950204));
#414636=CARTESIAN_POINT('Ctrl Pts',(-2.1236112157087,1.63405249574854,13.850479165618));
#414637=CARTESIAN_POINT('Ctrl Pts',(-2.13011469638593,1.63482769195082,
13.8448473071436));
#414638=CARTESIAN_POINT('Ctrl Pts',(-2.13607948675083,1.63651983374394,
13.8390832900376));
#414639=CARTESIAN_POINT('',(-2.17051483254976,1.64628957779267,13.8057746032556));
#414640=CARTESIAN_POINT('',(-2.13607948675083,1.63651983374394,13.8390832900376));
#414641=CARTESIAN_POINT('',(-2.22367281973875,1.5737481383698,13.8057746032556));
#414642=CARTESIAN_POINT('Origin',(0.,2.5406128344257E-15,13.8057746032556));
#414643=CARTESIAN_POINT('',(-2.20398339878361,1.54385553658406,13.8390832900376));
#414644=CARTESIAN_POINT('',(-2.22367281973875,1.5737481383698,13.8057746032556));
#414645=CARTESIAN_POINT('',(-2.26236341763185,1.4569641404359,13.8390832900376));
#414646=CARTESIAN_POINT('Ctrl Pts',(-2.2039833987836,1.54385553658406,13.8390832900376));
#414647=CARTESIAN_POINT('Ctrl Pts',(-2.20014887649421,1.53803365609445,
13.8455641171218));
#414648=CARTESIAN_POINT('Ctrl Pts',(-2.19720518702096,1.53119466416283,
13.851896480191));
#414649=CARTESIAN_POINT('Ctrl Pts',(-2.19572835639182,1.52358479539047,
13.8574481026913));
#414650=CARTESIAN_POINT('Ctrl Pts',(-2.19473014078716,1.51844115223462,
13.8612005412592));
#414651=CARTESIAN_POINT('Ctrl Pts',(-2.1943963057643,1.51282102503506,13.8646714234115));
#414652=CARTESIAN_POINT('Ctrl Pts',(-2.19499053298945,1.5070225676198,13.8674635290331));
#414653=CARTESIAN_POINT('Ctrl Pts',(-2.19546943412051,1.5023494599314,13.8697137499649));
#414654=CARTESIAN_POINT('Ctrl Pts',(-2.19657620269664,1.49745254910681,
13.8715630732995));
#414655=CARTESIAN_POINT('Ctrl Pts',(-2.19836682239391,1.49271507677678,
13.8727429581918));
#414656=CARTESIAN_POINT('Ctrl Pts',(-2.20017808015684,1.487923001973,13.873936442031));
#414657=CARTESIAN_POINT('Ctrl Pts',(-2.20275816293707,1.48315501525987,
13.8744652622107));
#414658=CARTESIAN_POINT('Ctrl Pts',(-2.20588586116382,1.4789292114314,13.8742206332401));
#414659=CARTESIAN_POINT('Ctrl Pts',(-2.20857806948188,1.47529179394649,
13.8740100655633));
#414660=CARTESIAN_POINT('Ctrl Pts',(-2.21174474720841,1.47195727545613,
13.8732246156103));
#414661=CARTESIAN_POINT('Ctrl Pts',(-2.2150993566024,1.46914746377755,13.8719820486038));
#414662=CARTESIAN_POINT('Ctrl Pts',(-2.21851177370854,1.46628923251693,
13.8707180692815));
#414663=CARTESIAN_POINT('Ctrl Pts',(-2.22219074085963,1.46390247970253,
13.868960862563));
#414664=CARTESIAN_POINT('Ctrl Pts',(-2.22587779950755,1.46203247474225,
13.8669057591701));
#414665=CARTESIAN_POINT('Ctrl Pts',(-2.23155502164105,1.45915309728611,
13.8637413727084));
#414666=CARTESIAN_POINT('Ctrl Pts',(-2.23741542271437,1.45738618680638,
13.8597962563956));
#414667=CARTESIAN_POINT('Ctrl Pts',(-2.24303433088457,1.45653565216792,
13.855546950204));
#414668=CARTESIAN_POINT('Ctrl Pts',(-2.24973552278078,1.45552129214386,
13.850479165618));
#414669=CARTESIAN_POINT('Ctrl Pts',(-2.25628054934961,1.45576381489416,
13.8448473071436));
#414670=CARTESIAN_POINT('Ctrl Pts',(-2.26236341763184,1.4569641404359,13.8390832900376));
#414671=CARTESIAN_POINT('',(-2.2974805074962,1.46389457610249,13.8057746032556));
#414672=CARTESIAN_POINT('',(-2.26236341763185,1.4569641404359,13.8390832900376));
#414673=CARTESIAN_POINT('',(-2.34454881511321,1.38726164288447,13.8057746032556));
#414674=CARTESIAN_POINT('Origin',(0.,2.5406128344257E-15,13.8057746032556));
#414675=CARTESIAN_POINT('',(-2.32248838452712,1.35907337686072,13.8390832900376));
#414676=CARTESIAN_POINT('',(-2.34454881511321,1.38726164288447,13.8057746032556));
#414677=CARTESIAN_POINT('',(-2.37359169323221,1.26771259115543,13.8390832900376));
#414678=CARTESIAN_POINT('Ctrl Pts',(-2.32248838452712,1.35907337686072,
13.8390832900376));
#414679=CARTESIAN_POINT('Ctrl Pts',(-2.31819208398671,1.35358341736272,
13.8455641171218));
#414680=CARTESIAN_POINT('Ctrl Pts',(-2.31470074806482,1.34700711963253,
13.851896480191));
#414681=CARTESIAN_POINT('Ctrl Pts',(-2.31260855651624,1.33954294747724,
13.8574481026913));
#414682=CARTESIAN_POINT('Ctrl Pts',(-2.31119440772321,1.33449778320843,
13.8612005412592));
#414683=CARTESIAN_POINT('Ctrl Pts',(-2.31040359096736,1.32892356717203,
13.8646714234115));
#414684=CARTESIAN_POINT('Ctrl Pts',(-2.31052321284085,1.32309596861009,
13.8674635290331));
#414685=CARTESIAN_POINT('Ctrl Pts',(-2.31061961880828,1.31839937541394,
13.8697137499649));
#414686=CARTESIAN_POINT('Ctrl Pts',(-2.31132356101037,1.31342854674246,
13.8715630732995));
#414687=CARTESIAN_POINT('Ctrl Pts',(-2.31272207459287,1.30856088583217,
13.8727429581918));
#414688=CARTESIAN_POINT('Ctrl Pts',(-2.31413670696105,1.3036371219394,13.873936442031));
#414689=CARTESIAN_POINT('Ctrl Pts',(-2.31631956954772,1.29867469960982,
13.8744652622107));
#414690=CARTESIAN_POINT('Ctrl Pts',(-2.31909241837417,1.29420802035337,
13.8742206332401));
#414691=CARTESIAN_POINT('Ctrl Pts',(-2.32147918529799,1.29036326610391,
13.8740100655633));
#414692=CARTESIAN_POINT('Ctrl Pts',(-2.32436353195249,1.28678172931604,
13.8732246156103));
#414693=CARTESIAN_POINT('Ctrl Pts',(-2.32747795342363,1.28370783524574,
13.8719820486038));
#414694=CARTESIAN_POINT('Ctrl Pts',(-2.33064604361109,1.28058097084037,
13.8707180692815));
#414695=CARTESIAN_POINT('Ctrl Pts',(-2.33411822679057,1.27790228977239,
13.868960862563));
#414696=CARTESIAN_POINT('Ctrl Pts',(-2.33764059429046,1.27573797759056,
13.8669057591701));
#414697=CARTESIAN_POINT('Ctrl Pts',(-2.34306422994214,1.27240543471673,
13.8637413727084));
#414698=CARTESIAN_POINT('Ctrl Pts',(-2.34876111140704,1.27016672639309,
13.8597962563956));
#414699=CARTESIAN_POINT('Ctrl Pts',(-2.35429199665482,1.2688610286592,13.855546950204));
#414700=CARTESIAN_POINT('Ctrl Pts',(-2.36088821112899,1.26730383448407,
13.850479165618));
#414701=CARTESIAN_POINT('Ctrl Pts',(-2.36743122751746,1.2670120698335,13.8448473071436));
#414702=CARTESIAN_POINT('Ctrl Pts',(-2.37359169323221,1.26771259115543,
13.8390832900376));
#414703=CARTESIAN_POINT('',(-2.40915682872285,1.27175759753395,13.8057746032556));
#414704=CARTESIAN_POINT('',(-2.37359169323221,1.26771259115543,13.8390832900376));
#414705=CARTESIAN_POINT('',(-2.44982222494642,1.19154315004781,13.8057746032556));
#414706=CARTESIAN_POINT('Origin',(0.,2.5406128344257E-15,13.8057746032556));
#414707=CARTESIAN_POINT('',(-2.42553759325522,1.16524680804569,13.8390832900376));
#414708=CARTESIAN_POINT('',(-2.44982222494642,1.19154315004781,13.8057746032556));
#414709=CARTESIAN_POINT('',(-2.46902410772919,1.07002462373867,13.8390832900376));
#414710=CARTESIAN_POINT('Ctrl Pts',(-2.42553759325522,1.16524680804569,
13.8390832900376));
#414711=CARTESIAN_POINT('Ctrl Pts',(-2.42080810563505,1.16012530431399,
13.8455641171218));
#414712=CARTESIAN_POINT('Ctrl Pts',(-2.41679235752905,1.1538554649616,13.851896480191));
#414713=CARTESIAN_POINT('Ctrl Pts',(-2.4140987282506,1.14658666225758,13.8574481026913));
#414714=CARTESIAN_POINT('Ctrl Pts',(-2.41227805719609,1.14167355161162,
13.8612005412592));
#414715=CARTESIAN_POINT('Ctrl Pts',(-2.4110355214623,1.13618234222643,13.8646714234115));
#414716=CARTESIAN_POINT('Ctrl Pts',(-2.41067974192029,1.13036438422476,
13.8674635290331));
#414717=CARTESIAN_POINT('Ctrl Pts',(-2.41039301115828,1.12567556057369,
13.8697137499649));
#414718=CARTESIAN_POINT('Ctrl Pts',(-2.41068944236712,1.1206638941,13.8715630732995));
#414719=CARTESIAN_POINT('Ctrl Pts',(-2.41168654295769,1.1156984380897,13.8727429581918));
#414720=CARTESIAN_POINT('Ctrl Pts',(-2.41269513578612,1.11067575194429,
13.873936442031));
#414721=CARTESIAN_POINT('Ctrl Pts',(-2.41446625158886,1.10555191810012,
13.8744652622107));
#414722=CARTESIAN_POINT('Ctrl Pts',(-2.41686579816356,1.10087408842919,
13.8742206332401));
#414723=CARTESIAN_POINT('Ctrl Pts',(-2.41893124015304,1.09684758362037,
13.8740100655633));
#414724=CARTESIAN_POINT('Ctrl Pts',(-2.42151406088441,1.09304286307139,
13.8732246156103));
#414725=CARTESIAN_POINT('Ctrl Pts',(-2.42436756847166,1.08972534286726,
13.8719820486038));
#414726=CARTESIAN_POINT('Ctrl Pts',(-2.42727024862294,1.08635065408386,
13.8707180692815));
#414727=CARTESIAN_POINT('Ctrl Pts',(-2.43051254102462,1.08339787094285,
13.868960862563));
#414728=CARTESIAN_POINT('Ctrl Pts',(-2.43384677660192,1.08095365467996,
13.8669057591701));
#414729=CARTESIAN_POINT('Ctrl Pts',(-2.43898073237136,1.07719012391144,
13.8637413727084));
#414730=CARTESIAN_POINT('Ctrl Pts',(-2.44447618242161,1.0744945159784,13.8597962563956));
#414731=CARTESIAN_POINT('Ctrl Pts',(-2.44988223761817,1.07274234435208,
13.855546950204));
#414732=CARTESIAN_POINT('Ctrl Pts',(-2.45632957795126,1.0706526788962,13.850479165618));
#414733=CARTESIAN_POINT('Ctrl Pts',(-2.46282704146483,1.06982856849037,
13.8448473071436));
#414734=CARTESIAN_POINT('Ctrl Pts',(-2.46902410772918,1.07002462373867,
13.8390832900376));
#414735=CARTESIAN_POINT('',(-2.50480060873725,1.07115728197906,13.8057746032556));
#414736=CARTESIAN_POINT('',(-2.46902410772919,1.07002462373867,13.8390832900376));
#414737=CARTESIAN_POINT('',(-2.53879247206483,0.98789513413836,13.8057746032556));
#414738=CARTESIAN_POINT('Origin',(0.,2.5406128344257E-15,13.8057746032556));
#414739=CARTESIAN_POINT('',(-2.51244524948573,0.963665713975314,13.8390832900376));
#414740=CARTESIAN_POINT('',(-2.53879247206483,0.98789513413836,13.8057746032556));
#414741=CARTESIAN_POINT('',(-2.54802557414952,0.865215818992561,13.8390832900376));
#414742=CARTESIAN_POINT('Ctrl Pts',(-2.51244524948573,0.963665713975314,
13.8390832900376));
#414743=CARTESIAN_POINT('Ctrl Pts',(-2.50731404874562,0.958946748772246,
13.8455641171218));
#414744=CARTESIAN_POINT('Ctrl Pts',(-2.50280061259659,0.953025092544104,
13.851896480191));
#414745=CARTESIAN_POINT('Ctrl Pts',(-2.49952347124671,0.946000031974073,
13.8574481026913));
#414746=CARTESIAN_POINT('Ctrl Pts',(-2.4973083941962,0.941251670891716,
13.8612005412592));
#414747=CARTESIAN_POINT('Ctrl Pts',(-2.49562240835476,0.935880011250207,
13.8646714234115));
#414748=CARTESIAN_POINT('Ctrl Pts',(-2.49479359505141,0.930110411359408,
13.8674635290331));
#414749=CARTESIAN_POINT('Ctrl Pts',(-2.49412563570588,0.925460560601219,
13.8697137499649));
#414750=CARTESIAN_POINT('Ctrl Pts',(-2.49401258322068,0.920441408138835,
13.8715630732995));
#414751=CARTESIAN_POINT('Ctrl Pts',(-2.49460163527941,0.91541120131902,
13.8727429581918));
#414752=CARTESIAN_POINT('Ctrl Pts',(-2.4951974765492,0.910323018068578,
13.873936442031));
#414753=CARTESIAN_POINT('Ctrl Pts',(-2.49654505908457,0.905071870978679,
13.8744652622107));
#414754=CARTESIAN_POINT('Ctrl Pts',(-2.49855533482095,0.900214021077945,
13.8742206332401));
#414755=CARTESIAN_POINT('Ctrl Pts',(-2.50028570670044,0.896032561434943,
13.8740100655633));
#414756=CARTESIAN_POINT('Ctrl Pts',(-2.50254981326285,0.892029976912383,
13.8732246156103));
#414757=CARTESIAN_POINT('Ctrl Pts',(-2.505123417344,0.888490908124015,13.8719820486038));
#414758=CARTESIAN_POINT('Ctrl Pts',(-2.50774137060161,0.884890852959653,
13.8707180692815));
#414759=CARTESIAN_POINT('Ctrl Pts',(-2.5107321953045,0.881683618030249,
13.868960862563));
#414760=CARTESIAN_POINT('Ctrl Pts',(-2.51385611017155,0.878975763542255,
13.8669057591701));
#414761=CARTESIAN_POINT('Ctrl Pts',(-2.51866622043013,0.874806290555372,
13.8637413727084));
#414762=CARTESIAN_POINT('Ctrl Pts',(-2.52392366775234,0.871671721838992,
13.8597962563956));
#414763=CARTESIAN_POINT('Ctrl Pts',(-2.52916891649229,0.869484736733329,
13.855546950204));
#414764=CARTESIAN_POINT('Ctrl Pts',(-2.53542447669813,0.866876506375528,
13.850479165618));
#414765=CARTESIAN_POINT('Ctrl Pts',(-2.54183314778912,0.865525534533235,
13.8448473071436));
#414766=CARTESIAN_POINT('Ctrl Pts',(-2.54802557414952,0.865215818992561,
13.8390832900376));
#414767=CARTESIAN_POINT('',(-2.58377535396352,0.863428591441109,13.8057746032556));
#414768=CARTESIAN_POINT('',(-2.54802557414952,0.865215818992561,13.8390832900376));
#414769=CARTESIAN_POINT('',(-2.61086747415291,0.777672839102445,13.8057746032556));
#414770=CARTESIAN_POINT('Origin',(0.,2.5406128344257E-15,13.8057746032556));
#414771=CARTESIAN_POINT('',(-2.58263299710521,0.755671583572082,13.8390832900376));
#414772=CARTESIAN_POINT('',(-2.61086747415291,0.777672839102445,13.8057746032556));
#414773=CARTESIAN_POINT('',(-2.61007035076852,0.654649145721622,13.8390832900376));
#414774=CARTESIAN_POINT('Ctrl Pts',(-2.58263299710521,0.755671583572082,
13.8390832900376));
#414775=CARTESIAN_POINT('Ctrl Pts',(-2.57713423053948,0.751386560832503,
13.8455641171218));
#414776=CARTESIAN_POINT('Ctrl Pts',(-2.57215314252033,0.7458524953738,13.851896480191));
#414777=CARTESIAN_POINT('Ctrl Pts',(-2.56831429793401,0.739117927556801,
13.8574481026913));
#414778=CARTESIAN_POINT('Ctrl Pts',(-2.56571955585981,0.734565915597623,
13.8612005412592));
#414779=CARTESIAN_POINT('Ctrl Pts',(-2.56360133986834,0.729349553208446,
13.8646714234115));
#414780=CARTESIAN_POINT('Ctrl Pts',(-2.56230500841943,0.723666707163876,
13.8674635290331));
#414781=CARTESIAN_POINT('Ctrl Pts',(-2.56126026564962,0.719086773288191,
13.8697137499649));
#414782=CARTESIAN_POINT('Ctrl Pts',(-2.56073848181602,0.714093536468648,
13.8715630732995));
#414783=CARTESIAN_POINT('Ctrl Pts',(-2.56091556529863,0.709032054035785,
13.8727429581918));
#414784=CARTESIAN_POINT('Ctrl Pts',(-2.56109468978446,0.703912234700355,
13.873936442031));
#414785=CARTESIAN_POINT('Ctrl Pts',(-2.562009771113,0.698568719882228,13.8744652622107));
#414786=CARTESIAN_POINT('Ctrl Pts',(-2.56361739795772,0.693563177941289,
13.8742206332401));
#414787=CARTESIAN_POINT('Ctrl Pts',(-2.56500118438785,0.689254590388136,
13.8740100655633));
#414788=CARTESIAN_POINT('Ctrl Pts',(-2.56693150952567,0.685080778431609,
13.8732246156103));
#414789=CARTESIAN_POINT('Ctrl Pts',(-2.5692080831902,0.681343712977893,
13.8719820486038));
#414790=CARTESIAN_POINT('Ctrl Pts',(-2.57152388750712,0.677542249205719,
13.8707180692815));
#414791=CARTESIAN_POINT('Ctrl Pts',(-2.57424334106628,0.674101906107217,
13.868960862563));
#414792=CARTESIAN_POINT('Ctrl Pts',(-2.57713614608504,0.671148433718975,
13.8669057591701));
#414793=CARTESIAN_POINT('Ctrl Pts',(-2.58159040034262,0.666600765668538,
13.8637413727084));
#414794=CARTESIAN_POINT('Ctrl Pts',(-2.58657485749227,0.66304809620646,
13.8597962563956));
#414795=CARTESIAN_POINT('Ctrl Pts',(-2.59162439351065,0.660440851646503,
13.855546950204));
#414796=CARTESIAN_POINT('Ctrl Pts',(-2.59764654386817,0.657331413729489,
13.850479165618));
#414797=CARTESIAN_POINT('Ctrl Pts',(-2.60392377388782,0.655462570945439,
13.8448473071436));
#414798=CARTESIAN_POINT('Ctrl Pts',(-2.61007035076852,0.654649145721622,
13.8390832900376));
#414799=CARTESIAN_POINT('',(-2.64555550050208,0.649953926082808,13.8057746032556));
#414800=CARTESIAN_POINT('',(-2.61007035076852,0.654649145721622,13.8390832900376));
#414801=CARTESIAN_POINT('',(-2.66556758396333,0.562275259629291,13.8057746032556));
#414802=CARTESIAN_POINT('Origin',(0.,2.5406128344257E-15,13.8057746032556));
#414803=CARTESIAN_POINT('',(-2.6356337482334,0.542648583457214,13.8390832900376));
#414804=CARTESIAN_POINT('',(-2.66556758396333,0.562275259629291,13.8057746032556));
#414805=CARTESIAN_POINT('',(-2.65474553983446,0.439725890395412,13.8390832900376));
#414806=CARTESIAN_POINT('Ctrl Pts',(-2.6356337482334,0.542648583457214,
13.8390832900376));
#414807=CARTESIAN_POINT('Ctrl Pts',(-2.62980400922631,0.538826019300476,
13.8455641171218));
#414808=CARTESIAN_POINT('Ctrl Pts',(-2.624388417656,0.533716372903784,13.851896480191));
#414809=CARTESIAN_POINT('Ctrl Pts',(-2.6200134167106,0.527317115277512,
13.8574481026913));
#414810=CARTESIAN_POINT('Ctrl Pts',(-2.6170562771931,0.522991745330072,
13.8612005412592));
#414811=CARTESIAN_POINT('Ctrl Pts',(-2.61451992742954,0.517965394224288,
13.8646714234115));
#414812=CARTESIAN_POINT('Ctrl Pts',(-2.61276470470699,0.512407120428769,
13.8674635290331));
#414813=CARTESIAN_POINT('Ctrl Pts',(-2.61135013110366,0.507927582139896,
13.8697137499649));
#414814=CARTESIAN_POINT('Ctrl Pts',(-2.61042308830698,0.502993490130399,
13.8715630732995));
#414815=CARTESIAN_POINT('Ctrl Pts',(-2.61018702475212,0.497934415414992,
13.8727429581918));
#414816=CARTESIAN_POINT('Ctrl Pts',(-2.60994824041008,0.49281703154754,
13.873936442031));
#414817=CARTESIAN_POINT('Ctrl Pts',(-2.61042473081654,0.487416709210687,
13.8744652622107));
#414818=CARTESIAN_POINT('Ctrl Pts',(-2.61161901027819,0.482296786285305,
13.8742206332401));
#414819=CARTESIAN_POINT('Ctrl Pts',(-2.61264700238856,0.477889743761299,
13.8740100655633));
#414820=CARTESIAN_POINT('Ctrl Pts',(-2.6142307001065,0.473572480400745,
13.8732246156103));
#414821=CARTESIAN_POINT('Ctrl Pts',(-2.61619509313225,0.469662287835703,
13.8719820486038));
#414822=CARTESIAN_POINT('Ctrl Pts',(-2.61819333721286,0.465684713569924,
13.8707180692815));
#414823=CARTESIAN_POINT('Ctrl Pts',(-2.62062332211352,0.462034157218028,
13.868960862563));
#414824=CARTESIAN_POINT('Ctrl Pts',(-2.62326576614388,0.458854721800992,
13.8669057591701));
#414825=CARTESIAN_POINT('Ctrl Pts',(-2.62733452207326,0.453959122667565,
13.8637413727084));
#414826=CARTESIAN_POINT('Ctrl Pts',(-2.6320128183104,0.450011994888908,
13.8597962563956));
#414827=CARTESIAN_POINT('Ctrl Pts',(-2.63683303777813,0.447001841657038,
13.855546950204));
#414828=CARTESIAN_POINT('Ctrl Pts',(-2.64258170187027,0.443411888977129,
13.850479165618));
#414829=CARTESIAN_POINT('Ctrl Pts',(-2.64868571688848,0.44103761209171,
13.8448473071436));
#414830=CARTESIAN_POINT('Ctrl Pts',(-2.65474553983446,0.43972589039541,
13.8390832900376));
#414831=CARTESIAN_POINT('',(-2.68972991167074,0.432153924581275,13.8057746032556));
#414832=CARTESIAN_POINT('',(-2.65474553983446,0.439725890395412,13.8390832900376));
#414833=CARTESIAN_POINT('',(-2.70252878129016,0.34313583107219,13.8057746032556));
#414834=CARTESIAN_POINT('Origin',(0.,2.5406128344257E-15,13.8057746032556));
#414835=CARTESIAN_POINT('',(-2.67109479161606,0.326014346550151,13.8390832900376));
#414836=CARTESIAN_POINT('',(-2.70252878129016,0.34313583107219,13.8057746032556));
#414837=CARTESIAN_POINT('',(-2.68175383533497,0.221876331818285,13.8390832900376));
#414838=CARTESIAN_POINT('Ctrl Pts',(-2.67109479161606,0.326014346550149,
13.8390832900376));
#414839=CARTESIAN_POINT('Ctrl Pts',(-2.66497287611887,0.322679679510038,
13.8455641171218));
#414840=CARTESIAN_POINT('Ctrl Pts',(-2.65915882086578,0.318028456029097,
13.851896480191));
#414841=CARTESIAN_POINT('Ctrl Pts',(-2.65427677847076,0.312007094597252,
13.8574481026913));
#414842=CARTESIAN_POINT('Ctrl Pts',(-2.65097692078557,0.307937151284914,
13.8612005412592));
#414843=CARTESIAN_POINT('Ctrl Pts',(-2.64803931623913,0.30313426099984,
13.8646714234115));
#414844=CARTESIAN_POINT('Ctrl Pts',(-2.64583688296055,0.297737548848432,
13.8674635290331));
#414845=CARTESIAN_POINT('Ctrl Pts',(-2.64406189227765,0.29338821673461,
13.8697137499649));
#414846=CARTESIAN_POINT('Ctrl Pts',(-2.64273575983475,0.288546105103419,
13.8715630732995));
#414847=CARTESIAN_POINT('Ctrl Pts',(-2.64208812020644,0.28352310541301,
13.8727429581918));
#414848=CARTESIAN_POINT('Ctrl Pts',(-2.64143301610692,0.278442212358865,
13.873936442031));
#414849=CARTESIAN_POINT('Ctrl Pts',(-2.64146774462626,0.273021020757444,
13.8744652622107));
#414850=CARTESIAN_POINT('Ctrl Pts',(-2.64224072897206,0.267820789089958,
13.8742206332401));
#414851=CARTESIAN_POINT('Ctrl Pts',(-2.64290608564479,0.263344619735988,
13.8740100655633));
#414852=CARTESIAN_POINT('Ctrl Pts',(-2.64413261669582,0.258912635646773,
13.8732246156103));
#414853=CARTESIAN_POINT('Ctrl Pts',(-2.64577175637132,0.254855337656788,
13.8719820486038));
#414854=CARTESIAN_POINT('Ctrl Pts',(-2.64743914223093,0.250728122997891,
13.8707180692815));
#414855=CARTESIAN_POINT('Ctrl Pts',(-2.64956348732451,0.246891647242822,
13.868960862563));
#414856=CARTESIAN_POINT('Ctrl Pts',(-2.65193798533742,0.243507407415124,
13.8669057591701));
#414857=CARTESIAN_POINT('Ctrl Pts',(-2.65559416603919,0.238296456603223,
13.8637413727084));
#414858=CARTESIAN_POINT('Ctrl Pts',(-2.65993516807423,0.233981137992124,
13.8597962563956));
#414859=CARTESIAN_POINT('Ctrl Pts',(-2.66449399322602,0.230588108161459,
13.855546950204));
#414860=CARTESIAN_POINT('Ctrl Pts',(-2.66993091464172,0.226541531261439,
13.850479165618));
#414861=CARTESIAN_POINT('Ctrl Pts',(-2.67582109344563,0.223677620695598,
13.8448473071436));
#414862=CARTESIAN_POINT('Ctrl Pts',(-2.68175383533497,0.221876331818284,
13.8390832900376));
#414863=CARTESIAN_POINT('',(-2.71600461405142,0.211478010012032,13.8057746032556));
#414864=CARTESIAN_POINT('',(-2.68175383533497,0.221876331818285,13.8390832900376));
#414865=CARTESIAN_POINT('',(-2.72150509546337,0.121712890172733,13.8057746032556));
#414866=CARTESIAN_POINT('Origin',(0.,2.5406128344257E-15,13.8057746032556));
#414867=CARTESIAN_POINT('',(-2.68878013986014,0.107210537955378,13.8390832900376));
#414868=CARTESIAN_POINT('',(-2.72150509546337,0.121712890172733,13.8057746032556));
#414869=CARTESIAN_POINT('',(-2.69091550151957,0.00255022285992577,13.8390832900376));
#414870=CARTESIAN_POINT('Ctrl Pts',(-2.68878013986013,0.107210537955379,
13.8390832900376));
#414871=CARTESIAN_POINT('Ctrl Pts',(-2.68240678821043,0.104385959690864,
13.8455641171218));
#414872=CARTESIAN_POINT('Ctrl Pts',(-2.67623296085302,0.100224112250538,
13.851896480191));
#414873=CARTESIAN_POINT('Ctrl Pts',(-2.67087636619504,0.0946207181799948,
13.8574481026913));
#414874=CARTESIAN_POINT('Ctrl Pts',(-2.66725575035062,0.0908332863040082,
13.8612005412592));
#414875=CARTESIAN_POINT('Ctrl Pts',(-2.66393644029487,0.0862858192820752,
13.8646714234115));
#414876=CARTESIAN_POINT('Ctrl Pts',(-2.66130145329037,0.0810865830037507,
13.8674635290331));
#414877=CARTESIAN_POINT('Ctrl Pts',(-2.65917785779804,0.0768964011526091,
13.8697137499649));
#414878=CARTESIAN_POINT('Ctrl Pts',(-2.65746146090153,0.0721784933537311,
13.8715630732994));
#414879=CARTESIAN_POINT('Ctrl Pts',(-2.65640655513463,0.0672249959225243,
13.8727429581918));
#414880=CARTESIAN_POINT('Ctrl Pts',(-2.65533949088734,0.0622144061866732,
13.873936442031));
#414881=CARTESIAN_POINT('Ctrl Pts',(-2.654932226407,0.0568084224563586,
13.8744652622107));
#414882=CARTESIAN_POINT('Ctrl Pts',(-2.65527877155365,0.0515624887305395,
13.8742206332401));
#414883=CARTESIAN_POINT('Ctrl Pts',(-2.65557706494987,0.0470469807151382,
13.8740100655633));
#414884=CARTESIAN_POINT('Ctrl Pts',(-2.6564382669722,0.0425297700201496,
13.8732246156103));
#414885=CARTESIAN_POINT('Ctrl Pts',(-2.65774124509335,0.0383523672539394,
13.8719820486038));
#414886=CARTESIAN_POINT('Ctrl Pts',(-2.65906667655417,0.0341029781345346,
13.8707180692815));
#414887=CARTESIAN_POINT('Ctrl Pts',(-2.66087124467455,0.0301061140894697,
13.868960862563));
#414888=CARTESIAN_POINT('Ctrl Pts',(-2.6629619947775,0.0265395914088023,
13.8669057591701));
#414889=CARTESIAN_POINT('Ctrl Pts',(-2.66618126897233,0.0210479669363342,
13.8637413727084));
#414890=CARTESIAN_POINT('Ctrl Pts',(-2.67015608815293,0.0163931752261725,
13.8597962563956));
#414891=CARTESIAN_POINT('Ctrl Pts',(-2.67442318075955,0.0126398488504258,
13.855546950204));
#414892=CARTESIAN_POINT('Ctrl Pts',(-2.67951217768382,0.0081635770319262,
13.850479165618));
#414893=CARTESIAN_POINT('Ctrl Pts',(-2.6851493221053,0.00482909163796583,
13.8448473071436));
#414894=CARTESIAN_POINT('Ctrl Pts',(-2.69091550151957,0.0025502228599249,
13.8390832900376));
#414895=CARTESIAN_POINT('',(-2.72420475383482,-0.0106052558224246,13.8057746032556));
#414896=CARTESIAN_POINT('',(-2.69091550151957,0.00255022285992577,13.8390832900376));
#414897=CARTESIAN_POINT('',(-2.722370242243,-0.100520029929612,13.8057746032556));
#414898=CARTESIAN_POINT('Origin',(0.,2.5406128344257E-15,13.8057746032556));
#414899=CARTESIAN_POINT('',(-2.68857209989094,-0.112306739080994,13.8390832900376));
#414900=CARTESIAN_POINT('',(-2.722370242243,-0.100520029929612,13.8057746032556));
#414901=CARTESIAN_POINT('',(-2.68216956901137,-0.21679285741081,13.8390832900376));
#414902=CARTESIAN_POINT('Ctrl Pts',(-2.68857209989094,-0.112306739080995,
13.8390832900376));
#414903=CARTESIAN_POINT('Ctrl Pts',(-2.68198972569242,-0.114602431467585,
13.8455641171218));
#414904=CARTESIAN_POINT('Ctrl Pts',(-2.67549721203314,-0.118247206459234,
13.851896480191));
#414905=CARTESIAN_POINT('Ctrl Pts',(-2.66970171236588,-0.123395343505431,
13.8574481026913));
#414906=CARTESIAN_POINT('Ctrl Pts',(-2.6657844329633,-0.126875059210813,
13.8612005412592));
#414907=CARTESIAN_POINT('Ctrl Pts',(-2.66210550685903,-0.131136840326858,
13.8646714234115));
#414908=CARTESIAN_POINT('Ctrl Pts',(-2.65905550153238,-0.136104000672482,
13.8674635290331));
#414909=CARTESIAN_POINT('Ctrl Pts',(-2.65659743340824,-0.140107147292054,
13.8697137499649));
#414910=CARTESIAN_POINT('Ctrl Pts',(-2.65450219439629,-0.144669454360612,
13.8715630732994));
#414911=CARTESIAN_POINT('Ctrl Pts',(-2.65304704271464,-0.149520484824482,
13.8727429581918));
#414912=CARTESIAN_POINT('Ctrl Pts',(-2.65157511945608,-0.154427426594036,
13.873936442031));
#414913=CARTESIAN_POINT('Ctrl Pts',(-2.65072857225398,-0.159782226523443,
13.8744652622107));
#414914=CARTESIAN_POINT('Ctrl Pts',(-2.65064637200072,-0.165038951484169,
13.8742206332401));
#414915=CARTESIAN_POINT('Ctrl Pts',(-2.65057561702708,-0.169563748200165,
13.8740100655633));
#414916=CARTESIAN_POINT('Ctrl Pts',(-2.65106575886334,-0.174136124209039,
13.8732246156103));
#414917=CARTESIAN_POINT('Ctrl Pts',(-2.65202390432573,-0.178405831825289,
13.8719820486038));
#414918=CARTESIAN_POINT('Ctrl Pts',(-2.65299856086007,-0.182749116421712,
13.8707180692815));
#414919=CARTESIAN_POINT('Ctrl Pts',(-2.65447134290414,-0.186879770285992,
13.868960862563));
#414920=CARTESIAN_POINT('Ctrl Pts',(-2.65626443150014,-0.190604841199624,
13.8669057591701));
#414921=CARTESIAN_POINT('Ctrl Pts',(-2.6590253754494,-0.196340593477848,
13.8637413727084));
#414922=CARTESIAN_POINT('Ctrl Pts',(-2.66260756000972,-0.201303881416225,
13.8597962563956));
#414923=CARTESIAN_POINT('Ctrl Pts',(-2.6665545232739,-0.205392526569279,
13.855546950204));
#414924=CARTESIAN_POINT('Ctrl Pts',(-2.67126172927182,-0.210268704455839,
13.850479165618));
#414925=CARTESIAN_POINT('Ctrl Pts',(-2.67660832504481,-0.214051574227772,
13.8448473071436));
#414926=CARTESIAN_POINT('Ctrl Pts',(-2.68216956901137,-0.21679285741081,
13.8390832900376));
#414927=CARTESIAN_POINT('',(-2.71427576044359,-0.232617945429128,13.8057746032556));
#414928=CARTESIAN_POINT('',(-2.68216956901137,-0.21679285741081,13.8390832900376));
#414929=CARTESIAN_POINT('',(-2.70511846421998,-0.322084005817412,13.8057746032556));
#414930=CARTESIAN_POINT('Origin',(0.,2.5406128344257E-15,13.8057746032556));
#414931=CARTESIAN_POINT('',(-2.67047205618014,-0.33107663329809,13.8390832900376));
#414932=CARTESIAN_POINT('',(-2.70511846421998,-0.322084005817412,13.8057746032556));
#414933=CARTESIAN_POINT('',(-2.65557424054822,-0.434693216983779,13.8390832900376));
#414934=CARTESIAN_POINT('Ctrl Pts',(-2.67047205618014,-0.33107663329809,
13.8390832900376));
#414935=CARTESIAN_POINT('Ctrl Pts',(-2.66372446404708,-0.332828162352686,
13.8455641171218));
#414936=CARTESIAN_POINT('Ctrl Pts',(-2.65695647069315,-0.335931609519436,
13.851896480191));
#414937=CARTESIAN_POINT('Ctrl Pts',(-2.6507606341107,-0.340590229538627,
13.8574481026913));
#414938=CARTESIAN_POINT('Ctrl Pts',(-2.64657275999809,-0.343739072139498,
13.8612005412592));
#414939=CARTESIAN_POINT('Ctrl Pts',(-2.64255870049154,-0.34768680589947,
13.8646714234115));
#414940=CARTESIAN_POINT('Ctrl Pts',(-2.63911397412497,-0.352388834679815,
13.8674635290331));
#414941=CARTESIAN_POINT('Ctrl Pts',(-2.63633779140684,-0.356178305787539,
13.8697137499649));
#414942=CARTESIAN_POINT('Ctrl Pts',(-2.63387765374937,-0.360554650724966,
13.8715630732994));
#414943=CARTESIAN_POINT('Ctrl Pts',(-2.63203193994732,-0.365270931414125,
13.8727429581918));
#414944=CARTESIAN_POINT('Ctrl Pts',(-2.63016495308394,-0.370041570329494,
13.873936442031));
#414945=CARTESIAN_POINT('Ctrl Pts',(-2.62888475679204,-0.375309551147947,
13.8744652622107));
#414946=CARTESIAN_POINT('Ctrl Pts',(-2.62837435816798,-0.380542084706265,
13.8742206332401));
#414947=CARTESIAN_POINT('Ctrl Pts',(-2.62793502568717,-0.385046058347249,
13.8740100655633));
#414948=CARTESIAN_POINT('Ctrl Pts',(-2.62805084552431,-0.389643171262055,
13.8732246156103));
#414949=CARTESIAN_POINT('Ctrl Pts',(-2.62865778202796,-0.393976769528611,
13.8719820486038));
#414950=CARTESIAN_POINT('Ctrl Pts',(-2.62927517745739,-0.398385045759653,
13.8707180692815));
#414951=CARTESIAN_POINT('Ctrl Pts',(-2.63040637230365,-0.402622000623186,
13.868960862563));
#414952=CARTESIAN_POINT('Ctrl Pts',(-2.63188986668393,-0.406480830037446,
13.8669057591701));
#414953=CARTESIAN_POINT('Ctrl Pts',(-2.63417410676116,-0.412422539636349,
13.8637413727084));
#414954=CARTESIAN_POINT('Ctrl Pts',(-2.63733981785397,-0.417661293940601,
13.8597962563956));
#414955=CARTESIAN_POINT('Ctrl Pts',(-2.64094038538639,-0.422058048612047,
13.855546950204));
#414956=CARTESIAN_POINT('Ctrl Pts',(-2.64523447477869,-0.427301682407345,
13.850479165618));
#414957=CARTESIAN_POINT('Ctrl Pts',(-2.65025494119044,-0.431507762183049,
13.8448473071436));
#414958=CARTESIAN_POINT('Ctrl Pts',(-2.65557424054822,-0.434693216983779,
13.8390832900376));
#414959=CARTESIAN_POINT('',(-2.68628370969058,-0.453082600988259,13.8057746032556));
#414960=CARTESIAN_POINT('',(-2.65557424054822,-0.434693216983779,13.8390832900376));
#414961=CARTESIAN_POINT('',(-2.66986456913071,-0.541504565786618,13.8057746032556));
#414962=CARTESIAN_POINT('Origin',(0.,2.5406128344257E-15,13.8057746032556));
#414963=CARTESIAN_POINT('',(-2.63460046153234,-0.547643267144387,13.8390832900376));
#414964=CARTESIAN_POINT('',(-2.66986456913071,-0.541504565786618,13.8057746032556));
#414965=CARTESIAN_POINT('',(-2.61130650365314,-0.649700764917055,13.8390832900376));
#414966=CARTESIAN_POINT('Ctrl Pts',(-2.63460046153233,-0.547643267144386,
13.8390832900376));
#414967=CARTESIAN_POINT('Ctrl Pts',(-2.62773255557711,-0.548838976730111,
13.8455641171218));
#414968=CARTESIAN_POINT('Ctrl Pts',(-2.62073412240766,-0.5513804431431,
13.851896480191));
#414969=CARTESIAN_POINT('Ctrl Pts',(-2.61417918118023,-0.555518543787676,
13.8574481026913));
#414970=CARTESIAN_POINT('Ctrl Pts',(-2.60974858196886,-0.558315558256049,
13.8612005412592));
#414971=CARTESIAN_POINT('Ctrl Pts',(-2.60542610196377,-0.561922973143106,
13.8646714234115));
#414972=CARTESIAN_POINT('Ctrl Pts',(-2.60160957864291,-0.566328579132419,
13.8674635290331));
#414973=CARTESIAN_POINT('Ctrl Pts',(-2.59853375636875,-0.569879156423292,
13.8697137499649));
#414974=CARTESIAN_POINT('Ctrl Pts',(-2.59572509187598,-0.574040415376077,
13.8715630732994));
#414975=CARTESIAN_POINT('Ctrl Pts',(-2.59350109887437,-0.578590560220671,
13.8727429581918));
#414976=CARTESIAN_POINT('Ctrl Pts',(-2.5912514728957,-0.583193148466973,
13.873936442031));
#414977=CARTESIAN_POINT('Ctrl Pts',(-2.5895461470091,-0.588339252631275,
13.8744652622107));
#414978=CARTESIAN_POINT('Ctrl Pts',(-2.58861094663289,-0.593512773139661,
13.8742206332401));
#414979=CARTESIAN_POINT('Ctrl Pts',(-2.58780596033007,-0.597965950504156,
13.8740100655633));
#414980=CARTESIAN_POINT('Ctrl Pts',(-2.58754668740619,-0.602557207296923,
13.8732246156103));
#414981=CARTESIAN_POINT('Ctrl Pts',(-2.5877983758888,-0.606925856832314,
13.8719820486038));
#414982=CARTESIAN_POINT('Ctrl Pts',(-2.5880544015486,-0.611369788346972,
13.8707180692815));
#414983=CARTESIAN_POINT('Ctrl Pts',(-2.58883648128198,-0.615684847974192,
13.868960862563));
#414984=CARTESIAN_POINT('Ctrl Pts',(-2.59000050903621,-0.61965175601599,
13.8669057591701));
#414985=CARTESIAN_POINT('Ctrl Pts',(-2.59179284400056,-0.625759881838503,
13.8637413727084));
#414986=CARTESIAN_POINT('Ctrl Pts',(-2.59452101434085,-0.631239239463067,
13.8597962563956));
#414987=CARTESIAN_POINT('Ctrl Pts',(-2.59775122495862,-0.63591484397598,
13.855546950204));
#414988=CARTESIAN_POINT('Ctrl Pts',(-2.60160362128887,-0.641491038162247,
13.850479165618));
#414989=CARTESIAN_POINT('Ctrl Pts',(-2.60626454796374,-0.646092337174765,
13.8448473071436));
#414990=CARTESIAN_POINT('Ctrl Pts',(-2.61130650365314,-0.649700764917052,
13.8390832900376));
#414991=CARTESIAN_POINT('',(-2.6404148840552,-0.670532066591181,13.8057746032556));
#414992=CARTESIAN_POINT('',(-2.61130650365314,-0.649700764917055,13.8390832900376));
#414993=CARTESIAN_POINT('',(-2.61684316583052,-0.757321502212479,13.8057746032556));
#414994=CARTESIAN_POINT('Origin',(0.,2.5406128344257E-15,13.8057746032556));
#414995=CARTESIAN_POINT('',(-2.58119603549152,-0.760565425402617,13.8390832900376));
#414996=CARTESIAN_POINT('',(-2.61684316583052,-0.757321502212479,13.8057746032556));
#414997=CARTESIAN_POINT('',(-2.54966095281149,-0.860384661452888,13.8390832900376));
#414998=CARTESIAN_POINT('Ctrl Pts',(-2.58119603549151,-0.760565425402616,
13.8390832900376));
#414999=CARTESIAN_POINT('Ctrl Pts',(-2.57425352049513,-0.761197358269454,
13.8455641171218));
#415000=CARTESIAN_POINT('Ctrl Pts',(-2.56707122092824,-0.763159930889019,
13.851896480191));
#415001=CARTESIAN_POINT('Ctrl Pts',(-2.56020079710822,-0.766749973781928,
13.8574481026913));
#415002=CARTESIAN_POINT('Ctrl Pts',(-2.55555695770483,-0.769176546447992,
13.8612005412592));
#415003=CARTESIAN_POINT('Ctrl Pts',(-2.55095482259248,-0.772419635711239,
13.8646714234115));
#415004=CARTESIAN_POINT('Ctrl Pts',(-2.54679190065035,-0.776499500328535,
13.8674635290331));
#415005=CARTESIAN_POINT('Ctrl Pts',(-2.54343690790991,-0.779787555296489,
13.8697137499649));
#415006=CARTESIAN_POINT('Ctrl Pts',(-2.54029840778065,-0.783706035772858,
13.8715630732994));
#415007=CARTESIAN_POINT('Ctrl Pts',(-2.53771093588596,-0.788059764309667,
13.8727429581918));
#415008=CARTESIAN_POINT('Ctrl Pts',(-2.53509364168175,-0.792463672421497,
13.873936442031));
#415009=CARTESIAN_POINT('Ctrl Pts',(-2.53297453486286,-0.797453653457486,
13.8744652622107));
#415010=CARTESIAN_POINT('Ctrl Pts',(-2.53162075633869,-0.802533731990528,
13.8742206332401));
#415011=CARTESIAN_POINT('Ctrl Pts',(-2.5304554732649,-0.806906477917896,
13.8740100655633));
#415012=CARTESIAN_POINT('Ctrl Pts',(-2.52982283299853,-0.811461324532166,
13.8732246156103));
#415013=CARTESIAN_POINT('Ctrl Pts',(-2.52971759851478,-0.81583595269451,
13.8719820486038));
#415014=CARTESIAN_POINT('Ctrl Pts',(-2.52961055059642,-0.820285965861752,
13.8707180692815));
#415015=CARTESIAN_POINT('Ctrl Pts',(-2.53003831060533,-0.824650414242775,
13.868960862563));
#415016=CARTESIAN_POINT('Ctrl Pts',(-2.53087512532085,-0.828699001793586,
13.8669057591701));
#415017=CARTESIAN_POINT('Ctrl Pts',(-2.53216362747886,-0.834932895270131,
13.8637413727084));
#415018=CARTESIAN_POINT('Ctrl Pts',(-2.53443610154312,-0.840616391994046,
13.8597962563956));
#415019=CARTESIAN_POINT('Ctrl Pts',(-2.53727445872754,-0.845539730971813,
13.855546950204));
#415020=CARTESIAN_POINT('Ctrl Pts',(-2.54065952493376,-0.851411376896747,
13.850479165618));
#415021=CARTESIAN_POINT('Ctrl Pts',(-2.54492989417372,-0.856377274260319,
13.8448473071436));
#415022=CARTESIAN_POINT('Ctrl Pts',(-2.54966095281148,-0.860384661452887,
13.8390832900376));
#415023=CARTESIAN_POINT('',(-2.57697453300422,-0.883519251920942,13.8057746032556));
#415024=CARTESIAN_POINT('',(-2.54966095281149,-0.860384661452888,13.8390832900376));
#415025=CARTESIAN_POINT('',(-2.54640710301046,-0.968098588990368,13.8057746032556));
#415026=CARTESIAN_POINT('Origin',(0.,2.5406128344257E-15,13.8057746032556));
#415027=CARTESIAN_POINT('',(-2.51061417570187,-0.968426146239254,13.8390832900376));
#415028=CARTESIAN_POINT('',(-2.54640710301046,-0.968098588990368,13.8057746032556));
#415029=CARTESIAN_POINT('',(-2.47104782899332,-1.06534284002023,13.8390832900376));
#415030=CARTESIAN_POINT('Ctrl Pts',(-2.51061417570186,-0.968426146239253,
13.8390832900376));
#415031=CARTESIAN_POINT('Ctrl Pts',(-2.50364325295619,-0.968490096978238,
13.8455641171218));
#415032=CARTESIAN_POINT('Ctrl Pts',(-2.49632488401048,-0.969860715207392,
13.851896480191));
#415033=CARTESIAN_POINT('Ctrl Pts',(-2.48918469913484,-0.972878809205498,
13.8574481026913));
#415034=CARTESIAN_POINT('Ctrl Pts',(-2.4843585235245,-0.974918791628515,
13.8612005412592));
#415035=CARTESIAN_POINT('Ctrl Pts',(-2.47950735975475,-0.977775973043983,
13.8646714234115));
#415036=CARTESIAN_POINT('Ctrl Pts',(-2.47502574275005,-0.981502945463366,
13.8674635290331));
#415037=CARTESIAN_POINT('Ctrl Pts',(-2.47141390646648,-0.984506596645081,
13.8697137499649));
#415038=CARTESIAN_POINT('Ctrl Pts',(-2.46796645690127,-0.988156221803966,
13.8715630732994));
#415039=CARTESIAN_POINT('Ctrl Pts',(-2.46503272531207,-0.992284560687893,
13.8727429581918));
#415040=CARTESIAN_POINT('Ctrl Pts',(-2.4620651805434,-0.99646048138336,
13.873936442031));
#415041=CARTESIAN_POINT('Ctrl Pts',(-2.45954639509848,-1.00126113179053,
13.8744652622107));
#415042=CARTESIAN_POINT('Ctrl Pts',(-2.45778304759909,-1.00621396126374,
13.8742206332401));
#415043=CARTESIAN_POINT('Ctrl Pts',(-2.45626522252092,-1.01047717585129,
13.8740100655633));
#415044=CARTESIAN_POINT('Ctrl Pts',(-2.45526342502865,-1.01496530053435,
13.8732246156103));
#415045=CARTESIAN_POINT('Ctrl Pts',(-2.45480196789667,-1.01931679489499,
13.8719820486038));
#415046=CARTESIAN_POINT('Ctrl Pts',(-2.45433255878639,-1.02374327561139,
13.8707180692815));
#415047=CARTESIAN_POINT('Ctrl Pts',(-2.45440315239855,-1.02812806806232,
13.868960862563));
#415048=CARTESIAN_POINT('Ctrl Pts',(-2.45490718521148,-1.03223139243996,
13.8669057591701));
#415049=CARTESIAN_POINT('Ctrl Pts',(-2.45568327979387,-1.03854956803797,
13.8637413727084));
#415050=CARTESIAN_POINT('Ctrl Pts',(-2.45748493464214,-1.04439938112825,
13.8597962563956));
#415051=CARTESIAN_POINT('Ctrl Pts',(-2.45991254959444,-1.04953769056227,
13.855546950204));
#415052=CARTESIAN_POINT('Ctrl Pts',(-2.46280775861952,-1.05566571339099,
13.850479165618));
#415053=CARTESIAN_POINT('Ctrl Pts',(-2.46665915182185,-1.06096316187798,
13.8448473071436));
#415054=CARTESIAN_POINT('Ctrl Pts',(-2.47104782899332,-1.06534284002023,
13.8390832900376));
#415055=CARTESIAN_POINT('',(-2.49638484160697,-1.09062676239959,13.8057746032556));
#415056=CARTESIAN_POINT('',(-2.47104782899332,-1.06534284002023,13.8390832900376));
#415057=CARTESIAN_POINT('',(-2.45902512104747,-1.17243313938355,13.8057746032556));
#415058=CARTESIAN_POINT('Origin',(0.,2.5406128344257E-15,13.8057746032556));
#415059=CARTESIAN_POINT('',(-2.42332459279511,-1.16984215085174,13.8390832900376));
#415060=CARTESIAN_POINT('',(-2.45902512104747,-1.17243313938355,13.8057746032556));
#415061=CARTESIAN_POINT('',(-2.3759902895674,-1.26321133775643,13.8390832900376));
#415062=CARTESIAN_POINT('Ctrl Pts',(-2.4233245927951,-1.16984215085174,
13.8390832900376));
#415063=CARTESIAN_POINT('Ctrl Pts',(-2.41637165264089,-1.16933769388125,
13.8455641171218));
#415064=CARTESIAN_POINT('Ctrl Pts',(-2.40896591685425,-1.17010723648182,
13.851896480191));
#415065=CARTESIAN_POINT('Ctrl Pts',(-2.4016034876753,-1.17253329666751,
13.8574481026913));
#415066=CARTESIAN_POINT('Ctrl Pts',(-2.39662709326041,-1.17417311310103,
13.8612005412592));
#415067=CARTESIAN_POINT('Ctrl Pts',(-2.39155918452778,-1.1766253725978,
13.8646714234115));
#415068=CARTESIAN_POINT('Ctrl Pts',(-2.38678869688225,-1.17997465043272,
13.8674635290331));
#415069=CARTESIAN_POINT('Ctrl Pts',(-2.38294405323011,-1.18267390902515,
13.8697137499649));
#415070=CARTESIAN_POINT('Ctrl Pts',(-2.37921059643702,-1.18603039121327,
13.8715630732994));
#415071=CARTESIAN_POINT('Ctrl Pts',(-2.375950128653,-1.18990586703017,13.8727429581918));
#415072=CARTESIAN_POINT('Ctrl Pts',(-2.37265208184071,-1.19382601024602,
13.873936442031));
#415073=CARTESIAN_POINT('Ctrl Pts',(-2.36975037987132,-1.19840538248796,
13.8744652622107));
#415074=CARTESIAN_POINT('Ctrl Pts',(-2.36758919818337,-1.20319800263837,
13.8742206332401));
#415075=CARTESIAN_POINT('Ctrl Pts',(-2.3657289319763,-1.20732331489639,
13.8740100655633));
#415076=CARTESIAN_POINT('Ctrl Pts',(-2.36436464405516,-1.21171484991895,
13.8732246156103));
#415077=CARTESIAN_POINT('Ctrl Pts',(-2.36355003519602,-1.21601425200087,
13.8719820486038));
#415078=CARTESIAN_POINT('Ctrl Pts',(-2.36272138873401,-1.22038774276757,
13.8707180692815));
#415079=CARTESIAN_POINT('Ctrl Pts',(-2.36243434616056,-1.22476369921809,
13.868960862563));
#415080=CARTESIAN_POINT('Ctrl Pts',(-2.36260224281571,-1.22889445347584,
13.8669057591701));
#415081=CARTESIAN_POINT('Ctrl Pts',(-2.36286076504108,-1.23525486477913,
13.8637413727084));
#415082=CARTESIAN_POINT('Ctrl Pts',(-2.3641796109576,-1.24123206469481,
13.8597962563956));
#415083=CARTESIAN_POINT('Ctrl Pts',(-2.3661803283008,-1.24655114998356,
13.855546950204));
#415084=CARTESIAN_POINT('Ctrl Pts',(-2.36856641300636,-1.2528947687352,
13.850479165618));
#415085=CARTESIAN_POINT('Ctrl Pts',(-2.37197319978472,-1.25848851469993,
13.8448473071436));
#415086=CARTESIAN_POINT('Ctrl Pts',(-2.3759902895674,-1.26321133775643,
13.8390832900376));
#415087=CARTESIAN_POINT('',(-2.39918212096334,-1.29047633171521,13.8057746032556));
#415088=CARTESIAN_POINT('',(-2.3759902895674,-1.26321133775643,13.8390832900376));
#415089=CARTESIAN_POINT('',(-2.35527873261449,-1.36896534067199,13.8057746032556));
#415090=CARTESIAN_POINT('Origin',(0.,2.5406128344257E-15,13.8057746032556));
#415091=CARTESIAN_POINT('',(-2.31990818454371,-1.36347304896067,13.8390832900376));
#415092=CARTESIAN_POINT('',(-2.35527873261449,-1.36896534067199,13.8057746032556));
#415093=CARTESIAN_POINT('',(-2.26512092677521,-1.45267337245507,13.8390832900376));
#415094=CARTESIAN_POINT('Ctrl Pts',(-2.3199081845437,-1.36347304896067,
13.8390832900376));
#415095=CARTESIAN_POINT('Ctrl Pts',(-2.31301949765052,-1.36240354135862,
13.8455641171218));
#415096=CARTESIAN_POINT('Ctrl Pts',(-2.30557567897275,-1.36256688715156,
13.851896480191));
#415097=CARTESIAN_POINT('Ctrl Pts',(-2.29804000124195,-1.36438476849458,
13.8574481026913));
#415098=CARTESIAN_POINT('Ctrl Pts',(-2.29294650510632,-1.36561350623079,
13.8612005412592));
#415099=CARTESIAN_POINT('Ctrl Pts',(-2.28769557750727,-1.3676445244265,
13.8646714234115));
#415100=CARTESIAN_POINT('Ctrl Pts',(-2.28266796602911,-1.37059381878557,
13.8674635290331));
#415101=CARTESIAN_POINT('Ctrl Pts',(-2.27861610047759,-1.37297072166812,
13.8697137499649));
#415102=CARTESIAN_POINT('Ctrl Pts',(-2.27462148199559,-1.37601172405029,
13.8715630732994));
#415103=CARTESIAN_POINT('Ctrl Pts',(-2.27105597589192,-1.37960854614801,
13.8727429581918));
#415104=CARTESIAN_POINT('Ctrl Pts',(-2.2674493749934,-1.38324682397793,
13.873936442031));
#415105=CARTESIAN_POINT('Ctrl Pts',(-2.26418406684741,-1.38757444308791,
13.8744652622107));
#415106=CARTESIAN_POINT('Ctrl Pts',(-2.26163943327847,-1.39217495981913,
13.8742206332401));
#415107=CARTESIAN_POINT('Ctrl Pts',(-2.25944910570718,-1.39613491647519,
13.8740100655633));
#415108=CARTESIAN_POINT('Ctrl Pts',(-2.25773140646819,-1.40040063689623,
13.8732246156103));
#415109=CARTESIAN_POINT('Ctrl Pts',(-2.25656906696945,-1.40461933488791,
13.8719820486038));
#415110=CARTESIAN_POINT('Ctrl Pts',(-2.25538669766119,-1.40891073084545,
13.8707180692815));
#415111=CARTESIAN_POINT('Ctrl Pts',(-2.25474392912311,-1.41324873002736,
13.868960862563));
#415112=CARTESIAN_POINT('Ctrl Pts',(-2.25457457229593,-1.41737942467715,
13.8669057591701));
#415113=CARTESIAN_POINT('Ctrl Pts',(-2.25431380174153,-1.4237397441979,
13.8637413727084));
#415114=CARTESIAN_POINT('Ctrl Pts',(-2.25514106202431,-1.42980455365971,
13.8597962563956));
#415115=CARTESIAN_POINT('Ctrl Pts',(-2.25670156731458,-1.43526901716817,
13.855546950204));
#415116=CARTESIAN_POINT('Ctrl Pts',(-2.25856264870058,-1.44178601610656,
13.850479165618));
#415117=CARTESIAN_POINT('Ctrl Pts',(-2.26150215745105,-1.44763883409255,
13.8448473071436));
#415118=CARTESIAN_POINT('Ctrl Pts',(-2.26512092677521,-1.45267337245507,
13.8390832900376));
#415119=CARTESIAN_POINT('',(-2.28601323914187,-1.48173799395688,13.8057746032556));
#415120=CARTESIAN_POINT('',(-2.26512092677521,-1.45267337245507,13.8390832900376));
#415121=CARTESIAN_POINT('',(-2.2358583528096,-1.55638730348163,13.8057746032556));
#415122=CARTESIAN_POINT('Origin',(0.,2.5406128344257E-15,13.8057746032556));
#415123=CARTESIAN_POINT('',(-2.20105317008208,-1.54803025888599,13.8390832900376));
#415124=CARTESIAN_POINT('',(-2.2358583528096,-1.55638730348163,13.8057746032556));
#415125=CARTESIAN_POINT('',(-2.13917755793398,-1.63246810553425,13.8390832900376));
#415126=CARTESIAN_POINT('Ctrl Pts',(-2.20105317008207,-1.54803025888599,
13.8390832900376));
#415127=CARTESIAN_POINT('Ctrl Pts',(-2.19427457952464,-1.54640281804902,
13.8455641171218));
#415128=CARTESIAN_POINT('Ctrl Pts',(-2.18684221534089,-1.54595887999502,
13.851896480191));
#415129=CARTESIAN_POINT('Ctrl Pts',(-2.17918343775026,-1.54715648479496,
13.8574481026913));
#415130=CARTESIAN_POINT('Ctrl Pts',(-2.17400673627028,-1.54796596678695,
13.8612005412592));
#415131=CARTESIAN_POINT('Ctrl Pts',(-2.16860773386164,-1.54956222759061,
13.8646714234115));
#415132=CARTESIAN_POINT('Ctrl Pts',(-2.16335645647575,-1.55209191140646,
13.8674635290331));
#415133=CARTESIAN_POINT('Ctrl Pts',(-2.15912433352158,-1.55413064068262,
13.8697137499649));
#415134=CARTESIAN_POINT('Ctrl Pts',(-2.15489513687762,-1.55683592588971,
13.8715630732994));
#415135=CARTESIAN_POINT('Ctrl Pts',(-2.15104832030914,-1.56013015801062,
13.8727429581918));
#415136=CARTESIAN_POINT('Ctrl Pts',(-2.14715716665832,-1.56346235831592,
13.873936442031));
#415137=CARTESIAN_POINT('Ctrl Pts',(-2.1435499824227,-1.56750942470278,
13.8744652622107));
#415138=CARTESIAN_POINT('Ctrl Pts',(-2.14063883108934,-1.571887222335,13.8742206332401));
#415139=CARTESIAN_POINT('Ctrl Pts',(-2.13813301842244,-1.57565547053088,
13.8740100655633));
#415140=CARTESIAN_POINT('Ctrl Pts',(-2.13607333887064,-1.57976698868481,
13.8732246156103));
#415141=CARTESIAN_POINT('Ctrl Pts',(-2.13457100390989,-1.58387690784716,
13.8719820486038));
#415142=CARTESIAN_POINT('Ctrl Pts',(-2.13304278022804,-1.58805765046345,
13.8707180692815));
#415143=CARTESIAN_POINT('Ctrl Pts',(-2.13204856324391,-1.59232882370792,
13.868960862563));
#415144=CARTESIAN_POINT('Ctrl Pts',(-2.13154307997614,-1.59643196965837,
13.8669057591701));
#415145=CARTESIAN_POINT('Ctrl Pts',(-2.13076475202698,-1.60274987051955,
13.8637413727084));
#415146=CARTESIAN_POINT('Ctrl Pts',(-2.13109492139534,-1.60886192922114,
13.8597962563956));
#415147=CARTESIAN_POINT('Ctrl Pts',(-2.13220482972745,-1.61443540584625,
13.855546950204));
#415148=CARTESIAN_POINT('Ctrl Pts',(-2.13352852260432,-1.62108241541868,
13.850479165618));
#415149=CARTESIAN_POINT('Ctrl Pts',(-2.13598119138114,-1.62715535588788,
13.8448473071436));
#415150=CARTESIAN_POINT('Ctrl Pts',(-2.13917755793398,-1.63246810553424,
13.8390832900376));
#415151=CARTESIAN_POINT('',(-2.15763131637956,-1.66313893431832,13.8057746032556));
#415152=CARTESIAN_POINT('',(-2.13917755793398,-1.63246810553425,13.8390832900376));
#415153=CARTESIAN_POINT('',(-2.10155870455742,-1.73345176557244,13.8057746032556));
#415154=CARTESIAN_POINT('Origin',(0.,2.5406128344257E-15,13.8057746032556));
#415155=CARTESIAN_POINT('',(-2.06755050992176,-1.72228558284544,13.8390832900376));
#415156=CARTESIAN_POINT('',(-2.10155870455742,-1.73345176557244,13.8057746032556));
#415157=CARTESIAN_POINT('',(-1.99899831538416,-1.80139903270938,13.8390832900376));
#415158=CARTESIAN_POINT('Ctrl Pts',(-2.06755050992176,-1.72228558284543,
13.8390832900376));
#415159=CARTESIAN_POINT('Ctrl Pts',(-2.06092712610185,-1.7201110391238,
13.8455641171218));
#415160=CARTESIAN_POINT('Ctrl Pts',(-2.05355567756952,-1.71906277155738,
13.851896480191));
#415161=CARTESIAN_POINT('Ctrl Pts',(-2.04582476802029,-1.71963212995188,
13.8574481026913));
#415162=CARTESIAN_POINT('Ctrl Pts',(-2.04059931129023,-1.72001696923055,
13.8612005412592));
#415163=CARTESIAN_POINT('Ctrl Pts',(-2.03508816354226,-1.72116784978987,
13.8646714234115));
#415164=CARTESIAN_POINT('Ctrl Pts',(-2.02964816663325,-1.72326108843407,
13.8674635290331));
#415165=CARTESIAN_POINT('Ctrl Pts',(-2.02526395035643,-1.72494807669687,
13.8697137499649));
#415166=CARTESIAN_POINT('Ctrl Pts',(-2.02082832015639,-1.72729964150218,
13.8715630732994));
#415167=CARTESIAN_POINT('Ctrl Pts',(-2.01672579305269,-1.73026936107504,
13.8727429581918));
#415168=CARTESIAN_POINT('Ctrl Pts',(-2.01257598163513,-1.73327330861246,
13.873936442031));
#415169=CARTESIAN_POINT('Ctrl Pts',(-2.00865092652582,-1.7370128897171,
13.8744652622107));
#415170=CARTESIAN_POINT('Ctrl Pts',(-2.00539263065985,-1.74113883472936,
13.8742206332401));
#415171=CARTESIAN_POINT('Ctrl Pts',(-2.00258800866722,-1.74469029739505,
13.8740100655633));
#415172=CARTESIAN_POINT('Ctrl Pts',(-2.00020005563019,-1.74862025180689,
13.8732246156103));
#415173=CARTESIAN_POINT('Ctrl Pts',(-1.99836772299873,-1.75259404130597,
13.8719820486038));
#415174=CARTESIAN_POINT('Ctrl Pts',(-1.99650381501977,-1.7566363084287,
13.8707180692815));
#415175=CARTESIAN_POINT('Ctrl Pts',(-1.99516476593957,-1.76081223178248,
13.868960862563));
#415176=CARTESIAN_POINT('Ctrl Pts',(-1.99432652013897,-1.76486052327426,
13.8669057591701));
#415177=CARTESIAN_POINT('Ctrl Pts',(-1.99303581443913,-1.77109396088801,
13.8637413727084));
#415178=CARTESIAN_POINT('Ctrl Pts',(-1.99286669567039,-1.77721259408715,
13.8597962563956));
#415179=CARTESIAN_POINT('Ctrl Pts',(-1.9935186207875,-1.78285799326152,
13.855546950204));
#415180=CARTESIAN_POINT('Ctrl Pts',(-1.99429611619754,-1.78959077871597,
13.850479165618));
#415181=CARTESIAN_POINT('Ctrl Pts',(-1.99624562289467,-1.79584342725151,
13.8448473071436));
#415182=CARTESIAN_POINT('Ctrl Pts',(-1.99899831538415,-1.80139903270938,
13.8390832900376));
#415183=CARTESIAN_POINT('',(-2.01489071319085,-1.83347195947049,13.8057746032556));
#415184=CARTESIAN_POINT('',(-1.99899831538416,-1.80139903270938,13.8390832900376));
#415185=CARTESIAN_POINT('',(-1.95327352985919,-1.89898039216277,13.8057746032556));
#415186=CARTESIAN_POINT('Origin',(0.,2.5406128344257E-15,13.8057746032556));
#415187=CARTESIAN_POINT('',(-1.92028864223974,-1.88507938040817,13.8390832900376));
#415188=CARTESIAN_POINT('',(-1.95327352985919,-1.89898039216277,13.8057746032556));
#415189=CARTESIAN_POINT('',(-1.84551606885696,-1.95834194653175,13.8390832900376));
#415190=CARTESIAN_POINT('Ctrl Pts',(-1.92028864223974,-1.88507938040816,
13.8390832900376));
#415191=CARTESIAN_POINT('Ctrl Pts',(-1.91386454268389,-1.88237220503155,
13.8455641171218));
#415192=CARTESIAN_POINT('Ctrl Pts',(-1.90660306557675,-1.88072658400041,
13.851896480191));
#415193=CARTESIAN_POINT('Ctrl Pts',(-1.89885147199648,-1.8806639070033,
13.8574481026913));
#415194=CARTESIAN_POINT('Ctrl Pts',(-1.89361203456873,-1.88062154252675,
13.8612005412592));
#415195=CARTESIAN_POINT('Ctrl Pts',(-1.88802541726042,-1.88131938392148,
13.8646714234115));
#415196=CARTESIAN_POINT('Ctrl Pts',(-1.88243290311017,-1.88296224723623,
13.8674635290331));
#415197=CARTESIAN_POINT('Ctrl Pts',(-1.87792576974669,-1.88428626785711,
13.8697137499649));
#415198=CARTESIAN_POINT('Ctrl Pts',(-1.87331322437773,-1.88626846298484,
13.8715630732994));
#415199=CARTESIAN_POINT('Ctrl Pts',(-1.86898228837981,-1.88889390701584,
13.8727429581918));
#415200=CARTESIAN_POINT('Ctrl Pts',(-1.86460143550582,-1.89154961101014,
13.873936442031));
#415201=CARTESIAN_POINT('Ctrl Pts',(-1.86038463011699,-1.89495682053731,
13.8744652622107));
#415202=CARTESIAN_POINT('Ctrl Pts',(-1.85680087313982,-1.89880345544629,
13.8742206332401));
#415203=CARTESIAN_POINT('Ctrl Pts',(-1.85371610611807,-1.90211449818369,
13.8740100655633));
#415204=CARTESIAN_POINT('Ctrl Pts',(-1.85101577102931,-1.90583673565523,
13.8732246156103));
#415205=CARTESIAN_POINT('Ctrl Pts',(-1.84886563459848,-1.90964795057756,
13.8719820486038));
#415206=CARTESIAN_POINT('Ctrl Pts',(-1.84667844632248,-1.91352484158593,
13.8707180692815));
#415207=CARTESIAN_POINT('Ctrl Pts',(-1.84500347629691,-1.91757772496808,
13.868960862563));
#415208=CARTESIAN_POINT('Ctrl Pts',(-1.84383804635098,-1.92154422128925,
13.8669057591701));
#415209=CARTESIAN_POINT('Ctrl Pts',(-1.84204355233396,-1.9276517131567,
13.8637413727084));
#415210=CARTESIAN_POINT('Ctrl Pts',(-1.84137627088561,-1.93373620235893,
13.8597962563956));
#415211=CARTESIAN_POINT('Ctrl Pts',(-1.84156587433364,-1.93941595488249,
13.855546950204));
#415212=CARTESIAN_POINT('Ctrl Pts',(-1.84179199817318,-1.94618971064259,
13.850479165618));
#415213=CARTESIAN_POINT('Ctrl Pts',(-1.84322536914519,-1.95258045690009,
13.8448473071436));
#415214=CARTESIAN_POINT('Ctrl Pts',(-1.84551606885695,-1.95834194653174,
13.8390832900376));
#415215=CARTESIAN_POINT('',(-1.85874134473942,-1.99160353123396,13.8057746032556));
#415216=CARTESIAN_POINT('',(-1.84551606885696,-1.95834194653175,13.8390832900376));
#415217=CARTESIAN_POINT('',(-1.7919896420872,-2.05187161755297,13.8057746032556));
#415218=CARTESIAN_POINT('Origin',(0.,2.5406128344257E-15,13.8057746032556));
#415219=CARTESIAN_POINT('',(-1.76024757046894,-2.03532828571048,13.8390832900376));
#415220=CARTESIAN_POINT('',(-1.7919896420872,-2.05187161755297,13.8057746032556));
#415221=CARTESIAN_POINT('',(-1.67975221738023,-2.10225241780362,13.8390832900376));
#415222=CARTESIAN_POINT('Ctrl Pts',(-1.76024757046894,-2.03532828571048,
13.8390832900376));
#415223=CARTESIAN_POINT('Ctrl Pts',(-1.7540655064998,-2.03210649448438,
13.8455641171218));
#415224=CARTESIAN_POINT('Ctrl Pts',(-1.74696232474994,-2.02987447132497,
13.851896480191));
#415225=CARTESIAN_POINT('Ctrl Pts',(-1.73924163271497,-2.02918017604132,
13.8574481026913));
#415226=CARTESIAN_POINT('Ctrl Pts',(-1.73402308218118,-2.02871088973814,
13.8612005412592));
#415227=CARTESIAN_POINT('Ctrl Pts',(-1.72839817332898,-2.02895104794895,
13.8646714234115));
#415228=CARTESIAN_POINT('Ctrl Pts',(-1.72269035919646,-2.03013260294993,
13.8674635290331));
#415229=CARTESIAN_POINT('Ctrl Pts',(-1.71809030297523,-2.03108484479011,
13.8697137499649));
#415230=CARTESIAN_POINT('Ctrl Pts',(-1.71333153816577,-2.03268447905872,
13.8715630732994));
#415231=CARTESIAN_POINT('Ctrl Pts',(-1.70880101493814,-2.03494817565101,
13.8727429581918));
#415232=CARTESIAN_POINT('Ctrl Pts',(-1.70421827446081,-2.03723796283027,
13.873936442031));
#415233=CARTESIAN_POINT('Ctrl Pts',(-1.69973778093659,-2.04029012636271,
13.8744652622107));
#415234=CARTESIAN_POINT('Ctrl Pts',(-1.69585241215962,-2.04383185244774,
13.8742206332401));
#415235=CARTESIAN_POINT('Ctrl Pts',(-1.69250802872435,-2.04688044081372,
13.8740100655633));
#415236=CARTESIAN_POINT('Ctrl Pts',(-1.68951328186832,-2.05037019046872,
13.8732246156103));
#415237=CARTESIAN_POINT('Ctrl Pts',(-1.68705965044134,-2.05399346780779,
13.8719820486038));
#415238=CARTESIAN_POINT('Ctrl Pts',(-1.68456373724541,-2.05767918263179,
13.8707180692815));
#415239=CARTESIAN_POINT('Ctrl Pts',(-1.68256399292365,-2.06158205477208,
13.868960862563));
#415240=CARTESIAN_POINT('Ctrl Pts',(-1.68107913457639,-2.06544035954403,
13.8669057591701));
#415241=CARTESIAN_POINT('Ctrl Pts',(-1.67879279430379,-2.07138126131447,
13.8637413727084));
#415242=CARTESIAN_POINT('Ctrl Pts',(-1.67763179082379,-2.07739111524804,
13.8597962563956));
#415243=CARTESIAN_POINT('Ctrl Pts',(-1.67735781082307,-2.08306742330483,
13.855546950204));
#415244=CARTESIAN_POINT('Ctrl Pts',(-1.67703105827525,-2.08983707114359,
13.850479165618));
#415245=CARTESIAN_POINT('Ctrl Pts',(-1.67793875467482,-2.0963233857611,
13.8448473071436));
#415246=CARTESIAN_POINT('Ctrl Pts',(-1.67975221738023,-2.10225241780362,
13.8390832900376));
#415247=CARTESIAN_POINT('',(-1.69022235930949,-2.13648131008852,13.8057746032556));
#415248=CARTESIAN_POINT('',(-1.67975221738023,-2.10225241780362,13.8390832900376));
#415249=CARTESIAN_POINT('',(-1.6187803589046,-2.19110797586335,13.8057746032556));
#415250=CARTESIAN_POINT('Origin',(0.,2.5406128344257E-15,13.8057746032556));
#415251=CARTESIAN_POINT('',(-1.58849234153707,-2.17203241707693,13.8390832900376));
#415252=CARTESIAN_POINT('',(-1.6187803589046,-2.19110797586335,13.8057746032556));
#415253=CARTESIAN_POINT('',(-1.50280989203645,-2.23217274608225,13.8390832900376));
#415254=CARTESIAN_POINT('Ctrl Pts',(-1.58849234153707,-2.17203241707693,
13.8390832900376));
#415255=CARTESIAN_POINT('Ctrl Pts',(-1.58259345377038,-2.16831745049039,
13.8455641171218));
#415256=CARTESIAN_POINT('Ctrl Pts',(-1.57569583788041,-2.16551387894857,
13.851896480191));
#415257=CARTESIAN_POINT('Ctrl Pts',(-1.56805742732242,-2.16419258579895,
13.8574481026913));
#415258=CARTESIAN_POINT('Ctrl Pts',(-1.56289449227537,-2.16329950069206,
13.8612005412592));
#415259=CARTESIAN_POINT('Ctrl Pts',(-1.55726872471966,-2.16308037750568,
13.8646714234115));
#415260=CARTESIAN_POINT('Ctrl Pts',(-1.5514835951662,-2.1637927611393,13.8674635290331));
#415261=CARTESIAN_POINT('Ctrl Pts',(-1.54682122870241,-2.16436688718645,
13.8697137499649));
#415262=CARTESIAN_POINT('Ctrl Pts',(-1.54194791324711,-2.1655733152938,
13.8715630732994));
#415263=CARTESIAN_POINT('Ctrl Pts',(-1.53724795267438,-2.16746019992005,
13.8727429581918));
#415264=CARTESIAN_POINT('Ctrl Pts',(-1.53249382197548,-2.16936883212836,
13.873936442031));
#415265=CARTESIAN_POINT('Ctrl Pts',(-1.52777945726104,-2.17204563802134,
13.8744652622107));
#415266=CARTESIAN_POINT('Ctrl Pts',(-1.52361833317245,-2.17525888567967,
13.8742206332401));
#415267=CARTESIAN_POINT('Ctrl Pts',(-1.52003658964363,-2.17802473182164,
13.8740100655633));
#415268=CARTESIAN_POINT('Ctrl Pts',(-1.51676736056658,-2.1812587699519,
13.8732246156103));
#415269=CARTESIAN_POINT('Ctrl Pts',(-1.51402656265576,-2.18466999739483,
13.8719820486038));
#415270=CARTESIAN_POINT('Ctrl Pts',(-1.51123853443043,-2.18814000821041,
13.8707180692815));
#415271=CARTESIAN_POINT('Ctrl Pts',(-1.508927323781,-2.19186689613867,13.868960862563));
#415272=CARTESIAN_POINT('Ctrl Pts',(-1.50713291851973,-2.19559133297972,
13.8669057591701));
#415273=CARTESIAN_POINT('Ctrl Pts',(-1.50436994720885,-2.20132610893205,
13.8637413727084));
#415274=CARTESIAN_POINT('Ctrl Pts',(-1.50272294798381,-2.20722133301058,
13.8597962563956));
#415275=CARTESIAN_POINT('Ctrl Pts',(-1.50198720782604,-2.21285642170701,
13.855546950204));
#415276=CARTESIAN_POINT('Ctrl Pts',(-1.50110975337516,-2.21957691073497,
13.850479165618));
#415277=CARTESIAN_POINT('Ctrl Pts',(-1.50148573463251,-2.22611562835888,
13.8448473071436));
#415278=CARTESIAN_POINT('Ctrl Pts',(-1.50280989203645,-2.23217274608225,
13.8390832900376));
#415279=CARTESIAN_POINT('',(-1.51045522294541,-2.26714115831904,13.8057746032556));
#415280=CARTESIAN_POINT('',(-1.50280989203645,-2.23217274608225,13.8390832900376));
#415281=CARTESIAN_POINT('',(-1.43479835951345,-2.31576287210172,13.8057746032556));
#415282=CARTESIAN_POINT('Origin',(0.,2.5406128344257E-15,13.8057746032556));
#415283=CARTESIAN_POINT('',(-1.40616595815507,-2.29428203106785,13.8390832900376));
#415284=CARTESIAN_POINT('',(-1.43479835951345,-2.31576287210172,13.8057746032556));
#415285=CARTESIAN_POINT('',(-1.31586661480734,-2.34723833301828,13.8390832900376));
#415286=CARTESIAN_POINT('Ctrl Pts',(-1.40616595815506,-2.29428203106785,
13.8390832900376));
#415287=CARTESIAN_POINT('Ctrl Pts',(-1.40058950271566,-2.29009861161057,
13.8455641171218));
#415288=CARTESIAN_POINT('Ctrl Pts',(-1.3939433551813,-2.28674214899241,
13.851896480191));
#415289=CARTESIAN_POINT('Ctrl Pts',(-1.38643805846229,-2.28480265096473,
13.8574481026913));
#415290=CARTESIAN_POINT('Ctrl Pts',(-1.38136509738292,-2.28349171038817,
13.8612005412592));
#415291=CARTESIAN_POINT('Ctrl Pts',(-1.37577590967858,-2.28281476403325,
13.8646714234115));
#415292=CARTESIAN_POINT('Ctrl Pts',(-1.36995196378689,-2.28305323550397,
13.8674635290331));
#415293=CARTESIAN_POINT('Ctrl Pts',(-1.36525831436012,-2.28324542504396,
13.8697137499649));
#415294=CARTESIAN_POINT('Ctrl Pts',(-1.36030287936929,-2.28405061841004,
13.8715630732994));
#415295=CARTESIAN_POINT('Ctrl Pts',(-1.35546475891363,-2.28554813416437,
13.8727429581918));
#415296=CARTESIAN_POINT('Ctrl Pts',(-1.35057087594858,-2.28706290976931,
13.873936442031));
#415297=CARTESIAN_POINT('Ctrl Pts',(-1.3456540133633,-2.28934654432125,
13.8744652622107));
#415298=CARTESIAN_POINT('Ctrl Pts',(-1.34124482555735,-2.29220992991985,
13.8742206332401));
#415299=CARTESIAN_POINT('Ctrl Pts',(-1.33744955784721,-2.29467462758807,
13.8740100655632));
#415300=CARTESIAN_POINT('Ctrl Pts',(-1.33392760272927,-2.29763143220342,
13.8732246156103));
#415301=CARTESIAN_POINT('Ctrl Pts',(-1.3309178778925,-2.30080790859438,
13.8719820486038));
#415302=CARTESIAN_POINT('Ctrl Pts',(-1.32785628850562,-2.30403912305207,
13.8707180692815));
#415303=CARTESIAN_POINT('Ctrl Pts',(-1.32524899225408,-2.30756522494404,
13.868960862563));
#415304=CARTESIAN_POINT('Ctrl Pts',(-1.32315698154976,-2.31113100834151,
13.8669057591701));
#415305=CARTESIAN_POINT('Ctrl Pts',(-1.3199357663188,-2.31662149448792,
13.8637413727084));
#415306=CARTESIAN_POINT('Ctrl Pts',(-1.31781373185682,-2.32236285696783,
13.8597962563956));
#415307=CARTESIAN_POINT('Ctrl Pts',(-1.31662112777136,-2.32791922571834,
13.855546950204));
#415308=CARTESIAN_POINT('Ctrl Pts',(-1.31519881073203,-2.33454583218982,
13.850479165618));
#415309=CARTESIAN_POINT('Ctrl Pts',(-1.31504057475392,-2.34109343873316,
13.8448473071436));
#415310=CARTESIAN_POINT('Ctrl Pts',(-1.31586661480734,-2.34723833301828,
13.8390832900376));
#415311=CARTESIAN_POINT('',(-1.3206362562802,-2.38271355619292,13.8057746032556));
#415312=CARTESIAN_POINT('',(-1.31586661480734,-2.34723833301828,13.8390832900376));
#415313=CARTESIAN_POINT('',(-1.2412680137648,-2.42500674850023,13.8057746032556));
#415314=CARTESIAN_POINT('Origin',(0.,2.5406128344257E-15,13.8057746032556));
#415315=CARTESIAN_POINT('',(-1.21448177232259,-2.40126357667191,13.8390832900376));
#415316=CARTESIAN_POINT('',(-1.2412680137648,-2.42500674850023,13.8057746032556));
#415317=CARTESIAN_POINT('',(-1.1201664623594,-2.44668343611514,13.8390832900376));
#415318=CARTESIAN_POINT('Ctrl Pts',(-1.21448177232259,-2.40126357667191,
13.8390832900376));
#415319=CARTESIAN_POINT('Ctrl Pts',(-1.20926485960137,-2.39663954431017,
13.8455641171218));
#415320=CARTESIAN_POINT('Ctrl Pts',(-1.20291440943792,-2.39275252732061,
13.851896480191));
#415321=CARTESIAN_POINT('Ctrl Pts',(-1.19559217306928,-2.39020773145424,
13.8574481026913));
#415322=CARTESIAN_POINT('Ctrl Pts',(-1.19064294567658,-2.38848765950126,
13.8612005412592));
#415323=CARTESIAN_POINT('Ctrl Pts',(-1.18512753294564,-2.3873573949441,
13.8646714234115));
#415324=CARTESIAN_POINT('Ctrl Pts',(-1.17930352811473,-2.38712036726362,
13.8674635290331));
#415325=CARTESIAN_POINT('Ctrl Pts',(-1.17460983118752,-2.38692934130678,
13.8697137499649));
#415326=CARTESIAN_POINT('Ctrl Pts',(-1.16960525426345,-2.38732794150259,
13.8715630732994));
#415327=CARTESIAN_POINT('Ctrl Pts',(-1.16466117081825,-2.38842612266473,
13.8727429581918));
#415328=CARTESIAN_POINT('Ctrl Pts',(-1.15966010357076,-2.38953696108456,
13.873936442031));
#415329=CARTESIAN_POINT('Ctrl Pts',(-1.1545734640239,-2.39141222708429,
13.8744652622107));
#415330=CARTESIAN_POINT('Ctrl Pts',(-1.14994555491799,-2.39390669526444,
13.8742206332401));
#415331=CARTESIAN_POINT('Ctrl Pts',(-1.14596201990697,-2.39605384230257,
13.8740100655633));
#415332=CARTESIAN_POINT('Ctrl Pts',(-1.14221077677835,-2.39871373635613,
13.8732246156103));
#415333=CARTESIAN_POINT('Ctrl Pts',(-1.13895215423787,-2.40163432276882,
13.8719820486038));
#415334=CARTESIAN_POINT('Ctrl Pts',(-1.13563737806167,-2.40460523766952,
13.8707180692815));
#415335=CARTESIAN_POINT('Ctrl Pts',(-1.13275134733439,-2.40790708789886,
13.868960862563));
#415336=CARTESIAN_POINT('Ctrl Pts',(-1.1303756531731,-2.41129048815256,
13.8669057591701));
#415337=CARTESIAN_POINT('Ctrl Pts',(-1.12671763067797,-2.41650014621362,
13.8637413727084));
#415338=CARTESIAN_POINT('Ctrl Pts',(-1.12413468276829,-2.42204943927485,
13.8597962563956));
#415339=CARTESIAN_POINT('Ctrl Pts',(-1.12249315133856,-2.42749011136215,
13.855546950204));
#415340=CARTESIAN_POINT('Ctrl Pts',(-1.12053543699601,-2.43397873630441,
13.850479165618));
#415341=CARTESIAN_POINT('Ctrl Pts',(-1.11984403681677,-2.4404916585259,
13.8448473071436));
#415342=CARTESIAN_POINT('Ctrl Pts',(-1.1201664623594,-2.44668343611514,
13.8390832900376));
#415343=CARTESIAN_POINT('',(-1.12202867321909,-2.48242938847039,13.8057746032556));
#415344=CARTESIAN_POINT('',(-1.1201664623594,-2.44668343611514,13.8390832900376));
#415345=CARTESIAN_POINT('',(-1.03947723417935,-2.51811260508543,13.8057746032556));
#415346=CARTESIAN_POINT('Origin',(0.,2.5406128344257E-15,13.8057746032556));
#415347=CARTESIAN_POINT('',(-1.01471541067069,-2.49226510935382,13.8390832900376));
#415348=CARTESIAN_POINT('',(-1.03947723417935,-2.51811260508543,13.8057746032556));
#415349=CARTESIAN_POINT('',(-0.917011786918914,-2.52984626461901,13.8390832900376));
#415350=CARTESIAN_POINT('Ctrl Pts',(-1.01471541067069,-2.49226510935381,
13.8390832900376));
#415351=CARTESIAN_POINT('Ctrl Pts',(-1.0098927583611,-2.48723123626007,
13.8455641171218));
#415352=CARTESIAN_POINT('Ctrl Pts',(-1.00388026676664,-2.48283953235586,
13.851896480191));
#415353=CARTESIAN_POINT('Ctrl Pts',(-0.996789819023321,-2.47970637384743,
13.8574481026913));
#415354=CARTESIAN_POINT('Ctrl Pts',(-0.991997261609015,-2.4775886173131,
13.8612005412592));
#415355=CARTESIAN_POINT('Ctrl Pts',(-0.986592328013226,-2.47601255627784,
13.8646714234115));
#415356=CARTESIAN_POINT('Ctrl Pts',(-0.980807022034365,-2.47530160682628,
13.8674635290331));
#415357=CARTESIAN_POINT('Ctrl Pts',(-0.976144513385357,-2.47472863661882,
13.8697137499649));
#415358=CARTESIAN_POINT('Ctrl Pts',(-0.971124099161771,-2.47471799102583,
13.8715630732994));
#415359=CARTESIAN_POINT('Ctrl Pts',(-0.966106954786642,-2.47540952938133,
13.8727429581918));
#415360=CARTESIAN_POINT('Ctrl Pts',(-0.961031984534124,-2.47610903816964,
13.873936442031));
#415361=CARTESIAN_POINT('Ctrl Pts',(-0.955809418772643,-2.47756345603133,
13.8744652622107));
#415362=CARTESIAN_POINT('Ctrl Pts',(-0.95099358633831,-2.47967240651884,
13.8742206332401));
#415363=CARTESIAN_POINT('Ctrl Pts',(-0.946848293794672,-2.4814877140176,
13.8740100655632));
#415364=CARTESIAN_POINT('Ctrl Pts',(-0.942892726559494,-2.4838329963533,
13.8732246156103));
#415365=CARTESIAN_POINT('Ctrl Pts',(-0.939406891910658,-2.48647825676701,
13.8719820486038));
#415366=CARTESIAN_POINT('Ctrl Pts',(-0.935860988233707,-2.48916910116222,
13.8707180692815));
#415367=CARTESIAN_POINT('Ctrl Pts',(-0.932715429089015,-2.49222472646043,
13.868960862563));
#415368=CARTESIAN_POINT('Ctrl Pts',(-0.930071861323431,-2.49540322759987,
13.8669057591701));
#415369=CARTESIAN_POINT('Ctrl Pts',(-0.926001375100309,-2.50029738816073,
13.8637413727084));
#415370=CARTESIAN_POINT('Ctrl Pts',(-0.922974702835103,-2.50561768217352,
13.8597962563956));
#415371=CARTESIAN_POINT('Ctrl Pts',(-0.920895168181939,-2.51090645082252,
13.855546950204));
#415372=CARTESIAN_POINT('Ctrl Pts',(-0.918415084802115,-2.5172139135071,
13.850479165618));
#415373=CARTESIAN_POINT('Ctrl Pts',(-0.917195121575857,-2.52364880898393,
13.8448473071436));
#415374=CARTESIAN_POINT('Ctrl Pts',(-0.917011786918912,-2.52984626461901,
13.8390832900376));
#415375=CARTESIAN_POINT('',(-0.915954174459406,-2.56562506273962,13.8057746032556));
#415376=CARTESIAN_POINT('',(-0.917011786918914,-2.52984626461901,13.8390832900376));
#415377=CARTESIAN_POINT('',(-0.830768905102112,-2.59446083774312,13.8057746032556));
#415378=CARTESIAN_POINT('Origin',(0.,2.5406128344257E-15,13.8057746032556));
#415379=CARTESIAN_POINT('',(-0.808196285377042,-2.56668102892777,13.8390832900376));
#415380=CARTESIAN_POINT('',(-0.830768905102112,-2.59446083774312,13.8057746032556));
#415381=CARTESIAN_POINT('',(-0.707754549332778,-2.59617338362709,13.8390832900376));
#415382=CARTESIAN_POINT('Ctrl Pts',(-0.808196285377041,-2.56668102892777,
13.8390832900376));
#415383=CARTESIAN_POINT('Ctrl Pts',(-0.803799987434504,-2.56127081469693,
13.8455641171218));
#415384=CARTESIAN_POINT('Ctrl Pts',(-0.798165466548616,-2.55640364994298,
13.851896480191));
#415385=CARTESIAN_POINT('Ctrl Pts',(-0.791353993190503,-2.55270297944543,
13.8574481026913));
#415386=CARTESIAN_POINT('Ctrl Pts',(-0.786749999433474,-2.55020163165006,
13.8612005412592));
#415387=CARTESIAN_POINT('Ctrl Pts',(-0.781491513914159,-2.54819026256287,
13.8646714234115));
#415388=CARTESIAN_POINT('Ctrl Pts',(-0.775783407044123,-2.54701012259152,
13.8674635290331));
#415389=CARTESIAN_POINT('Ctrl Pts',(-0.77118311489912,-2.54605902115565,
13.8697137499649));
#415390=CARTESIAN_POINT('Ctrl Pts',(-0.766180273404364,-2.54563920061852,
13.8715630732994));
#415391=CARTESIAN_POINT('Ctrl Pts',(-0.761123456367358,-2.54591949409372,
13.8727429581918));
#415392=CARTESIAN_POINT('Ctrl Pts',(-0.756008356199529,-2.54620301813494,
13.873936442031));
#415393=CARTESIAN_POINT('Ctrl Pts',(-0.750684619536904,-2.54722690894767,
13.8744652622107));
#415394=CARTESIAN_POINT('Ctrl Pts',(-0.745712912344444,-2.54893630702501,
13.8742206332401));
#415395=CARTESIAN_POINT('Ctrl Pts',(-0.741433448506141,-2.55040769441249,
13.8740100655632));
#415396=CARTESIAN_POINT('Ctrl Pts',(-0.737299880811726,-2.55242275756334,
13.8732246156103));
#415397=CARTESIAN_POINT('Ctrl Pts',(-0.733610031709007,-2.55477508820644,
13.8719820486038));
#415398=CARTESIAN_POINT('Ctrl Pts',(-0.729856597935234,-2.55716795497067,
13.8707180692815));
#415399=CARTESIAN_POINT('Ctrl Pts',(-0.726472443550261,-2.55995702065554,
13.868960862563));
#415400=CARTESIAN_POINT('Ctrl Pts',(-0.723578594687708,-2.56290947028007,
13.8669057591701));
#415401=CARTESIAN_POINT('Ctrl Pts',(-0.71912273315082,-2.56745556350967,
13.8637413727084));
#415402=CARTESIAN_POINT('Ctrl Pts',(-0.715672478534653,-2.57251145279515,
13.8597962563956));
#415403=CARTESIAN_POINT('Ctrl Pts',(-0.713168779618072,-2.57761312212307,
13.855546950204));
#415404=CARTESIAN_POINT('Ctrl Pts',(-0.710182831746682,-2.58369744742648,
13.850479165618));
#415405=CARTESIAN_POINT('Ctrl Pts',(-0.708442424127407,-2.59001149299092,
13.8448473071436));
#415406=CARTESIAN_POINT('Ctrl Pts',(-0.707754549332779,-2.59617338362709,
13.8390832900376));
#415407=CARTESIAN_POINT('',(-0.703784151790496,-2.63174692551465,13.8057746032556));
#415408=CARTESIAN_POINT('',(-0.707754549332778,-2.59617338362709,13.8390832900376));
#415409=CARTESIAN_POINT('',(-0.61653194602864,-2.65354336158153,13.8057746032556));
#415410=CARTESIAN_POINT('Origin',(0.,2.5406128344257E-15,13.8057746032556));
#415411=CARTESIAN_POINT('',(-0.596298747147209,-2.62401610972678,13.8390832900376));
#415412=CARTESIAN_POINT('',(-0.61653194602864,-2.65354336158153,13.8057746032556));
#415413=CARTESIAN_POINT('',(-0.493787321992115,-2.64522339710559,13.8390832900376));
#415414=CARTESIAN_POINT('Ctrl Pts',(-0.596298747147209,-2.62401610972677,
13.8390832900376));
#415415=CARTESIAN_POINT('Ctrl Pts',(-0.592358060209198,-2.61826555844192,
13.8455641171218));
#415416=CARTESIAN_POINT('Ctrl Pts',(-0.587139006838742,-2.61295532301663,
13.851896480191));
#415417=CARTESIAN_POINT('Ctrl Pts',(-0.58065183709722,-2.60871176788156,
13.8574481026913));
#415418=CARTESIAN_POINT('Ctrl Pts',(-0.576267045816317,-2.60584347488205,
13.8612005412592));
#415419=CARTESIAN_POINT('Ctrl Pts',(-0.571190002727019,-2.60341018307235,
13.8646714234115));
#415420=CARTESIAN_POINT('Ctrl Pts',(-0.565597081475258,-2.60176870621801,
13.8674635290331));
#415421=CARTESIAN_POINT('Ctrl Pts',(-0.561089620019488,-2.60044580297686,
13.8697137499649));
#415422=CARTESIAN_POINT('Ctrl Pts',(-0.5561376443383,-2.599619601332,13.8715630732994));
#415423=CARTESIAN_POINT('Ctrl Pts',(-0.55107480692248,-2.59948678462006,
13.8727429581918));
#415424=CARTESIAN_POINT('Ctrl Pts',(-0.545953616987025,-2.59935243710847,
13.873936442031));
#415425=CARTESIAN_POINT('Ctrl Pts',(-0.540564138012391,-2.59993898704783,
13.8744652622107));
#415426=CARTESIAN_POINT('Ctrl Pts',(-0.535469641952897,-2.60123745695282,
13.8742206332401));
#415427=CARTESIAN_POINT('Ctrl Pts',(-0.531084485945711,-2.60235513238873,
13.8740100655632));
#415428=CARTESIAN_POINT('Ctrl Pts',(-0.526800426003079,-2.6040265664419,
13.8732246156103));
#415429=CARTESIAN_POINT('Ctrl Pts',(-0.522931117783473,-2.60607031294209,
13.8719820486038));
#415430=CARTESIAN_POINT('Ctrl Pts',(-0.518995132395369,-2.60814927794181,
13.8707180692815));
#415431=CARTESIAN_POINT('Ctrl Pts',(-0.5153949037592,-2.61065322324136,
13.868960862563));
#415432=CARTESIAN_POINT('Ctrl Pts',(-0.512270031886407,-2.61335997328585,
13.8669057591701));
#415433=CARTESIAN_POINT('Ctrl Pts',(-0.50745844805912,-2.61752774568379,
13.8637413727084));
#415434=CARTESIAN_POINT('Ctrl Pts',(-0.503607571967207,-2.62228558413294,
13.8597962563956));
#415435=CARTESIAN_POINT('Ctrl Pts',(-0.500696370490418,-2.62716620337213,
13.855546950204));
#415436=CARTESIAN_POINT('Ctrl Pts',(-0.497224429117898,-2.6329869011133,
13.850479165618));
#415437=CARTESIAN_POINT('Ctrl Pts',(-0.494975159231157,-2.63913807783387,
13.8448473071436));
#415438=CARTESIAN_POINT('Ctrl Pts',(-0.493787321992114,-2.64522339710559,
13.8390832900376));
#415439=CARTESIAN_POINT('',(-0.486930561707634,-2.68035494670806,13.8057746032556));
#415440=CARTESIAN_POINT('',(-0.493787321992115,-2.64522339710559,13.8390832900376));
#415441=CARTESIAN_POINT('',(-0.398192068574959,-2.69496699215246,13.8057746032556));
#415442=CARTESIAN_POINT('Origin',(0.,2.5406128344257E-15,13.8057746032556));
#415443=CARTESIAN_POINT('',(-0.380432939137479,-2.66388879624773,13.8390832900376));
#415444=CARTESIAN_POINT('',(-0.398192068574959,-2.69496699215246,13.8057746032556));
#415445=CARTESIAN_POINT('',(-0.276534021492768,-2.67666988530749,13.8390832900376));
#415446=CARTESIAN_POINT('Ctrl Pts',(-0.380432939137479,-2.66388879624773,
13.8390832900376));
#415447=CARTESIAN_POINT('Ctrl Pts',(-0.376974087825399,-2.65783617687889,
13.8455641171218));
#415448=CARTESIAN_POINT('Ctrl Pts',(-0.372205233909475,-2.6521182095229,
13.851896480191));
#415449=CARTESIAN_POINT('Ctrl Pts',(-0.366085538828865,-2.64736000990959,
13.8574481026913));
#415450=CARTESIAN_POINT('Ctrl Pts',(-0.361949130086624,-2.6441438597226,
13.8612005412592));
#415451=CARTESIAN_POINT('Ctrl Pts',(-0.357087316311448,-2.64130483834592,
13.8646714234115));
#415452=CARTESIAN_POINT('Ctrl Pts',(-0.351646800646126,-2.63921294836624,
13.8674635290331));
#415453=CARTESIAN_POINT('Ctrl Pts',(-0.347262166291898,-2.63752704702261,
13.8697137499649));
#415454=CARTESIAN_POINT('Ctrl Pts',(-0.342394011005417,-2.63629996250565,
13.8715630732994));
#415455=CARTESIAN_POINT('Ctrl Pts',(-0.337358845558476,-2.63575491947989,
13.8727429581918));
#415456=CARTESIAN_POINT('Ctrl Pts',(-0.332265646529479,-2.63520359447602,
13.873936442031));
#415457=CARTESIAN_POINT('Ctrl Pts',(-0.326846291336212,-2.63534890014893,
13.8744652622107));
#415458=CARTESIAN_POINT('Ctrl Pts',(-0.321662909440426,-2.63622780077858,
13.8742206332401));
#415459=CARTESIAN_POINT('Ctrl Pts',(-0.317201243754086,-2.63698432631728,
13.8740100655632));
#415460=CARTESIAN_POINT('Ctrl Pts',(-0.312795201275329,-2.63830100815493,
13.8732246156103));
#415461=CARTESIAN_POINT('Ctrl Pts',(-0.308772183546646,-2.64002256971644,
13.8719820486038));
#415462=CARTESIAN_POINT('Ctrl Pts',(-0.304679839877579,-2.64177379778259,
13.8707180692815));
#415463=CARTESIAN_POINT('Ctrl Pts',(-0.300887495917791,-2.64397595935398,
13.868960862563));
#415464=CARTESIAN_POINT('Ctrl Pts',(-0.297552396541504,-2.64641899684345,
13.8669057591701));
#415465=CARTESIAN_POINT('Ctrl Pts',(-0.292417110720329,-2.65018071257207,
13.8637413727084));
#415466=CARTESIAN_POINT('Ctrl Pts',(-0.288191240097716,-2.654608837555,
13.8597962563956));
#415467=CARTESIAN_POINT('Ctrl Pts',(-0.284891909626231,-2.65923592698965,
13.855546950204));
#415468=CARTESIAN_POINT('Ctrl Pts',(-0.280957079949588,-2.66475426138547,
13.850479165618));
#415469=CARTESIAN_POINT('Ctrl Pts',(-0.278213916315381,-2.67070163419597,
13.8448473071436));
#415470=CARTESIAN_POINT('Ctrl Pts',(-0.276534021492769,-2.67666988530749,
13.8390832900376));
#415471=CARTESIAN_POINT('',(-0.266836529074495,-2.71112564795857,13.8057746032556));
#415472=CARTESIAN_POINT('',(-0.276534021492768,-2.67666988530749,13.8390832900376));
#415473=CARTESIAN_POINT('',(-0.177202288601978,-2.71845606202887,13.8057746032556));
#415474=CARTESIAN_POINT('Origin',(0.,2.5406128344257E-15,13.8057746032556));
#415475=CARTESIAN_POINT('',(-0.162035412684806,-2.68603374234038,13.8390832900376));
#415476=CARTESIAN_POINT('',(-0.177202288601978,-2.71845606202887,13.8057746032556));
#415477=CARTESIAN_POINT('',(-0.057440432705288,-2.69030357704212,13.8390832900376));
#415478=CARTESIAN_POINT('Ctrl Pts',(-0.162035412684806,-2.68603374234037,
13.8390832900376));
#415479=CARTESIAN_POINT('Ctrl Pts',(-0.15908141508347,-2.67971933407083,
13.8455641171218));
#415480=CARTESIAN_POINT('Ctrl Pts',(-0.15479449655808,-2.67363168691349,
13.851896480191));
#415481=CARTESIAN_POINT('Ctrl Pts',(-0.149083001699466,-2.66839050785533,
13.8574481026913));
#415482=CARTESIAN_POINT('Ctrl Pts',(-0.145222502613606,-2.66484790342974,
13.8612005412592));
#415483=CARTESIAN_POINT('Ctrl Pts',(-0.140608272721084,-2.66162204570493,
13.8646714234115));
#415484=CARTESIAN_POINT('Ctrl Pts',(-0.13535636837633,-2.65909366378258,
13.8674635290331));
#415485=CARTESIAN_POINT('Ctrl Pts',(-0.131123740141859,-2.65705598373177,
13.8697137499649));
#415486=CARTESIAN_POINT('Ctrl Pts',(-0.126371802020328,-2.65543618238771,
13.8715630732994));
#415487=CARTESIAN_POINT('Ctrl Pts',(-0.121397816737571,-2.65448254021954,
13.8727429581918));
#415488=CARTESIAN_POINT('Ctrl Pts',(-0.116366503014253,-2.65351790670031,
13.873936442031));
#415489=CARTESIAN_POINT('Ctrl Pts',(-0.110953336517032,-2.65322100112149,
13.8744652622107));
#415490=CARTESIAN_POINT('Ctrl Pts',(-0.105715563336274,-2.65367448353713,
13.8742206332401));
#415491=CARTESIAN_POINT('Ctrl Pts',(-0.101207079619797,-2.65406482462599,
13.8740100655632));
#415492=CARTESIAN_POINT('Ctrl Pts',(-0.0967083760906725,-2.65501799194772,
13.8732246156103));
#415493=CARTESIAN_POINT('Ctrl Pts',(-0.0925584213721455,-2.65640591186238,
13.8719820486038));
#415494=CARTESIAN_POINT('Ctrl Pts',(-0.0883369532940422,-2.65781774886112,
13.8707180692815));
#415495=CARTESIAN_POINT('Ctrl Pts',(-0.0843777314339956,-2.65970347168242,
13.868960862563));
#415496=CARTESIAN_POINT('Ctrl Pts',(-0.0808545990903116,-2.66186653860547,
13.8669057591701));
#415497=CARTESIAN_POINT('Ctrl Pts',(-0.0754297857551275,-2.66519716406723,
13.8637413727084));
#415498=CARTESIAN_POINT('Ctrl Pts',(-0.070857043073586,-2.66926610714275,
13.8597962563956));
#415499=CARTESIAN_POINT('Ctrl Pts',(-0.0671915401073441,-2.67360887425611,
13.855546950204));
#415500=CARTESIAN_POINT('Ctrl Pts',(-0.0628200077688717,-2.67878812170163,
13.850479165618));
#415501=CARTESIAN_POINT('Ctrl Pts',(-0.059601205688587,-2.68449211181725,
13.8448473071436));
#415502=CARTESIAN_POINT('Ctrl Pts',(-0.0574404327052869,-2.69030357704211,
13.8390832900376));
#415503=CARTESIAN_POINT('',(-0.0449667433652931,-2.72385425532615,13.8057746032556));
#415504=CARTESIAN_POINT('',(-0.057440432705288,-2.69030357704212,13.8390832900376));
#415505=CARTESIAN_POINT('',(-3.33621391227898E-16,-2.72422539674441,13.8057746032556));
#415506=CARTESIAN_POINT('Origin',(0.,2.5406128344257E-15,13.8057746032556));
#415507=CARTESIAN_POINT('',(-3.12992118721904E-16,-2.55577460325558,13.9742253967444));
#415508=CARTESIAN_POINT('',(-3.33621391227897E-16,-2.72422539674441,13.8057746032556));
#415509=CARTESIAN_POINT('',(3.12992118721905E-16,2.55577460325559,13.9742253967444));
#415510=CARTESIAN_POINT('Origin',(0.,2.5406128344257E-15,13.9742253967444));
#415511=CARTESIAN_POINT('Origin',(0.,2.5406128344257E-15,13.9742253967444));
#415512=CARTESIAN_POINT('',(0.04496674336533,-2.72385425532615,13.8057746032556));
#415513=CARTESIAN_POINT('Origin',(0.,2.5406128344257E-15,13.8057746032556));
#415514=CARTESIAN_POINT('',(0.0574404327053243,-2.69030357704212,13.8390832900376));
#415515=CARTESIAN_POINT('',(0.04496674336533,-2.72385425532615,13.8057746032556));
#415516=CARTESIAN_POINT('',(0.162035412684842,-2.68603374234037,13.8390832900376));
#415517=CARTESIAN_POINT('Ctrl Pts',(0.057440432705324,-2.69030357704211,
13.8390832900376));
#415518=CARTESIAN_POINT('Ctrl Pts',(0.0598699182292554,-2.6837694012171,
13.8455641171218));
#415519=CARTESIAN_POINT('Ctrl Pts',(0.0636463726286157,-2.67735258654585,
13.851896480191));
#415520=CARTESIAN_POINT('Ctrl Pts',(0.0689116582092796,-2.67166330722473,
13.8574481026913));
#415521=CARTESIAN_POINT('Ctrl Pts',(0.0724705566542799,-2.6678178240085,
13.8612005412592));
#415522=CARTESIAN_POINT('Ctrl Pts',(0.0768064957255092,-2.66422659748649,
13.8646714234115));
#415523=CARTESIAN_POINT('Ctrl Pts',(0.0818348381927834,-2.66127854958601,
13.8674635290331));
#415524=CARTESIAN_POINT('Ctrl Pts',(0.0858872928649317,-2.65890265125256,
13.8697137499649));
#415525=CARTESIAN_POINT('Ctrl Pts',(0.0904913904573281,-2.65690091259211,
13.8715630732994));
#415526=CARTESIAN_POINT('Ctrl Pts',(0.0953710945244929,-2.65554501761281,
13.8727429581918));
#415527=CARTESIAN_POINT('Ctrl Pts',(0.100307040379415,-2.65417349505516,
13.873936442031));
#415528=CARTESIAN_POINT('Ctrl Pts',(0.105677994450658,-2.65343635408224,
13.8744652622107));
#415529=CARTESIAN_POINT('Ctrl Pts',(0.110935302400043,-2.65346140043321,
13.8742206332401));
#415530=CARTESIAN_POINT('Ctrl Pts',(0.115460600931368,-2.65348295941668,
13.8740100655632));
#415531=CARTESIAN_POINT('Ctrl Pts',(0.120022027381112,-2.65406626905123,
13.8732246156103));
#415532=CARTESIAN_POINT('Ctrl Pts',(0.124271301825525,-2.65511131094102,
13.8719820486038));
#415533=CARTESIAN_POINT('Ctrl Pts',(0.128593801139098,-2.65617436133005,
13.8707180692815));
#415534=CARTESIAN_POINT('Ctrl Pts',(0.132693552931151,-2.657731096227,13.868960862563));
#415535=CARTESIAN_POINT('Ctrl Pts',(0.136381272377762,-2.65959979773012,
13.8669057591701));
#415536=CARTESIAN_POINT('Ctrl Pts',(0.14205951198924,-2.66247716816209,
13.8637413727084));
#415537=CARTESIAN_POINT('Ctrl Pts',(0.146948695881612,-2.66615985118538,
13.8597962563956));
#415538=CARTESIAN_POINT('Ctrl Pts',(0.150955978025139,-2.6701893955788,
13.855546950204));
#415539=CARTESIAN_POINT('Ctrl Pts',(0.155735121198977,-2.67499508903679,
13.850479165618));
#415540=CARTESIAN_POINT('Ctrl Pts',(0.159408141128555,-2.68041773734441,
13.8448473071436));
#415541=CARTESIAN_POINT('Ctrl Pts',(0.162035412684842,-2.68603374234037,
13.8390832900376));
#415542=CARTESIAN_POINT('',(0.177202288602015,-2.71845606202886,13.8057746032556));
#415543=CARTESIAN_POINT('',(0.162035412684842,-2.68603374234037,13.8390832900376));
#415544=CARTESIAN_POINT('',(0.266836529074531,-2.71112564795856,13.8057746032556));
#415545=CARTESIAN_POINT('Origin',(0.,2.5406128344257E-15,13.8057746032556));
#415546=CARTESIAN_POINT('',(0.276534021492804,-2.67666988530749,13.8390832900376));
#415547=CARTESIAN_POINT('',(0.266836529074531,-2.71112564795856,13.8057746032556));
#415548=CARTESIAN_POINT('',(0.380432939137515,-2.66388879624773,13.8390832900376));
#415549=CARTESIAN_POINT('Ctrl Pts',(0.276534021492803,-2.67666988530748,
13.8390832900376));
#415550=CARTESIAN_POINT('Ctrl Pts',(0.278422827114005,-2.66995942578906,
13.8455641171218));
#415551=CARTESIAN_POINT('Ctrl Pts',(0.281663685706382,-2.66325614644683,
13.851896480191));
#415552=CARTESIAN_POINT('Ctrl Pts',(0.286447722402268,-2.65715662807797,
13.8574481026913));
#415553=CARTESIAN_POINT('Ctrl Pts',(0.289681336324433,-2.65303385712744,
13.8612005412592));
#415554=CARTESIAN_POINT('Ctrl Pts',(0.293710129615224,-2.64910116082823,
13.8646714234115));
#415555=CARTESIAN_POINT('Ctrl Pts',(0.298481447415517,-2.64575306572201,
13.8674635290331));
#415556=CARTESIAN_POINT('Ctrl Pts',(0.302326760108108,-2.64305476031733,
13.8697137499649));
#415557=CARTESIAN_POINT('Ctrl Pts',(0.306752377661515,-2.640684405581,13.8715630732994));
#415558=CARTESIAN_POINT('Ctrl Pts',(0.311505326887615,-2.63893528104795,
13.8727429581918));
#415559=CARTESIAN_POINT('Ctrl Pts',(0.316313056968849,-2.63716599670821,
13.873936442031));
#415560=CARTESIAN_POINT('Ctrl Pts',(0.321606055800918,-2.63599352589276,
13.8744652622107));
#415561=CARTESIAN_POINT('Ctrl Pts',(0.326847912001921,-2.63558996949972,
13.8742206332401));
#415562=CARTESIAN_POINT('Ctrl Pts',(0.331359910232991,-2.63524260290633,
13.8740100655632));
#415563=CARTESIAN_POINT('Ctrl Pts',(0.335953704062915,-2.63545217302432,
13.8732246156103));
#415564=CARTESIAN_POINT('Ctrl Pts',(0.340274020012868,-2.63614738230787,
13.8719820486038));
#415565=CARTESIAN_POINT('Ctrl Pts',(0.34466878504214,-2.63685457166224,
13.8707180692815));
#415566=CARTESIAN_POINT('Ctrl Pts',(0.348881783594433,-2.63807195882096,
13.868960862563));
#415567=CARTESIAN_POINT('Ctrl Pts',(0.352709548979483,-2.63963385900397,
13.8669057591701));
#415568=CARTESIAN_POINT('Ctrl Pts',(0.358603427119485,-2.64203882598065,
13.8637413727084));
#415569=CARTESIAN_POINT('Ctrl Pts',(0.363776515510545,-2.64531074130378,
13.8597962563956));
#415570=CARTESIAN_POINT('Ctrl Pts',(0.368098909029846,-2.64900024702416,
13.855546950204));
#415571=CARTESIAN_POINT('Ctrl Pts',(0.373253858629733,-2.65340040539754,
13.850479165618));
#415572=CARTESIAN_POINT('Ctrl Pts',(0.377356653066979,-2.65850562506734,
13.8448473071436));
#415573=CARTESIAN_POINT('Ctrl Pts',(0.380432939137514,-2.66388879624772,
13.8390832900376));
#415574=CARTESIAN_POINT('',(0.398192068574995,-2.69496699215245,13.8057746032556));
#415575=CARTESIAN_POINT('',(0.380432939137515,-2.66388879624773,13.8390832900376));
#415576=CARTESIAN_POINT('',(0.48693056170767,-2.68035494670805,13.8057746032556));
#415577=CARTESIAN_POINT('Origin',(0.,2.5406128344257E-15,13.8057746032556));
#415578=CARTESIAN_POINT('',(0.493787321992151,-2.64522339710558,13.8390832900376));
#415579=CARTESIAN_POINT('',(0.48693056170767,-2.68035494670805,13.8057746032556));
#415580=CARTESIAN_POINT('',(0.596298747147245,-2.62401610972677,13.8390832900376));
#415581=CARTESIAN_POINT('Ctrl Pts',(0.49378732199215,-2.64522339710558,
13.8390832900376));
#415582=CARTESIAN_POINT('Ctrl Pts',(0.495122878020844,-2.63838131089468,
13.8455641171218));
#415583=CARTESIAN_POINT('Ctrl Pts',(0.497806573427004,-2.63143617609955,
13.851896480191));
#415584=CARTESIAN_POINT('Ctrl Pts',(0.502077524263211,-2.62496700997134,
13.8574481026913));
#415585=CARTESIAN_POINT('Ctrl Pts',(0.504964334495399,-2.62059438764698,
13.8612005412592));
#415586=CARTESIAN_POINT('Ctrl Pts',(0.508659171051115,-2.61634639301559,
13.8646714234115));
#415587=CARTESIAN_POINT('Ctrl Pts',(0.513141711851679,-2.61262053172415,
13.8674635290331));
#415588=CARTESIAN_POINT('Ctrl Pts',(0.516754292643173,-2.60961777602553,
13.8697137499649));
#415589=CARTESIAN_POINT('Ctrl Pts',(0.520971978402944,-2.60689457953301,
13.8715630732994));
#415590=CARTESIAN_POINT('Ctrl Pts',(0.525566542695062,-2.6047638655814,
13.8727429581918));
#415591=CARTESIAN_POINT('Ctrl Pts',(0.530214062352137,-2.60260859375493,
13.873936442031));
#415592=CARTESIAN_POINT('Ctrl Pts',(0.535393881911091,-2.60100859569678,
13.8744652622107));
#415593=CARTESIAN_POINT('Ctrl Pts',(0.540585402675539,-2.60017912216095,
13.8742206332401));
#415594=CARTESIAN_POINT('Ctrl Pts',(0.545054074002554,-2.59946514165806,
13.8740100655632));
#415595=CARTESIAN_POINT('Ctrl Pts',(0.549649664272639,-2.59929957760493,
13.8732246156103));
#415596=CARTESIAN_POINT('Ctrl Pts',(0.554012270738286,-2.59964032777916,
13.8719820486038));
#415597=CARTESIAN_POINT('Ctrl Pts',(0.558450055047073,-2.5999869498704,
13.8707180692815));
#415598=CARTESIAN_POINT('Ctrl Pts',(0.562748263549338,-2.60085688778019,
13.868960862563));
#415599=CARTESIAN_POINT('Ctrl Pts',(0.566690601725727,-2.60210159245507,
13.8669057591701));
#415600=CARTESIAN_POINT('Ctrl Pts',(0.572760895607653,-2.60401815131803,
13.8637413727084));
#415601=CARTESIAN_POINT('Ctrl Pts',(0.578183462447657,-2.60685752488436,
13.8597962563956));
#415602=CARTESIAN_POINT('Ctrl Pts',(0.582792202527004,-2.61018243887984,
13.855546950204));
#415603=CARTESIAN_POINT('Ctrl Pts',(0.588288653213859,-2.61414777984062,
13.850479165618));
#415604=CARTESIAN_POINT('Ctrl Pts',(0.592793918738707,-2.61890159647799,
13.8448473071436));
#415605=CARTESIAN_POINT('Ctrl Pts',(0.596298747147244,-2.62401610972677,
13.8390832900376));
#415606=CARTESIAN_POINT('',(0.616531946028676,-2.65354336158152,13.8057746032556));
#415607=CARTESIAN_POINT('',(0.596298747147245,-2.62401610972677,13.8390832900376));
#415608=CARTESIAN_POINT('',(0.703784151790532,-2.63174692551464,13.8057746032556));
#415609=CARTESIAN_POINT('Origin',(0.,2.5406128344257E-15,13.8057746032556));
#415610=CARTESIAN_POINT('',(0.707754549332813,-2.59617338362708,13.8390832900376));
#415611=CARTESIAN_POINT('',(0.703784151790532,-2.63174692551464,13.8057746032556));
#415612=CARTESIAN_POINT('',(0.808196285377077,-2.56668102892776,13.8390832900376));
#415613=CARTESIAN_POINT('Ctrl Pts',(0.707754549332813,-2.59617338362708,
13.8390832900376));
#415614=CARTESIAN_POINT('Ctrl Pts',(0.70852796786398,-2.58924520367858,
13.8455641171218));
#415615=CARTESIAN_POINT('Ctrl Pts',(0.710636640533773,-2.58210443215673,
13.851896480191));
#415616=CARTESIAN_POINT('Ctrl Pts',(0.714366083037144,-2.57530866950241,
13.8574481026913));
#415617=CARTESIAN_POINT('Ctrl Pts',(0.716886878333549,-2.57071529488436,
13.8612005412592));
#415618=CARTESIAN_POINT('Ctrl Pts',(0.720223169626513,-2.5661802716242,
13.8646714234115));
#415619=CARTESIAN_POINT('Ctrl Pts',(0.724387102857885,-2.56210143913972,
13.8674635290331));
#415620=CARTESIAN_POINT('Ctrl Pts',(0.727742910619151,-2.5588142159909,
13.8697137499649));
#415621=CARTESIAN_POINT('Ctrl Pts',(0.731724596582433,-2.55575630016556,
13.8715630732994));
#415622=CARTESIAN_POINT('Ctrl Pts',(0.736130199873256,-2.55325817634519,
13.8727429581918));
#415623=CARTESIAN_POINT('Ctrl Pts',(0.740586580629639,-2.55073126001041,
13.873936442031));
#415624=CARTESIAN_POINT('Ctrl Pts',(0.745618750070919,-2.54871438243265,
13.8744652622107));
#415625=CARTESIAN_POINT('Ctrl Pts',(0.750725386684666,-2.54746451176355,
13.8742206332401));
#415626=CARTESIAN_POINT('Ctrl Pts',(0.755120992837223,-2.54638866877362,
13.8740100655633));
#415627=CARTESIAN_POINT('Ctrl Pts',(0.75968779665244,-2.54584907235083,
13.8732246156103));
#415628=CARTESIAN_POINT('Ctrl Pts',(0.764063661207532,-2.54583309577955,
13.8719820486038));
#415629=CARTESIAN_POINT('Ctrl Pts',(0.768514932073442,-2.54581684389483,
13.8707180692815));
#415630=CARTESIAN_POINT('Ctrl Pts',(0.77286974665725,-2.54633354326244,
13.868960862563));
#415631=CARTESIAN_POINT('Ctrl Pts',(0.776900422014854,-2.54725276912493,
13.8669057591701));
#415632=CARTESIAN_POINT('Ctrl Pts',(0.783106734834446,-2.54866816549114,
13.8637413727084));
#415633=CARTESIAN_POINT('Ctrl Pts',(0.788742693835735,-2.55105610173805,
13.8597962563956));
#415634=CARTESIAN_POINT('Ctrl Pts',(0.79360711007029,-2.55399429725457,
13.855546950204));
#415635=CARTESIAN_POINT('Ctrl Pts',(0.799408483871643,-2.55749843211288,
13.850479165618));
#415636=CARTESIAN_POINT('Ctrl Pts',(0.804286238685342,-2.56186920985244,
13.8448473071436));
#415637=CARTESIAN_POINT('Ctrl Pts',(0.808196285377076,-2.56668102892776,
13.8390832900376));
#415638=CARTESIAN_POINT('',(0.830768905102147,-2.5944608377431,13.8057746032556));
#415639=CARTESIAN_POINT('',(0.808196285377077,-2.56668102892776,13.8390832900376));
#415640=CARTESIAN_POINT('',(0.915954174459439,-2.5656250627396,13.8057746032556));
#415641=CARTESIAN_POINT('Origin',(0.,2.5406128344257E-15,13.8057746032556));
#415642=CARTESIAN_POINT('',(0.917011786918948,-2.529846264619,13.8390832900376));
#415643=CARTESIAN_POINT('',(0.915954174459439,-2.5656250627396,13.8057746032556));
#415644=CARTESIAN_POINT('',(1.01471541067073,-2.4922651093538,13.8390832900376));
#415645=CARTESIAN_POINT('Ctrl Pts',(0.917011786918946,-2.529846264619,13.8390832900376));
#415646=CARTESIAN_POINT('Ctrl Pts',(0.917217920979866,-2.52287809682738,
13.8455641171218));
#415647=CARTESIAN_POINT('Ctrl Pts',(0.918737538044587,-2.51558920923515,
13.851896480191));
#415648=CARTESIAN_POINT('Ctrl Pts',(0.921900653390576,-2.50851207473398,
13.8574481026913));
#415649=CARTESIAN_POINT('Ctrl Pts',(0.924038658274404,-2.50372851597246,
13.8612005412592));
#415650=CARTESIAN_POINT('Ctrl Pts',(0.926994201836504,-2.49893664391509,
13.8646714234115));
#415651=CARTESIAN_POINT('Ctrl Pts',(0.930811817210032,-2.4945319841948,
13.8674635290331));
#415652=CARTESIAN_POINT('Ctrl Pts',(0.933888519594087,-2.49098216952349,
13.8697137499649));
#415653=CARTESIAN_POINT('Ctrl Pts',(0.937607708297721,-2.48760988429062,
13.8715630732994));
#415654=CARTESIAN_POINT('Ctrl Pts',(0.941795032024219,-2.48476097520335,
13.8727429581918));
#415655=CARTESIAN_POINT('Ctrl Pts',(0.94603061740123,-2.48187923057155,
13.873936442031));
#415656=CARTESIAN_POINT('Ctrl Pts',(0.950881648467455,-2.47945889546171,
13.8744652622107));
#415657=CARTESIAN_POINT('Ctrl Pts',(0.955869417106374,-2.47779694534243,
13.8742206332401));
#415658=CARTESIAN_POINT('Ctrl Pts',(0.960162706050751,-2.47636639942305,
13.8740100655632));
#415659=CARTESIAN_POINT('Ctrl Pts',(0.964670332085183,-2.47545636155576,
13.8732246156103));
#415660=CARTESIAN_POINT('Ctrl Pts',(0.969030334073073,-2.47508376456042,
13.8719820486038));
#415661=CARTESIAN_POINT('Ctrl Pts',(0.973465469022901,-2.47470474685335,
13.8707180692815));
#415662=CARTESIAN_POINT('Ctrl Pts',(0.977847909115691,-2.47486476912973,
13.868960862563));
#415663=CARTESIAN_POINT('Ctrl Pts',(0.98194009817502,-2.47545239888339,
13.8669057591701));
#415664=CARTESIAN_POINT('Ctrl Pts',(0.988241127944434,-2.47635721352356,
13.8637413727084));
#415665=CARTESIAN_POINT('Ctrl Pts',(0.994052972729721,-2.4782778211293,
13.8597962563956));
#415666=CARTESIAN_POINT('Ctrl Pts',(0.999140693232015,-2.48080974496047,
13.855546950204));
#415667=CARTESIAN_POINT('Ctrl Pts',(1.00520838296238,-2.48382935427698,
13.850479165618));
#415668=CARTESIAN_POINT('Ctrl Pts',(1.01042616641141,-2.48778800631399,
13.8448473071436));
#415669=CARTESIAN_POINT('Ctrl Pts',(1.01471541067073,-2.4922651093538,13.8390832900376));
#415670=CARTESIAN_POINT('',(1.03947723417938,-2.51811260508541,13.8057746032556));
#415671=CARTESIAN_POINT('',(1.01471541067073,-2.4922651093538,13.8390832900376));
#415672=CARTESIAN_POINT('',(1.12202867321912,-2.48242938847038,13.8057746032556));
#415673=CARTESIAN_POINT('Origin',(0.,2.5406128344257E-15,13.8057746032556));
#415674=CARTESIAN_POINT('',(1.12016646235943,-2.44668343611513,13.8390832900376));
#415675=CARTESIAN_POINT('',(1.12202867321912,-2.48242938847038,13.8057746032556));
#415676=CARTESIAN_POINT('',(1.21448177232262,-2.40126357667189,13.8390832900376));
#415677=CARTESIAN_POINT('Ctrl Pts',(1.12016646235943,-2.44668343611513,
13.8390832900376));
#415678=CARTESIAN_POINT('Ctrl Pts',(1.11980394016194,-2.43972165248739,
13.8455641171218));
#415679=CARTESIAN_POINT('Ctrl Pts',(1.12072438882074,-2.43233315516911,
13.851896480191));
#415680=CARTESIAN_POINT('Ctrl Pts',(1.1233001269986,-2.42502174598354,13.8574481026913));
#415681=CARTESIAN_POINT('Ctrl Pts',(1.12504111340009,-2.42007983687289,
13.8612005412592));
#415682=CARTESIAN_POINT('Ctrl Pts',(1.12759624057656,-2.41506300513624,
13.8646714234115));
#415683=CARTESIAN_POINT('Ctrl Pts',(1.13104213249179,-2.41036183046386,
13.8674635290331));
#415684=CARTESIAN_POINT('Ctrl Pts',(1.13381925455189,-2.40657304770102,
13.8697137499649));
#415685=CARTESIAN_POINT('Ctrl Pts',(1.13725119540868,-2.40290883506246,
13.8715630732994));
#415686=CARTESIAN_POINT('Ctrl Pts',(1.14119237362231,-2.39972809972824,
13.8727429581918));
#415687=CARTESIAN_POINT('Ctrl Pts',(1.14517897649809,-2.39651070433449,
13.873936442031));
#415688=CARTESIAN_POINT('Ctrl Pts',(1.14981658637787,-2.39370301862339,
13.8744652622107));
#415689=CARTESIAN_POINT('Ctrl Pts',(1.15465229426459,-2.39164004905777,
13.8742206332401));
#415690=CARTESIAN_POINT('Ctrl Pts',(1.15881469487121,-2.38986432025601,
13.8740100655633));
#415691=CARTESIAN_POINT('Ctrl Pts',(1.1632331456173,-2.38858989709609,13.8732246156103));
#415692=CARTESIAN_POINT('Ctrl Pts',(1.16754826994411,-2.38786315924821,
13.8719820486038));
#415693=CARTESIAN_POINT('Ctrl Pts',(1.17193775388651,-2.38712389801911,
13.8707180692815));
#415694=CARTESIAN_POINT('Ctrl Pts',(1.17631865507252,-2.38692617828241,
13.868960862563));
#415695=CARTESIAN_POINT('Ctrl Pts',(1.18044512499054,-2.38717830134817,
13.8669057591701));
#415696=CARTESIAN_POINT('Ctrl Pts',(1.18679893939626,-2.38756651287016,
13.8637413727084));
#415697=CARTESIAN_POINT('Ctrl Pts',(1.19274799309739,-2.38900701050799,
13.8597962563956));
#415698=CARTESIAN_POINT('Ctrl Pts',(1.19802515992689,-2.39111581311846,
13.855546950204));
#415699=CARTESIAN_POINT('Ctrl Pts',(1.20431878611221,-2.39363080189135,
13.850479165618));
#415700=CARTESIAN_POINT('Ctrl Pts',(1.2098418747086,-2.39715098404964,13.8448473071436));
#415701=CARTESIAN_POINT('Ctrl Pts',(1.21448177232262,-2.40126357667189,
13.8390832900376));
#415702=CARTESIAN_POINT('',(1.24126801376483,-2.42500674850021,13.8057746032556));
#415703=CARTESIAN_POINT('',(1.21448177232262,-2.40126357667189,13.8390832900376));
#415704=CARTESIAN_POINT('',(1.32063625628023,-2.3827135561929,13.8057746032556));
#415705=CARTESIAN_POINT('Origin',(0.,2.5406128344257E-15,13.8057746032556));
#415706=CARTESIAN_POINT('',(1.31586661480737,-2.34723833301827,13.8390832900376));
#415707=CARTESIAN_POINT('',(1.32063625628023,-2.3827135561929,13.8057746032556));
#415708=CARTESIAN_POINT('',(1.4061659581551,-2.29428203106783,13.8390832900376));
#415709=CARTESIAN_POINT('Ctrl Pts',(1.31586661480737,-2.34723833301826,
13.8390832900376));
#415710=CARTESIAN_POINT('Ctrl Pts',(1.31493784887688,-2.34032926307583,
13.8455641171218));
#415711=CARTESIAN_POINT('Ctrl Pts',(1.31525300369579,-2.33289032526215,
13.851896480191));
#415712=CARTESIAN_POINT('Ctrl Pts',(1.31722422359291,-2.32539329761401,
13.8574481026913));
#415713=CARTESIAN_POINT('Ctrl Pts',(1.31855660553481,-2.320325925744,13.8612005412592));
#415714=CARTESIAN_POINT('Ctrl Pts',(1.32069431237585,-2.31511752051557,
13.8646714234115));
#415715=CARTESIAN_POINT('Ctrl Pts',(1.32374554899063,-2.3101511164329,13.8674635290331));
#415716=CARTESIAN_POINT('Ctrl Pts',(1.32620460943766,-2.30614857930271,
13.8697137499649));
#415717=CARTESIAN_POINT('Ctrl Pts',(1.32932646344742,-2.30221682398901,
13.8715630732994));
#415718=CARTESIAN_POINT('Ctrl Pts',(1.33299526825743,-2.2987254296767,13.8727429581918));
#415719=CARTESIAN_POINT('Ctrl Pts',(1.33670635844757,-2.29519379475651,
13.873936442031));
#415720=CARTESIAN_POINT('Ctrl Pts',(1.34109968461233,-2.29201744312933,
13.8744652622107));
#415721=CARTESIAN_POINT('Ctrl Pts',(1.3457511509087,-2.28956718283947,13.8742206332401));
#415722=CARTESIAN_POINT('Ctrl Pts',(1.34975496308826,-2.28745808833752,
13.8740100655633));
#415723=CARTESIAN_POINT('Ctrl Pts',(1.35405483448529,-2.28582776096083,
13.8732246156103));
#415724=CARTESIAN_POINT('Ctrl Pts',(1.35829636471057,-2.2847517185809,13.8719820486038));
#415725=CARTESIAN_POINT('Ctrl Pts',(1.36261098635412,-2.28365713349126,
13.8707180692815));
#415726=CARTESIAN_POINT('Ctrl Pts',(1.36696119445875,-2.28310298753372,
13.868960862563));
#415727=CARTESIAN_POINT('Ctrl Pts',(1.37109448425899,-2.28301792607418,
13.8669057591701));
#415728=CARTESIAN_POINT('Ctrl Pts',(1.37745879971445,-2.28288695099435,
13.8637413727084));
#415729=CARTESIAN_POINT('Ctrl Pts',(1.38350547236056,-2.28383775239016,
13.8597962563956));
#415730=CARTESIAN_POINT('Ctrl Pts',(1.38893696684269,-2.28550940004648,
13.855546950204));
#415731=CARTESIAN_POINT('Ctrl Pts',(1.39541464643907,-2.28750303144043,
13.850479165618));
#415732=CARTESIAN_POINT('Ctrl Pts',(1.40120628493946,-2.29056131748852,
13.8448473071436));
#415733=CARTESIAN_POINT('Ctrl Pts',(1.40616595815509,-2.29428203106783,
13.8390832900376));
#415734=CARTESIAN_POINT('',(1.43479835951348,-2.3157628721017,13.8057746032556));
#415735=CARTESIAN_POINT('',(1.4061659581551,-2.29428203106783,13.8390832900376));
#415736=CARTESIAN_POINT('',(1.51045522294544,-2.26714115831902,13.8057746032556));
#415737=CARTESIAN_POINT('Origin',(0.,2.5406128344257E-15,13.8057746032556));
#415738=CARTESIAN_POINT('',(1.50280989203648,-2.23217274608223,13.8390832900376));
#415739=CARTESIAN_POINT('',(1.51045522294544,-2.26714115831902,13.8057746032556));
#415740=CARTESIAN_POINT('',(1.5884923415371,-2.17203241707691,13.8390832900376));
#415741=CARTESIAN_POINT('Ctrl Pts',(1.50280989203647,-2.23217274608223,
13.8390832900376));
#415742=CARTESIAN_POINT('Ctrl Pts',(1.50132106315701,-2.22536236854565,
13.8455641171218));
#415743=CARTESIAN_POINT('Ctrl Pts',(1.50102882683272,-2.21792249514038,
13.851896480191));
#415744=CARTESIAN_POINT('Ctrl Pts',(1.50238241030592,-2.21028974051175,
13.8574481026913));
#415745=CARTESIAN_POINT('Ctrl Pts',(1.50329732100622,-2.20513062840611,
13.8612005412592));
#415746=CARTESIAN_POINT('Ctrl Pts',(1.50500338142551,-2.19976531076337,
13.8646714234115));
#415747=CARTESIAN_POINT('Ctrl Pts',(1.50763965726358,-2.19456672787018,
13.8674635290331));
#415748=CARTESIAN_POINT('Ctrl Pts',(1.50976429145597,-2.19037707259687,
13.8697137499649));
#415749=CARTESIAN_POINT('Ctrl Pts',(1.51255528319535,-2.18620393979096,
13.8715630732994));
#415750=CARTESIAN_POINT('Ctrl Pts',(1.51592729931104,-2.18242512115366,
13.8727429581918));
#415751=CARTESIAN_POINT('Ctrl Pts',(1.51933818012262,-2.17860274915475,
13.873936442031));
#415752=CARTESIAN_POINT('Ctrl Pts',(1.52345798571156,-2.1750788697075,13.8744652622107));
#415753=CARTESIAN_POINT('Ctrl Pts',(1.52789425567682,-2.17225762477136,
13.8742206332401));
#415754=CARTESIAN_POINT('Ctrl Pts',(1.53171283471986,-2.16982920024517,
13.8740100655633));
#415755=CARTESIAN_POINT('Ctrl Pts',(1.53586551183311,-2.16785381821142,
13.8732246156103));
#415756=CARTESIAN_POINT('Ctrl Pts',(1.54000522127301,-2.16643563218393,
13.8719820486038));
#415757=CARTESIAN_POINT('Ctrl Pts',(1.54421626752253,-2.16499300751694,
13.8707180692815));
#415758=CARTESIAN_POINT('Ctrl Pts',(1.54850683262858,-2.16408612308847,
13.868960862563));
#415759=CARTESIAN_POINT('Ctrl Pts',(1.55261943594936,-2.16366444317361,
13.8669057591701));
#415760=CARTESIAN_POINT('Ctrl Pts',(1.55895189898524,-2.16301515310951,
13.8637413727084));
#415761=CARTESIAN_POINT('Ctrl Pts',(1.5650559509675,-2.16346993083689,13.8597962563956));
#415762=CARTESIAN_POINT('Ctrl Pts',(1.57060562740263,-2.1646932989997,13.855546950204));
#415763=CARTESIAN_POINT('Ctrl Pts',(1.5772242525211,-2.1661523057267,13.850479165618));
#415764=CARTESIAN_POINT('Ctrl Pts',(1.58324589852681,-2.16872834327552,
13.8448473071436));
#415765=CARTESIAN_POINT('Ctrl Pts',(1.5884923415371,-2.17203241707691,13.8390832900376));
#415766=CARTESIAN_POINT('',(1.61878035890463,-2.19110797586332,13.8057746032556));
#415767=CARTESIAN_POINT('',(1.5884923415371,-2.17203241707691,13.8390832900376));
#415768=CARTESIAN_POINT('',(1.69022235930951,-2.13648131008849,13.8057746032556));
#415769=CARTESIAN_POINT('Origin',(0.,2.5406128344257E-15,13.8057746032556));
#415770=CARTESIAN_POINT('',(1.67975221738026,-2.1022524178036,13.8390832900376));
#415771=CARTESIAN_POINT('',(1.69022235930951,-2.13648131008849,13.8057746032556));
#415772=CARTESIAN_POINT('',(1.76024757046897,-2.03532828571046,13.8390832900376));
#415773=CARTESIAN_POINT('Ctrl Pts',(1.67975221738026,-2.1022524178036,13.8390832900376));
#415774=CARTESIAN_POINT('Ctrl Pts',(1.67771323346238,-2.09558605461174,
13.8455641171218));
#415775=CARTESIAN_POINT('Ctrl Pts',(1.67681555077941,-2.0881947567449,13.851896480191));
#415776=CARTESIAN_POINT('Ctrl Pts',(1.67754248995399,-2.08047706985852,
13.8574481026913));
#415777=CARTESIAN_POINT('Ctrl Pts',(1.67803384083294,-2.07526055055712,
13.8612005412592));
#415778=CARTESIAN_POINT('Ctrl Pts',(1.67929690127987,-2.06977402580377,
13.8646714234115));
#415779=CARTESIAN_POINT('Ctrl Pts',(1.68150067236047,-2.06437785981151,
13.8674635290331));
#415780=CARTESIAN_POINT('Ctrl Pts',(1.68327674120823,-2.06002896785967,
13.8697137499649));
#415781=CARTESIAN_POINT('Ctrl Pts',(1.68571829708768,-2.05564222907186,
13.8715630732994));
#415782=CARTESIAN_POINT('Ctrl Pts',(1.68877108429812,-2.05160113352414,
13.8727429581918));
#415783=CARTESIAN_POINT('Ctrl Pts',(1.69185905688211,-2.04751346170152,
13.873936442031));
#415784=CARTESIAN_POINT('Ctrl Pts',(1.69567792526876,-2.04366550527053,
13.8744652622107));
#415785=CARTESIAN_POINT('Ctrl Pts',(1.69986947625822,-2.04049205060769,
13.8742206332401));
#415786=CARTESIAN_POINT('Ctrl Pts',(1.70347741015123,-2.03776045682181,
13.8740100655632));
#415787=CARTESIAN_POINT('Ctrl Pts',(1.70745525759965,-2.03545316597251,
13.8732246156103));
#415788=CARTESIAN_POINT('Ctrl Pts',(1.71146559717085,-2.0337022740915,13.8719820486038));
#415789=CARTESIAN_POINT('Ctrl Pts',(1.71554504420834,-2.0319212102763,13.8707180692815));
#415790=CARTESIAN_POINT('Ctrl Pts',(1.71974741331291,-2.03066762254314,
13.868960862563));
#415791=CARTESIAN_POINT('Ctrl Pts',(1.72381196145766,-2.02991213038323,
13.8669057591701));
#415792=CARTESIAN_POINT('Ctrl Pts',(1.73007043057724,-2.02874884625311,
13.8637413727084));
#415793=CARTESIAN_POINT('Ctrl Pts',(1.73619124043682,-2.02870457384131,
13.8597962563956));
#415794=CARTESIAN_POINT('Ctrl Pts',(1.74182216664388,-2.02947152119733,
13.855546950204));
#415795=CARTESIAN_POINT('Ctrl Pts',(1.74853769142628,-2.03038619380833,
13.850479165618));
#415796=CARTESIAN_POINT('Ctrl Pts',(1.75474927187666,-2.03246283975302,
13.8448473071436));
#415797=CARTESIAN_POINT('Ctrl Pts',(1.76024757046896,-2.03532828571046,
13.8390832900376));
#415798=CARTESIAN_POINT('',(1.79198964208723,-2.05187161755295,13.8057746032556));
#415799=CARTESIAN_POINT('',(1.76024757046897,-2.03532828571046,13.8390832900376));
#415800=CARTESIAN_POINT('',(1.85874134473945,-1.99160353123393,13.8057746032556));
#415801=CARTESIAN_POINT('Origin',(0.,2.5406128344257E-15,13.8057746032556));
#415802=CARTESIAN_POINT('',(1.84551606885698,-1.95834194653172,13.8390832900376));
#415803=CARTESIAN_POINT('',(1.85874134473945,-1.99160353123393,13.8057746032556));
#415804=CARTESIAN_POINT('',(1.92028864223977,-1.88507938040814,13.8390832900376));
#415805=CARTESIAN_POINT('Ctrl Pts',(1.84551606885698,-1.95834194653172,
13.8390832900376));
#415806=CARTESIAN_POINT('Ctrl Pts',(1.84294049900225,-1.95186396123175,
13.8455641171218));
#415807=CARTESIAN_POINT('Ctrl Pts',(1.84144334389075,-1.94457042677117,
13.851896480191));
#415808=CARTESIAN_POINT('Ctrl Pts',(1.84153880110644,-1.93681916755994,
13.8574481026913));
#415809=CARTESIAN_POINT('Ctrl Pts',(1.84160332230502,-1.93157995613807,
13.8612005412592));
#415810=CARTESIAN_POINT('Ctrl Pts',(1.84241497732068,-1.92600873619112,
13.8646714234115));
#415811=CARTESIAN_POINT('Ctrl Pts',(1.84417157791089,-1.92045089769417,
13.8674635290331));
#415812=CARTESIAN_POINT('Ctrl Pts',(1.84558726196885,-1.91597171022223,
13.8697137499649));
#415813=CARTESIAN_POINT('Ctrl Pts',(1.84766313383683,-1.91140055847537,
13.8715630732994));
#415814=CARTESIAN_POINT('Ctrl Pts',(1.85037637634683,-1.90712407884138,
13.8727429581918));
#415815=CARTESIAN_POINT('Ctrl Pts',(1.85312089075514,-1.90279830997661,
13.873936442031));
#415816=CARTESIAN_POINT('Ctrl Pts',(1.85661340800045,-1.89865188407705,
13.8744652622107));
#415817=CARTESIAN_POINT('Ctrl Pts',(1.86053234593384,-1.89514733850471,
13.8742206332401));
#415818=CARTESIAN_POINT('Ctrl Pts',(1.86390562447202,-1.89213075376511,
13.8740100655633));
#415819=CARTESIAN_POINT('Ctrl Pts',(1.86768217033715,-1.88950690874019,
13.8732246156103));
#415820=CARTESIAN_POINT('Ctrl Pts',(1.87153645189147,-1.88743496290225,
13.8719820486038));
#415821=CARTESIAN_POINT('Ctrl Pts',(1.87545715166994,-1.88532731262467,
13.8707180692815));
#415822=CARTESIAN_POINT('Ctrl Pts',(1.8795433587,-1.88373536400636,13.868960862563));
#415823=CARTESIAN_POINT('Ctrl Pts',(1.88353280277142,-1.88265108727707,
13.8669057591701));
#415824=CARTESIAN_POINT('Ctrl Pts',(1.88967562889528,-1.88098155054489,
13.8637413727084));
#415825=CARTESIAN_POINT('Ctrl Pts',(1.89577246365241,-1.8804385226195,13.8597962563956));
#415826=CARTESIAN_POINT('Ctrl Pts',(1.90144716674655,-1.88074394526063,
13.855546950204));
#415827=CARTESIAN_POINT('Ctrl Pts',(1.90821490048343,-1.88110819676032,
13.850479165618));
#415828=CARTESIAN_POINT('Ctrl Pts',(1.91457507833541,-1.88267163136473,
13.8448473071436));
#415829=CARTESIAN_POINT('Ctrl Pts',(1.92028864223976,-1.88507938040814,
13.8390832900376));
#415830=CARTESIAN_POINT('',(1.95327352985922,-1.89898039216275,13.8057746032556));
#415831=CARTESIAN_POINT('',(1.92028864223977,-1.88507938040814,13.8390832900376));
#415832=CARTESIAN_POINT('',(2.01489071319087,-1.83347195947046,13.8057746032556));
#415833=CARTESIAN_POINT('Origin',(0.,2.5406128344257E-15,13.8057746032556));
#415834=CARTESIAN_POINT('',(1.99899831538418,-1.80139903270935,13.8390832900376));
#415835=CARTESIAN_POINT('',(2.01489071319087,-1.83347195947046,13.8057746032556));
#415836=CARTESIAN_POINT('',(2.06755050992179,-1.72228558284541,13.8390832900376));
#415837=CARTESIAN_POINT('Ctrl Pts',(1.99899831538418,-1.80139903270935,
13.8390832900376));
#415838=CARTESIAN_POINT('Ctrl Pts',(1.99590329958504,-1.79515253522466,
13.8455641171218));
#415839=CARTESIAN_POINT('Ctrl Pts',(1.99381663536526,-1.78800530143882,
13.851896480191));
#415840=CARTESIAN_POINT('Ctrl Pts',(1.99327997537005,-1.78027205325392,
13.8574481026913));
#415841=CARTESIAN_POINT('Ctrl Pts',(1.99291723751031,-1.77504501579918,
13.8612005412592));
#415842=CARTESIAN_POINT('Ctrl Pts',(1.99327208566451,-1.76942617620819,
13.8646714234115));
#415843=CARTESIAN_POINT('Ctrl Pts',(1.99456982587721,-1.76374365170476,
13.8674635290331));
#415844=CARTESIAN_POINT('Ctrl Pts',(1.99561570400154,-1.75916397696634,
13.8697137499649));
#415845=CARTESIAN_POINT('Ctrl Pts',(1.99731207727325,-1.75443883252113,
13.8715630732994));
#415846=CARTESIAN_POINT('Ctrl Pts',(1.99966771890155,-1.74995542806726,
13.8727429581918));
#415847=CARTESIAN_POINT('Ctrl Pts',(2.00205051084362,-1.74542034943843,
13.873936442031));
#415848=CARTESIAN_POINT('Ctrl Pts',(2.00519343482156,-1.74100304785055,
13.8744652622107));
#415849=CARTESIAN_POINT('Ctrl Pts',(2.0088136798135,-1.73719073354128,13.8742206332401));
#415850=CARTESIAN_POINT('Ctrl Pts',(2.01192985438474,-1.7339092327217,13.8740100655633));
#415851=CARTESIAN_POINT('Ctrl Pts',(2.01547996637693,-1.7309862947769,13.8732246156103));
#415852=CARTESIAN_POINT('Ctrl Pts',(2.01915254030653,-1.72860708343973,
13.8719820486038));
#415853=CARTESIAN_POINT('Ctrl Pts',(2.02288840121583,-1.72618687276463,
13.8707180692815));
#415854=CARTESIAN_POINT('Ctrl Pts',(2.02683125313777,-1.72426715741658,
13.868960862563));
#415855=CARTESIAN_POINT('Ctrl Pts',(2.03071904404377,-1.72286131180065,
13.8669057591701));
#415856=CARTESIAN_POINT('Ctrl Pts',(2.03670534767756,-1.7206966329579,13.8637413727084));
#415857=CARTESIAN_POINT('Ctrl Pts',(2.04273763390285,-1.71965846328019,
13.8597962563956));
#415858=CARTESIAN_POINT('Ctrl Pts',(2.04841834967123,-1.71950032866912,
13.855546950204));
#415859=CARTESIAN_POINT('Ctrl Pts',(2.05519325421116,-1.71931173502386,
13.850479165618));
#415860=CARTESIAN_POINT('Ctrl Pts',(2.0616597035305,-1.72035155388866,13.8448473071436));
#415861=CARTESIAN_POINT('Ctrl Pts',(2.06755050992178,-1.72228558284541,
13.8390832900376));
#415862=CARTESIAN_POINT('',(2.10155870455744,-1.73345176557241,13.8057746032556));
#415863=CARTESIAN_POINT('',(2.06755050992179,-1.72228558284541,13.8390832900376));
#415864=CARTESIAN_POINT('',(2.15763131637958,-1.66313893431829,13.8057746032556));
#415865=CARTESIAN_POINT('Origin',(0.,2.5406128344257E-15,13.8057746032556));
#415866=CARTESIAN_POINT('',(2.13917755793401,-1.63246810553422,13.8390832900376));
#415867=CARTESIAN_POINT('',(2.15763131637958,-1.66313893431829,13.8057746032556));
#415868=CARTESIAN_POINT('',(2.2010531700821,-1.54803025888596,13.8390832900376));
#415869=CARTESIAN_POINT('Ctrl Pts',(2.139177557934,-1.63246810553422,13.8390832900376));
#415870=CARTESIAN_POINT('Ctrl Pts',(2.13558369300996,-1.62649466527496,
13.8455641171218));
#415871=CARTESIAN_POINT('Ctrl Pts',(2.132921406088,-1.6195412958255,13.851896480191));
#415872=CARTESIAN_POINT('Ctrl Pts',(2.13175620026561,-1.6118775221577,13.8574481026913));
#415873=CARTESIAN_POINT('Ctrl Pts',(2.13096861730817,-1.60669744374196,
13.8612005412592));
#415874=CARTESIAN_POINT('Ctrl Pts',(2.13086429714498,-1.60106837695737,
13.8646714234115));
#415875=CARTESIAN_POINT('Ctrl Pts',(2.13169454073316,-1.59529898271048,
13.8674635290331));
#415876=CARTESIAN_POINT('Ctrl Pts',(2.13236365277751,-1.59064929768537,
13.8697137499649));
#415877=CARTESIAN_POINT('Ctrl Pts',(2.13366923836871,-1.58580160559849,
13.8715630732994));
#415878=CARTESIAN_POINT('Ctrl Pts',(2.13565160270894,-1.58114111264167,
13.8727429581918));
#415879=CARTESIAN_POINT('Ctrl Pts',(2.13765681509752,-1.57642690444882,
13.873936442031));
#415880=CARTESIAN_POINT('Ctrl Pts',(2.14042923016756,-1.57176812358589,
13.8744652622107));
#415881=CARTESIAN_POINT('Ctrl Pts',(2.14372669008493,-1.56767341086243,
13.8742206332401));
#415882=CARTESIAN_POINT('Ctrl Pts',(2.1465650230616,-1.56414883180941,13.8740100655633));
#415883=CARTESIAN_POINT('Ctrl Pts',(2.14986507577125,-1.56094625261451,
13.8732246156103));
#415884=CARTESIAN_POINT('Ctrl Pts',(2.15333150170257,-1.55827560903701,
13.8719820486038));
#415885=CARTESIAN_POINT('Ctrl Pts',(2.15685766220472,-1.55555894406714,
13.8707180692815));
#415886=CARTESIAN_POINT('Ctrl Pts',(2.16063091998952,-1.55332423737825,
13.868960862563));
#415887=CARTESIAN_POINT('Ctrl Pts',(2.16439118512307,-1.5516061785463,13.8669057591701));
#415888=CARTESIAN_POINT('Ctrl Pts',(2.17018112840377,-1.54896076317355,
13.8637413727084));
#415889=CARTESIAN_POINT('Ctrl Pts',(2.17610872222764,-1.54743436059142,
13.8597962563956));
#415890=CARTESIAN_POINT('Ctrl Pts',(2.18175764644407,-1.54681372108791,
13.855546950204));
#415891=CARTESIAN_POINT('Ctrl Pts',(2.18849463591514,-1.5460735373573,13.850479165618));
#415892=CARTESIAN_POINT('Ctrl Pts',(2.1950243235485,-1.54658282065948,13.8448473071436));
#415893=CARTESIAN_POINT('Ctrl Pts',(2.2010531700821,-1.54803025888596,13.8390832900376));
#415894=CARTESIAN_POINT('',(2.23585835280962,-1.55638730348161,13.8057746032556));
#415895=CARTESIAN_POINT('',(2.2010531700821,-1.54803025888596,13.8390832900376));
#415896=CARTESIAN_POINT('',(2.28601323914189,-1.48173799395684,13.8057746032556));
#415897=CARTESIAN_POINT('Origin',(0.,2.5406128344257E-15,13.8057746032556));
#415898=CARTESIAN_POINT('',(2.26512092677523,-1.45267337245503,13.8390832900376));
#415899=CARTESIAN_POINT('',(2.28601323914189,-1.48173799395684,13.8057746032556));
#415900=CARTESIAN_POINT('',(2.31990818454372,-1.36347304896064,13.8390832900376));
#415901=CARTESIAN_POINT('Ctrl Pts',(2.26512092677523,-1.45267337245503,
13.8390832900376));
#415902=CARTESIAN_POINT('Ctrl Pts',(2.26105212930441,-1.44701274168059,
13.8455641171218));
#415903=CARTESIAN_POINT('Ctrl Pts',(2.25783193676049,-1.44029951009396,
13.851896480191));
#415904=CARTESIAN_POINT('Ctrl Pts',(2.25604593936343,-1.4327562120926,13.8574481026913));
#415905=CARTESIAN_POINT('Ctrl Pts',(2.25483875254292,-1.42765756528305,
13.8612005412592));
#415906=CARTESIAN_POINT('Ctrl Pts',(2.25427595829582,-1.42205573181558,
13.8646714234115));
#415907=CARTESIAN_POINT('Ctrl Pts',(2.25463318012539,-1.41623786219207,
13.8674635290331));
#415908=CARTESIAN_POINT('Ctrl Pts',(2.25492107325948,-1.41154910976695,
13.8697137499649));
#415909=CARTESIAN_POINT('Ctrl Pts',(2.25582718271348,-1.40661113062945,
13.8715630732994));
#415910=CARTESIAN_POINT('Ctrl Pts',(2.25742307745801,-1.40180456398137,
13.8727429581918));
#415911=CARTESIAN_POINT('Ctrl Pts',(2.2590373659355,-1.39694259850223,13.873936442031));
#415912=CARTESIAN_POINT('Ctrl Pts',(2.26142082213276,-1.39207334178225,
13.8744652622107));
#415913=CARTESIAN_POINT('Ctrl Pts',(2.26437355292386,-1.38772348028219,
13.8742206332401));
#415914=CARTESIAN_POINT('Ctrl Pts',(2.26691515566827,-1.38397927848782,
13.8740100655633));
#415915=CARTESIAN_POINT('Ctrl Pts',(2.26994318778909,-1.38051837067896,
13.8732246156103));
#415916=CARTESIAN_POINT('Ctrl Pts',(2.27318039722948,-1.37757406755353,
13.8719820486038));
#415917=CARTESIAN_POINT('Ctrl Pts',(2.27647339130811,-1.37457902724603,
13.8707180692815));
#415918=CARTESIAN_POINT('Ctrl Pts',(2.28005194454775,-1.37204420082063,
13.868960862563));
#415919=CARTESIAN_POINT('Ctrl Pts',(2.28365965996478,-1.37002536217072,
13.8669057591701));
#415920=CARTESIAN_POINT('Ctrl Pts',(2.28921471177514,-1.36691681507081,
13.8637413727084));
#415921=CARTESIAN_POINT('Ctrl Pts',(2.29499816603867,-1.36491233754161,
13.8597962563956));
#415922=CARTESIAN_POINT('Ctrl Pts',(2.30057770604451,-1.36383332339915,
13.855546950204));
#415923=CARTESIAN_POINT('Ctrl Pts',(2.3072319468933,-1.36254647538379,13.850479165618));
#415924=CARTESIAN_POINT('Ctrl Pts',(2.3137814188468,-1.36252183392703,13.8448473071436));
#415925=CARTESIAN_POINT('Ctrl Pts',(2.31990818454372,-1.36347304896064,
13.8390832900376));
#415926=CARTESIAN_POINT('',(2.35527873261451,-1.36896534067195,13.8057746032556));
#415927=CARTESIAN_POINT('',(2.31990818454372,-1.36347304896064,13.8390832900376));
#415928=CARTESIAN_POINT('',(2.39918212096335,-1.29047633171518,13.8057746032556));
#415929=CARTESIAN_POINT('Origin',(0.,2.5406128344257E-15,13.8057746032556));
#415930=CARTESIAN_POINT('',(2.37599028956742,-1.2632113377564,13.8390832900376));
#415931=CARTESIAN_POINT('',(2.39918212096335,-1.29047633171518,13.8057746032556));
#415932=CARTESIAN_POINT('',(2.42332459279512,-1.1698421508517,13.8390832900376));
#415933=CARTESIAN_POINT('Ctrl Pts',(2.37599028956742,-1.2632113377564,13.8390832900376));
#415934=CARTESIAN_POINT('Ctrl Pts',(2.37147363672568,-1.25790118703063,
13.8455641171218));
#415935=CARTESIAN_POINT('Ctrl Pts',(2.36771696840989,-1.25147276875544,
13.851896480191));
#415936=CARTESIAN_POINT('Ctrl Pts',(2.36532206495616,-1.24410014582415,
13.8574481026913));
#415937=CARTESIAN_POINT('Ctrl Pts',(2.3637033079017,-1.2391168612741,13.8612005412592));
#415938=CARTESIAN_POINT('Ctrl Pts',(2.36268578487355,-1.23357954040124,
13.8646714234115));
#415939=CARTESIAN_POINT('Ctrl Pts',(2.36256760769217,-1.22775191236357,
13.8674635290331));
#415940=CARTESIAN_POINT('Ctrl Pts',(2.36247236603471,-1.22305529541225,
13.8697137499649));
#415941=CARTESIAN_POINT('Ctrl Pts',(2.36297296934257,-1.21805989066056,
13.8715630732994));
#415942=CARTESIAN_POINT('Ctrl Pts',(2.36417177407519,-1.21313923722925,
13.8727429581918));
#415943=CARTESIAN_POINT('Ctrl Pts',(2.3653843958181,-1.20816187004193,13.873936442031));
#415944=CARTESIAN_POINT('Ctrl Pts',(2.36736303163483,-1.20311454156498,
13.8744652622107));
#415945=CARTESIAN_POINT('Ctrl Pts',(2.36995138336341,-1.19853847889894,
13.8742206332401));
#415946=CARTESIAN_POINT('Ctrl Pts',(2.37217934192864,-1.19459957140841,
13.8740100655633));
#415947=CARTESIAN_POINT('Ctrl Pts',(2.37491520240646,-1.19090336675605,
13.8732246156103));
#415948=CARTESIAN_POINT('Ctrl Pts',(2.37790165226118,-1.1877049979342,13.8719820486038));
#415949=CARTESIAN_POINT('Ctrl Pts',(2.38093956558401,-1.18445151378818,
13.8707180692815));
#415950=CARTESIAN_POINT('Ctrl Pts',(2.3842995995971,-1.1816334364779,13.868960862563));
#415951=CARTESIAN_POINT('Ctrl Pts',(2.38773075654675,-1.17932725304818,
13.8669057591701));
#415952=CARTESIAN_POINT('Ctrl Pts',(2.39301394893348,-1.17577626108917,
13.8637413727084));
#415953=CARTESIAN_POINT('Ctrl Pts',(2.39861477570277,-1.17330704808014,
13.8597962563956));
#415954=CARTESIAN_POINT('Ctrl Pts',(2.40408780057982,-1.17177683995984,
13.855546950204));
#415955=CARTESIAN_POINT('Ctrl Pts',(2.41061500993135,-1.16995189142096,
13.850479165618));
#415956=CARTESIAN_POINT('Ctrl Pts',(2.41714068054974,-1.16939348919007,
13.8448473071436));
#415957=CARTESIAN_POINT('Ctrl Pts',(2.42332459279512,-1.1698421508517,13.8390832900376));
#415958=CARTESIAN_POINT('',(2.45902512104748,-1.17243313938352,13.8057746032556));
#415959=CARTESIAN_POINT('',(2.42332459279512,-1.1698421508517,13.8390832900376));
#415960=CARTESIAN_POINT('',(2.49638484160699,-1.09062676239955,13.8057746032556));
#415961=CARTESIAN_POINT('Origin',(0.,2.5406128344257E-15,13.8057746032556));
#415962=CARTESIAN_POINT('',(2.47104782899334,-1.06534284002019,13.8390832900376));
#415963=CARTESIAN_POINT('',(2.49638484160699,-1.09062676239955,13.8057746032556));
#415964=CARTESIAN_POINT('',(2.51061417570188,-0.96842614623922,13.8390832900376));
#415965=CARTESIAN_POINT('Ctrl Pts',(2.47104782899333,-1.06534284002019,
13.8390832900376));
#415966=CARTESIAN_POINT('Ctrl Pts',(2.46611337836014,-1.06041850752007,
13.8455641171218));
#415967=CARTESIAN_POINT('Ctrl Pts',(2.46184523428033,-1.05431768261933,
13.851896480191));
#415968=CARTESIAN_POINT('Ctrl Pts',(2.45885736245727,-1.04716479834732,
13.8574481026913));
#415969=CARTESIAN_POINT('Ctrl Pts',(2.45683780772999,-1.04233003899326,
13.8612005412592));
#415970=CARTESIAN_POINT('Ctrl Pts',(2.45537232736866,-1.03689408067184,
13.8646714234115));
#415971=CARTESIAN_POINT('Ctrl Pts',(2.45477953762597,-1.03109547612309,
13.8674635290331));
#415972=CARTESIAN_POINT('Ctrl Pts',(2.45430179499447,-1.0264222498565,13.8697137499649));
#415973=CARTESIAN_POINT('Ctrl Pts',(2.45439356072379,-1.02140266308507,
13.8715630732994));
#415974=CARTESIAN_POINT('Ctrl Pts',(2.45518729759679,-1.01640066900726,
13.8727429581918));
#415975=CARTESIAN_POINT('Ctrl Pts',(2.4559901828075,-1.01134102366916,13.873936442031));
#415976=CARTESIAN_POINT('Ctrl Pts',(2.45755083074879,-1.00614921257353,
13.8744652622107));
#415977=CARTESIAN_POINT('Ctrl Pts',(2.45975757836114,-1.00137740168355,
13.8742206332401));
#415978=CARTESIAN_POINT('Ctrl Pts',(2.46165706605052,-0.99727000127633,
13.8740100655633));
#415979=CARTESIAN_POINT('Ctrl Pts',(2.46408254818524,-0.993363097412604,
13.8732246156103));
#415980=CARTESIAN_POINT('Ctrl Pts',(2.46679836412324,-0.989931947511155,
13.8719820486038));
#415981=CARTESIAN_POINT('Ctrl Pts',(2.46956097987833,-0.986441670926813,
13.8707180692815));
#415982=CARTESIAN_POINT('Ctrl Pts',(2.47268013419288,-0.983359096571208,
13.868960862563));
#415983=CARTESIAN_POINT('Ctrl Pts',(2.47591189889175,-0.980780915631897,
13.8669057591701));
#415984=CARTESIAN_POINT('Ctrl Pts',(2.48088807308118,-0.976811110079414,
13.8637413727084));
#415985=CARTESIAN_POINT('Ctrl Pts',(2.48626899977814,-0.973893593795741,
13.8597962563956));
#415986=CARTESIAN_POINT('Ctrl Pts',(2.49159908744885,-0.97192237498016,
13.855546950204));
#415987=CARTESIAN_POINT('Ctrl Pts',(2.4979558278018,-0.969571470649191,
13.850479165618));
#415988=CARTESIAN_POINT('Ctrl Pts',(2.50441426982377,-0.968483023718886,
13.8448473071436));
#415989=CARTESIAN_POINT('Ctrl Pts',(2.51061417570188,-0.96842614623922,
13.8390832900376));
#415990=CARTESIAN_POINT('',(2.54640710301047,-0.968098588990333,13.8057746032556));
#415991=CARTESIAN_POINT('',(2.51061417570188,-0.96842614623922,13.8390832900376));
#415992=CARTESIAN_POINT('',(2.57697453300423,-0.883519251920907,13.8057746032556));
#415993=CARTESIAN_POINT('Origin',(0.,2.5406128344257E-15,13.8057746032556));
#415994=CARTESIAN_POINT('',(2.5496609528115,-0.860384661452853,13.8390832900376));
#415995=CARTESIAN_POINT('',(2.57697453300423,-0.883519251920907,13.8057746032556));
#415996=CARTESIAN_POINT('',(2.58119603549153,-0.760565425402582,13.8390832900376));
#415997=CARTESIAN_POINT('Ctrl Pts',(2.5496609528115,-0.860384661452853,
13.8390832900376));
#415998=CARTESIAN_POINT('Ctrl Pts',(2.54434154234169,-0.855878917798706,
13.8455641171218));
#415999=CARTESIAN_POINT('Ctrl Pts',(2.5395903262925,-0.850146286255557,
13.851896480191));
#416000=CARTESIAN_POINT('Ctrl Pts',(2.53602936989415,-0.843260741907522,
13.8574481026913));
#416001=CARTESIAN_POINT('Ctrl Pts',(2.53362245729755,-0.838606682275279,
13.8612005412592));
#416002=CARTESIAN_POINT('Ctrl Pts',(2.53171877213306,-0.833308261911033,
13.8646714234115));
#416003=CARTESIAN_POINT('Ctrl Pts',(2.53065531474699,-0.827577269607798,
13.8674635290331));
#416004=CARTESIAN_POINT('Ctrl Pts',(2.52979825043985,-0.822958533575708,
13.8697137499649));
#416005=CARTESIAN_POINT('Ctrl Pts',(2.52948056790483,-0.817948169306319,
13.8715630732994));
#416006=CARTESIAN_POINT('Ctrl Pts',(2.52986395473027,-0.812898122027324,
13.8727429581918));
#416007=CARTESIAN_POINT('Ctrl Pts',(2.53025176034016,-0.807789869643406,
13.873936442031));
#416008=CARTESIAN_POINT('Ctrl Pts',(2.53138403455146,-0.802488126575336,
13.8744652622107));
#416009=CARTESIAN_POINT('Ctrl Pts',(2.5331944925063,-0.797552323075592,
13.8742206332401));
#416010=CARTESIAN_POINT('Ctrl Pts',(2.53475286854267,-0.793303763823721,
13.8740100655633));
#416011=CARTESIAN_POINT('Ctrl Pts',(2.53685183115084,-0.789212160549251,
13.8732246156103));
#416012=CARTESIAN_POINT('Ctrl Pts',(2.53927893986515,-0.785571063304695,
13.8719820486038));
#416013=CARTESIAN_POINT('Ctrl Pts',(2.54174787330044,-0.781867221496848,
13.8707180692815));
#416014=CARTESIAN_POINT('Ctrl Pts',(2.54460539045911,-0.778540664119665,
13.868960862563));
#416015=CARTESIAN_POINT('Ctrl Pts',(2.54761625604633,-0.775707643039546,
13.8669057591701));
#416016=CARTESIAN_POINT('Ctrl Pts',(2.55225229642025,-0.771345442294568,
13.8637413727084));
#416017=CARTESIAN_POINT('Ctrl Pts',(2.5573775138655,-0.767999038325763,
13.8597962563956));
#416018=CARTESIAN_POINT('Ctrl Pts',(2.56252919347581,-0.765599926950894,
13.855546950204));
#416019=CARTESIAN_POINT('Ctrl Pts',(2.56867316177193,-0.762738711708286,
13.850479165618));
#416020=CARTESIAN_POINT('Ctrl Pts',(2.57502139533138,-0.761127463513312,
13.8448473071436));
#416021=CARTESIAN_POINT('Ctrl Pts',(2.58119603549152,-0.760565425402582,
13.8390832900376));
#416022=CARTESIAN_POINT('',(2.61684316583053,-0.757321502212443,13.8057746032556));
#416023=CARTESIAN_POINT('',(2.58119603549153,-0.760565425402582,13.8390832900376));
#416024=CARTESIAN_POINT('',(2.64041488405521,-0.670532066591146,13.8057746032556));
#416025=CARTESIAN_POINT('Origin',(0.,2.5406128344257E-15,13.8057746032556));
#416026=CARTESIAN_POINT('',(2.61130650365315,-0.649700764917019,13.8390832900376));
#416027=CARTESIAN_POINT('',(2.64041488405521,-0.670532066591146,13.8057746032556));
#416028=CARTESIAN_POINT('',(2.63460046153234,-0.547643267144351,13.8390832900376));
#416029=CARTESIAN_POINT('Ctrl Pts',(2.61130650365314,-0.649700764917019,
13.8390832900376));
#416030=CARTESIAN_POINT('Ctrl Pts',(2.60563753314576,-0.645643595089471,
13.8455641171218));
#416031=CARTESIAN_POINT('Ctrl Pts',(2.6004348636861,-0.640317306621022,
13.851896480191));
#416032=CARTESIAN_POINT('Ctrl Pts',(2.59632452028977,-0.633744924358559,
13.8574481026913));
#416033=CARTESIAN_POINT('Ctrl Pts',(2.59354626743007,-0.629302536447119,
13.8612005412592));
#416034=CARTESIAN_POINT('Ctrl Pts',(2.5912170461731,-0.624176914153404,
13.8646714234115));
#416035=CARTESIAN_POINT('Ctrl Pts',(2.5896899982771,-0.618551672903904,
13.8674635290331));
#416036=CARTESIAN_POINT('Ctrl Pts',(2.58845931591587,-0.614018164032572,
13.8697137499649));
#416037=CARTESIAN_POINT('Ctrl Pts',(2.58773429924137,-0.609050365412783,
13.8715630732994));
#416038=CARTESIAN_POINT('Ctrl Pts',(2.58770478464319,-0.603985872164047,
13.8727429581918));
#416039=CARTESIAN_POINT('Ctrl Pts',(2.58767492986991,-0.598863007311117,
13.873936442031));
#416040=CARTESIAN_POINT('Ctrl Pts',(2.58837129525315,-0.593486614496006,
13.8744652622107));
#416041=CARTESIAN_POINT('Ctrl Pts',(2.58977341525151,-0.588419665344441,
13.8742206332401));
#416042=CARTESIAN_POINT('Ctrl Pts',(2.59098030889944,-0.584058220708777,
13.8740100655633));
#416043=CARTESIAN_POINT('Ctrl Pts',(2.59273878373123,-0.579809146968282,
13.8732246156103));
#416044=CARTESIAN_POINT('Ctrl Pts',(2.59486103321378,-0.575982333282046,
13.8719820486038));
#416045=CARTESIAN_POINT('Ctrl Pts',(2.59701985398461,-0.572089574706832,
13.8707180692815));
#416046=CARTESIAN_POINT('Ctrl Pts',(2.59959671768218,-0.568541171998573,
13.868960862563));
#416047=CARTESIAN_POINT('Ctrl Pts',(2.60236664734402,-0.565472164065521,
13.8669057591701));
#416048=CARTESIAN_POINT('Ctrl Pts',(2.60663170181863,-0.560746597854291,
13.8637413727084));
#416049=CARTESIAN_POINT('Ctrl Pts',(2.61146710253567,-0.556993575966648,
13.8597962563956));
#416050=CARTESIAN_POINT('Ctrl Pts',(2.61640609050775,-0.554182537722866,
13.855546950204));
#416051=CARTESIAN_POINT('Ctrl Pts',(2.62229639965171,-0.550830052483992,
13.850479165618));
#416052=CARTESIAN_POINT('Ctrl Pts',(2.62849217830169,-0.548706725615247,
13.8448473071436));
#416053=CARTESIAN_POINT('Ctrl Pts',(2.63460046153234,-0.547643267144351,
13.8390832900376));
#416054=CARTESIAN_POINT('',(2.66986456913072,-0.541504565786582,13.8057746032556));
#416055=CARTESIAN_POINT('',(2.63460046153234,-0.547643267144351,13.8390832900376));
#416056=CARTESIAN_POINT('',(2.68628370969059,-0.453082600988223,13.8057746032556));
#416057=CARTESIAN_POINT('Origin',(0.,2.5406128344257E-15,13.8057746032556));
#416058=CARTESIAN_POINT('',(2.65557424054823,-0.434693216983744,13.8390832900376));
#416059=CARTESIAN_POINT('',(2.68628370969059,-0.453082600988223,13.8057746032556));
#416060=CARTESIAN_POINT('',(2.67047205618014,-0.331076633298054,13.8390832900376));
#416061=CARTESIAN_POINT('Ctrl Pts',(2.65557424054823,-0.434693216983744,
13.8390832900376));
#416062=CARTESIAN_POINT('Ctrl Pts',(2.64959343606668,-0.43111162077861,
13.8455641171218));
#416063=CARTESIAN_POINT('Ctrl Pts',(2.64397393610343,-0.426227120955838,
13.851896480191));
#416064=CARTESIAN_POINT('Ctrl Pts',(2.63934155936626,-0.420011638898538,
13.8574481026913));
#416065=CARTESIAN_POINT('Ctrl Pts',(2.63621045505786,-0.415810486066509,
13.8612005412592));
#416066=CARTESIAN_POINT('Ctrl Pts',(2.63347119829158,-0.41089177201402,
13.8646714234115));
#416067=CARTESIAN_POINT('Ctrl Pts',(2.63149072213746,-0.405409716870673,
13.8674635290331));
#416068=CARTESIAN_POINT('Ctrl Pts',(2.6298946117102,-0.40099160491366,13.8697137499649));
#416069=CARTESIAN_POINT('Ctrl Pts',(2.62876708576257,-0.396099431823667,
13.8715630732994));
#416070=CARTESIAN_POINT('Ctrl Pts',(2.62832486615555,-0.391054195972177,
13.8727429581918));
#416071=CARTESIAN_POINT('Ctrl Pts',(2.6278775496777,-0.385950810470619,
13.873936442031));
#416072=CARTESIAN_POINT('Ctrl Pts',(2.62813337203614,-0.3805355469156,13.8744652622107));
#416073=CARTESIAN_POINT('Ctrl Pts',(2.62911782320076,-0.375371171822829,
13.8742206332401));
#416074=CARTESIAN_POINT('Ctrl Pts',(2.62996520278216,-0.370925866497836,
13.8740100655633));
#416075=CARTESIAN_POINT('Ctrl Pts',(2.63137148747768,-0.366547599176018,
13.8732246156103));
#416076=CARTESIAN_POINT('Ctrl Pts',(2.63317475450832,-0.362560535861801,
13.8719820486038));
#416077=CARTESIAN_POINT('Ctrl Pts',(2.63500909601863,-0.358504766185281,
13.8707180692815));
#416078=CARTESIAN_POINT('Ctrl Pts',(2.63728815765234,-0.354758132180522,
13.868960862563));
#416079=CARTESIAN_POINT('Ctrl Pts',(2.63979871796391,-0.351473561135978,
13.8669057591701));
#416080=CARTESIAN_POINT('Ctrl Pts',(2.64366440330536,-0.34641607732197,
13.8637413727084));
#416081=CARTESIAN_POINT('Ctrl Pts',(2.64817780850021,-0.342281413256947,
13.8597962563956));
#416082=CARTESIAN_POINT('Ctrl Pts',(2.65287123668398,-0.339077155139974,
13.855546950204));
#416083=CARTESIAN_POINT('Ctrl Pts',(2.65846868764025,-0.335255710140978,
13.850479165618));
#416084=CARTESIAN_POINT('Ctrl Pts',(2.66447077949609,-0.33263443498845,
13.8448473071436));
#416085=CARTESIAN_POINT('Ctrl Pts',(2.67047205618014,-0.331076633298055,
13.8390832900376));
#416086=CARTESIAN_POINT('',(2.70511846421999,-0.322084005817376,13.8057746032556));
#416087=CARTESIAN_POINT('',(2.67047205618014,-0.331076633298054,13.8390832900376));
#416088=CARTESIAN_POINT('',(2.71427576044359,-0.232617945429092,13.8057746032556));
#416089=CARTESIAN_POINT('Origin',(0.,2.5406128344257E-15,13.8057746032556));
#416090=CARTESIAN_POINT('',(2.68216956901137,-0.216792857410774,13.8390832900376));
#416091=CARTESIAN_POINT('',(2.71427576044359,-0.232617945429092,13.8057746032556));
#416092=CARTESIAN_POINT('',(2.68857209989094,-0.112306739080959,13.8390832900376));
#416093=CARTESIAN_POINT('Ctrl Pts',(2.68216956901137,-0.216792857410774,
13.8390832900376));
#416094=CARTESIAN_POINT('Ctrl Pts',(2.67591673182272,-0.213710669759878,
13.8455641171218));
#416095=CARTESIAN_POINT('Ctrl Pts',(2.66991779820098,-0.209300464123221,
13.851896480191));
#416096=CARTESIAN_POINT('Ctrl Pts',(2.66479421582587,-0.203483245278693,
13.8574481026913));
#416097=CARTESIAN_POINT('Ctrl Pts',(2.66133109705134,-0.199551285505029,
13.8612005412592));
#416098=CARTESIAN_POINT('Ctrl Pts',(2.65820003407759,-0.194872212924259,
13.8646714234115));
#416099=CARTESIAN_POINT('Ctrl Pts',(2.6557793094074,-0.189569826059568,
13.8674635290331));
#416100=CARTESIAN_POINT('Ctrl Pts',(2.65382839276567,-0.18529651282301,
13.8697137499649));
#416101=CARTESIAN_POINT('Ctrl Pts',(2.65230586104407,-0.180512521867566,
13.8715630732994));
#416102=CARTESIAN_POINT('Ctrl Pts',(2.65145387932672,-0.175520118625508,
13.8727429581918));
#416103=CARTESIAN_POINT('Ctrl Pts',(2.65059207796165,-0.170470174663835,
13.873936442031));
#416104=CARTESIAN_POINT('Ctrl Pts',(2.65040565483971,-0.165052078054418,
13.8744652622107));
#416105=CARTESIAN_POINT('Ctrl Pts',(2.65096588581051,-0.159824645084622,
13.8742206332401));
#416106=CARTESIAN_POINT('Ctrl Pts',(2.65144811215407,-0.155325061843814,
13.8740100655633));
#416107=CARTESIAN_POINT('Ctrl Pts',(2.6524928481207,-0.150846737587331,
13.8732246156103));
#416108=CARTESIAN_POINT('Ctrl Pts',(2.65396513225485,-0.146725957893671,
13.8719820486038));
#416109=CARTESIAN_POINT('Ctrl Pts',(2.65546278726455,-0.142534167593885,
13.8707180692815));
#416110=CARTESIAN_POINT('Ctrl Pts',(2.65742888005524,-0.13861423552378,
13.868960862563));
#416111=CARTESIAN_POINT('Ctrl Pts',(2.65966336365188,-0.135135959646133,
13.8669057591701));
#416112=CARTESIAN_POINT('Ctrl Pts',(2.66310395436203,-0.129780214949702,
13.8637413727084));
#416113=CARTESIAN_POINT('Ctrl Pts',(2.66726532806777,-0.125291424214479,
13.8597962563956));
#416114=CARTESIAN_POINT('Ctrl Pts',(2.67168196247302,-0.12171527003342,
13.855546950204));
#416115=CARTESIAN_POINT('Ctrl Pts',(2.67694930512901,-0.117450296360274,
13.850479165618));
#416116=CARTESIAN_POINT('Ctrl Pts',(2.68271776725967,-0.114348517077624,
13.8448473071436));
#416117=CARTESIAN_POINT('Ctrl Pts',(2.68857209989094,-0.112306739080959,
13.8390832900376));
#416118=CARTESIAN_POINT('',(2.722370242243,-0.100520029929576,13.8057746032556));
#416119=CARTESIAN_POINT('',(2.68857209989094,-0.112306739080959,13.8390832900376));
#416120=CARTESIAN_POINT('',(2.72420475383482,-0.010605255822389,13.8057746032556));
#416121=CARTESIAN_POINT('Origin',(0.,2.5406128344257E-15,13.8057746032556));
#416122=CARTESIAN_POINT('',(2.69091550151957,0.00255022285996096,13.8390832900376));
#416123=CARTESIAN_POINT('',(2.72420475383482,-0.010605255822389,13.8057746032556));
#416124=CARTESIAN_POINT('',(2.68878013986014,0.107210537955413,13.8390832900376));
#416125=CARTESIAN_POINT('Ctrl Pts',(2.69091550151957,0.00255022285996075,
13.8390832900376));
#416126=CARTESIAN_POINT('Ctrl Pts',(2.68443224322366,0.00511249050632783,
13.8455641171218));
#416127=CARTESIAN_POINT('Ctrl Pts',(2.67809379785693,0.00901905276598984,
13.851896480191));
#416128=CARTESIAN_POINT('Ctrl Pts',(2.67251310643925,0.0143992957661106,
13.8574481026913));
#416129=CARTESIAN_POINT('Ctrl Pts',(2.66874101968268,0.0180358959378414,
13.8612005412592));
#416130=CARTESIAN_POINT('Ctrl Pts',(2.66523898720895,0.0224441885908644,
13.8646714234115));
#416131=CARTESIAN_POINT('Ctrl Pts',(2.66239412354597,0.0275316206671468,
13.8674635290331));
#416132=CARTESIAN_POINT('Ctrl Pts',(2.66010138371815,0.0316316969887058,
13.8697137499649));
#416133=CARTESIAN_POINT('Ctrl Pts',(2.65819397841997,0.0362756691390899,
13.8715630732994));
#416134=CARTESIAN_POINT('Ctrl Pts',(2.65693790439007,0.0411820161518279,
13.8727429581918));
#416135=CARTESIAN_POINT('Ctrl Pts',(2.65566735328368,0.0461449120297329,
13.873936442031));
#416136=CARTESIAN_POINT('Ctrl Pts',(2.65503992529648,0.0515297851545395,
13.8744652622107));
#416137=CARTESIAN_POINT('Ctrl Pts',(2.65517220782878,0.0567854882974133,
13.8742206332401));
#416138=CARTESIAN_POINT('Ctrl Pts',(2.65528607179774,0.0613094054699473,
13.8740100655633));
#416139=CARTESIAN_POINT('Ctrl Pts',(2.65596230648999,0.0658579841520367,
13.8732246156103));
#416140=CARTESIAN_POINT('Ctrl Pts',(2.65709380991966,0.070085057116158,
13.8719820486038));
#416141=CARTESIAN_POINT('Ctrl Pts',(2.65824481178174,0.0743849723663609,
13.8707180692815));
#416142=CARTESIAN_POINT('Ctrl Pts',(2.65988485170627,0.0784521160006324,
13.868960862563));
#416143=CARTESIAN_POINT('Ctrl Pts',(2.66182838846831,0.0821009493592947,
13.8669057591701));
#416144=CARTESIAN_POINT('Ctrl Pts',(2.66482098798363,0.0877193133408292,
13.8637413727084));
#416145=CARTESIAN_POINT('Ctrl Pts',(2.66860263694484,0.0925323585845062,
13.8597962563956));
#416146=CARTESIAN_POINT('Ctrl Pts',(2.6727130855983,0.0964566101136009,
13.855546950204));
#416147=CARTESIAN_POINT('Ctrl Pts',(2.67761526665769,0.101136729764772,
13.850479165618));
#416148=CARTESIAN_POINT('Ctrl Pts',(2.68311171089942,0.104698371348177,
13.8448473071436));
#416149=CARTESIAN_POINT('Ctrl Pts',(2.68878013986013,0.107210537955413,
13.8390832900376));
#416150=CARTESIAN_POINT('',(2.72150509546337,0.121712890172768,13.8057746032556));
#416151=CARTESIAN_POINT('',(2.68878013986014,0.107210537955413,13.8390832900376));
#416152=CARTESIAN_POINT('',(2.71600461405142,0.211478010012068,13.8057746032556));
#416153=CARTESIAN_POINT('Origin',(0.,2.5406128344257E-15,13.8057746032556));
#416154=CARTESIAN_POINT('',(2.68175383533497,0.22187633181832,13.8390832900376));
#416155=CARTESIAN_POINT('',(2.71600461405142,0.211478010012068,13.8057746032556));
#416156=CARTESIAN_POINT('',(2.67109479161606,0.326014346550186,13.8390832900376));
#416157=CARTESIAN_POINT('Ctrl Pts',(2.68175383533497,0.22187633181832,13.8390832900376));
#416158=CARTESIAN_POINT('Ctrl Pts',(2.67508330094609,0.223901627991715,
13.8455641171218));
#416159=CARTESIAN_POINT('Ctrl Pts',(2.66844752514252,0.227278549347082,
13.851896480191));
#416160=CARTESIAN_POINT('Ctrl Pts',(2.66244686326291,0.232186011873307,
13.8574481026913));
#416161=CARTESIAN_POINT('Ctrl Pts',(2.6583909111393,0.235503051468959,13.8612005412592));
#416162=CARTESIAN_POINT('Ctrl Pts',(2.65454121461392,0.239611227733946,
13.8646714234115));
#416163=CARTESIAN_POINT('Ctrl Pts',(2.65129114405646,0.244449849000719,
13.8674635290331));
#416164=CARTESIAN_POINT('Ctrl Pts',(2.64867183884781,0.248349403075825,
13.8697137499649));
#416165=CARTESIAN_POINT('Ctrl Pts',(2.64639225344063,0.252822451552694,
13.8715630732994));
#416166=CARTESIAN_POINT('Ctrl Pts',(2.6447404460636,0.257610091406232,13.8727429581918));
#416167=CARTESIAN_POINT('Ctrl Pts',(2.64306960052388,0.262452911947122,
13.873936442031));
#416168=CARTESIAN_POINT('Ctrl Pts',(2.64200534310115,0.267768726145111,
13.8744652622107));
#416169=CARTESIAN_POINT('Ctrl Pts',(2.64170879687653,0.273017723623774,
13.8742206332401));
#416170=CARTESIAN_POINT('Ctrl Pts',(2.64145354072497,0.277535868805646,
13.8740100655633));
#416171=CARTESIAN_POINT('Ctrl Pts',(2.64175677391253,0.282124431872679,
13.8732246156103));
#416172=CARTESIAN_POINT('Ctrl Pts',(2.64253996666907,0.286429667634104,
13.8719820486038));
#416173=CARTESIAN_POINT('Ctrl Pts',(2.64333665565605,0.29080909260817,13.8707180692815));
#416174=CARTESIAN_POINT('Ctrl Pts',(2.64463972851931,0.294996381636749,
13.868960862563));
#416175=CARTESIAN_POINT('Ctrl Pts',(2.64627938453026,0.298791490092439,
13.8669057591701));
#416176=CARTESIAN_POINT('Ctrl Pts',(2.64880407759472,0.304635084073745,
13.8637413727084));
#416177=CARTESIAN_POINT('Ctrl Pts',(2.65218083556149,0.309740353803876,
13.8597962563956));
#416178=CARTESIAN_POINT('Ctrl Pts',(2.65595774410555,0.313986587434537,
13.855546950204));
#416179=CARTESIAN_POINT('Ctrl Pts',(2.66046214036218,0.319050707639619,
13.850479165618));
#416180=CARTESIAN_POINT('Ctrl Pts',(2.66564998878541,0.32304850938667,13.8448473071436));
#416181=CARTESIAN_POINT('Ctrl Pts',(2.67109479161606,0.326014346550185,
13.8390832900376));
#416182=CARTESIAN_POINT('',(2.70252878129015,0.343135831072226,13.8057746032556));
#416183=CARTESIAN_POINT('',(2.67109479161606,0.326014346550186,13.8390832900376));
#416184=CARTESIAN_POINT('',(2.68972991167073,0.432153924581312,13.8057746032556));
#416185=CARTESIAN_POINT('Origin',(0.,2.5406128344257E-15,13.8057746032556));
#416186=CARTESIAN_POINT('',(2.65474553983445,0.439725890395448,13.8390832900376));
#416187=CARTESIAN_POINT('',(2.68972991167073,0.432153924581312,13.8057746032556));
#416188=CARTESIAN_POINT('',(2.6356337482334,0.54264858345725,13.8390832900376));
#416189=CARTESIAN_POINT('Ctrl Pts',(2.65474553983445,0.439725890395448,
13.8390832900376));
#416190=CARTESIAN_POINT('Ctrl Pts',(2.64793212065841,0.441200737083988,
13.8455641171218));
#416191=CARTESIAN_POINT('Ctrl Pts',(2.64104317441114,0.444025544680594,
13.851896480191));
#416192=CARTESIAN_POINT('Ctrl Pts',(2.63466247548437,0.448427568379484,
13.8574481026913));
#416193=CARTESIAN_POINT('Ctrl Pts',(2.63034964968591,0.451402973047822,
13.8612005412592));
#416194=CARTESIAN_POINT('Ctrl Pts',(2.6261779082041,0.45518369368953,13.8646714234115));
#416195=CARTESIAN_POINT('Ctrl Pts',(2.6225442594355,0.459741303920579,13.8674635290331));
#416196=CARTESIAN_POINT('Ctrl Pts',(2.61961581989004,0.463414384860244,
13.8697137499649));
#416197=CARTESIAN_POINT('Ctrl Pts',(2.61697922463863,0.467686742263982,
13.8715630732995));
#416198=CARTESIAN_POINT('Ctrl Pts',(2.61494267642004,0.472323814005002,
13.8727429581918));
#416199=CARTESIAN_POINT('Ctrl Pts',(2.61288265564838,0.477014331037186,
13.873936442031));
#416200=CARTESIAN_POINT('Ctrl Pts',(2.61138865124768,0.482225710441918,
13.8744652622107));
#416201=CARTESIAN_POINT('Ctrl Pts',(2.61066524973233,0.487433071044176,
13.8742206332401));
#416202=CARTESIAN_POINT('Ctrl Pts',(2.61004257214782,0.491915376724641,
13.8740100655633));
#416203=CARTESIAN_POINT('Ctrl Pts',(2.60997078586386,0.496513388046464,
13.8732246156103));
#416204=CARTESIAN_POINT('Ctrl Pts',(2.6104004559287,0.500868135971515,13.8719820486038));
#416205=CARTESIAN_POINT('Ctrl Pts',(2.61083753020681,0.505297926318795,
13.8707180692815));
#416206=CARTESIAN_POINT('Ctrl Pts',(2.6117949642739,0.509577495024053,13.868960862563));
#416207=CARTESIAN_POINT('Ctrl Pts',(2.61311982789352,0.513493622756147,
13.8669057591701));
#416208=CARTESIAN_POINT('Ctrl Pts',(2.61515981309133,0.519523558583403,
13.8637413727084));
#416209=CARTESIAN_POINT('Ctrl Pts',(2.6181092082965,0.524887078072245,13.8597962563956));
#416210=CARTESIAN_POINT('Ctrl Pts',(2.62152744202795,0.529427035820237,
13.855546950204));
#416211=CARTESIAN_POINT('Ctrl Pts',(2.62560407746791,0.534841455694789,
13.850479165618));
#416212=CARTESIAN_POINT('Ctrl Pts',(2.63044880579731,0.53924881289445,13.8448473071436));
#416213=CARTESIAN_POINT('Ctrl Pts',(2.63563374823339,0.542648583457249,
13.8390832900376));
#416214=CARTESIAN_POINT('',(2.66556758396332,0.562275259629327,13.8057746032556));
#416215=CARTESIAN_POINT('',(2.6356337482334,0.54264858345725,13.8390832900376));
#416216=CARTESIAN_POINT('',(2.64555550050207,0.649953926082844,13.8057746032556));
#416217=CARTESIAN_POINT('Origin',(0.,2.5406128344257E-15,13.8057746032556));
#416218=CARTESIAN_POINT('',(2.61007035076852,0.654649145721658,13.8390832900376));
#416219=CARTESIAN_POINT('',(2.64555550050207,0.649953926082844,13.8057746032556));
#416220=CARTESIAN_POINT('',(2.5826329971052,0.755671583572118,13.8390832900376));
#416221=CARTESIAN_POINT('Ctrl Pts',(2.61007035076851,0.654649145721657,
13.8390832900376));
#416222=CARTESIAN_POINT('Ctrl Pts',(2.60315938898579,0.655563728063963,
13.8455641171218));
#416223=CARTESIAN_POINT('Ctrl Pts',(2.5960631170955,0.657817623273311,13.851896480191));
#416224=CARTESIAN_POINT('Ctrl Pts',(2.58934484362018,0.661684913403435,
13.8574481026913));
#416225=CARTESIAN_POINT('Ctrl Pts',(2.58480384529101,0.664298882317296,
13.8612005412592));
#416226=CARTESIAN_POINT('Ctrl Pts',(2.58033782110404,0.667726987263631,
13.8646714234115));
#416227=CARTESIAN_POINT('Ctrl Pts',(2.57634477545734,0.671973256314823,
13.8674635290331));
#416228=CARTESIAN_POINT('Ctrl Pts',(2.57312668985709,0.675395420371407,
13.8697137499649));
#416229=CARTESIAN_POINT('Ctrl Pts',(2.57015063086784,0.679438654868381,
13.8715630732995));
#416230=CARTESIAN_POINT('Ctrl Pts',(2.56774289470007,0.683894299549507,
13.8727429581918));
#416231=CARTESIAN_POINT('Ctrl Pts',(2.56530740779484,0.688401298456017,
13.873936442031));
#416232=CARTESIAN_POINT('Ctrl Pts',(2.56339359876896,0.693473562197373,
13.8744652622107));
#416233=CARTESIAN_POINT('Ctrl Pts',(2.56224815608062,0.698604631797571,
13.8742206332401));
#416234=CARTESIAN_POINT('Ctrl Pts',(2.56126220087975,0.703021268971854,
13.8740100655633));
#416235=CARTESIAN_POINT('Ctrl Pts',(2.56081587285014,0.70759812954174,13.8732246156103));
#416236=CARTESIAN_POINT('Ctrl Pts',(2.56088916083988,0.711973409501458,
13.8719820486038));
#416237=CARTESIAN_POINT('Ctrl Pts',(2.56096371175193,0.716424085698055,
13.8707180692815));
#416238=CARTESIAN_POINT('Ctrl Pts',(2.56156913545708,0.720767454256337,
13.868960862563));
#416239=CARTESIAN_POINT('Ctrl Pts',(2.56257038993658,0.724778540080894,
13.8669057591701));
#416240=CARTESIAN_POINT('Ctrl Pts',(2.56411209150282,0.73095468952604,13.8637413727084));
#416241=CARTESIAN_POINT('Ctrl Pts',(2.56661449620793,0.736540765436313,
13.8597962563956));
#416242=CARTESIAN_POINT('Ctrl Pts',(2.56965130734524,0.741344234631866,
13.855546950204));
#416243=CARTESIAN_POINT('Ctrl Pts',(2.57327305263227,0.747072922104936,
13.850479165618));
#416244=CARTESIAN_POINT('Ctrl Pts',(2.57774242000014,0.751860504522207,
13.8448473071436));
#416245=CARTESIAN_POINT('Ctrl Pts',(2.5826329971052,0.755671583572117,13.8390832900376));
#416246=CARTESIAN_POINT('',(2.6108674741529,0.777672839102481,13.8057746032556));
#416247=CARTESIAN_POINT('',(2.5826329971052,0.755671583572118,13.8390832900376));
#416248=CARTESIAN_POINT('',(2.5837753539635,0.863428591441144,13.8057746032556));
#416249=CARTESIAN_POINT('Origin',(0.,2.5406128344257E-15,13.8057746032556));
#416250=CARTESIAN_POINT('',(2.54802557414951,0.865215818992596,13.8390832900376));
#416251=CARTESIAN_POINT('',(2.5837753539635,0.863428591441144,13.8057746032556));
#416252=CARTESIAN_POINT('',(2.51244524948572,0.963665713975349,13.8390832900376));
#416253=CARTESIAN_POINT('Ctrl Pts',(2.54802557414951,0.865215818992595,
13.8390832900376));
#416254=CARTESIAN_POINT('Ctrl Pts',(2.54106306107054,0.865564050594074,
13.8455641171218));
#416255=CARTESIAN_POINT('Ctrl Pts',(2.53380668805586,0.867232034115413,
13.851896480191));
#416256=CARTESIAN_POINT('Ctrl Pts',(2.52679554903354,0.870538854499011,
13.8574481026913));
#416257=CARTESIAN_POINT('Ctrl Pts',(2.52205659776832,0.872773992126551,
13.8612005412592));
#416258=CARTESIAN_POINT('Ctrl Pts',(2.5173260115303,0.87582666790469,13.8646714234115));
#416259=CARTESIAN_POINT('Ctrl Pts',(2.51300014206548,0.879733337556075,
13.8674635290331));
#416260=CARTESIAN_POINT('Ctrl Pts',(2.50951382623916,0.882881810792399,
13.8697137499649));
#416261=CARTESIAN_POINT('Ctrl Pts',(2.50621810869362,0.88666901532412,13.8715630732995));
#416262=CARTESIAN_POINT('Ctrl Pts',(2.50345520766364,0.890913581365129,
13.8727429581918));
#416263=CARTESIAN_POINT('Ctrl Pts',(2.50066046238834,0.895207068811845,
13.873936442031));
#416264=CARTESIAN_POINT('Ctrl Pts',(2.49833958482061,0.900106461811489,
13.8744652622107));
#416265=CARTESIAN_POINT('Ctrl Pts',(2.49677972369137,0.905127093988005,
13.8742206332401));
#416266=CARTESIAN_POINT('Ctrl Pts',(2.49543705224334,0.909448670664406,
13.8740100655633));
#416267=CARTESIAN_POINT('Ctrl Pts',(2.49461915270749,0.91397392223039,13.8732246156103));
#416268=CARTESIAN_POINT('Ctrl Pts',(2.49433557090265,0.918340617458513,
13.8719820486038));
#416269=CARTESIAN_POINT('Ctrl Pts',(2.4940471023246,0.92278256098865,13.8707180692815));
#416270=CARTESIAN_POINT('Ctrl Pts',(2.49429648667295,0.927160824998806,
13.868960862563));
#416271=CARTESIAN_POINT('Ctrl Pts',(2.49496746882896,0.931240175801445,
13.8669057591701));
#416272=CARTESIAN_POINT('Ctrl Pts',(2.49600062699407,0.937521437608915,
13.8637413727084));
#416273=CARTESIAN_POINT('Ctrl Pts',(2.49803938810867,0.943292895527074,
13.8597962563956));
#416274=CARTESIAN_POINT('Ctrl Pts',(2.50067456717477,0.948327909875208,
13.855546950204));
#416275=CARTESIAN_POINT('Ctrl Pts',(2.50381732019154,0.954332741476831,
13.850479165618));
#416276=CARTESIAN_POINT('Ctrl Pts',(2.50788158369544,0.959468688540621,
13.8448473071436));
#416277=CARTESIAN_POINT('Ctrl Pts',(2.51244524948572,0.96366571397535,13.8390832900376));
#416278=CARTESIAN_POINT('',(2.53879247206481,0.987895134138395,13.8057746032556));
#416279=CARTESIAN_POINT('',(2.51244524948572,0.963665713975349,13.8390832900376));
#416280=CARTESIAN_POINT('',(2.50480060873724,1.07115728197909,13.8057746032556));
#416281=CARTESIAN_POINT('Origin',(0.,2.5406128344257E-15,13.8057746032556));
#416282=CARTESIAN_POINT('',(2.46902410772917,1.0700246237387,13.8390832900376));
#416283=CARTESIAN_POINT('',(2.50480060873724,1.07115728197909,13.8057746032556));
#416284=CARTESIAN_POINT('',(2.4255375932552,1.16524680804573,13.8390832900376));
#416285=CARTESIAN_POINT('Ctrl Pts',(2.46902410772917,1.0700246237387,13.8390832900376));
#416286=CARTESIAN_POINT('Ctrl Pts',(2.46205637772976,1.0698041871755,13.8455641171218));
#416287=CARTESIAN_POINT('Ctrl Pts',(2.45468819355588,1.07087515885369,13.851896480191));
#416288=CARTESIAN_POINT('Ctrl Pts',(2.44743084695999,1.0735995031467,13.8574481026913));
#416289=CARTESIAN_POINT('Ctrl Pts',(2.44252547969752,1.07544093501578,13.8612005412592));
#416290=CARTESIAN_POINT('Ctrl Pts',(2.43756181267939,1.07809786657207,13.8646714234115));
#416291=CARTESIAN_POINT('Ctrl Pts',(2.43293190734402,1.08163893858167,13.8674635290331));
#416292=CARTESIAN_POINT('Ctrl Pts',(2.42920056214825,1.08449276842781,13.8697137499649));
#416293=CARTESIAN_POINT('Ctrl Pts',(2.42560711850294,1.08799873977297,13.8715630732995));
#416294=CARTESIAN_POINT('Ctrl Pts',(2.42250743926123,1.09200398028716,13.8727429581918));
#416295=CARTESIAN_POINT('Ctrl Pts',(2.4193720341846,1.0960553838235,13.873936442031));
#416296=CARTESIAN_POINT('Ctrl Pts',(2.41665953313229,1.10074930142936,13.8744652622107));
#416297=CARTESIAN_POINT('Ctrl Pts',(2.41469563418062,1.10562608470341,13.8742206332401));
#416298=CARTESIAN_POINT('Ctrl Pts',(2.41300518174238,1.10982384150215,13.8740100655633));
#416299=CARTESIAN_POINT('Ctrl Pts',(2.41182115368675,1.11426736926168,13.8732246156103));
#416300=CARTESIAN_POINT('Ctrl Pts',(2.41118258927746,1.11859642012192,13.8719820486038));
#416301=CARTESIAN_POINT('Ctrl Pts',(2.41053302092011,1.12300007058427,13.8707180692815));
#416302=CARTESIAN_POINT('Ctrl Pts',(2.41042470629996,1.12738409342168,13.868960862563));
#416303=CARTESIAN_POINT('Ctrl Pts',(2.41076095085695,1.13150456179585,13.8669057591701));
#416304=CARTESIAN_POINT('Ctrl Pts',(2.41127869012379,1.13784913520465,13.8637413727084));
#416305=CARTESIAN_POINT('Ctrl Pts',(2.41284024002903,1.14376756703048,13.8597962563956));
#416306=CARTESIAN_POINT('Ctrl Pts',(2.41505625034202,1.14900061934142,13.855546950204));
#416307=CARTESIAN_POINT('Ctrl Pts',(2.41769909658571,1.15524163390802,13.850479165618));
#416308=CARTESIAN_POINT('Ctrl Pts',(2.42133120922257,1.16069176673799,13.8448473071436));
#416309=CARTESIAN_POINT('Ctrl Pts',(2.4255375932552,1.16524680804572,13.8390832900376));
#416310=CARTESIAN_POINT('',(2.4498222249464,1.19154315004784,13.8057746032556));
#416311=CARTESIAN_POINT('',(2.4255375932552,1.16524680804573,13.8390832900376));
#416312=CARTESIAN_POINT('',(2.40915682872283,1.27175759753398,13.8057746032556));
#416313=CARTESIAN_POINT('Origin',(0.,2.5406128344257E-15,13.8057746032556));
#416314=CARTESIAN_POINT('',(2.3735916932322,1.26771259115546,13.8390832900376));
#416315=CARTESIAN_POINT('',(2.40915682872283,1.27175759753398,13.8057746032556));
#416316=CARTESIAN_POINT('',(2.3224883845271,1.35907337686075,13.8390832900376));
#416317=CARTESIAN_POINT('Ctrl Pts',(2.3735916932322,1.26771259115546,13.8390832900376));
#416318=CARTESIAN_POINT('Ctrl Pts',(2.36666511540589,1.26692495339653,13.8455641171218));
#416319=CARTESIAN_POINT('Ctrl Pts',(2.35923415412283,1.26739178609176,13.851896480191));
#416320=CARTESIAN_POINT('Ctrl Pts',(2.3517788963976,1.26951552423239,13.8574481026913));
#416321=CARTESIAN_POINT('Ctrl Pts',(2.34673975754768,1.27095099591773,13.8612005412592));
#416322=CARTESIAN_POINT('Ctrl Pts',(2.34157604213449,1.27319450181105,13.8646714234115));
#416323=CARTESIAN_POINT('Ctrl Pts',(2.33667291218469,1.27634641092888,13.8674635290331));
#416324=CARTESIAN_POINT('Ctrl Pts',(2.33272136910612,1.27888660561805,13.8697137499649));
#416325=CARTESIAN_POINT('Ctrl Pts',(2.32885411313562,1.28208801211578,13.8715630732995));
#416326=CARTESIAN_POINT('Ctrl Pts',(2.32543828353614,1.28582727288836,13.8727429581918));
#416327=CARTESIAN_POINT('Ctrl Pts',(2.32198308426163,1.28960963109222,13.873936442031));
#416328=CARTESIAN_POINT('Ctrl Pts',(2.31889701097173,1.29406683605708,13.8744652622107));
#416329=CARTESIAN_POINT('Ctrl Pts',(2.31654214362114,1.29876731624057,13.8742206332401));
#416330=CARTESIAN_POINT('Ctrl Pts',(2.31451515987476,1.30281331778275,13.8740100655633));
#416331=CARTESIAN_POINT('Ctrl Pts',(2.31297288281071,1.30714555079171,13.8732246156103));
#416332=CARTESIAN_POINT('Ctrl Pts',(2.31198358533776,1.31140814816483,13.8719820486038));
#416333=CARTESIAN_POINT('Ctrl Pts',(2.31097723997135,1.31574419999212,13.8707180692815));
#416334=CARTESIAN_POINT('Ctrl Pts',(2.31051194719864,1.32010480670811,13.868960862563));
#416335=CARTESIAN_POINT('Ctrl Pts',(2.31051121650454,1.32423897161662,13.8669057591701));
#416336=CARTESIAN_POINT('Ctrl Pts',(2.31051009140371,1.3306046345375,13.8637413727084));
#416337=CARTESIAN_POINT('Ctrl Pts',(2.31158403824262,1.33663065408365,13.8597962563956));
#416338=CARTESIAN_POINT('Ctrl Pts',(2.31336613261947,1.34202691925768,13.855546950204));
#416339=CARTESIAN_POINT('Ctrl Pts',(2.31549148438438,1.348462583867,13.850479165618));
#416340=CARTESIAN_POINT('Ctrl Pts',(2.31866727504386,1.35419063272837,13.8448473071436));
#416341=CARTESIAN_POINT('Ctrl Pts',(2.3224883845271,1.35907337686075,13.8390832900376));
#416342=CARTESIAN_POINT('',(2.34454881511319,1.3872616428845,13.8057746032556));
#416343=CARTESIAN_POINT('',(2.3224883845271,1.35907337686075,13.8390832900376));
#416344=CARTESIAN_POINT('',(2.29748050749618,1.46389457610252,13.8057746032556));
#416345=CARTESIAN_POINT('Origin',(0.,2.5406128344257E-15,13.8057746032556));
#416346=CARTESIAN_POINT('',(2.26236341763183,1.45696414043593,13.8390832900376));
#416347=CARTESIAN_POINT('',(2.29748050749618,1.46389457610252,13.8057746032556));
#416348=CARTESIAN_POINT('',(2.20398339878359,1.54385553658409,13.8390832900376));
#416349=CARTESIAN_POINT('Ctrl Pts',(2.26236341763183,1.45696414043593,13.8390832900376));
#416350=CARTESIAN_POINT('Ctrl Pts',(2.25552408721126,1.45561454308062,13.8455641171218));
#416351=CARTESIAN_POINT('Ctrl Pts',(2.24807980064034,1.45547413009832,13.851896480191));
#416352=CARTESIAN_POINT('Ctrl Pts',(2.24047624529588,1.45698312895964,13.8574481026913));
#416353=CARTESIAN_POINT('Ctrl Pts',(2.23533686949616,1.45800308763402,13.8612005412592));
#416354=CARTESIAN_POINT('Ctrl Pts',(2.23000746936204,1.45981823770277,13.8646714234115));
#416355=CARTESIAN_POINT('Ctrl Pts',(2.22486374431866,1.46256000849368,13.8674635290331));
#416356=CARTESIAN_POINT('Ctrl Pts',(2.22071830022452,1.46476966344934,13.8697137499649));
#416357=CARTESIAN_POINT('Ctrl Pts',(2.21660296787927,1.4676452002676,13.8715630732995));
#416358=CARTESIAN_POINT('Ctrl Pts',(2.21289371970442,1.47109359713505,13.8727429581918));
#416359=CARTESIAN_POINT('Ctrl Pts',(2.20914172001316,1.47458173903663,13.873936442031));
#416360=CARTESIAN_POINT('Ctrl Pts',(2.20570261179423,1.47877256939683,13.8744652622107));
#416361=CARTESIAN_POINT('Ctrl Pts',(2.2029724472984,1.48326546556968,13.8742206332401));
#416362=CARTESIAN_POINT('Ctrl Pts',(2.20062242148629,1.48713278638257,13.8740100655633));
#416363=CARTESIAN_POINT('Ctrl Pts',(2.19873215901322,1.49132489434505,13.8732246156103));
#416364=CARTESIAN_POINT('Ctrl Pts',(2.19739871208807,1.49549267134882,13.8719820486038));
#416365=CARTESIAN_POINT('Ctrl Pts',(2.19604228677498,1.49973226883154,13.8707180692815));
#416366=CARTESIAN_POINT('Ctrl Pts',(2.19522311229634,1.50404044030786,13.868960862563));
#416367=CARTESIAN_POINT('Ctrl Pts',(2.1948854112138,1.50816078956533,13.8669057591701));
#416368=CARTESIAN_POINT('Ctrl Pts',(2.19436542923268,1.51450517956181,13.8637413727084));
#416369=CARTESIAN_POINT('Ctrl Pts',(2.19494462606623,1.52059868466244,13.8597962563956));
#416370=CARTESIAN_POINT('Ctrl Pts',(2.19628094496288,1.52612225144513,13.855546950204));
#416371=CARTESIAN_POINT('Ctrl Pts',(2.19787465838367,1.53270973781101,13.850479165618));
#416372=CARTESIAN_POINT('Ctrl Pts',(2.2005729927029,1.53867758348368,13.8448473071436));
#416373=CARTESIAN_POINT('Ctrl Pts',(2.20398339878358,1.54385553658408,13.8390832900376));
#416374=CARTESIAN_POINT('',(2.22367281973873,1.57374813836983,13.8057746032556));
#416375=CARTESIAN_POINT('',(2.20398339878359,1.54385553658409,13.8390832900376));
#416376=CARTESIAN_POINT('',(2.17051483254974,1.6462895777927,13.8057746032556));
#416377=CARTESIAN_POINT('Origin',(0.,2.5406128344257E-15,13.8057746032556));
#416378=CARTESIAN_POINT('',(2.13607948675081,1.63651983374397,13.8390832900376));
#416379=CARTESIAN_POINT('',(2.17051483254974,1.6462895777927,13.8057746032556));
#416380=CARTESIAN_POINT('',(2.07081126715283,1.71836359242969,13.8390832900376));
#416381=CARTESIAN_POINT('Ctrl Pts',(2.13607948675081,1.63651983374397,13.8390832900376));
#416382=CARTESIAN_POINT('Ctrl Pts',(2.12937291835152,1.63461725814,13.8455641171218));
#416383=CARTESIAN_POINT('Ctrl Pts',(2.12196484699164,1.6338705339054,13.851896480191));
#416384=CARTESIAN_POINT('Ctrl Pts',(2.11426359443428,1.63475475134896,13.8574481026913));
#416385=CARTESIAN_POINT('Ctrl Pts',(2.10905818338277,1.63535240935567,13.8612005412592));
#416386=CARTESIAN_POINT('Ctrl Pts',(2.10359856480631,1.63672712407565,13.8646714234115));
#416387=CARTESIAN_POINT('Ctrl Pts',(2.09824847531087,1.63904051050738,13.8674635290331));
#416388=CARTESIAN_POINT('Ctrl Pts',(2.09393671744766,1.64090492084036,13.8697137499649));
#416389=CARTESIAN_POINT('Ctrl Pts',(2.08960069558542,1.64343545175605,13.8715630732995));
#416390=CARTESIAN_POINT('Ctrl Pts',(2.08562271326984,1.64657003620617,13.8727429581918));
#416391=CARTESIAN_POINT('Ctrl Pts',(2.08159888210072,1.64974074879662,13.873936442031));
#416392=CARTESIAN_POINT('Ctrl Pts',(2.07782962565056,1.65363731526754,13.8744652622107));
#416393=CARTESIAN_POINT('Ctrl Pts',(2.07474233280376,1.657892727947,13.8742206332401));
#416394=CARTESIAN_POINT('Ctrl Pts',(2.07208490395997,1.66155563164865,13.8740100655633));
#416395=CARTESIAN_POINT('Ctrl Pts',(2.06985923546278,1.66557971677782,13.8732246156103));
#416396=CARTESIAN_POINT('Ctrl Pts',(2.06819051295471,1.66962493754391,13.8719820486038));
#416397=CARTESIAN_POINT('Ctrl Pts',(2.06649303448161,1.67373986686029,13.8707180692815));
#416398=CARTESIAN_POINT('Ctrl Pts',(2.06532542976803,1.67796693292656,13.868960862563));
#416399=CARTESIAN_POINT('Ctrl Pts',(2.06465300564205,1.68204604628849,13.8669057591701));
#416400=CARTESIAN_POINT('Ctrl Pts',(2.06361762717491,1.6883269424919,13.8637413727084));
#416401=CARTESIAN_POINT('Ctrl Pts',(2.06369821954374,1.69444738187593,13.8597962563956));
#416402=CARTESIAN_POINT('Ctrl Pts',(2.06457986997842,1.70006149184166,13.855546950204));
#416403=CARTESIAN_POINT('Ctrl Pts',(2.06563133915521,1.7067569613292,13.850479165618));
#416404=CARTESIAN_POINT('Ctrl Pts',(2.0678342601645,1.71292488878483,13.8448473071436));
#416405=CARTESIAN_POINT('Ctrl Pts',(2.07081126715283,1.71836359242969,13.8390832900376));
#416406=CARTESIAN_POINT('',(2.08799864862909,1.74976159964447,13.8057746032556));
#416407=CARTESIAN_POINT('',(2.07081126715283,1.71836359242969,13.8390832900376));
#416408=CARTESIAN_POINT('',(2.02910473950242,1.81772879396133,13.8057746032556));
#416409=CARTESIAN_POINT('Origin',(0.,2.5406128344257E-15,13.8057746032556));
#416410=CARTESIAN_POINT('',(1.99558029931377,1.80518475756521,13.8390832900376));
#416411=CARTESIAN_POINT('',(2.02910473950242,1.81772879396133,13.8057746032556));
#416412=CARTESIAN_POINT('',(1.92385822819898,1.88143622207771,13.8390832900376));
#416413=CARTESIAN_POINT('Ctrl Pts',(1.99558029931377,1.80518475756521,13.8390832900376));
#416414=CARTESIAN_POINT('Ctrl Pts',(1.98905112404195,1.80274186503932,13.8455641171218));
#416415=CARTESIAN_POINT('Ctrl Pts',(1.98172856738576,1.801393798879,13.851896480191));
#416416=CARTESIAN_POINT('Ctrl Pts',(1.97398086818066,1.80164735058359,13.8574481026913));
#416417=CARTESIAN_POINT('Ctrl Pts',(1.96874406302907,1.80181873060722,13.8612005412592));
#416418=CARTESIAN_POINT('Ctrl Pts',(1.96319055887113,1.80274386147876,13.8646714234115));
#416419=CARTESIAN_POINT('Ctrl Pts',(1.95766970888652,1.8046134683463,13.8674635290331));
#416420=CARTESIAN_POINT('Ctrl Pts',(1.95322033129143,1.80612022671344,13.8697137499649));
#416421=CARTESIAN_POINT('Ctrl Pts',(1.94869247542231,1.80828891146083,13.8715630732995));
#416422=CARTESIAN_POINT('Ctrl Pts',(1.94447223178197,1.81108882335126,13.8727429581918));
#416423=CARTESIAN_POINT('Ctrl Pts',(1.94020334706754,1.81392100606143,13.873936442031));
#416424=CARTESIAN_POINT('Ctrl Pts',(1.93612902616594,1.81749737763611,13.8744652622107));
#416425=CARTESIAN_POINT('Ctrl Pts',(1.93270515039271,1.82148698775288,13.8742206332401));
#416426=CARTESIAN_POINT('Ctrl Pts',(1.92975800326775,1.8249210983235,13.8740100655633));
#416427=CARTESIAN_POINT('Ctrl Pts',(1.92721174020306,1.82875038099674,13.8732246156103));
#416428=CARTESIAN_POINT('Ctrl Pts',(1.92521884718504,1.83264612524836,13.8719820486038));
#416429=CARTESIAN_POINT('Ctrl Pts',(1.92319161199111,1.83660900222272,13.8707180692815));
#416430=CARTESIAN_POINT('Ctrl Pts',(1.92168334725933,1.8407268324517,13.868960862563));
#416431=CARTESIAN_POINT('Ctrl Pts',(1.92068067496151,1.84473756409168,13.8669057591701));
#416432=CARTESIAN_POINT('Ctrl Pts',(1.91913679028124,1.85091316817404,13.8637413727084));
#416433=CARTESIAN_POINT('Ctrl Pts',(1.91871824185642,1.85701981132716,13.8597962563956));
#416434=CARTESIAN_POINT('Ctrl Pts',(1.91913935659095,1.86268710350039,13.855546950204));
#416435=CARTESIAN_POINT('Ctrl Pts',(1.91964158416986,1.86944599886481,13.850479165618));
#416436=CARTESIAN_POINT('Ctrl Pts',(1.92133443179333,1.87577296156384,13.8448473071436));
#416437=CARTESIAN_POINT('Ctrl Pts',(1.92385822819898,1.88143622207771,13.8390832900376));
#416438=CARTESIAN_POINT('',(1.93842919100836,1.91413068616381,13.8057746032556));
#416439=CARTESIAN_POINT('',(1.92385822819898,1.88143622207771,13.8390832900376));
#416440=CARTESIAN_POINT('',(1.87419128919243,1.97707132491028,13.8057746032556));
#416441=CARTESIAN_POINT('Origin',(0.,2.5406128344257E-15,13.8057746032556));
#416442=CARTESIAN_POINT('',(1.84180085423237,1.96183647465937,13.8390832900376));
#416443=CARTESIAN_POINT('',(1.87419128919243,1.97707132491028,13.8057746032556));
#416444=CARTESIAN_POINT('',(1.76410223015073,2.03198820408293,13.8390832900376));
#416445=CARTESIAN_POINT('Ctrl Pts',(1.84180085423237,1.96183647465937,13.8390832900376));
#416446=CARTESIAN_POINT('Ctrl Pts',(1.83549252267221,1.95886952225828,13.8455641171218));
#416447=CARTESIAN_POINT('Ctrl Pts',(1.82830421112613,1.95692908533012,13.851896480191));
#416448=CARTESIAN_POINT('Ctrl Pts',(1.82056162493321,1.95655028395099,13.8574481026913));
#416449=CARTESIAN_POINT('Ctrl Pts',(1.81532827575582,1.95629424548574,13.8612005412592));
#416450=CARTESIAN_POINT('Ctrl Pts',(1.80971784367031,1.95676363591553,13.8646714234115));
#416451=CARTESIAN_POINT('Ctrl Pts',(1.8040629735423,1.95817702129363,13.8674635290331));
#416452=CARTESIAN_POINT('Ctrl Pts',(1.79950558608912,1.9593161004666,13.8697137499649));
#416453=CARTESIAN_POINT('Ctrl Pts',(1.79481602834688,1.9611085068065,13.8715630732995));
#416454=CARTESIAN_POINT('Ctrl Pts',(1.79038160840693,1.96355511318558,13.8727429581918));
#416455=CARTESIAN_POINT('Ctrl Pts',(1.78589607887065,1.9660299183068,13.873936442031));
#416456=CARTESIAN_POINT('Ctrl Pts',(1.78154380745099,1.96926229482246,13.8744652622107));
#416457=CARTESIAN_POINT('Ctrl Pts',(1.77780613407969,1.97295955217946,13.8742206332401));
#416458=CARTESIAN_POINT('Ctrl Pts',(1.77458888145144,1.97614201617978,13.8740100655633));
#416459=CARTESIAN_POINT('Ctrl Pts',(1.77173896877985,1.9797510131527,13.8732246156103));
#416460=CARTESIAN_POINT('Ctrl Pts',(1.76943516762612,1.98347135535462,13.8719820486038));
#416461=CARTESIAN_POINT('Ctrl Pts',(1.76709166662709,1.98725580769452,13.8707180692815));
#416462=CARTESIAN_POINT('Ctrl Pts',(1.76525277913004,1.99123699860542,13.868960862563));
#416463=CARTESIAN_POINT('Ctrl Pts',(1.76392653127912,1.9951526577661,13.8669057591701));
#416464=CARTESIAN_POINT('Ctrl Pts',(1.76188441468353,2.00118187210117,13.8637413727084));
#416465=CARTESIAN_POINT('Ctrl Pts',(1.76096951083578,2.00723408032072,13.8597962563956));
#416466=CARTESIAN_POINT('Ctrl Pts',(1.76092728742108,2.01291683980706,13.855546950204));
#416467=CARTESIAN_POINT('Ctrl Pts',(1.76087693116042,2.01969418171487,13.850479165618));
#416468=CARTESIAN_POINT('Ctrl Pts',(1.76204843977646,2.02613807476439,13.8448473071436));
#416469=CARTESIAN_POINT('Ctrl Pts',(1.76410223015073,2.03198820408293,13.8390832900376));
#416470=CARTESIAN_POINT('',(1.77595980693977,2.06576154877607,13.8057746032556));
#416471=CARTESIAN_POINT('',(1.76410223015073,2.03198820408293,13.8390832900376));
#416472=CARTESIAN_POINT('',(1.70680540507266,2.12325677238577,13.8057746032556));
#416473=CARTESIAN_POINT('Origin',(0.,2.5406128344257E-15,13.8057746032556));
#416474=CARTESIAN_POINT('',(1.6757645283418,2.10543249369491,13.8390832900376));
#416475=CARTESIAN_POINT('',(1.70680540507266,2.12325677238577,13.8057746032556));
#416476=CARTESIAN_POINT('',(1.59260642281721,2.16901763984444,13.8390832900376));
#416477=CARTESIAN_POINT('Ctrl Pts',(1.6757645283418,2.10543249369491,13.8390832900376));
#416478=CARTESIAN_POINT('Ctrl Pts',(1.66971902139905,2.10196122599733,13.8455641171218));
#416479=CARTESIAN_POINT('Ctrl Pts',(1.66271279199042,2.09944133158894,13.851896480191));
#416480=CARTESIAN_POINT('Ctrl Pts',(1.65502684444336,2.09843269798676,13.8574481026913));
#416481=CARTESIAN_POINT('Ctrl Pts',(1.6498317783155,2.09775094492638,13.8612005412592));
#416482=CARTESIAN_POINT('Ctrl Pts',(1.64420175480229,2.09776147119857,13.8646714234115));
#416483=CARTESIAN_POINT('Ctrl Pts',(1.63845049675859,2.09870922924073,13.8674635290331));
#416484=CARTESIAN_POINT('Ctrl Pts',(1.63381542810891,2.09947304883556,13.8697137499649));
#416485=CARTESIAN_POINT('Ctrl Pts',(1.62899537672661,2.10087724859951,13.8715630732995));
#416486=CARTESIAN_POINT('Ctrl Pts',(1.62437629082011,2.10295426770544,13.8727429581918));
#416487=CARTESIAN_POINT('Ctrl Pts',(1.61970396692098,2.10505522581794,13.873936442031));
#416488=CARTESIAN_POINT('Ctrl Pts',(1.61510270863149,2.10792209634218,13.8744652622107));
#416489=CARTESIAN_POINT('Ctrl Pts',(1.61107611126174,2.1113023963017,13.8742206332401));
#416490=CARTESIAN_POINT('Ctrl Pts',(1.60761016341562,2.11421203495888,13.8740100655633));
#416491=CARTESIAN_POINT('Ctrl Pts',(1.60447556683576,2.11757672895205,13.8732246156103));
#416492=CARTESIAN_POINT('Ctrl Pts',(1.60187618896289,2.12109691084073,13.8719820486038));
#416493=CARTESIAN_POINT('Ctrl Pts',(1.59923201777126,2.12467775364024,13.8707180692815));
#416494=CARTESIAN_POINT('Ctrl Pts',(1.59707474500186,2.12849581106441,13.868960862563));
#416495=CARTESIAN_POINT('Ctrl Pts',(1.59543374755844,2.13229033968011,13.8669057591701));
#416496=CARTESIAN_POINT('Ctrl Pts',(1.59290698899657,2.13813304084123,13.8637413727084));
#416497=CARTESIAN_POINT('Ctrl Pts',(1.59150181826004,2.14409053768006,13.8597962563956));
#416498=CARTESIAN_POINT('Ctrl Pts',(1.59099653768597,2.14975094665272,13.855546950204));
#416499=CARTESIAN_POINT('Ctrl Pts',(1.59039393269836,2.15650163301169,13.850479165618));
#416500=CARTESIAN_POINT('Ctrl Pts',(1.59103630611039,2.16301957336664,13.8448473071436));
#416501=CARTESIAN_POINT('Ctrl Pts',(1.59260642281721,2.16901763984444,13.8390832900376));
#416502=CARTESIAN_POINT('',(1.60167170336874,2.2036451091079,13.8057746032556));
#416503=CARTESIAN_POINT('',(1.59260642281721,2.16901763984444,13.8390832900376));
#416504=CARTESIAN_POINT('',(1.5280610125852,2.25531229635374,13.8057746032556));
#416505=CARTESIAN_POINT('Origin',(0.,2.5406128344257E-15,13.8057746032556));
#416506=CARTESIAN_POINT('',(1.49857626599681,2.23501720685682,13.8390832900376));
#416507=CARTESIAN_POINT('',(1.5280610125852,2.25531229635374,13.8057746032556));
#416508=CARTESIAN_POINT('',(1.41051208250141,2.2916126210755,13.8390832900376));
#416509=CARTESIAN_POINT('Ctrl Pts',(1.49857626599681,2.23501720685682,13.8390832900376));
#416510=CARTESIAN_POINT('Ctrl Pts',(1.49283381552271,2.23106472457656,13.8455641171218));
#416511=CARTESIAN_POINT('Ctrl Pts',(1.48605629355232,2.22798214216948,13.851896480191));
#416512=CARTESIAN_POINT('Ctrl Pts',(1.47847813336395,2.22635038863446,13.8574481026913));
#416513=CARTESIAN_POINT('Ctrl Pts',(1.47335592259357,2.22524745793309,13.8612005412592));
#416514=CARTESIAN_POINT('Ctrl Pts',(1.46774377453025,2.22479904999705,13.8646714234115));
#416515=CARTESIAN_POINT('Ctrl Pts',(1.46193440224425,2.22527487352988,13.8674635290331));
#416516=CARTESIAN_POINT('Ctrl Pts',(1.4572524980152,2.2256583504532,13.8697137499649));
#416517=CARTESIAN_POINT('Ctrl Pts',(1.45233402963954,2.22666499892343,13.8715630732995));
#416518=CARTESIAN_POINT('Ctrl Pts',(1.44756101702111,2.22835860853675,13.8727429581918));
#416519=CARTESIAN_POINT('Ctrl Pts',(1.4427329923038,2.23007173811093,13.873936442031));
#416520=CARTESIAN_POINT('Ctrl Pts',(1.43791336775924,2.23255402409341,13.8744652622107));
#416521=CARTESIAN_POINT('Ctrl Pts',(1.43362464273219,2.23559487131693,13.8742206332401));
#416522=CARTESIAN_POINT('Ctrl Pts',(1.42993306497928,2.23821232146575,13.8740100655633));
#416523=CARTESIAN_POINT('Ctrl Pts',(1.42653464471422,2.2413103209958,13.8732246156103));
#416524=CARTESIAN_POINT('Ctrl Pts',(1.42365698855308,2.24460691634155,13.8719820486038));
#416525=CARTESIAN_POINT('Ctrl Pts',(1.42072974369188,2.24796031968264,13.8707180692815));
#416526=CARTESIAN_POINT('Ctrl Pts',(1.41826844194447,2.25158983507785,13.868960862563));
#416527=CARTESIAN_POINT('Ctrl Pts',(1.41632361547581,2.25523798118669,13.8669057591701));
#416528=CARTESIAN_POINT('Ctrl Pts',(1.41332903010898,2.26085528696161,13.8637413727084));
#416529=CARTESIAN_POINT('Ctrl Pts',(1.4114429436631,2.26667842626117,13.8597962563956));
#416530=CARTESIAN_POINT('Ctrl Pts',(1.41047796848851,2.27227881563235,13.855546950204));
#416531=CARTESIAN_POINT('Ctrl Pts',(1.40932712501071,2.27895792173855,13.850479165618));
#416532=CARTESIAN_POINT('Ctrl Pts',(1.40943608832967,2.28550653358124,13.8448473071436));
#416533=CARTESIAN_POINT('Ctrl Pts',(1.41051208250141,2.2916126210755,13.8390832900376));
#416534=CARTESIAN_POINT('',(1.41672473886902,2.32686377481446,13.8057746032556));
#416535=CARTESIAN_POINT('',(1.41051208250141,2.2916126210755,13.8390832900376));
#416536=CARTESIAN_POINT('',(1.33914762617131,2.37235908908981,13.8057746032556));
#416537=CARTESIAN_POINT('Origin',(0.,2.5406128344257E-15,13.8057746032556));
#416538=CARTESIAN_POINT('',(1.31141522584929,2.34972824925897,13.8390832900376));
#416539=CARTESIAN_POINT('',(1.33914762617131,2.37235908908981,13.8057746032556));
#416540=CARTESIAN_POINT('',(1.21903101699467,2.39895729840277,13.8390832900376));
#416541=CARTESIAN_POINT('Ctrl Pts',(1.31141522584929,2.34972824925897,13.8390832900376));
#416542=CARTESIAN_POINT('Ctrl Pts',(1.30601404690432,2.3453208555135,13.8455641171218));
#416543=CARTESIAN_POINT('Ctrl Pts',(1.29951033566265,2.34169609918505,13.851896480191));
#416544=CARTESIAN_POINT('Ctrl Pts',(1.29209039423872,2.33945208476775,13.8574481026913));
#416545=CARTESIAN_POINT('Ctrl Pts',(1.2870751262934,2.33793531624723,13.8612005412592));
#416546=CARTESIAN_POINT('Ctrl Pts',(1.28151820159939,2.33703095818381,13.8646714234115));
#416547=CARTESIAN_POINT('Ctrl Pts',(1.27568937548518,2.3370316806802,13.8674635290331));
#416548=CARTESIAN_POINT('Ctrl Pts',(1.27099179297695,2.33703226295634,13.8697137499649));
#416549=CARTESIAN_POINT('Ctrl Pts',(1.26600763920347,2.33763466105338,13.8715630732995));
#416550=CARTESIAN_POINT('Ctrl Pts',(1.26111246348459,2.33893359048154,13.8727429581918));
#416551=CARTESIAN_POINT('Ctrl Pts',(1.25616086765703,2.34024749092273,13.873936442031));
#416552=CARTESIAN_POINT('Ctrl Pts',(1.25115495066356,2.34232867315978,13.8744652622107));
#416553=CARTESIAN_POINT('Ctrl Pts',(1.24663263873668,2.34500983131073,13.8742206332401));
#416554=CARTESIAN_POINT('Ctrl Pts',(1.24273999791786,2.34731767425231,13.8740100655633));
#416555=CARTESIAN_POINT('Ctrl Pts',(1.23910036989375,2.35012836264349,13.8732246156103));
#416556=CARTESIAN_POINT('Ctrl Pts',(1.23596358577132,2.35317943314819,13.8719820486038));
#416557=CARTESIAN_POINT('Ctrl Pts',(1.23277274757214,2.3562830806849,13.8707180692815));
#416558=CARTESIAN_POINT('Ctrl Pts',(1.23002379640377,2.35969990022501,13.868960862563));
#416559=CARTESIAN_POINT('Ctrl Pts',(1.22778808340914,2.36317738601655,13.8669057591701));
#416560=CARTESIAN_POINT('Ctrl Pts',(1.22434559970891,2.36853191416212,13.8637413727084));
#416561=CARTESIAN_POINT('Ctrl Pts',(1.22199114914778,2.37418194389113,13.8597962563956));
#416562=CARTESIAN_POINT('Ctrl Pts',(1.22057290112324,2.37968504399355,13.855546950204));
#416563=CARTESIAN_POINT('Ctrl Pts',(1.21888147782873,2.38624812149782,13.850479165618));
#416564=CARTESIAN_POINT('Ctrl Pts',(1.21845630592171,2.39278382489689,13.8448473071436));
#416565=CARTESIAN_POINT('Ctrl Pts',(1.21903101699467,2.39895729840277,13.8390832900376));
#416566=CARTESIAN_POINT('',(1.22234970497526,2.43459754600513,13.8057746032556));
#416567=CARTESIAN_POINT('',(1.21903101699467,2.39895729840277,13.8390832900376));
#416568=CARTESIAN_POINT('',(1.14132243324905,2.47361822349969,13.8057746032556));
#416569=CARTESIAN_POINT('Origin',(0.,2.5406128344257E-15,13.8057746032556));
#416570=CARTESIAN_POINT('',(1.11552693374202,2.44880223784019,13.8390832900376));
#416571=CARTESIAN_POINT('',(1.14132243324905,2.47361822349969,13.8057746032556));
#416572=CARTESIAN_POINT('',(1.01943750119579,2.49033731070927,13.8390832900376));
#416573=CARTESIAN_POINT('Ctrl Pts',(1.11552693374202,2.44880223784019,13.8390832900376));
#416574=CARTESIAN_POINT('Ctrl Pts',(1.11050297028093,2.44396926310771,13.8455641171218));
#416575=CARTESIAN_POINT('Ctrl Pts',(1.10431635089327,2.43982645501321,13.851896480191));
#416576=CARTESIAN_POINT('Ctrl Pts',(1.09710400671974,2.43698511325934,13.8574481026913));
#416577=CARTESIAN_POINT('Ctrl Pts',(1.0922290573802,2.43506460076393,13.8612005412592));
#416578=CARTESIAN_POINT('Ctrl Pts',(1.08676433647251,2.43371031092683,13.8646714234115));
#416579=CARTESIAN_POINT('Ctrl Pts',(1.08095484640619,2.43323592757868,13.8674635290331));
#416580=CARTESIAN_POINT('Ctrl Pts',(1.07627284725532,2.43285361133269,13.8697137499649));
#416581=CARTESIAN_POINT('Ctrl Pts',(1.07125617680505,2.4330477501966,13.8715630732995));
#416582=CARTESIAN_POINT('Ctrl Pts',(1.06627141457249,2.43394335527855,13.8727429581918));
#416583=CARTESIAN_POINT('Ctrl Pts',(1.06122919968795,2.43484928279609,13.873936442031));
#416584=CARTESIAN_POINT('Ctrl Pts',(1.05607030379724,2.43651551136331,13.8744652622107));
#416585=CARTESIAN_POINT('Ctrl Pts',(1.05134450021028,2.43881913777655,13.8742206332401));
#416586=CARTESIAN_POINT('Ctrl Pts',(1.04727670120795,2.44080201519688,13.8740100655633));
#416587=CARTESIAN_POINT('Ctrl Pts',(1.04342008654881,2.44330668778168,13.8732246156103));
#416588=CARTESIAN_POINT('Ctrl Pts',(1.04004504924589,2.44609192907451,13.8719820486038));
#416589=CARTESIAN_POINT('Ctrl Pts',(1.0366118522105,2.44892516654454,13.8707180692815));
#416590=CARTESIAN_POINT('Ctrl Pts',(1.03359354543764,2.45210655185927,13.868960862563));
#416591=CARTESIAN_POINT('Ctrl Pts',(1.03108182421815,2.45539023523929,13.8669057591701));
#416592=CARTESIAN_POINT('Ctrl Pts',(1.02721435134557,2.46044635225415,13.8637413727084));
#416593=CARTESIAN_POINT('Ctrl Pts',(1.02440720514922,2.46588567239695,13.8597962563956));
#416594=CARTESIAN_POINT('Ctrl Pts',(1.02254512248136,2.47125486100738,13.855546950204));
#416595=CARTESIAN_POINT('Ctrl Pts',(1.02032437551309,2.47765823371176,13.850479165618));
#416596=CARTESIAN_POINT('Ctrl Pts',(1.01936789782898,2.4841375346394,13.8448473071436));
#416597=CARTESIAN_POINT('Ctrl Pts',(1.01943750119579,2.49033731070927,13.8390832900376));
#416598=CARTESIAN_POINT('',(1.01984013546839,2.52612947220745,13.8057746032556));
#416599=CARTESIAN_POINT('',(1.01943750119579,2.49033731070927,13.8390832900376));
#416600=CARTESIAN_POINT('',(0.935901927838467,2.55841583675045,13.8057746032556));
#416601=CARTESIAN_POINT('Origin',(0.,2.5406128344257E-15,13.8057746032556));
#416602=CARTESIAN_POINT('',(0.912214993939689,2.5315798515525,13.8390832900376));
#416603=CARTESIAN_POINT('',(0.935901927838467,2.55841583675045,13.8057746032556));
#416604=CARTESIAN_POINT('',(0.813059797021804,2.56514453908973,13.8390832900376));
#416605=CARTESIAN_POINT('Ctrl Pts',(0.912214993939688,2.5315798515525,13.8390832900376));
#416606=CARTESIAN_POINT('Ctrl Pts',(0.907601679610414,2.52635345848247,
13.8455641171218));
#416607=CARTESIAN_POINT('Ctrl Pts',(0.901773323008058,2.52172016832629,
13.851896480191));
#416608=CARTESIAN_POINT('Ctrl Pts',(0.894816573045464,2.51830040789643,
13.8574481026913));
#416609=CARTESIAN_POINT('Ctrl Pts',(0.890114384295236,2.51598893211992,
13.8612005412592));
#416610=CARTESIAN_POINT('Ctrl Pts',(0.884778233989902,2.51419372308456,
13.8646714234115));
#416611=CARTESIAN_POINT('Ctrl Pts',(0.879026741169359,2.51324739083479,
13.8674635290331));
#416612=CARTESIAN_POINT('Ctrl Pts',(0.874391483307722,2.51248472031822,
13.8697137499649));
#416613=CARTESIAN_POINT('Ctrl Pts',(0.869375681294828,2.51226930798688,
13.8715630732995));
#416614=CARTESIAN_POINT('Ctrl Pts',(0.864334505318809,2.51275562861857,
13.8727429581918));
#416615=CARTESIAN_POINT('Ctrl Pts',(0.859235226485449,2.51324755441431,
13.873936442031));
#416616=CARTESIAN_POINT('Ctrl Pts',(0.853957683298495,2.51448774083547,
13.8744652622107));
#416617=CARTESIAN_POINT('Ctrl Pts',(0.849059837494611,2.5163985052573,13.8742206332401));
#416618=CARTESIAN_POINT('Ctrl Pts',(0.844843950840004,2.5180432214343,13.8740100655633));
#416619=CARTESIAN_POINT('Ctrl Pts',(0.840796014680084,2.52022521002991,
13.8732246156103));
#416620=CARTESIAN_POINT('Ctrl Pts',(0.837205184513088,2.5227260867896,13.8719820486038));
#416621=CARTESIAN_POINT('Ctrl Pts',(0.833552476001309,2.52527005946504,
13.8707180692815));
#416622=CARTESIAN_POINT('Ctrl Pts',(0.830284899957549,2.52819483896,13.868960862563));
#416623=CARTESIAN_POINT('Ctrl Pts',(0.827513885603518,2.53126286755739,
13.8669057591701));
#416624=CARTESIAN_POINT('Ctrl Pts',(0.823247160952463,2.535986925817,13.8637413727084));
#416625=CARTESIAN_POINT('Ctrl Pts',(0.820006000215689,2.54117933859546,
13.8597962563956));
#416626=CARTESIAN_POINT('Ctrl Pts',(0.817712474757428,2.54637888464955,
13.855546950204));
#416627=CARTESIAN_POINT('Ctrl Pts',(0.814977182820077,2.55257993916518,
13.850479165618));
#416628=CARTESIAN_POINT('Ctrl Pts',(0.813495764560061,2.55895971894273,
13.8448473071436));
#416629=CARTESIAN_POINT('Ctrl Pts',(0.813059797021804,2.56514453908973,
13.8390832900376));
#416630=CARTESIAN_POINT('',(0.810543698121754,2.60085042355426,13.8057746032556));
#416631=CARTESIAN_POINT('',(0.813059797021804,2.56514453908973,13.8390832900376));
#416632=CARTESIAN_POINT('',(0.72425314951107,2.62618761471654,13.8057746032556));
#416633=CARTESIAN_POINT('Origin',(0.,2.5406128344257E-15,13.8057746032556));
#416634=CARTESIAN_POINT('',(0.702832413857569,2.59751021903401,13.8390832900376));
#416635=CARTESIAN_POINT('',(0.72425314951107,2.62618761471654,13.8057746032556));
#416636=CARTESIAN_POINT('',(0.601271314044061,2.6228811537816,13.8390832900376));
#416637=CARTESIAN_POINT('Ctrl Pts',(0.702832413857569,2.59751021903401,
13.8390832900376));
#416638=CARTESIAN_POINT('Ctrl Pts',(0.698660449505827,2.59192518841002,
13.8455641171218));
#416639=CARTESIAN_POINT('Ctrl Pts',(0.693229142440357,2.58683224997369,
13.851896480191));
#416640=CARTESIAN_POINT('Ctrl Pts',(0.686574282711912,2.58285682880929,
13.8574481026913));
#416641=CARTESIAN_POINT('Ctrl Pts',(0.682076146841327,2.58016977224161,
13.8612005412592));
#416642=CARTESIAN_POINT('Ctrl Pts',(0.676904078338221,2.57794559082794,
13.8646714234115));
#416643=CARTESIAN_POINT('Ctrl Pts',(0.67124885799925,2.57653360736153,13.8674635290331));
#416644=CARTESIAN_POINT('Ctrl Pts',(0.666691188303154,2.57539565802083,
13.8697137499649));
#416645=CARTESIAN_POINT('Ctrl Pts',(0.661709634062478,2.57477212802776,
13.8715630732995));
#416646=CARTESIAN_POINT('Ctrl Pts',(0.656645592537388,2.57484592782563,
13.8727429581918));
#416647=CARTESIAN_POINT('Ctrl Pts',(0.651523184614516,2.57492057821455,
13.873936442031));
#416648=CARTESIAN_POINT('Ctrl Pts',(0.6461621153105,2.57572646925365,13.8744652622107));
#416649=CARTESIAN_POINT('Ctrl Pts',(0.641124821645433,2.57723165586209,
13.8742206332401));
#416650=CARTESIAN_POINT('Ctrl Pts',(0.636788903368657,2.57852726548096,
13.8740100655633));
#416651=CARTESIAN_POINT('Ctrl Pts',(0.632576584055241,2.58037204931328,
13.8732246156103));
#416652=CARTESIAN_POINT('Ctrl Pts',(0.628793857406481,2.58257191861761,
13.8719820486038));
#416653=CARTESIAN_POINT('Ctrl Pts',(0.624945945590808,2.58480969678004,
13.8707180692815));
#416654=CARTESIAN_POINT('Ctrl Pts',(0.621450845455611,2.58745840653024,
13.868960862563));
#416655=CARTESIAN_POINT('Ctrl Pts',(0.618438978610375,2.59029036312087,
13.8669057591701));
#416656=CARTESIAN_POINT('Ctrl Pts',(0.61380139652944,2.59465092479693,13.8637413727084));
#416657=CARTESIAN_POINT('Ctrl Pts',(0.610147790642189,2.59956187556069,
13.8597962563956));
#416658=CARTESIAN_POINT('Ctrl Pts',(0.607438085427048,2.60455717693733,
13.855546950204));
#416659=CARTESIAN_POINT('Ctrl Pts',(0.604206451437169,2.61051464626949,
13.850479165618));
#416660=CARTESIAN_POINT('Ctrl Pts',(0.602209951195348,2.61675244851512,
13.8448473071436));
#416661=CARTESIAN_POINT('Ctrl Pts',(0.601271314044061,2.6228811537816,13.8390832900376));
#416662=CARTESIAN_POINT('',(0.595853226194419,2.65826314444243,13.8057746032556));
#416663=CARTESIAN_POINT('',(0.601271314044061,2.6228811537816,13.8390832900376));
#416664=CARTESIAN_POINT('',(0.507784585967034,2.67648254739715,13.8057746032556));
#416665=CARTESIAN_POINT('Origin',(0.,2.5406128344257E-15,13.8057746032556));
#416666=CARTESIAN_POINT('',(0.488772600020414,2.64615458456687,13.8390832900376));
#416667=CARTESIAN_POINT('',(0.507784585967034,2.67648254739715,13.8057746032556));
#416668=CARTESIAN_POINT('',(0.385481469674138,2.66316292713999,13.8390832900376));
#416669=CARTESIAN_POINT('Ctrl Pts',(0.488772600020413,2.64615458456687,
13.8390832900376));
#416670=CARTESIAN_POINT('Ctrl Pts',(0.48506974938064,2.64024808384625,13.8455641171218));
#416671=CARTESIAN_POINT('Ctrl Pts',(0.48007163630447,2.6347293897948,13.851896480191));
#416672=CARTESIAN_POINT('Ctrl Pts',(0.473762953803692,2.6302247636678,13.8574481026913));
#416673=CARTESIAN_POINT('Ctrl Pts',(0.469498805164829,2.62718000822708,
13.8612005412592));
#416674=CARTESIAN_POINT('Ctrl Pts',(0.46452523772651,2.62454165599543,13.8646714234115));
#416675=CARTESIAN_POINT('Ctrl Pts',(0.459003924427422,2.62267341782939,
13.8674635290331));
#416676=CARTESIAN_POINT('Ctrl Pts',(0.454554173436733,2.62116776252968,
13.8697137499649));
#416677=CARTESIAN_POINT('Ctrl Pts',(0.449640018389848,2.62014026436412,
13.8715630732995));
#416678=CARTESIAN_POINT('Ctrl Pts',(0.444586811676528,2.61980105220269,
13.8727429581918));
#416679=CARTESIAN_POINT('Ctrl Pts',(0.439475363443734,2.61945793039877,
13.873936442031));
#416680=CARTESIAN_POINT('Ctrl Pts',(0.434066445054353,2.6198241629839,13.8744652622107));
#416681=CARTESIAN_POINT('Ctrl Pts',(0.428923225886351,2.62091375501042,
13.8742206332401));
#416682=CARTESIAN_POINT('Ctrl Pts',(0.424496130808162,2.6218516360029,13.8740100655633));
#416683=CARTESIAN_POINT('Ctrl Pts',(0.420147460631299,2.62334693833989,
13.8732246156103));
#416684=CARTESIAN_POINT('Ctrl Pts',(0.416198010922517,2.62523116042159,
13.8719820486038));
#416685=CARTESIAN_POINT('Ctrl Pts',(0.412180503021224,2.62714785202654,
13.8707180692815));
#416686=CARTESIAN_POINT('Ctrl Pts',(0.408481138109338,2.6295028653056,13.868960862563));
#416687=CARTESIAN_POINT('Ctrl Pts',(0.405248462249829,2.63207990368561,
13.8669057591701));
#416688=CARTESIAN_POINT('Ctrl Pts',(0.400270885082617,2.63604794995961,
13.8637413727084));
#416689=CARTESIAN_POINT('Ctrl Pts',(0.396229148189263,2.64064475714159,
13.8597962563956));
#416690=CARTESIAN_POINT('Ctrl Pts',(0.39312129585838,2.64540257093427,13.855546950204));
#416691=CARTESIAN_POINT('Ctrl Pts',(0.389414825806991,2.65107680910749,
13.850479165618));
#416692=CARTESIAN_POINT('Ctrl Pts',(0.386916529963079,2.65713112227642,
13.8448473071436));
#416693=CARTESIAN_POINT('Ctrl Pts',(0.385481469674138,2.66316292713999,
13.8390832900376));
#416694=CARTESIAN_POINT('',(0.377197449355622,2.69798556268689,13.8057746032556));
#416695=CARTESIAN_POINT('',(0.385481469674138,2.66316292713999,13.8390832900376));
#416696=CARTESIAN_POINT('',(0.287936799781948,2.70896593031337,13.8057746032556));
#416697=CARTESIAN_POINT('Origin',(0.,2.5406128344257E-15,13.8057746032556));
#416698=CARTESIAN_POINT('',(0.271460085171925,2.67718922792421,13.8390832900376));
#416699=CARTESIAN_POINT('',(0.287936799781948,2.70896593031337,13.8057746032556));
#416700=CARTESIAN_POINT('',(0.1671263097235,2.68572179060922,13.8390832900376));
#416701=CARTESIAN_POINT('Ctrl Pts',(0.271460085171925,2.67718922792421,
13.8390832900376));
#416702=CARTESIAN_POINT('Ctrl Pts',(0.268250990104199,2.67100056389476,
13.8455641171218));
#416703=CARTESIAN_POINT('Ctrl Pts',(0.263719332635224,2.66509284022658,
13.851896480191));
#416704=CARTESIAN_POINT('Ctrl Pts',(0.257798810603297,2.66008898668065,
13.8574481026913));
#416705=CARTESIAN_POINT('Ctrl Pts',(0.253797026401811,2.65670679471198,
13.8612005412592));
#416706=CARTESIAN_POINT('Ctrl Pts',(0.249055058299,2.65367182946117,13.8646714234115));
#416707=CARTESIAN_POINT('Ctrl Pts',(0.243704395468847,2.65135976941226,
13.8674635290331));
#416708=CARTESIAN_POINT('Ctrl Pts',(0.239392175542249,2.64949642804114,
13.8697137499649));
#416709=CARTESIAN_POINT('Ctrl Pts',(0.234578122580215,2.64807179953385,
13.8715630732995));
#416710=CARTESIAN_POINT('Ctrl Pts',(0.229569378935621,2.64732183281409,
13.8727429581918));
#416711=CARTESIAN_POINT('Ctrl Pts',(0.224502906237564,2.64656322223632,
13.873936442031));
#416712=CARTESIAN_POINT('Ctrl Pts',(0.219082134222294,2.64648735915005,
13.8744652622107));
#416713=CARTESIAN_POINT('Ctrl Pts',(0.213867216826347,2.64715410553948,
13.8742206332401));
#416714=CARTESIAN_POINT('Ctrl Pts',(0.209378406534072,2.64772801646231,
13.8740100655633));
#416715=CARTESIAN_POINT('Ctrl Pts',(0.204922325176305,2.64886388631363,
13.8732246156103));
#416716=CARTESIAN_POINT('Ctrl Pts',(0.2008324353437,2.65041992198562,13.8719820486038));
#416717=CARTESIAN_POINT('Ctrl Pts',(0.196672067209027,2.65200277176669,
13.8707180692815));
#416718=CARTESIAN_POINT('Ctrl Pts',(0.192793056183592,2.6540484163498,13.868960862563));
#416719=CARTESIAN_POINT('Ctrl Pts',(0.1893610842343,2.65635338675394,13.8669057591701));
#416720=CARTESIAN_POINT('Ctrl Pts',(0.184076636935616,2.6599025109326,13.8637413727084));
#416721=CARTESIAN_POINT('Ctrl Pts',(0.179673666128347,2.66415458353943,
13.8597962563956));
#416722=CARTESIAN_POINT('Ctrl Pts',(0.176188348926224,2.66864324728235,
13.855546950204));
#416723=CARTESIAN_POINT('Ctrl Pts',(0.172031708759995,2.67399649317776,
13.850479165618));
#416724=CARTESIAN_POINT('Ctrl Pts',(0.169048243060639,2.67982702681473,
13.8448473071436));
#416725=CARTESIAN_POINT('Ctrl Pts',(0.1671263097235,2.68572179060922,13.8390832900376));
#416726=CARTESIAN_POINT('',(0.156031485724562,2.71975333214795,13.8057746032556));
#416727=CARTESIAN_POINT('',(0.1671263097235,2.68572179060922,13.8390832900376));
#416728=CARTESIAN_POINT('',(0.0661728417005766,2.72342159191127,13.8057746032556));
#416729=CARTESIAN_POINT('Origin',(0.,2.5406128344257E-15,13.8057746032556));
#416730=CARTESIAN_POINT('',(0.0523410482444132,2.69040761867485,13.8390832900376));
#416731=CARTESIAN_POINT('',(0.0661728417005766,2.72342159191127,13.8057746032556));
#416732=CARTESIAN_POINT('Ctrl Pts',(0.0523410482444132,2.69040761867485,
13.8390832900376));
#416733=CARTESIAN_POINT('Ctrl Pts',(0.0496470647469476,2.68397797587462,
13.8455641171218));
#416734=CARTESIAN_POINT('Ctrl Pts',(0.0456120587089066,2.67772051809082,
13.851896480191));
#416735=CARTESIAN_POINT('Ctrl Pts',(0.0401285192509084,2.67226017679703,
13.8574385412955));
#416736=CARTESIAN_POINT('Ctrl Pts',(0.0364062442971185,2.66855364896174,
13.8612005412592));
#416737=CARTESIAN_POINT('Ctrl Pts',(0.031927461700894,2.66514225178075,
13.8646714234115));
#416738=CARTESIAN_POINT('Ctrl Pts',(0.0267845789591358,2.66240257155708,
13.8674627013498));
#416739=CARTESIAN_POINT('Ctrl Pts',(0.0226370596760621,2.66019313433526,
13.8697137499649));
#416740=CARTESIAN_POINT('Ctrl Pts',(0.0179551393667713,2.65838087216932,
13.8715630732995));
#416741=CARTESIAN_POINT('Ctrl Pts',(0.0130142993447968,2.657222802874,13.8727453272031));
#416742=CARTESIAN_POINT('Ctrl Pts',(0.0088450433803829,2.6562455829488,
13.8737429549582));
#416743=CARTESIAN_POINT('Ctrl Pts',(0.00439692111021513,2.65571825406977,
13.8742817459302));
#416744=CARTESIAN_POINT('Ctrl Pts',(3.72770476910004E-12,2.65571825406948,
13.8742817459305));
#416745=CARTESIAN_POINT('Origin',(0.,2.60208521396521E-15,13.912));
#416746=CARTESIAN_POINT('',(-3.05371705427032E-16,2.49354920651117,14.));
#416747=CARTESIAN_POINT('Origin',(0.,2.5406128344257E-15,14.));
#416748=CARTESIAN_POINT('Origin',(-3.05371705427032E-16,2.49354920651117,
13.912));
#416749=CARTESIAN_POINT('Origin',(0.,2.5406128344257E-15,14.));
#416750=CARTESIAN_POINT('',(-0.037827685004575,-2.74973981791863,13.7435492065112));
#416751=CARTESIAN_POINT('',(0.0378276850046121,-2.74973981791863,13.7435492065112));
#416752=CARTESIAN_POINT('Origin',(0.,2.5406128344257E-15,13.7435492065112));
#416753=CARTESIAN_POINT('',(-0.037827685004575,-2.74973981791863,12.5369868989719));
#416754=CARTESIAN_POINT('',(-0.037827685004575,-2.74973981791863,14.));
#416755=CARTESIAN_POINT('Ctrl Pts',(-0.0729573509223692,-2.74903205236796,
12.4908873016278));
#416756=CARTESIAN_POINT('Ctrl Pts',(-0.0707767921054796,-2.74908992284447,
12.4908873016278));
#416757=CARTESIAN_POINT('Ctrl Pts',(-0.0685838718709331,-2.74914546989179,
12.4911020829134));
#416758=CARTESIAN_POINT('Ctrl Pts',(-0.0664485864717655,-2.74919708012283,
12.4915448903141));
#416759=CARTESIAN_POINT('Ctrl Pts',(-0.0627953733565572,-2.749285378939,
12.4923024798169));
#416760=CARTESIAN_POINT('Ctrl Pts',(-0.0592269615777823,-2.7493639210411,
12.4937722312795));
#416761=CARTESIAN_POINT('Ctrl Pts',(-0.0560965908340369,-2.74942779001319,
12.4958030942394));
#416762=CARTESIAN_POINT('Ctrl Pts',(-0.0529883153033171,-2.74949120817652,
12.4978196226833));
#416763=CARTESIAN_POINT('Ctrl Pts',(-0.0502197797679206,-2.74954236051975,
12.5004326847668));
#416764=CARTESIAN_POINT('Ctrl Pts',(-0.0479357073569643,-2.74958218061585,
12.5033504258767));
#416765=CARTESIAN_POINT('Ctrl Pts',(-0.0452066442771379,-2.749629758597,
12.5068366111226));
#416766=CARTESIAN_POINT('Ctrl Pts',(-0.0430813958680921,-2.7496629604294,
12.5108395010833));
#416767=CARTESIAN_POINT('Ctrl Pts',(-0.0415315315886475,-2.7496863697309,
12.5149868989719));
#416768=CARTESIAN_POINT('Ctrl Pts',(-0.0389283867661261,-2.74972568788464,
12.5219528491417));
#416769=CARTESIAN_POINT('Ctrl Pts',(-0.0378276849660689,-2.74973981791945,
12.5295503425868));
#416770=CARTESIAN_POINT('Ctrl Pts',(-0.037827685004575,-2.74973981791863,
12.5369868989719));
#416771=CARTESIAN_POINT('',(-0.186427505996059,-2.74367359301505,12.5369868989719));
#416772=CARTESIAN_POINT('Ctrl Pts',(-0.186427505996059,-2.74367359301504,
12.5369868989719));
#416773=CARTESIAN_POINT('Ctrl Pts',(-0.186427505996057,-2.74367359301504,
12.5309445149785));
#416774=CARTESIAN_POINT('Ctrl Pts',(-0.185705362546179,-2.74372306599812,
12.5248274368704));
#416775=CARTESIAN_POINT('Ctrl Pts',(-0.184052403196883,-2.74383394411496,
12.5190199595513));
#416776=CARTESIAN_POINT('Ctrl Pts',(-0.182664021058617,-2.74392707477603,
12.5141420429941));
#416777=CARTESIAN_POINT('Ctrl Pts',(-0.180576035463166,-2.74406644051104,
12.5093757677094));
#416778=CARTESIAN_POINT('Ctrl Pts',(-0.177695111376414,-2.74425298531183,
12.5051960112707));
#416779=CARTESIAN_POINT('Ctrl Pts',(-0.175770455473429,-2.7443776100993,
12.5024036458141));
#416780=CARTESIAN_POINT('Ctrl Pts',(-0.173445221259834,-2.74452614690824,
12.4998248032393));
#416781=CARTESIAN_POINT('Ctrl Pts',(-0.170801591843253,-2.74469065947764,
12.4976950015772));
#416782=CARTESIAN_POINT('Ctrl Pts',(-0.168083475609416,-2.74485980734789,
12.495505190692));
#416783=CARTESIAN_POINT('Ctrl Pts',(-0.164958669846826,-2.74504999977299,
12.4937456938368));
#416784=CARTESIAN_POINT('Ctrl Pts',(-0.161668310532495,-2.74524377011761,
12.4925987732155));
#416785=CARTESIAN_POINT('Ctrl Pts',(-0.158378721149558,-2.74543749512071,
12.4914521209692));
#416786=CARTESIAN_POINT('Ctrl Pts',(-0.154841629042532,-2.74563949730457,
12.4908873016276));
#416787=CARTESIAN_POINT('Ctrl Pts',(-0.151357041680656,-2.74583157639606,
12.4908873016278));
#416788=CARTESIAN_POINT('',(-0.186427505996058,-2.74367359301505,13.7435492065112));
#416789=CARTESIAN_POINT('',(-0.186427505996058,-2.74367359301505,14.));
#416790=CARTESIAN_POINT('',(-0.261831139002666,-2.73750697800911,13.7435492065112));
#416791=CARTESIAN_POINT('Origin',(0.,2.5406128344257E-15,13.7435492065112));
#416792=CARTESIAN_POINT('',(-0.261831139002667,-2.73750697800911,12.5369868989719));
#416793=CARTESIAN_POINT('',(-0.261831139002667,-2.73750697800911,14.));
#416794=CARTESIAN_POINT('Ctrl Pts',(-0.296786224392158,-2.73393817358971,
12.4908873016278));
#416795=CARTESIAN_POINT('Ctrl Pts',(-0.294617638185927,-2.73417358729388,
12.4908873016278));
#416796=CARTESIAN_POINT('Ctrl Pts',(-0.292436542312588,-2.73440769287018,
12.4911020829134));
#416797=CARTESIAN_POINT('Ctrl Pts',(-0.290312568612394,-2.73463317695549,
12.4915448903141));
#416798=CARTESIAN_POINT('Ctrl Pts',(-0.286678708435701,-2.7350189527483,
12.4923024798169));
#416799=CARTESIAN_POINT('Ctrl Pts',(-0.283128572163218,-2.73538809219552,
12.4937722312795));
#416800=CARTESIAN_POINT('Ctrl Pts',(-0.28001382338404,-2.73570690292543,
12.4958030942394));
#416801=CARTESIAN_POINT('Ctrl Pts',(-0.276921059552791,-2.73602346338163,
12.4978196226833));
#416802=CARTESIAN_POINT('Ctrl Pts',(-0.274165905481849,-2.73630010686762,
12.5004326847668));
#416803=CARTESIAN_POINT('Ctrl Pts',(-0.271892678840921,-2.73652596757143,
12.5033504258767));
#416804=CARTESIAN_POINT('Ctrl Pts',(-0.269176574540517,-2.73679583121716,
12.5068366111226));
#416805=CARTESIAN_POINT('Ctrl Pts',(-0.267061103977803,-2.73700215004838,
12.5108395010833));
#416806=CARTESIAN_POINT('Ctrl Pts',(-0.265518304819288,-2.73715180978438,
12.5149868989719));
#416807=CARTESIAN_POINT('Ctrl Pts',(-0.262927026540961,-2.73740317757966,
12.5219528491417));
#416808=CARTESIAN_POINT('Ctrl Pts',(-0.261831138964355,-2.73750697801306,
12.5295503425868));
#416809=CARTESIAN_POINT('Ctrl Pts',(-0.261831139002667,-2.73750697800911,
12.5369868989719));
#416810=CARTESIAN_POINT('',(-0.409442052702697,-2.71934867302423,12.5369868989719));
#416811=CARTESIAN_POINT('Ctrl Pts',(-0.409442052702696,-2.71934867302422,
12.5369868989719));
#416812=CARTESIAN_POINT('Ctrl Pts',(-0.409442052702695,-2.71934867302422,
12.5309445149785));
#416813=CARTESIAN_POINT('Ctrl Pts',(-0.408726344632979,-2.71945684278525,
12.5248274368704));
#416814=CARTESIAN_POINT('Ctrl Pts',(-0.407087922965423,-2.71970208349659,
12.5190199595513));
#416815=CARTESIAN_POINT('Ctrl Pts',(-0.405711751567649,-2.71990807030645,
12.5141420429941));
#416816=CARTESIAN_POINT('Ctrl Pts',(-0.403642073173232,-2.72021716252342,
12.5093757677094));
#416817=CARTESIAN_POINT('Ctrl Pts',(-0.400785940256781,-2.72063790867004,
12.5051960112707));
#416818=CARTESIAN_POINT('Ctrl Pts',(-0.398877846564678,-2.72091899610253,
12.5024036458141));
#416819=CARTESIAN_POINT('Ctrl Pts',(-0.396572456504988,-2.72125656684232,
12.4998248032393));
#416820=CARTESIAN_POINT('Ctrl Pts',(-0.393951032848873,-2.72163601234943,
12.4976950015772));
#416821=CARTESIAN_POINT('Ctrl Pts',(-0.391255748044293,-2.72202614910091,
12.495505190692));
#416822=CARTESIAN_POINT('Ctrl Pts',(-0.388156842263406,-2.72247040935534,
12.4937456938368));
#416823=CARTESIAN_POINT('Ctrl Pts',(-0.38489322543022,-2.72293172977545,
12.4925987732155));
#416824=CARTESIAN_POINT('Ctrl Pts',(-0.381630372270791,-2.72339294224835,
12.4914521209692));
#416825=CARTESIAN_POINT('Ctrl Pts',(-0.378121514599243,-2.72388257813009,
12.4908873016276));
#416826=CARTESIAN_POINT('Ctrl Pts',(-0.374664178143486,-2.72435804431357,
12.4908873016278));
#416827=CARTESIAN_POINT('',(-0.409442052702696,-2.71934867302422,13.7435492065112));
#416828=CARTESIAN_POINT('',(-0.409442052702696,-2.71934867302423,14.));
#416829=CARTESIAN_POINT('',(-0.484092149969793,-2.7070564808178,13.7435492065112));
#416830=CARTESIAN_POINT('Origin',(0.,2.5406128344257E-15,13.7435492065112));
#416831=CARTESIAN_POINT('',(-0.484092149969793,-2.7070564808178,12.5369868989719));
#416832=CARTESIAN_POINT('',(-0.484092149969793,-2.7070564808178,14.));
#416833=CARTESIAN_POINT('Ctrl Pts',(-0.518640034504897,-2.70065038733427,
12.4908873016278));
#416834=CARTESIAN_POINT('Ctrl Pts',(-0.516497852492736,-2.70106177762674,
12.4908873016278));
#416835=CARTESIAN_POINT('Ctrl Pts',(-0.514343095813786,-2.70147288379803,
12.4911020829134));
#416836=CARTESIAN_POINT('Ctrl Pts',(-0.512244568507109,-2.70187074117823,
12.4915448903141));
#416837=CARTESIAN_POINT('Ctrl Pts',(-0.508654244008863,-2.70255142667342,
12.4923024798169));
#416838=CARTESIAN_POINT('Ctrl Pts',(-0.505146008813833,-2.70320870690365,
12.4937722312795));
#416839=CARTESIAN_POINT('Ctrl Pts',(-0.502067610138451,-2.70378033775857,
12.4958030942394));
#416840=CARTESIAN_POINT('Ctrl Pts',(-0.4990109398397,-2.70434793385003,
12.4978196226833));
#416841=CARTESIAN_POINT('Ctrl Pts',(-0.496287502328985,-2.70484822746203,
12.5004326847668));
#416842=CARTESIAN_POINT('Ctrl Pts',(-0.494040249406326,-2.70525862570782,
12.5033504258767));
#416843=CARTESIAN_POINT('Ctrl Pts',(-0.491355179111337,-2.7057489791201,
12.5068366111226));
#416844=CARTESIAN_POINT('Ctrl Pts',(-0.489263564502522,-2.70612704193236,
12.5108395010833));
#416845=CARTESIAN_POINT('Ctrl Pts',(-0.487738097538792,-2.706401956142,
12.5149868989719));
#416846=CARTESIAN_POINT('Ctrl Pts',(-0.485175930334071,-2.70686370076762,
12.5219528491417));
#416847=CARTESIAN_POINT('Ctrl Pts',(-0.484092149931931,-2.70705648082486,
12.5295503425868));
#416848=CARTESIAN_POINT('Ctrl Pts',(-0.484092149969793,-2.7070564808178,
12.5369868989719));
#416849=CARTESIAN_POINT('',(-0.629731830101783,-2.67692693627538,12.5369868989719));
#416850=CARTESIAN_POINT('Ctrl Pts',(-0.629731830101782,-2.67692693627537,
12.5369868989719));
#416851=CARTESIAN_POINT('Ctrl Pts',(-0.62973183010178,-2.67692693627537,
12.5309445149785));
#416852=CARTESIAN_POINT('Ctrl Pts',(-0.629027320331347,-2.67709308296243,
12.5248274368704));
#416853=CARTESIAN_POINT('Ctrl Pts',(-0.627414339771407,-2.67747105423181,
12.5190199595513));
#416854=CARTESIAN_POINT('Ctrl Pts',(-0.626059537307725,-2.67778852638223,
12.5141420429941));
#416855=CARTESIAN_POINT('Ctrl Pts',(-0.624021939482584,-2.67826528812344,
12.5093757677094));
#416856=CARTESIAN_POINT('Ctrl Pts',(-0.621209604829764,-2.6789174356197,
12.5051960112707));
#416857=CARTESIAN_POINT('Ctrl Pts',(-0.619330771397252,-2.67935311510673,
12.5024036458141));
#416858=CARTESIAN_POINT('Ctrl Pts',(-0.617060567481951,-2.6798774732998,
12.4998248032393));
#416859=CARTESIAN_POINT('Ctrl Pts',(-0.614478794728229,-2.68046932659736,
12.4976950015772));
#416860=CARTESIAN_POINT('Ctrl Pts',(-0.61182427802859,-2.68107785593437,
12.495505190692));
#416861=CARTESIAN_POINT('Ctrl Pts',(-0.608771894936094,-2.68177322753943,
12.4937456938368));
#416862=CARTESIAN_POINT('Ctrl Pts',(-0.60555673941562,-2.68249902802374,
12.4925987732155));
#416863=CARTESIAN_POINT('Ctrl Pts',(-0.602342336229141,-2.68322465867353,
12.4914521209692));
#416864=CARTESIAN_POINT('Ctrl Pts',(-0.598885063861954,-2.68399866980714,
12.4908873016276));
#416865=CARTESIAN_POINT('Ctrl Pts',(-0.59547798631601,-2.68475435893361,
12.4908873016278));
#416866=CARTESIAN_POINT('',(-0.629731830101781,-2.67692693627537,13.7435492065112));
#416867=CARTESIAN_POINT('',(-0.629731830101781,-2.67692693627538,14.));
#416868=CARTESIAN_POINT('',(-0.703131607548452,-2.65859096937952,13.7435492065112));
#416869=CARTESIAN_POINT('Origin',(0.,2.5406128344257E-15,13.7435492065112));
#416870=CARTESIAN_POINT('',(-0.703131607548453,-2.65859096937952,12.5369868989719));
#416871=CARTESIAN_POINT('',(-0.703131607548453,-2.65859096937952,14.));
#416872=CARTESIAN_POINT('Ctrl Pts',(-0.737042380757589,-2.64939021832708,
12.4908873016278));
#416873=CARTESIAN_POINT('Ctrl Pts',(-0.734940858807353,-2.64997484747332,
12.4908873016278));
#416874=CARTESIAN_POINT('Ctrl Pts',(-0.732826780872981,-2.65056021839586,
12.4911020829134));
#416875=CARTESIAN_POINT('Ctrl Pts',(-0.730767665312814,-2.65112780139571,
12.4915448903141));
#416876=CARTESIAN_POINT('Ctrl Pts',(-0.727244769510189,-2.65209886674363,
12.4923024798169));
#416877=CARTESIAN_POINT('Ctrl Pts',(-0.723801782119017,-2.65303991366538,
12.4937722312795));
#416878=CARTESIAN_POINT('Ctrl Pts',(-0.720780219782716,-2.65386056053629,
12.4958030942394));
#416879=CARTESIAN_POINT('Ctrl Pts',(-0.717779984652985,-2.65467541500467,
12.4978196226833));
#416880=CARTESIAN_POINT('Ctrl Pts',(-0.715106387729797,-2.65539602937123,
12.5004326847668));
#416881=CARTESIAN_POINT('Ctrl Pts',(-0.712900063622835,-2.65598823402638,
12.5033504258767));
#416882=CARTESIAN_POINT('Ctrl Pts',(-0.71026389603307,-2.65669581398415,
12.5068366111226));
#416883=CARTESIAN_POINT('Ctrl Pts',(-0.708210056728283,-2.65724310483181,
12.5108395010833));
#416884=CARTESIAN_POINT('Ctrl Pts',(-0.706712073690298,-2.65764144400639,
12.5149868989719));
#416885=CARTESIAN_POINT('Ctrl Pts',(-0.704196068359202,-2.65831049262804,
12.5219528491417));
#416886=CARTESIAN_POINT('Ctrl Pts',(-0.703131607511292,-2.65859096938964,
12.5295503425868));
#416887=CARTESIAN_POINT('Ctrl Pts',(-0.703131607548453,-2.65859096937952,
12.5369868989719));
#416888=CARTESIAN_POINT('',(-0.845830846069979,-2.61669069242747,12.5369868989719));
#416889=CARTESIAN_POINT('Ctrl Pts',(-0.845830846069978,-2.61669069242747,
12.5369868989719));
#416890=CARTESIAN_POINT('Ctrl Pts',(-0.845830846069976,-2.61669069242747,
12.5309445149785));
#416891=CARTESIAN_POINT('Ctrl Pts',(-0.845142222995113,-2.61691371036177,
12.5248274368704));
#416892=CARTESIAN_POINT('Ctrl Pts',(-0.843565417662293,-2.61742189685275,
12.5190199595513));
#416893=CARTESIAN_POINT('Ctrl Pts',(-0.842241000119572,-2.61784874161894,
12.5141420429941));
#416894=CARTESIAN_POINT('Ctrl Pts',(-0.840249042741053,-2.61849000011367,
12.5093757677094));
#416895=CARTESIAN_POINT('Ctrl Pts',(-0.837499221974976,-2.61936920902558,
12.5051960112707));
#416896=CARTESIAN_POINT('Ctrl Pts',(-0.835662152128562,-2.61995658119205,
12.5024036458141));
#416897=CARTESIAN_POINT('Ctrl Pts',(-0.833442242190149,-2.62066423732113,
12.4998248032393));
#416898=CARTESIAN_POINT('Ctrl Pts',(-0.830917301610533,-2.6214645597231,
12.4976950015772));
#416899=CARTESIAN_POINT('Ctrl Pts',(-0.828321218386507,-2.62228743198329,
12.495505190692));
#416900=CARTESIAN_POINT('Ctrl Pts',(-0.825335671088275,-2.62322928735568,
12.4937456938368));
#416901=CARTESIAN_POINT('Ctrl Pts',(-0.822190373210037,-2.62421473782172,
12.4925987732155));
#416902=CARTESIAN_POINT('Ctrl Pts',(-0.819045811319376,-2.62519995769615,
12.4914521209692));
#416903=CARTESIAN_POINT('Ctrl Pts',(-0.815663131833744,-2.62625319316524,
12.4908873016276));
#416904=CARTESIAN_POINT('Ctrl Pts',(-0.812328986736553,-2.62728407624824,
12.4908873016278));
#416905=CARTESIAN_POINT('',(-0.845830846069977,-2.61669069242747,13.7435492065112));
#416906=CARTESIAN_POINT('',(-0.845830846069978,-2.61669069242747,14.));
#416907=CARTESIAN_POINT('',(-0.917491840287427,-2.59243297367666,13.7435492065112));
#416908=CARTESIAN_POINT('Origin',(0.,2.5406128344257E-15,13.7435492065112));
#416909=CARTESIAN_POINT('',(-0.917491840287428,-2.59243297367666,12.5369868989719));
#416910=CARTESIAN_POINT('',(-0.917491840287428,-2.59243297367666,14.));
#416911=CARTESIAN_POINT('Ctrl Pts',(-0.950539831569773,-2.58049879453553,
12.4908873016278));
#416912=CARTESIAN_POINT('Ctrl Pts',(-0.948492954963315,-2.58125277192504,
12.4908873016278));
#416913=CARTESIAN_POINT('Ctrl Pts',(-0.946433624613375,-2.58200851205192,
12.4911020829134));
#416914=CARTESIAN_POINT('Ctrl Pts',(-0.944427623874041,-2.58274204350021,
12.4915448903141));
#416915=CARTESIAN_POINT('Ctrl Pts',(-0.940995601057367,-2.58399702642117,
12.4923024798169));
#416916=CARTESIAN_POINT('Ctrl Pts',(-0.937640773983089,-2.58521557752243,
12.4937722312795));
#416917=CARTESIAN_POINT('Ctrl Pts',(-0.934696155984694,-2.58627977913981,
12.4958030942394));
#416918=CARTESIAN_POINT('Ctrl Pts',(-0.931772322093767,-2.58733646926306,
12.4978196226833));
#416919=CARTESIAN_POINT('Ctrl Pts',(-0.929166358104517,-2.58827260881446,
12.5004326847668));
#416920=CARTESIAN_POINT('Ctrl Pts',(-0.927015645536167,-2.58904267885471,
12.5033504258767));
#416921=CARTESIAN_POINT('Ctrl Pts',(-0.924445923911998,-2.58996277653009,
12.5068366111226));
#416922=CARTESIAN_POINT('Ctrl Pts',(-0.922443527872953,-2.59067565328286,
12.5108395010833));
#416923=CARTESIAN_POINT('Ctrl Pts',(-0.92098299759068,-2.59119476654089,
12.5149868989719));
#416924=CARTESIAN_POINT('Ctrl Pts',(-0.918529897733577,-2.59206666675038,
12.5219528491417));
#416925=CARTESIAN_POINT('Ctrl Pts',(-0.917491840251216,-2.59243297368978,
12.5295503425868));
#416926=CARTESIAN_POINT('Ctrl Pts',(-0.917491840287428,-2.59243297367666,
12.5369868989719));
#416927=CARTESIAN_POINT('',(-1.05630099730985,-2.53904080374503,12.5369868989719));
#416928=CARTESIAN_POINT('Ctrl Pts',(-1.05630099730985,-2.53904080374503,
12.5369868989719));
#416929=CARTESIAN_POINT('Ctrl Pts',(-1.05630099730984,-2.53904080374503,
12.5309445149785));
#416930=CARTESIAN_POINT('Ctrl Pts',(-1.0556328436035,-2.53931920877903,
12.5248274368704));
#416931=CARTESIAN_POINT('Ctrl Pts',(-1.05410270687713,-2.53995422859434,
12.5190199595513));
#416932=CARTESIAN_POINT('Ctrl Pts',(-1.05281748803561,-2.54048760539481,
12.5141420429941));
#416933=CARTESIAN_POINT('Ctrl Pts',(-1.05088442725141,-2.54128909317358,
12.5093757677094));
#416934=CARTESIAN_POINT('Ctrl Pts',(-1.04821541997559,-2.54238951251089,
12.5051960112707));
#416935=CARTESIAN_POINT('Ctrl Pts',(-1.04643233911201,-2.54312466849194,
12.5024036458141));
#416936=CARTESIAN_POINT('Ctrl Pts',(-1.04427749628486,-2.54401091322224,
12.4998248032393));
#416937=CARTESIAN_POINT('Ctrl Pts',(-1.04182619094233,-2.5450143787151,
12.4976950015772));
#416938=CARTESIAN_POINT('Ctrl Pts',(-1.03930581769944,-2.54604611781934,
12.495505190692));
#416939=CARTESIAN_POINT('Ctrl Pts',(-1.03640697452017,-2.54722818906695,
12.4937456938368));
#416940=CARTESIAN_POINT('Ctrl Pts',(-1.03335246572261,-2.54846673150445,
12.4925987732155));
#416941=CARTESIAN_POINT('Ctrl Pts',(-1.03029867166833,-2.5497049841278,
12.4914521209692));
#416942=CARTESIAN_POINT('Ctrl Pts',(-1.02701309623813,-2.5510304348241,
12.4908873016276));
#416943=CARTESIAN_POINT('Ctrl Pts',(-1.02377407177521,-2.55232965150679,
12.4908873016278));
#416944=CARTESIAN_POINT('',(-1.05630099730985,-2.53904080374503,13.7435492065112));
#416945=CARTESIAN_POINT('',(-1.05630099730985,-2.53904080374504,14.));
#416946=CARTESIAN_POINT('',(-1.12574631620479,-2.50902276425531,13.7435492065112));
#416947=CARTESIAN_POINT('Origin',(0.,2.5406128344257E-15,13.7435492065112));
#416948=CARTESIAN_POINT('',(-1.12574631620479,-2.50902276425531,12.5369868989719));
#416949=CARTESIAN_POINT('',(-1.12574631620479,-2.50902276425531,14.));
#416950=CARTESIAN_POINT('Ctrl Pts',(-1.15771159663089,-2.49443457701868,
12.4908873016278));
#416951=CARTESIAN_POINT('Ctrl Pts',(-1.15573298699432,-2.49535288505633,
12.4908873016278));
#416952=CARTESIAN_POINT('Ctrl Pts',(-1.15374210873252,-2.49627396506169,
12.4911020829134));
#416953=CARTESIAN_POINT('Ctrl Pts',(-1.15180257241798,-2.49716856342766,
12.4915448903141));
#416954=CARTESIAN_POINT('Ctrl Pts',(-1.14848426213285,-2.49869911221738,
12.4923024798169));
#416955=CARTESIAN_POINT('Ctrl Pts',(-1.14523992119614,-2.50018705824162,
12.4937722312795));
#416956=CARTESIAN_POINT('Ctrl Pts',(-1.1423918434826,-2.50148773251928,
12.4958030942394));
#416957=CARTESIAN_POINT('Ctrl Pts',(-1.13956386846263,-2.50277922619898,
12.4978196226833));
#416958=CARTESIAN_POINT('Ctrl Pts',(-1.13704287966771,-2.50392466108096,
12.5004326847668));
#416959=CARTESIAN_POINT('Ctrl Pts',(-1.13496209127527,-2.50486747181724,
12.5033504258767));
#416960=CARTESIAN_POINT('Ctrl Pts',(-1.13247591669013,-2.50599396411201,
12.5068366111226));
#416961=CARTESIAN_POINT('Ctrl Pts',(-1.1305382895321,-2.50686768269271,
12.5108395010833));
#416962=CARTESIAN_POINT('Ctrl Pts',(-1.12912493159359,-2.5075041154211,
12.5149868989719));
#416963=CARTESIAN_POINT('Ctrl Pts',(-1.1267510621853,-2.5085730648664,12.5219528491417));
#416964=CARTESIAN_POINT('Ctrl Pts',(-1.12574631616977,-2.50902276427134,
12.5295503425868));
#416965=CARTESIAN_POINT('Ctrl Pts',(-1.12574631620479,-2.50902276425531,
12.5369868989719));
#416966=CARTESIAN_POINT('',(-1.25974163969002,-2.44449401742592,12.5369868989719));
#416967=CARTESIAN_POINT('Ctrl Pts',(-1.25974163969001,-2.44449401742592,
12.5369868989719));
#416968=CARTESIAN_POINT('Ctrl Pts',(-1.25974163969001,-2.44449401742592,
12.5309445149785));
#416969=CARTESIAN_POINT('Ctrl Pts',(-1.25909840180486,-2.44482595682003,
12.5248274368704));
#416970=CARTESIAN_POINT('Ctrl Pts',(-1.25762511649241,-2.4455835840076,
12.5190199595513));
#416971=CARTESIAN_POINT('Ctrl Pts',(-1.25638764927142,-2.44621994330773,
12.5141420429941));
#416972=CARTESIAN_POINT('Ctrl Pts',(-1.25452634928214,-2.44717632660161,
12.5093757677094));
#416973=CARTESIAN_POINT('Ctrl Pts',(-1.25195591729964,-2.44849063325519,
12.5051960112707));
#416974=CARTESIAN_POINT('Ctrl Pts',(-1.25023869152784,-2.44936868070905,
12.5024036458141));
#416975=CARTESIAN_POINT('Ctrl Pts',(-1.24816325593546,-2.45042761622812,
12.4998248032393));
#416976=CARTESIAN_POINT('Ctrl Pts',(-1.24580189886262,-2.45162754691455,
12.4976950015772));
#416977=CARTESIAN_POINT('Ctrl Pts',(-1.24337400826898,-2.45286128680934,
12.495505190692));
#416978=CARTESIAN_POINT('Ctrl Pts',(-1.24058116053174,-2.45427570744305,
12.4937456938368));
#416979=CARTESIAN_POINT('Ctrl Pts',(-1.23763776806695,-2.45575909955644,
12.4925987732155));
#416980=CARTESIAN_POINT('Ctrl Pts',(-1.23469506434464,-2.45724214456179,
12.4914521209692));
#416981=CARTESIAN_POINT('Ctrl Pts',(-1.23152845793228,-2.4588309898296,
12.4908873016276));
#416982=CARTESIAN_POINT('Ctrl Pts',(-1.22840610927704,-2.46038989403932,
12.4908873016278));
#416983=CARTESIAN_POINT('',(-1.25974163969001,-2.44449401742592,13.7435492065112));
#416984=CARTESIAN_POINT('',(-1.25974163969001,-2.44449401742592,14.));
#416985=CARTESIAN_POINT('',(-1.32650913612287,-2.40891542229746,13.7435492065112));
#416986=CARTESIAN_POINT('Origin',(0.,2.5406128344257E-15,13.7435492065112));
#416987=CARTESIAN_POINT('',(-1.32650913612287,-2.40891542229746,12.5369868989719));
#416988=CARTESIAN_POINT('',(-1.32650913612287,-2.40891542229746,14.));
#416989=CARTESIAN_POINT('Ctrl Pts',(-1.3571789820254,-2.39177030894451,
12.4908873016278));
#416990=CARTESIAN_POINT('Ctrl Pts',(-1.35528180667939,-2.39284683644181,
12.4908873016278));
#416991=CARTESIAN_POINT('Ctrl Pts',(-1.3533726294721,-2.39392712669018,
12.4911020829134));
#416992=CARTESIAN_POINT('Ctrl Pts',(-1.35151246487652,-2.3949768385693,
12.4915448903141));
#416993=CARTESIAN_POINT('Ctrl Pts',(-1.34832994993041,-2.39677276767812,
12.4923024798169));
#416994=CARTESIAN_POINT('Ctrl Pts',(-1.34521768568492,-2.39852020659005,
12.4937722312795));
#416995=CARTESIAN_POINT('Ctrl Pts',(-1.34248510174352,-2.40004869775525,
12.4958030942394));
#416996=CARTESIAN_POINT('Ctrl Pts',(-1.33977180530167,-2.40156640031404,
12.4978196226833));
#416997=CARTESIAN_POINT('Ctrl Pts',(-1.33735256846558,-2.40291350784645,
12.5004326847668));
#416998=CARTESIAN_POINT('Ctrl Pts',(-1.3353555515525,-2.40402278502886,
12.5033504258767));
#416999=CARTESIAN_POINT('Ctrl Pts',(-1.33296946908807,-2.40534817532266,
12.5068366111226));
#417000=CARTESIAN_POINT('Ctrl Pts',(-1.33110950540009,-2.4063769212783,
12.5108395010833));
#417001=CARTESIAN_POINT('Ctrl Pts',(-1.32975272546925,-2.40712643812225,
12.5149868989719));
#417002=CARTESIAN_POINT('Ctrl Pts',(-1.32747388421902,-2.40838532312115,
12.5219528491417));
#417003=CARTESIAN_POINT('Ctrl Pts',(-1.32650913608927,-2.40891542231629,
12.5295503425868));
#417004=CARTESIAN_POINT('Ctrl Pts',(-1.32650913612287,-2.40891542229746,
12.5369868989719));
#417005=CARTESIAN_POINT('',(-1.45479890930079,-2.33367952673396,12.5369868989719));
#417006=CARTESIAN_POINT('Ctrl Pts',(-1.45479890930078,-2.33367952673396,
12.5369868989719));
#417007=CARTESIAN_POINT('Ctrl Pts',(-1.45479890930078,-2.33367952673396,
12.5309445149785));
#417008=CARTESIAN_POINT('Ctrl Pts',(-1.45418486787883,-2.33406279148629,
12.5248274368704));
#417009=CARTESIAN_POINT('Ctrl Pts',(-1.45277823845097,-2.33493798416217,
12.5190199595513));
#417010=CARTESIAN_POINT('Ctrl Pts',(-1.45159675799071,-2.33567309109583,
12.5141420429941));
#417011=CARTESIAN_POINT('Ctrl Pts',(-1.44981960544068,-2.33677800533178,
12.5093757677094));
#417012=CARTESIAN_POINT('Ctrl Pts',(-1.44736485455224,-2.33829745280769,
12.5051960112707));
#417013=CARTESIAN_POINT('Ctrl Pts',(-1.44572491172643,-2.33931254847343,
12.5024036458141));
#417014=CARTESIAN_POINT('Ctrl Pts',(-1.44374269505025,-2.34053712774011,
12.4998248032393));
#417015=CARTESIAN_POINT('Ctrl Pts',(-1.44148700068882,-2.34192553827937,
12.4976950015772));
#417016=CARTESIAN_POINT('Ctrl Pts',(-1.43916774995576,-2.34335306862925,
12.495505190692));
#417017=CARTESIAN_POINT('Ctrl Pts',(-1.43649948360146,-2.3449904259131,
12.4937456938368));
#417018=CARTESIAN_POINT('Ctrl Pts',(-1.43368679526066,-2.34670879597261,
12.4925987732155));
#417019=CARTESIAN_POINT('Ctrl Pts',(-1.43087476507809,-2.34842676394015,
12.4914521209692));
#417020=CARTESIAN_POINT('Ctrl Pts',(-1.42784820092678,-2.35026843027634,
12.4908873016276));
#417021=CARTESIAN_POINT('Ctrl Pts',(-1.42486330679437,-2.35207664776278,
12.4908873016278));
#417022=CARTESIAN_POINT('',(-1.45479890930078,-2.33367952673396,13.7435492065112));
#417023=CARTESIAN_POINT('',(-1.45479890930078,-2.33367952673396,14.));
#417024=CARTESIAN_POINT('',(-1.51844425659866,-2.29277714564729,13.7435492065112));
#417025=CARTESIAN_POINT('Origin',(0.,2.5406128344257E-15,13.7435492065112));
#417026=CARTESIAN_POINT('',(-1.51844425659866,-2.29277714564729,12.5369868989719));
#417027=CARTESIAN_POINT('',(-1.51844425659866,-2.29277714564729,14.));
#417028=CARTESIAN_POINT('Ctrl Pts',(-1.5476145652133,-2.27318920407863,
12.4908873016278));
#417029=CARTESIAN_POINT('Ctrl Pts',(-1.54581144954677,-2.27441678692272,
12.4908873016278));
#417030=CARTESIAN_POINT('Ctrl Pts',(-1.54399667865332,-2.27564909826073,
12.4911020829134));
#417031=CARTESIAN_POINT('Ctrl Pts',(-1.54222826486516,-2.27684693799364,
12.4915448903141));
#417032=CARTESIAN_POINT('Ctrl Pts',(-1.53920272436996,-2.27889629580963,
12.4923024798169));
#417033=CARTESIAN_POINT('Ctrl Pts',(-1.53624324842076,-2.28089159869159,
12.4937722312795));
#417034=CARTESIAN_POINT('Ctrl Pts',(-1.53364434314679,-2.28263773488783,
12.4958030942394));
#417035=CARTESIAN_POINT('Ctrl Pts',(-1.53106378182322,-2.28437154626559,
12.4978196226833));
#417036=CARTESIAN_POINT('Ctrl Pts',(-1.52876239656796,-2.28591136167005,
12.5004326847668));
#417037=CARTESIAN_POINT('Ctrl Pts',(-1.52686244095231,-2.28717972324196,
12.5033504258767));
#417038=CARTESIAN_POINT('Ctrl Pts',(-1.5245923295937,-2.28869519128105,
12.5068366111226));
#417039=CARTESIAN_POINT('Ctrl Pts',(-1.52282240712726,-2.28987211847702,
12.5108395010833));
#417040=CARTESIAN_POINT('Ctrl Pts',(-1.52153123435067,-2.2907297315256,
12.5149868989719));
#417041=CARTESIAN_POINT('Ctrl Pts',(-1.51936258657103,-2.29217017440614,
12.5219528491417));
#417042=CARTESIAN_POINT('Ctrl Pts',(-1.51844425656671,-2.2927771456688,
12.5295503425868));
#417043=CARTESIAN_POINT('Ctrl Pts',(-1.51844425659866,-2.29277714564729,
12.5369868989719));
#417044=CARTESIAN_POINT('',(-1.64017473219509,-2.20733478382161,12.5369868989719));
#417045=CARTESIAN_POINT('Ctrl Pts',(-1.64017473219508,-2.20733478382161,
12.5369868989719));
#417046=CARTESIAN_POINT('Ctrl Pts',(-1.64017473219508,-2.20733478382161,
12.5309445149785));
#417047=CARTESIAN_POINT('Ctrl Pts',(-1.63959397358067,-2.20776682336847,
12.5248274368704));
#417048=CARTESIAN_POINT('Ctrl Pts',(-1.63826336092418,-2.20875375726979,
12.5190199595513));
#417049=CARTESIAN_POINT('Ctrl Pts',(-1.63714572978217,-2.20958271982161,
12.5141420429941));
#417050=CARTESIAN_POINT('Ctrl Pts',(-1.6354645513284,-2.2108288119777,12.5093757677094));
#417051=CARTESIAN_POINT('Ctrl Pts',(-1.63314181749619,-2.21254328860369,
12.5051960112707));
#417052=CARTESIAN_POINT('Ctrl Pts',(-1.63159007116529,-2.21368867718713,
12.5024036458141));
#417053=CARTESIAN_POINT('Ctrl Pts',(-1.62971426473026,-2.21507075082842,
12.4998248032393));
#417054=CARTESIAN_POINT('Ctrl Pts',(-1.62757924435406,-2.21663840157745,
12.4976950015772));
#417055=CARTESIAN_POINT('Ctrl Pts',(-1.62538406771255,-2.21825022240348,
12.495505190692));
#417056=CARTESIAN_POINT('Ctrl Pts',(-1.62285813961354,-2.22009961999489,
12.4937456938368));
#417057=CARTESIAN_POINT('Ctrl Pts',(-1.62019487337358,-2.22204153253128,
12.4925987732155));
#417058=CARTESIAN_POINT('Ctrl Pts',(-1.61753223032766,-2.22398299066762,
12.4914521209692));
#417059=CARTESIAN_POINT('Ctrl Pts',(-1.61466584972249,-2.22606522208659,
12.4908873016276));
#417060=CARTESIAN_POINT('Ctrl Pts',(-1.61183827409089,-2.2281107194607,
12.4908873016278));
#417061=CARTESIAN_POINT('',(-1.64017473219508,-2.20733478382161,13.7435492065112));
#417062=CARTESIAN_POINT('',(-1.64017473219508,-2.20733478382161,14.));
#417063=CARTESIAN_POINT('',(-1.70027438107246,-2.16138081537444,13.7435492065112));
#417064=CARTESIAN_POINT('Origin',(0.,2.5406128344257E-15,13.7435492065112));
#417065=CARTESIAN_POINT('',(-1.70027438107246,-2.16138081537444,12.5369868989719));
#417066=CARTESIAN_POINT('',(-1.70027438107246,-2.16138081537444,14.));
#417067=CARTESIAN_POINT('Ctrl Pts',(-1.72775102880814,-2.13948040010943,
12.4908873016278));
#417068=CARTESIAN_POINT('Ctrl Pts',(-1.72605397225836,-2.140850868939,12.4908873016278));
#417069=CARTESIAN_POINT('Ctrl Pts',(-1.72434568467961,-2.14222700053803,
12.4911020829134));
#417070=CARTESIAN_POINT('Ctrl Pts',(-1.72268079020089,-2.14356499669892,
12.4915448903141));
#417071=CARTESIAN_POINT('Ctrl Pts',(-1.71983235862941,-2.14585414508395,
12.4923024798169));
#417072=CARTESIAN_POINT('Ctrl Pts',(-1.71704536580065,-2.14808403352447,
12.4937722312795));
#417073=CARTESIAN_POINT('Ctrl Pts',(-1.71459743447992,-2.15003619450345,
12.4958030942394));
#417074=CARTESIAN_POINT('Ctrl Pts',(-1.71216678148448,-2.15197457647151,
12.4978196226833));
#417075=CARTESIAN_POINT('Ctrl Pts',(-1.70999856314922,-2.15369685253056,
12.5004326847668));
#417076=CARTESIAN_POINT('Ctrl Pts',(-1.70820831272215,-2.15511585775498,
12.5033504258767));
#417077=CARTESIAN_POINT('Ctrl Pts',(-1.70606927968592,-2.1568113183496,
12.5068366111226));
#417078=CARTESIAN_POINT('Ctrl Pts',(-1.70440117698301,-2.15812859452958,
12.5108395010833));
#417079=CARTESIAN_POINT('Ctrl Pts',(-1.70318420390247,-2.15908859650944,
12.5149868989719));
#417080=CARTESIAN_POINT('Ctrl Pts',(-1.7011401815866,-2.16070101136191,
12.5219528491417));
#417081=CARTESIAN_POINT('Ctrl Pts',(-1.70027438104236,-2.16138081539848,
12.5295503425868));
#417082=CARTESIAN_POINT('Ctrl Pts',(-1.70027438107246,-2.16138081537444,
12.5369868989719));
#417083=CARTESIAN_POINT('',(-1.81463546285641,-2.06630059210753,12.5369868989719));
#417084=CARTESIAN_POINT('Ctrl Pts',(-1.81463546285641,-2.06630059210752,
12.5369868989719));
#417085=CARTESIAN_POINT('Ctrl Pts',(-1.8146354628564,-2.06630059210752,
12.5309445149785));
#417086=CARTESIAN_POINT('Ctrl Pts',(-1.81409185190231,-2.06677853129701,
12.5248274368704));
#417087=CARTESIAN_POINT('Ctrl Pts',(-1.81284611102486,-2.0678706385415,
12.5190199595513));
#417088=CARTESIAN_POINT('Ctrl Pts',(-1.81179976685197,-2.06878794010247,
12.5141420429941));
#417089=CARTESIAN_POINT('Ctrl Pts',(-1.81022575045969,-2.07016691764099,
12.5093757677094));
#417090=CARTESIAN_POINT('Ctrl Pts',(-1.80805049109414,-2.07206501385797,
12.5051960112707));
#417091=CARTESIAN_POINT('Ctrl Pts',(-1.80659726787397,-2.07333307298707,
12.5024036458141));
#417092=CARTESIAN_POINT('Ctrl Pts',(-1.80484035486241,-2.07486344353092,
12.4998248032393));
#417093=CARTESIAN_POINT('Ctrl Pts',(-1.8028402166798,-2.07659990203263,
12.4976950015772));
#417094=CARTESIAN_POINT('Ctrl Pts',(-1.8007837226682,-2.07838528693313,
12.495505190692));
#417095=CARTESIAN_POINT('Ctrl Pts',(-1.79841694245924,-2.08043441739626,
12.4937456938368));
#417096=CARTESIAN_POINT('Ctrl Pts',(-1.79592082191755,-2.082586949302,12.4925987732155));
#417097=CARTESIAN_POINT('Ctrl Pts',(-1.79342528545844,-2.08473897752356,
12.4914521209692));
#417098=CARTESIAN_POINT('Ctrl Pts',(-1.7907381636894,-2.08704791711876,
12.4908873016276));
#417099=CARTESIAN_POINT('Ctrl Pts',(-1.78808672360792,-2.08931708193301,
12.4908873016278));
#417100=CARTESIAN_POINT('',(-1.81463546285641,-2.06630059210753,13.7435492065112));
#417101=CARTESIAN_POINT('',(-1.81463546285641,-2.06630059210753,14.));
#417102=CARTESIAN_POINT('',(-1.87078946006574,-2.01560085237801,13.7435492065112));
#417103=CARTESIAN_POINT('Origin',(0.,2.5406128344257E-15,13.7435492065112));
#417104=CARTESIAN_POINT('',(-1.87078946006574,-2.01560085237801,12.5369868989719));
#417105=CARTESIAN_POINT('',(-1.87078946006574,-2.01560085237801,14.));
#417106=CARTESIAN_POINT('Ctrl Pts',(-1.89638959436511,-1.99153370706693,
12.4908873016278));
#417107=CARTESIAN_POINT('Ctrl Pts',(-1.89480989056343,-1.99303794163803,
12.4908873016278));
#417108=CARTESIAN_POINT('Ctrl Pts',(-1.89321945467138,-1.99454873556932,
12.4911020829134));
#417109=CARTESIAN_POINT('Ctrl Pts',(-1.89166915910015,-1.99601798401451,
12.4915448903141));
#417110=CARTESIAN_POINT('Ctrl Pts',(-1.88901679229454,-1.99853168906375,
12.4923024798169));
#417111=CARTESIAN_POINT('Ctrl Pts',(-1.88642082956369,-2.00098132352316,
12.4937722312795));
#417112=CARTESIAN_POINT('Ctrl Pts',(-1.88414016277525,-2.00312651797565,
12.4958030942394));
#417113=CARTESIAN_POINT('Ctrl Pts',(-1.8818755937026,-2.00525657092182,
12.4978196226833));
#417114=CARTESIAN_POINT('Ctrl Pts',(-1.87985497142262,-2.00714984617245,
12.5004326847668));
#417115=CARTESIAN_POINT('Ctrl Pts',(-1.87818634000535,-2.00871005180372,
12.5033504258767));
#417116=CARTESIAN_POINT('Ctrl Pts',(-1.87619262020345,-2.01057422194334,
12.5068366111226));
#417117=CARTESIAN_POINT('Ctrl Pts',(-1.87463743821233,-2.01202308085171,
12.5108395010833));
#417118=CARTESIAN_POINT('Ctrl Pts',(-1.87350276358291,-2.01307908310806,
12.5149868989719));
#417119=CARTESIAN_POINT('Ctrl Pts',(-1.87159696936208,-2.01485273957765,
12.5219528491417));
#417120=CARTESIAN_POINT('Ctrl Pts',(-1.87078946003771,-2.01560085240442,
12.5295503425868));
#417121=CARTESIAN_POINT('Ctrl Pts',(-1.87078946006574,-2.01560085237801,
12.5369868989719));
#417122=CARTESIAN_POINT('',(-1.9770200939062,-1.91151551086857,12.5369868989719));
#417123=CARTESIAN_POINT('Ctrl Pts',(-1.9770200939062,-1.91151551086857,
12.5369868989719));
#417124=CARTESIAN_POINT('Ctrl Pts',(-1.9770200939062,-1.91151551086857,
12.5309445149785));
#417125=CARTESIAN_POINT('Ctrl Pts',(-1.97651724825362,-1.91203616909422,
12.5248274368704));
#417126=CARTESIAN_POINT('Ctrl Pts',(-1.97536466935523,-1.91322618188836,
12.5190199595513));
#417127=CARTESIAN_POINT('Ctrl Pts',(-1.97439657539929,-1.91422571796793,
12.5141420429941));
#417128=CARTESIAN_POINT('Ctrl Pts',(-1.9729401958879,-1.91572840402087,
12.5093757677094));
#417129=CARTESIAN_POINT('Ctrl Pts',(-1.97092688698119,-1.91779748831169,
12.5051960112707));
#417130=CARTESIAN_POINT('Ctrl Pts',(-1.96958185783251,-1.91917977926215,
12.5024036458141));
#417131=CARTESIAN_POINT('Ctrl Pts',(-1.96795553021065,-1.9208482623451,
12.4998248032393));
#417132=CARTESIAN_POINT('Ctrl Pts',(-1.96610358481123,-1.92274197275465,
12.4976950015772));
#417133=CARTESIAN_POINT('Ctrl Pts',(-1.9641994590579,-1.92468904028768,
12.495505190692));
#417134=CARTESIAN_POINT('Ctrl Pts',(-1.96200757727078,-1.92692426699738,
12.4937456938368));
#417135=CARTESIAN_POINT('Ctrl Pts',(-1.95969521369772,-1.92927309352777,
12.4925987732155));
#417136=CARTESIAN_POINT('Ctrl Pts',(-1.95738339120883,-1.93162137044181,
12.4914521209692));
#417137=CARTESIAN_POINT('Ctrl Pts',(-1.95489341062797,-1.93414165260117,
12.4908873016276));
#417138=CARTESIAN_POINT('Ctrl Pts',(-1.95243575099289,-1.93661938393811,
12.4908873016278));
#417139=CARTESIAN_POINT('',(-1.9770200939062,-1.91151551086857,13.7435492065112));
#417140=CARTESIAN_POINT('',(-1.9770200939062,-1.91151551086857,14.));
#417141=CARTESIAN_POINT('',(-2.02885474386082,-1.85640739825973,13.7435492065112));
#417142=CARTESIAN_POINT('Origin',(0.,2.5406128344257E-15,13.7435492065112));
#417143=CARTESIAN_POINT('',(-2.02885474386082,-1.85640739825973,12.5369868989719));
#417144=CARTESIAN_POINT('',(-2.02885474386082,-1.85640739825973,14.));
#417145=CARTESIAN_POINT('Ctrl Pts',(-2.05240800005384,-1.83033368578382,
12.4908873016278));
#417146=CARTESIAN_POINT('Ctrl Pts',(-2.05095616166842,-1.83196167566357,
12.4908873016278));
#417147=CARTESIAN_POINT('Ctrl Pts',(-2.04949416155152,-1.83359707784278,
12.4911020829134));
#417148=CARTESIAN_POINT('Ctrl Pts',(-2.04806878184904,-1.83518780096627,
12.4915448903141));
#417149=CARTESIAN_POINT('Ctrl Pts',(-2.04563013087279,-1.83790933438735,
12.4923024798169));
#417150=CARTESIAN_POINT('Ctrl Pts',(-2.04324247394351,-1.84056241295248,
12.4937722312795));
#417151=CARTESIAN_POINT('Ctrl Pts',(-2.04114424914856,-1.84288636496334,
12.4958030942394));
#417152=CARTESIAN_POINT('Ctrl Pts',(-2.03906083433224,-1.8451939137367,
12.4978196226833));
#417153=CARTESIAN_POINT('Ctrl Pts',(-2.03720125501545,-1.84724558874448,
12.5004326847668));
#417154=CARTESIAN_POINT('Ctrl Pts',(-2.03566534707476,-1.84893661187154,
12.5033504258767));
#417155=CARTESIAN_POINT('Ctrl Pts',(-2.03383020838352,-1.85095708581146,
12.5068366111226));
#417156=CARTESIAN_POINT('Ctrl Pts',(-2.03239829658376,-1.8525278855312,
12.5108395010833));
#417157=CARTESIAN_POINT('Ctrl Pts',(-2.0313534714779,-1.85367286054327,
12.5149868989719));
#417158=CARTESIAN_POINT('Ctrl Pts',(-2.02959858809823,-1.8555959552388,
12.5219528491417));
#417159=CARTESIAN_POINT('Ctrl Pts',(-2.02885474383503,-1.85640739828834,
12.5295503425868));
#417160=CARTESIAN_POINT('Ctrl Pts',(-2.02885474386082,-1.85640739825973,
12.5369868989719));
#417161=CARTESIAN_POINT('',(-2.1262479824164,-1.74400960928264,12.5369868989719));
#417162=CARTESIAN_POINT('Ctrl Pts',(-2.1262479824164,-1.74400960928264,
12.5369868989719));
#417163=CARTESIAN_POINT('Ctrl Pts',(-2.1262479824164,-1.74400960928264,
12.5309445149785));
#417164=CARTESIAN_POINT('Ctrl Pts',(-2.12578924842019,-1.74456952164988,
12.5248274368704));
#417165=CARTESIAN_POINT('Ctrl Pts',(-2.12473750172327,-1.74584952065485,
12.5190199595513));
#417166=CARTESIAN_POINT('Ctrl Pts',(-2.12385410048983,-1.74692463950532,
12.5141420429941));
#417167=CARTESIAN_POINT('Ctrl Pts',(-2.12252504982469,-1.74854103394493,
12.5093757677094));
#417168=CARTESIAN_POINT('Ctrl Pts',(-2.12068708961543,-1.750767336895,12.5051960112707));
#417169=CARTESIAN_POINT('Ctrl Pts',(-2.11945920548531,-1.75225466074862,
12.5024036458141));
#417170=CARTESIAN_POINT('Ctrl Pts',(-2.11797428619515,-1.75405015289102,
12.4998248032393));
#417171=CARTESIAN_POINT('Ctrl Pts',(-2.11628285796999,-1.75608851287808,
12.4976950015772));
#417172=CARTESIAN_POINT('Ctrl Pts',(-2.11454377211767,-1.75818430563045,
12.495505190692));
#417173=CARTESIAN_POINT('Ctrl Pts',(-2.11254137536405,-1.76059075352176,
12.4937456938368));
#417174=CARTESIAN_POINT('Ctrl Pts',(-2.1104281571577,-1.76312024362377,
12.4925987732155));
#417175=CARTESIAN_POINT('Ctrl Pts',(-2.10831543343625,-1.76564914183486,
12.4914521209692));
#417176=CARTESIAN_POINT('Ctrl Pts',(-2.10603916445351,-1.76836399449644,
12.4908873016276));
#417177=CARTESIAN_POINT('Ctrl Pts',(-2.10379164058422,-1.7710338034628,
12.4908873016278));
#417178=CARTESIAN_POINT('',(-2.1262479824164,-1.74400960928264,13.7435492065112));
#417179=CARTESIAN_POINT('',(-2.1262479824164,-1.74400960928264,14.));
#417180=CARTESIAN_POINT('',(-2.17341833407298,-1.68485985919169,13.7435492065112));
#417181=CARTESIAN_POINT('Origin',(0.,2.5406128344257E-15,13.7435492065112));
#417182=CARTESIAN_POINT('',(-2.17341833407298,-1.6848598591917,12.5369868989719));
#417183=CARTESIAN_POINT('',(-2.17341833407298,-1.6848598591917,14.));
#417184=CARTESIAN_POINT('Ctrl Pts',(-2.1947679691257,-1.65695309580563,
12.4908873016278));
#417185=CARTESIAN_POINT('Ctrl Pts',(-2.19345365790146,-1.65869400698998,
12.4908873016278));
#417186=CARTESIAN_POINT('Ctrl Pts',(-2.19212982292928,-1.66044313408541,
12.4911020829134));
#417187=CARTESIAN_POINT('Ctrl Pts',(-2.19083884476229,-1.66214474588727,
12.4915448903141));
#417188=CARTESIAN_POINT('Ctrl Pts',(-2.18863013843529,-1.6650559963243,
12.4923024798169));
#417189=CARTESIAN_POINT('Ctrl Pts',(-2.18646667677051,-1.66789486319503,
12.4937722312795));
#417190=CARTESIAN_POINT('Ctrl Pts',(-2.18456485730888,-1.67038210724704,
12.4958030942394));
#417191=CARTESIAN_POINT('Ctrl Pts',(-2.18267646153076,-1.67285179549123,
12.4978196226833));
#417192=CARTESIAN_POINT('Ctrl Pts',(-2.18099030037069,-1.67504821669748,
12.5004326847668));
#417193=CARTESIAN_POINT('Ctrl Pts',(-2.17959733712052,-1.67685880384043,
12.5033504258767));
#417194=CARTESIAN_POINT('Ctrl Pts',(-2.17793299208515,-1.67902213565991,
12.5068366111226));
#417195=CARTESIAN_POINT('Ctrl Pts',(-2.17663387961354,-1.68070442277808,
12.5108395010833));
#417196=CARTESIAN_POINT('Ctrl Pts',(-2.17568585716995,-1.68193075092606,
12.5149868989719));
#417197=CARTESIAN_POINT('Ctrl Pts',(-2.17409356309077,-1.68399048596961,
12.5219528491417));
#417198=CARTESIAN_POINT('Ctrl Pts',(-2.17341833404961,-1.68485985922231,
12.5295503425868));
#417199=CARTESIAN_POINT('Ctrl Pts',(-2.17341833407298,-1.6848598591917,
12.5369868989719));
#417200=CARTESIAN_POINT('',(-2.26132604140984,-1.56489761148827,12.5369868989719));
#417201=CARTESIAN_POINT('Ctrl Pts',(-2.26132604140984,-1.56489761148827,
12.5369868989719));
#417202=CARTESIAN_POINT('Ctrl Pts',(-2.26132604140984,-1.56489761148827,
12.5309445149785));
#417203=CARTESIAN_POINT('Ctrl Pts',(-2.26091447186907,-1.56549305187266,
12.5248274368704));
#417204=CARTESIAN_POINT('Ctrl Pts',(-2.25997055657435,-1.56685451890628,
12.5190199595513));
#417205=CARTESIAN_POINT('Ctrl Pts',(-2.25917772695287,-1.56799806578909,
12.5141420429941));
#417206=CARTESIAN_POINT('Ctrl Pts',(-2.25798484974689,-1.56971741177706,
12.5093757677094));
#417207=CARTESIAN_POINT('Ctrl Pts',(-2.25633446955702,-1.57208611770757,
12.5051960112707));
#417208=CARTESIAN_POINT('Ctrl Pts',(-2.25523190181175,-1.57366857656948,
12.5024036458141));
#417209=CARTESIAN_POINT('Ctrl Pts',(-2.25389827274618,-1.57557912906736,
12.4998248032393));
#417210=CARTESIAN_POINT('Ctrl Pts',(-2.25237861787107,-1.57774857368252,
12.4976950015772));
#417211=CARTESIAN_POINT('Ctrl Pts',(-2.25081614524916,-1.57997914449925,
12.495505190692));
#417212=CARTESIAN_POINT('Ctrl Pts',(-2.24901655914907,-1.58254079905848,
12.4937456938368));
#417213=CARTESIAN_POINT('Ctrl Pts',(-2.24711654942792,-1.58523411939283,
12.4925987732155));
#417214=CARTESIAN_POINT('Ctrl Pts',(-2.24521698430172,-1.5879268095006,
12.4914521209692));
#417215=CARTESIAN_POINT('Ctrl Pts',(-2.24316957511162,-1.59081816576785,
12.4908873016276));
#417216=CARTESIAN_POINT('Ctrl Pts',(-2.24114714390866,-1.59366228522547,
12.4908873016278));
#417217=CARTESIAN_POINT('',(-2.26132604140984,-1.56489761148827,13.7435492065112));
#417218=CARTESIAN_POINT('',(-2.26132604140984,-1.56489761148827,14.));
#417219=CARTESIAN_POINT('',(-2.30351818386066,-1.50209985574305,13.7435492065112));
#417220=CARTESIAN_POINT('Origin',(0.,2.5406128344257E-15,13.7435492065112));
#417221=CARTESIAN_POINT('',(-2.30351818386066,-1.50209985574305,12.5369868989719));
#417222=CARTESIAN_POINT('',(-2.30351818386066,-1.50209985574305,14.));
#417223=CARTESIAN_POINT('Ctrl Pts',(-2.32252211947425,-1.47254575635286,
12.4908873016278));
#417224=CARTESIAN_POINT('Ctrl Pts',(-2.32135408193554,-1.47438800336511,
12.4908873016278));
#417225=CARTESIAN_POINT('Ctrl Pts',(-2.32017722201141,-1.47623921522455,
12.4911020829134));
#417226=CARTESIAN_POINT('Ctrl Pts',(-2.31902923662661,-1.47804039175897,
12.4915448903141));
#417227=CARTESIAN_POINT('Ctrl Pts',(-2.31706517352506,-1.48112198532061,
12.4923024798169));
#417228=CARTESIAN_POINT('Ctrl Pts',(-2.31514030460521,-1.4841277483063,
12.4937722312795));
#417229=CARTESIAN_POINT('Ctrl Pts',(-2.31344754677164,-1.48676173220066,
12.4958030942394));
#417230=CARTESIAN_POINT('Ctrl Pts',(-2.31176673699406,-1.48937712454788,
12.4978196226833));
#417231=CARTESIAN_POINT('Ctrl Pts',(-2.31026521511504,-1.49170367513186,
12.5004326847668));
#417232=CARTESIAN_POINT('Ctrl Pts',(-2.30902446649599,-1.49362177713198,
12.5033504258767));
#417233=CARTESIAN_POINT('Ctrl Pts',(-2.30754199105811,-1.49591357021471,
12.5068366111226));
#417234=CARTESIAN_POINT('Ctrl Pts',(-2.30638432329381,-1.49769614938807,
12.5108395010833));
#417235=CARTESIAN_POINT('Ctrl Pts',(-2.30553941244542,-1.49899566966047,
12.5149868989719));
#417236=CARTESIAN_POINT('Ctrl Pts',(-2.30412030412113,-1.50117833785518,
12.5219528491417));
#417237=CARTESIAN_POINT('Ctrl Pts',(-2.30351818383986,-1.50209985577547,
12.5295503425868));
#417238=CARTESIAN_POINT('Ctrl Pts',(-2.30351818386066,-1.50209985574305,
12.5369868989719));
#417239=CARTESIAN_POINT('',(-2.38135534869024,-1.37537147827938,12.5369868989719));
#417240=CARTESIAN_POINT('Ctrl Pts',(-2.38135534869024,-1.37537147827937,
12.5369868989719));
#417241=CARTESIAN_POINT('Ctrl Pts',(-2.38135534869024,-1.37537147827938,
12.5309445149785));
#417242=CARTESIAN_POINT('Ctrl Pts',(-2.38099368253228,-1.37599848412341,
12.5248274368704));
#417243=CARTESIAN_POINT('Ctrl Pts',(-2.38016388024033,-1.37743235884718,
12.5190199595513));
#417244=CARTESIAN_POINT('Ctrl Pts',(-2.37946689838113,-1.3786367236465,
12.5141420429941));
#417245=CARTESIAN_POINT('Ctrl Pts',(-2.37841813303529,-1.38044757921895,
12.5093757677094));
#417246=CARTESIAN_POINT('Ctrl Pts',(-2.37696631587268,-1.38294292478273,
12.5051960112707));
#417247=CARTESIAN_POINT('Ctrl Pts',(-2.37599640191872,-1.38460998765031,
12.5024036458141));
#417248=CARTESIAN_POINT('Ctrl Pts',(-2.37482293815912,-1.38662288609201,
12.4998248032393));
#417249=CARTESIAN_POINT('Ctrl Pts',(-2.37348516968652,-1.38890897803929,
12.4976950015772));
#417250=CARTESIAN_POINT('Ctrl Pts',(-2.37210970829254,-1.39125948283961,
12.495505190692));
#417251=CARTESIAN_POINT('Ctrl Pts',(-2.37052490879456,-1.39395929667832,
12.4937456938368));
#417252=CARTESIAN_POINT('Ctrl Pts',(-2.36885075180983,-1.39679852364254,
12.4925987732155));
#417253=CARTESIAN_POINT('Ctrl Pts',(-2.36717698657139,-1.3996370862386,
12.4914521209692));
#417254=CARTESIAN_POINT('Ctrl Pts',(-2.36537206234429,-1.4026857046126,
12.4908873016276));
#417255=CARTESIAN_POINT('Ctrl Pts',(-2.36358818275363,-1.40568520741572,
12.4908873016278));
#417256=CARTESIAN_POINT('',(-2.38135534869024,-1.37537147827938,13.7435492065112));
#417257=CARTESIAN_POINT('',(-2.38135534869024,-1.37537147827938,14.));
#417258=CARTESIAN_POINT('',(-2.4182885001885,-1.30934362558346,13.7435492065112));
#417259=CARTESIAN_POINT('Origin',(0.,2.5406128344257E-15,13.7435492065112));
#417260=CARTESIAN_POINT('',(-2.4182885001885,-1.30934362558346,12.5369868989719));
#417261=CARTESIAN_POINT('',(-2.4182885001885,-1.30934362558346,14.));
#417262=CARTESIAN_POINT('Ctrl Pts',(-2.43482026830688,-1.27833886784452,
12.4908873016278));
#417263=CARTESIAN_POINT('Ctrl Pts',(-2.43380627755081,-1.28027019083474,
12.4908873016278));
#417264=CARTESIAN_POINT('Ctrl Pts',(-2.43278422448335,-1.28221116794868,
12.4911020829134));
#417265=CARTESIAN_POINT('Ctrl Pts',(-2.43178687153408,-1.28409992268301,
12.4915448903141));
#417266=CARTESIAN_POINT('Ctrl Pts',(-2.43008052217386,-1.28733135187254,
12.4923024798169));
#417267=CARTESIAN_POINT('Ctrl Pts',(-2.42840705568404,-1.29048400811643,
12.4937722312795));
#417268=CARTESIAN_POINT('Ctrl Pts',(-2.42693462450261,-1.2932472031249,
12.4958030942394));
#417269=CARTESIAN_POINT('Ctrl Pts',(-2.42547258623732,-1.29599089457059,
12.4978196226833));
#417270=CARTESIAN_POINT('Ctrl Pts',(-2.42416569601973,-1.29843209172202,
12.5004326847668));
#417271=CARTESIAN_POINT('Ctrl Pts',(-2.42308541900916,-1.30044494392697,
12.5033504258767));
#417272=CARTESIAN_POINT('Ctrl Pts',(-2.42179467879822,-1.30284994676809,
12.5068366111226));
#417273=CARTESIAN_POINT('Ctrl Pts',(-2.42078615982918,-1.30472095522636,
12.5108395010833));
#417274=CARTESIAN_POINT('Ctrl Pts',(-2.4200499833183,-1.30608501953017,
12.5149868989719));
#417275=CARTESIAN_POINT('Ctrl Pts',(-2.41881350468066,-1.3083760955793,
12.5219528491417));
#417276=CARTESIAN_POINT('Ctrl Pts',(-2.41828850017042,-1.30934362561747,
12.5295503425868));
#417277=CARTESIAN_POINT('Ctrl Pts',(-2.4182885001885,-1.30934362558346,
12.5369868989719));
#417278=CARTESIAN_POINT('',(-2.48553712902108,-1.17669247480285,12.5369868989719));
#417279=CARTESIAN_POINT('Ctrl Pts',(-2.48553712902108,-1.17669247480285,
12.5369868989719));
#417280=CARTESIAN_POINT('Ctrl Pts',(-2.48553712902107,-1.17669247480285,
12.5309445149785));
#417281=CARTESIAN_POINT('Ctrl Pts',(-2.48522777307455,-1.17734687348608,
12.5248274368704));
#417282=CARTESIAN_POINT('Ctrl Pts',(-2.4845176059827,-1.1788436137003,12.5190199595513));
#417283=CARTESIAN_POINT('Ctrl Pts',(-2.48392111018507,-1.18010078156709,
12.5141420429941));
#417284=CARTESIAN_POINT('Ctrl Pts',(-2.48302343605972,-1.18199109577896,
12.5093757677094));
#417285=CARTESIAN_POINT('Ctrl Pts',(-2.48177984352806,-1.18459647486299,
12.5051960112707));
#417286=CARTESIAN_POINT('Ctrl Pts',(-2.48094903798272,-1.18633704770789,
12.5024036458141));
#417287=CARTESIAN_POINT('Ctrl Pts',(-2.47994354873682,-1.18843889658639,
12.4998248032393));
#417288=CARTESIAN_POINT('Ctrl Pts',(-2.4787965692952,-1.19082642230106,
12.4976950015772));
#417289=CARTESIAN_POINT('Ctrl Pts',(-2.47761727259779,-1.19328121886333,
12.495505190692));
#417290=CARTESIAN_POINT('Ctrl Pts',(-2.4762578062811,-1.19610122516585,
12.4937456938368));
#417291=CARTESIAN_POINT('Ctrl Pts',(-2.47482064327132,-1.19906746417294,
12.4925987732155));
#417292=CARTESIAN_POINT('Ctrl Pts',(-2.47338381655214,-1.20203300909154,
12.4914521209692));
#417293=CARTESIAN_POINT('Ctrl Pts',(-2.47183338876099,-1.20521860152,12.4908873016276));
#417294=CARTESIAN_POINT('Ctrl Pts',(-2.47029993220698,-1.20835352647236,
12.4908873016278));
#417295=CARTESIAN_POINT('',(-2.48553712902108,-1.17669247480285,13.7435492065112));
#417296=CARTESIAN_POINT('',(-2.48553712902108,-1.17669247480285,14.));
#417297=CARTESIAN_POINT('',(-2.5169655055371,-1.10787392962211,13.7435492065112));
#417298=CARTESIAN_POINT('Origin',(0.,2.5406128344257E-15,13.7435492065112));
#417299=CARTESIAN_POINT('',(-2.51696550553711,-1.10787392962211,12.5369868989719));
#417300=CARTESIAN_POINT('',(-2.51696550553711,-1.10787392962211,14.));
#417301=CARTESIAN_POINT('Ctrl Pts',(-2.530915089971,-1.07562484508174,12.4908873016278));
#417302=CARTESIAN_POINT('Ctrl Pts',(-2.53006189393875,-1.07763239141408,
12.4908873016278));
#417303=CARTESIAN_POINT('Ctrl Pts',(-2.52920144932249,-1.07965021690007,
12.4911020829134));
#417304=CARTESIAN_POINT('Ctrl Pts',(-2.52836136602808,-1.08161398048317,
12.4915448903141));
#417305=CARTESIAN_POINT('Ctrl Pts',(-2.52692408588266,-1.08497374067248,
12.4923024798169));
#417306=CARTESIAN_POINT('Ctrl Pts',(-2.52551315846624,-1.08825230976742,
12.4937722312795));
#417307=CARTESIAN_POINT('Ctrl Pts',(-2.52427085272355,-1.09112632728312,
12.4958030942394));
#417308=CARTESIAN_POINT('Ctrl Pts',(-2.52303731559399,-1.09398005901338,
12.4978196226833));
#417309=CARTESIAN_POINT('Ctrl Pts',(-2.52193375417659,-1.09651965696798,
12.5004326847668));
#417310=CARTESIAN_POINT('Ctrl Pts',(-2.52102113783977,-1.09861386417844,
12.5033504258767));
#417311=CARTESIAN_POINT('Ctrl Pts',(-2.51993072251891,-1.10111607188084,
12.5068366111226));
#417312=CARTESIAN_POINT('Ctrl Pts',(-2.51907806387249,-1.10306305837143,
12.5108395010833));
#417313=CARTESIAN_POINT('Ctrl Pts',(-2.51845552083233,-1.10448258908376,
12.5149868989719));
#417314=CARTESIAN_POINT('Ctrl Pts',(-2.51740990044268,-1.10686682625421,
12.5219528491417));
#417315=CARTESIAN_POINT('Ctrl Pts',(-2.51696550552185,-1.10787392965748,
12.5295503425868));
#417316=CARTESIAN_POINT('Ctrl Pts',(-2.51696550553711,-1.10787392962211,
12.5369868989719));
#417317=CARTESIAN_POINT('',(-2.57317806984304,-0.97018277704711,12.5369868989719));
#417318=CARTESIAN_POINT('Ctrl Pts',(-2.57317806984304,-0.970182777047109,
12.5369868989719));
#417319=CARTESIAN_POINT('Ctrl Pts',(-2.57317806984304,-0.970182777047111,
12.5309445149785));
#417320=CARTESIAN_POINT('Ctrl Pts',(-2.57292308282073,-0.970860213654265,
12.5248274368704));
#417321=CARTESIAN_POINT('Ctrl Pts',(-2.57233727697381,-0.972409858799751,
12.5190199595513));
#417322=CARTESIAN_POINT('Ctrl Pts',(-2.57184523681886,-0.97371146348928,
12.5141420429941));
#417323=CARTESIAN_POINT('Ctrl Pts',(-2.57110462778719,-0.975668656611362,
12.5093757677094));
#417324=CARTESIAN_POINT('Ctrl Pts',(-2.5700775357896,-0.978366730847705,
12.5051960112707));
#417325=CARTESIAN_POINT('Ctrl Pts',(-2.56939136752673,-0.980169230444812,
12.5024036458141));
#417326=CARTESIAN_POINT('Ctrl Pts',(-2.56856054415956,-0.982346042302609,
12.4998248032393));
#417327=CARTESIAN_POINT('Ctrl Pts',(-2.56761198670786,-0.984819113194947,
12.4976950015772));
#417328=CARTESIAN_POINT('Ctrl Pts',(-2.56663670273197,-0.987361865253058,
12.495505190692));
#417329=CARTESIAN_POINT('Ctrl Pts',(-2.56551161662063,-0.990283297342725,
12.4937456938368));
#417330=CARTESIAN_POINT('Ctrl Pts',(-2.5643210116685,-0.993356808561481,
12.4925987732155));
#417331=CARTESIAN_POINT('Ctrl Pts',(-2.56313068531333,-0.996429600590463,
12.4914521209692));
#417332=CARTESIAN_POINT('Ctrl Pts',(-2.56184507179927,-0.999730967481363,
12.4908873016276));
#417333=CARTESIAN_POINT('Ctrl Pts',(-2.56057224318229,-1.00298045217462,
12.4908873016278));
#417334=CARTESIAN_POINT('',(-2.57317806984304,-0.970182777047111,13.7435492065112));
#417335=CARTESIAN_POINT('',(-2.57317806984304,-0.970182777047112,14.));
#417336=CARTESIAN_POINT('',(-2.59889252071644,-0.899031515445461,13.7435492065112));
#417337=CARTESIAN_POINT('Origin',(0.,2.5406128344257E-15,13.7435492065112));
#417338=CARTESIAN_POINT('',(-2.59889252071644,-0.899031515445462,12.5369868989719));
#417339=CARTESIAN_POINT('',(-2.59889252071644,-0.899031515445462,14.));
#417340=CARTESIAN_POINT('Ctrl Pts',(-2.61016708928295,-0.865752716440546,
12.4908873016278));
#417341=CARTESIAN_POINT('Ctrl Pts',(-2.60948036585335,-0.867823126225396,
12.4908873016278));
#417342=CARTESIAN_POINT('Ctrl Pts',(-2.60878725580526,-0.869904371787742,
12.4911020829134));
#417343=CARTESIAN_POINT('Ctrl Pts',(-2.60811003278142,-0.871930075696962,
12.4915448903141));
#417344=CARTESIAN_POINT('Ctrl Pts',(-2.60695138671304,-0.875395808236311,
12.4923024798169));
#417345=CARTESIAN_POINT('Ctrl Pts',(-2.60581238785919,-0.878778471845899,
12.4937722312795));
#417346=CARTESIAN_POINT('Ctrl Pts',(-2.60480847489498,-0.881744185756441,
12.4958030942394));
#417347=CARTESIAN_POINT('Ctrl Pts',(-2.60381164788723,-0.884688966657447,
12.4978196226833));
#417348=CARTESIAN_POINT('Ctrl Pts',(-2.60291875928919,-0.887310064809837,
12.5004326847668));
#417349=CARTESIAN_POINT('Ctrl Pts',(-2.60217987693727,-0.889471690422325,
12.5033504258767));
#417350=CARTESIAN_POINT('Ctrl Pts',(-2.60129704304054,-0.892054451206593,
12.5068366111226));
#417351=CARTESIAN_POINT('Ctrl Pts',(-2.60060591901935,-0.894064458855623,
12.5108395010833));
#417352=CARTESIAN_POINT('Ctrl Pts',(-2.60010115237114,-0.895530009233791,
12.5149868989719));
#417353=CARTESIAN_POINT('Ctrl Pts',(-2.59925334866065,-0.89799154082057,
12.5219528491417));
#417354=CARTESIAN_POINT('Ctrl Pts',(-2.59889252070412,-0.899031515481953,
12.5295503425868));
#417355=CARTESIAN_POINT('Ctrl Pts',(-2.59889252071644,-0.899031515445462,
12.5369868989719));
#417356=CARTESIAN_POINT('',(-2.6436949351547,-0.75721667297901,12.5369868989719));
#417357=CARTESIAN_POINT('Ctrl Pts',(-2.6436949351547,-0.757216672979009,
12.5369868989719));
#417358=CARTESIAN_POINT('Ctrl Pts',(-2.6436949351547,-0.757216672979011,
12.5309445149785));
#417359=CARTESIAN_POINT('Ctrl Pts',(-2.64349601395317,-0.757912639281242,
12.5248274368704));
#417360=CARTESIAN_POINT('Ctrl Pts',(-2.64303846779244,-0.759504876725223,
12.5190199595513));
#417361=CARTESIAN_POINT('Ctrl Pts',(-2.64265415772621,-0.760842256273028,
12.5141420429941));
#417362=CARTESIAN_POINT('Ctrl Pts',(-2.64207554241915,-0.762853303508013,
12.5093757677094));
#417363=CARTESIAN_POINT('Ctrl Pts',(-2.64127178608342,-0.76562611765777,
12.5051960112707));
#417364=CARTESIAN_POINT('Ctrl Pts',(-2.64073482143959,-0.767478548669664,
12.5024036458141));
#417365=CARTESIAN_POINT('Ctrl Pts',(-2.64008419294358,-0.769715837182991,
12.4998248032393));
#417366=CARTESIAN_POINT('Ctrl Pts',(-2.63934036997515,-0.77225799537424,
12.4976950015772));
#417367=CARTESIAN_POINT('Ctrl Pts',(-2.63857558907473,-0.774871781332769,
12.495505190692));
#417368=CARTESIAN_POINT('Ctrl Pts',(-2.63769237043116,-0.777875197561024,
12.4937456938368));
#417369=CARTESIAN_POINT('Ctrl Pts',(-2.63675624681621,-0.781035527281383,
12.4925987732155));
#417370=CARTESIAN_POINT('Ctrl Pts',(-2.63582034225057,-0.784195117496772,
12.4914521209692));
#417371=CARTESIAN_POINT('Ctrl Pts',(-2.63480809855942,-0.787590288798135,
12.4908873016276));
#417372=CARTESIAN_POINT('Ctrl Pts',(-2.63380436834391,-0.790932708447788,
12.4908873016278));
#417373=CARTESIAN_POINT('',(-2.6436949351547,-0.757216672979011,13.7435492065112));
#417374=CARTESIAN_POINT('',(-2.6436949351547,-0.757216672979012,14.));
#417375=CARTESIAN_POINT('',(-2.66352433495749,-0.684206194863278,13.7435492065112));
#417376=CARTESIAN_POINT('Origin',(0.,2.5406128344257E-15,13.7435492065112));
#417377=CARTESIAN_POINT('',(-2.66352433495749,-0.684206194863278,12.5369868989719));
#417378=CARTESIAN_POINT('',(-2.66352433495749,-0.684206194863278,14.));
#417379=CARTESIAN_POINT('Ctrl Pts',(-2.67204885726298,-0.650119146310585,
12.4908873016278));
#417380=CARTESIAN_POINT('Ctrl Pts',(-2.67153317646716,-0.652238641312415,
12.4908873016278));
#417381=CARTESIAN_POINT('Ctrl Pts',(-2.67101201352024,-0.654369456605282,
12.4911020829134));
#417382=CARTESIAN_POINT('Ctrl Pts',(-2.67050215757447,-0.656443620115327,
12.4915448903141));
#417383=CARTESIAN_POINT('Ctrl Pts',(-2.66962985618155,-0.659992261126472,
12.4923024798169));
#417384=CARTESIAN_POINT('Ctrl Pts',(-2.66877036573973,-0.663456508182488,
12.4937722312795));
#417385=CARTESIAN_POINT('Ctrl Pts',(-2.66801152642914,-0.666494182151103,
12.4958030942394));
#417386=CARTESIAN_POINT('Ctrl Pts',(-2.66725804326247,-0.669510415191811,
12.4978196226833));
#417387=CARTESIAN_POINT('Ctrl Pts',(-2.66658176951009,-0.672195570566237,
12.5004326847668));
#417388=CARTESIAN_POINT('Ctrl Pts',(-2.66602153828321,-0.674410229318952,
12.5033504258767));
#417389=CARTESIAN_POINT('Ctrl Pts',(-2.66535216092455,-0.677056355338186,
12.5068366111226));
#417390=CARTESIAN_POINT('Ctrl Pts',(-2.66482717084492,-0.679116007876387,
12.5108395010833));
#417391=CARTESIAN_POINT('Ctrl Pts',(-2.66444353972741,-0.680617824924426,
12.5149868989719));
#417392=CARTESIAN_POINT('Ctrl Pts',(-2.6637991946899,-0.683140269840942,
12.5219528491417));
#417393=CARTESIAN_POINT('Ctrl Pts',(-2.66352433494818,-0.684206194900652,
12.5295503425868));
#417394=CARTESIAN_POINT('Ctrl Pts',(-2.66352433495749,-0.684206194863278,
12.5369868989719));
#417395=CARTESIAN_POINT('',(-2.69661844685186,-0.539211416884192,12.5369868989719));
#417396=CARTESIAN_POINT('Ctrl Pts',(-2.69661844685186,-0.539211416884191,
12.5369868989719));
#417397=CARTESIAN_POINT('Ctrl Pts',(-2.69661844685186,-0.539211416884193,
12.5309445149785));
#417398=CARTESIAN_POINT('Ctrl Pts',(-2.69647691525889,-0.539921281340585,
12.5248274368704));
#417399=CARTESIAN_POINT('Ctrl Pts',(-2.69615067367856,-0.541545515005572,
12.5190199595513));
#417400=CARTESIAN_POINT('Ctrl Pts',(-2.69587665122115,-0.542909769371416,
12.5141420429941));
#417401=CARTESIAN_POINT('Ctrl Pts',(-2.69546388022809,-0.544961287531754,
12.5093757677094));
#417402=CARTESIAN_POINT('Ctrl Pts',(-2.69488880842001,-0.547790388974241,
12.5051960112707));
#417403=CARTESIAN_POINT('Ctrl Pts',(-2.69450462080634,-0.549680423778167,
12.5024036458141));
#417404=CARTESIAN_POINT('Ctrl Pts',(-2.69403851700679,-0.551963300161093,
12.4998248032393));
#417405=CARTESIAN_POINT('Ctrl Pts',(-2.69350437854076,-0.554557628007917,
12.4976950015772));
#417406=CARTESIAN_POINT('Ctrl Pts',(-2.69295519020651,-0.557225053552556,
12.495505190692));
#417407=CARTESIAN_POINT('Ctrl Pts',(-2.69231971670508,-0.560290466679928,
12.4937456938368));
#417408=CARTESIAN_POINT('Ctrl Pts',(-2.69164430417551,-0.563516583429017,
12.4925987732155));
#417409=CARTESIAN_POINT('Ctrl Pts',(-2.69096904968987,-0.566741945279226,
12.4914521209692));
#417410=CARTESIAN_POINT('Ctrl Pts',(-2.6902369121364,-0.570208326686206,
12.4908873016276));
#417411=CARTESIAN_POINT('Ctrl Pts',(-2.68950895998132,-0.573621438040947,
12.4908873016278));
#417412=CARTESIAN_POINT('',(-2.69661844685186,-0.539211416884193,13.7435492065112));
#417413=CARTESIAN_POINT('',(-2.69661844685186,-0.539211416884193,14.));
#417414=CARTESIAN_POINT('',(-2.71043083419997,-0.464827594940355,13.7435492065112));
#417415=CARTESIAN_POINT('Origin',(0.,2.5406128344257E-15,13.7435492065112));
#417416=CARTESIAN_POINT('',(-2.71043083419997,-0.464827594940355,12.5369868989719));
#417417=CARTESIAN_POINT('',(-2.71043083419998,-0.464827594940355,14.));
#417418=CARTESIAN_POINT('Ctrl Pts',(-2.71614858095496,-0.430159140524035,
12.4908873016278));
#417419=CARTESIAN_POINT('Ctrl Pts',(-2.71580737456352,-0.4323136158533,
12.4908873016278));
#417420=CARTESIAN_POINT('Ctrl Pts',(-2.71546162697122,-0.434479820652474,
12.4911020829134));
#417421=CARTESIAN_POINT('Ctrl Pts',(-2.7151225311107,-0.436588640547398,
12.4915448903141));
#417422=CARTESIAN_POINT('Ctrl Pts',(-2.71454237941509,-0.440196574409895,
12.4923024798169));
#417423=CARTESIAN_POINT('Ctrl Pts',(-2.71396811715238,-0.443719350919741,
12.4937722312795));
#417424=CARTESIAN_POINT('Ctrl Pts',(-2.71345940144583,-0.446808769727349,
12.4958030942394));
#417425=CARTESIAN_POINT('Ctrl Pts',(-2.7129542764264,-0.449876382374515,
12.4978196226833));
#417426=CARTESIAN_POINT('Ctrl Pts',(-2.71249911800992,-0.452607725704981,
12.5004326847668));
#417427=CARTESIAN_POINT('Ctrl Pts',(-2.71212126615447,-0.454860679409316,
12.5033504258767));
#417428=CARTESIAN_POINT('Ctrl Pts',(-2.71166979992975,-0.457552561131439,
12.5068366111226));
#417429=CARTESIAN_POINT('Ctrl Pts',(-2.71131443751405,-0.459648151910989,
12.5108395010833));
#417430=CARTESIAN_POINT('Ctrl Pts',(-2.71105449492904,-0.461176241284225,
12.5149868989719));
#417431=CARTESIAN_POINT('Ctrl Pts',(-2.71061789657441,-0.463742813075734,
12.5219528491417));
#417432=CARTESIAN_POINT('Ctrl Pts',(-2.71043083419375,-0.464827594978363,
12.5295503425868));
#417433=CARTESIAN_POINT('Ctrl Pts',(-2.71043083419997,-0.464827594940355,
12.5369868989719));
#417434=CARTESIAN_POINT('',(-2.73159640769595,-0.31761779777363,12.5369868989719));
#417435=CARTESIAN_POINT('Ctrl Pts',(-2.73159640769595,-0.317617797773629,
12.5369868989719));
#417436=CARTESIAN_POINT('Ctrl Pts',(-2.73159640769595,-0.317617797773631,
12.5309445149785));
#417437=CARTESIAN_POINT('Ctrl Pts',(-2.73151320758094,-0.318336836353346,
12.5248274368704));
#417438=CARTESIAN_POINT('Ctrl Pts',(-2.7313204416649,-0.319982257232279,
12.5190199595513));
#417439=CARTESIAN_POINT('Ctrl Pts',(-2.73115853039054,-0.321364307528444,
12.5141420429941));
#417440=CARTESIAN_POINT('Ctrl Pts',(-2.73091435063435,-0.323442644099255,
12.5093757677094));
#417441=CARTESIAN_POINT('Ctrl Pts',(-2.73057179036193,-0.326309205631141,
12.5051960112707));
#417442=CARTESIAN_POINT('Ctrl Pts',(-2.7303429364836,-0.328224266357311,
12.5024036458141));
#417443=CARTESIAN_POINT('Ctrl Pts',(-2.73006445922439,-0.330537538444158,
12.4998248032393));
#417444=CARTESIAN_POINT('Ctrl Pts',(-2.72974355986412,-0.333166771122769,
12.4976950015772));
#417445=CARTESIAN_POINT('Ctrl Pts',(-2.72941361885381,-0.335870084976612,
12.495505190692));
#417446=CARTESIAN_POINT('Ctrl Pts',(-2.72903011946582,-0.338977095184496,
12.4937456938368));
#417447=CARTESIAN_POINT('Ctrl Pts',(-2.72861991278058,-0.342247529687623,
12.4925987732155));
#417448=CARTESIAN_POINT('Ctrl Pts',(-2.72820980208213,-0.345517198921685,
12.4914521209692));
#417449=CARTESIAN_POINT('Ctrl Pts',(-2.72776264292095,-0.349031722237931,
12.4908873016276));
#417450=CARTESIAN_POINT('Ctrl Pts',(-2.72731531322781,-0.352492811604818,
12.4908873016278));
#417451=CARTESIAN_POINT('',(-2.73159640769595,-0.317617797773631,13.7435492065112));
#417452=CARTESIAN_POINT('',(-2.73159640769595,-0.317617797773632,14.));
#417453=CARTESIAN_POINT('',(-2.73929986343047,-0.242355644064259,13.7435492065112));
#417454=CARTESIAN_POINT('Origin',(0.,2.5406128344257E-15,13.7435492065112));
#417455=CARTESIAN_POINT('',(-2.73929986343047,-0.24235564406426,12.5369868989719));
#417456=CARTESIAN_POINT('',(-2.73929986343047,-0.24235564406426,14.));
#417457=CARTESIAN_POINT('Ctrl Pts',(-2.74217278397365,-0.207336496628562,
12.4908873016278));
#417458=CARTESIAN_POINT('Ctrl Pts',(-2.74200832265884,-0.209511614607407,
12.4908873016278));
#417459=CARTESIAN_POINT('Ctrl Pts',(-2.74184029131432,-0.211698793177349,
12.4911020829134));
#417460=CARTESIAN_POINT('Ctrl Pts',(-2.74167421216608,-0.213828235608682,
12.4915448903141));
#417461=CARTESIAN_POINT('Ctrl Pts',(-2.74139007098159,-0.217471452117943,
12.4923024798169));
#417462=CARTESIAN_POINT('Ctrl Pts',(-2.7411048585186,-0.221029314585163,
12.4937722312795));
#417463=CARTESIAN_POINT('Ctrl Pts',(-2.74084965183518,-0.224149918659317,
12.4958030942394));
#417464=CARTESIAN_POINT('Ctrl Pts',(-2.74059624648665,-0.227248496456896,
12.4978196226833));
#417465=CARTESIAN_POINT('Ctrl Pts',(-2.74036523241025,-0.230007851104178,
12.5004326847668));
#417466=CARTESIAN_POINT('Ctrl Pts',(-2.74017227446798,-0.232284106724942,
12.5033504258767));
#417467=CARTESIAN_POINT('Ctrl Pts',(-2.73994172381044,-0.235003830121222,
12.5068366111226));
#417468=CARTESIAN_POINT('Ctrl Pts',(-2.73975835393691,-0.23712141333123,
12.5108395010833));
#417469=CARTESIAN_POINT('Ctrl Pts',(-2.73962382975943,-0.238665605847002,
12.5149868989719));
#417470=CARTESIAN_POINT('Ctrl Pts',(-2.7393978835777,-0.241259224401685,
12.5219528491417));
#417471=CARTESIAN_POINT('Ctrl Pts',(-2.73929986342736,-0.242355644102649,
12.5295503425868));
#417472=CARTESIAN_POINT('Ctrl Pts',(-2.73929986343047,-0.24235564406426,
12.5369868989719));
#417473=CARTESIAN_POINT('',(-2.74839604512851,-0.0939104846221332,12.5369868989719));
#417474=CARTESIAN_POINT('Ctrl Pts',(-2.74839604512851,-0.093910484622133,
12.5369868989719));
#417475=CARTESIAN_POINT('Ctrl Pts',(-2.74839604512851,-0.0939104846221349,
12.5309445149785));
#417476=CARTESIAN_POINT('Ctrl Pts',(-2.74837173017449,-0.0946339122420582,
12.5248274368704));
#417477=CARTESIAN_POINT('Ctrl Pts',(-2.74831372274811,-0.0962895703304627,
12.5190199595513));
#417478=CARTESIAN_POINT('Ctrl Pts',(-2.74826500014963,-0.0976802192402491,
12.5141420429941));
#417479=CARTESIAN_POINT('Ctrl Pts',(-2.74819103660629,-0.0997715432345554,
12.5093757677094));
#417480=CARTESIAN_POINT('Ctrl Pts',(-2.74808326755163,-0.102656488361795,
12.5051960112707));
#417481=CARTESIAN_POINT('Ctrl Pts',(-2.74801127039343,-0.10458383059704,
12.5024036458141));
#417482=CARTESIAN_POINT('Ctrl Pts',(-2.74792227289478,-0.106912103943732,
12.4998248032393));
#417483=CARTESIAN_POINT('Ctrl Pts',(-2.74781674817257,-0.109558744344448,
12.4976950015772));
#417484=CARTESIAN_POINT('Ctrl Pts',(-2.74770825018919,-0.112279956399813,
12.495505190692));
#417485=CARTESIAN_POINT('Ctrl Pts',(-2.74757927703979,-0.115407887047896,
12.4937456938368));
#417486=CARTESIAN_POINT('Ctrl Pts',(-2.74743700605669,-0.118700875103026,
12.4925987732155));
#417487=CARTESIAN_POINT('Ctrl Pts',(-2.74729476836446,-0.121993092611647,
12.4914521209692));
#417488=CARTESIAN_POINT('Ctrl Pts',(-2.74713556336602,-0.125532369264345,
12.4908873016276));
#417489=CARTESIAN_POINT('Ctrl Pts',(-2.74697183304012,-0.129018403664679,
12.4908873016278));
#417490=CARTESIAN_POINT('',(-2.74839604512851,-0.0939104846221349,13.7435492065112));
#417491=CARTESIAN_POINT('',(-2.74839604512851,-0.093910484622135,14.));
#417492=CARTESIAN_POINT('',(-2.7499393040225,-0.0182708563627825,13.7435492065112));
#417493=CARTESIAN_POINT('Origin',(0.,2.5406128344257E-15,13.7435492065112));
#417494=CARTESIAN_POINT('',(-2.74993930402251,-0.0182708563627825,12.5369868989719));
#417495=CARTESIAN_POINT('',(-2.74993930402251,-0.0182708563627825,14.));
#417496=CARTESIAN_POINT('Ctrl Pts',(-2.74994827954166,0.0168659374438614,
12.4908873016278));
#417497=CARTESIAN_POINT('Ctrl Pts',(-2.7499616577664,0.0146846518667144,
12.4908873016278));
#417498=CARTESIAN_POINT('Ctrl Pts',(-2.74997246089054,0.0124910548385303,
12.4911020829134));
#417499=CARTESIAN_POINT('Ctrl Pts',(-2.74998050368389,0.0103551609588346,
12.4915448903141));
#417500=CARTESIAN_POINT('Ctrl Pts',(-2.74999426392324,0.00670090680759111,
12.4923024798169));
#417501=CARTESIAN_POINT('Ctrl Pts',(-2.74999999930185,0.00313163537071014,
12.4937722312795));
#417502=CARTESIAN_POINT('Ctrl Pts',(-2.74999999999993,6.13135258656274E-7,
12.4958030942394));
#417503=CARTESIAN_POINT('Ctrl Pts',(-2.75000000069309,-0.00310830928871901,
12.4978196226833));
#417504=CARTESIAN_POINT('Ctrl Pts',(-2.74999466831732,-0.00587731220289936,
12.5004326847668));
#417505=CARTESIAN_POINT('Ctrl Pts',(-2.74998788839151,-0.00816172163449239,
12.5033504258767));
#417506=CARTESIAN_POINT('Ctrl Pts',(-2.74997978757774,-0.0108911873944495,
12.5068366111226));
#417507=CARTESIAN_POINT('Ctrl Pts',(-2.74996963054264,-0.0130166708680302,
12.5108395010833));
#417508=CARTESIAN_POINT('Ctrl Pts',(-2.74996142000887,-0.0145666901799197,
12.5149868989719));
#417509=CARTESIAN_POINT('Ctrl Pts',(-2.74994762963462,-0.0171700953942134,
12.5219528491417));
#417510=CARTESIAN_POINT('Ctrl Pts',(-2.74993930402254,-0.0182708564012972,
12.5295503425868));
#417511=CARTESIAN_POINT('Ctrl Pts',(-2.74993930402251,-0.0182708563627825,
12.5369868989719));
#417512=CARTESIAN_POINT('',(-2.74690556033417,0.130421787310385,12.5369868989719));
#417513=CARTESIAN_POINT('Ctrl Pts',(-2.74690556033417,0.130421787310385,
12.5369868989719));
#417514=CARTESIAN_POINT('Ctrl Pts',(-2.74690556033417,0.130421787310383,
12.5309445149785));
#417515=CARTESIAN_POINT('Ctrl Pts',(-2.74694029235315,0.129698784941705,
12.5248274368704));
#417516=CARTESIAN_POINT('Ctrl Pts',(-2.74701742944628,0.128043907775242,
12.5190199595513));
#417517=CARTESIAN_POINT('Ctrl Pts',(-2.74708221976453,0.126653914790889,
12.5141420429941));
#417518=CARTESIAN_POINT('Ctrl Pts',(-2.74717896464922,0.124563520789225,
12.5093757677094));
#417519=CARTESIAN_POINT('Ctrl Pts',(-2.74730670399759,0.12167939090047,
12.5051960112707));
#417520=CARTESIAN_POINT('Ctrl Pts',(-2.74739204268874,0.119752593300737,
12.5024036458141));
#417521=CARTESIAN_POINT('Ctrl Pts',(-2.74749311721431,0.117424812969185,
12.4998248032393));
#417522=CARTESIAN_POINT('Ctrl Pts',(-2.74760366937978,0.114778377801565,
12.4976950015772));
#417523=CARTESIAN_POINT('Ctrl Pts',(-2.7477173364595,0.112057376761939,
12.495505190692));
#417524=CARTESIAN_POINT('Ctrl Pts',(-2.74784374784373,0.108929341536047,
12.4937456938368));
#417525=CARTESIAN_POINT('Ctrl Pts',(-2.7479703593527,0.105635714221117,
12.4925987732155));
#417526=CARTESIAN_POINT('Ctrl Pts',(-2.74809694123506,0.10234285760228,
12.4914521209692));
#417527=CARTESIAN_POINT('Ctrl Pts',(-2.74822674988235,0.0988023809153136,
12.4908873016276));
#417528=CARTESIAN_POINT('Ctrl Pts',(-2.748347708522,0.0953146004653097,
12.4908873016278));
#417529=CARTESIAN_POINT('',(-2.74690556033417,0.130421787310383,13.7435492065112));
#417530=CARTESIAN_POINT('',(-2.74690556033417,0.130421787310383,14.));
#417531=CARTESIAN_POINT('',(-2.74227835225431,0.205935520873309,13.7435492065112));
#417532=CARTESIAN_POINT('Origin',(0.,2.5406128344257E-15,13.7435492065112));
#417533=CARTESIAN_POINT('',(-2.74227835225432,0.205935520873309,12.5369868989719));
#417534=CARTESIAN_POINT('',(-2.74227835225432,0.205935520873309,14.));
#417535=CARTESIAN_POINT('Ctrl Pts',(-2.73942332301885,0.240956131485279,
12.4908873016278));
#417536=CARTESIAN_POINT('Ctrl Pts',(-2.73961445175325,0.23878319440546,
12.4908873016278));
#417537=CARTESIAN_POINT('Ctrl Pts',(-2.73980401745305,0.236597776945337,
12.4911020829134));
#417538=CARTESIAN_POINT('Ctrl Pts',(-2.73998612866454,0.234469645638651,
12.4915448903141));
#417539=CARTESIAN_POINT('Ctrl Pts',(-2.74029769875559,0.230828672303891,
12.4923024798169));
#417540=CARTESIAN_POINT('Ctrl Pts',(-2.7405943438078,0.227271744809874,
12.4937722312795));
#417541=CARTESIAN_POINT('Ctrl Pts',(-2.74084955188275,0.22415114084952,
12.4958030942394));
#417542=CARTESIAN_POINT('Ctrl Pts',(-2.74110295861298,0.221052563164939,
12.4978196226833));
#417543=CARTESIAN_POINT('Ctrl Pts',(-2.74132334342393,0.2182923392414,12.5004326847668));
#417544=CARTESIAN_POINT('Ctrl Pts',(-2.74150278663385,0.216014978366845,
12.5033504258767));
#417545=CARTESIAN_POINT('Ctrl Pts',(-2.74171718957344,0.213293934387513,
12.5068366111226));
#417546=CARTESIAN_POINT('Ctrl Pts',(-2.74188031297015,0.211174695392196,
12.5108395010833));
#417547=CARTESIAN_POINT('Ctrl Pts',(-2.74199847071986,0.209629164406974,
12.5149868989719));
#417548=CARTESIAN_POINT('Ctrl Pts',(-2.74219692792574,0.20703329776524,
12.5219528491417));
#417549=CARTESIAN_POINT('Ctrl Pts',(-2.74227835225749,0.205935520834925,
12.5295503425868));
#417550=CARTESIAN_POINT('Ctrl Pts',(-2.74227835225432,0.205935520873309,
12.5369868989719));
#417551=CARTESIAN_POINT('',(-2.72713487224332,0.353886123766432,12.5369868989719));
#417552=CARTESIAN_POINT('Ctrl Pts',(-2.72713487224332,0.353886123766432,
12.5369868989719));
#417553=CARTESIAN_POINT('Ctrl Pts',(-2.72713487224332,0.35388612376643,
12.5309445149785));
#417554=CARTESIAN_POINT('Ctrl Pts',(-2.72722842009945,0.353168358110474,
12.5248274368704));
#417555=CARTESIAN_POINT('Ctrl Pts',(-2.72744018837746,0.351525274800461,
12.5190199595513));
#417556=CARTESIAN_POINT('Ctrl Pts',(-2.72761806044356,0.350145187915518,
12.5141420429941));
#417557=CARTESIAN_POINT('Ctrl Pts',(-2.72788486993503,0.348069635133687,
12.5093757677094));
#417558=CARTESIAN_POINT('Ctrl Pts',(-2.72824726760215,0.345205513891979,
12.5051960112707));
#417559=CARTESIAN_POINT('Ctrl Pts',(-2.72848937422774,0.343292083447885,
12.5024036458141));
#417560=CARTESIAN_POINT('Ctrl Pts',(-2.72877984814325,0.340980287125521,
12.4998248032393));
#417561=CARTESIAN_POINT('Ctrl Pts',(-2.72910574148997,0.338351668780409,
12.4976950015772));
#417562=CARTESIAN_POINT('Ctrl Pts',(-2.72944081719713,0.335648986569506,
12.495505190692));
#417563=CARTESIAN_POINT('Ctrl Pts',(-2.72982177186808,0.332541663324144,
12.4937456938368));
#417564=CARTESIAN_POINT('Ctrl Pts',(-2.7302164232904,0.329269315295784,
12.4925987732155));
#417565=CARTESIAN_POINT('Ctrl Pts',(-2.73061098236582,0.325997732984245,
12.4914521209692));
#417566=CARTESIAN_POINT('Ctrl Pts',(-2.73102894080372,0.322479617551225,
12.4908873016276));
#417567=CARTESIAN_POINT('Ctrl Pts',(-2.73143378344912,0.319013301655004,
12.4908873016278));
#417568=CARTESIAN_POINT('',(-2.72713487224332,0.35388612376643,13.7435492065112));
#417569=CARTESIAN_POINT('',(-2.72713487224332,0.353886123766431,14.));
#417570=CARTESIAN_POINT('',(-2.71636799049595,0.428771431194959,13.7435492065112));
#417571=CARTESIAN_POINT('Origin',(0.,2.5406128344257E-15,13.7435492065112));
#417572=CARTESIAN_POINT('',(-2.71636799049596,0.428771431194959,12.5369868989719));
#417573=CARTESIAN_POINT('',(-2.71636799049596,0.428771431194959,14.));
#417574=CARTESIAN_POINT('Ctrl Pts',(-2.71066795625439,0.463442802226626,
12.4908873016278));
#417575=CARTESIAN_POINT('Ctrl Pts',(-2.71103556356826,0.461292674181891,
12.4908873016278));
#417576=CARTESIAN_POINT('Ctrl Pts',(-2.71140263031526,0.459129979882459,
12.4911020829134));
#417577=CARTESIAN_POINT('Ctrl Pts',(-2.71175759802481,0.457023773511512,
12.4915448903141));
#417578=CARTESIAN_POINT('Ctrl Pts',(-2.71236490452002,0.45342031107006,
12.4923024798169));
#417579=CARTESIAN_POINT('Ctrl Pts',(-2.71295048512196,0.449899398284527,
12.4937722312795));
#417580=CARTESIAN_POINT('Ctrl Pts',(-2.71345920220613,0.446809979703764,
12.4958030942394));
#417581=CARTESIAN_POINT('Ctrl Pts',(-2.71396432859346,0.443742367281841,
12.4978196226833));
#417582=CARTESIAN_POINT('Ctrl Pts',(-2.71440896396657,0.44100929118375,
12.5004326847668));
#417583=CARTESIAN_POINT('Ctrl Pts',(-2.71477343614727,0.438754134327114,
12.5033504258767));
#417584=CARTESIAN_POINT('Ctrl Pts',(-2.71520891602402,0.436059620227148,
12.5068366111226));
#417585=CARTESIAN_POINT('Ctrl Pts',(-2.71554423429326,0.43396072889596,
12.5108395010833));
#417586=CARTESIAN_POINT('Ctrl Pts',(-2.71578797400611,0.432429971491118,
12.5149868989719));
#417587=CARTESIAN_POINT('Ctrl Pts',(-2.71619735809216,0.429858918486156,
12.5219528491417));
#417588=CARTESIAN_POINT('Ctrl Pts',(-2.71636799050224,0.428771431156961,
12.5295503425868));
#417589=CARTESIAN_POINT('Ctrl Pts',(-2.71636799049596,0.428771431194959,
12.5369868989719));
#417590=CARTESIAN_POINT('',(-2.68921555152327,0.574995406455915,12.5369868989719));
#417591=CARTESIAN_POINT('Ctrl Pts',(-2.68921555152327,0.574995406455915,
12.5369868989719));
#417592=CARTESIAN_POINT('Ctrl Pts',(-2.68921555152327,0.574995406455913,
12.5309445149785));
#417593=CARTESIAN_POINT('Ctrl Pts',(-2.689367292671,0.574287654124696,12.5248274368704));
#417594=CARTESIAN_POINT('Ctrl Pts',(-2.68971228285094,0.57266729911947,
12.5190199595513));
#417595=CARTESIAN_POINT('Ctrl Pts',(-2.69000205295564,0.571306302584459,
12.5141420429941));
#417596=CARTESIAN_POINT('Ctrl Pts',(-2.69043715148075,0.569259403483782,
12.5093757677094));
#417597=CARTESIAN_POINT('Ctrl Pts',(-2.69103179576993,0.566434351143439,
12.5051960112707));
#417598=CARTESIAN_POINT('Ctrl Pts',(-2.69142905915031,0.564547021418895,
12.5024036458141));
#417599=CARTESIAN_POINT('Ctrl Pts',(-2.69190699939977,0.562266593728825,
12.4998248032393));
#417600=CARTESIAN_POINT('Ctrl Pts',(-2.69244606516129,0.559673285227614,
12.4976950015772));
#417601=CARTESIAN_POINT('Ctrl Pts',(-2.69300031962234,0.557006907749637,
12.495505190692));
#417602=CARTESIAN_POINT('Ctrl Pts',(-2.69363328238953,0.553940975208331,
12.4937456938368));
#417603=CARTESIAN_POINT('Ctrl Pts',(-2.69429334738511,0.55071168340277,
12.4925987732155));
#417604=CARTESIAN_POINT('Ctrl Pts',(-2.69495325792803,0.547483147239041,
12.4914521209692));
#417605=CARTESIAN_POINT('Ctrl Pts',(-2.69565658471209,0.544010805537726,
12.4908873016276));
#417606=CARTESIAN_POINT('Ctrl Pts',(-2.69634261720224,0.540589021955674,
12.4908873016278));
#417607=CARTESIAN_POINT('',(-2.68921555152327,0.574995406455913,13.7435492065112));
#417608=CARTESIAN_POINT('',(-2.68921555152327,0.574995406455914,14.));
#417609=CARTESIAN_POINT('',(-2.67238064793001,0.648753938384312,13.7435492065112));
#417610=CARTESIAN_POINT('Origin',(0.,2.5406128344257E-15,13.7435492065112));
#417611=CARTESIAN_POINT('',(-2.67238064793002,0.648753938384312,12.5369868989719));
#417612=CARTESIAN_POINT('',(-2.67238064793002,0.648753938384313,14.));
#417613=CARTESIAN_POINT('Ctrl Pts',(-2.66387354146978,0.682845337581834,
12.4908873016278));
#417614=CARTESIAN_POINT('Ctrl Pts',(-2.6644151809971,0.680732327319576,
12.4908873016278));
#417615=CARTESIAN_POINT('Ctrl Pts',(-2.66495730602266,0.678606748554576,
12.4911020829134));
#417616=CARTESIAN_POINT('Ctrl Pts',(-2.66548276797874,0.676536483575267,
12.4915448903141));
#417617=CARTESIAN_POINT('Ctrl Pts',(-2.66638176935357,0.672994512475143,
12.4923024798169));
#417618=CARTESIAN_POINT('Ctrl Pts',(-2.66725238856295,0.669533045491771,
12.4937722312795));
#417619=CARTESIAN_POINT('Ctrl Pts',(-2.66801122922809,0.666495371861536,
12.4958030942394));
#417620=CARTESIAN_POINT('Ctrl Pts',(-2.66876471373974,0.663479139156819,
12.4978196226833));
#417621=CARTESIAN_POINT('Ctrl Pts',(-2.66943064069996,0.660791399054683,
12.5004326847668));
#417622=CARTESIAN_POINT('Ctrl Pts',(-2.66997771634922,0.658573453912772,
12.5033504258767));
#417623=CARTESIAN_POINT('Ctrl Pts',(-2.6706313751164,0.655923401238945,
12.5068366111226));
#417624=CARTESIAN_POINT('Ctrl Pts',(-2.67113665677041,0.653858825347401,
12.5108395010833));
#417625=CARTESIAN_POINT('Ctrl Pts',(-2.67150435639882,0.652353028460911,
12.5149868989719));
#417626=CARTESIAN_POINT('Ctrl Pts',(-2.67212194298149,0.649823899026276,
12.5219528491417));
#417627=CARTESIAN_POINT('Ctrl Pts',(-2.67238064793938,0.648753938346953,
12.5295503425868));
#417628=CARTESIAN_POINT('Ctrl Pts',(-2.67238064793002,0.648753938384312,
12.5369868989719));
#417629=CARTESIAN_POINT('',(-2.63339994499717,0.792278189582998,12.5369868989719));
#417630=CARTESIAN_POINT('Ctrl Pts',(-2.63339994499717,0.792278189582997,
12.5369868989719));
#417631=CARTESIAN_POINT('Ctrl Pts',(-2.63339994499717,0.792278189582996,
12.5309445149785));
#417632=CARTESIAN_POINT('Ctrl Pts',(-2.63360886962419,0.79158516055151,
12.5248274368704));
#417633=CARTESIAN_POINT('Ctrl Pts',(-2.63408478585334,0.789998317046293,
12.5190199595513));
#417634=CARTESIAN_POINT('Ctrl Pts',(-2.6344845256244,0.788665468068605,
12.5141420429941));
#417635=CARTESIAN_POINT('Ctrl Pts',(-2.63508501767425,0.786660844424882,
12.5093757677094));
#417636=CARTESIAN_POINT('Ctrl Pts',(-2.63590795132585,0.783893661243128,
12.5051960112707));
#417637=CARTESIAN_POINT('Ctrl Pts',(-2.63645772773878,0.782044992106063,
12.5024036458141));
#417638=CARTESIAN_POINT('Ctrl Pts',(-2.63711995370868,0.779811108918321,
12.4998248032393));
#417639=CARTESIAN_POINT('Ctrl Pts',(-2.6378686044913,0.777270368301222,
12.4976950015772));
#417640=CARTESIAN_POINT('Ctrl Pts',(-2.63863834923425,0.774658039858365,
12.495505190692));
#417641=CARTESIAN_POINT('Ctrl Pts',(-2.63951910783489,0.771653901296335,
12.4937456938368));
#417642=CARTESIAN_POINT('Ctrl Pts',(-2.64044019378009,0.768489156117743,
12.4925987732155));
#417643=CARTESIAN_POINT('Ctrl Pts',(-2.64136106419473,0.765325151477321,
12.4914521209692));
#417644=CARTESIAN_POINT('Ctrl Pts',(-2.64234507880124,0.761921691368837,
12.4908873016276));
#417645=CARTESIAN_POINT('Ctrl Pts',(-2.64330773570309,0.75856721150614,
12.4908873016278));
#417646=CARTESIAN_POINT('',(-2.63339994499717,0.792278189582995,13.7435492065112));
#417647=CARTESIAN_POINT('',(-2.63339994499717,0.792278189582996,14.));
#417648=CARTESIAN_POINT('',(-2.61060905306387,0.864419095150583,13.7435492065112));
#417649=CARTESIAN_POINT('Origin',(0.,2.5406128344257E-15,13.7435492065112));
#417650=CARTESIAN_POINT('',(-2.61060905306387,0.864419095150584,12.5369868989719));
#417651=CARTESIAN_POINT('',(-2.61060905306387,0.864419095150584,14.));
#417652=CARTESIAN_POINT('Ctrl Pts',(-2.59935148777489,0.897703649876986,
12.4908873016278));
#417653=CARTESIAN_POINT('Ctrl Pts',(-2.60006355499397,0.895641819131877,
12.4908873016278));
#417654=CARTESIAN_POINT('Ctrl Pts',(-2.60077713054549,0.893567501277296,
12.4911020829134));
#417655=CARTESIAN_POINT('Ctrl Pts',(-2.60146958988548,0.891546954961492,
12.4915448903141));
#417656=CARTESIAN_POINT('Ctrl Pts',(-2.60265430343411,0.888090046435982,
12.4923024798169));
#417657=CARTESIAN_POINT('Ctrl Pts',(-2.60380416742372,0.884711060746445,
12.4937722312795));
#417658=CARTESIAN_POINT('Ctrl Pts',(-2.6048080817104,0.881745347283566,
12.4958030942394));
#417659=CARTESIAN_POINT('Ctrl Pts',(-2.60580491003127,0.878800566827061,
12.4978196226833));
#417660=CARTESIAN_POINT('Ctrl Pts',(-2.60668769694455,0.876176049187813,
12.5004326847668));
#417661=CARTESIAN_POINT('Ctrl Pts',(-2.60741373536419,0.874010075819612,
12.5033504258767));
#417662=CARTESIAN_POINT('Ctrl Pts',(-2.60828122303054,0.87142212023524,
12.5068366111226));
#417663=CARTESIAN_POINT('Ctrl Pts',(-2.60895310550328,0.869405599195268,
12.5108395010833));
#417664=CARTESIAN_POINT('Ctrl Pts',(-2.6094423180669,0.867934783656971,
12.5149868989719));
#417665=CARTESIAN_POINT('Ctrl Pts',(-2.61026399720937,0.865464408731773,
12.5219528491417));
#417666=CARTESIAN_POINT('Ctrl Pts',(-2.61060905307625,0.864419095114112,
12.5295503425868));
#417667=CARTESIAN_POINT('Ctrl Pts',(-2.61060905306387,0.864419095150584,
12.5369868989719));
#417668=CARTESIAN_POINT('',(-2.56005949631752,1.00428849207511,12.5369868989719));
#417669=CARTESIAN_POINT('Ctrl Pts',(-2.56005949631752,1.0042884920751,12.5369868989719));
#417670=CARTESIAN_POINT('Ctrl Pts',(-2.56005949631752,1.0042884920751,12.5309445149785));
#417671=CARTESIAN_POINT('Ctrl Pts',(-2.56032421406491,1.00361479833721,
12.5248274368704));
#417672=CARTESIAN_POINT('Ctrl Pts',(-2.56092788919928,1.00207202651372,
12.5190199595513));
#417673=CARTESIAN_POINT('Ctrl Pts',(-2.56143493843448,1.0007761949834,12.5141420429941));
#417674=CARTESIAN_POINT('Ctrl Pts',(-2.56219682783355,0.998827187236239,
12.5093757677094));
#417675=CARTESIAN_POINT('Ctrl Pts',(-2.5632425743599,0.996136288360594,
12.5051960112707));
#417676=CARTESIAN_POINT('Ctrl Pts',(-2.56394120513404,0.994338582399107,
12.5024036458141));
#417677=CARTESIAN_POINT('Ctrl Pts',(-2.56478330981982,0.992166109837743,
12.4998248032393));
#417678=CARTESIAN_POINT('Ctrl Pts',(-2.5657365634761,0.989694845314369,
12.4976950015772));
#417679=CARTESIAN_POINT('Ctrl Pts',(-2.56671667597669,0.987153950521416,
12.495505190692));
#417680=CARTESIAN_POINT('Ctrl Pts',(-2.56783936910761,0.984231597985143,
12.4937456938368));
#417681=CARTESIAN_POINT('Ctrl Pts',(-2.56901534632743,0.981152460290538,
12.4925987732155));
#417682=CARTESIAN_POINT('Ctrl Pts',(-2.5701910483731,0.978074043102282,
12.4914521209692));
#417683=CARTESIAN_POINT('Ctrl Pts',(-2.57144920234721,0.97476211405212,
12.4908873016276));
#417684=CARTESIAN_POINT('Ctrl Pts',(-2.57268207733792,0.971497261418812,
12.4908873016278));
#417685=CARTESIAN_POINT('',(-2.56005949631752,1.0042884920751,13.7435492065112));
#417686=CARTESIAN_POINT('',(-2.56005949631752,1.0042884920751,14.));
#417687=CARTESIAN_POINT('',(-2.53146428566977,1.07433168545774,13.7435492065112));
#417688=CARTESIAN_POINT('Origin',(0.,2.5406128344257E-15,13.7435492065112));
#417689=CARTESIAN_POINT('',(-2.53146428566977,1.07433168545774,12.5369868989719));
#417690=CARTESIAN_POINT('',(-2.53146428566977,1.07433168545774,14.));
#417691=CARTESIAN_POINT('Ctrl Pts',(-2.51753117879167,1.10658789249288,
12.4908873016278));
#417692=CARTESIAN_POINT('Ctrl Pts',(-2.51840893501265,1.10459096240835,
12.4908873016278));
#417693=CARTESIAN_POINT('Ctrl Pts',(-2.51928921236256,1.10258170970728,
12.4911020829134));
#417694=CARTESIAN_POINT('Ctrl Pts',(-2.52014406088379,1.10062432845734,
12.4915448903141));
#417695=CARTESIAN_POINT('Ctrl Pts',(-2.52160660253303,1.09727548766233,
12.4923024798169));
#417696=CARTESIAN_POINT('Ctrl Pts',(-2.52302805914774,1.0940014698589,12.4937722312795));
#417697=CARTESIAN_POINT('Ctrl Pts',(-2.52427036617201,1.09112745289717,
12.4958030942394));
#417698=CARTESIAN_POINT('Ctrl Pts',(-2.52550390457409,1.08827372171696,
12.4978196226833));
#417699=CARTESIAN_POINT('Ctrl Pts',(-2.52659767663917,1.08572989227247,
12.5004326847668));
#417700=CARTESIAN_POINT('Ctrl Pts',(-2.52749784616328,1.08363030487339,
12.5033504258767));
#417701=CARTESIAN_POINT('Ctrl Pts',(-2.52857338974152,1.0811216687959,12.5068366111226));
#417702=CARTESIAN_POINT('Ctrl Pts',(-2.52940740176599,1.07916662222232,
12.5108395010833));
#417703=CARTESIAN_POINT('Ctrl Pts',(-2.53001487163591,1.07774057606695,
12.5149868989719));
#417704=CARTESIAN_POINT('Ctrl Pts',(-2.53103517519907,1.07534539558874,
12.5219528491417));
#417705=CARTESIAN_POINT('Ctrl Pts',(-2.53146428568508,1.0743316854224,12.5295503425868));
#417706=CARTESIAN_POINT('Ctrl Pts',(-2.53146428566977,1.07433168545774,
12.5369868989719));
#417707=CARTESIAN_POINT('',(-2.46968227406997,1.20961542034839,12.5369868989719));
#417708=CARTESIAN_POINT('Ctrl Pts',(-2.46968227406996,1.20961542034839,
12.5369868989719));
#417709=CARTESIAN_POINT('Ctrl Pts',(-2.46968227406996,1.20961542034839,
12.5309445149785));
#417710=CARTESIAN_POINT('Ctrl Pts',(-2.4700010232848,1.20896554522477,12.5248274368704));
#417711=CARTESIAN_POINT('Ctrl Pts',(-2.47072843996596,1.20747711197495,
12.5190199595513));
#417712=CARTESIAN_POINT('Ctrl Pts',(-2.47133942433629,1.20622692143703,
12.5141420429941));
#417713=CARTESIAN_POINT('Ctrl Pts',(-2.47225764083634,1.20434649991142,
12.5093757677094));
#417714=CARTESIAN_POINT('Ctrl Pts',(-2.47351924096685,1.20174979282994,
12.5051960112707));
#417715=CARTESIAN_POINT('Ctrl Pts',(-2.47436207682967,1.2000150134806,12.5024036458141));
#417716=CARTESIAN_POINT('Ctrl Pts',(-2.47537845616357,1.19791840899208,
12.4998248032393));
#417717=CARTESIAN_POINT('Ctrl Pts',(-2.47652996894771,1.19553306642011,
12.4976950015772));
#417718=CARTESIAN_POINT('Ctrl Pts',(-2.47771392671894,1.19308051451269,
12.495505190692));
#417719=CARTESIAN_POINT('Ctrl Pts',(-2.47907108304259,1.19025939577614,
12.4937456938368));
#417720=CARTESIAN_POINT('Ctrl Pts',(-2.48049412560265,1.18728635671886,
12.4925987732155));
#417721=CARTESIAN_POINT('Ctrl Pts',(-2.48191683517623,1.18431401334126,
12.4914521209692));
#417722=CARTESIAN_POINT('Ctrl Pts',(-2.48344075571082,1.18111565569081,
12.4908873016276));
#417723=CARTESIAN_POINT('Ctrl Pts',(-2.48493564421073,1.17796215734251,
12.4908873016278));
#417724=CARTESIAN_POINT('',(-2.46968227406996,1.20961542034839,13.7435492065112));
#417725=CARTESIAN_POINT('',(-2.46968227406997,1.20961542034839,14.));
#417726=CARTESIAN_POINT('',(-2.43547304111673,1.27709477565043,13.7435492065112));
#417727=CARTESIAN_POINT('Origin',(0.,2.5406128344257E-15,13.7435492065112));
#417728=CARTESIAN_POINT('',(-2.43547304111673,1.27709477565043,12.5369868989719));
#417729=CARTESIAN_POINT('',(-2.43547304111674,1.27709477565043,14.));
#417730=CARTESIAN_POINT('Ctrl Pts',(-2.41895711517699,1.30810797525839,
12.4908873016278));
#417731=CARTESIAN_POINT('Ctrl Pts',(-2.41999471907704,1.30618923507468,
12.4908873016278));
#417732=CARTESIAN_POINT('Ctrl Pts',(-2.42103584012481,1.30425841877233,
12.4911020829134));
#417733=CARTESIAN_POINT('Ctrl Pts',(-2.42204738895142,1.30237722863754,
12.4915448903141));
#417734=CARTESIAN_POINT('Ctrl Pts',(-2.42377802572789,1.299158741556,12.4923024798169));
#417735=CARTESIAN_POINT('Ctrl Pts',(-2.42546161540846,1.29601147968699,
12.4937722312795));
#417736=CARTESIAN_POINT('Ctrl Pts',(-2.42693404782204,1.29324828533509,
12.4958030942394));
#417737=CARTESIAN_POINT('Ctrl Pts',(-2.42839608731078,1.29050459454135,
12.4978196226833));
#417738=CARTESIAN_POINT('Ctrl Pts',(-2.42969356565503,1.28805838205688,
12.5004326847668));
#417739=CARTESIAN_POINT('Ctrl Pts',(-2.43076187580395,1.28603915303464,
12.5033504258767));
#417740=CARTESIAN_POINT('Ctrl Pts',(-2.43203831772902,1.28362653102324,
12.5068366111226));
#417741=CARTESIAN_POINT('Ctrl Pts',(-2.43302890909279,1.28174596942844,
12.5108395010833));
#417742=CARTESIAN_POINT('Ctrl Pts',(-2.43375059365726,1.28037418275789,
12.5149868989719));
#417743=CARTESIAN_POINT('Ctrl Pts',(-2.43496273168923,1.27807013625756,
12.5219528491417));
#417744=CARTESIAN_POINT('Ctrl Pts',(-2.43547304113487,1.27709477561645,
12.5295503425868));
#417745=CARTESIAN_POINT('Ctrl Pts',(-2.43547304111673,1.27709477565043,
12.5369868989719));
#417746=CARTESIAN_POINT('',(-2.36286972375737,1.40689255757176,12.5369868989719));
#417747=CARTESIAN_POINT('Ctrl Pts',(-2.36286972375737,1.40689255757175,
12.5369868989719));
#417748=CARTESIAN_POINT('Ctrl Pts',(-2.36286972375737,1.40689255757175,
12.5309445149785));
#417749=CARTESIAN_POINT('Ctrl Pts',(-2.3632403832162,1.40627082587413,12.5248274368704));
#417750=CARTESIAN_POINT('Ctrl Pts',(-2.36408670060617,1.40484663647568,
12.5190199595513));
#417751=CARTESIAN_POINT('Ctrl Pts',(-2.36479755411145,1.40365040674193,
12.5141420429941));
#417752=CARTESIAN_POINT('Ctrl Pts',(-2.36586598713316,1.40185108533289,
12.5093757677094));
#417753=CARTESIAN_POINT('Ctrl Pts',(-2.3673350451271,1.39936585070276,12.5051960112707));
#417754=CARTESIAN_POINT('Ctrl Pts',(-2.368316477145,1.39770554263593,12.5024036458141));
#417755=CARTESIAN_POINT('Ctrl Pts',(-2.36950036729026,1.3956987587772,12.4998248032393));
#417756=CARTESIAN_POINT('Ctrl Pts',(-2.37084247607465,1.39341521221789,
12.4976950015772));
#417757=CARTESIAN_POINT('Ctrl Pts',(-2.37222240007291,1.3910673245243,12.495505190692));
#417758=CARTESIAN_POINT('Ctrl Pts',(-2.37380498793786,1.38836621366723,
12.4937456938368));
#417759=CARTESIAN_POINT('Ctrl Pts',(-2.37546562572471,1.38551905833168,
12.4925987732155));
#417760=CARTESIAN_POINT('Ctrl Pts',(-2.37712587492872,1.3826725692195,12.4914521209692));
#417761=CARTESIAN_POINT('Ctrl Pts',(-2.37890542058405,1.37960906751125,
12.4908873016276));
#417762=CARTESIAN_POINT('Ctrl Pts',(-2.38065237435684,1.37658790945917,
12.4908873016278));
#417763=CARTESIAN_POINT('',(-2.36286972375737,1.40689255757175,13.7435492065112));
#417764=CARTESIAN_POINT('',(-2.36286972375737,1.40689255757175,14.));
#417765=CARTESIAN_POINT('',(-2.32327412529984,1.47135901081696,13.7435492065112));
#417766=CARTESIAN_POINT('Origin',(0.,2.5406128344257E-15,13.7435492065112));
#417767=CARTESIAN_POINT('',(-2.32327412529984,1.47135901081697,12.5369868989719));
#417768=CARTESIAN_POINT('',(-2.32327412529984,1.47135901081697,14.));
#417769=CARTESIAN_POINT('Ctrl Pts',(-2.30428529106065,1.50092281527118,
12.4908873016278));
#417770=CARTESIAN_POINT('Ctrl Pts',(-2.305475837557,1.49909503388765,12.4908873016278));
#417771=CARTESIAN_POINT('Ctrl Pts',(-2.30667087381384,1.49725550324795,
12.4911020829134));
#417772=CARTESIAN_POINT('Ctrl Pts',(-2.30783239125528,1.49546302323827,
12.4915448903141));
#417773=CARTESIAN_POINT('Ctrl Pts',(-2.30981960605676,1.49239630837073,
12.4923024798169));
#417774=CARTESIAN_POINT('Ctrl Pts',(-2.31175412479163,1.48939674694459,
12.4937722312795));
#417775=CARTESIAN_POINT('Ctrl Pts',(-2.31344688379974,1.48676276380506,
12.4958030942394));
#417776=CARTESIAN_POINT('Ctrl Pts',(-2.31512769474357,1.48414737220734,
12.4978196226833));
#417777=CARTESIAN_POINT('Ctrl Pts',(-2.31662024486267,1.48181505582337,
12.5004326847668));
#417778=CARTESIAN_POINT('Ctrl Pts',(-2.31784958620863,1.47988962281398,
12.5033504258767));
#417779=CARTESIAN_POINT('Ctrl Pts',(-2.31931843197011,1.4775890704701,12.5068366111226));
#417780=CARTESIAN_POINT('Ctrl Pts',(-2.32045901045109,1.47579550868121,
12.5108395010833));
#417781=CARTESIAN_POINT('Ctrl Pts',(-2.32129010701841,1.47448711050944,
12.5149868989719));
#417782=CARTESIAN_POINT('Ctrl Pts',(-2.32268601294057,1.47228953103631,
12.5219528491417));
#417783=CARTESIAN_POINT('Ctrl Pts',(-2.32327412532069,1.47135901078458,
12.5295503425868));
#417784=CARTESIAN_POINT('Ctrl Pts',(-2.32327412529984,1.47135901081697,
12.5369868989719));
#417785=CARTESIAN_POINT('',(-2.24033266527923,1.59480705694541,12.5369868989719));
#417786=CARTESIAN_POINT('Ctrl Pts',(-2.24033266527923,1.59480705694541,
12.5369868989719));
#417787=CARTESIAN_POINT('Ctrl Pts',(-2.24033266527923,1.59480705694541,
12.5309445149785));
#417788=CARTESIAN_POINT('Ctrl Pts',(-2.24075276830452,1.59421760619565,
12.5248274368704));
#417789=CARTESIAN_POINT('Ctrl Pts',(-2.2417123543007,1.59286713839405,12.5190199595513));
#417790=CARTESIAN_POINT('Ctrl Pts',(-2.24251834632814,1.59173283017597,
12.5141420429941));
#417791=CARTESIAN_POINT('Ctrl Pts',(-2.24372988562603,1.5900265830706,12.5093757677094));
#417792=CARTESIAN_POINT('Ctrl Pts',(-2.24539662514483,1.58766935971827,
12.5051960112707));
#417793=CARTESIAN_POINT('Ctrl Pts',(-2.24651012204964,1.58609457201019,
12.5024036458141));
#417794=CARTESIAN_POINT('Ctrl Pts',(-2.24785364441266,1.58419096359675,
12.4998248032393));
#417795=CARTESIAN_POINT('Ctrl Pts',(-2.24937741768479,1.58202440967569,
12.4976950015772));
#417796=CARTESIAN_POINT('Ctrl Pts',(-2.25094412474353,1.57979681100116,
12.495505190692));
#417797=CARTESIAN_POINT('Ctrl Pts',(-2.25274161228866,1.57723368347067,
12.4937456938368));
#417798=CARTESIAN_POINT('Ctrl Pts',(-2.25462879403181,1.57453135920586,
12.4925987732155));
#417799=CARTESIAN_POINT('Ctrl Pts',(-2.25651553418172,1.57182966727451,
12.4914521209692));
#417800=CARTESIAN_POINT('Ctrl Pts',(-2.25853886237507,1.56892140860688,
12.4908873016276));
#417801=CARTESIAN_POINT('Ctrl Pts',(-2.2605262557316,1.56605269615939,12.4908873016278));
#417802=CARTESIAN_POINT('',(-2.24033266527923,1.59480705694541,13.7435492065112));
#417803=CARTESIAN_POINT('',(-2.24033266527923,1.59480705694541,14.));
#417804=CARTESIAN_POINT('',(-2.19561420349232,1.65583159452367,13.7435492065112));
#417805=CARTESIAN_POINT('Origin',(0.,2.5406128344257E-15,13.7435492065112));
#417806=CARTESIAN_POINT('',(-2.19561420349232,1.65583159452367,12.5369868989719));
#417807=CARTESIAN_POINT('',(-2.19561420349232,1.65583159452367,14.));
#417808=CARTESIAN_POINT('Ctrl Pts',(-2.1742788285126,1.68374926158317,12.4908873016278));
#417809=CARTESIAN_POINT('Ctrl Pts',(-2.17561439471476,1.68202460258336,
12.4908873016278));
#417810=CARTESIAN_POINT('Ctrl Pts',(-2.17695539341154,1.68028859937922,
12.4911020829134));
#417811=CARTESIAN_POINT('Ctrl Pts',(-2.17825914976087,1.67859675815339,
12.4915448903141));
#417812=CARTESIAN_POINT('Ctrl Pts',(-2.18048971800073,1.6757022239813,12.4923024798169));
#417813=CARTESIAN_POINT('Ctrl Pts',(-2.1826622918869,1.67287032458445,12.4937722312795));
#417814=CARTESIAN_POINT('Ctrl Pts',(-2.18456411245763,1.6703830813805,12.4958030942394));
#417815=CARTESIAN_POINT('Ctrl Pts',(-2.18645250933703,1.66791339397838,
12.4978196226833));
#417816=CARTESIAN_POINT('Ctrl Pts',(-2.1881301985562,1.66571049487564,12.5004326847668));
#417817=CARTESIAN_POINT('Ctrl Pts',(-2.18951239003535,1.66389167131809,
12.5033504258767));
#417818=CARTESIAN_POINT('Ctrl Pts',(-2.19116386470704,1.66171849843801,
12.5068366111226));
#417819=CARTESIAN_POINT('Ctrl Pts',(-2.19244683994363,1.66002387231283,
12.5108395010833));
#417820=CARTESIAN_POINT('Ctrl Pts',(-2.19338181770325,1.6587875698138,12.5149868989719));
#417821=CARTESIAN_POINT('Ctrl Pts',(-2.19495220199201,1.6567110818967,12.5219528491417));
#417822=CARTESIAN_POINT('Ctrl Pts',(-2.19561420351574,1.65583159449309,
12.5295503425868));
#417823=CARTESIAN_POINT('Ctrl Pts',(-2.19561420349232,1.65583159452367,
12.5369868989719));
#417824=CARTESIAN_POINT('',(-2.10288656254252,1.77210837847974,12.5369868989719));
#417825=CARTESIAN_POINT('Ctrl Pts',(-2.10288656254252,1.77210837847974,
12.5369868989719));
#417826=CARTESIAN_POINT('Ctrl Pts',(-2.10288656254253,1.77210837847974,
12.5309445149785));
#417827=CARTESIAN_POINT('Ctrl Pts',(-2.10335331341796,1.77155513137533,
12.5248274368704));
#417828=CARTESIAN_POINT('Ctrl Pts',(-2.10441978213385,1.77028737231098,
12.5190199595513));
#417829=CARTESIAN_POINT('Ctrl Pts',(-2.10531554893949,1.76922253424263,
12.5141420429941));
#417830=CARTESIAN_POINT('Ctrl Pts',(-2.10666213191942,1.76762071623391,
12.5093757677094));
#417831=CARTESIAN_POINT('Ctrl Pts',(-2.10851546108658,1.76540719109186,
12.5051960112707));
#417832=CARTESIAN_POINT('Ctrl Pts',(-2.10975361274012,1.76392840369491,
12.5024036458141));
#417833=CARTESIAN_POINT('Ctrl Pts',(-2.11124782640125,1.76214063892666,
12.4998248032393));
#417834=CARTESIAN_POINT('Ctrl Pts',(-2.11294312370139,1.76010549570275,
12.4976950015772));
#417835=CARTESIAN_POINT('Ctrl Pts',(-2.11468618764363,1.75801301034894,
12.495505190692));
#417836=CARTESIAN_POINT('Ctrl Pts',(-2.11668661288588,1.75560492333584,
12.4937456938368));
#417837=CARTESIAN_POINT('Ctrl Pts',(-2.1187877797022,1.75306541366391,12.4925987732155));
#417838=CARTESIAN_POINT('Ctrl Pts',(-2.12088845485359,1.75052649822744,
12.4914521209692));
#417839=CARTESIAN_POINT('Ctrl Pts',(-2.12314210066966,1.74779283658204,
12.4908873016276));
#417840=CARTESIAN_POINT('Ctrl Pts',(-2.12535670783504,1.74509566054718,
12.4908873016278));
#417841=CARTESIAN_POINT('',(-2.10288656254252,1.77210837847974,13.7435492065112));
#417842=CARTESIAN_POINT('',(-2.10288656254253,1.77210837847974,14.));
#417843=CARTESIAN_POINT('',(-2.05334283141141,1.82928489216179,13.7435492065112));
#417844=CARTESIAN_POINT('Origin',(0.,2.5406128344257E-15,13.7435492065112));
#417845=CARTESIAN_POINT('',(-2.05334283141141,1.8292848921618,12.5369868989719));
#417846=CARTESIAN_POINT('',(-2.05334283141141,1.8292848921618,14.));
#417847=CARTESIAN_POINT('Ctrl Pts',(-2.02980289909156,1.8553706343584,12.4908873016278));
#417848=CARTESIAN_POINT('Ctrl Pts',(-2.03127459702679,1.8537605750634,12.4908873016278));
#417849=CARTESIAN_POINT('Ctrl Pts',(-2.03275263403844,1.85213965210973,
12.4911020829134));
#417850=CARTESIAN_POINT('Ctrl Pts',(-2.03418995301227,1.85055970859196,
12.4915448903141));
#417851=CARTESIAN_POINT('Ctrl Pts',(-2.03664903062688,1.84785661776268,
12.4923024798169));
#417852=CARTESIAN_POINT('Ctrl Pts',(-2.03904520154358,1.84521122621838,
12.4937722312795));
#417853=CARTESIAN_POINT('Ctrl Pts',(-2.04114342737482,1.84288727514316,
12.4958030942394));
#417854=CARTESIAN_POINT('Ctrl Pts',(-2.04322684322012,1.84057972729882,
12.4978196226833));
#417855=CARTESIAN_POINT('Ctrl Pts',(-2.0450785067944,1.83852090540739,12.5004326847668));
#417856=CARTESIAN_POINT('Ctrl Pts',(-2.0466043501505,1.83682079527238,12.5033504258767));
#417857=CARTESIAN_POINT('Ctrl Pts',(-2.04842746344094,1.83478946396307,
12.5068366111226));
#417858=CARTESIAN_POINT('Ctrl Pts',(-2.04984429744461,1.83320505095887,
12.5108395010833));
#417859=CARTESIAN_POINT('Ctrl Pts',(-2.05087693427381,1.83204907152174,
12.5149868989719));
#417860=CARTESIAN_POINT('Ctrl Pts',(-2.05261134628081,1.83010749384515,
12.5219528491417));
#417861=CARTESIAN_POINT('Ctrl Pts',(-2.05334283143724,1.82928489213323,
12.5295503425868));
#417862=CARTESIAN_POINT('Ctrl Pts',(-2.05334283141141,1.8292848921618,12.5369868989719));
#417863=CARTESIAN_POINT('',(-1.95144609668396,1.93761661113259,12.5369868989719));
#417864=CARTESIAN_POINT('Ctrl Pts',(-1.95144609668396,1.93761661113259,
12.5369868989719));
#417865=CARTESIAN_POINT('Ctrl Pts',(-1.95144609668396,1.93761661113259,
12.5309445149785));
#417866=CARTESIAN_POINT('Ctrl Pts',(-1.95195638925947,1.93710324944173,
12.5248274368704));
#417867=CARTESIAN_POINT('Ctrl Pts',(-1.95312264352173,1.93592663584204,
12.5190199595513));
#417868=CARTESIAN_POINT('Ctrl Pts',(-1.95410222392526,1.93493835424507,
12.5141420429941));
#417869=CARTESIAN_POINT('Ctrl Pts',(-1.95557488929968,1.93345162516757,
12.5093757677094));
#417870=CARTESIAN_POINT('Ctrl Pts',(-1.95760247451537,1.93139652888042,
12.5051960112707));
#417871=CARTESIAN_POINT('Ctrl Pts',(-1.95895704122267,1.93002358288074,
12.5024036458141));
#417872=CARTESIAN_POINT('Ctrl Pts',(-1.96059200243651,1.92836355903727,
12.4998248032393));
#417873=CARTESIAN_POINT('Ctrl Pts',(-1.96244754184083,1.92647337005288,
12.4976950015772));
#417874=CARTESIAN_POINT('Ctrl Pts',(-1.96435536286362,1.92452992316457,
12.495505190692));
#417875=CARTESIAN_POINT('Ctrl Pts',(-1.96654541330306,1.92229290209064,
12.4937456938368));
#417876=CARTESIAN_POINT('Ctrl Pts',(-1.96884658227405,1.91993310702946,
12.4925987732155));
#417877=CARTESIAN_POINT('Ctrl Pts',(-1.97114721278038,1.91757386415122,
12.4914521209692));
#417878=CARTESIAN_POINT('Ctrl Pts',(-1.97361617857809,1.91503299159526,
12.4908873016276));
#417879=CARTESIAN_POINT('Ctrl Pts',(-1.97604326170702,1.91252530123455,
12.4908873016278));
#417880=CARTESIAN_POINT('',(-1.95144609668396,1.93761661113259,13.7435492065112));
#417881=CARTESIAN_POINT('',(-1.95144609668396,1.93761661113259,14.));
#417882=CARTESIAN_POINT('',(-1.89740680156517,1.99056460065335,13.7435492065112));
#417883=CARTESIAN_POINT('Origin',(0.,2.5406128344257E-15,13.7435492065112));
#417884=CARTESIAN_POINT('',(-1.89740680156517,1.99056460065335,12.5369868989719));
#417885=CARTESIAN_POINT('',(-1.89740680156517,1.99056460065335,14.));
#417886=CARTESIAN_POINT('Ctrl Pts',(-1.87181896627098,2.01464482167658,
12.4908873016278));
#417887=CARTESIAN_POINT('Ctrl Pts',(-1.87341700203234,2.01316007676537,
12.4908873016278));
#417888=CARTESIAN_POINT('Ctrl Pts',(-1.8750222412664,2.01166502103698,12.4911020829134));
#417889=CARTESIAN_POINT('Ctrl Pts',(-1.87658355774408,2.01020748949072,
12.4915448903141));
#417890=CARTESIAN_POINT('Ctrl Pts',(-1.87925477997766,2.00771383062773,
12.4923024798169));
#417891=CARTESIAN_POINT('Ctrl Pts',(-1.88185860180278,2.00527255158024,
12.4937722312795));
#417892=CARTESIAN_POINT('Ctrl Pts',(-1.88413926954779,2.00312735814474,
12.4958030942394));
#417893=CARTESIAN_POINT('Ctrl Pts',(-1.88640383957027,2.00099730620838,
12.4978196226833));
#417894=CARTESIAN_POINT('Ctrl Pts',(-1.88841715498409,1.99909626264826,
12.5004326847668));
#417895=CARTESIAN_POINT('Ctrl Pts',(-1.89007649598135,1.99752617988823,
12.5033504258767));
#417896=CARTESIAN_POINT('Ctrl Pts',(-1.89205911537238,1.99565020832441,
12.5068366111226));
#417897=CARTESIAN_POINT('Ctrl Pts',(-1.8936003793466,1.99418655244832,12.5108395010833));
#417898=CARTESIAN_POINT('Ctrl Pts',(-1.89472380321766,1.99311858892551,
12.5149868989719));
#417899=CARTESIAN_POINT('Ctrl Pts',(-1.89661070071715,1.99132484236854,
12.5219528491417));
#417900=CARTESIAN_POINT('Ctrl Pts',(-1.89740680159325,1.99056460062698,
12.5295503425868));
#417901=CARTESIAN_POINT('Ctrl Pts',(-1.89740680156517,1.99056460065335,
12.5369868989719));
#417902=CARTESIAN_POINT('',(-1.78701907901791,2.09023032492259,12.5369868989719));
#417903=CARTESIAN_POINT('Ctrl Pts',(-1.78701907901791,2.09023032492259,
12.5369868989719));
#417904=CARTESIAN_POINT('Ctrl Pts',(-1.78701907901791,2.09023032492258,
12.5309445149785));
#417905=CARTESIAN_POINT('Ctrl Pts',(-1.78756951738059,2.08976026498263,
12.5248274368704));
#417906=CARTESIAN_POINT('Ctrl Pts',(-1.78882779595953,2.08868262701698,
12.5190199595513));
#417907=CARTESIAN_POINT('Ctrl Pts',(-1.78988467101499,2.08777747874237,
12.5141420429941));
#417908=CARTESIAN_POINT('Ctrl Pts',(-1.79147361843879,2.0864157325328,12.5093757677094));
#417909=CARTESIAN_POINT('Ctrl Pts',(-1.79366196645792,2.08453274142727,
12.5051960112707));
#417910=CARTESIAN_POINT('Ctrl Pts',(-1.79512393380103,2.08327477355398,
12.5024036458141));
#417911=CARTESIAN_POINT('Ctrl Pts',(-1.79688876217047,2.08175353782007,
12.4998248032393));
#417912=CARTESIAN_POINT('Ctrl Pts',(-1.79889219537038,2.08002088197103,
12.4976950015772));
#417913=CARTESIAN_POINT('Ctrl Pts',(-1.80095207723957,2.07823940686663,
12.495505190692));
#417914=CARTESIAN_POINT('Ctrl Pts',(-1.80331717845186,2.07618833873803,
12.4937456938368));
#417915=CARTESIAN_POINT('Ctrl Pts',(-1.80580303567769,2.07402396233439,
12.4925987732155));
#417916=CARTESIAN_POINT('Ctrl Pts',(-1.80828831122251,2.07186009238648,
12.4914521209692));
#417917=CARTESIAN_POINT('Ctrl Pts',(-1.81095616644182,2.06952891800762,
12.4908873016276));
#417918=CARTESIAN_POINT('Ctrl Pts',(-1.81357957369652,2.06722740158666,
12.4908873016278));
#417919=CARTESIAN_POINT('',(-1.78701907901791,2.09023032492258,13.7435492065112));
#417920=CARTESIAN_POINT('',(-1.78701907901791,2.09023032492259,14.));
#417921=CARTESIAN_POINT('',(-1.72884384250461,2.1385974301476,13.7435492065112));
#417922=CARTESIAN_POINT('Origin',(0.,2.5406128344257E-15,13.7435492065112));
#417923=CARTESIAN_POINT('',(-1.72884384250461,2.1385974301476,12.5369868989719));
#417924=CARTESIAN_POINT('',(-1.72884384250461,2.1385974301476,14.));
#417925=CARTESIAN_POINT('Ctrl Pts',(-1.70137838705825,2.1605118800995,12.4908873016278));
#417926=CARTESIAN_POINT('Ctrl Pts',(-1.7030921259814,2.15916233030449,12.4908873016278));
#417927=CARTESIAN_POINT('Ctrl Pts',(-1.70481388483562,2.15780309115059,
12.4911020829134));
#417928=CARTESIAN_POINT('Ctrl Pts',(-1.70648880851361,2.1564776712078,12.4915448903141));
#417929=CARTESIAN_POINT('Ctrl Pts',(-1.70935439882289,2.15421003919943,
12.4923024798169));
#417930=CARTESIAN_POINT('Ctrl Pts',(-1.71214854355179,2.15198911895802,
12.4937722312795));
#417931=CARTESIAN_POINT('Ctrl Pts',(-1.71459647574302,2.15003695907061,
12.4958030942394));
#417932=CARTESIAN_POINT('Ctrl Pts',(-1.71702712960282,2.14809857818643,
12.4978196226833));
#417933=CARTESIAN_POINT('Ctrl Pts',(-1.71918869857426,2.14636796408887,
12.5004326847668));
#417934=CARTESIAN_POINT('Ctrl Pts',(-1.72097049457212,2.14493835734555,
12.5033504258767));
#417935=CARTESIAN_POINT('Ctrl Pts',(-1.7230994260588,2.14323022980845,12.5068366111226));
#417936=CARTESIAN_POINT('Ctrl Pts',(-1.72475486314611,2.14189707144884,
12.5108395010833));
#417937=CARTESIAN_POINT('Ctrl Pts',(-1.72596159785851,2.14092423096141,
12.5149868989719));
#417938=CARTESIAN_POINT('Ctrl Pts',(-1.72798842385895,2.13929025261145,
12.5219528491417));
#417939=CARTESIAN_POINT('Ctrl Pts',(-1.72884384253474,2.13859743012361,
12.5295503425868));
#417940=CARTESIAN_POINT('Ctrl Pts',(-1.72884384250461,2.1385974301476,12.5369868989719));
#417941=CARTESIAN_POINT('',(-1.61069974421839,2.22893390076396,12.5369868989719));
#417942=CARTESIAN_POINT('Ctrl Pts',(-1.61069974421839,2.22893390076395,
12.5369868989719));
#417943=CARTESIAN_POINT('Ctrl Pts',(-1.61069974421839,2.22893390076395,
12.5309445149785));
#417944=CARTESIAN_POINT('Ctrl Pts',(-1.61128666529176,2.22851027074625,
12.5248274368704));
#417945=CARTESIAN_POINT('Ctrl Pts',(-1.61262859455103,2.22753877991751,
12.5190199595513));
#417946=CARTESIAN_POINT('Ctrl Pts',(-1.61375573092929,2.22672278857768,
12.5141420429941));
#417947=CARTESIAN_POINT('Ctrl Pts',(-1.61545038621954,2.22549508743239,
12.5093757677094));
#417948=CARTESIAN_POINT('Ctrl Pts',(-1.6177849339471,2.22379673250362,12.5051960112707));
#417949=CARTESIAN_POINT('Ctrl Pts',(-1.61934457277456,2.22266211432536,
12.5024036458141));
#417950=CARTESIAN_POINT('Ctrl Pts',(-1.62122752365795,2.22128979027384,
12.4998248032393));
#417951=CARTESIAN_POINT('Ctrl Pts',(-1.62336551813605,2.21972619809896,
12.4976950015772));
#417952=CARTESIAN_POINT('Ctrl Pts',(-1.62556375267767,2.21811855020135,
12.495505190692));
#417953=CARTESIAN_POINT('Ctrl Pts',(-1.62808816530445,2.21626708453809,
12.4937456938368));
#417954=CARTESIAN_POINT('Ctrl Pts',(-1.63074216781542,2.21431253035986,
12.4925987732155));
#417955=CARTESIAN_POINT('Ctrl Pts',(-1.63339554930003,2.21235843353977,
12.4914521209692));
#417956=CARTESIAN_POINT('Ctrl Pts',(-1.63624453980463,2.21025247091888,
12.4908873016276));
#417957=CARTESIAN_POINT('Ctrl Pts',(-1.63904681284264,2.20817244464973,
12.4908873016278));
#417958=CARTESIAN_POINT('',(-1.61069974421839,2.22893390076395,13.7435492065112));
#417959=CARTESIAN_POINT('',(-1.61069974421839,2.22893390076395,14.));
#417960=CARTESIAN_POINT('',(-1.54877571291133,2.27239824658795,13.7435492065112));
#417961=CARTESIAN_POINT('Origin',(0.,2.5406128344257E-15,13.7435492065112));
#417962=CARTESIAN_POINT('',(-1.54877571291133,2.27239824658796,12.5369868989719));
#417963=CARTESIAN_POINT('',(-1.54877571291133,2.27239824658796,14.));
#417964=CARTESIAN_POINT('Ctrl Pts',(-1.51961541538732,2.29200108841973,
12.4908873016278));
#417965=CARTESIAN_POINT('Ctrl Pts',(-1.52143345282248,2.29079571477214,
12.4908873016278));
#417966=CARTESIAN_POINT('Ctrl Pts',(-1.52326027327575,2.28958133770505,
12.4911020829134));
#417967=CARTESIAN_POINT('Ctrl Pts',(-1.52503765781331,2.28839684981677,
12.4915448903141));
#417968=CARTESIAN_POINT('Ctrl Pts',(-1.52807854616758,2.28637033537988,
12.4923024798169));
#417969=CARTESIAN_POINT('Ctrl Pts',(-1.53104441922809,2.28438455380235,
12.4937722312795));
#417970=CARTESIAN_POINT('Ctrl Pts',(-1.53364332528069,2.282638418765,12.4958030942394));
#417971=CARTESIAN_POINT('Ctrl Pts',(-1.53622388737739,2.28090460853797,
12.4978196226833));
#417972=CARTESIAN_POINT('Ctrl Pts',(-1.53851932502158,2.27935594085425,
12.5004326847668));
#417973=CARTESIAN_POINT('Ctrl Pts',(-1.54041171846165,2.27807632392465,
12.5033504258767));
#417974=CARTESIAN_POINT('Ctrl Pts',(-1.54267279435619,2.27654740772122,
12.5068366111226));
#417975=CARTESIAN_POINT('Ctrl Pts',(-1.5444313878959,2.27535361882702,12.5108395010833));
#417976=CARTESIAN_POINT('Ctrl Pts',(-1.54571340282923,2.2744823754679,12.5149868989719));
#417977=CARTESIAN_POINT('Ctrl Pts',(-1.547866669138,2.27301903918127,12.5219528491417));
#417978=CARTESIAN_POINT('Ctrl Pts',(-1.54877571294331,2.2723982465665,12.5295503425868));
#417979=CARTESIAN_POINT('Ctrl Pts',(-1.54877571291133,2.27239824658796,
12.5369868989719));
#417980=CARTESIAN_POINT('',(-1.42366146836785,2.35280428924395,12.5369868989719));
#417981=CARTESIAN_POINT('Ctrl Pts',(-1.42366146836785,2.35280428924394,
12.5369868989719));
#417982=CARTESIAN_POINT('Ctrl Pts',(-1.42366146836785,2.35280428924394,
12.5309445149785));
#417983=CARTESIAN_POINT('Ctrl Pts',(-1.42428096628899,2.35242990833637,
12.5248274368704));
#417984=CARTESIAN_POINT('Ctrl Pts',(-1.42569761591078,2.35157102975571,
12.5190199595513));
#417985=CARTESIAN_POINT('Ctrl Pts',(-1.42688751270522,2.3508496256384,12.5141420429941));
#417986=CARTESIAN_POINT('Ctrl Pts',(-1.42867659821055,2.34976413970596,
12.5093757677094));
#417987=CARTESIAN_POINT('Ctrl Pts',(-1.43114180961658,2.34826172322579,
12.5051960112707));
#417988=CARTESIAN_POINT('Ctrl Pts',(-1.43278874078931,2.34725800543934,
12.5024036458141));
#417989=CARTESIAN_POINT('Ctrl Pts',(-1.43477728345921,2.34604372566035,
12.4998248032393));
#417990=CARTESIAN_POINT('Ctrl Pts',(-1.43703561121499,2.34465960260759,
12.4976950015772));
#417991=CARTESIAN_POINT('Ctrl Pts',(-1.43935756954084,2.34323648054829,
12.495505190692));
#417992=CARTESIAN_POINT('Ctrl Pts',(-1.44202449403258,2.34159693854887,
12.4937456938368));
#417993=CARTESIAN_POINT('Ctrl Pts',(-1.44482897987985,2.33986521383163,
12.4925987732155));
#417994=CARTESIAN_POINT('Ctrl Pts',(-1.44763280948825,2.3381338943313,12.4914521209692));
#417995=CARTESIAN_POINT('Ctrl Pts',(-1.45064397571638,2.33626715830216,
12.4908873016276));
#417996=CARTESIAN_POINT('Ctrl Pts',(-1.45360646587299,2.33442246441647,
12.4908873016278));
#417997=CARTESIAN_POINT('',(-1.42366146836785,2.35280428924394,13.7435492065112));
#417998=CARTESIAN_POINT('',(-1.42366146836785,2.35280428924395,14.));
#417999=CARTESIAN_POINT('',(-1.35840073647863,2.39107662761659,13.7435492065112));
#418000=CARTESIAN_POINT('Origin',(0.,2.5406128344257E-15,13.7435492065112));
#418001=CARTESIAN_POINT('',(-1.35840073647863,2.39107662761659,12.5369868989719));
#418002=CARTESIAN_POINT('',(-1.35840073647863,2.39107662761659,14.));
#418003=CARTESIAN_POINT('Ctrl Pts',(-1.32773965384588,2.40823740765009,
12.4908873016278));
#418004=CARTESIAN_POINT('Ctrl Pts',(-1.32964989105388,2.40718423171268,
12.4908873016278));
#418005=CARTESIAN_POINT('Ctrl Pts',(-1.33156961591748,2.40612279821141,
12.4911020829134));
#418006=CARTESIAN_POINT('Ctrl Pts',(-1.33343763311376,2.40508712494911,
12.4915448903141));
#418007=CARTESIAN_POINT('Ctrl Pts',(-1.33663358290274,2.40331521420294,
12.4923024798169));
#418008=CARTESIAN_POINT('Ctrl Pts',(-1.33975144689897,2.40157778633805,
12.4937722312795));
#418009=CARTESIAN_POINT('Ctrl Pts',(-1.34248403152195,2.40004929639134,
12.4958030942394));
#418010=CARTESIAN_POINT('Ctrl Pts',(-1.34519732864057,2.39853159504246,
12.4978196226833));
#418011=CARTESIAN_POINT('Ctrl Pts',(-1.34761135919871,2.39717517990051,
12.5004326847668));
#418012=CARTESIAN_POINT('Ctrl Pts',(-1.34960175651487,2.39605406842417,
12.5033504258767));
#418013=CARTESIAN_POINT('Ctrl Pts',(-1.35197992973024,2.39471453823949,
12.5068366111226));
#418014=CARTESIAN_POINT('Ctrl Pts',(-1.35382997657249,2.39366806327883,
12.5108395010833));
#418015=CARTESIAN_POINT('Ctrl Pts',(-1.35517874012889,2.39290421502882,
12.5149868989719));
#418016=CARTESIAN_POINT('Ctrl Pts',(-1.35744411711395,2.39162125906708,
12.5219528491417));
#418017=CARTESIAN_POINT('Ctrl Pts',(-1.35840073651226,2.39107662759781,
12.5295503425868));
#418018=CARTESIAN_POINT('Ctrl Pts',(-1.35840073647863,2.39107662761659,
12.5369868989719));
#418019=CARTESIAN_POINT('',(-1.22714896033293,2.4610171533644,12.5369868989719));
#418020=CARTESIAN_POINT('Ctrl Pts',(-1.22714896033293,2.4610171533644,12.5369868989719));
#418021=CARTESIAN_POINT('Ctrl Pts',(-1.22714896033293,2.4610171533644,12.5309445149785));
#418022=CARTESIAN_POINT('Ctrl Pts',(-1.2277969124454,2.46069451301012,12.5248274368704));
#418023=CARTESIAN_POINT('Ctrl Pts',(-1.22927885486019,2.4599539623728,12.5190199595513));
#418024=CARTESIAN_POINT('Ctrl Pts',(-1.23052359350396,2.45933194630339,
12.5141420429941));
#418025=CARTESIAN_POINT('Ctrl Pts',(-1.23239520315551,2.45839589931358,
12.5093757677094));
#418026=CARTESIAN_POINT('Ctrl Pts',(-1.23497467266485,2.45709941961581,
12.5051960112707));
#418027=CARTESIAN_POINT('Ctrl Pts',(-1.23669793612762,2.45623328179743,
12.5024036458141));
#418028=CARTESIAN_POINT('Ctrl Pts',(-1.23877883716064,2.45518512712256,
12.4998248032393));
#418029=CARTESIAN_POINT('Ctrl Pts',(-1.24114246939548,2.45398968430246,
12.4976950015772));
#418030=CARTESIAN_POINT('Ctrl Pts',(-1.243572699256,2.45276055872399,12.495505190692));
#418031=CARTESIAN_POINT('Ctrl Pts',(-1.24636438767022,2.45134385126991,
12.4937456938368));
#418032=CARTESIAN_POINT('Ctrl Pts',(-1.24930069346319,2.44984648035594,
12.4925987732155));
#418033=CARTESIAN_POINT('Ctrl Pts',(-1.25223631217193,2.44834945982099,
12.4914521209692));
#418034=CARTESIAN_POINT('Ctrl Pts',(-1.25538961530914,2.44673437320389,
12.4908873016276));
#418035=CARTESIAN_POINT('Ctrl Pts',(-1.25849260770113,2.44513728783511,
12.4908873016278));
#418036=CARTESIAN_POINT('',(-1.22714896033293,2.4610171533644,13.7435492065112));
#418037=CARTESIAN_POINT('',(-1.22714896033293,2.4610171533644,14.));
#418038=CARTESIAN_POINT('',(-1.15898582726502,2.49384278818831,13.7435492065112));
#418039=CARTESIAN_POINT('Origin',(0.,2.5406128344257E-15,13.7435492065112));
#418040=CARTESIAN_POINT('',(-1.15898582726502,2.49384278818831,12.5369868989719));
#418041=CARTESIAN_POINT('',(-1.15898582726502,2.49384278818831,14.));
#418042=CARTESIAN_POINT('Ctrl Pts',(-1.12702800396973,2.50844730426374,
12.4908873016278));
#418043=CARTESIAN_POINT('Ctrl Pts',(-1.12901772863711,2.50755333474861,
12.4908873016278));
#418044=CARTESIAN_POINT('Ctrl Pts',(-1.13101758245881,2.506651908478,12.4911020829134));
#418045=CARTESIAN_POINT('Ctrl Pts',(-1.13296380096757,2.50577194207636,
12.4915448903141));
#418046=CARTESIAN_POINT('Ctrl Pts',(-1.13629354367271,2.50426642679458,
12.4923024798169));
#418047=CARTESIAN_POINT('Ctrl Pts',(-1.13954264973418,2.50278891493811,
12.4937722312795));
#418048=CARTESIAN_POINT('Ctrl Pts',(-1.14239072802771,2.50148824193046,
12.4958030942394));
#418049=CARTESIAN_POINT('Ctrl Pts',(-1.14521870362358,2.5001967495118,12.4978196226833));
#418050=CARTESIAN_POINT('Ctrl Pts',(-1.1477352621206,2.49904161363059,12.5004326847668));
#418051=CARTESIAN_POINT('Ctrl Pts',(-1.14981041754709,2.49808646841942,
12.5033504258767));
#418052=CARTESIAN_POINT('Ctrl Pts',(-1.15228986173292,2.49694523860587,
12.5068366111226));
#418053=CARTESIAN_POINT('Ctrl Pts',(-1.15421905012122,2.49605304169695,
12.5108395010833));
#418054=CARTESIAN_POINT('Ctrl Pts',(-1.15562558650174,2.49540167184013,
12.5149868989719));
#418055=CARTESIAN_POINT('Ctrl Pts',(-1.15798799845303,2.49430763406354,
12.5219528491417));
#418056=CARTESIAN_POINT('Ctrl Pts',(-1.15898582730006,2.49384278817234,
12.5295503425868));
#418057=CARTESIAN_POINT('Ctrl Pts',(-1.15898582726502,2.49384278818831,
12.5369868989719));
#418058=CARTESIAN_POINT('',(-1.02246997843232,2.55285235436847,12.5369868989719));
#418059=CARTESIAN_POINT('Ctrl Pts',(-1.02246997843232,2.55285235436847,
12.5369868989719));
#418060=CARTESIAN_POINT('Ctrl Pts',(-1.02246997843232,2.55285235436847,
12.5309445149785));
#418061=CARTESIAN_POINT('Ctrl Pts',(-1.0231420727217,2.55258360168581,12.5248274368704));
#418062=CARTESIAN_POINT('Ctrl Pts',(-1.02467944584725,2.55196630723413,
12.5190199595513));
#418063=CARTESIAN_POINT('Ctrl Pts',(-1.02597074281003,2.55144781862693,
12.5141420429941));
#418064=CARTESIAN_POINT('Ctrl Pts',(-1.02791242135437,2.55066743981805,
12.5093757677094));
#418065=CARTESIAN_POINT('Ctrl Pts',(-1.030588983023,2.54958552476116,12.5051960112707));
#418066=CARTESIAN_POINT('Ctrl Pts',(-1.03237711074179,2.54886273091513,
12.5024036458141));
#418067=CARTESIAN_POINT('Ctrl Pts',(-1.03453652208488,2.5479876766408,12.4998248032393));
#418068=CARTESIAN_POINT('Ctrl Pts',(-1.03698972921624,2.5469888695281,12.4976950015772));
#418069=CARTESIAN_POINT('Ctrl Pts',(-1.03951205783267,2.54596192005838,
12.495505190692));
#418070=CARTESIAN_POINT('Ctrl Pts',(-1.04240993194356,2.54477747510402,
12.4937456938368));
#418071=CARTESIAN_POINT('Ctrl Pts',(-1.04545851705164,2.5435244227497,12.4925987732155));
#418072=CARTESIAN_POINT('Ctrl Pts',(-1.04850638880256,2.5422716636048,12.4914521209692));
#418073=CARTESIAN_POINT('Ctrl Pts',(-1.05178084413673,2.5409189745347,12.4908873016276));
#418074=CARTESIAN_POINT('Ctrl Pts',(-1.05500368886169,2.53958012602246,
12.4908873016278));
#418075=CARTESIAN_POINT('',(-1.02246997843232,2.55285235436846,13.7435492065112));
#418076=CARTESIAN_POINT('',(-1.02246997843232,2.55285235436847,14.));
#418077=CARTESIAN_POINT('',(-0.951858058590151,2.58001283645973,13.7435492065112));
#418078=CARTESIAN_POINT('Origin',(0.,2.5406128344257E-15,13.7435492065112));
#418079=CARTESIAN_POINT('',(-0.951858058590152,2.58001283645973,12.5369868989719));
#418080=CARTESIAN_POINT('',(-0.951858058590152,2.58001283645973,14.));
#418081=CARTESIAN_POINT('Ctrl Pts',(-0.918816168673682,2.59196389793219,
12.4908873016278));
#418082=CARTESIAN_POINT('Ctrl Pts',(-0.920872139511063,2.59123508405896,
12.4908873016278));
#418083=CARTESIAN_POINT('Ctrl Pts',(-0.922938813593644,2.59049966386211,
12.4911020829134));
#418084=CARTESIAN_POINT('Ctrl Pts',(-0.924950281651809,2.58978126035236,
12.4915448903141));
#418085=CARTESIAN_POINT('Ctrl Pts',(-0.928391658384763,2.58855215949077,
12.4923024798169));
#418086=CARTESIAN_POINT('Ctrl Pts',(-0.9317503842467,2.58734439624036,12.4937722312795));
#418087=CARTESIAN_POINT('Ctrl Pts',(-0.93469500271964,2.58628019593604,
12.4958030942394));
#418088=CARTESIAN_POINT('Ctrl Pts',(-0.937618837081762,2.58522350711657,
12.4978196226833));
#418089=CARTESIAN_POINT('Ctrl Pts',(-0.940221176236059,2.58427733773481,
12.5004326847668));
#418090=CARTESIAN_POINT('Ctrl Pts',(-0.942367279955908,2.58349451512259,
12.5033504258767));
#418091=CARTESIAN_POINT('Ctrl Pts',(-0.94493149482021,2.58255918037628,
12.5068366111226));
#418092=CARTESIAN_POINT('Ctrl Pts',(-0.94692698632412,2.58182719894233,
12.5108395010833));
#418093=CARTESIAN_POINT('Ctrl Pts',(-0.94838193526122,2.58129264223764,
12.5149868989719));
#418094=CARTESIAN_POINT('Ctrl Pts',(-0.950825660716975,2.58039480328709,
12.5219528491417));
#418095=CARTESIAN_POINT('Ctrl Pts',(-0.951858058626384,2.58001283644667,
12.5295503425868));
#418096=CARTESIAN_POINT('Ctrl Pts',(-0.951858058590152,2.58001283645973,
12.5369868989719));
#418097=CARTESIAN_POINT('',(-0.810986627520914,2.6276987441452,12.5369868989719));
#418098=CARTESIAN_POINT('Ctrl Pts',(-0.810986627520913,2.6276987441452,
12.5369868989719));
#418099=CARTESIAN_POINT('Ctrl Pts',(-0.810986627520915,2.6276987441452,
12.5309445149785));
#418100=CARTESIAN_POINT('Ctrl Pts',(-0.81167839131061,2.62748566763893,
12.5248274368704));
#418101=CARTESIAN_POINT('Ctrl Pts',(-0.813260964182396,2.62699573736562,
12.5190199595513));
#418102=CARTESIAN_POINT('Ctrl Pts',(-0.81459022609596,2.62658422667677,
12.5141420429941));
#418103=CARTESIAN_POINT('Ctrl Pts',(-0.816589051982728,2.62596470934103,
12.5093757677094));
#418104=CARTESIAN_POINT('Ctrl Pts',(-0.819344893734357,2.62510455889122,
12.5051960112707));
#418105=CARTESIAN_POINT('Ctrl Pts',(-0.82118598601421,2.62452991909133,
12.5024036458141));
#418106=CARTESIAN_POINT('Ctrl Pts',(-0.823409537141162,2.62383378855938,
12.4998248032393));
#418107=CARTESIAN_POINT('Ctrl Pts',(-0.825935993480318,2.62303826405062,
12.4976950015772));
#418108=CARTESIAN_POINT('Ctrl Pts',(-0.828533635171877,2.62222032486894,
12.495505190692));
#418109=CARTESIAN_POINT('Ctrl Pts',(-0.831518410105352,2.62127602470004,
12.4937456938368));
#418110=CARTESIAN_POINT('Ctrl Pts',(-0.834658986697622,2.62027562976205,
12.4925987732155));
#418111=CARTESIAN_POINT('Ctrl Pts',(-0.837798828407076,2.61927546891262,
12.4914521209692));
#418112=CARTESIAN_POINT('Ctrl Pts',(-0.841172644978215,2.61819417931211,
12.4908873016276));
#418113=CARTESIAN_POINT('Ctrl Pts',(-0.844493894536227,2.61712247747236,
12.4908873016278));
#418114=CARTESIAN_POINT('',(-0.810986627520915,2.6276987441452,13.7435492065112));
#418115=CARTESIAN_POINT('',(-0.810986627520915,2.6276987441452,14.));
#418116=CARTESIAN_POINT('',(-0.738395831580896,2.64901332497667,13.7435492065112));
#418117=CARTESIAN_POINT('Origin',(0.,2.5406128344257E-15,13.7435492065112));
#418118=CARTESIAN_POINT('',(-0.738395831580896,2.64901332497667,12.5369868989719));
#418119=CARTESIAN_POINT('',(-0.738395831580896,2.64901332497667,14.));
#418120=CARTESIAN_POINT('Ctrl Pts',(-0.704489763369112,2.65823139950384,
12.4908873016278));
#418121=CARTESIAN_POINT('Ctrl Pts',(-0.706598298229784,2.65767259140861,
12.4908873016278));
#418122=CARTESIAN_POINT('Ctrl Pts',(-0.708718039198195,2.65710807138559,
12.4911020829134));
#418123=CARTESIAN_POINT('Ctrl Pts',(-0.710781370817709,2.65655601162455,
12.4915448903141));
#418124=CARTESIAN_POINT('Ctrl Pts',(-0.714311479784112,2.6556115046466,
12.4923024798169));
#418125=CARTESIAN_POINT('Ctrl Pts',(-0.717757473680055,2.6546815274674,
12.4937722312795));
#418126=CARTESIAN_POINT('Ctrl Pts',(-0.720779036382295,2.65386088194386,
12.4958030942394));
#418127=CARTESIAN_POINT('Ctrl Pts',(-0.723779271875384,2.65304602881333,
12.4978196226833));
#418128=CARTESIAN_POINT('Ctrl Pts',(-0.726450073549245,2.65231512253215,
12.5004326847668));
#418129=CARTESIAN_POINT('Ctrl Pts',(-0.728652843596273,2.65170983207422,
12.5033504258767));
#418130=CARTESIAN_POINT('Ctrl Pts',(-0.731284764712195,2.65098661689357,
12.5068366111226));
#418131=CARTESIAN_POINT('Ctrl Pts',(-0.733333279664994,2.65041972215026,
12.5108395010833));
#418132=CARTESIAN_POINT('Ctrl Pts',(-0.734826958713545,2.65000553598437,
12.5149868989719));
#418133=CARTESIAN_POINT('Ctrl Pts',(-0.737335735084039,2.64930987082994,
12.5219528491417));
#418134=CARTESIAN_POINT('Ctrl Pts',(-0.738395831618072,2.64901332496661,
12.5295503425868));
#418135=CARTESIAN_POINT('Ctrl Pts',(-0.738395831580896,2.64901332497667,
12.5369868989719));
#418136=CARTESIAN_POINT('',(-0.594106294406732,2.68505823231943,12.5369868989719));
#418137=CARTESIAN_POINT('Ctrl Pts',(-0.594106294406732,2.68505823231942,
12.5369868989719));
#418138=CARTESIAN_POINT('Ctrl Pts',(-0.594106294406734,2.68505823231942,
12.5309445149785));
#418139=CARTESIAN_POINT('Ctrl Pts',(-0.594813124122851,2.68490224997853,
12.5248274368704));
#418140=CARTESIAN_POINT('Ctrl Pts',(-0.596430364979523,2.68454294428873,
12.5190199595513));
#418141=CARTESIAN_POINT('Ctrl Pts',(-0.597788745825149,2.68424115005398,
12.5141420429941));
#418142=CARTESIAN_POINT('Ctrl Pts',(-0.599831417197852,2.68378661697702,
12.5093757677094));
#418143=CARTESIAN_POINT('Ctrl Pts',(-0.6026481993603,2.68315395529362,12.5051960112707));
#418144=CARTESIAN_POINT('Ctrl Pts',(-0.604530004035857,2.68273129367294,
12.5024036458141));
#418145=CARTESIAN_POINT('Ctrl Pts',(-0.606802897580777,2.68221871951719,
12.4998248032393));
#418146=CARTESIAN_POINT('Ctrl Pts',(-0.609385789977635,2.68163177169673,
12.4976950015772));
#418147=CARTESIAN_POINT('Ctrl Pts',(-0.612041457867441,2.68102828605339,
12.495505190692));
#418148=CARTESIAN_POINT('Ctrl Pts',(-0.615093270438773,2.68033041483178,
12.4937456938368));
#418149=CARTESIAN_POINT('Ctrl Pts',(-0.61830493849617,2.67958933477338,
12.4925987732155));
#418150=CARTESIAN_POINT('Ctrl Pts',(-0.621515855035623,2.67884842812486,
12.4914521209692));
#418151=CARTESIAN_POINT('Ctrl Pts',(-0.624966580651088,2.67804573379783,
12.4908873016276));
#418152=CARTESIAN_POINT('Ctrl Pts',(-0.628364132674314,2.67724831062949,
12.4908873016278));
#418153=CARTESIAN_POINT('',(-0.594106294406733,2.68505823231942,13.7435492065112));
#418154=CARTESIAN_POINT('',(-0.594106294406734,2.68505823231942,14.));
#418155=CARTESIAN_POINT('',(-0.520019702139206,2.70038506687233,13.7435492065112));
#418156=CARTESIAN_POINT('Origin',(0.,2.5406128344257E-15,13.7435492065112));
#418157=CARTESIAN_POINT('',(-0.520019702139206,2.70038506687233,12.5369868989719));
#418158=CARTESIAN_POINT('',(-0.520019702139207,2.70038506687233,14.));
#418159=CARTESIAN_POINT('Ctrl Pts',(-0.485475094921951,2.7068088096891,
12.4908873016278));
#418160=CARTESIAN_POINT('Ctrl Pts',(-0.487622161854298,2.70642372614753,
12.4908873016278));
#418161=CARTESIAN_POINT('Ctrl Pts',(-0.489780863182127,2.70603386308596,
12.4911020829134));
#418162=CARTESIAN_POINT('Ctrl Pts',(-0.491882327231488,2.70565182094026,
12.4915448903141));
#418163=CARTESIAN_POINT('Ctrl Pts',(-0.495477676138597,2.70499819338406,
12.4923024798169));
#418164=CARTESIAN_POINT('Ctrl Pts',(-0.498988005547716,2.70435219112078,
12.4937722312795));
#418165=CARTESIAN_POINT('Ctrl Pts',(-0.502066404477997,2.70378056163856,
12.4958030942394));
#418166=CARTESIAN_POINT('Ctrl Pts',(-0.505123075029849,2.70321296691012,
12.4978196226833));
#418167=CARTESIAN_POINT('Ctrl Pts',(-0.507844565478785,2.70270218779023,
12.5004326847668));
#418168=CARTESIAN_POINT('Ctrl Pts',(-0.510089342781761,2.70227845759472,
12.5033504258767));
#418169=CARTESIAN_POINT('Ctrl Pts',(-0.512771455148514,2.70177217485743,
12.5068366111226));
#418170=CARTESIAN_POINT('Ctrl Pts',(-0.514859361021171,2.70137413939576,
12.5108395010833));
#418171=CARTESIAN_POINT('Ctrl Pts',(-0.516381829993545,2.70108308010926,
12.5149868989719));
#418172=CARTESIAN_POINT('Ctrl Pts',(-0.518938961785951,2.70059421828779,
12.5219528491417));
#418173=CARTESIAN_POINT('Ctrl Pts',(-0.520019702177079,2.70038506686532,
12.5295503425868));
#418174=CARTESIAN_POINT('Ctrl Pts',(-0.520019702139206,2.70038506687233,
12.5369868989719));
#418175=CARTESIAN_POINT('',(-0.373272281923912,2.72454910096099,12.5369868989719));
#418176=CARTESIAN_POINT('Ctrl Pts',(-0.373272281923913,2.72454910096099,
12.5369868989719));
#418177=CARTESIAN_POINT('Ctrl Pts',(-0.373272281923915,2.72454910096099,
12.5309445149785));
#418178=CARTESIAN_POINT('Ctrl Pts',(-0.373989473731312,2.72445125082222,
12.5248274368704));
#418179=CARTESIAN_POINT('Ctrl Pts',(-0.375630620101797,2.72422496083601,
12.5190199595513));
#418180=CARTESIAN_POINT('Ctrl Pts',(-0.37700908007907,2.72403489144618,
12.5141420429941));
#418181=CARTESIAN_POINT('Ctrl Pts',(-0.379082003296741,2.72374836747066,
12.5093757677094));
#418182=CARTESIAN_POINT('Ctrl Pts',(-0.381940980649454,2.72334740481279,
12.5051960112707));
#418183=CARTESIAN_POINT('Ctrl Pts',(-0.383850974621075,2.72307953411467,
12.5024036458141));
#418184=CARTESIAN_POINT('Ctrl Pts',(-0.386158084852425,2.72275392743156,
12.4998248032393));
#418185=CARTESIAN_POINT('Ctrl Pts',(-0.388780224584233,2.7223794623403,
12.4976950015772));
#418186=CARTESIAN_POINT('Ctrl Pts',(-0.391476245640631,2.72199444633269,
12.495505190692));
#418187=CARTESIAN_POINT('Ctrl Pts',(-0.39457478654067,2.72154764827621,
12.4937456938368));
#418188=CARTESIAN_POINT('Ctrl Pts',(-0.397836172942162,2.72107081486292,
12.4925987732155));
#418189=CARTESIAN_POINT('Ctrl Pts',(-0.401096796191809,2.72059409302681,
12.4914521209692));
#418190=CARTESIAN_POINT('Ctrl Pts',(-0.404601466841955,2.72007533577157,
12.4908873016276));
#418191=CARTESIAN_POINT('Ctrl Pts',(-0.408052711182237,2.71955749799427,
12.4908873016278));
#418192=CARTESIAN_POINT('',(-0.373272281923914,2.72454910096099,13.7435492065112));
#418193=CARTESIAN_POINT('',(-0.373272281923914,2.72454910096099,14.));
#418194=CARTESIAN_POINT('',(-0.298182927376992,2.73378619168012,13.7435492065112));
#418195=CARTESIAN_POINT('Origin',(0.,2.5406128344257E-15,13.7435492065112));
#418196=CARTESIAN_POINT('',(-0.298182927376992,2.73378619168012,12.5369868989719));
#418197=CARTESIAN_POINT('',(-0.298182927376992,2.73378619168012,14.));
#418198=CARTESIAN_POINT('Ctrl Pts',(-0.263229669815836,2.7373728538379,
12.4908873016278));
#418199=CARTESIAN_POINT('Ctrl Pts',(-0.265400980443666,2.73716405751743,
12.4908873016278));
#418200=CARTESIAN_POINT('Ctrl Pts',(-0.267584276329737,2.73695144589166,
12.4911020829134));
#418201=CARTESIAN_POINT('Ctrl Pts',(-0.269709887912413,2.73674196378875,
12.4915448903141));
#418202=CARTESIAN_POINT('Ctrl Pts',(-0.273346550306441,2.73638356543784,
12.4923024798169));
#418203=CARTESIAN_POINT('Ctrl Pts',(-0.276897854565684,2.73602583712895,
12.4937722312795));
#418204=CARTESIAN_POINT('Ctrl Pts',(-0.280012603487024,2.73570702778796,
12.4958030942394));
#418205=CARTESIAN_POINT('Ctrl Pts',(-0.283105367459432,2.73539046871088,
12.4978196226833));
#418206=CARTESIAN_POINT('Ctrl Pts',(-0.28585943561352,2.73510321590304,
12.5004326847668));
#418207=CARTESIAN_POINT('Ctrl Pts',(-0.288131281549855,2.73486386582449,
12.5033504258767));
#418208=CARTESIAN_POINT('Ctrl Pts',(-0.290845736152154,2.73457788475865,
12.5068366111226));
#418209=CARTESIAN_POINT('Ctrl Pts',(-0.292959138275568,2.73435135743893,
12.5108395010833));
#418210=CARTESIAN_POINT('Ctrl Pts',(-0.294500265391943,2.73418536198336,
12.5149868989719));
#418211=CARTESIAN_POINT('Ctrl Pts',(-0.297088735316081,2.7339065567896,
12.5219528491417));
#418212=CARTESIAN_POINT('Ctrl Pts',(-0.29818292741531,2.73378619167623,
12.5295503425868));
#418213=CARTESIAN_POINT('Ctrl Pts',(-0.298182927376992,2.73378619168012,
12.5369868989719));
#418214=CARTESIAN_POINT('',(-0.14995420399048,2.74590854485462,12.5369868989719));
#418215=CARTESIAN_POINT('Ctrl Pts',(-0.14995420399048,2.74590854485462,
12.5369868989719));
#418216=CARTESIAN_POINT('Ctrl Pts',(-0.149954203990483,2.74590854485462,
12.5309445149785));
#418217=CARTESIAN_POINT('Ctrl Pts',(-0.150676985096012,2.7458694780945,
12.5248274368704));
#418218=CARTESIAN_POINT('Ctrl Pts',(-0.152331115421984,2.7457777097344,
12.5190199595513));
#418219=CARTESIAN_POINT('Ctrl Pts',(-0.153720481107187,2.74570063006994,
12.5141420429941));
#418220=CARTESIAN_POINT('Ctrl Pts',(-0.155809861207817,2.74558402196563,
12.5093757677094));
#418221=CARTESIAN_POINT('Ctrl Pts',(-0.15869200772821,2.74541742667362,
12.5051960112707));
#418222=CARTESIAN_POINT('Ctrl Pts',(-0.160617480301142,2.74530612953335,
12.5024036458141));
#418223=CARTESIAN_POINT('Ctrl Pts',(-0.162943453780979,2.74516965718165,
12.4998248032393));
#418224=CARTESIAN_POINT('Ctrl Pts',(-0.165587390940443,2.74501016682298,
12.4976950015772));
#418225=CARTESIAN_POINT('Ctrl Pts',(-0.168305823588117,2.74484618266911,
12.495505190692));
#418226=CARTESIAN_POINT('Ctrl Pts',(-0.171430472538395,2.74465343114511,
12.4937456938368));
#418227=CARTESIAN_POINT('Ctrl Pts',(-0.174719873295569,2.74444401762462,
12.4925987732155));
#418228=CARTESIAN_POINT('Ctrl Pts',(-0.178008504345647,2.74423465310609,
12.4914521209692));
#418229=CARTESIAN_POINT('Ctrl Pts',(-0.181543797025532,2.74400328516659,
12.4908873016276));
#418230=CARTESIAN_POINT('Ctrl Pts',(-0.185025766221201,2.74376847890529,
12.4908873016278));
#418231=CARTESIAN_POINT('',(-0.149954203990482,2.74590854485461,13.7435492065112));
#418232=CARTESIAN_POINT('',(-0.149954203990482,2.74590854485462,14.));
#418233=CARTESIAN_POINT('',(-0.0743617944298036,2.74899442042525,13.7435492065112));
#418234=CARTESIAN_POINT('Origin',(0.,2.5406128344257E-15,13.7435492065112));
#418235=CARTESIAN_POINT('',(-0.0743617944298037,2.74899442042526,12.5369868989719));
#418236=CARTESIAN_POINT('',(-0.0743617944298037,2.74899442042526,14.));
#418237=CARTESIAN_POINT('Ctrl Pts',(-0.0392324946869358,2.74972013327914,
12.4908873016278));
#418238=CARTESIAN_POINT('Ctrl Pts',(-0.0414135992962603,2.74968901368484,
12.4908873016278));
#418239=CARTESIAN_POINT('Ctrl Pts',(-0.0436069602666705,2.74965506839015,
12.4911020829134));
#418240=CARTESIAN_POINT('Ctrl Pts',(-0.0457425737882799,2.74961954039886,
12.4915448903141));
#418241=CARTESIAN_POINT('Ctrl Pts',(-0.0493963482810018,2.74955875633514,
12.4923024798169));
#418242=CARTESIAN_POINT('Ctrl Pts',(-0.0529649940464467,2.74949168260351,
12.4937722312795));
#418243=CARTESIAN_POINT('Ctrl Pts',(-0.0560953648186719,2.74942781502731,
12.4958030942394));
#418244=CARTESIAN_POINT('Ctrl Pts',(-0.0592036403776707,2.74936439825002,
12.4978196226833));
#418245=CARTESIAN_POINT('Ctrl Pts',(-0.0619719583677341,2.74930258337428,
12.5004326847668));
#418246=CARTESIAN_POINT('Ctrl Pts',(-0.0642557541775498,2.74924920624797,
12.5033504258767));
#418247=CARTESIAN_POINT('Ctrl Pts',(-0.0669844867678712,2.74918543001039,
12.5068366111226));
#418248=CARTESIAN_POINT('Ctrl Pts',(-0.0691093207995963,2.74913191833457,
12.5108395010833));
#418249=CARTESIAN_POINT('Ctrl Pts',(-0.0706588501132809,2.74909209138229,
12.5149868989719));
#418250=CARTESIAN_POINT('Ctrl Pts',(-0.0732614323288725,2.74902519821882,
12.5219528491417));
#418251=CARTESIAN_POINT('Ctrl Pts',(-0.0743617944682905,2.7489944204245,
12.5295503425868));
#418252=CARTESIAN_POINT('Ctrl Pts',(-0.0743617944298037,2.74899442042526,
12.5369868989719));
#418253=CARTESIAN_POINT('',(-3.36777869765522E-16,2.75,14.));
#418254=CARTESIAN_POINT('',(0.0743617944298038,2.74899442042526,12.5369868989719));
#418255=CARTESIAN_POINT('Ctrl Pts',(0.0743617944298037,2.74899442042526,
12.5369868989719));
#418256=CARTESIAN_POINT('Ctrl Pts',(0.0743617944298037,2.74899442042526,
12.5309445149785));
#418257=CARTESIAN_POINT('Ctrl Pts',(0.0736382340151502,2.74901439702663,
12.5248274368704));
#418258=CARTESIAN_POINT('Ctrl Pts',(0.0719821276980976,2.74905776099595,
12.5190199595513));
#418259=CARTESIAN_POINT('Ctrl Pts',(0.070591102304372,2.7490941840093,12.5141420429941));
#418260=CARTESIAN_POINT('Ctrl Pts',(0.0684991698006262,2.7491482677839,
12.5093757677094));
#418261=CARTESIAN_POINT('Ctrl Pts',(0.0656130343221262,2.74921714852193,
12.5051960112707));
#418262=CARTESIAN_POINT('Ctrl Pts',(0.0636848968501762,2.74926316560363,
12.5024036458141));
#418263=CARTESIAN_POINT('Ctrl Pts',(0.061355539091602,2.7493167357843,12.4998248032393));
#418264=CARTESIAN_POINT('Ctrl Pts',(0.0587073994700591,2.74937328154026,
12.4976950015772));
#418265=CARTESIAN_POINT('Ctrl Pts',(0.0559846459518707,2.74943142052762,
12.495505190692));
#418266=CARTESIAN_POINT('Ctrl Pts',(0.0528546829745851,2.74949399826569,
12.4937456938368));
#418267=CARTESIAN_POINT('Ctrl Pts',(0.0495591582810547,2.74955339825043,
12.4925987732155));
#418268=CARTESIAN_POINT('Ctrl Pts',(0.0462644047275967,2.7496127843358,
12.4914521209692));
#418269=CARTESIAN_POINT('Ctrl Pts',(0.042722016807478,2.7496703454275,12.4908873016276));
#418270=CARTESIAN_POINT('Ctrl Pts',(0.0392324946869349,2.74972013327914,
12.4908873016278));
#418271=CARTESIAN_POINT('',(0.0743617944298037,2.74899442042525,13.7435492065112));
#418272=CARTESIAN_POINT('',(0.0743617944298038,2.74899442042526,14.));
#418273=CARTESIAN_POINT('',(0.149954203990446,2.74590854485462,13.7435492065112));
#418274=CARTESIAN_POINT('Origin',(0.,2.5406128344257E-15,13.7435492065112));
#418275=CARTESIAN_POINT('',(0.149954203990446,2.74590854485462,12.5369868989719));
#418276=CARTESIAN_POINT('',(0.149954203990446,2.74590854485462,14.));
#418277=CARTESIAN_POINT('Ctrl Pts',(0.185025766221164,2.7437684789053,12.4908873016278));
#418278=CARTESIAN_POINT('Ctrl Pts',(0.182849382521663,2.74391524313292,
12.4908873016278));
#418279=CARTESIAN_POINT('Ctrl Pts',(0.180660552922293,2.74406019006967,
12.4911020829134));
#418280=CARTESIAN_POINT('Ctrl Pts',(0.178529149617384,2.74419885262291,
12.4915448903141));
#418281=CARTESIAN_POINT('Ctrl Pts',(0.174882578292387,2.7444360873543,12.4923024798169));
#418282=CARTESIAN_POINT('Ctrl Pts',(0.171320339769525,2.74466011456455,
12.4937722312795));
#418283=CARTESIAN_POINT('Ctrl Pts',(0.168195179247428,2.74485161378132,
12.4958030942394));
#418284=CARTESIAN_POINT('Ctrl Pts',(0.165092077162855,2.745041761332,12.4978196226833));
#418285=CARTESIAN_POINT('Ctrl Pts',(0.1623279320363,2.74520579575617,12.5004326847668));
#418286=CARTESIAN_POINT('Ctrl Pts',(0.160047384637318,2.74533874679806,
12.5033504258767));
#418287=CARTESIAN_POINT('Ctrl Pts',(0.157322533324154,2.74549759980908,
12.5068366111226));
#418288=CARTESIAN_POINT('Ctrl Pts',(0.155200407804025,2.74561745988853,
12.5108395010833));
#418289=CARTESIAN_POINT('Ctrl Pts',(0.153652788154959,2.74570406648135,
12.5149868989719));
#418290=CARTESIAN_POINT('Ctrl Pts',(0.151053413403163,2.74584953051112,
12.5219528491417));
#418291=CARTESIAN_POINT('Ctrl Pts',(0.149954203952006,2.745908544857,12.5295503425868));
#418292=CARTESIAN_POINT('Ctrl Pts',(0.149954203990446,2.74590854485462,
12.5369868989719));
#418293=CARTESIAN_POINT('',(0.298182927376958,2.73378619168012,12.5369868989719));
#418294=CARTESIAN_POINT('Ctrl Pts',(0.298182927376958,2.73378619168012,
12.5369868989719));
#418295=CARTESIAN_POINT('Ctrl Pts',(0.298182927376955,2.73378619168012,
12.5309445149785));
#418296=CARTESIAN_POINT('Ctrl Pts',(0.297463402828359,2.73386507870201,
12.5248274368704));
#418297=CARTESIAN_POINT('Ctrl Pts',(0.295816341634529,2.73404328642068,
12.5190199595513));
#418298=CARTESIAN_POINT('Ctrl Pts',(0.294432913576771,2.73419296972269,
12.5141420429941));
#418299=CARTESIAN_POINT('Ctrl Pts',(0.292352350135577,2.7344173854576,12.5093757677094));
#418300=CARTESIAN_POINT('Ctrl Pts',(0.2894814324544,2.73472128383573,12.5051960112707));
#418301=CARTESIAN_POINT('Ctrl Pts',(0.287563461520187,2.73492430890331,
12.5024036458141));
#418302=CARTESIAN_POINT('Ctrl Pts',(0.285246220974444,2.73516756511565,
12.4998248032393));
#418303=CARTESIAN_POINT('Ctrl Pts',(0.282611501823092,2.73543977068356,
12.4976950015772));
#418304=CARTESIAN_POINT('Ctrl Pts',(0.279902546909829,2.73571964590677,
12.495505190692));
#418305=CARTESIAN_POINT('Ctrl Pts',(0.276788099292741,2.73603713646238,
12.4937456938368));
#418306=CARTESIAN_POINT('Ctrl Pts',(0.273508381835966,2.73636495465526,
12.4925987732155));
#418307=CARTESIAN_POINT('Ctrl Pts',(0.270229431820431,2.73669269613994,
12.4914521209692));
#418308=CARTESIAN_POINT('Ctrl Pts',(0.266703522667235,2.73703880320326,
12.4908873016276));
#418309=CARTESIAN_POINT('Ctrl Pts',(0.2632296698158,2.7373728538379,12.4908873016278));
#418310=CARTESIAN_POINT('',(0.298182927376956,2.73378619168012,13.7435492065112));
#418311=CARTESIAN_POINT('',(0.298182927376956,2.73378619168012,14.));
#418312=CARTESIAN_POINT('',(0.373272281923878,2.72454910096099,13.7435492065112));
#418313=CARTESIAN_POINT('Origin',(0.,2.5406128344257E-15,13.7435492065112));
#418314=CARTESIAN_POINT('',(0.373272281923878,2.72454910096099,12.5369868989719));
#418315=CARTESIAN_POINT('',(0.373272281923878,2.72454910096099,14.));
#418316=CARTESIAN_POINT('Ctrl Pts',(0.408052711182201,2.71955749799427,
12.4908873016278));
#418317=CARTESIAN_POINT('Ctrl Pts',(0.405895531866964,2.71988116935211,
12.4908873016278));
#418318=CARTESIAN_POINT('Ctrl Pts',(0.403725799938487,2.72020404392233,
12.4911020829134));
#418319=CARTESIAN_POINT('Ctrl Pts',(0.401612790987617,2.7205159742437,12.4915448903141));
#418320=CARTESIAN_POINT('Ctrl Pts',(0.397997690160871,2.72104964901219,
12.4923024798169));
#418321=CARTESIAN_POINT('Ctrl Pts',(0.394465564990232,2.72156328630021,
12.4937722312795));
#418322=CARTESIAN_POINT('Ctrl Pts',(0.391366412145924,2.72200887791426,
12.4958030942394));
#418323=CARTESIAN_POINT('Ctrl Pts',(0.388289134168174,2.72245132439233,
12.4978196226833));
#418324=CARTESIAN_POINT('Ctrl Pts',(0.385547556834892,2.72284011649437,
12.5004326847668));
#418325=CARTESIAN_POINT('Ctrl Pts',(0.38328543451342,2.72315851093723,12.5033504258767));
#418326=CARTESIAN_POINT('Ctrl Pts',(0.380582597913333,2.72353893605627,
12.5068366111226));
#418327=CARTESIAN_POINT('Ctrl Pts',(0.378477303300012,2.72383137024193,
12.5108395010833));
#418328=CARTESIAN_POINT('Ctrl Pts',(0.376941892468989,2.72404383402726,
12.5149868989719));
#418329=CARTESIAN_POINT('Ctrl Pts',(0.374363023591095,2.72440068721116,
12.5219528491417));
#418330=CARTESIAN_POINT('Ctrl Pts',(0.37327228188576,2.7245491009665,12.5295503425868));
#418331=CARTESIAN_POINT('Ctrl Pts',(0.373272281923878,2.72454910096099,
12.5369868989719));
#418332=CARTESIAN_POINT('',(0.520019702139173,2.70038506687233,12.5369868989719));
#418333=CARTESIAN_POINT('Ctrl Pts',(0.520019702139173,2.70038506687233,
12.5369868989719));
#418334=CARTESIAN_POINT('Ctrl Pts',(0.520019702139171,2.70038506687233,
12.5309445149785));
#418335=CARTESIAN_POINT('Ctrl Pts',(0.519309001773788,2.70052233933461,
12.5248274368704));
#418336=CARTESIAN_POINT('Ctrl Pts',(0.517681946623677,2.70083420485966,
12.5190199595513));
#418337=CARTESIAN_POINT('Ctrl Pts',(0.516315322387364,2.70109615233266,
12.5141420429941));
#418338=CARTESIAN_POINT('Ctrl Pts',(0.514259973815156,2.70148940657819,
12.5093757677094));
#418339=CARTESIAN_POINT('Ctrl Pts',(0.5114233794148,2.70202630020286,12.5051960112707));
#418340=CARTESIAN_POINT('Ctrl Pts',(0.509528338798451,2.70238498215798,
12.5024036458141));
#418341=CARTESIAN_POINT('Ctrl Pts',(0.507238636319051,2.70281630557204,
12.4998248032393));
#418342=CARTESIAN_POINT('Ctrl Pts',(0.504634871259143,2.70330235946874,
12.4976950015772));
#418343=CARTESIAN_POINT('Ctrl Pts',(0.501957742598808,2.70380210840438,
12.495505190692));
#418344=CARTESIAN_POINT('Ctrl Pts',(0.498879536476964,2.70437239893028,
12.4937456938368));
#418345=CARTESIAN_POINT('Ctrl Pts',(0.495637452235504,2.7049664537553,12.4925987732155));
#418346=CARTESIAN_POINT('Ctrl Pts',(0.492396126629256,2.70556036957378,
12.4914521209692));
#418347=CARTESIAN_POINT('Ctrl Pts',(0.488910160586661,2.70619271932333,
12.4908873016276));
#418348=CARTESIAN_POINT('Ctrl Pts',(0.485475094921914,2.70680880968911,
12.4908873016278));
#418349=CARTESIAN_POINT('',(0.52001970213917,2.70038506687233,13.7435492065112));
#418350=CARTESIAN_POINT('',(0.520019702139171,2.70038506687234,14.));
#418351=CARTESIAN_POINT('',(0.594106294406697,2.68505823231943,13.7435492065112));
#418352=CARTESIAN_POINT('Origin',(0.,2.5406128344257E-15,13.7435492065112));
#418353=CARTESIAN_POINT('',(0.594106294406698,2.68505823231943,12.5369868989719));
#418354=CARTESIAN_POINT('',(0.594106294406698,2.68505823231943,14.));
#418355=CARTESIAN_POINT('Ctrl Pts',(0.628364132674278,2.6772483106295,12.4908873016278));
#418356=CARTESIAN_POINT('Ctrl Pts',(0.62624051341574,2.67774673513806,12.4908873016278));
#418357=CARTESIAN_POINT('Ctrl Pts',(0.624104318366159,2.67824538866476,
12.4911020829134));
#418358=CARTESIAN_POINT('Ctrl Pts',(0.622023765495274,2.67872851090944,
12.4915448903141));
#418359=CARTESIAN_POINT('Ctrl Pts',(0.61846419306633,2.6795550741975,12.4923024798169));
#418360=CARTESIAN_POINT('Ctrl Pts',(0.614985686958166,2.68035490339187,
12.4937722312795));
#418361=CARTESIAN_POINT('Ctrl Pts',(0.611933166142502,2.68105162206453,
12.4958030942394));
#418362=CARTESIAN_POINT('Ctrl Pts',(0.608902191048801,2.68174342306169,
12.4978196226833));
#418363=CARTESIAN_POINT('Ctrl Pts',(0.606201426253617,2.6823543854943,12.5004326847668));
#418364=CARTESIAN_POINT('Ctrl Pts',(0.60397278306048,2.68285610447564,12.5033504258767));
#418365=CARTESIAN_POINT('Ctrl Pts',(0.601309948105109,2.68345557003629,
12.5068366111226));
#418366=CARTESIAN_POINT('Ctrl Pts',(0.599235494786896,2.68391863222692,
12.5108395010833));
#418367=CARTESIAN_POINT('Ctrl Pts',(0.597722510679673,2.68425553929331,
12.5149868989719));
#418368=CARTESIAN_POINT('Ctrl Pts',(0.595181309622579,2.68482140683228,
12.5219528491417));
#418369=CARTESIAN_POINT('Ctrl Pts',(0.594106294369155,2.68505823232803,
12.5295503425868));
#418370=CARTESIAN_POINT('Ctrl Pts',(0.594106294406698,2.68505823231943,
12.5369868989719));
#418371=CARTESIAN_POINT('',(0.738395831580863,2.64901332497668,12.5369868989719));
#418372=CARTESIAN_POINT('Ctrl Pts',(0.738395831580863,2.64901332497668,
12.5369868989719));
#418373=CARTESIAN_POINT('Ctrl Pts',(0.738395831580862,2.64901332497668,
12.5309445149785));
#418374=CARTESIAN_POINT('Ctrl Pts',(0.737698684992366,2.64920806935377,
12.5248274368704));
#418375=CARTESIAN_POINT('Ctrl Pts',(0.736102463669554,2.64965151727159,
12.5190199595513));
#418376=CARTESIAN_POINT('Ctrl Pts',(0.7347617379135,2.65002398569836,12.5141420429941));
#418377=CARTESIAN_POINT('Ctrl Pts',(0.732745282215917,2.65058346141239,
12.5093757677094));
#418378=CARTESIAN_POINT('Ctrl Pts',(0.729961888164113,2.6513497773451,12.5051960112707));
#418379=CARTESIAN_POINT('Ctrl Pts',(0.728102389048269,2.65186172921853,
12.5024036458141));
#418380=CARTESIAN_POINT('Ctrl Pts',(0.725855462227438,2.65247824944814,
12.4998248032393));
#418381=CARTESIAN_POINT('Ctrl Pts',(0.723299978885857,2.65317491706516,
12.4976950015772));
#418382=CARTESIAN_POINT('Ctrl Pts',(0.720672492327989,2.65389121396651,
12.495505190692));
#418383=CARTESIAN_POINT('Ctrl Pts',(0.717651012655261,2.65471050927333,
12.4937456938368));
#418384=CARTESIAN_POINT('Ctrl Pts',(0.714468137164836,2.65556684739364,
12.4925987732155));
#418385=CARTESIAN_POINT('Ctrl Pts',(0.711286006455004,2.65642298513414,
12.4914521209692));
#418386=CARTESIAN_POINT('Ctrl Pts',(0.707863182051883,2.65733736938667,
12.4908873016276));
#418387=CARTESIAN_POINT('Ctrl Pts',(0.704489763369076,2.65823139950385,
12.4908873016278));
#418388=CARTESIAN_POINT('',(0.73839583158086,2.64901332497668,13.7435492065112));
#418389=CARTESIAN_POINT('',(0.738395831580861,2.64901332497668,14.));
#418390=CARTESIAN_POINT('',(0.81098662752088,2.62769874414521,13.7435492065112));
#418391=CARTESIAN_POINT('Origin',(0.,2.5406128344257E-15,13.7435492065112));
#418392=CARTESIAN_POINT('',(0.81098662752088,2.62769874414521,12.5369868989719));
#418393=CARTESIAN_POINT('',(0.81098662752088,2.62769874414521,14.));
#418394=CARTESIAN_POINT('Ctrl Pts',(0.844493894536193,2.61712247747237,
12.4908873016278));
#418395=CARTESIAN_POINT('Ctrl Pts',(0.842417967670147,2.61779233819878,
12.4908873016278));
#418396=CARTESIAN_POINT('Ctrl Pts',(0.840329525525069,2.61846345222502,
12.4911020829134));
#418397=CARTESIAN_POINT('Ctrl Pts',(0.838295274470257,2.61911455129417,
12.4915448903141));
#418398=CARTESIAN_POINT('Ctrl Pts',(0.834814918806343,2.62022850245949,
12.4923024798169));
#418399=CARTESIAN_POINT('Ctrl Pts',(0.83141318064489,2.62130920082889,12.4937722312795));
#418400=CARTESIAN_POINT('Ctrl Pts',(0.828427605880267,2.62225241001234,
12.4958030942394));
#418401=CARTESIAN_POINT('Ctrl Pts',(0.825463104309788,2.62318896170709,
12.4978196226833));
#418402=CARTESIAN_POINT('Ctrl Pts',(0.822821125196819,2.62401802861609,
12.5004326847668));
#418403=CARTESIAN_POINT('Ctrl Pts',(0.820640792384768,2.62469973327886,
12.5033504258767));
#418404=CARTESIAN_POINT('Ctrl Pts',(0.818035679801402,2.62551424993673,
12.5068366111226));
#418405=CARTESIAN_POINT('Ctrl Pts',(0.816005872922871,2.62614485852983,
12.5108395010833));
#418406=CARTESIAN_POINT('Ctrl Pts',(0.814525384199056,2.62660396681635,
12.5149868989719));
#418407=CARTESIAN_POINT('Ctrl Pts',(0.812038762236529,2.62737508295528,
12.5219528491417));
#418408=CARTESIAN_POINT('Ctrl Pts',(0.810986627484164,2.62769874415684,
12.5295503425868));
#418409=CARTESIAN_POINT('Ctrl Pts',(0.81098662752088,2.62769874414521,12.5369868989719));
#418410=CARTESIAN_POINT('',(0.951858058590119,2.58001283645975,12.5369868989719));
#418411=CARTESIAN_POINT('Ctrl Pts',(0.951858058590119,2.58001283645974,
12.5369868989719));
#418412=CARTESIAN_POINT('Ctrl Pts',(0.951858058590117,2.58001283645975,
12.5309445149785));
#418413=CARTESIAN_POINT('Ctrl Pts',(0.951179105174035,2.58026375675994,
12.5248274368704));
#418414=CARTESIAN_POINT('Ctrl Pts',(0.94962434026807,2.5808358359978,12.5190199595513));
#418415=CARTESIAN_POINT('Ctrl Pts',(0.948318435300976,2.58131634666242,
12.5141420429941));
#418416=CARTESIAN_POINT('Ctrl Pts',(0.946354291657993,2.58203832062637,
12.5093757677094));
#418417=CARTESIAN_POINT('Ctrl Pts',(0.943642620982929,2.58302895916102,
12.5051960112707));
#418418=CARTESIAN_POINT('Ctrl Pts',(0.941831038027408,2.58369077399752,
12.5024036458141));
#418419=CARTESIAN_POINT('Ctrl Pts',(0.939641839792423,2.58448838820228,
12.4998248032393));
#418420=CARTESIAN_POINT('Ctrl Pts',(0.937151644489183,2.58539103333156,
12.4976950015772));
#418421=CARTESIAN_POINT('Ctrl Pts',(0.934591285523319,2.58631911136092,
12.495505190692));
#418422=CARTESIAN_POINT('Ctrl Pts',(0.93164663974842,2.58738195917357,12.4937456938368));
#418423=CARTESIAN_POINT('Ctrl Pts',(0.928544154520281,2.58849488180028,
12.4925987732155));
#418424=CARTESIAN_POINT('Ctrl Pts',(0.925442395261725,2.58960754400738,
12.4914521209692));
#418425=CARTESIAN_POINT('Ctrl Pts',(0.922105490829752,2.59079787768654,
12.4908873016276));
#418426=CARTESIAN_POINT('Ctrl Pts',(0.918816168673647,2.5919638979322,12.4908873016278));
#418427=CARTESIAN_POINT('',(0.951858058590117,2.58001283645974,13.7435492065112));
#418428=CARTESIAN_POINT('',(0.951858058590117,2.58001283645975,14.));
#418429=CARTESIAN_POINT('',(1.02246997843229,2.55285235436848,13.7435492065112));
#418430=CARTESIAN_POINT('Origin',(0.,2.5406128344257E-15,13.7435492065112));
#418431=CARTESIAN_POINT('',(1.02246997843229,2.55285235436848,12.5369868989719));
#418432=CARTESIAN_POINT('',(1.02246997843229,2.55285235436848,14.));
#418433=CARTESIAN_POINT('Ctrl Pts',(1.05500368886165,2.53958012602247,12.4908873016278));
#418434=CARTESIAN_POINT('Ctrl Pts',(1.05298926933889,2.54041696515413,12.4908873016278));
#418435=CARTESIAN_POINT('Ctrl Pts',(1.05096247833622,2.54125607352678,12.4911020829134));
#418436=CARTESIAN_POINT('Ctrl Pts',(1.04898806670263,2.54207081646352,12.4915448903141));
#418437=CARTESIAN_POINT('Ctrl Pts',(1.04561008899647,2.54346474234489,12.4923024798169));
#418438=CARTESIAN_POINT('Ctrl Pts',(1.04230775678794,2.54481911801997,12.4937722312795));
#418439=CARTESIAN_POINT('Ctrl Pts',(1.03940899658183,2.54600254081271,12.4958030942394));
#418440=CARTESIAN_POINT('Ctrl Pts',(1.03653069680342,2.54717761060804,12.4978196226833));
#418441=CARTESIAN_POINT('Ctrl Pts',(1.03396508530777,2.54821926468994,12.5004326847668));
#418442=CARTESIAN_POINT('Ctrl Pts',(1.03184757263194,2.54907641840208,12.5033504258767));
#418443=CARTESIAN_POINT('Ctrl Pts',(1.029317519015,2.5501005656832,12.5068366111226));
#418444=CARTESIAN_POINT('Ctrl Pts',(1.02734586660604,2.55089452408264,12.5108395010833));
#418445=CARTESIAN_POINT('Ctrl Pts',(1.02590772567382,2.55147277829938,12.5149868989719));
#418446=CARTESIAN_POINT('Ctrl Pts',(1.02349223086476,2.55244401138759,12.5219528491417));
#418447=CARTESIAN_POINT('Ctrl Pts',(1.02246997839664,2.55285235438306,12.5295503425868));
#418448=CARTESIAN_POINT('Ctrl Pts',(1.02246997843229,2.55285235436848,12.5369868989719));
#418449=CARTESIAN_POINT('',(1.15898582726498,2.49384278818832,12.5369868989719));
#418450=CARTESIAN_POINT('Ctrl Pts',(1.15898582726498,2.49384278818832,12.5369868989719));
#418451=CARTESIAN_POINT('Ctrl Pts',(1.15898582726498,2.49384278818832,12.5309445149785));
#418452=CARTESIAN_POINT('Ctrl Pts',(1.15832958534428,2.49414821457842,12.5248274368704));
#418453=CARTESIAN_POINT('Ctrl Pts',(1.15682662355909,2.49484511804338,12.5190199595513));
#418454=CARTESIAN_POINT('Ctrl Pts',(1.15556422996305,2.49543047322665,12.5141420429941));
#418455=CARTESIAN_POINT('Ctrl Pts',(1.15366546942655,2.49631014082293,12.5093757677094));
#418456=CARTESIAN_POINT('Ctrl Pts',(1.15104356784918,2.49751850942351,12.5051960112707));
#418457=CARTESIAN_POINT('Ctrl Pts',(1.14929195683966,2.49832578295453,12.5024036458141));
#418458=CARTESIAN_POINT('Ctrl Pts',(1.14717505594358,2.49929918314349,12.4998248032393));
#418459=CARTESIAN_POINT('Ctrl Pts',(1.14476672051757,2.50040179883063,12.4976950015772));
#418460=CARTESIAN_POINT('Ctrl Pts',(1.1422905279102,2.50153548178184,12.495505190692));
#418461=CARTESIAN_POINT('Ctrl Pts',(1.13944231216493,2.50283480902348,12.4937456938368));
#418462=CARTESIAN_POINT('Ctrl Pts',(1.1364408637264,2.50419690984012,12.4925987732155));
#418463=CARTESIAN_POINT('Ctrl Pts',(1.13344011761523,2.50555869193042,12.4914521209692));
#418464=CARTESIAN_POINT('Ctrl Pts',(1.13021133970285,2.50701705356197,12.4908873016276));
#418465=CARTESIAN_POINT('Ctrl Pts',(1.12702800396969,2.50844730426376,12.4908873016278));
#418466=CARTESIAN_POINT('',(1.15898582726498,2.49384278818832,13.7435492065112));
#418467=CARTESIAN_POINT('',(1.15898582726498,2.49384278818833,14.));
#418468=CARTESIAN_POINT('',(1.2271489603329,2.46101715336442,13.7435492065112));
#418469=CARTESIAN_POINT('Origin',(0.,2.5406128344257E-15,13.7435492065112));
#418470=CARTESIAN_POINT('',(1.2271489603329,2.46101715336442,12.5369868989719));
#418471=CARTESIAN_POINT('',(1.2271489603329,2.46101715336442,14.));
#418472=CARTESIAN_POINT('Ctrl Pts',(1.2584926077011,2.44513728783512,12.4908873016278));
#418473=CARTESIAN_POINT('Ctrl Pts',(1.25655310115118,2.44613553634567,12.4908873016278));
#418474=CARTESIAN_POINT('Ctrl Pts',(1.25460144925065,2.44713705493696,12.4911020829134));
#418475=CARTESIAN_POINT('Ctrl Pts',(1.25270001642194,2.44811001976147,12.4915448903141));
#418476=CARTESIAN_POINT('Ctrl Pts',(1.24944689655784,2.44977464401213,12.4923024798169));
#418477=CARTESIAN_POINT('Ctrl Pts',(1.24626594677824,2.45139368384623,12.4937722312795));
#418478=CARTESIAN_POINT('Ctrl Pts',(1.24347329190156,2.45280944476482,12.4958030942394));
#418479=CARTESIAN_POINT('Ctrl Pts',(1.24070034852535,2.45421521276512,12.4978196226833));
#418480=CARTESIAN_POINT('Ctrl Pts',(1.23822817836822,2.45546252198386,12.5004326847668));
#418481=CARTESIAN_POINT('Ctrl Pts',(1.2361875775261,2.45648942052885,12.5033504258767));
#418482=CARTESIAN_POINT('Ctrl Pts',(1.233749419965,2.45771638290202,12.5068366111226));
#418483=CARTESIAN_POINT('Ctrl Pts',(1.23184904304708,2.45866840744564,12.5108395010833));
#418484=CARTESIAN_POINT('Ctrl Pts',(1.23046282049709,2.45936195940621,12.5149868989719));
#418485=CARTESIAN_POINT('Ctrl Pts',(1.22813452756092,2.46052684604774,12.5219528491417));
#418486=CARTESIAN_POINT('Ctrl Pts',(1.22714896029856,2.46101715338186,12.5295503425868));
#418487=CARTESIAN_POINT('Ctrl Pts',(1.2271489603329,2.46101715336442,12.5369868989719));
#418488=CARTESIAN_POINT('',(1.3584007364786,2.39107662761661,12.5369868989719));
#418489=CARTESIAN_POINT('Ctrl Pts',(1.3584007364786,2.39107662761661,12.5369868989719));
#418490=CARTESIAN_POINT('Ctrl Pts',(1.3584007364786,2.39107662761661,12.5309445149785));
#418491=CARTESIAN_POINT('Ctrl Pts',(1.35777157323498,2.39143452753438,12.5248274368704));
#418492=CARTESIAN_POINT('Ctrl Pts',(1.35633041653328,2.39225161744886,12.5190199595513));
#418493=CARTESIAN_POINT('Ctrl Pts',(1.3551199353294,2.39293792170861,12.5141420429941));
#418494=CARTESIAN_POINT('Ctrl Pts',(1.35329919383748,2.39396942889448,12.5093757677094));
#418495=CARTESIAN_POINT('Ctrl Pts',(1.35078450968021,2.39538748606734,12.5051960112707));
#418496=CARTESIAN_POINT('Ctrl Pts',(1.34910452729897,2.39633484602071,12.5024036458141));
#418497=CARTESIAN_POINT('Ctrl Pts',(1.347074011368,2.39747755437623,12.4998248032393));
#418498=CARTESIAN_POINT('Ctrl Pts',(1.34476356289413,2.39877280289574,12.4976950015772));
#418499=CARTESIAN_POINT('Ctrl Pts',(1.34238801529851,2.40010454629581,12.495505190692));
#418500=CARTESIAN_POINT('Ctrl Pts',(1.33965518398873,2.40163170615802,12.4937456938368));
#418501=CARTESIAN_POINT('Ctrl Pts',(1.33677474648396,2.40323392060839,12.4925987732155));
#418502=CARTESIAN_POINT('Ctrl Pts',(1.33389498299045,2.40483576014675,12.4914521209692));
#418503=CARTESIAN_POINT('Ctrl Pts',(1.33079581858196,2.40655244457465,12.4908873016276));
#418504=CARTESIAN_POINT('Ctrl Pts',(1.32773965384585,2.40823740765011,12.4908873016278));
#418505=CARTESIAN_POINT('',(1.3584007364786,2.39107662761661,13.7435492065112));
#418506=CARTESIAN_POINT('',(1.3584007364786,2.39107662761661,14.));
#418507=CARTESIAN_POINT('',(1.42366146836782,2.35280428924396,13.7435492065112));
#418508=CARTESIAN_POINT('Origin',(0.,2.5406128344257E-15,13.7435492065112));
#418509=CARTESIAN_POINT('',(1.42366146836782,2.35280428924396,12.5369868989719));
#418510=CARTESIAN_POINT('',(1.42366146836782,2.35280428924396,14.));
#418511=CARTESIAN_POINT('Ctrl Pts',(1.45360646587295,2.33442246441649,12.4908873016278));
#418512=CARTESIAN_POINT('Ctrl Pts',(1.45175477939198,2.33557547912678,12.4908873016278));
#418513=CARTESIAN_POINT('Ctrl Pts',(1.44989125451499,2.33673274299572,12.4911020829134));
#418514=CARTESIAN_POINT('Ctrl Pts',(1.44807545421291,2.33785745478763,12.4915448903141));
#418515=CARTESIAN_POINT('Ctrl Pts',(1.44496884116685,2.33978169960783,12.4923024798169));
#418516=CARTESIAN_POINT('Ctrl Pts',(1.44193044251215,2.34165462915798,12.4937722312795));
#418517=CARTESIAN_POINT('Ctrl Pts',(1.43926247762233,2.3432933065471,12.4958030942394));
#418518=CARTESIAN_POINT('Ctrl Pts',(1.43661334412899,2.34492041759825,12.4978196226833));
#418519=CARTESIAN_POINT('Ctrl Pts',(1.43425106719491,2.34636508131678,12.5004326847668));
#418520=CARTESIAN_POINT('Ctrl Pts',(1.43230095804843,2.34755489085422,12.5033504258767));
#418521=CARTESIAN_POINT('Ctrl Pts',(1.42997092207945,2.34897650308729,12.5068366111226));
#418522=CARTESIAN_POINT('Ctrl Pts',(1.42815446734742,2.35008025820883,12.5108395010833));
#418523=CARTESIAN_POINT('Ctrl Pts',(1.42682938826203,2.35088449243935,12.5149868989719));
#418524=CARTESIAN_POINT('Ctrl Pts',(1.42460379160409,2.35223528050579,12.5219528491417));
#418525=CARTESIAN_POINT('Ctrl Pts',(1.42366146833502,2.35280428926415,12.5295503425868));
#418526=CARTESIAN_POINT('Ctrl Pts',(1.42366146836782,2.35280428924396,12.5369868989719));
#418527=CARTESIAN_POINT('',(1.5487757129113,2.27239824658798,12.5369868989719));
#418528=CARTESIAN_POINT('Ctrl Pts',(1.5487757129113,2.27239824658798,12.5369868989719));
#418529=CARTESIAN_POINT('Ctrl Pts',(1.5487757129113,2.27239824658798,12.5309445149785));
#418530=CARTESIAN_POINT('Ctrl Pts',(1.54817781532235,2.27280623826852,12.5248274368704));
#418531=CARTESIAN_POINT('Ctrl Pts',(1.5468080543642,2.27373807703395,12.5190199595513));
#418532=CARTESIAN_POINT('Ctrl Pts',(1.54565754110519,2.27452076312857,12.5141420429941));
#418533=CARTESIAN_POINT('Ctrl Pts',(1.54392693539208,2.2756972453939,12.5093757677094));
#418534=CARTESIAN_POINT('Ctrl Pts',(1.54153620346308,2.2773155542025,12.5051960112707));
#418535=CARTESIAN_POINT('Ctrl Pts',(1.53993902971568,2.27839669605405,12.5024036458141));
#418536=CARTESIAN_POINT('Ctrl Pts',(1.53800841149833,2.27970110804054,12.4998248032393));
#418537=CARTESIAN_POINT('Ctrl Pts',(1.53581122563,2.28118036972724,12.4976950015772));
#418538=CARTESIAN_POINT('Ctrl Pts',(1.53355213192344,2.28270131104355,12.495505190692));
#418539=CARTESIAN_POINT('Ctrl Pts',(1.53095287159063,2.28444614052942,12.4937456938368));
#418540=CARTESIAN_POINT('Ctrl Pts',(1.52821261385598,2.28627780614069,12.4925987732155));
#418541=CARTESIAN_POINT('Ctrl Pts',(1.52547299733106,2.28810904314927,12.4914521209692));
#418542=CARTESIAN_POINT('Ctrl Pts',(1.52252407085427,2.29007262612189,12.4908873016276));
#418543=CARTESIAN_POINT('Ctrl Pts',(1.51961541538728,2.29200108841975,12.4908873016278));
#418544=CARTESIAN_POINT('',(1.5487757129113,2.27239824658798,13.7435492065112));
#418545=CARTESIAN_POINT('',(1.5487757129113,2.27239824658798,14.));
#418546=CARTESIAN_POINT('',(1.61069974421836,2.22893390076397,13.7435492065112));
#418547=CARTESIAN_POINT('Origin',(0.,2.5406128344257E-15,13.7435492065112));
#418548=CARTESIAN_POINT('',(1.61069974421836,2.22893390076398,12.5369868989719));
#418549=CARTESIAN_POINT('',(1.61069974421836,2.22893390076398,14.));
#418550=CARTESIAN_POINT('Ctrl Pts',(1.63904681284261,2.20817244464976,12.4908873016278));
#418551=CARTESIAN_POINT('Ctrl Pts',(1.63729526909861,2.20947255243714,12.4908873016278));
#418552=CARTESIAN_POINT('Ctrl Pts',(1.63553227269574,2.21077786018362,12.4911020829134));
#418553=CARTESIAN_POINT('Ctrl Pts',(1.63381418877174,2.2120468341715,12.4915448903141));
#418554=CARTESIAN_POINT('Ctrl Pts',(1.63087475654097,2.21421789402945,12.4923024798169));
#418555=CARTESIAN_POINT('Ctrl Pts',(1.62799912905291,2.2163322492585,12.4937722312795));
#418556=CARTESIAN_POINT('Ctrl Pts',(1.62547360901613,2.21818293799049,12.4958030942394));
#418557=CARTESIAN_POINT('Ctrl Pts',(1.62296591495198,2.22002056393691,12.4978196226833));
#418558=CARTESIAN_POINT('Ctrl Pts',(1.62072925180418,2.22165296815653,12.5004326847668));
#418559=CARTESIAN_POINT('Ctrl Pts',(1.61888261200797,2.22299777070025,12.5033504258767));
#418560=CARTESIAN_POINT('Ctrl Pts',(1.61667620363606,2.22460457219836,12.5068366111226));
#418561=CARTESIAN_POINT('Ctrl Pts',(1.61495575929647,2.22585271258959,12.5108395010833));
#418562=CARTESIAN_POINT('Ctrl Pts',(1.61370064185836,2.22676227704395,12.5149868989719));
#418563=CARTESIAN_POINT('Ctrl Pts',(1.61159255245722,2.22828997726358,12.5219528491417));
#418564=CARTESIAN_POINT('Ctrl Pts',(1.61069974418731,2.22893390078676,12.5295503425868));
#418565=CARTESIAN_POINT('Ctrl Pts',(1.61069974421836,2.22893390076398,12.5369868989719));
#418566=CARTESIAN_POINT('',(1.72884384250458,2.13859743014762,12.5369868989719));
#418567=CARTESIAN_POINT('Ctrl Pts',(1.72884384250458,2.13859743014762,12.5369868989719));
#418568=CARTESIAN_POINT('Ctrl Pts',(1.72884384250458,2.13859743014762,12.5309445149785));
#418569=CARTESIAN_POINT('Ctrl Pts',(1.72828118948011,2.13905279847361,12.5248274368704));
#418570=CARTESIAN_POINT('Ctrl Pts',(1.72699193979871,2.14009318485675,12.5190199595513));
#418571=CARTESIAN_POINT('Ctrl Pts',(1.72590905096046,2.14096704413941,12.5141420429941));
#418572=CARTESIAN_POINT('Ctrl Pts',(1.72428009792165,2.14228067218884,12.5093757677094));
#418573=CARTESIAN_POINT('Ctrl Pts',(1.72202922814747,2.14408846305507,12.5051960112707));
#418574=CARTESIAN_POINT('Ctrl Pts',(1.72052549196169,2.14529619198414,12.5024036458141));
#418575=CARTESIAN_POINT('Ctrl Pts',(1.71870761940366,2.14675362695506,12.4998248032393));
#418576=CARTESIAN_POINT('Ctrl Pts',(1.71663831805031,2.14840705756647,12.4976950015772));
#418577=CARTESIAN_POINT('Ctrl Pts',(1.71451071212871,2.1501070751855,12.495505190692));
#418578=CARTESIAN_POINT('Ctrl Pts',(1.71206232042154,2.15205796274268,12.4937456938368));
#418579=CARTESIAN_POINT('Ctrl Pts',(1.70948047842012,2.15410689008242,12.4925987732155));
#418580=CARTESIAN_POINT('Ctrl Pts',(1.70689924055976,2.15615533798106,12.4914521209692));
#418581=CARTESIAN_POINT('Ctrl Pts',(1.70412017663384,2.15835275217767,12.4908873016276));
#418582=CARTESIAN_POINT('Ctrl Pts',(1.70137838705821,2.16051188009953,12.4908873016278));
#418583=CARTESIAN_POINT('',(1.72884384250458,2.13859743014762,13.7435492065112));
#418584=CARTESIAN_POINT('',(1.72884384250458,2.13859743014762,14.));
#418585=CARTESIAN_POINT('',(1.78701907901789,2.09023032492261,13.7435492065112));
#418586=CARTESIAN_POINT('Origin',(0.,2.5406128344257E-15,13.7435492065112));
#418587=CARTESIAN_POINT('',(1.78701907901789,2.09023032492261,12.5369868989719));
#418588=CARTESIAN_POINT('',(1.78701907901789,2.09023032492261,14.));
#418589=CARTESIAN_POINT('Ctrl Pts',(1.81357957369649,2.06722740158669,12.4908873016278));
#418590=CARTESIAN_POINT('Ctrl Pts',(1.81193982892409,2.06866595044833,12.4908873016278));
#418591=CARTESIAN_POINT('Ctrl Pts',(1.81028909344554,2.07011061546466,12.4911020829134));
#418592=CARTESIAN_POINT('Ctrl Pts',(1.80868015946465,2.071515406836,12.4915448903141));
#418593=CARTESIAN_POINT('Ctrl Pts',(1.8059274694857,2.07391883368654,12.4923024798169));
#418594=CARTESIAN_POINT('Ctrl Pts',(1.80323374999077,2.07626054390928,12.4937722312795));
#418595=CARTESIAN_POINT('Ctrl Pts',(1.80086748172618,2.07831092795597,12.4958030942394));
#418596=CARTESIAN_POINT('Ctrl Pts',(1.79851791538149,2.08034683970017,12.4978196226833));
#418597=CARTESIAN_POINT('Ctrl Pts',(1.7964217506442,2.08215612104013,12.5004326847668));
#418598=CARTESIAN_POINT('Ctrl Pts',(1.79469086928142,2.08364696715108,12.5033504258767));
#418599=CARTESIAN_POINT('Ctrl Pts',(1.79262277179027,2.08542826491537,12.5068366111226));
#418600=CARTESIAN_POINT('Ctrl Pts',(1.79100978711635,2.08681248440791,12.5108395010833));
#418601=CARTESIAN_POINT('Ctrl Pts',(1.78983298392499,2.08782132608473,12.5149868989719));
#418602=CARTESIAN_POINT('Ctrl Pts',(1.78785643076781,2.08951577186464,12.5219528491417));
#418603=CARTESIAN_POINT('Ctrl Pts',(1.7870190789888,2.09023032494785,12.5295503425868));
#418604=CARTESIAN_POINT('Ctrl Pts',(1.78701907901789,2.09023032492261,12.5369868989719));
#418605=CARTESIAN_POINT('',(1.89740680156515,1.99056460065338,12.5369868989719));
#418606=CARTESIAN_POINT('Ctrl Pts',(1.89740680156515,1.99056460065337,12.5369868989719));
#418607=CARTESIAN_POINT('Ctrl Pts',(1.89740680156515,1.99056460065338,12.5309445149785));
#418608=CARTESIAN_POINT('Ctrl Pts',(1.8968831374682,1.99106431522373,12.5248274368704));
#418609=CARTESIAN_POINT('Ctrl Pts',(1.89568297880746,1.99220632562485,12.5190199595513));
#418610=CARTESIAN_POINT('Ctrl Pts',(1.89467492083654,1.99316554270621,12.5141420429941));
#418611=CARTESIAN_POINT('Ctrl Pts',(1.89315846088574,1.99460757456179,12.5093757677094));
#418612=CARTESIAN_POINT('Ctrl Pts',(1.89106243243336,1.9965928169357,12.5051960112707));
#418613=CARTESIAN_POINT('Ctrl Pts',(1.88966214092542,1.99791909570554,12.5024036458141));
#418614=CARTESIAN_POINT('Ctrl Pts',(1.88796911166866,1.9995198546716,12.4998248032393));
#418615=CARTESIAN_POINT('Ctrl Pts',(1.88604146568939,2.0013364508998,12.4976950015772));
#418616=CARTESIAN_POINT('Ctrl Pts',(1.88405950641913,2.00320423148479,12.495505190692));
#418617=CARTESIAN_POINT('Ctrl Pts',(1.88177827698045,2.00534819427845,12.4937456938368));
#418618=CARTESIAN_POINT('Ctrl Pts',(1.8793720324448,2.00760074807326,12.4925987732155));
#418619=CARTESIAN_POINT('Ctrl Pts',(1.87696635096109,2.00985277477916,12.4914521209692));
#418620=CARTESIAN_POINT('Ctrl Pts',(1.87437564379794,2.01226939677085,12.4908873016276));
#418621=CARTESIAN_POINT('Ctrl Pts',(1.87181896627095,2.01464482167661,12.4908873016278));
#418622=CARTESIAN_POINT('',(1.89740680156514,1.99056460065337,13.7435492065112));
#418623=CARTESIAN_POINT('',(1.89740680156515,1.99056460065338,14.));
#418624=CARTESIAN_POINT('',(1.95144609668394,1.93761661113261,13.7435492065112));
#418625=CARTESIAN_POINT('Origin',(0.,2.5406128344257E-15,13.7435492065112));
#418626=CARTESIAN_POINT('',(1.95144609668394,1.93761661113261,12.5369868989719));
#418627=CARTESIAN_POINT('',(1.95144609668394,1.93761661113261,14.));
#418628=CARTESIAN_POINT('Ctrl Pts',(1.97604326170699,1.91252530123458,12.4908873016278));
#418629=CARTESIAN_POINT('Ctrl Pts',(1.97452622813711,1.91409271786515,12.4908873016278));
#418630=CARTESIAN_POINT('Ctrl Pts',(1.97299873895513,1.915667126144,12.4911020829134));
#418631=CARTESIAN_POINT('Ctrl Pts',(1.97150966210755,1.917198386244,12.4915448903141));
#418632=CARTESIAN_POINT('Ctrl Pts',(1.96896203307807,1.91981818567797,12.4923024798169));
#418633=CARTESIAN_POINT('Ctrl Pts',(1.96646814783507,1.92237166719923,12.4937722312795));
#418634=CARTESIAN_POINT('Ctrl Pts',(1.96427687846757,1.92460810159307,12.4958030942394));
#418635=CARTESIAN_POINT('Ctrl Pts',(1.9621010758187,1.9268287504783,12.4978196226833));
#418636=CARTESIAN_POINT('Ctrl Pts',(1.9601593591224,1.92880286846979,12.5004326847668));
#418637=CARTESIAN_POINT('Ctrl Pts',(1.95855575492296,1.93042983681308,12.5033504258767));
#418638=CARTESIAN_POINT('Ctrl Pts',(1.95663973116016,1.93237377660081,12.5068366111226));
#418639=CARTESIAN_POINT('Ctrl Pts',(1.95514494029879,1.93388486344232,12.5108395010833));
#418640=CARTESIAN_POINT('Ctrl Pts',(1.95405428278525,1.93498626866669,12.5149868989719));
#418641=CARTESIAN_POINT('Ctrl Pts',(1.95222241950718,1.93683618374979,12.5219528491417));
#418642=CARTESIAN_POINT('Ctrl Pts',(1.95144609665701,1.93761661116014,12.5295503425868));
#418643=CARTESIAN_POINT('Ctrl Pts',(1.95144609668394,1.93761661113261,12.5369868989719));
#418644=CARTESIAN_POINT('',(2.05334283141139,1.82928489216182,12.5369868989719));
#418645=CARTESIAN_POINT('Ctrl Pts',(2.05334283141138,1.82928489216182,12.5369868989719));
#418646=CARTESIAN_POINT('Ctrl Pts',(2.05334283141138,1.82928489216182,12.5309445149785));
#418647=CARTESIAN_POINT('Ctrl Pts',(2.05286164114013,1.82982562745853,12.5248274368704));
#418648=CARTESIAN_POINT('Ctrl Pts',(2.05175856035793,1.83106166198683,12.5190199595513));
#418649=CARTESIAN_POINT('Ctrl Pts',(2.05083204171381,1.83209985343546,12.5141420429941));
#418650=CARTESIAN_POINT('Ctrl Pts',(2.0494381666418,1.83366069261312,12.5093757677094));
#418651=CARTESIAN_POINT('Ctrl Pts',(2.04751092823475,1.83581017503425,12.5051960112707));
#418652=CARTESIAN_POINT('Ctrl Pts',(2.0462234001136,1.83724617747846,12.5024036458141));
#418653=CARTESIAN_POINT('Ctrl Pts',(2.04466648098848,1.83897960765286,12.4998248032393));
#418654=CARTESIAN_POINT('Ctrl Pts',(2.04289331854924,1.84094728034967,12.4976950015772));
#418655=CARTESIAN_POINT('Ctrl Pts',(2.04107019554226,1.84297039412899,12.495505190692));
#418656=CARTESIAN_POINT('Ctrl Pts',(2.03897130957761,1.84529316444047,12.4937456938368));
#418657=CARTESIAN_POINT('Ctrl Pts',(2.03675667566812,1.84773435431649,12.4925987732155));
#418658=CARTESIAN_POINT('Ctrl Pts',(2.03454255997442,1.85017497296348,12.4914521209692));
#418659=CARTESIAN_POINT('Ctrl Pts',(2.03215745030278,1.8527947205296,12.4908873016276));
#418660=CARTESIAN_POINT('Ctrl Pts',(2.02980289909154,1.85537063435843,12.4908873016278));
#418661=CARTESIAN_POINT('',(2.05334283141138,1.82928489216182,13.7435492065112));
#418662=CARTESIAN_POINT('',(2.05334283141138,1.82928489216182,14.));
#418663=CARTESIAN_POINT('',(2.1028865625425,1.77210837847977,13.7435492065112));
#418664=CARTESIAN_POINT('Origin',(0.,2.5406128344257E-15,13.7435492065112));
#418665=CARTESIAN_POINT('',(2.1028865625425,1.77210837847977,12.5369868989719));
#418666=CARTESIAN_POINT('',(2.1028865625425,1.77210837847977,14.));
#418667=CARTESIAN_POINT('Ctrl Pts',(2.12535670783502,1.74509566054721,12.4908873016278));
#418668=CARTESIAN_POINT('Ctrl Pts',(2.12397248107577,1.74678151404765,12.4908873016278));
#418669=CARTESIAN_POINT('Ctrl Pts',(2.12257840337886,1.74847518816168,12.4911020829134));
#418670=CARTESIAN_POINT('Ctrl Pts',(2.12121909322532,1.75012272670701,12.4915448903141));
#418671=CARTESIAN_POINT('Ctrl Pts',(2.11889347919617,1.75294146439141,12.4923024798169));
#418672=CARTESIAN_POINT('Ctrl Pts',(2.11661602459994,1.75568972421297,12.4937722312795));
#418673=CARTESIAN_POINT('Ctrl Pts',(2.11461433666563,1.75809732585206,12.4958030942394));
#418674=CARTESIAN_POINT('Ctrl Pts',(2.11262677732022,1.76048793382636,12.4978196226833));
#418675=CARTESIAN_POINT('Ctrl Pts',(2.11085243046918,1.76261375103985,12.5004326847668));
#418676=CARTESIAN_POINT('Ctrl Pts',(2.10938677515444,1.76436601440959,12.5033504258767));
#418677=CARTESIAN_POINT('Ctrl Pts',(2.107635575942,1.7664596596222,12.5068366111226));
#418678=CARTESIAN_POINT('Ctrl Pts',(2.10626892647974,1.76808755777907,12.5108395010833));
#418679=CARTESIAN_POINT('Ctrl Pts',(2.10527167278984,1.76927419688094,12.5149868989719));
#418680=CARTESIAN_POINT('Ctrl Pts',(2.10359669013875,1.77126727038755,12.5219528491417));
#418681=CARTESIAN_POINT('Ctrl Pts',(2.1028865625179,1.7721083785094,12.5295503425868));
#418682=CARTESIAN_POINT('Ctrl Pts',(2.1028865625425,1.77210837847977,12.5369868989719));
#418683=CARTESIAN_POINT('',(2.1956142034923,1.65583159452369,12.5369868989719));
#418684=CARTESIAN_POINT('Ctrl Pts',(2.1956142034923,1.65583159452369,12.5369868989719));
#418685=CARTESIAN_POINT('Ctrl Pts',(2.1956142034923,1.6558315945237,12.5309445149785));
#418686=CARTESIAN_POINT('Ctrl Pts',(2.1951786892886,1.65640975204257,12.5248274368704));
#418687=CARTESIAN_POINT('Ctrl Pts',(2.19418002720554,1.6577315850922,12.5190199595513));
#418688=CARTESIAN_POINT('Ctrl Pts',(2.19334121371695,1.6588418419153,12.5141420429941));
#418689=CARTESIAN_POINT('Ctrl Pts',(2.19207919953236,1.66051110128783,12.5093757677094));
#418690=CARTESIAN_POINT('Ctrl Pts',(2.19033357662426,1.6628105193053,12.5051960112707));
#418691=CARTESIAN_POINT('Ctrl Pts',(2.18916738017712,1.66434668906455,12.5024036458141));
#418692=CARTESIAN_POINT('Ctrl Pts',(2.18775693222355,1.66620125475547,12.4998248032393));
#418693=CARTESIAN_POINT('Ctrl Pts',(2.18615005342782,1.66830690938374,12.4976950015772));
#418694=CARTESIAN_POINT('Ctrl Pts',(2.18449789926693,1.67047189286897,12.495505190692));
#418695=CARTESIAN_POINT('Ctrl Pts',(2.18259532451612,1.67295801304508,12.4937456938368));
#418696=CARTESIAN_POINT('Ctrl Pts',(2.18058703925606,1.67557159328645,12.4925987732155));
#418697=CARTESIAN_POINT('Ctrl Pts',(2.17857922392701,1.67818456196012,12.4914521209692));
#418698=CARTESIAN_POINT('Ctrl Pts',(2.17641558425824,1.68099000111283,12.4908873016276));
#418699=CARTESIAN_POINT('Ctrl Pts',(2.17427882851258,1.6837492615832,12.4908873016278));
#418700=CARTESIAN_POINT('',(2.1956142034923,1.65583159452369,13.7435492065112));
#418701=CARTESIAN_POINT('',(2.1956142034923,1.6558315945237,14.));
#418702=CARTESIAN_POINT('',(2.2403326652792,1.59480705694544,13.7435492065112));
#418703=CARTESIAN_POINT('Origin',(0.,2.5406128344257E-15,13.7435492065112));
#418704=CARTESIAN_POINT('',(2.24033266527921,1.59480705694544,12.5369868989719));
#418705=CARTESIAN_POINT('',(2.24033266527921,1.59480705694544,14.));
#418706=CARTESIAN_POINT('Ctrl Pts',(2.26052625573157,1.56605269615942,12.4908873016278));
#418707=CARTESIAN_POINT('Ctrl Pts',(2.25928404758366,1.56784576745282,12.4908873016278));
#418708=CARTESIAN_POINT('Ctrl Pts',(2.25803265872888,1.56964743628024,12.4911020829134));
#418709=CARTESIAN_POINT('Ctrl Pts',(2.25681216125419,1.5714002891737,12.4915448903141));
#418710=CARTESIAN_POINT('Ctrl Pts',(2.25472403880304,1.57439920687432,12.4923024798169));
#418711=CARTESIAN_POINT('Ctrl Pts',(2.25267817093815,1.57732395578048,12.4937722312795));
#418712=CARTESIAN_POINT('Ctrl Pts',(2.25087938533999,1.57988670247315,12.4958030942394));
#418713=CARTESIAN_POINT('Ctrl Pts',(2.24909329617757,1.58243136043487,12.4978196226833));
#418714=CARTESIAN_POINT('Ctrl Pts',(2.24749812715732,1.58469472990755,12.5004326847668));
#418715=CARTESIAN_POINT('Ctrl Pts',(2.24618017442159,1.5865606272801,12.5033504258767));
#418716=CARTESIAN_POINT('Ctrl Pts',(2.24460545370135,1.58879004505414,12.5068366111226));
#418717=CARTESIAN_POINT('Ctrl Pts',(2.24337604046489,1.59052392113271,12.5108395010833));
#418718=CARTESIAN_POINT('Ctrl Pts',(2.24247882715739,1.59178789722463,12.5149868989719));
#418719=CARTESIAN_POINT('Ctrl Pts',(2.24097187186648,1.59391086557942,12.5219528491417));
#418720=CARTESIAN_POINT('Ctrl Pts',(2.2403326652571,1.59480705697698,12.5295503425868));
#418721=CARTESIAN_POINT('Ctrl Pts',(2.24033266527921,1.59480705694544,12.5369868989719));
#418722=CARTESIAN_POINT('',(2.32327412529982,1.47135901081699,12.5369868989719));
#418723=CARTESIAN_POINT('Ctrl Pts',(2.32327412529982,1.47135901081699,12.5369868989719));
#418724=CARTESIAN_POINT('Ctrl Pts',(2.32327412529982,1.471359010817,12.5309445149785));
#418725=CARTESIAN_POINT('Ctrl Pts',(2.32288718543885,1.47197074301514,12.5248274368704));
#418726=CARTESIAN_POINT('Ctrl Pts',(2.32199958798633,1.47336957800523,12.5190199595513));
#418727=CARTESIAN_POINT('Ctrl Pts',(2.32125406181863,1.47454451162683,12.5141420429941));
#418728=CARTESIAN_POINT('Ctrl Pts',(2.32013230701764,1.47631108254852,12.5093757677094));
#418729=CARTESIAN_POINT('Ctrl Pts',(2.31857991644094,1.4787451339148,12.5051960112707));
#418730=CARTESIAN_POINT('Ctrl Pts',(2.31754281251276,1.48037124803278,12.5024036458141));
#418731=CARTESIAN_POINT('Ctrl Pts',(2.31628822202915,1.48233460741154,12.4998248032393));
#418732=CARTESIAN_POINT('Ctrl Pts',(2.31485832039021,1.48456423118712,12.4976950015772));
#418733=CARTESIAN_POINT('Ctrl Pts',(2.31338812988877,1.48685667677036,12.495505190692));
#418734=CARTESIAN_POINT('Ctrl Pts',(2.31169452767286,1.48948960209151,12.4937456938368));
#418735=CARTESIAN_POINT('Ctrl Pts',(2.3099059558693,1.49225817975294,12.4925987732155));
#418736=CARTESIAN_POINT('Ctrl Pts',(2.30811780258464,1.49502610957787,12.4914521209692));
#418737=CARTESIAN_POINT('Ctrl Pts',(2.30619003158375,1.49799857058249,12.4908873016276));
#418738=CARTESIAN_POINT('Ctrl Pts',(2.30428529106062,1.50092281527121,12.4908873016278));
#418739=CARTESIAN_POINT('',(2.32327412529982,1.471359010817,13.7435492065112));
#418740=CARTESIAN_POINT('',(2.32327412529982,1.471359010817,14.));
#418741=CARTESIAN_POINT('',(2.36286972375735,1.40689255757178,13.7435492065112));
#418742=CARTESIAN_POINT('Origin',(0.,2.5406128344257E-15,13.7435492065112));
#418743=CARTESIAN_POINT('',(2.36286972375735,1.40689255757179,12.5369868989719));
#418744=CARTESIAN_POINT('',(2.36286972375735,1.40689255757179,14.));
#418745=CARTESIAN_POINT('Ctrl Pts',(2.38065237435682,1.3765879094592,12.4908873016278));
#418746=CARTESIAN_POINT('Ctrl Pts',(2.37956045151052,1.37847626595194,12.4908873016278));
#418747=CARTESIAN_POINT('Ctrl Pts',(2.37846007928423,1.38037393968396,12.4911020829134));
#418748=CARTESIAN_POINT('Ctrl Pts',(2.37738651669771,1.38222044197875,12.4915448903141));
#418749=CARTESIAN_POINT('Ctrl Pts',(2.37554978193495,1.38537958239306,12.4923024798169));
#418750=CARTESIAN_POINT('Ctrl Pts',(2.37374911571451,1.38846135666241,12.4937722312795));
#418751=CARTESIAN_POINT('Ctrl Pts',(2.37216520307387,1.39116219375223,12.4958030942394));
#418752=CARTESIAN_POINT('Ctrl Pts',(2.37059247022313,1.39384396742249,12.4978196226833));
#418753=CARTESIAN_POINT('Ctrl Pts',(2.36918709462032,1.39622982680393,12.5004326847668));
#418754=CARTESIAN_POINT('Ctrl Pts',(2.3680256152216,1.39819694094014,12.5033504258767));
#418755=CARTESIAN_POINT('Ctrl Pts',(2.36663785250014,1.40054729486815,12.5068366111226));
#418756=CARTESIAN_POINT('Ctrl Pts',(2.36555385703173,1.40237561020919,12.5108395010833));
#418757=CARTESIAN_POINT('Ctrl Pts',(2.36476265491317,1.40370851173882,12.5149868989719));
#418758=CARTESIAN_POINT('Ctrl Pts',(2.36343375552127,1.40594724693764,12.5219528491417));
#418759=CARTESIAN_POINT('Ctrl Pts',(2.36286972373789,1.40689255760502,12.5295503425868));
#418760=CARTESIAN_POINT('Ctrl Pts',(2.36286972375735,1.40689255757179,12.5369868989719));
#418761=CARTESIAN_POINT('',(2.43547304111672,1.27709477565046,12.5369868989719));
#418762=CARTESIAN_POINT('Ctrl Pts',(2.43547304111672,1.27709477565046,12.5369868989719));
#418763=CARTESIAN_POINT('Ctrl Pts',(2.43547304111672,1.27709477565046,12.5309445149785));
#418764=CARTESIAN_POINT('Ctrl Pts',(2.43513725061941,1.27773601155102,12.5248274368704));
#418765=CARTESIAN_POINT('Ctrl Pts',(2.43436662461203,1.27920253946551,12.5190199595513));
#418766=CARTESIAN_POINT('Ctrl Pts',(2.43371934711886,1.2804343308962,12.5141420429941));
#418767=CARTESIAN_POINT('Ctrl Pts',(2.4327453167946,1.28228645712903,12.5093757677094));
#418768=CARTESIAN_POINT('Ctrl Pts',(2.43139648945247,1.28483894363388,12.5051960112707));
#418769=CARTESIAN_POINT('Ctrl Pts',(2.43049537979877,1.28654418058943,12.5024036458141));
#418770=CARTESIAN_POINT('Ctrl Pts',(2.42940499587781,1.28860326782327,12.4998248032393));
#418771=CARTESIAN_POINT('Ctrl Pts',(2.42816158715514,1.29094202296781,12.4976950015772));
#418772=CARTESIAN_POINT('Ctrl Pts',(2.42688314418837,1.29334667480194,12.495505190692));
#418773=CARTESIAN_POINT('Ctrl Pts',(2.42540978515068,1.29610888358451,12.4937456938368));
#418774=CARTESIAN_POINT('Ctrl Pts',(2.42385282945388,1.29901403423845,12.4925987732155));
#418775=CARTESIAN_POINT('Ctrl Pts',(2.4222962380787,1.30191850509833,12.4914521209692));
#418776=CARTESIAN_POINT('Ctrl Pts',(2.42061716474365,1.30503820671729,12.4908873016276));
#418777=CARTESIAN_POINT('Ctrl Pts',(2.41895711517697,1.30810797525842,12.4908873016278));
#418778=CARTESIAN_POINT('',(2.43547304111672,1.27709477565046,13.7435492065112));
#418779=CARTESIAN_POINT('',(2.43547304111672,1.27709477565046,14.));
#418780=CARTESIAN_POINT('',(2.46968227406995,1.20961542034842,13.7435492065112));
#418781=CARTESIAN_POINT('Origin',(0.,2.5406128344257E-15,13.7435492065112));
#418782=CARTESIAN_POINT('',(2.46968227406995,1.20961542034842,12.5369868989719));
#418783=CARTESIAN_POINT('',(2.46968227406995,1.20961542034842,14.));
#418784=CARTESIAN_POINT('Ctrl Pts',(2.48493564421071,1.17796215734254,12.4908873016278));
#418785=CARTESIAN_POINT('Ctrl Pts',(2.48400127323241,1.17993323233373,12.4908873016278));
#418786=CARTESIAN_POINT('Ctrl Pts',(2.48305924043024,1.18191428226474,12.4911020829134));
#418787=CARTESIAN_POINT('Ctrl Pts',(2.48213975711378,1.18384214579275,12.4915448903141));
#418788=CARTESIAN_POINT('Ctrl Pts',(2.48056663320621,1.18714048536252,12.4923024798169));
#418789=CARTESIAN_POINT('Ctrl Pts',(2.47902315176683,1.19035877629576,12.4937722312795));
#418790=CARTESIAN_POINT('Ctrl Pts',(2.477664652761,1.1931797301575,12.4958030942394));
#418791=CARTESIAN_POINT('Ctrl Pts',(2.47631574249958,1.19598077277497,12.4978196226833));
#418792=CARTESIAN_POINT('Ctrl Pts',(2.47510951285698,1.19847324456464,12.5004326847668));
#418793=CARTESIAN_POINT('Ctrl Pts',(2.47411223624904,1.20052848464449,12.5033504258767));
#418794=CARTESIAN_POINT('Ctrl Pts',(2.47292066685831,1.20298413350885,12.5068366111226));
#418795=CARTESIAN_POINT('Ctrl Pts',(2.47198930296894,1.20489472097542,12.5108395010833));
#418796=CARTESIAN_POINT('Ctrl Pts',(2.47130937735888,1.20628767770299,12.5149868989719));
#418797=CARTESIAN_POINT('Ctrl Pts',(2.47016737747219,1.20862728133245,12.5219528491417));
#418798=CARTESIAN_POINT('Ctrl Pts',(2.46968227405327,1.20961542038314,12.5295503425868));
#418799=CARTESIAN_POINT('Ctrl Pts',(2.46968227406995,1.20961542034842,12.5369868989719));
#418800=CARTESIAN_POINT('',(2.53146428566975,1.07433168545777,12.5369868989719));
#418801=CARTESIAN_POINT('Ctrl Pts',(2.53146428566975,1.07433168545777,12.5369868989719));
#418802=CARTESIAN_POINT('Ctrl Pts',(2.53146428566975,1.07433168545777,12.5309445149785));
#418803=CARTESIAN_POINT('Ctrl Pts',(2.53118187916646,1.07499815774164,12.5248274368704));
#418804=CARTESIAN_POINT('Ctrl Pts',(2.53053335299317,1.07652261907921,12.5190199595513));
#418805=CARTESIAN_POINT('Ctrl Pts',(2.52998863169945,1.07780307095026,12.5141420429941));
#418806=CARTESIAN_POINT('Ctrl Pts',(2.52916880786301,1.07972842689972,12.5093757677094));
#418807=CARTESIAN_POINT('Ctrl Pts',(2.52803251997887,1.08238236216657,12.5051960112707));
#418808=CARTESIAN_POINT('Ctrl Pts',(2.52727340133573,1.08415537388909,12.5024036458141));
#418809=CARTESIAN_POINT('Ctrl Pts',(2.52635448030251,1.08629648609222,12.4998248032393));
#418810=CARTESIAN_POINT('Ctrl Pts',(2.52530583917602,1.08872880857609,12.4976950015772));
#418811=CARTESIAN_POINT('Ctrl Pts',(2.52422765157093,1.09122966409989,12.495505190692));
#418812=CARTESIAN_POINT('Ctrl Pts',(2.52298434067277,1.09410277430017,12.4937456938368));
#418813=CARTESIAN_POINT('Ctrl Pts',(2.52166936236601,1.09712516464832,12.4925987732155));
#418814=CARTESIAN_POINT('Ctrl Pts',(2.5203546917591,1.10014684776879,12.4914521209692));
#418815=CARTESIAN_POINT('Ctrl Pts',(2.51893549004589,1.10339302890254,12.4908873016276));
#418816=CARTESIAN_POINT('Ctrl Pts',(2.51753117879165,1.10658789249292,12.4908873016278));
#418817=CARTESIAN_POINT('',(2.53146428566975,1.07433168545777,13.7435492065112));
#418818=CARTESIAN_POINT('',(2.53146428566975,1.07433168545777,14.));
#418819=CARTESIAN_POINT('',(2.56005949631751,1.00428849207514,13.7435492065112));
#418820=CARTESIAN_POINT('Origin',(0.,2.5406128344257E-15,13.7435492065112));
#418821=CARTESIAN_POINT('',(2.56005949631751,1.00428849207514,12.5369868989719));
#418822=CARTESIAN_POINT('',(2.56005949631751,1.00428849207514,14.));
#418823=CARTESIAN_POINT('Ctrl Pts',(2.57268207733791,0.971497261418848,
12.4908873016278));
#418824=CARTESIAN_POINT('Ctrl Pts',(2.5719114763123,0.973537937729611,12.4908873016278));
#418825=CARTESIAN_POINT('Ctrl Pts',(2.57113405200711,0.975589180299189,
12.4911020829134));
#418826=CARTESIAN_POINT('Ctrl Pts',(2.57037476697048,0.977585575446697,
12.4915448903141));
#418827=CARTESIAN_POINT('Ctrl Pts',(2.56907572279817,0.98100116426628,12.4923024798169));
#418828=CARTESIAN_POINT('Ctrl Pts',(2.56779969775416,0.984334554668221,
12.4937722312795));
#418829=CARTESIAN_POINT('Ctrl Pts',(2.5666756529699,0.987256852319363,12.4958030942394));
#418830=CARTESIAN_POINT('Ctrl Pts',(2.56555954207303,0.99015852340758,12.4978196226833));
#418831=CARTESIAN_POINT('Ctrl Pts',(2.5645604856499,0.992741020616945,12.5004326847668));
#418832=CARTESIAN_POINT('Ctrl Pts',(2.56373404854403,0.99487070935678,12.5033504258767));
#418833=CARTESIAN_POINT('Ctrl Pts',(2.56274660218172,0.997415311219456,
12.5068366111226));
#418834=CARTESIAN_POINT('Ctrl Pts',(2.56197406794442,0.999395456167186,
12.5108395010833));
#418835=CARTESIAN_POINT('Ctrl Pts',(2.56140994363562,1.0008391981955,12.5149868989719));
#418836=CARTESIAN_POINT('Ctrl Pts',(2.56046244307496,1.00326410057947,12.5219528491417));
#418837=CARTESIAN_POINT('Ctrl Pts',(2.56005949630371,1.0042884921111,12.5295503425868));
#418838=CARTESIAN_POINT('Ctrl Pts',(2.56005949631751,1.00428849207514,12.5369868989719));
#418839=CARTESIAN_POINT('',(2.61060905306386,0.864419095150618,12.5369868989719));
#418840=CARTESIAN_POINT('Ctrl Pts',(2.61060905306386,0.864419095150617,
12.5369868989719));
#418841=CARTESIAN_POINT('Ctrl Pts',(2.61060905306386,0.864419095150619,
12.5309445149785));
#418842=CARTESIAN_POINT('Ctrl Pts',(2.61038190992327,0.865106368554689,
12.5248274368704));
#418843=CARTESIAN_POINT('Ctrl Pts',(2.60985979941874,0.866678618276671,
12.5190199595513));
#418844=CARTESIAN_POINT('Ctrl Pts',(2.60942125935482,0.86799920939213,12.5141420429941));
#418845=CARTESIAN_POINT('Ctrl Pts',(2.60876109779858,0.869984982132039,
12.5093757677094));
#418846=CARTESIAN_POINT('Ctrl Pts',(2.60784491118082,0.872722704659571,
12.5051960112707));
#418847=CARTESIAN_POINT('Ctrl Pts',(2.60723283535757,0.874551692048575,
12.5024036458141));
#418848=CARTESIAN_POINT('Ctrl Pts',(2.60649149247995,0.876760580472532,
12.4998248032393));
#418849=CARTESIAN_POINT('Ctrl Pts',(2.60564459748331,0.879270283590905,
12.4976950015772));
#418850=CARTESIAN_POINT('Ctrl Pts',(2.60477384040054,0.881850700023472,
12.495505190692));
#418851=CARTESIAN_POINT('Ctrl Pts',(2.6037688516708,0.884815591567119,12.4937456938368));
#418852=CARTESIAN_POINT('Ctrl Pts',(2.60270460171775,0.88793510810038,12.4925987732155));
#418853=CARTESIAN_POINT('Ctrl Pts',(2.60164060079509,0.891053894678799,
12.4914521209692));
#418854=CARTESIAN_POINT('Ctrl Pts',(2.60049071525699,0.894404952527469,
12.4908873016276));
#418855=CARTESIAN_POINT('Ctrl Pts',(2.59935148777488,0.897703649877021,
12.4908873016278));
#418856=CARTESIAN_POINT('',(2.61060905306386,0.864419095150619,13.7435492065112));
#418857=CARTESIAN_POINT('',(2.61060905306386,0.864419095150619,14.));
#418858=CARTESIAN_POINT('',(2.63339994499716,0.792278189583031,13.7435492065112));
#418859=CARTESIAN_POINT('Origin',(0.,2.5406128344257E-15,13.7435492065112));
#418860=CARTESIAN_POINT('',(2.63339994499716,0.792278189583032,12.5369868989719));
#418861=CARTESIAN_POINT('',(2.63339994499716,0.792278189583032,14.));
#418862=CARTESIAN_POINT('Ctrl Pts',(2.64330773570308,0.758567211506177,
12.4908873016278));
#418863=CARTESIAN_POINT('Ctrl Pts',(2.64270603285286,0.760663908772356,
12.4908873016278));
#418864=CARTESIAN_POINT('Ctrl Pts',(2.64209839067514,0.762771693299628,
12.4911020829134));
#418865=CARTESIAN_POINT('Ctrl Pts',(2.64150435683498,0.764823334386318,
12.4915448903141));
#418866=CARTESIAN_POINT('Ctrl Pts',(2.64048803732257,0.76833344227565,12.4923024798169));
#418867=CARTESIAN_POINT('Ctrl Pts',(2.63948796041007,0.77175974898314,12.4937722312795));
#418868=CARTESIAN_POINT('Ctrl Pts',(2.63860585017996,0.774763943014961,
12.4958030942394));
#418869=CARTESIAN_POINT('Ctrl Pts',(2.63772996618152,0.777746932431566,
12.4978196226833));
#418870=CARTESIAN_POINT('Ctrl Pts',(2.63694473153352,0.78040226896778,12.5004326847668));
#418871=CARTESIAN_POINT('Ctrl Pts',(2.6362946337323,0.782592233640416,12.5033504258767));
#418872=CARTESIAN_POINT('Ctrl Pts',(2.63551788169105,0.785208854595842,
12.5068366111226));
#418873=CARTESIAN_POINT('Ctrl Pts',(2.6349093181937,0.787245379486807,12.5108395010833));
#418874=CARTESIAN_POINT('Ctrl Pts',(2.63446474934035,0.788730298950861,
12.5149868989719));
#418875=CARTESIAN_POINT('Ctrl Pts',(2.63371805356563,0.791224362764048,
12.5219528491417));
#418876=CARTESIAN_POINT('Ctrl Pts',(2.63339994498634,0.792278189619995,
12.5295503425868));
#418877=CARTESIAN_POINT('Ctrl Pts',(2.63339994499716,0.792278189583032,
12.5369868989719));
#418878=CARTESIAN_POINT('',(2.67238064793001,0.648753938384347,12.5369868989719));
#418879=CARTESIAN_POINT('Ctrl Pts',(2.67238064793001,0.648753938384347,
12.5369868989719));
#418880=CARTESIAN_POINT('Ctrl Pts',(2.67238064793001,0.648753938384349,
12.5309445149785));
#418881=CARTESIAN_POINT('Ctrl Pts',(2.67221027975225,0.649457439217514,
12.5248274368704));
#418882=CARTESIAN_POINT('Ctrl Pts',(2.67181805947575,0.651067014261405,
12.5190199595513));
#418883=CARTESIAN_POINT('Ctrl Pts',(2.67148861905339,0.652418956305285,
12.5141420429941));
#418884=CARTESIAN_POINT('Ctrl Pts',(2.67099251304359,0.654451930845692,
12.5093757677094));
#418885=CARTESIAN_POINT('Ctrl Pts',(2.67030252476298,0.657255221542169,
12.5051960112707));
#418886=CARTESIAN_POINT('Ctrl Pts',(2.66984156502323,0.659128012988347,
12.5024036458141));
#418887=CARTESIAN_POINT('Ctrl Pts',(2.66928273381576,0.66138997784511,12.4998248032393));
#418888=CARTESIAN_POINT('Ctrl Pts',(2.66864322089545,0.663960359937809,
12.4976950015772));
#418889=CARTESIAN_POINT('Ctrl Pts',(2.66798568907971,0.666603165033526,
12.495505190692));
#418890=CARTESIAN_POINT('Ctrl Pts',(2.66722571055259,0.669640107056481,
12.4937456938368));
#418891=CARTESIAN_POINT('Ctrl Pts',(2.6664192713611,0.672835989907007,12.4925987732155));
#418892=CARTESIAN_POINT('Ctrl Pts',(2.66561302087327,0.676031124933269,
12.4914521209692));
#418893=CARTESIAN_POINT('Ctrl Pts',(2.66474010380881,0.679464758759762,
12.4908873016276));
#418894=CARTESIAN_POINT('Ctrl Pts',(2.66387354146977,0.682845337581871,
12.4908873016278));
#418895=CARTESIAN_POINT('',(2.67238064793001,0.648753938384349,13.7435492065112));
#418896=CARTESIAN_POINT('',(2.67238064793001,0.648753938384349,14.));
#418897=CARTESIAN_POINT('',(2.68921555152326,0.57499540645595,13.7435492065112));
#418898=CARTESIAN_POINT('Origin',(0.,2.5406128344257E-15,13.7435492065112));
#418899=CARTESIAN_POINT('',(2.68921555152326,0.57499540645595,12.5369868989719));
#418900=CARTESIAN_POINT('',(2.68921555152326,0.57499540645595,14.));
#418901=CARTESIAN_POINT('Ctrl Pts',(2.69634261720223,0.540589021955712,
12.4908873016278));
#418902=CARTESIAN_POINT('Ctrl Pts',(2.69591381676059,0.542727787002933,
12.4908873016278));
#418903=CARTESIAN_POINT('Ctrl Pts',(2.69548000046878,0.544878086529629,
12.4911020829134));
#418904=CARTESIAN_POINT('Ctrl Pts',(2.69505517102229,0.546971320222566,
12.4915448903141));
#418905=CARTESIAN_POINT('Ctrl Pts',(2.69432833960845,0.550552587992772,
12.4923024798169));
#418906=CARTESIAN_POINT('Ctrl Pts',(2.69361086617432,0.554049009499973,
12.4937722312795));
#418907=CARTESIAN_POINT('Ctrl Pts',(2.6929765607964,0.557115107496846,12.4958030942394));
#418908=CARTESIAN_POINT('Ctrl Pts',(2.69234673255987,0.560159563939431,
12.4978196226833));
#418909=CARTESIAN_POINT('Ctrl Pts',(2.69178054529403,0.562870068975945,
12.5004326847668));
#418910=CARTESIAN_POINT('Ctrl Pts',(2.69131111309108,0.565105735727806,
12.5033504258767));
#418911=CARTESIAN_POINT('Ctrl Pts',(2.69075022452756,0.567776962595234,
12.5068366111226));
#418912=CARTESIAN_POINT('Ctrl Pts',(2.69030968165983,0.569856314692288,
12.5108395010833));
#418913=CARTESIAN_POINT('Ctrl Pts',(2.68998762679431,0.571372529698046,
12.5149868989719));
#418914=CARTESIAN_POINT('Ctrl Pts',(2.68944670494271,0.573919157357266,
12.5219528491417));
#418915=CARTESIAN_POINT('Ctrl Pts',(2.68921555151549,0.574995406493672,
12.5295503425868));
#418916=CARTESIAN_POINT('Ctrl Pts',(2.68921555152326,0.57499540645595,12.5369868989719));
#418917=CARTESIAN_POINT('',(2.71636799049595,0.428771431194994,12.5369868989719));
#418918=CARTESIAN_POINT('Ctrl Pts',(2.71636799049595,0.428771431194994,
12.5369868989719));
#418919=CARTESIAN_POINT('Ctrl Pts',(2.71636799049595,0.428771431194996,
12.5309445149785));
#418920=CARTESIAN_POINT('Ctrl Pts',(2.71625553105313,0.429486477775282,
12.5248274368704));
#418921=CARTESIAN_POINT('Ctrl Pts',(2.71599581116589,0.431122666684725,
12.5190199595513));
#418922=CARTESIAN_POINT('Ctrl Pts',(2.71577766275676,0.432496962705779,
12.5141420429941));
#418923=CARTESIAN_POINT('Ctrl Pts',(2.71544891379703,0.434563609936534,
12.5093757677094));
#418924=CARTESIAN_POINT('Ctrl Pts',(2.71498971561175,0.437413813364882,
12.5051960112707));
#418925=CARTESIAN_POINT('Ctrl Pts',(2.71468293956652,0.439317945750148,
12.5024036458141));
#418926=CARTESIAN_POINT('Ctrl Pts',(2.71431033895867,0.441617934036794,
12.4998248032393));
#418927=CARTESIAN_POINT('Ctrl Pts',(2.71388246396767,0.444231889635074,
12.4976950015772));
#418928=CARTESIAN_POINT('Ctrl Pts',(2.71344253318471,0.446919495962061,
12.495505190692));
#418929=CARTESIAN_POINT('Ctrl Pts',(2.71293262239191,0.450008278116222,
12.4937456938368));
#418930=CARTESIAN_POINT('Ctrl Pts',(2.71238936068175,0.453259259210928,
12.4925987732155));
#418931=CARTESIAN_POINT('Ctrl Pts',(2.71184622609274,0.456509479588592,
12.4914521209692));
#418932=CARTESIAN_POINT('Ctrl Pts',(2.71125608662096,0.460002839126303,
12.4908873016276));
#418933=CARTESIAN_POINT('Ctrl Pts',(2.71066795625438,0.463442802226663,
12.4908873016278));
#418934=CARTESIAN_POINT('',(2.71636799049595,0.428771431194996,13.7435492065112));
#418935=CARTESIAN_POINT('',(2.71636799049595,0.428771431194996,14.));
#418936=CARTESIAN_POINT('',(2.72713487224331,0.353886123766466,13.7435492065112));
#418937=CARTESIAN_POINT('Origin',(0.,2.5406128344257E-15,13.7435492065112));
#418938=CARTESIAN_POINT('',(2.72713487224331,0.353886123766466,12.5369868989719));
#418939=CARTESIAN_POINT('',(2.72713487224331,0.353886123766466,14.));
#418940=CARTESIAN_POINT('Ctrl Pts',(2.73143378344912,0.31901330165504,12.4908873016278));
#418941=CARTESIAN_POINT('Ctrl Pts',(2.73118073901225,0.321179901354785,
12.4908873016278));
#418942=CARTESIAN_POINT('Ctrl Pts',(2.73092363558219,0.32335840599233,12.4911020829134));
#418943=CARTESIAN_POINT('Ctrl Pts',(2.73067083769925,0.325479302166645,
12.4915448903141));
#418944=CARTESIAN_POINT('Ctrl Pts',(2.73023833132712,0.329107897071582,
12.4923024798169));
#418945=CARTESIAN_POINT('Ctrl Pts',(2.72980823603868,0.332651165270232,
12.4937722312795));
#418946=CARTESIAN_POINT('Ctrl Pts',(2.72942595671059,0.335758762855861,
12.4958030942394));
#418947=CARTESIAN_POINT('Ctrl Pts',(2.72904637563899,0.338844425969099,
12.4978196226833));
#418948=CARTESIAN_POINT('Ctrl Pts',(2.72870300363815,0.341592061542097,
12.5004326847668));
#418949=CARTESIAN_POINT('Ctrl Pts',(2.72841736102732,0.343858552379808,
12.5033504258767));
#418950=CARTESIAN_POINT('Ctrl Pts',(2.72807606856238,0.346566608585158,
12.5068366111226));
#418951=CARTESIAN_POINT('Ctrl Pts',(2.72780647806437,0.348674950143163,
12.5108395010833));
#418952=CARTESIAN_POINT('Ctrl Pts',(2.72760908040867,0.350212370529921,
12.5149868989719));
#418953=CARTESIAN_POINT('Ctrl Pts',(2.72727753222588,0.352794614648265,
12.5219528491417));
#418954=CARTESIAN_POINT('Ctrl Pts',(2.72713487223864,0.353886123804696,
12.5295503425868));
#418955=CARTESIAN_POINT('Ctrl Pts',(2.72713487224331,0.353886123766466,
12.5369868989719));
#418956=CARTESIAN_POINT('',(2.74227835225431,0.205935520873343,12.5369868989719));
#418957=CARTESIAN_POINT('Ctrl Pts',(2.74227835225431,0.205935520873343,
12.5369868989719));
#418958=CARTESIAN_POINT('Ctrl Pts',(2.74227835225431,0.205935520873345,
12.5309445149785));
#418959=CARTESIAN_POINT('Ctrl Pts',(2.74222454994548,0.206657354683734,
12.5248274368704));
#418960=CARTESIAN_POINT('Ctrl Pts',(2.74209905884049,0.20830926889149,12.5190199595513));
#418961=CARTESIAN_POINT('Ctrl Pts',(2.74199365418625,0.20969677317644,12.5141420429941));
#418962=CARTESIAN_POINT('Ctrl Pts',(2.74183445004669,0.211783339901194,
12.5093757677094));
#418963=CARTESIAN_POINT('Ctrl Pts',(2.7416090978449,0.214661488427848,12.5051960112707));
#418964=CARTESIAN_POINT('Ctrl Pts',(2.74145854703816,0.216584290065338,
12.5024036458141));
#418965=CARTESIAN_POINT('Ctrl Pts',(2.7412746566255,0.218906995739292,12.4998248032393));
#418966=CARTESIAN_POINT('Ctrl Pts',(2.74106126700128,0.221547129399919,
12.4976950015772));
#418967=CARTESIAN_POINT('Ctrl Pts',(2.74084186491788,0.224261651381494,
12.495505190692));
#418968=CARTESIAN_POINT('Ctrl Pts',(2.74058541523159,0.227381718331238,
12.4937456938368));
#418969=CARTESIAN_POINT('Ctrl Pts',(2.74030894631981,0.230666162927312,
12.4925987732155));
#418970=CARTESIAN_POINT('Ctrl Pts',(2.74003254210069,0.233949838976013,
12.4914521209692));
#418971=CARTESIAN_POINT('Ctrl Pts',(2.73972910750241,0.237479676493582,
12.4908873016276));
#418972=CARTESIAN_POINT('Ctrl Pts',(2.73942332301885,0.240956131485315,
12.4908873016278));
#418973=CARTESIAN_POINT('',(2.74227835225431,0.205935520873345,13.7435492065112));
#418974=CARTESIAN_POINT('',(2.74227835225431,0.205935520873345,14.));
#418975=CARTESIAN_POINT('',(2.74690556033417,0.130421787310419,13.7435492065112));
#418976=CARTESIAN_POINT('Origin',(0.,2.5406128344257E-15,13.7435492065112));
#418977=CARTESIAN_POINT('',(2.74690556033417,0.130421787310419,12.5369868989719));
#418978=CARTESIAN_POINT('',(2.74690556033417,0.130421787310419,14.));
#418979=CARTESIAN_POINT('Ctrl Pts',(2.748347708522,0.0953146004653459,12.4908873016278));
#418980=CARTESIAN_POINT('Ctrl Pts',(2.74827210405888,0.0974946164540769,
12.4908873016278));
#418981=CARTESIAN_POINT('Ctrl Pts',(2.74819342447149,0.0996868286135354,
12.4911020829134));
#418982=CARTESIAN_POINT('Ctrl Pts',(2.74811434048029,0.101821273055113,
12.4915448903141));
#418983=CARTESIAN_POINT('Ctrl Pts',(2.74797903740842,0.105473047394364,
12.4923024798169));
#418984=CARTESIAN_POINT('Ctrl Pts',(2.74783918247886,0.1090395824192,12.4937722312795));
#418985=CARTESIAN_POINT('Ctrl Pts',(2.74771147320646,0.112167999044369,
12.4958030942394));
#418986=CARTESIAN_POINT('Ctrl Pts',(2.74758466534919,0.11527433424934,12.4978196226833));
#418987=CARTESIAN_POINT('Ctrl Pts',(2.74746639369736,0.118040815297413,
12.5004326847668));
#418988=CARTESIAN_POINT('Ctrl Pts',(2.7473664415831,0.120323047098392,12.5033504258767));
#418989=CARTESIAN_POINT('Ctrl Pts',(2.74724701646178,0.123049910974415,
12.5068366111226));
#418990=CARTESIAN_POINT('Ctrl Pts',(2.74715017241379,0.125173211328155,
12.5108395010833));
#418991=CARTESIAN_POINT('Ctrl Pts',(2.74707874561673,0.126721605816895,
12.5149868989719));
#418992=CARTESIAN_POINT('Ctrl Pts',(2.7469587775012,0.129322281985796,12.5219528491417));
#418993=CARTESIAN_POINT('Ctrl Pts',(2.74690556033263,0.130421787348903,
12.5295503425868));
#418994=CARTESIAN_POINT('Ctrl Pts',(2.74690556033417,0.130421787310419,
12.5369868989719));
#418995=CARTESIAN_POINT('',(2.74993930402251,-0.0182708563627483,12.5369868989719));
#418996=CARTESIAN_POINT('Ctrl Pts',(2.7499393040225,-0.0182708563627482,
12.5369868989719));
#418997=CARTESIAN_POINT('Ctrl Pts',(2.7499393040225,-0.0182708563627464,
12.5309445149785));
#418998=CARTESIAN_POINT('Ctrl Pts',(2.74994451689314,-0.0175470390071679,
12.5248274368704));
#418999=CARTESIAN_POINT('Ctrl Pts',(2.749954089693,-0.015890392717606,12.5190199595513));
#419000=CARTESIAN_POINT('Ctrl Pts',(2.74996213024424,-0.0144989137808532,
12.5141420429941));
#419001=CARTESIAN_POINT('Ctrl Pts',(2.74997353040213,-0.0124063133193932,
12.5093757677094));
#419002=CARTESIAN_POINT('Ctrl Pts',(2.74998352386555,-0.00951937329801796,
12.5051960112707));
#419003=CARTESIAN_POINT('Ctrl Pts',(2.74999020018808,-0.00759069833596158,
12.5024036458141));
#419004=CARTESIAN_POINT('Ctrl Pts',(2.74999624373097,-0.00526073249774117,
12.4998248032393));
#419005=CARTESIAN_POINT('Ctrl Pts',(2.74999875954626,-0.00261199042868737,
12.4976950015772));
#419006=CARTESIAN_POINT('Ctrl Pts',(2.75000134624709,0.000111382511553625,
12.495505190692));
#419007=CARTESIAN_POINT('Ctrl Pts',(2.75000006429767,0.00324197072610468,
12.4937456938368));
#419008=CARTESIAN_POINT('Ctrl Pts',(2.74999222803926,0.00653802138665501,
12.4925987732155));
#419009=CARTESIAN_POINT('Ctrl Pts',(2.74998439361451,0.00983330078405806,
12.4914521209692));
#419010=CARTESIAN_POINT('Ctrl Pts',(2.74996968319692,0.0133761257951871,
12.4908873016276));
#419011=CARTESIAN_POINT('Ctrl Pts',(2.74994827954166,0.0168659374438978,
12.4908873016278));
#419012=CARTESIAN_POINT('',(2.7499393040225,-0.0182708563627466,13.7435492065112));
#419013=CARTESIAN_POINT('',(2.74993930402251,-0.0182708563627466,14.));
#419014=CARTESIAN_POINT('',(2.74839604512851,-0.0939104846220984,13.7435492065112));
#419015=CARTESIAN_POINT('Origin',(0.,2.5406128344257E-15,13.7435492065112));
#419016=CARTESIAN_POINT('',(2.74839604512851,-0.0939104846220985,12.5369868989719));
#419017=CARTESIAN_POINT('',(2.74839604512851,-0.0939104846220985,14.));
#419018=CARTESIAN_POINT('Ctrl Pts',(2.74697183304013,-0.129018403664643,
12.4908873016278));
#419019=CARTESIAN_POINT('Ctrl Pts',(2.74707417168598,-0.126839479033654,
12.4908873016278));
#419020=CARTESIAN_POINT('Ctrl Pts',(2.74717443954093,-0.124648148162513,
12.4911020829134));
#419021=CARTESIAN_POINT('Ctrl Pts',(2.7472695957324,-0.122514359829273,
12.4915448903141));
#419022=CARTESIAN_POINT('Ctrl Pts',(2.7474323963804,-0.118863708011436,
12.4923024798169));
#419023=CARTESIAN_POINT('Ctrl Pts',(2.7475837125212,-0.115297640862568,
12.4937722312795));
#419024=CARTESIAN_POINT('Ctrl Pts',(2.74771142318862,-0.112169224294347,
12.4958030942394));
#419025=CARTESIAN_POINT('Ctrl Pts',(2.74783823243105,-0.109062889145921,
12.4978196226833));
#419026=CARTESIAN_POINT('Ctrl Pts',(2.74794584820655,-0.106295973097713,
12.5004326847668));
#419027=CARTESIAN_POINT('Ctrl Pts',(2.7480322517537,-0.104013188209558,
12.5033504258767));
#419028=CARTESIAN_POINT('Ctrl Pts',(2.74813548873049,-0.101285663492056,
12.5068366111226));
#419029=CARTESIAN_POINT('Ctrl Pts',(2.74821203561366,-0.0991615345561148,
12.5108395010833));
#419030=CARTESIAN_POINT('Ctrl Pts',(2.74826705500881,-0.0976124702752494,
12.5149868989719));
#419031=CARTESIAN_POINT('Ctrl Pts',(2.74835946532855,-0.0950106691266142,
12.5219528491417));
#419032=CARTESIAN_POINT('Ctrl Pts',(2.74839604513011,-0.093910484583617,
12.5295503425868));
#419033=CARTESIAN_POINT('Ctrl Pts',(2.74839604512851,-0.0939104846220985,
12.5369868989719));
#419034=CARTESIAN_POINT('',(2.73929986343048,-0.242355644064225,12.5369868989719));
#419035=CARTESIAN_POINT('Ctrl Pts',(2.73929986343047,-0.242355644064225,
12.5369868989719));
#419036=CARTESIAN_POINT('Ctrl Pts',(2.73929986343047,-0.242355644064223,
12.5309445149785));
#419037=CARTESIAN_POINT('Ctrl Pts',(2.73936405678979,-0.241634660048535,
12.5248274368704));
#419038=CARTESIAN_POINT('Ctrl Pts',(2.7395086297891,-0.239984306384896,
12.5190199595513));
#419039=CARTESIAN_POINT('Ctrl Pts',(2.73963006203727,-0.238598112859088,
12.5141420429941));
#419040=CARTESIAN_POINT('Ctrl Pts',(2.73981199062644,-0.236513404571738,
12.5093757677094));
#419041=CARTESIAN_POINT('Ctrl Pts',(2.74005726325022,-0.233636885165171,
12.5051960112707));
#419042=CARTESIAN_POINT('Ctrl Pts',(2.74022112227219,-0.231715171892212,
12.5024036458141));
#419043=CARTESIAN_POINT('Ctrl Pts',(2.74041705955186,-0.229393451427962,
12.4998248032393));
#419044=CARTESIAN_POINT('Ctrl Pts',(2.74063546406433,-0.226753727891939,
12.4976950015772));
#419045=CARTESIAN_POINT('Ctrl Pts',(2.74086002233531,-0.224039627590625,
12.495505190692));
#419046=CARTESIAN_POINT('Ctrl Pts',(2.74111391665392,-0.220919351659323,
12.4937456938368));
#419047=CARTESIAN_POINT('Ctrl Pts',(2.74137476519789,-0.217633629607633,
12.4925987732155));
#419048=CARTESIAN_POINT('Ctrl Pts',(2.74163555270431,-0.214348676402234,
12.4914521209692));
#419049=CARTESIAN_POINT('Ctrl Pts',(2.74190966436281,-0.210816440813469,
12.4908873016276));
#419050=CARTESIAN_POINT('Ctrl Pts',(2.74217278397365,-0.207336496628525,
12.4908873016278));
#419051=CARTESIAN_POINT('',(2.73929986343048,-0.242355644064223,13.7435492065112));
#419052=CARTESIAN_POINT('',(2.73929986343048,-0.242355644064223,14.));
#419053=CARTESIAN_POINT('',(2.73159640769596,-0.317617797773595,13.7435492065112));
#419054=CARTESIAN_POINT('Origin',(0.,2.5406128344257E-15,13.7435492065112));
#419055=CARTESIAN_POINT('',(2.73159640769596,-0.317617797773595,12.5369868989719));
#419056=CARTESIAN_POINT('',(2.73159640769596,-0.317617797773595,14.));
#419057=CARTESIAN_POINT('Ctrl Pts',(2.72731531322782,-0.352492811604782,
12.4908873016278));
#419058=CARTESIAN_POINT('Ctrl Pts',(2.72759491393585,-0.350329478715456,
12.4908873016278));
#419059=CARTESIAN_POINT('Ctrl Pts',(2.7278734619671,-0.348153612078037,
12.4911020829134));
#419060=CARTESIAN_POINT('Ctrl Pts',(2.72814222509247,-0.346034679862442,
12.4915448903141));
#419061=CARTESIAN_POINT('Ctrl Pts',(2.7286020460489,-0.342409445051551,
12.4923024798169));
#419062=CARTESIAN_POINT('Ctrl Pts',(2.72904352627611,-0.338867577367167,
12.4937722312795));
#419063=CARTESIAN_POINT('Ctrl Pts',(2.72942580698993,-0.335759979952003,
12.4958030942394));
#419064=CARTESIAN_POINT('Ctrl Pts',(2.72980538943748,-0.332674317008026,
12.4978196226833));
#419065=CARTESIAN_POINT('Ctrl Pts',(2.73013817647509,-0.329925379329474,
12.5004326847668));
#419066=CARTESIAN_POINT('Ctrl Pts',(2.73041036068228,-0.327657232910942,
12.5033504258767));
#419067=CARTESIAN_POINT('Ctrl Pts',(2.73073557273213,-0.324947198578946,
12.5068366111226));
#419068=CARTESIAN_POINT('Ctrl Pts',(2.73098500113959,-0.322836376788416,
12.5108395010833));
#419069=CARTESIAN_POINT('Ctrl Pts',(2.73116610058194,-0.321296951482636,
12.5149868989719));
#419070=CARTESIAN_POINT('Ctrl Pts',(2.73147027436152,-0.318711339911643,
12.5219528491417));
#419071=CARTESIAN_POINT('Ctrl Pts',(2.73159640770069,-0.317617797735372,
12.5295503425868));
#419072=CARTESIAN_POINT('Ctrl Pts',(2.73159640769596,-0.317617797773595,
12.5369868989719));
#419073=CARTESIAN_POINT('',(2.71043083419998,-0.464827594940321,12.5369868989719));
#419074=CARTESIAN_POINT('Ctrl Pts',(2.71043083419998,-0.46482759494032,
12.5369868989719));
#419075=CARTESIAN_POINT('Ctrl Pts',(2.71043083419998,-0.464827594940319,
12.5309445149785));
#419076=CARTESIAN_POINT('Ctrl Pts',(2.71055358085175,-0.464114242294192,
12.5248274368704));
#419077=CARTESIAN_POINT('Ctrl Pts',(2.71083219194106,-0.462481164087819,
12.5190199595513));
#419078=CARTESIAN_POINT('Ctrl Pts',(2.71106620777459,-0.461109480862163,
12.5141420429941));
#419079=CARTESIAN_POINT('Ctrl Pts',(2.71141745409029,-0.459046538138622,
12.5093757677094));
#419080=CARTESIAN_POINT('Ctrl Pts',(2.71189637362559,-0.456199582108923,
12.5051960112707));
#419081=CARTESIAN_POINT('Ctrl Pts',(2.71221632489224,-0.454297619209833,
12.5024036458141));
#419082=CARTESIAN_POINT('Ctrl Pts',(2.71260085197841,-0.451999594786184,
12.4998248032393));
#419083=CARTESIAN_POINT('Ctrl Pts',(2.71303369174207,-0.449386456707801,
12.4976950015772));
#419084=CARTESIAN_POINT('Ctrl Pts',(2.71347872718496,-0.446699690935124,
12.495505190692));
#419085=CARTESIAN_POINT('Ctrl Pts',(2.7139861081468,-0.443610492208585,
12.4937456938368));
#419086=CARTESIAN_POINT('Ctrl Pts',(2.71451390558913,-0.440356964703903,
12.4925987732155));
#419087=CARTESIAN_POINT('Ctrl Pts',(2.7150415795289,-0.437104198512112,
12.4914521209692));
#419088=CARTESIAN_POINT('Ctrl Pts',(2.71560268909562,-0.433606058790776,
12.4908873016276));
#419089=CARTESIAN_POINT('Ctrl Pts',(2.71614858095496,-0.430159140523998,
12.4908873016278));
#419090=CARTESIAN_POINT('',(2.71043083419998,-0.464827594940319,13.7435492065112));
#419091=CARTESIAN_POINT('',(2.71043083419998,-0.464827594940319,14.));
#419092=CARTESIAN_POINT('',(2.69661844685187,-0.539211416884157,13.7435492065112));
#419093=CARTESIAN_POINT('Origin',(0.,2.5406128344257E-15,13.7435492065112));
#419094=CARTESIAN_POINT('',(2.69661844685187,-0.539211416884157,12.5369868989719));
#419095=CARTESIAN_POINT('',(2.69661844685187,-0.539211416884157,14.));
#419096=CARTESIAN_POINT('Ctrl Pts',(2.68950895998134,-0.573621438040911,
12.4908873016278));
#419097=CARTESIAN_POINT('Ctrl Pts',(2.68996396205496,-0.571488093516703,
12.4908873016278));
#419098=CARTESIAN_POINT('Ctrl Pts',(2.69041893657132,-0.569342171146484,
12.4911020829134));
#419099=CARTESIAN_POINT('Ctrl Pts',(2.69085951805634,-0.56725219619283,
12.4915448903141));
#419100=CARTESIAN_POINT('Ctrl Pts',(2.6916132992886,-0.563676503728429,
12.4923024798169));
#419101=CARTESIAN_POINT('Ctrl Pts',(2.69234200562415,-0.560182406053602,
12.4937722312795));
#419102=CARTESIAN_POINT('Ctrl Pts',(2.69297631236929,-0.557116308339575,
12.4958030942394));
#419103=CARTESIAN_POINT('Ctrl Pts',(2.69360614196338,-0.554071852177842,
12.4978196226833));
#419104=CARTESIAN_POINT('Ctrl Pts',(2.69416188562028,-0.551359186595653,
12.5004326847668));
#419105=CARTESIAN_POINT('Ctrl Pts',(2.69461803914653,-0.549120772786941,
12.5033504258767));
#419106=CARTESIAN_POINT('Ctrl Pts',(2.6951630620369,-0.546446263671806,
12.5068366111226));
#419107=CARTESIAN_POINT('Ctrl Pts',(2.69558371206375,-0.544362796197442,
12.5108395010833));
#419108=CARTESIAN_POINT('Ctrl Pts',(2.6958896863664,-0.542843254488171,
12.5149868989719));
#419109=CARTESIAN_POINT('Ctrl Pts',(2.6964035993795,-0.54029103931323,12.5219528491417));
#419110=CARTESIAN_POINT('Ctrl Pts',(2.6966184468597,-0.539211416846447,
12.5295503425868));
#419111=CARTESIAN_POINT('Ctrl Pts',(2.69661844685187,-0.539211416884157,
12.5369868989719));
#419112=CARTESIAN_POINT('',(2.6635243349575,-0.684206194863244,12.5369868989719));
#419113=CARTESIAN_POINT('Ctrl Pts',(2.66352433495749,-0.684206194863243,
12.5369868989719));
#419114=CARTESIAN_POINT('Ctrl Pts',(2.66352433495749,-0.684206194863241,
12.5309445149785));
#419115=CARTESIAN_POINT('Ctrl Pts',(2.66370481804301,-0.683505220830841,
12.5248274368704));
#419116=CARTESIAN_POINT('Ctrl Pts',(2.66411561311148,-0.681900285947758,
12.5190199595513));
#419117=CARTESIAN_POINT('Ctrl Pts',(2.66446065519361,-0.680552241347809,
12.5141420429941));
#419118=CARTESIAN_POINT('Ctrl Pts',(2.66497888174957,-0.678524792731542,
12.5093757677094));
#419119=CARTESIAN_POINT('Ctrl Pts',(2.66568826106589,-0.675726346101373,
12.5051960112707));
#419120=CARTESIAN_POINT('Ctrl Pts',(2.66616217535433,-0.673856790825442,
12.5024036458141));
#419121=CARTESIAN_POINT('Ctrl Pts',(2.66673273328269,-0.671597755415789,
12.4998248032393));
#419122=CARTESIAN_POINT('Ctrl Pts',(2.66737712782032,-0.669028592797819,
12.4976950015772));
#419123=CARTESIAN_POINT('Ctrl Pts',(2.66803967879768,-0.666387041536711,
12.495505190692));
#419124=CARTESIAN_POINT('Ctrl Pts',(2.66879716986615,-0.663349478122779,
12.4937456938368));
#419125=CARTESIAN_POINT('Ctrl Pts',(2.66958840380194,-0.660149796853853,
12.4925987732155));
#419126=CARTESIAN_POINT('Ctrl Pts',(2.67037945259204,-0.656950864298008,
12.4914521209692));
#419127=CARTESIAN_POINT('Ctrl Pts',(2.67122382597541,-0.653510099986794,
12.4908873016276));
#419128=CARTESIAN_POINT('Ctrl Pts',(2.67204885726299,-0.650119146310548,
12.4908873016278));
#419129=CARTESIAN_POINT('',(2.66352433495749,-0.684206194863242,13.7435492065112));
#419130=CARTESIAN_POINT('',(2.6635243349575,-0.684206194863242,14.));
#419131=CARTESIAN_POINT('',(2.64369493515471,-0.757216672978976,13.7435492065112));
#419132=CARTESIAN_POINT('Origin',(0.,2.5406128344257E-15,13.7435492065112));
#419133=CARTESIAN_POINT('',(2.64369493515471,-0.757216672978976,12.5369868989719));
#419134=CARTESIAN_POINT('',(2.64369493515471,-0.757216672978976,14.));
#419135=CARTESIAN_POINT('Ctrl Pts',(2.63380436834392,-0.790932708447753,
12.4908873016278));
#419136=CARTESIAN_POINT('Ctrl Pts',(2.6344317438194,-0.788843549344495,
12.4908873016278));
#419137=CARTESIAN_POINT('Ctrl Pts',(2.63506011704054,-0.786741852000797,
12.4911020829134));
#419138=CARTESIAN_POINT('Ctrl Pts',(2.63566958488812,-0.784694742747579,
12.4915448903141));
#419139=CARTESIAN_POINT('Ctrl Pts',(2.63671231010647,-0.781192388273072,
12.4923024798169));
#419140=CARTESIAN_POINT('Ctrl Pts',(2.63772339312991,-0.777769313251341,
12.4937722312795));
#419141=CARTESIAN_POINT('Ctrl Pts',(2.63860550469964,-0.774765119612869,
12.4958030942394));
#419142=CARTESIAN_POINT('Ctrl Pts',(2.63948139002826,-0.771782130586836,
12.4978196226833));
#419143=CARTESIAN_POINT('Ctrl Pts',(2.64025639192208,-0.769123789442901,
12.5004326847668));
#419144=CARTESIAN_POINT('Ctrl Pts',(2.64089347914094,-0.766930004518594,
12.5033504258767));
#419145=CARTESIAN_POINT('Ctrl Pts',(2.64165468583441,-0.764308819037219,
12.5068366111226));
#419146=CARTESIAN_POINT('Ctrl Pts',(2.64224375812413,-0.762266571011315,
12.5108395010833));
#419147=CARTESIAN_POINT('Ctrl Pts',(2.64267257107857,-0.760777025197919,
12.5149868989719));
#419148=CARTESIAN_POINT('Ctrl Pts',(2.64339280331889,-0.758275190989934,
12.5219528491417));
#419149=CARTESIAN_POINT('Ctrl Pts',(2.64369493516559,-0.75721667294203,
12.5295503425868));
#419150=CARTESIAN_POINT('Ctrl Pts',(2.64369493515471,-0.757216672978976,
12.5369868989719));
#419151=CARTESIAN_POINT('',(2.59889252071645,-0.899031515445429,12.5369868989719));
#419152=CARTESIAN_POINT('Ctrl Pts',(2.59889252071645,-0.899031515445427,
12.5369868989719));
#419153=CARTESIAN_POINT('Ctrl Pts',(2.59889252071645,-0.899031515445425,
12.5309445149785));
#419154=CARTESIAN_POINT('Ctrl Pts',(2.59912953915055,-0.898347584893284,
12.5248274368704));
#419155=CARTESIAN_POINT('Ctrl Pts',(2.59966978442478,-0.896781473910343,
12.5190199595513));
#419156=CARTESIAN_POINT('Ctrl Pts',(2.60012355655737,-0.895466038950502,
12.5141420429941));
#419157=CARTESIAN_POINT('Ctrl Pts',(2.60080531464136,-0.893487576777544,
12.5093757677094));
#419158=CARTESIAN_POINT('Ctrl Pts',(2.6017404329364,-0.890756262747518,
12.5051960112707));
#419159=CARTESIAN_POINT('Ctrl Pts',(2.60236515642523,-0.888931556676653,
12.5024036458141));
#419160=CARTESIAN_POINT('Ctrl Pts',(2.6031179482269,-0.886726543788931,
12.4998248032393));
#419161=CARTESIAN_POINT('Ctrl Pts',(2.60396960919917,-0.884218453984716,
12.4976950015772));
#419162=CARTESIAN_POINT('Ctrl Pts',(2.60484526654355,-0.881639696322995,
12.495505190692));
#419163=CARTESIAN_POINT('Ctrl Pts',(2.60584782674059,-0.878673982705026,
12.4937456938368));
#419164=CARTESIAN_POINT('Ctrl Pts',(2.60689723163854,-0.875549441022792,
12.4925987732155));
#419165=CARTESIAN_POINT('Ctrl Pts',(2.60794639097979,-0.872425630471265,
12.4914521209692));
#419166=CARTESIAN_POINT('Ctrl Pts',(2.60906840901424,-0.869065139288977,
12.4908873016276));
#419167=CARTESIAN_POINT('Ctrl Pts',(2.61016708928296,-0.865752716440509,
12.4908873016278));
#419168=CARTESIAN_POINT('',(2.59889252071645,-0.899031515445426,13.7435492065112));
#419169=CARTESIAN_POINT('',(2.59889252071645,-0.899031515445427,14.));
#419170=CARTESIAN_POINT('',(2.57317806984305,-0.970182777047077,13.7435492065112));
#419171=CARTESIAN_POINT('Origin',(0.,2.5406128344257E-15,13.7435492065112));
#419172=CARTESIAN_POINT('',(2.57317806984306,-0.970182777047077,12.5369868989719));
#419173=CARTESIAN_POINT('',(2.57317806984306,-0.970182777047077,14.));
#419174=CARTESIAN_POINT('Ctrl Pts',(2.56057224318231,-1.00298045217459,
12.4908873016278));
#419175=CARTESIAN_POINT('Ctrl Pts',(2.56136781697937,-1.00094938150142,
12.4908873016278));
#419176=CARTESIAN_POINT('Ctrl Pts',(2.56216540718517,-0.998905895633315,
12.4911020829134));
#419177=CARTESIAN_POINT('Ctrl Pts',(2.56293970548734,-0.996915275254863,
12.4915448903141));
#419178=CARTESIAN_POINT('Ctrl Pts',(2.56426443552748,-0.99350956636143,
12.4923024798169));
#419179=CARTESIAN_POINT('Ctrl Pts',(2.56555116664813,-0.990180293992298,
12.4937722312795));
#419180=CARTESIAN_POINT('Ctrl Pts',(2.56667521273549,-0.987257996842386,
12.4958030942394));
#419181=CARTESIAN_POINT('Ctrl Pts',(2.56779132492627,-0.984356326251862,
12.4978196226833));
#419182=CARTESIAN_POINT('Ctrl Pts',(2.56878042754729,-0.9817700003679,12.5004326847668));
#419183=CARTESIAN_POINT('Ctrl Pts',(2.56959420874842,-0.979635443604719,
12.5033504258767));
#419184=CARTESIAN_POINT('Ctrl Pts',(2.57056653354004,-0.977085025314017,
12.5068366111226));
#419185=CARTESIAN_POINT('Ctrl Pts',(2.57132010791373,-0.975097587560238,
12.5108395010833));
#419186=CARTESIAN_POINT('Ctrl Pts',(2.5718689058405,-0.97364795032435,12.5149868989719));
#419187=CARTESIAN_POINT('Ctrl Pts',(2.5727906642813,-0.971213146377201,
12.5219528491417));
#419188=CARTESIAN_POINT('Ctrl Pts',(2.57317806985691,-0.970182777011141,
12.5295503425868));
#419189=CARTESIAN_POINT('Ctrl Pts',(2.57317806984306,-0.970182777047077,
12.5369868989719));
#419190=CARTESIAN_POINT('',(2.51696550553712,-1.10787392962208,12.5369868989719));
#419191=CARTESIAN_POINT('Ctrl Pts',(2.51696550553712,-1.10787392962208,
12.5369868989719));
#419192=CARTESIAN_POINT('Ctrl Pts',(2.51696550553712,-1.10787392962208,
12.5309445149785));
#419193=CARTESIAN_POINT('Ctrl Pts',(2.51725748200124,-1.10721159399518,
12.5248274368704));
#419194=CARTESIAN_POINT('Ctrl Pts',(2.51792358223806,-1.10569472912258,
12.5190199595513));
#419195=CARTESIAN_POINT('Ctrl Pts',(2.51848306464244,-1.10442065780548,
12.5141420429941));
#419196=CARTESIAN_POINT('Ctrl Pts',(2.51932381726689,-1.10250434841516,
12.5093757677094));
#419197=CARTESIAN_POINT('Ctrl Pts',(2.52047845148267,-1.09985834342952,
12.5051960112707));
#419198=CARTESIAN_POINT('Ctrl Pts',(2.52124982674015,-1.09809062968156,
12.5024036458141));
#419199=CARTESIAN_POINT('Ctrl Pts',(2.52217984270989,-1.09595431331274,
12.4998248032393));
#419200=CARTESIAN_POINT('Ctrl Pts',(2.52323310245354,-1.09352398724612,
12.4976950015772));
#419201=CARTESIAN_POINT('Ctrl Pts',(2.5243160388098,-1.09102518439056,12.495505190692));
#419202=CARTESIAN_POINT('Ctrl Pts',(2.52555699626269,-1.08815105690337,
12.4937456938368));
#419203=CARTESIAN_POINT('Ctrl Pts',(2.52685758850634,-1.08512244811721,
12.4925987732155));
#419204=CARTESIAN_POINT('Ctrl Pts',(2.52815787641643,-1.08209454801383,
12.4914521209692));
#419205=CARTESIAN_POINT('Ctrl Pts',(2.52955007225706,-1.07883669347485,
12.4908873016276));
#419206=CARTESIAN_POINT('Ctrl Pts',(2.53091508997101,-1.0756248450817,12.4908873016278));
#419207=CARTESIAN_POINT('',(2.51696550553712,-1.10787392962208,13.7435492065112));
#419208=CARTESIAN_POINT('',(2.51696550553712,-1.10787392962208,14.));
#419209=CARTESIAN_POINT('',(2.48553712902109,-1.17669247480282,13.7435492065112));
#419210=CARTESIAN_POINT('Origin',(0.,2.5406128344257E-15,13.7435492065112));
#419211=CARTESIAN_POINT('',(2.48553712902109,-1.17669247480282,12.5369868989719));
#419212=CARTESIAN_POINT('',(2.4855371290211,-1.17669247480282,14.));
#419213=CARTESIAN_POINT('Ctrl Pts',(2.470299932207,-1.20835352647233,12.4908873016278));
#419214=CARTESIAN_POINT('Ctrl Pts',(2.47125840991329,-1.20639406066948,
12.4908873016278));
#419215=CARTESIAN_POINT('Ctrl Pts',(2.47221990927252,-1.20442238533826,
12.4911020829134));
#419216=CARTESIAN_POINT('Ctrl Pts',(2.47315388520183,-1.20250150108477,
12.4915448903141));
#419217=CARTESIAN_POINT('Ctrl Pts',(2.47475180420392,-1.19921510220319,
12.4923024798169));
#419218=CARTESIAN_POINT('Ctrl Pts',(2.47630562043845,-1.19600178824498,
12.4937722312795));
#419219=CARTESIAN_POINT('Ctrl Pts',(2.47766412070218,-1.19318083498902,
12.4958030942394));
#419220=CARTESIAN_POINT('Ctrl Pts',(2.47901303221264,-1.19037979297304,
12.4978196226833));
#419221=CARTESIAN_POINT('Ctrl Pts',(2.48020965324611,-1.1878826939211,12.5004326847668));
#419222=CARTESIAN_POINT('Ctrl Pts',(2.48119471284988,-1.18582157044213,
12.5033504258767));
#419223=CARTESIAN_POINT('Ctrl Pts',(2.48237168507859,-1.18335889195503,
12.5068366111226));
#419224=CARTESIAN_POINT('Ctrl Pts',(2.48328474662312,-1.18143949054373,
12.5108395010833));
#419225=CARTESIAN_POINT('Ctrl Pts',(2.48394987736256,-1.18003940898198,
12.5149868989719));
#419226=CARTESIAN_POINT('Ctrl Pts',(2.4850670278535,-1.17768783851422,12.5219528491417));
#419227=CARTESIAN_POINT('Ctrl Pts',(2.48553712903783,-1.17669247476813,
12.5295503425868));
#419228=CARTESIAN_POINT('Ctrl Pts',(2.48553712902109,-1.17669247480282,
12.5369868989719));
#419229=CARTESIAN_POINT('',(2.41828850018852,-1.30934362558343,12.5369868989719));
#419230=CARTESIAN_POINT('Ctrl Pts',(2.41828850018852,-1.30934362558343,
12.5369868989719));
#419231=CARTESIAN_POINT('Ctrl Pts',(2.41828850018852,-1.30934362558343,
12.5309445149785));
#419232=CARTESIAN_POINT('Ctrl Pts',(2.41863349162745,-1.30870729261609,
12.5248274368704));
#419233=CARTESIAN_POINT('Ctrl Pts',(2.41942101403969,-1.3072497683393,12.5190199595513));
#419234=CARTESIAN_POINT('Ctrl Pts',(2.42008248345277,-1.30602553939934,
12.5141420429941));
#419235=CARTESIAN_POINT('Ctrl Pts',(2.42107663554767,-1.3041841355145,12.5093757677094));
#419236=CARTESIAN_POINT('Ctrl Pts',(2.422443101784,-1.30164104829985,12.5051960112707));
#419237=CARTESIAN_POINT('Ctrl Pts',(2.42335599543505,-1.29994209071815,
12.5024036458141));
#419238=CARTESIAN_POINT('Ctrl Pts',(2.42445704647003,-1.29788868770119,
12.4998248032393));
#419239=CARTESIAN_POINT('Ctrl Pts',(2.42570489571525,-1.29555229879116,
12.4976950015772));
#419240=CARTESIAN_POINT('Ctrl Pts',(2.4269879043206,-1.29315007986249,12.495505190692));
#419241=CARTESIAN_POINT('Ctrl Pts',(2.42845900066224,-1.29038666535032,
12.4937456938368));
#419242=CARTESIAN_POINT('Ctrl Pts',(2.4300021250248,-1.28747414435202,12.4925987732155));
#419243=CARTESIAN_POINT('Ctrl Pts',(2.4315448883022,-1.2845623048724,12.4914521209692));
#419244=CARTESIAN_POINT('Ctrl Pts',(2.4331979971154,-1.28142876746117,12.4908873016276));
#419245=CARTESIAN_POINT('Ctrl Pts',(2.4348202683069,-1.27833886784448,12.4908873016278));
#419246=CARTESIAN_POINT('',(2.41828850018852,-1.30934362558343,13.7435492065112));
#419247=CARTESIAN_POINT('',(2.41828850018852,-1.30934362558343,14.));
#419248=CARTESIAN_POINT('',(2.38135534869026,-1.37537147827934,13.7435492065112));
#419249=CARTESIAN_POINT('Origin',(0.,2.5406128344257E-15,13.7435492065112));
#419250=CARTESIAN_POINT('',(2.38135534869026,-1.37537147827934,12.5369868989719));
#419251=CARTESIAN_POINT('',(2.38135534869026,-1.37537147827935,14.));
#419252=CARTESIAN_POINT('Ctrl Pts',(2.36358818275365,-1.40568520741569,
12.4908873016278));
#419253=CARTESIAN_POINT('Ctrl Pts',(2.36470318585817,-1.4038103864048,12.4908873016278));
#419254=CARTESIAN_POINT('Ctrl Pts',(2.36582219575124,-1.40192364278449,
12.4911020829134));
#419255=CARTESIAN_POINT('Ctrl Pts',(2.36690963385196,-1.40008527782374,
12.4915448903141));
#419256=CARTESIAN_POINT('Ctrl Pts',(2.36877010792868,-1.39694005939636,
12.4923024798169));
#419257=CARTESIAN_POINT('Ctrl Pts',(2.37058066888642,-1.39386408792331,
12.4937722312795));
#419258=CARTESIAN_POINT('Ctrl Pts',(2.37216458273141,-1.39116325153978,
12.4958030942394));
#419259=CARTESIAN_POINT('Ctrl Pts',(2.373737316778,-1.38848147857083,12.4978196226833));
#419260=CARTESIAN_POINT('Ctrl Pts',(2.37513349290836,-1.3860902241331,12.5004326847668));
#419261=CARTESIAN_POINT('Ctrl Pts',(2.37628327550563,-1.38411625037503,
12.5033504258767));
#419262=CARTESIAN_POINT('Ctrl Pts',(2.37765706261544,-1.38175770041056,
12.5068366111226));
#419263=CARTESIAN_POINT('Ctrl Pts',(2.37872353505688,-1.37991910864144,
12.5108395010833));
#419264=CARTESIAN_POINT('Ctrl Pts',(2.37950057227366,-1.37857790006563,
12.5149868989719));
#419265=CARTESIAN_POINT('Ctrl Pts',(2.38080568036253,-1.37632521239074,
12.5219528491417));
#419266=CARTESIAN_POINT('Ctrl Pts',(2.38135534870977,-1.37537147824614,
12.5295503425868));
#419267=CARTESIAN_POINT('Ctrl Pts',(2.38135534869026,-1.37537147827934,
12.5369868989719));
#419268=CARTESIAN_POINT('',(2.30351818386068,-1.50209985574302,12.5369868989719));
#419269=CARTESIAN_POINT('Ctrl Pts',(2.30351818386068,-1.50209985574302,
12.5369868989719));
#419270=CARTESIAN_POINT('Ctrl Pts',(2.30351818386068,-1.50209985574302,
12.5309445149785));
#419271=CARTESIAN_POINT('Ctrl Pts',(2.30391389441333,-1.50149376012615,
12.5248274368704));
#419272=CARTESIAN_POINT('Ctrl Pts',(2.30481759816925,-1.50010527602875,
12.5190199595513));
#419273=CARTESIAN_POINT('Ctrl Pts',(2.30557665262123,-1.49893903650754,
12.5141420429941));
#419274=CARTESIAN_POINT('Ctrl Pts',(2.30671758826842,-1.49718479236722,
12.5093757677094));
#419275=CARTESIAN_POINT('Ctrl Pts',(2.30828679291793,-1.49476154674939,
12.5051960112707));
#419276=CARTESIAN_POINT('Ctrl Pts',(2.30933512980593,-1.49314265161635,
12.5024036458141));
#419277=CARTESIAN_POINT('Ctrl Pts',(2.31059988859316,-1.49118582700954,
12.4998248032393));
#419278=CARTESIAN_POINT('Ctrl Pts',(2.31203402310911,-1.48895892353883,
12.4976950015772));
#419279=CARTESIAN_POINT('Ctrl Pts',(2.31350856575296,-1.48666927490768,
12.495505190692));
#419280=CARTESIAN_POINT('Ctrl Pts',(2.31520001107991,-1.48403496343817,
12.4937456938368));
#419281=CARTESIAN_POINT('Ctrl Pts',(2.31697539832334,-1.48125791257444,
12.4925987732155));
#419282=CARTESIAN_POINT('Ctrl Pts',(2.318750370133,-1.4784815115299,12.4914521209692));
#419283=CARTESIAN_POINT('Ctrl Pts',(2.32065339075235,-1.4754931444209,12.4908873016276));
#419284=CARTESIAN_POINT('Ctrl Pts',(2.32252211947427,-1.47254575635283,
12.4908873016278));
#419285=CARTESIAN_POINT('',(2.30351818386068,-1.50209985574302,13.7435492065112));
#419286=CARTESIAN_POINT('',(2.30351818386068,-1.50209985574302,14.));
#419287=CARTESIAN_POINT('',(2.26132604140986,-1.56489761148824,13.7435492065112));
#419288=CARTESIAN_POINT('Origin',(0.,2.5406128344257E-15,13.7435492065112));
#419289=CARTESIAN_POINT('',(2.26132604140986,-1.56489761148824,12.5369868989719));
#419290=CARTESIAN_POINT('',(2.26132604140986,-1.56489761148824,14.));
#419291=CARTESIAN_POINT('Ctrl Pts',(2.24114714390868,-1.59366228522544,
12.4908873016278));
#419292=CARTESIAN_POINT('Ctrl Pts',(2.24241125224972,-1.591884585631,12.4908873016278));
#419293=CARTESIAN_POINT('Ctrl Pts',(2.24368032585042,-1.59009532968911,
12.4911020829134));
#419294=CARTESIAN_POINT('Ctrl Pts',(2.24491398940142,-1.5883517180366,12.4915448903141));
#419295=CARTESIAN_POINT('Ctrl Pts',(2.24702463740474,-1.58536861097313,
12.4923024798169));
#419296=CARTESIAN_POINT('Ctrl Pts',(2.24907989410123,-1.58245045206789,
12.4937722312795));
#419297=CARTESIAN_POINT('Ctrl Pts',(2.25087868084216,-1.57988770617733,
12.4958030942394));
#419298=CARTESIAN_POINT('Ctrl Pts',(2.25266477113929,-1.57734304901205,
12.4978196226833));
#419299=CARTESIAN_POINT('Ctrl Pts',(2.25425121104475,-1.57507355259229,
12.5004326847668));
#419300=CARTESIAN_POINT('Ctrl Pts',(2.25555806502204,-1.57319986502479,
12.5033504258767));
#419301=CARTESIAN_POINT('Ctrl Pts',(2.25711952468639,-1.57096113934383,
12.5068366111226));
#419302=CARTESIAN_POINT('Ctrl Pts',(2.25833231082659,-1.56921559274178,
12.5108395010833));
#419303=CARTESIAN_POINT('Ctrl Pts',(2.25921608346623,-1.56794218267368,
12.5149868989719));
#419304=CARTESIAN_POINT('Ctrl Pts',(2.26070046387404,-1.56580336905648,
12.5219528491417));
#419305=CARTESIAN_POINT('Ctrl Pts',(2.26132604143202,-1.56489761145674,
12.5295503425868));
#419306=CARTESIAN_POINT('Ctrl Pts',(2.26132604140986,-1.56489761148824,
12.5369868989719));
#419307=CARTESIAN_POINT('',(2.173418334073,-1.68485985919167,12.5369868989719));
#419308=CARTESIAN_POINT('Ctrl Pts',(2.17341833407299,-1.68485985919167,
12.5369868989719));
#419309=CARTESIAN_POINT('Ctrl Pts',(2.17341833407299,-1.68485985919166,
12.5309445149785));
#419310=CARTESIAN_POINT('Ctrl Pts',(2.17386213035091,-1.68428803439161,
12.5248274368704));
#419311=CARTESIAN_POINT('Ctrl Pts',(2.17487600145114,-1.68297783060618,
12.5190199595513));
#419312=CARTESIAN_POINT('Ctrl Pts',(2.17572758955986,-1.68187734163532,
12.5141420429941));
#419313=CARTESIAN_POINT('Ctrl Pts',(2.17700771602085,-1.68022193144484,
12.5093757677094));
#419314=CARTESIAN_POINT('Ctrl Pts',(2.17876921628551,-1.67793465372362,
12.5051960112707));
#419315=CARTESIAN_POINT('Ctrl Pts',(2.17994601990143,-1.67640659451924,
12.5024036458141));
#419316=CARTESIAN_POINT('Ctrl Pts',(2.18136606967986,-1.67455937066749,
12.4998248032393));
#419317=CARTESIAN_POINT('Ctrl Pts',(2.18297694553794,-1.67245677231128,
12.4976950015772));
#419318=CARTESIAN_POINT('Ctrl Pts',(2.18463320938228,-1.67029493121153,
12.495505190692));
#419319=CARTESIAN_POINT('Ctrl Pts',(2.18653374740496,-1.66780725369287,
12.4937456938368));
#419320=CARTESIAN_POINT('Ctrl Pts',(2.18852958262007,-1.66518415377903,
12.4925987732155));
#419321=CARTESIAN_POINT('Ctrl Pts',(2.19052495081744,-1.66256166766046,
12.4914521209692));
#419322=CARTESIAN_POINT('Ctrl Pts',(2.1926652189547,-1.65973835794374,12.4908873016276));
#419323=CARTESIAN_POINT('Ctrl Pts',(2.19476796912572,-1.6569530958056,12.4908873016278));
#419324=CARTESIAN_POINT('',(2.173418334073,-1.68485985919167,13.7435492065112));
#419325=CARTESIAN_POINT('',(2.173418334073,-1.68485985919167,14.));
#419326=CARTESIAN_POINT('',(2.12624798241642,-1.74400960928261,13.7435492065112));
#419327=CARTESIAN_POINT('Origin',(0.,2.5406128344257E-15,13.7435492065112));
#419328=CARTESIAN_POINT('',(2.12624798241642,-1.74400960928262,12.5369868989719));
#419329=CARTESIAN_POINT('',(2.12624798241642,-1.74400960928262,14.));
#419330=CARTESIAN_POINT('Ctrl Pts',(2.10379164058425,-1.77103380346278,
12.4908873016278));
#419331=CARTESIAN_POINT('Ctrl Pts',(2.10519644172938,-1.76936505558229,
12.4908873016278));
#419332=CARTESIAN_POINT('Ctrl Pts',(2.10660713356226,-1.76768519452191,
12.4911020829134));
#419333=CARTESIAN_POINT('Ctrl Pts',(2.10797881273614,-1.76604793962552,
12.4915448903141));
#419334=CARTESIAN_POINT('Ctrl Pts',(2.11032558865184,-1.76324679601128,
12.4923024798169));
#419335=CARTESIAN_POINT('Ctrl Pts',(2.11261186369286,-1.7605058695399,12.4937722312795));
#419336=CARTESIAN_POINT('Ctrl Pts',(2.11461355270075,-1.75809826879339,
12.4958030942394));
#419337=CARTESIAN_POINT('Ctrl Pts',(2.11660111311217,-1.75570766170538,
12.4978196226833));
#419338=CARTESIAN_POINT('Ctrl Pts',(2.11836725929691,-1.75357502642782,
12.5004326847668));
#419339=CARTESIAN_POINT('Ctrl Pts',(2.11982248775662,-1.75181409413252,
12.5033504258767));
#419340=CARTESIAN_POINT('Ctrl Pts',(2.12156122871905,-1.74971009108511,
12.5068366111226));
#419341=CARTESIAN_POINT('Ctrl Pts',(2.12291225766636,-1.74806920597476,
12.5108395010833));
#419342=CARTESIAN_POINT('Ctrl Pts',(2.12389688436776,-1.7468720687483,12.5149868989719));
#419343=CARTESIAN_POINT('Ctrl Pts',(2.12555065878779,-1.74486136264051,
12.5219528491417));
#419344=CARTESIAN_POINT('Ctrl Pts',(2.12624798244107,-1.74400960925302,
12.5295503425868));
#419345=CARTESIAN_POINT('Ctrl Pts',(2.12624798241642,-1.74400960928262,
12.5369868989719));
#419346=CARTESIAN_POINT('',(2.02885474386084,-1.8564073982597,12.5369868989719));
#419347=CARTESIAN_POINT('Ctrl Pts',(2.02885474386084,-1.8564073982597,12.5369868989719));
#419348=CARTESIAN_POINT('Ctrl Pts',(2.02885474386084,-1.8564073982597,12.5309445149785));
#419349=CARTESIAN_POINT('Ctrl Pts',(2.02934367247302,-1.85587364967614,
12.5248274368704));
#419350=CARTESIAN_POINT('Ctrl Pts',(2.03046096377265,-1.85465044539272,
12.5190199595513));
#419351=CARTESIAN_POINT('Ctrl Pts',(2.03139941835976,-1.85362303054475,
12.5141420429941));
#419352=CARTESIAN_POINT('Ctrl Pts',(2.03281021660416,-1.85207747078579,
12.5093757677094));
#419353=CARTESIAN_POINT('Ctrl Pts',(2.03475228999032,-1.84994138241705,
12.5051960112707));
#419354=CARTESIAN_POINT('Ctrl Pts',(2.03604972890026,-1.84851432812322,
12.5024036458141));
#419355=CARTESIAN_POINT('Ctrl Pts',(2.03761561947291,-1.8467889979965,12.4998248032393));
#419356=CARTESIAN_POINT('Ctrl Pts',(2.03939251656006,-1.84482469719994,
12.4976950015772));
#419357=CARTESIAN_POINT('Ctrl Pts',(2.04121947944228,-1.84280505032742,
12.495505190692));
#419358=CARTESIAN_POINT('Ctrl Pts',(2.04331646239371,-1.84048056184307,
12.4937456938368));
#419359=CARTESIAN_POINT('Ctrl Pts',(2.04551946362644,-1.83802886917627,
12.4925987732155));
#419360=CARTESIAN_POINT('Ctrl Pts',(2.04772194936537,-1.8355777501961,12.4914521209692));
#419361=CARTESIAN_POINT('Ctrl Pts',(2.0500852218892,-1.83293828653202,12.4908873016276));
#419362=CARTESIAN_POINT('Ctrl Pts',(2.05240800005387,-1.83033368578379,
12.4908873016278));
#419363=CARTESIAN_POINT('',(2.02885474386084,-1.8564073982597,13.7435492065112));
#419364=CARTESIAN_POINT('',(2.02885474386084,-1.8564073982597,14.));
#419365=CARTESIAN_POINT('',(1.97702009390622,-1.91151551086854,13.7435492065112));
#419366=CARTESIAN_POINT('Origin',(0.,2.5406128344257E-15,13.7435492065112));
#419367=CARTESIAN_POINT('',(1.97702009390622,-1.91151551086855,12.5369868989719));
#419368=CARTESIAN_POINT('',(1.97702009390622,-1.91151551086855,14.));
#419369=CARTESIAN_POINT('Ctrl Pts',(1.95243575099292,-1.93661938393808,
12.4908873016278));
#419370=CARTESIAN_POINT('Ctrl Pts',(1.95397189622228,-1.93507069301338,
12.4908873016278));
#419371=CARTESIAN_POINT('Ctrl Pts',(1.95551481836595,-1.9335114060327,12.4911020829134));
#419372=CARTESIAN_POINT('Ctrl Pts',(1.95701538486413,-1.93199140355362,
12.4915448903141));
#419373=CARTESIAN_POINT('Ctrl Pts',(1.95958267128567,-1.92939086453722,
12.4923024798169));
#419374=CARTESIAN_POINT('Ctrl Pts',(1.96208474988803,-1.92684541091315,
12.4937722312795));
#419375=CARTESIAN_POINT('Ctrl Pts',(1.9642760202528,-1.92460897749643,12.4958030942394));
#419376=CARTESIAN_POINT('Ctrl Pts',(1.9664518238919,-1.92238832958143,12.4978196226833));
#419377=CARTESIAN_POINT('Ctrl Pts',(1.96838592294445,-1.92040674778198,
12.5004326847668));
#419378=CARTESIAN_POINT('Ctrl Pts',(1.96997984158126,-1.91877028947278,
12.5033504258767));
#419379=CARTESIAN_POINT('Ctrl Pts',(1.97188429280756,-1.91681501085207,
12.5068366111226));
#419380=CARTESIAN_POINT('Ctrl Pts',(1.97336457368722,-1.9152897070531,12.5108395010833));
#419381=CARTESIAN_POINT('Ctrl Pts',(1.97444350192213,-1.91417680941899,
12.5149868989719));
#419382=CARTESIAN_POINT('Ctrl Pts',(1.97625566475848,-1.91230759173804,
12.5219528491417));
#419383=CARTESIAN_POINT('Ctrl Pts',(1.9770200939332,-1.91151551084106,12.5295503425868));
#419384=CARTESIAN_POINT('Ctrl Pts',(1.97702009390622,-1.91151551086855,
12.5369868989719));
#419385=CARTESIAN_POINT('',(1.87078946006577,-2.01560085237798,12.5369868989719));
#419386=CARTESIAN_POINT('Ctrl Pts',(1.87078946006576,-2.01560085237798,
12.5369868989719));
#419387=CARTESIAN_POINT('Ctrl Pts',(1.87078946006576,-2.01560085237798,
12.5309445149785));
#419388=CARTESIAN_POINT('Ctrl Pts',(1.87132026727296,-2.01510873201969,
12.5248274368704));
#419389=CARTESIAN_POINT('Ctrl Pts',(1.87253354338274,-2.01398066746096,
12.5190199595513));
#419390=CARTESIAN_POINT('Ctrl Pts',(1.87355261918778,-2.01303316401217,
12.5141420429941));
#419391=CARTESIAN_POINT('Ctrl Pts',(1.87508470058604,-2.01160774012995,
12.5093757677094));
#419392=CARTESIAN_POINT('Ctrl Pts',(1.87719442291575,-2.00963705642934,
12.5051960112707));
#419393=CARTESIAN_POINT('Ctrl Pts',(1.87860386287782,-2.00832050385694,
12.5024036458141));
#419394=CARTESIAN_POINT('Ctrl Pts',(1.88030517350127,-2.00672854924258,
12.4998248032393));
#419395=CARTESIAN_POINT('Ctrl Pts',(1.88223626686055,-2.00491561810338,
12.4976950015772));
#419396=CARTESIAN_POINT('Ctrl Pts',(1.88422177064409,-2.00305160587482,
12.495505190692));
#419397=CARTESIAN_POINT('Ctrl Pts',(1.88650124344871,-2.00090577551213,
12.4937456938368));
#419398=CARTESIAN_POINT('Ctrl Pts',(1.88889675008932,-1.99864180570256,
12.4925987732155));
#419399=CARTESIAN_POINT('Ctrl Pts',(1.89129169619061,-1.99637836565319,
12.4914521209692));
#419400=CARTESIAN_POINT('Ctrl Pts',(1.89386224591228,-1.99394031323696,
12.4908873016276));
#419401=CARTESIAN_POINT('Ctrl Pts',(1.89638959436514,-1.9915337070669,12.4908873016278));
#419402=CARTESIAN_POINT('',(1.87078946006577,-2.01560085237798,13.7435492065112));
#419403=CARTESIAN_POINT('',(1.87078946006577,-2.01560085237798,14.));
#419404=CARTESIAN_POINT('',(1.81463546285643,-2.0663005921075,13.7435492065112));
#419405=CARTESIAN_POINT('Origin',(0.,2.5406128344257E-15,13.7435492065112));
#419406=CARTESIAN_POINT('',(1.81463546285643,-2.0663005921075,12.5369868989719));
#419407=CARTESIAN_POINT('',(1.81463546285644,-2.06630059210751,14.));
#419408=CARTESIAN_POINT('Ctrl Pts',(1.78808672360795,-2.08931708193299,
12.4908873016278));
#419409=CARTESIAN_POINT('Ctrl Pts',(1.7897439901285,-2.08789875424664,12.4908873016278));
#419410=CARTESIAN_POINT('Ctrl Pts',(1.79140887469066,-2.08647041814326,
12.4911020829134));
#419411=CARTESIAN_POINT('Ctrl Pts',(1.79302834249066,-2.08507778344723,
12.4915448903141));
#419412=CARTESIAN_POINT('Ctrl Pts',(1.79579905455048,-2.08269515518675,
12.4923024798169));
#419413=CARTESIAN_POINT('Ctrl Pts',(1.7985002857939,-2.08036211398388,12.4937722312795));
#419414=CARTESIAN_POINT('Ctrl Pts',(1.80086655497279,-2.07831173099236,
12.4958030942394));
#419415=CARTESIAN_POINT('Ctrl Pts',(1.80321612222533,-2.07627582029587,
12.4978196226833));
#419416=CARTESIAN_POINT('Ctrl Pts',(1.8053053030356,-2.07445847907447,12.5004326847668));
#419417=CARTESIAN_POINT('Ctrl Pts',(1.80702730458398,-2.07295738511142,
12.5033504258767));
#419418=CARTESIAN_POINT('Ctrl Pts',(1.80908479226544,-2.07116384297402,
12.5068366111226));
#419419=CARTESIAN_POINT('Ctrl Pts',(1.81068447405243,-2.06976427113156,
12.5108395010833));
#419420=CARTESIAN_POINT('Ctrl Pts',(1.81185052373146,-2.06874301923995,
12.5149868989719));
#419421=CARTESIAN_POINT('Ctrl Pts',(1.81380901533943,-2.06702772932109,
12.5219528491417));
#419422=CARTESIAN_POINT('Ctrl Pts',(1.81463546288556,-2.06630059208231,
12.5295503425868));
#419423=CARTESIAN_POINT('Ctrl Pts',(1.81463546285643,-2.0663005921075,12.5369868989719));
#419424=CARTESIAN_POINT('',(1.70027438107248,-2.16138081537442,12.5369868989719));
#419425=CARTESIAN_POINT('Ctrl Pts',(1.70027438107248,-2.16138081537442,
12.5369868989719));
#419426=CARTESIAN_POINT('Ctrl Pts',(1.70027438107248,-2.16138081537442,
12.5309445149785));
#419427=CARTESIAN_POINT('Ctrl Pts',(1.70084353444031,-2.16093359822118,
12.5248274368704));
#419428=CARTESIAN_POINT('Ctrl Pts',(1.70214472120789,-2.15990818047066,
12.5190199595513));
#419429=CARTESIAN_POINT('Ctrl Pts',(1.70323763644954,-2.15904689390019,
12.5141420429941));
#419430=CARTESIAN_POINT('Ctrl Pts',(1.70488080525272,-2.15775109185545,
12.5093757677094));
#419431=CARTESIAN_POINT('Ctrl Pts',(1.70714413667196,-2.15595892739786,
12.5051960112707));
#419432=CARTESIAN_POINT('Ctrl Pts',(1.70865619809574,-2.15476163798706,
12.5024036458141));
#419433=CARTESIAN_POINT('Ctrl Pts',(1.7104816068285,-2.15331365308035,12.4998248032393));
#419434=CARTESIAN_POINT('Ctrl Pts',(1.71255404535221,-2.15166415635614,
12.4976950015772));
#419435=CARTESIAN_POINT('Ctrl Pts',(1.71468487683697,-2.14996818346538,
12.495505190692));
#419436=CARTESIAN_POINT('Ctrl Pts',(1.71713166997936,-2.14801529137137,
12.4937456938368));
#419437=CARTESIAN_POINT('Ctrl Pts',(1.71970374032639,-2.14595411076458,
12.4925987732155));
#419438=CARTESIAN_POINT('Ctrl Pts',(1.72227520881887,-2.14389341246611,
12.4914521209692));
#419439=CARTESIAN_POINT('Ctrl Pts',(1.7250359291541,-2.14167299613431,12.4908873016276));
#419440=CARTESIAN_POINT('Ctrl Pts',(1.72775102880817,-2.13948040010941,
12.4908873016278));
#419441=CARTESIAN_POINT('',(1.70027438107248,-2.16138081537442,13.7435492065112));
#419442=CARTESIAN_POINT('',(1.70027438107249,-2.16138081537442,14.));
#419443=CARTESIAN_POINT('',(1.64017473219511,-2.20733478382159,13.7435492065112));
#419444=CARTESIAN_POINT('Origin',(0.,2.5406128344257E-15,13.7435492065112));
#419445=CARTESIAN_POINT('',(1.64017473219511,-2.20733478382159,12.5369868989719));
#419446=CARTESIAN_POINT('',(1.64017473219511,-2.20733478382159,14.));
#419447=CARTESIAN_POINT('Ctrl Pts',(1.61183827409092,-2.22811071946068,
12.4908873016278));
#419448=CARTESIAN_POINT('Ctrl Pts',(1.61360563306738,-2.22683219374945,
12.4908873016278));
#419449=CARTESIAN_POINT('Ctrl Pts',(1.61538140051596,-2.22554431386447,
12.4911020829134));
#419450=CARTESIAN_POINT('Ctrl Pts',(1.61710899232677,-2.22428831470561,
12.4915448903141));
#419451=CARTESIAN_POINT('Ctrl Pts',(1.62006469139325,-2.22213945319902,
12.4923024798169));
#419452=CARTESIAN_POINT('Ctrl Pts',(1.62294709902947,-2.22003435042165,
12.4937722312795));
#419453=CARTESIAN_POINT('Ctrl Pts',(1.62547261989151,-2.21818366281583,
12.4958030942394));
#419454=CARTESIAN_POINT('Ctrl Pts',(1.62798031477508,-2.21634603798763,
12.4978196226833));
#419455=CARTESIAN_POINT('Ctrl Pts',(1.63021067418946,-2.21470503145028,
12.5004326847668));
#419456=CARTESIAN_POINT('Ctrl Pts',(1.63204929901321,-2.21334929136603,
12.5033504258767));
#419457=CARTESIAN_POINT('Ctrl Pts',(1.63424613090877,-2.21172942143895,
12.5068366111226));
#419458=CARTESIAN_POINT('Ctrl Pts',(1.63595456798473,-2.21046489547271,
12.5108395010833));
#419459=CARTESIAN_POINT('Ctrl Pts',(1.63719997923966,-2.20954208558644,
12.5149868989719));
#419460=CARTESIAN_POINT('Ctrl Pts',(1.63929176618073,-2.20799213840108,
12.5219528491417));
#419461=CARTESIAN_POINT('Ctrl Pts',(1.6401747322262,-2.20733478379885,12.5295503425868));
#419462=CARTESIAN_POINT('Ctrl Pts',(1.64017473219511,-2.20733478382159,
12.5369868989719));
#419463=CARTESIAN_POINT('',(1.51844425659869,-2.29277714564727,12.5369868989719));
#419464=CARTESIAN_POINT('Ctrl Pts',(1.51844425659869,-2.29277714564727,
12.5369868989719));
#419465=CARTESIAN_POINT('Ctrl Pts',(1.51844425659869,-2.29277714564727,
12.5309445149785));
#419466=CARTESIAN_POINT('Ctrl Pts',(1.51904796850539,-2.29237780785546,
12.5248274368704));
#419467=CARTESIAN_POINT('Ctrl Pts',(1.52042840674753,-2.2914618608991,12.5190199595513));
#419468=CARTESIAN_POINT('Ctrl Pts',(1.52158788825515,-2.29069252292696,
12.5141420429941));
#419469=CARTESIAN_POINT('Ctrl Pts',(1.52333120944598,-2.28953496606852,
12.5093757677094));
#419470=CARTESIAN_POINT('Ctrl Pts',(1.52573308785756,-2.28793324741274,
12.5051960112707));
#419471=CARTESIAN_POINT('Ctrl Pts',(1.52733770822377,-2.28686318892701,
12.5024036458141));
#419472=CARTESIAN_POINT('Ctrl Pts',(1.52927506727189,-2.28556880982862,
12.4998248032393));
#419473=CARTESIAN_POINT('Ctrl Pts',(1.53147505922358,-2.28409372464795,
12.4976950015772));
#419474=CARTESIAN_POINT('Ctrl Pts',(1.5337370380776,-2.28257707751476,12.495505190692));
#419475=CARTESIAN_POINT('Ctrl Pts',(1.53633486855308,-2.28083011986411,
12.4937456938368));
#419476=CARTESIAN_POINT('Ctrl Pts',(1.53906638590273,-2.27898544527698,
12.4925987732155));
#419477=CARTESIAN_POINT('Ctrl Pts',(1.54179726408785,-2.27714120233658,
12.4914521209692));
#419478=CARTESIAN_POINT('Ctrl Pts',(1.54472978289828,-2.27515319859355,
12.4908873016276));
#419479=CARTESIAN_POINT('Ctrl Pts',(1.54761456521333,-2.27318920407861,
12.4908873016278));
#419480=CARTESIAN_POINT('',(1.51844425659869,-2.29277714564727,13.7435492065112));
#419481=CARTESIAN_POINT('',(1.51844425659869,-2.29277714564727,14.));
#419482=CARTESIAN_POINT('',(1.45479890930081,-2.33367952673394,13.7435492065112));
#419483=CARTESIAN_POINT('Origin',(0.,2.5406128344257E-15,13.7435492065112));
#419484=CARTESIAN_POINT('',(1.45479890930082,-2.33367952673394,12.5369868989719));
#419485=CARTESIAN_POINT('',(1.45479890930082,-2.33367952673394,14.));
#419486=CARTESIAN_POINT('Ctrl Pts',(1.42486330679441,-2.35207664776276,
12.4908873016278));
#419487=CARTESIAN_POINT('Ctrl Pts',(1.42672899674439,-2.3509464324043,12.4908873016278));
#419488=CARTESIAN_POINT('Ctrl Pts',(1.42860382963999,-2.34980757936588,
12.4911020829134));
#419489=CARTESIAN_POINT('Ctrl Pts',(1.43042804862314,-2.34869657421136,
12.4915448903141));
#419490=CARTESIAN_POINT('Ctrl Pts',(1.43354906500665,-2.34679577977746,
12.4923024798169));
#419491=CARTESIAN_POINT('Ctrl Pts',(1.43659346708843,-2.34493262453724,
12.4937722312795));
#419492=CARTESIAN_POINT('Ctrl Pts',(1.43926143270895,-2.34329394833781,
12.4958030942394));
#419493=CARTESIAN_POINT('Ctrl Pts',(1.44191056692785,-2.34166683846795,
12.4978196226833));
#419494=CARTESIAN_POINT('Ctrl Pts',(1.44426726227242,-2.34021308724239,
12.5004326847668));
#419495=CARTESIAN_POINT('Ctrl Pts',(1.44621027462669,-2.33901172326352,
12.5033504258767));
#419496=CARTESIAN_POINT('Ctrl Pts',(1.44853183118254,-2.33757630551388,
12.5068366111226));
#419497=CARTESIAN_POINT('Ctrl Pts',(1.4503376541806,-2.33645524063552,12.5108395010833));
#419498=CARTESIAN_POINT('Ctrl Pts',(1.45165413900499,-2.33563701390213,
12.5149868989719));
#419499=CARTESIAN_POINT('Ctrl Pts',(1.45386530078219,-2.33426272409307,
12.5219528491417));
#419500=CARTESIAN_POINT('Ctrl Pts',(1.45479890933365,-2.33367952671381,
12.5295503425868));
#419501=CARTESIAN_POINT('Ctrl Pts',(1.45479890930082,-2.33367952673394,
12.5369868989719));
#419502=CARTESIAN_POINT('',(1.3265091361229,-2.40891542229745,12.5369868989719));
#419503=CARTESIAN_POINT('Ctrl Pts',(1.3265091361229,-2.40891542229744,12.5369868989719));
#419504=CARTESIAN_POINT('Ctrl Pts',(1.3265091361229,-2.40891542229744,12.5309445149785));
#419505=CARTESIAN_POINT('Ctrl Pts',(1.32714338896534,-2.40856662139417,
12.5248274368704));
#419506=CARTESIAN_POINT('Ctrl Pts',(1.32859389209328,-2.40776624070785,
12.5190199595513));
#419507=CARTESIAN_POINT('Ctrl Pts',(1.32981222370875,-2.40709397115132,
12.5141420429941));
#419508=CARTESIAN_POINT('Ctrl Pts',(1.33164409577233,-2.40608236282909,
12.5093757677094));
#419509=CARTESIAN_POINT('Ctrl Pts',(1.33416853707172,-2.4046817491485,12.5051960112707));
#419510=CARTESIAN_POINT('Ctrl Pts',(1.33585503789656,-2.40374604265052,
12.5024036458141));
#419511=CARTESIAN_POINT('Ctrl Pts',(1.33789145445521,-2.40261388323979,
12.4998248032393));
#419512=CARTESIAN_POINT('Ctrl Pts',(1.34020435925141,-2.40132302605116,
12.4976950015772));
#419513=CARTESIAN_POINT('Ctrl Pts',(1.34258243237862,-2.39999579771198,
12.495505190692));
#419514=CARTESIAN_POINT('Ctrl Pts',(1.34531401205399,-2.39846640021964,
12.4937456938368));
#419515=CARTESIAN_POINT('Ctrl Pts',(1.34818679860896,-2.39685050765718,
12.4925987732155));
#419516=CARTESIAN_POINT('Ctrl Pts',(1.35105891294296,-2.39523499320736,
12.4914521209692));
#419517=CARTESIAN_POINT('Ctrl Pts',(1.35414371479976,-2.39349263189001,
12.4908873016276));
#419518=CARTESIAN_POINT('Ctrl Pts',(1.35717898202543,-2.39177030894448,
12.4908873016278));
#419519=CARTESIAN_POINT('',(1.3265091361229,-2.40891542229744,13.7435492065112));
#419520=CARTESIAN_POINT('',(1.32650913612291,-2.40891542229744,14.));
#419521=CARTESIAN_POINT('',(1.25974163969005,-2.4444940174259,13.7435492065112));
#419522=CARTESIAN_POINT('Origin',(0.,2.5406128344257E-15,13.7435492065112));
#419523=CARTESIAN_POINT('',(1.25974163969005,-2.4444940174259,12.5369868989719));
#419524=CARTESIAN_POINT('',(1.25974163969005,-2.44449401742591,14.));
#419525=CARTESIAN_POINT('Ctrl Pts',(1.22840610927708,-2.46038989403931,
12.4908873016278));
#419526=CARTESIAN_POINT('Ctrl Pts',(1.23035771434178,-2.45941551043036,
12.4908873016278));
#419527=CARTESIAN_POINT('Ctrl Pts',(1.23231913598081,-2.45843326311756,
12.4911020829134));
#419528=CARTESIAN_POINT('Ctrl Pts',(1.23422784225995,-2.4574746455234,12.4915448903141));
#419529=CARTESIAN_POINT('Ctrl Pts',(1.23749340611138,-2.45583456763553,
12.4923024798169));
#419530=CARTESIAN_POINT('Ctrl Pts',(1.24067954264514,-2.45422575892319,
12.4937722312795));
#419531=CARTESIAN_POINT('Ctrl Pts',(1.24347219815314,-2.45280999924988,
12.4958030942394));
#419532=CARTESIAN_POINT('Ctrl Pts',(1.2462451421562,-2.45140423248609,12.4978196226833));
#419533=CARTESIAN_POINT('Ctrl Pts',(1.24871249001229,-2.45014741104688,
12.5004326847668));
#419534=CARTESIAN_POINT('Ctrl Pts',(1.25074695947043,-2.44910841805247,
12.5033504258767));
#419535=CARTESIAN_POINT('Ctrl Pts',(1.25317779111071,-2.44786700494856,
12.5068366111226));
#419536=CARTESIAN_POINT('Ctrl Pts',(1.25506898257676,-2.44689686165989,
12.5108395010833));
#419537=CARTESIAN_POINT('Ctrl Pts',(1.25644777998133,-2.44618866324329,
12.5149868989719));
#419538=CARTESIAN_POINT('Ctrl Pts',(1.25876360167784,-2.44499917648246,
12.5219528491417));
#419539=CARTESIAN_POINT('Ctrl Pts',(1.25974163972441,-2.44449401740852,
12.5295503425868));
#419540=CARTESIAN_POINT('Ctrl Pts',(1.25974163969005,-2.4444940174259,12.5369868989719));
#419541=CARTESIAN_POINT('',(1.12574631620482,-2.5090227642553,12.5369868989719));
#419542=CARTESIAN_POINT('Ctrl Pts',(1.12574631620482,-2.50902276425529,
12.5369868989719));
#419543=CARTESIAN_POINT('Ctrl Pts',(1.12574631620482,-2.50902276425529,
12.5309445149785));
#419544=CARTESIAN_POINT('Ctrl Pts',(1.12640688913497,-2.50872682145303,
12.5248274368704));
#419545=CARTESIAN_POINT('Ctrl Pts',(1.12791780428972,-2.50804733343815,
12.5190199595513));
#419546=CARTESIAN_POINT('Ctrl Pts',(1.12918687821715,-2.50747660614022,
12.5141420429941));
#419547=CARTESIAN_POINT('Ctrl Pts',(1.13109511034713,-2.50661767844068,
12.5093757677094));
#419548=CARTESIAN_POINT('Ctrl Pts',(1.13372531479398,-2.50542749058824,
12.5051960112707));
#419549=CARTESIAN_POINT('Ctrl Pts',(1.13548247269271,-2.50463236305038,
12.5024036458141));
#419550=CARTESIAN_POINT('Ctrl Pts',(1.13760439474569,-2.50366995766138,
12.4998248032393));
#419551=CARTESIAN_POINT('Ctrl Pts',(1.14001482038658,-2.50257191890641,
12.4976950015772));
#419552=CARTESIAN_POINT('Ctrl Pts',(1.14249316210267,-2.50144294184686,
12.495505190692));
#419553=CARTESIAN_POINT('Ctrl Pts',(1.14534031276587,-2.5001412824008,12.4937456938368));
#419554=CARTESIAN_POINT('Ctrl Pts',(1.14833525060562,-2.49876492536143,
12.4925987732155));
#419555=CARTESIAN_POINT('Ctrl Pts',(1.15132948764148,-2.49738889038429,
12.4914521209692));
#419556=CARTESIAN_POINT('Ctrl Pts',(1.15454604369723,-2.49590376661972,
12.4908873016276));
#419557=CARTESIAN_POINT('Ctrl Pts',(1.15771159663093,-2.49443457701866,
12.4908873016278));
#419558=CARTESIAN_POINT('',(1.12574631620482,-2.50902276425529,13.7435492065112));
#419559=CARTESIAN_POINT('',(1.12574631620482,-2.5090227642553,14.));
#419560=CARTESIAN_POINT('',(1.05630099730988,-2.53904080374502,13.7435492065112));
#419561=CARTESIAN_POINT('Origin',(0.,2.5406128344257E-15,13.7435492065112));
#419562=CARTESIAN_POINT('',(1.05630099730988,-2.53904080374502,12.5369868989719));
#419563=CARTESIAN_POINT('',(1.05630099730988,-2.53904080374502,14.));
#419564=CARTESIAN_POINT('Ctrl Pts',(1.02377407177525,-2.55232965150678,
12.4908873016278));
#419565=CARTESIAN_POINT('Ctrl Pts',(1.02579860434496,-2.5515175840095,12.4908873016278));
#419566=CARTESIAN_POINT('Ctrl Pts',(1.02783356179003,-2.55069847911614,
12.4911020829134));
#419567=CARTESIAN_POINT('Ctrl Pts',(1.02981405323977,-2.54989862852426,
12.4915448903141));
#419568=CARTESIAN_POINT('Ctrl Pts',(1.03320243277048,-2.54853018163017,
12.4923024798169));
#419569=CARTESIAN_POINT('Ctrl Pts',(1.03650910054327,-2.54718642580225,
12.4937722312795));
#419570=CARTESIAN_POINT('Ctrl Pts',(1.03940786127709,-2.54600300430212,
12.4958030942394));
#419571=CARTESIAN_POINT('Ctrl Pts',(1.04228616157949,-2.54482793579027,
12.4978196226833));
#419572=CARTESIAN_POINT('Ctrl Pts',(1.04484774215418,-2.54377640807673,
12.5004326847668));
#419573=CARTESIAN_POINT('Ctrl Pts',(1.04696012965761,-2.54290670039373,
12.5033504258767));
#419574=CARTESIAN_POINT('Ctrl Pts',(1.04948405959883,-2.54186755333494,
12.5068366111226));
#419575=CARTESIAN_POINT('Ctrl Pts',(1.05144803396569,-2.54105478777947,
12.5108395010833));
#419576=CARTESIAN_POINT('Ctrl Pts',(1.05287996828117,-2.54046133062329,
12.5149868989719));
#419577=CARTESIAN_POINT('Ctrl Pts',(1.0552850384857,-2.53946456274884,12.5219528491417));
#419578=CARTESIAN_POINT('Ctrl Pts',(1.05630099734555,-2.53904080373049,
12.5295503425868));
#419579=CARTESIAN_POINT('Ctrl Pts',(1.05630099730988,-2.53904080374502,
12.5369868989719));
#419580=CARTESIAN_POINT('',(0.91749184028746,-2.59243297367665,12.5369868989719));
#419581=CARTESIAN_POINT('Ctrl Pts',(0.917491840287459,-2.59243297367664,
12.5369868989719));
#419582=CARTESIAN_POINT('Ctrl Pts',(0.91749184028746,-2.59243297367664,
12.5309445149785));
#419583=CARTESIAN_POINT('Ctrl Pts',(0.918174337301462,-2.59219185842591,
12.5248274368704));
#419584=CARTESIAN_POINT('Ctrl Pts',(0.919735609591948,-2.59163778496311,
12.5190199595513));
#419585=CARTESIAN_POINT('Ctrl Pts',(0.921046980353731,-2.59117239801977,
12.5141420429941));
#419586=CARTESIAN_POINT('Ctrl Pts',(0.923018873580121,-2.59047186696506,
12.5093757677094));
#419587=CARTESIAN_POINT('Ctrl Pts',(0.925737337597789,-2.58950002544455,
12.5051960112707));
#419588=CARTESIAN_POINT('Ctrl Pts',(0.927553458974509,-2.58885076830938,
12.5024036458141));
#419589=CARTESIAN_POINT('Ctrl Pts',(0.929746765480642,-2.58806452159121,
12.4998248032393));
#419590=CARTESIAN_POINT('Ctrl Pts',(0.932238670981287,-2.58716660853665,
12.4976950015772));
#419591=CARTESIAN_POINT('Ctrl Pts',(0.934800788331022,-2.58624339591279,
12.495505190692));
#419592=CARTESIAN_POINT('Ctrl Pts',(0.937744562664136,-2.58517813684187,
12.4937456938368));
#419593=CARTESIAN_POINT('Ctrl Pts',(0.940841720971482,-2.58405047475459,
12.4925987732155));
#419594=CARTESIAN_POINT('Ctrl Pts',(0.943938154555725,-2.58292307653588,
12.4914521209692));
#419595=CARTESIAN_POINT('Ctrl Pts',(0.947265059160576,-2.58170507357772,
12.4908873016276));
#419596=CARTESIAN_POINT('Ctrl Pts',(0.950539831569806,-2.58049879453551,
12.4908873016278));
#419597=CARTESIAN_POINT('',(0.917491840287462,-2.59243297367664,13.7435492065112));
#419598=CARTESIAN_POINT('',(0.917491840287462,-2.59243297367665,14.));
#419599=CARTESIAN_POINT('',(0.845830846070012,-2.61669069242746,13.7435492065112));
#419600=CARTESIAN_POINT('Origin',(0.,2.5406128344257E-15,13.7435492065112));
#419601=CARTESIAN_POINT('',(0.845830846070013,-2.61669069242746,12.5369868989719));
#419602=CARTESIAN_POINT('',(0.845830846070013,-2.61669069242746,14.));
#419603=CARTESIAN_POINT('Ctrl Pts',(0.812328986736591,-2.62728407624823,
12.4908873016278));
#419604=CARTESIAN_POINT('Ctrl Pts',(0.814412973881085,-2.62663972903783,
12.4908873016278));
#419605=CARTESIAN_POINT('Ctrl Pts',(0.81650792482613,-2.62598921757183,
12.4911020829134));
#419606=CARTESIAN_POINT('Ctrl Pts',(0.818547021602644,-2.62535345685594,
12.4915448903141));
#419607=CARTESIAN_POINT('Ctrl Pts',(0.822035667705896,-2.62426574774394,
12.4923024798169));
#419608=CARTESIAN_POINT('Ctrl Pts',(0.825440861389251,-2.62319598727377,
12.4937722312795));
#419609=CARTESIAN_POINT('Ctrl Pts',(0.828426436574467,-2.62225277942165,
12.4958030942394));
#419610=CARTESIAN_POINT('Ctrl Pts',(0.83139093856257,-2.62131622904882,
12.4978196226833));
#419611=CARTESIAN_POINT('Ctrl Pts',(0.834029704959774,-2.62047699280439,
12.5004326847668));
#419612=CARTESIAN_POINT('Ctrl Pts',(0.83620595291819,-2.61978235819394,
12.5033504258767));
#419613=CARTESIAN_POINT('Ctrl Pts',(0.838806184822998,-2.61895239253249,
12.5068366111226));
#419614=CARTESIAN_POINT('Ctrl Pts',(0.840829872165285,-2.61830241353091,
12.5108395010833));
#419615=CARTESIAN_POINT('Ctrl Pts',(0.842305414105079,-2.6178276469946,
12.5149868989719));
#419616=CARTESIAN_POINT('Ctrl Pts',(0.844783727472212,-2.61703023133227,
12.5219528491417));
#419617=CARTESIAN_POINT('Ctrl Pts',(0.845830846106748,-2.61669069241589,
12.5295503425868));
#419618=CARTESIAN_POINT('Ctrl Pts',(0.845830846070013,-2.61669069242746,
12.5369868989719));
#419619=CARTESIAN_POINT('',(0.703131607548487,-2.65859096937951,12.5369868989719));
#419620=CARTESIAN_POINT('Ctrl Pts',(0.703131607548485,-2.65859096937951,
12.5369868989719));
#419621=CARTESIAN_POINT('Ctrl Pts',(0.703131607548487,-2.65859096937951,
12.5309445149785));
#419622=CARTESIAN_POINT('Ctrl Pts',(0.703831486741316,-2.65840628626251,
12.5248274368704));
#419623=CARTESIAN_POINT('Ctrl Pts',(0.705432726158037,-2.65798131461928,
12.5190199595513));
#419624=CARTESIAN_POINT('Ctrl Pts',(0.706777666798115,-2.65762436510386,
12.5141420429941));
#419625=CARTESIAN_POINT('Ctrl Pts',(0.708800098496836,-2.65708689261255,
12.5093757677094));
#419626=CARTESIAN_POINT('Ctrl Pts',(0.7115887311558,-2.65633986486896,12.5051960112707));
#419627=CARTESIAN_POINT('Ctrl Pts',(0.713451730022383,-2.6558407988356,
12.5024036458141));
#419628=CARTESIAN_POINT('Ctrl Pts',(0.715701824888742,-2.65523594313044,
12.4998248032393));
#419629=CARTESIAN_POINT('Ctrl Pts',(0.718258627029167,-2.65454413123952,
12.4976950015772));
#419630=CARTESIAN_POINT('Ctrl Pts',(0.720887469544312,-2.65383282687905,
12.495505190692));
#419631=CARTESIAN_POINT('Ctrl Pts',(0.723908277214839,-2.65301105730662,
12.4937456938368));
#419632=CARTESIAN_POINT('Ctrl Pts',(0.727087044912233,-2.65213959457657,
12.4925987732155));
#419633=CARTESIAN_POINT('Ctrl Pts',(0.730265068790241,-2.65126833576544,
12.4914521209692));
#419634=CARTESIAN_POINT('Ctrl Pts',(0.733680181942947,-2.65032555922241,
12.4908873016276));
#419635=CARTESIAN_POINT('Ctrl Pts',(0.737042380757624,-2.64939021832706,
12.4908873016278));
#419636=CARTESIAN_POINT('',(0.703131607548488,-2.65859096937951,13.7435492065112));
#419637=CARTESIAN_POINT('',(0.703131607548488,-2.65859096937951,14.));
#419638=CARTESIAN_POINT('',(0.629731830101817,-2.67692693627537,13.7435492065112));
#419639=CARTESIAN_POINT('Origin',(0.,2.5406128344257E-15,13.7435492065112));
#419640=CARTESIAN_POINT('',(0.629731830101817,-2.67692693627537,12.5369868989719));
#419641=CARTESIAN_POINT('',(0.629731830101817,-2.67692693627537,14.));
#419642=CARTESIAN_POINT('Ctrl Pts',(0.595477986316048,-2.6847543589336,
12.4908873016278));
#419643=CARTESIAN_POINT('Ctrl Pts',(0.597607559444711,-2.68428202003446,
12.4908873016278));
#419644=CARTESIAN_POINT('Ctrl Pts',(0.599748562336841,-2.6838044310423,
12.4911020829134));
#419645=CARTESIAN_POINT('Ctrl Pts',(0.601832694587503,-2.68333699108509,
12.4915448903141));
#419646=CARTESIAN_POINT('Ctrl Pts',(0.605398390899067,-2.68253725827985,
12.4923024798169));
#419647=CARTESIAN_POINT('Ctrl Pts',(0.60887944949084,-2.68174861224686,
12.4937722312795));
#419648=CARTESIAN_POINT('Ctrl Pts',(0.611931970617183,-2.68105189493538,
12.4958030942394));
#419649=CARTESIAN_POINT('Ctrl Pts',(0.614962946019369,-2.68036009528978,
12.4978196226833));
#419650=CARTESIAN_POINT('Ctrl Pts',(0.61766133768408,-2.67973873549321,
12.5004326847668));
#419651=CARTESIAN_POINT('Ctrl Pts',(0.619886963526366,-2.67922379663403,
12.5033504258767));
#419652=CARTESIAN_POINT('Ctrl Pts',(0.622546193280448,-2.67860853565447,
12.5068366111226));
#419653=CARTESIAN_POINT('Ctrl Pts',(0.624616126292785,-2.67812566870979,
12.5108395010833));
#419654=CARTESIAN_POINT('Ctrl Pts',(0.626125456368726,-2.67777275228632,
12.5149868989719));
#419655=CARTESIAN_POINT('Ctrl Pts',(0.628660520131902,-2.67717999550579,
12.5219528491417));
#419656=CARTESIAN_POINT('Ctrl Pts',(0.629731830139373,-2.67692693626683,
12.5295503425868));
#419657=CARTESIAN_POINT('Ctrl Pts',(0.629731830101817,-2.67692693627537,
12.5369868989719));
#419658=CARTESIAN_POINT('',(0.484092149969828,-2.70705648081779,12.5369868989719));
#419659=CARTESIAN_POINT('Ctrl Pts',(0.484092149969827,-2.70705648081778,
12.5369868989719));
#419660=CARTESIAN_POINT('Ctrl Pts',(0.484092149969828,-2.70705648081778,
12.5309445149785));
#419661=CARTESIAN_POINT('Ctrl Pts',(0.484804753760929,-2.70692945887021,
12.5248274368704));
#419662=CARTESIAN_POINT('Ctrl Pts',(0.486435304319751,-2.7066364171627,
12.5190199595513));
#419663=CARTESIAN_POINT('Ctrl Pts',(0.487804864480063,-2.70639028051533,
12.5141420429941));
#419664=CARTESIAN_POINT('Ctrl Pts',(0.489864375701838,-2.70601944337819,
12.5093757677094));
#419665=CARTESIAN_POINT('Ctrl Pts',(0.492704619111845,-2.7055022007579,
12.5051960112707));
#419666=CARTESIAN_POINT('Ctrl Pts',(0.494602097518208,-2.70515664702846,
12.5024036458141));
#419667=CARTESIAN_POINT('Ctrl Pts',(0.496894006734697,-2.70473720755122,
12.4998248032393));
#419668=CARTESIAN_POINT('Ctrl Pts',(0.499498690418499,-2.70425610071794,
12.4976950015772));
#419669=CARTESIAN_POINT('Ctrl Pts',(0.502176763585845,-2.70376143823402,
12.495505190692));
#419670=CARTESIAN_POINT('Ctrl Pts',(0.505254501617137,-2.70318862690101,
12.4937456938368));
#419671=CARTESIAN_POINT('Ctrl Pts',(0.508493724530012,-2.70257916296888,
12.4925987732155));
#419672=CARTESIAN_POINT('Ctrl Pts',(0.511732189477214,-2.70196984164896,
12.4914521209692));
#419673=CARTESIAN_POINT('Ctrl Pts',(0.515212784163198,-2.70130856554342,
12.4908873016276));
#419674=CARTESIAN_POINT('Ctrl Pts',(0.518640034504933,-2.70065038733426,
12.4908873016278));
#419675=CARTESIAN_POINT('',(0.484092149969829,-2.70705648081779,13.7435492065112));
#419676=CARTESIAN_POINT('',(0.484092149969829,-2.70705648081779,14.));
#419677=CARTESIAN_POINT('',(0.409442052702732,-2.71934867302422,13.7435492065112));
#419678=CARTESIAN_POINT('Origin',(0.,2.5406128344257E-15,13.7435492065112));
#419679=CARTESIAN_POINT('',(0.409442052702732,-2.71934867302422,12.5369868989719));
#419680=CARTESIAN_POINT('',(0.409442052702732,-2.71934867302422,14.));
#419681=CARTESIAN_POINT('Ctrl Pts',(0.374664178143524,-2.72435804431357,
12.4908873016278));
#419682=CARTESIAN_POINT('Ctrl Pts',(0.376825165298539,-2.72406085706312,
12.4908873016278));
#419683=CARTESIAN_POINT('Ctrl Pts',(0.378997972116748,-2.72375936882074,
12.4911020829134));
#419684=CARTESIAN_POINT('Ctrl Pts',(0.381113270285288,-2.723463360358,12.4915448903141));
#419685=CARTESIAN_POINT('Ctrl Pts',(0.384732287684508,-2.7229569259494,
12.4923024798169));
#419686=CARTESIAN_POINT('Ctrl Pts',(0.388266045314105,-2.72245464266283,
12.4937722312795));
#419687=CARTESIAN_POINT('Ctrl Pts',(0.391365198357109,-2.72200905243074,
12.4958030942394));
#419688=CARTESIAN_POINT('Ctrl Pts',(0.394442476532154,-2.72156660732487,
12.4978196226833));
#419689=CARTESIAN_POINT('Ctrl Pts',(0.397182536113045,-2.72116725902309,
12.5004326847668));
#419690=CARTESIAN_POINT('Ctrl Pts',(0.399442728666425,-2.72083544274834,
12.5033504258767));
#419691=CARTESIAN_POINT('Ctrl Pts',(0.402143259534509,-2.72043898091097,
12.5068366111226));
#419692=CARTESIAN_POINT('Ctrl Pts',(0.404245663154215,-2.72012643942305,
12.5108395010833));
#419693=CARTESIAN_POINT('Ctrl Pts',(0.405778737023668,-2.71989772171299,
12.5149868989719));
#419694=CARTESIAN_POINT('Ctrl Pts',(0.408353680751798,-2.71951356851282,
12.5219528491417));
#419695=CARTESIAN_POINT('Ctrl Pts',(0.409442052740859,-2.71934867301877,
12.5295503425868));
#419696=CARTESIAN_POINT('Ctrl Pts',(0.409442052702732,-2.71934867302422,
12.5369868989719));
#419697=CARTESIAN_POINT('',(0.261831139002702,-2.73750697800911,12.5369868989719));
#419698=CARTESIAN_POINT('Ctrl Pts',(0.261831139002701,-2.7375069780091,
12.5369868989719));
#419699=CARTESIAN_POINT('Ctrl Pts',(0.261831139002703,-2.7375069780091,
12.5309445149785));
#419700=CARTESIAN_POINT('Ctrl Pts',(0.262551725131416,-2.73743846254104,
12.5248274368704));
#419701=CARTESIAN_POINT('Ctrl Pts',(0.264200735787393,-2.73727930091348,
12.5190199595513));
#419702=CARTESIAN_POINT('Ctrl Pts',(0.265585801271034,-2.73714561513294,
12.5141420429941));
#419703=CARTESIAN_POINT('Ctrl Pts',(0.267668686308478,-2.73694388120992,
12.5093757677094));
#419704=CARTESIAN_POINT('Ctrl Pts',(0.270541639118242,-2.73665986587723,
12.5051960112707));
#419705=CARTESIAN_POINT('Ctrl Pts',(0.272460969658652,-2.73647012405477,
12.5024036458141));
#419706=CARTESIAN_POINT('Ctrl Pts',(0.274779440947572,-2.73623889210599,
12.4998248032393));
#419707=CARTESIAN_POINT('Ctrl Pts',(0.277414672434579,-2.73597169201693,
12.4976950015772));
#419708=CARTESIAN_POINT('Ctrl Pts',(0.280124154119048,-2.73569696330678,
12.495505190692));
#419709=CARTESIAN_POINT('Ctrl Pts',(0.283238340672297,-2.7353769221781,
12.4937456938368));
#419710=CARTESIAN_POINT('Ctrl Pts',(0.286516462306602,-2.73503351292581,
12.4925987732155));
#419711=CARTESIAN_POINT('Ctrl Pts',(0.289793816873083,-2.73469018402996,
12.4914521209692));
#419712=CARTESIAN_POINT('Ctrl Pts',(0.293316730308969,-2.73431480904527,
12.4908873016276));
#419713=CARTESIAN_POINT('Ctrl Pts',(0.296786224392195,-2.7339381735897,
12.4908873016278));
#419714=CARTESIAN_POINT('',(0.261831139002703,-2.73750697800911,13.7435492065112));
#419715=CARTESIAN_POINT('',(0.261831139002704,-2.73750697800911,14.));
#419716=CARTESIAN_POINT('',(0.186427505996095,-2.74367359301504,13.7435492065112));
#419717=CARTESIAN_POINT('Origin',(0.,2.5406128344257E-15,13.7435492065112));
#419718=CARTESIAN_POINT('',(0.186427505996095,-2.74367359301505,12.5369868989719));
#419719=CARTESIAN_POINT('',(0.186427505996095,-2.74367359301505,14.));
#419720=CARTESIAN_POINT('Ctrl Pts',(0.151357041680694,-2.74583157639606,
12.4908873016278));
#419721=CARTESIAN_POINT('Ctrl Pts',(0.153535061849082,-2.74571151852644,
12.4908873016278));
#419722=CARTESIAN_POINT('Ctrl Pts',(0.155725212922482,-2.74558813738835,
12.4911020829134));
#419723=CARTESIAN_POINT('Ctrl Pts',(0.157857600048588,-2.74546553030755,
12.4915448903141));
#419724=CARTESIAN_POINT('Ctrl Pts',(0.161505854571769,-2.74525576453302,
12.4923024798169));
#419725=CARTESIAN_POINT('Ctrl Pts',(0.165068794665194,-2.74504318660527,
12.4937722312795));
#419726=CARTESIAN_POINT('Ctrl Pts',(0.168193955272682,-2.74485168878206,
12.4958030942394));
#419727=CARTESIAN_POINT('Ctrl Pts',(0.171297057442045,-2.74466154261511,
12.4978196226833));
#419728=CARTESIAN_POINT('Ctrl Pts',(0.174060550294684,-2.74448686340517,
12.5004326847668));
#419729=CARTESIAN_POINT('Ctrl Pts',(0.176340268350619,-2.7443403778974,
12.5033504258767));
#419730=CARTESIAN_POINT('Ctrl Pts',(0.179064128745335,-2.74416535359035,
12.5068366111226));
#419731=CARTESIAN_POINT('Ctrl Pts',(0.181185011823192,-2.74402521747121,
12.5108395010833));
#419732=CARTESIAN_POINT('Ctrl Pts',(0.182731627132496,-2.74392222055319,
12.5149868989719));
#419733=CARTESIAN_POINT('Ctrl Pts',(0.185329314999907,-2.74374922740956,
12.5219528491417));
#419734=CARTESIAN_POINT('Ctrl Pts',(0.186427506034539,-2.74367359301272,
12.5295503425868));
#419735=CARTESIAN_POINT('Ctrl Pts',(0.186427505996095,-2.74367359301505,
12.5369868989719));
#419736=CARTESIAN_POINT('',(0.0378276850046104,-2.74973981791863,12.5369868989719));
#419737=CARTESIAN_POINT('Ctrl Pts',(0.0378276850046103,-2.74973981791863,
12.5369868989719));
#419738=CARTESIAN_POINT('Ctrl Pts',(0.037827685004612,-2.74973981791863,
12.5309445149785));
#419739=CARTESIAN_POINT('Ctrl Pts',(0.0385514580891393,-2.74973026488922,
12.5248274368704));
#419740=CARTESIAN_POINT('Ctrl Pts',(0.0402079549484237,-2.74970604253597,
12.5190199595513));
#419741=CARTESIAN_POINT('Ctrl Pts',(0.0415993083731197,-2.74968569727908,
12.5141420429941));
#419742=CARTESIAN_POINT('Ctrl Pts',(0.0436917059699596,-2.74965440907616,
12.5093757677094));
#419743=CARTESIAN_POINT('Ctrl Pts',(0.0465782491525343,-2.74960551110625,
12.5051960112707));
#419744=CARTESIAN_POINT('Ctrl Pts',(0.0485066589989134,-2.74957284389129,
12.5024036458141));
#419745=CARTESIAN_POINT('Ctrl Pts',(0.0508362633163583,-2.74953135828142,
12.4998248032393));
#419746=CARTESIAN_POINT('Ctrl Pts',(0.0534845055758057,-2.74947984310911,
12.4976950015772));
#419747=CARTESIAN_POINT('Ctrl Pts',(0.0562073646238211,-2.74942687644696,
12.495505190692));
#419748=CARTESIAN_POINT('Ctrl Pts',(0.0593372753013208,-2.74936173534353,
12.4937456938368));
#419749=CARTESIAN_POINT('Ctrl Pts',(0.0626324802984313,-2.74928666610298,
12.4925987732155));
#419750=CARTESIAN_POINT('Ctrl Pts',(0.0659269142302771,-2.74921161442835,
12.4914521209692));
#419751=CARTESIAN_POINT('Ctrl Pts',(0.0694687020083875,-2.74912463862312,
12.4908873016276));
#419752=CARTESIAN_POINT('Ctrl Pts',(0.0729573509224067,-2.74903205236795,
12.4908873016278));
#419753=CARTESIAN_POINT('',(0.0378276850046121,-2.74973981791863,14.));
#419754=CARTESIAN_POINT('Origin',(0.,2.60208521396521E-15,13.7435492065112));
#419755=CARTESIAN_POINT('Origin',(0.0629611349460807,-2.65846395524141,
13.7420545896477));
#419756=CARTESIAN_POINT('Origin',(-0.0636035367449967,-2.65612979764794,
13.7415084174026));
#419757=CARTESIAN_POINT('Origin',(0.,2.60208521396521E-15,13.7435492065112));
#419758=CARTESIAN_POINT('Origin',(2.18006130902264,1.51868482600949,13.7415084174033));
#419759=CARTESIAN_POINT('Origin',(2.10713407931711,1.62215309930852,13.7420545896465));
#419760=CARTESIAN_POINT('Origin',(0.,2.60208521396521E-15,13.7435492065112));
#419761=CARTESIAN_POINT('Origin',(2.23234330142418,1.44500452954644,13.742054589647));
#419762=CARTESIAN_POINT('Origin',(2.29659424696376,1.33593629214936,13.7415084174048));
#419763=CARTESIAN_POINT('Origin',(0.,2.60208521396521E-15,13.7435492065112));
#419764=CARTESIAN_POINT('Origin',(2.3426966471724,1.25823969304925,13.7420545896481));
#419765=CARTESIAN_POINT('Origin',(2.39784372909656,1.1442973226725,13.7415084174029));
#419766=CARTESIAN_POINT('Origin',(0.,2.60208521396521E-15,13.7435492065112));
#419767=CARTESIAN_POINT('Origin',(2.43745973325144,1.06310147898929,13.7420545896491));
#419768=CARTESIAN_POINT('Origin',(2.48313595683433,0.945043243314494,13.741508417404));
#419769=CARTESIAN_POINT('Origin',(0.,2.60208521396521E-15,13.7435492065112));
#419770=CARTESIAN_POINT('Origin',(2.51600192695173,0.860888499985368,13.7420545896476));
#419771=CARTESIAN_POINT('Origin',(2.55190332446211,0.739500057089027,13.7415084174023));
#419772=CARTESIAN_POINT('Origin',(0.,2.60208521396521E-15,13.7435492065112));
#419773=CARTESIAN_POINT('Origin',(2.57780054294477,0.652946450051028,13.7420545896483));
#419774=CARTESIAN_POINT('Origin',(2.60368819650721,0.529035619997232,13.7415084174039));
#419775=CARTESIAN_POINT('Origin',(0.,2.60208521396521E-15,13.7435492065112));
#419776=CARTESIAN_POINT('Origin',(2.62244432163127,0.44065914921995,13.7420545896489));
#419777=CARTESIAN_POINT('Origin',(2.63814595317993,0.315050538137071,13.7415084174041));
#419778=CARTESIAN_POINT('Origin',(0.,2.60208521396521E-15,13.7435492065112));
#419779=CARTESIAN_POINT('Origin',(2.64963616603145,0.225439334453963,13.7420545896499));
#419780=CARTESIAN_POINT('Origin',(2.65504728379398,0.0989688469239032,13.7415084174028));
#419781=CARTESIAN_POINT('Origin',(0.,2.60208521396521E-15,13.7435492065112));
#419782=CARTESIAN_POINT('Origin',(2.65919511889896,0.00871925811366688,
13.7420545896483));
#419783=CARTESIAN_POINT('Origin',(2.65427971278744,-0.117771465635996,13.7415084174022));
#419784=CARTESIAN_POINT('Origin',(0.,2.60208521396521E-15,13.7435492065112));
#419785=CARTESIAN_POINT('Origin',(2.65105756699552,-0.208058843453515,13.7420545896502));
#419786=CARTESIAN_POINT('Origin',(2.63584834821942,-0.333728028522382,13.7415084174022));
#419787=CARTESIAN_POINT('Origin',(0.,2.60208521396521E-15,13.7435492065112));
#419788=CARTESIAN_POINT('Origin',(2.62527766436935,-0.42345234774179,13.7420545896487));
#419789=CARTESIAN_POINT('Origin',(2.59987584777974,-0.547463686440066,13.7415084174026));
#419790=CARTESIAN_POINT('Origin',(0.,2.60208521396521E-15,13.7435492065112));
#419791=CARTESIAN_POINT('Origin',(2.58202697203059,-0.636027846521902,13.7420545896488));
#419792=CARTESIAN_POINT('Origin',(2.54660160252169,-0.75755606384985,13.7415084174027));
#419793=CARTESIAN_POINT('Origin',(0.,2.60208521396521E-15,13.7435492065112));
#419794=CARTESIAN_POINT('Origin',(2.52159331619725,-0.844370684920506,13.7420545896486));
#419795=CARTESIAN_POINT('Origin',(2.47638014376077,-0.96260703064293,13.7415084174038));
#419796=CARTESIAN_POINT('Origin',(0.,2.60208521396521E-15,13.7435492065112));
#419797=CARTESIAN_POINT('Origin',(2.4443788728763,-1.04709437572065,13.7420545896477));
#419798=CARTESIAN_POINT('Origin',(2.38967878371463,-1.16125200646612,13.7415084174039));
#419799=CARTESIAN_POINT('Origin',(0.,2.60208521396521E-15,13.7435492065112));
#419800=CARTESIAN_POINT('Origin',(2.35089749145357,-1.24284982621121,13.742054589648));
#419801=CARTESIAN_POINT('Origin',(2.28707450563236,-1.35216904177949,13.7415084174041));
#419802=CARTESIAN_POINT('Origin',(0.,2.60208521396521E-15,13.7435492065112));
#419803=CARTESIAN_POINT('Origin',(2.24177127509384,-1.43033431616192,13.7420545896474));
#419804=CARTESIAN_POINT('Origin',(2.16925012404985,-1.5340876152101,13.7415084174021));
#419805=CARTESIAN_POINT('Origin',(0.,2.60208521396521E-15,13.7435492065112));
#419806=CARTESIAN_POINT('Origin',(2.11772644076833,-1.60830016723173,13.7420545896489));
#419807=CARTESIAN_POINT('Origin',(2.03698974080133,-1.70579708867073,13.7415084174032));
#419808=CARTESIAN_POINT('Origin',(0.,2.60208521396521E-15,13.7435492065112));
#419809=CARTESIAN_POINT('Origin',(1.97958848637722,-1.77556304603655,13.742054589649));
#419810=CARTESIAN_POINT('Origin',(1.8911735269064,-1.86615476394301,13.7415084174042));
#419811=CARTESIAN_POINT('Origin',(0.,2.60208521396521E-15,13.7435492065112));
#419812=CARTESIAN_POINT('Origin',(1.8282766972176,-1.93100984571577,13.7420545896482));
#419813=CARTESIAN_POINT('Origin',(1.73277186520649,-2.01409348715231,13.7415084174027));
#419814=CARTESIAN_POINT('Origin',(0.,2.60208521396521E-15,13.7435492065112));
#419815=CARTESIAN_POINT('Origin',(1.66479802828494,-2.07360609347156,13.7420545896501));
#419816=CARTESIAN_POINT('Origin',(1.56283889263393,-2.14862875050822,13.7415084174026));
#419817=CARTESIAN_POINT('Origin',(0.,2.60208521396521E-15,13.7435492065112));
#419818=CARTESIAN_POINT('Origin',(1.49024040314276,-2.20240283478712,13.7420545896481));
#419819=CARTESIAN_POINT('Origin',(1.3825054850803,-2.2688652440275,13.7415084174021));
#419820=CARTESIAN_POINT('Origin',(0.,2.60208521396521E-15,13.7435492065112));
#419821=CARTESIAN_POINT('Origin',(1.30576547399232,-2.31654294861448,13.7420545896488));
#419822=CARTESIAN_POINT('Origin',(1.19297173162209,-2.37400281368525,13.7415084174022));
#419823=CARTESIAN_POINT('Origin',(0.,2.60208521396521E-15,13.7435492065112));
#419824=CARTESIAN_POINT('Origin',(1.11260089104787,-2.41526685131816,13.7420545896482));
#419825=CARTESIAN_POINT('Origin',(0.995498948118894,-2.46334178630396,13.7415084174039));
#419826=CARTESIAN_POINT('Origin',(0.,2.60208521396521E-15,13.7435492065112));
#419827=CARTESIAN_POINT('Origin',(0.912032132740323,-2.49791755162278,13.7420545896496));
#419828=CARTESIAN_POINT('Origin',(0.791401283357222,-2.53628762575223,13.7415084174029));
#419829=CARTESIAN_POINT('Origin',(0.,2.60208521396521E-15,13.7435492065112));
#419830=CARTESIAN_POINT('Origin',(0.705393951063582,-2.56394502274485,13.7420545896495));
#419831=CARTESIAN_POINT('Origin',(0.582036973629713,-2.59235488951334,13.7415084174038));
#419832=CARTESIAN_POINT('Origin',(0.,2.60208521396521E-15,13.7435492065112));
#419833=CARTESIAN_POINT('Origin',(0.494061489024843,-2.61290986275703,13.7420545896477));
#419834=CARTESIAN_POINT('Origin',(0.368799303868886,-2.6311704591873,13.7415084174023));
#419835=CARTESIAN_POINT('Origin',(0.,2.60208521396521E-15,13.7435492065112));
#419836=CARTESIAN_POINT('Origin',(0.279441129291135,-2.64448621873616,13.7420545896472));
#419837=CARTESIAN_POINT('Origin',(0.153107335591366,-2.652476023574,13.7415084174032));
#419838=CARTESIAN_POINT('Origin',(0.,2.60208521396521E-15,13.7435492065112));
#419839=CARTESIAN_POINT('Origin',(-0.153937855364234,-2.65475005273974,
13.742054589648));
#419840=CARTESIAN_POINT('Origin',(-0.279891138037187,-2.64210746615306,
13.7415084174037));
#419841=CARTESIAN_POINT('Origin',(0.,2.60208521396521E-15,13.7435492065112));
#419842=CARTESIAN_POINT('Origin',(-0.369812414643718,-2.63336922663678,
13.7420545896469));
#419843=CARTESIAN_POINT('Origin',(-0.494316109985248,-2.61050234538536,
13.7415084174037));
#419844=CARTESIAN_POINT('Origin',(0.,2.60208521396521E-15,13.7435492065112));
#419845=CARTESIAN_POINT('Origin',(-0.58322593332106,-2.59446376281132,13.7420545896483));
#419846=CARTESIAN_POINT('Origin',(-0.70545148977777,-2.56152476221158,13.7415084174036));
#419847=CARTESIAN_POINT('Origin',(0.,2.60208521396521E-15,13.7435492065112));
#419848=CARTESIAN_POINT('Origin',(-0.79275817963557,-2.53829257069669,13.7420545896477));
#419849=CARTESIAN_POINT('Origin',(-0.911892206297038,-2.4955006543659,13.7415084174031));
#419850=CARTESIAN_POINT('Origin',(0.,2.60208521396521E-15,13.7435492065112));
#419851=CARTESIAN_POINT('Origin',(-0.997014751062135,-2.4652294603152,13.7420545896484));
#419852=CARTESIAN_POINT('Origin',(-1.11226443063565,-2.41286940140007,13.7415084174049));
#419853=CARTESIAN_POINT('Origin',(0.,2.60208521396521E-15,13.7435492065112));
#419854=CARTESIAN_POINT('Origin',(-1.19463635381647,-2.37576065460941,13.7420545896491));
#419855=CARTESIAN_POINT('Origin',(-1.3052347186976,-2.31418090065322,13.7415084174027));
#419856=CARTESIAN_POINT('Origin',(0.,2.60208521396521E-15,13.7435492065112));
#419857=CARTESIAN_POINT('Origin',(-1.38430784873633,-2.2704815537189,13.7420545896491));
#419858=CARTESIAN_POINT('Origin',(-1.48951888505758,-2.20009190783617,13.7415084174049));
#419859=CARTESIAN_POINT('Origin',(0.,2.60208521396521E-15,13.7435492065112));
#419860=CARTESIAN_POINT('Origin',(-1.56476700331623,-2.15009277269043,13.7420545896486));
#419861=CARTESIAN_POINT('Origin',(-1.6638905489877,-2.07136166635204,13.7415084174028));
#419862=CARTESIAN_POINT('Origin',(0.,2.60208521396521E-15,13.7435492065112));
#419863=CARTESIAN_POINT('Origin',(-1.73481289165434,-2.01539547899836,13.7420545896465));
#419864=CARTESIAN_POINT('Origin',(-1.82718929583891,-1.92884685473472,13.7415084174032));
#419865=CARTESIAN_POINT('Origin',(0.,2.60208521396521E-15,13.7435492065112));
#419866=CARTESIAN_POINT('Origin',(-1.89331388642696,-1.8672860609137,13.7420545896469));
#419867=CARTESIAN_POINT('Origin',(-1.97832839939094,-1.77349588553556,13.7415084174032));
#419868=CARTESIAN_POINT('Origin',(0.,2.60208521396521E-15,13.7435492065112));
#419869=CARTESIAN_POINT('Origin',(-2.03921518966487,-1.70675016217609,13.7420545896489));
#419870=CARTESIAN_POINT('Origin',(-2.11630205384649,-1.60634259382475,13.7415084174034));
#419871=CARTESIAN_POINT('Origin',(0.,2.60208521396521E-15,13.7435492065112));
#419872=CARTESIAN_POINT('Origin',(-2.17154585225241,-1.53485612269886,13.7420545896468));
#419873=CARTESIAN_POINT('Origin',(-2.24019206729996,-1.42849935718093,13.7415084174041));
#419874=CARTESIAN_POINT('Origin',(0.,2.60208521396521E-15,13.7435492065112));
#419875=CARTESIAN_POINT('Origin',(-2.28942523548034,-1.35274786896119,13.7420545896478));
#419876=CARTESIAN_POINT('Origin',(-2.34917397214803,-1.24114969299734,13.741508417403));
#419877=CARTESIAN_POINT('Origin',(0.,2.60208521396521E-15,13.7435492065112));
#419878=CARTESIAN_POINT('Origin',(-2.39206887149331,-1.16163730134264,13.7420545896483));
#419879=CARTESIAN_POINT('Origin',(-2.44252251179907,-1.04554038238373,13.7415084174027));
#419880=CARTESIAN_POINT('Origin',(0.,2.60208521396521E-15,13.7435492065112));
#419881=CARTESIAN_POINT('Origin',(-2.4787936838238,-0.96279622913968,13.7420545896461));
#419882=CARTESIAN_POINT('Origin',(-2.5196164671247,-0.842973173029527,13.7415084174036));
#419883=CARTESIAN_POINT('Origin',(0.,2.60208521396521E-15,13.7435492065112));
#419884=CARTESIAN_POINT('Origin',(-2.54902253317019,-0.757547906882836,
13.7420545896479));
#419885=CARTESIAN_POINT('Origin',(-2.579942790567,-0.634796116287876,13.7415084174037));
#419886=CARTESIAN_POINT('Origin',(0.,2.60208521396521E-15,13.7435492065112));
#419887=CARTESIAN_POINT('Origin',(-2.60228805811162,-0.5472582282921,13.742054589647));
#419888=CARTESIAN_POINT('Origin',(-2.62310002039505,-0.422394596124596,
13.741508417402));
#419889=CARTESIAN_POINT('Origin',(0.,2.60208521396521E-15,13.7435492065112));
#419890=CARTESIAN_POINT('Origin',(-2.63823578537793,-0.333326636482873,
13.7420545896481));
#419891=CARTESIAN_POINT('Origin',(-2.64880095237423,-0.207182109617279,
13.741508417403));
#419892=CARTESIAN_POINT('Origin',(0.,2.60208521396521E-15,13.7435492065112));
#419893=CARTESIAN_POINT('Origin',(-2.65662648876749,-0.117176810903261,
13.7420545896479));
#419894=CARTESIAN_POINT('Origin',(-2.65687455103644,0.00940913964739448,
13.7415084174036));
#419895=CARTESIAN_POINT('Origin',(0.,2.60208521396521E-15,13.7435492065112));
#419896=CARTESIAN_POINT('Origin',(-2.65733778119037,0.0997528070212094,
13.7420545896491));
#419897=CARTESIAN_POINT('Origin',(-2.64726708791042,0.225937772641397,13.7415084174026));
#419898=CARTESIAN_POINT('Origin',(0.,2.60208521396521E-15,13.7435492065112));
#419899=CARTESIAN_POINT('Origin',(-2.64036492910454,0.316018586471474,13.7420545896483));
#419900=CARTESIAN_POINT('Origin',(-2.62004249908263,0.440962827035131,13.7415084174016));
#419901=CARTESIAN_POINT('Origin',(0.,2.60208521396521E-15,13.7435492065112));
#419902=CARTESIAN_POINT('Origin',(-2.60582088404412,0.530181314367318,13.7420545896473));
#419903=CARTESIAN_POINT('Origin',(-2.57538195971003,0.653053346567803,13.7415084174044));
#419904=CARTESIAN_POINT('Origin',(0.,2.60208521396521E-15,13.7435492065112));
#419905=CARTESIAN_POINT('Origin',(-2.55393553093483,0.740815773091958,13.7420545896478));
#419906=CARTESIAN_POINT('Origin',(-2.51358267829733,0.860797903826238,13.7415084174048));
#419907=CARTESIAN_POINT('Origin',(0.,2.60208521396521E-15,13.7435492065112));
#419908=CARTESIAN_POINT('Origin',(-2.48505415823539,0.946520225071862,13.7420545896479));
#419909=CARTESIAN_POINT('Origin',(-2.43505591886255,1.06281399305533,13.7415084174013));
#419910=CARTESIAN_POINT('Origin',(0.,2.60208521396521E-15,13.7435492065112));
#419911=CARTESIAN_POINT('Origin',(-2.39963516011764,1.14592574111846,13.7420545896477));
#419912=CARTESIAN_POINT('Origin',(-2.3403242640558,1.25775723051356,13.7415084174024));
#419913=CARTESIAN_POINT('Origin',(0.,2.60208521396521E-15,13.7435492065112));
#419914=CARTESIAN_POINT('Origin',(-2.29824698592305,1.33770531042418,13.7420545896484));
#419915=CARTESIAN_POINT('Origin',(-2.23001813739833,1.44433030111864,13.7415084174037));
#419916=CARTESIAN_POINT('Origin',(0.,2.60208521396521E-15,13.7435492065112));
#419917=CARTESIAN_POINT('Origin',(-2.18156435721672,1.52058267158977,13.7420545896466));
#419918=CARTESIAN_POINT('Origin',(-2.10487160795666,1.62129159186549,13.7415084174024));
#419919=CARTESIAN_POINT('Origin',(0.,2.60208521396521E-15,13.7435492065112));
#419920=CARTESIAN_POINT('Origin',(-2.05036377765178,1.69334080596183,13.7420545896485));
#419921=CARTESIAN_POINT('Origin',(-1.96571750525081,1.7874634545656,13.7415084174041));
#419922=CARTESIAN_POINT('Origin',(0.,2.60208521396521E-15,13.7435492065112));
#419923=CARTESIAN_POINT('Origin',(-1.90551836542749,1.85483003664387,13.7420545896466));
#419924=CARTESIAN_POINT('Origin',(-1.81348187686654,1.94174004288618,13.741508417405));
#419925=CARTESIAN_POINT('Origin',(0.,2.60208521396521E-15,13.7435492065112));
#419926=CARTESIAN_POINT('Origin',(-1.74799204287233,2.00397567946144,13.7420545896466));
#419927=CARTESIAN_POINT('Origin',(-1.6491778257871,2.08309467158083,13.7415084174022));
#419928=CARTESIAN_POINT('Origin',(0.,2.60208521396521E-15,13.7435492065112));
#419929=CARTESIAN_POINT('Origin',(-1.57883312167183,2.13978519476937,13.7420545896485));
#419930=CARTESIAN_POINT('Origin',(-1.47389876838228,2.21058664892941,13.7415084174045));
#419931=CARTESIAN_POINT('Origin',(0.,2.60208521396521E-15,13.7435492065112));
#419932=CARTESIAN_POINT('Origin',(-1.39916732653332,2.26135479263981,13.7420545896478));
#419933=CARTESIAN_POINT('Origin',(-1.28881115784196,2.32336753684382,13.7415084174024));
#419934=CARTESIAN_POINT('Origin',(0.,2.60208521396521E-15,13.7435492065112));
#419935=CARTESIAN_POINT('Origin',(-1.21019030368429,2.36787544746751,13.7420545896492));
#419936=CARTESIAN_POINT('Origin',(-1.09514672169413,2.4206867971383,13.7415084174055));
#419937=CARTESIAN_POINT('Origin',(0.,2.60208521396521E-15,13.7435492065112));
#419938=CARTESIAN_POINT('Origin',(-1.01315966403005,2.4586382818545,13.7420545896468));
#419939=CARTESIAN_POINT('Origin',(-0.894194264790857,2.50189678617287,13.7415084174032));
#419940=CARTESIAN_POINT('Origin',(0.,2.60208521396521E-15,13.7435492065112));
#419941=CARTESIAN_POINT('Origin',(-0.809386613972477,2.53303928413104,13.7420545896474));
#419942=CARTESIAN_POINT('Origin',(-0.687291092593011,2.56645706488719,13.7415084174047));
#419943=CARTESIAN_POINT('Origin',(0.,2.60208521396521E-15,13.7435492065112));
#419944=CARTESIAN_POINT('Origin',(-0.600227229537934,2.59058332789403,13.7420545896484));
#419945=CARTESIAN_POINT('Origin',(-0.475814111565582,2.61393799526496,13.7415084174039));
#419946=CARTESIAN_POINT('Origin',(0.,2.60208521396521E-15,13.7435492065112));
#419947=CARTESIAN_POINT('Origin',(2.04902042275678,1.69132676291974,13.7415084174029));
#419948=CARTESIAN_POINT('Origin',(1.96790222757021,1.78850650783342,13.7420545896482));
#419949=CARTESIAN_POINT('Origin',(0.,2.60208521396521E-15,13.7435492065112));
#419950=CARTESIAN_POINT('Origin',(1.90434364364273,1.85271319927288,13.7415084174028));
#419951=CARTESIAN_POINT('Origin',(1.81557431117862,1.94295770063162,13.7420545896495));
#419952=CARTESIAN_POINT('Origin',(0.,2.60208521396521E-15,13.7435492065112));
#419953=CARTESIAN_POINT('Origin',(1.74699377177696,2.00177013496568,13.7415084174048));
#419954=CARTESIAN_POINT('Origin',(1.65116404728956,2.08447883049457,13.7420545896484));
#419955=CARTESIAN_POINT('Origin',(0.,2.60208521396521E-15,13.7435492065112));
#419956=CARTESIAN_POINT('Origin',(1.57801794458986,2.13750562067086,13.7415084174033));
#419957=CARTESIAN_POINT('Origin',(1.47576555909092,2.21212809765666,13.7420545896483));
#419958=CARTESIAN_POINT('Origin',(0.,2.60208521396521E-15,13.7435492065112));
#419959=CARTESIAN_POINT('Origin',(1.39854066833794,2.25901635913813,13.7415084174035));
#419960=CARTESIAN_POINT('Origin',(1.29054609457721,2.32505601730086,13.7420545896465));
#419961=CARTESIAN_POINT('Origin',(0.,2.60208521396521E-15,13.7435492065112));
#419962=CARTESIAN_POINT('Origin',(1.20975633468107,2.36549371644643,13.7415084174035));
#419963=CARTESIAN_POINT('Origin',(1.09673825873626,2.422511072764,13.7420545896482));
#419964=CARTESIAN_POINT('Origin',(0.,2.60208521396521E-15,13.7435492065112));
#419965=CARTESIAN_POINT('Origin',(1.01292127221245,2.45622910334862,13.7415084174024));
#419966=CARTESIAN_POINT('Origin',(0.8956318107298,2.50384471672177,13.7420545896489));
#419967=CARTESIAN_POINT('Origin',(0.,2.60208521396521E-15,13.7435492065112));
#419968=CARTESIAN_POINT('Origin',(0.809345385797912,2.53061869082039,13.7415084174029));
#419969=CARTESIAN_POINT('Origin',(0.688565080790549,2.56851568719345,13.7420545896486));
#419970=CARTESIAN_POINT('Origin',(0.,2.60208521396521E-15,13.7435492065112));
#419971=CARTESIAN_POINT('Origin',(0.60038343937335,2.58816742842705,13.741508417403));
#419972=CARTESIAN_POINT('Origin',(0.476916063842626,2.61609360953942,13.7420545896471));
#419973=CARTESIAN_POINT('Origin',(0.,2.60208521396521E-15,13.7435492065112));
#419974=CARTESIAN_POINT('Origin',(0.387426040215676,2.62849233881714,13.741508417404));
#419975=CARTESIAN_POINT('Origin',(0.262093249178328,2.64626186054439,13.7420545896481));
#419976=CARTESIAN_POINT('Origin',(0.,2.60208521396521E-15,13.7435492065112));
#419977=CARTESIAN_POINT('Origin',(0.171890384681917,2.65132506635799,13.7415084174029));
#419978=CARTESIAN_POINT('Origin',(0.0455262471821439,2.65881967546814,13.7420545896482));
#419979=CARTESIAN_POINT('Origin',(0.,2.60208521396521E-15,13.7435492065112));
#419980=CARTESIAN_POINT('Origin',(-0.387073431921677,2.63088746702105,13.7420545896474));
#419981=CARTESIAN_POINT('Origin',(-0.261170666129395,2.64402359955241,13.7415084174024));
#419982=CARTESIAN_POINT('Origin',(0.,2.69653690488338,12.5));
#419983=CARTESIAN_POINT('',(-0.0317307692307694,2.68331575103722,12.5893111709658));
#419984=CARTESIAN_POINT('',(-0.0317307692307694,2.68331575103722,13.8235269408515));
#419985=CARTESIAN_POINT('',(-0.0317307692307694,2.68331575103722,12.5));
#419986=CARTESIAN_POINT('',(0.00111954586465913,2.66218087500164,13.8587068136939));
#419987=CARTESIAN_POINT('Ctrl Pts',(-0.0317307692368139,2.68331575103455,
13.8235269408542));
#419988=CARTESIAN_POINT('Ctrl Pts',(-0.0310568083417728,2.68169824488647,
13.8262006681044));
#419989=CARTESIAN_POINT('Ctrl Pts',(-0.0302067330691194,2.68010978649456,
13.8288634856214));
#419990=CARTESIAN_POINT('Ctrl Pts',(-0.0291938585816618,2.6785496599764,
13.8314912288862));
#419991=CARTESIAN_POINT('Ctrl Pts',(-0.0281496894582509,2.67694133045577,
13.834200161153));
#419992=CARTESIAN_POINT('Ctrl Pts',(-0.0269317626839319,2.67536105356044,
13.8368750301949));
#419993=CARTESIAN_POINT('Ctrl Pts',(-0.0255098200583974,2.67381369830471,
13.8394886372968));
#419994=CARTESIAN_POINT('Ctrl Pts',(-0.0253999999802731,2.67369419230494,
13.8396904925131));
#419995=CARTESIAN_POINT('Ctrl Pts',(-0.0252889443323249,2.67357489463028,
13.8398919674349));
#419996=CARTESIAN_POINT('Ctrl Pts',(-0.0251766301202508,2.67345581452184,
13.8400930404591));
#419997=CARTESIAN_POINT('Ctrl Pts',(-0.0234266991348905,2.67160046631923,
13.8432258934518));
#419998=CARTESIAN_POINT('Ctrl Pts',(-0.0213809904682469,2.66980662883099,
13.8462331177034));
#419999=CARTESIAN_POINT('Ctrl Pts',(-0.0190426235063883,2.66820533811557,
13.8489036603661));
#420000=CARTESIAN_POINT('Ctrl Pts',(-0.0182774826235232,2.66768137715832,
13.8497774930041));
#420001=CARTESIAN_POINT('Ctrl Pts',(-0.0174811027381851,2.66717826280278,
13.85061494757));
#420002=CARTESIAN_POINT('Ctrl Pts',(-0.0166538759919881,2.66670124117228,
13.8514076489583));
#420003=CARTESIAN_POINT('Ctrl Pts',(-0.0149041721198265,2.66569227162696,
13.8530843267192));
#420004=CARTESIAN_POINT('Ctrl Pts',(-0.0128431198768504,2.66470349169249,
13.8546805203176));
#420005=CARTESIAN_POINT('Ctrl Pts',(-0.0105313231737223,2.66391531097655,
13.8559412814273));
#420006=CARTESIAN_POINT('Ctrl Pts',(-0.010221929801502,2.66380982683545,
13.8561100121513));
#420007=CARTESIAN_POINT('Ctrl Pts',(-0.0099081113111903,2.66370789632895,
13.8562727473908));
#420008=CARTESIAN_POINT('Ctrl Pts',(-0.0095900727650585,2.66360990524316,
13.8564289040185));
#420009=CARTESIAN_POINT('Ctrl Pts',(-0.00814777158665154,2.66316551678701,
13.8571370725437));
#420010=CARTESIAN_POINT('Ctrl Pts',(-0.00659265830578076,2.66279651133532,
13.8577210840554));
#420011=CARTESIAN_POINT('Ctrl Pts',(-0.00497840473373783,2.66254578735691,
13.8581177131616));
#420012=CARTESIAN_POINT('Ctrl Pts',(-0.00452377536693578,2.66247517485494,
13.8582294175695));
#420013=CARTESIAN_POINT('Ctrl Pts',(-0.00406451623070895,2.66241377743103,
13.8583265086086));
#420014=CARTESIAN_POINT('Ctrl Pts',(-0.00360195264082081,2.66236213234807,
13.8584082369006));
#420015=CARTESIAN_POINT('Ctrl Pts',(-0.00293737280347575,2.66228793221303,
13.8585256585398));
#420016=CARTESIAN_POINT('Ctrl Pts',(-0.002257673747352,2.66223326171001,
13.8586122832068));
#420017=CARTESIAN_POINT('Ctrl Pts',(-0.00158044877125891,2.66220032816512,
13.8586682984299));
#420018=CARTESIAN_POINT('Ctrl Pts',(-0.00103873592153746,2.6621739845938,
13.8587131050557));
#420019=CARTESIAN_POINT('Ctrl Pts',(-0.000492634257675246,2.66216102405791,
13.8587357943552));
#420020=CARTESIAN_POINT('Ctrl Pts',(5.79331281739812E-5,2.66216195132077,
13.8587355499465));
#420021=CARTESIAN_POINT('Ctrl Pts',(0.000413777955724857,2.66216255063287,
13.8587353919793));
#420022=CARTESIAN_POINT('Ctrl Pts',(0.000767640276359607,2.66216890620456,
13.8587257282814));
#420023=CARTESIAN_POINT('Ctrl Pts',(0.00111954586465914,2.66218087500164,
13.8587068136939));
#420024=CARTESIAN_POINT('',(0.0317307692307694,2.68331575103722,13.8235269408515));
#420025=CARTESIAN_POINT('Ctrl Pts',(0.00111954586465914,2.66218087500164,
13.8587068136939));
#420026=CARTESIAN_POINT('Ctrl Pts',(0.00227694416047025,2.66222023972277,
13.8586446046466));
#420027=CARTESIAN_POINT('Ctrl Pts',(0.0034132030282657,2.66232024878167,
13.858482427929));
#420028=CARTESIAN_POINT('Ctrl Pts',(0.00452901854825893,2.66247648613606,
13.8582284286032));
#420029=CARTESIAN_POINT('Ctrl Pts',(0.00567371547471972,2.66263676748737,
13.8579678548414));
#420030=CARTESIAN_POINT('Ctrl Pts',(0.00679948085161418,2.66285813397142,
13.857615680862));
#420031=CARTESIAN_POINT('Ctrl Pts',(0.00786380175605046,2.66312235077613,
13.8571944833187));
#420032=CARTESIAN_POINT('Ctrl Pts',(0.0105199234229024,2.66378173083418,
13.8561433417727));
#420033=CARTESIAN_POINT('Ctrl Pts',(0.0129187674764211,2.66473417359602,
13.8546163505474));
#420034=CARTESIAN_POINT('Ctrl Pts',(0.0149915607379914,2.66578467107066,
13.8528973491086));
#420035=CARTESIAN_POINT('Ctrl Pts',(0.0153702294856515,2.66597658146062,
13.8525833129072));
#420036=CARTESIAN_POINT('Ctrl Pts',(0.0157381315426899,2.66617168202568,
13.8522628768811));
#420037=CARTESIAN_POINT('Ctrl Pts',(0.016095007457731,2.66636870368544,
13.851937733538));
#420038=CARTESIAN_POINT('Ctrl Pts',(0.0182743991566692,2.66757188762613,
13.8499521282529));
#420039=CARTESIAN_POINT('Ctrl Pts',(0.020257204092566,2.66896986054969,
13.847639871647));
#420040=CARTESIAN_POINT('Ctrl Pts',(0.0219855079307009,2.67042348860387,
13.8452109780794));
#420041=CARTESIAN_POINT('Ctrl Pts',(0.0227631076015868,2.67107750595405,
13.8441181685877));
#420042=CARTESIAN_POINT('Ctrl Pts',(0.0234898124370233,2.67174243386388,
13.8430021611332));
#420043=CARTESIAN_POINT('Ctrl Pts',(0.0241635881008166,2.67240493103305,
13.8418824960098));
#420044=CARTESIAN_POINT('Ctrl Pts',(0.0257513576580267,2.67396612252969,
13.8392439765549));
#420045=CARTESIAN_POINT('Ctrl Pts',(0.027123754201243,2.67558575023078,
13.8364981347964));
#420046=CARTESIAN_POINT('Ctrl Pts',(0.0283105152282354,2.67724597470287,
13.8336931113419));
#420047=CARTESIAN_POINT('Ctrl Pts',(0.029466345102232,2.67886292790469,
13.8309611966328));
#420048=CARTESIAN_POINT('Ctrl Pts',(0.0304467890444241,2.68052033781573,
13.8281701127185));
#420049=CARTESIAN_POINT('Ctrl Pts',(0.0312412241942218,2.68221138008974,
13.825358068512));
#420050=CARTESIAN_POINT('Ctrl Pts',(0.031413458592073,2.68257799987976,
13.8247484142932));
#420051=CARTESIAN_POINT('Ctrl Pts',(0.0315767788941016,2.68294617422922,
13.8241378483365));
#420052=CARTESIAN_POINT('Ctrl Pts',(0.0317307692307694,2.68331575103722,
13.8235269408515));
#420053=CARTESIAN_POINT('',(0.0317307692307694,2.68331575103722,12.5893111709658));
#420054=CARTESIAN_POINT('',(0.0317307692307694,2.68331575103722,12.5));
#420055=CARTESIAN_POINT('',(-0.000122408502243047,2.66216281377041,12.5969504640361));
#420056=CARTESIAN_POINT('Origin',(1.95806035357092E-7,2.69656999029512,
12.584524458991));
#420057=CARTESIAN_POINT('Origin',(1.95806035357092E-7,2.69656999029512,
12.584524458991));
#420058=CARTESIAN_POINT('Origin',(-0.1375,2.93716190488338,12.5));
#420059=CARTESIAN_POINT('',(-0.0534592077666728,2.73546400352339,13.7435492065112));
#420060=CARTESIAN_POINT('',(-0.0454872776377203,2.71633137121391,13.7902182540695));
#420061=CARTESIAN_POINT('Origin',(-0.0245384230857362,2.66605412028915,
13.7418732680451));
#420062=CARTESIAN_POINT('',(-0.0454872776377203,2.71633137121391,13.7902182540695));
#420063=CARTESIAN_POINT('',(-0.0534592077666728,2.73546400352339,12.5369868989719));
#420064=CARTESIAN_POINT('Ctrl Pts',(-0.0317307692307694,2.68331575103722,
12.5893111709658));
#420065=CARTESIAN_POINT('Ctrl Pts',(-0.0389789705363253,2.70071143417056,
12.5718848856037));
#420066=CARTESIAN_POINT('Ctrl Pts',(-0.0462216773885433,2.71809393061588,
12.5544431401645));
#420067=CARTESIAN_POINT('Ctrl Pts',(-0.0534592077666728,2.73546400352339,
12.5369868989719));
#420068=CARTESIAN_POINT('',(-0.0534592077666728,2.73546400352339,12.5));
#420069=CARTESIAN_POINT('Origin',(0.0317307692307694,2.68331575103722,12.5));
#420070=CARTESIAN_POINT('',(0.0454872776377203,2.71633137121391,13.7902182540695));
#420071=CARTESIAN_POINT('',(0.0317307692307694,2.68331575103722,13.8235269408515));
#420072=CARTESIAN_POINT('',(0.0534592077666729,2.73546400352339,13.7435492065112));
#420073=CARTESIAN_POINT('Origin',(0.0272313623171153,2.67251802140762,13.7445212918687));
#420074=CARTESIAN_POINT('',(0.0534592077666728,2.73546400352339,12.5369868989719));
#420075=CARTESIAN_POINT('',(0.0534592077666729,2.73546400352339,12.5));
#420076=CARTESIAN_POINT('Ctrl Pts',(0.0534592077666728,2.73546400352339,
12.5369868989719));
#420077=CARTESIAN_POINT('Ctrl Pts',(0.0462216773885433,2.71809393061588,
12.5544431401645));
#420078=CARTESIAN_POINT('Ctrl Pts',(0.0389789705363253,2.70071143417056,
12.5718848856037));
#420079=CARTESIAN_POINT('Ctrl Pts',(0.0317307692307694,2.68331575103722,
12.5893111709658));
#420080=CARTESIAN_POINT('Origin',(0.,1.50000000000006,11.));
#420081=CARTESIAN_POINT('Origin',(0.,1.25,12.5));
#420082=CARTESIAN_POINT('',(1.25,0.721687836487034,12.5));
#420083=CARTESIAN_POINT('',(1.25,0.721687836487034,12.5));
#420084=CARTESIAN_POINT('',(1.25,-0.721687836487026,12.5));
#420085=CARTESIAN_POINT('Origin',(0.,1.25,12.5));
#420086=CARTESIAN_POINT('',(1.25,-0.721687836487026,12.5));
#420087=CARTESIAN_POINT('',(1.25,-0.721687836487026,12.5));
#420088=CARTESIAN_POINT('',(4.15041292089432E-16,-1.44337567297406,12.5));
#420089=CARTESIAN_POINT('Origin',(0.,1.25,12.5));
#420090=CARTESIAN_POINT('',(4.15041292089432E-16,-1.44337567297406,12.5));
#420091=CARTESIAN_POINT('',(4.15041292089432E-16,-1.44337567297406,12.5));
#420092=CARTESIAN_POINT('',(-1.25,-0.721687836487026,12.5));
#420093=CARTESIAN_POINT('Origin',(0.,1.25,12.5));
#420094=CARTESIAN_POINT('',(-1.25,-0.721687836487026,12.5));
#420095=CARTESIAN_POINT('',(-1.25,-0.721687836487026,12.5));
#420096=CARTESIAN_POINT('',(-1.25,0.721687836487034,12.5));
#420097=CARTESIAN_POINT('Origin',(0.,1.25,12.5));
#420098=CARTESIAN_POINT('',(-1.25,0.721687836487034,12.5));
#420099=CARTESIAN_POINT('',(-1.25,0.721687836487034,12.5));
#420100=CARTESIAN_POINT('',(0.,1.44337567297406,12.5));
#420101=CARTESIAN_POINT('Origin',(0.,2.49354920651117,14.));
#420102=CARTESIAN_POINT('',(-2.16840434497101E-15,1.44337567297406,14.));
#420103=CARTESIAN_POINT('',(-1.25,0.721687836487034,14.));
#420104=CARTESIAN_POINT('Origin',(0.,-1.34815096107107E-30,14.));
#420105=CARTESIAN_POINT('Origin',(0.,-1.34815096107107E-30,14.));
#420106=CARTESIAN_POINT('',(1.23599047663348E-14,-1.44337567297406,14.));
#420107=CARTESIAN_POINT('Origin',(0.,-1.34815096107107E-30,14.));
#420108=CARTESIAN_POINT('',(-1.25,-0.721687836487034,14.));
#420109=CARTESIAN_POINT('Origin',(0.,-1.34815096107107E-30,14.));
#420110=CARTESIAN_POINT('Origin',(0.,-1.34815096107107E-30,14.));
#420111=CARTESIAN_POINT('Origin',(0.,2.60208521396521E-15,13.7435492065112));
#420112=CARTESIAN_POINT('Origin',(-0.171343724478305,2.65368348412408,13.7420545896475));
#420113=CARTESIAN_POINT('Origin',(-0.0447891730027414,2.65651366302394,
13.7415084174035));
#420114=CARTESIAN_POINT('Origin',(1.25,0.721687836487034,12.5));
#420115=CARTESIAN_POINT('',(1.25,0.721687836487034,12.5));
#420116=CARTESIAN_POINT('Ctrl Pts',(4.61486004131587E-15,1.44337567297406,
14.));
#420117=CARTESIAN_POINT('Ctrl Pts',(0.624999999999999,1.08253175473055,
13.6391560817565));
#420118=CARTESIAN_POINT('Ctrl Pts',(1.24999999999999,0.721687836487036,
14.));
#420119=CARTESIAN_POINT('',(0.,1.44337567297406,12.5));
#420120=CARTESIAN_POINT('',(0.,1.44337567297406,12.5));
#420121=CARTESIAN_POINT('',(1.25,0.721687836487034,12.5));
#420122=CARTESIAN_POINT('Origin',(1.25,-0.721687836487026,12.5));
#420123=CARTESIAN_POINT('',(1.25,-0.721687836487026,12.5));
#420124=CARTESIAN_POINT('Origin',(4.15041292089432E-16,-1.44337567297406,
12.5));
#420125=CARTESIAN_POINT('',(4.15041292089432E-16,-1.44337567297406,12.5));
#420126=CARTESIAN_POINT('Ctrl Pts',(1.24999999999999,-0.721687836487028,
14.));
#420127=CARTESIAN_POINT('Ctrl Pts',(0.624999999999999,-1.08253175473054,
13.6391560817565));
#420128=CARTESIAN_POINT('Ctrl Pts',(6.39603409235004E-15,-1.44337567297405,
14.));
#420129=CARTESIAN_POINT('Origin',(-1.25,-0.721687836487026,12.5));
#420130=CARTESIAN_POINT('',(-1.25,-0.721687836487026,12.5));
#420131=CARTESIAN_POINT('Ctrl Pts',(5.2220784678048E-15,-1.44337567297406,
14.));
#420132=CARTESIAN_POINT('Ctrl Pts',(-0.624999999999994,-1.08253175473054,
13.6391560817565));
#420133=CARTESIAN_POINT('Ctrl Pts',(-1.24999999999999,-0.721687836487029,
14.));
#420134=CARTESIAN_POINT('Origin',(-1.25,0.721687836487034,12.5));
#420135=CARTESIAN_POINT('',(-1.25,0.721687836487034,12.5));
#420136=CARTESIAN_POINT('Ctrl Pts',(-1.25,-0.721687836487024,14.));
#420137=CARTESIAN_POINT('Ctrl Pts',(-1.25,1.77635683940025E-15,13.6391560817565));
#420138=CARTESIAN_POINT('Ctrl Pts',(-1.25,0.721687836487028,14.));
#420139=CARTESIAN_POINT('Origin',(0.,1.44337567297406,12.5));
#420140=CARTESIAN_POINT('Ctrl Pts',(-1.24999999999999,0.721687836487037,
14.));
#420141=CARTESIAN_POINT('Ctrl Pts',(-0.624999999999999,1.08253175473055,
13.6391560817565));
#420142=CARTESIAN_POINT('Ctrl Pts',(-5.38400338153518E-15,1.44337567297406,
14.));
#420143=CARTESIAN_POINT('',(0.,1.44337567297406,12.5));
#420144=CARTESIAN_POINT('Origin',(0.,1.25,12.5));
#420145=CARTESIAN_POINT('Origin',(0.,-1.34815096107107E-30,14.));
#420146=CARTESIAN_POINT('Origin',(0.,-1.34815096107107E-30,14.));
#420147=CARTESIAN_POINT('Origin',(0.,-1.34815096107107E-30,14.));
#420148=CARTESIAN_POINT('Origin',(0.,-1.34815096107107E-30,14.));
#420149=CARTESIAN_POINT('Origin',(0.,-1.34815096107107E-30,14.));
#420150=CARTESIAN_POINT('Origin',(0.,2.54061283442571E-15,-14.));
#420151=CARTESIAN_POINT('Ctrl Pts',(0.,1.52706329386832,-13.984375));
#420152=CARTESIAN_POINT('Ctrl Pts',(-0.881650403784468,1.52706329386832,
-13.9427083333333));
#420153=CARTESIAN_POINT('Ctrl Pts',(-1.3224756056767,0.76353164693416,-13.9010416666667));
#420154=CARTESIAN_POINT('Ctrl Pts',(-1.76330080756894,2.64858386892187E-15,
-13.859375));
#420155=CARTESIAN_POINT('Ctrl Pts',(-1.3224756056767,-0.763531646934155,
-13.8177083333333));
#420156=CARTESIAN_POINT('Ctrl Pts',(-0.881650403784469,-1.52706329386831,
-13.7760416666666));
#420157=CARTESIAN_POINT('Ctrl Pts',(-1.87011317493125E-16,-1.52706329386831,
-13.734375));
#420158=CARTESIAN_POINT('Ctrl Pts',(0.881650403784467,-1.52706329386831,
-13.6927083333333));
#420159=CARTESIAN_POINT('Ctrl Pts',(1.3224756056767,-0.763531646934156,
-13.6510416666667));
#420160=CARTESIAN_POINT('Ctrl Pts',(1.76330080756894,2.21669973093722E-15,
-13.609375));
#420161=CARTESIAN_POINT('Ctrl Pts',(1.3224756056767,0.763531646934159,-13.5677083333333));
#420162=CARTESIAN_POINT('Ctrl Pts',(0.881650403784469,1.52706329386832,
-13.5260416666666));
#420163=CARTESIAN_POINT('Ctrl Pts',(0.,1.52706329386832,-13.484375));
#420164=CARTESIAN_POINT('Ctrl Pts',(-0.881650403784468,1.52706329386832,
-13.4427083333333));
#420165=CARTESIAN_POINT('Ctrl Pts',(-1.3224756056767,0.76353164693416,-13.4010416666666));
#420166=CARTESIAN_POINT('Ctrl Pts',(-1.76330080756894,2.64858386892187E-15,
-13.359375));
#420167=CARTESIAN_POINT('Ctrl Pts',(-1.3224756056767,-0.763531646934155,
-13.3177083333333));
#420168=CARTESIAN_POINT('Ctrl Pts',(-0.881650403784469,-1.52706329386831,
-13.2760416666666));
#420169=CARTESIAN_POINT('Ctrl Pts',(-1.87011317493125E-16,-1.52706329386831,
-13.234375));
#420170=CARTESIAN_POINT('Ctrl Pts',(0.881650403784467,-1.52706329386831,
-13.1927083333333));
#420171=CARTESIAN_POINT('Ctrl Pts',(1.3224756056767,-0.763531646934156,
-13.1510416666667));
#420172=CARTESIAN_POINT('Ctrl Pts',(1.76330080756894,2.21669973093722E-15,
-13.109375));
#420173=CARTESIAN_POINT('Ctrl Pts',(1.3224756056767,0.763531646934159,-13.0677083333333));
#420174=CARTESIAN_POINT('Ctrl Pts',(0.881650403784469,1.52706329386832,
-13.0260416666667));
#420175=CARTESIAN_POINT('Ctrl Pts',(0.,1.52706329386832,-12.984375));
#420176=CARTESIAN_POINT('Ctrl Pts',(-0.881650403784468,1.52706329386832,
-12.9427083333333));
#420177=CARTESIAN_POINT('Ctrl Pts',(-1.3224756056767,0.76353164693416,-12.9010416666666));
#420178=CARTESIAN_POINT('Ctrl Pts',(-1.76330080756894,2.64858386892187E-15,
-12.859375));
#420179=CARTESIAN_POINT('Ctrl Pts',(-1.3224756056767,-0.763531646934155,
-12.8177083333333));
#420180=CARTESIAN_POINT('Ctrl Pts',(-0.881650403784469,-1.52706329386831,
-12.7760416666666));
#420181=CARTESIAN_POINT('Ctrl Pts',(-1.87011317493125E-16,-1.52706329386831,
-12.734375));
#420182=CARTESIAN_POINT('Ctrl Pts',(0.881650403784467,-1.52706329386831,
-12.6927083333333));
#420183=CARTESIAN_POINT('Ctrl Pts',(1.3224756056767,-0.763531646934156,
-12.6510416666666));
#420184=CARTESIAN_POINT('Ctrl Pts',(1.76330080756894,2.21669973093722E-15,
-12.609375));
#420185=CARTESIAN_POINT('Ctrl Pts',(1.3224756056767,0.763531646934159,-12.5677083333333));
#420186=CARTESIAN_POINT('Ctrl Pts',(0.881650403784469,1.52706329386832,
-12.5260416666666));
#420187=CARTESIAN_POINT('Ctrl Pts',(0.,1.52706329386832,-12.484375));
#420188=CARTESIAN_POINT('Ctrl Pts',(-0.881650403784468,1.52706329386832,
-12.4427083333333));
#420189=CARTESIAN_POINT('Ctrl Pts',(-1.3224756056767,0.76353164693416,-12.4010416666666));
#420190=CARTESIAN_POINT('Ctrl Pts',(-1.76330080756894,2.64858386892187E-15,
-12.359375));
#420191=CARTESIAN_POINT('Ctrl Pts',(-1.3224756056767,-0.763531646934155,
-12.3177083333333));
#420192=CARTESIAN_POINT('Ctrl Pts',(-0.881650403784469,-1.52706329386831,
-12.2760416666666));
#420193=CARTESIAN_POINT('Ctrl Pts',(-1.87011317493125E-16,-1.52706329386831,
-12.234375));
#420194=CARTESIAN_POINT('Ctrl Pts',(0.881650403784467,-1.52706329386831,
-12.1927083333333));
#420195=CARTESIAN_POINT('Ctrl Pts',(1.3224756056767,-0.763531646934156,
-12.1510416666666));
#420196=CARTESIAN_POINT('Ctrl Pts',(1.76330080756894,2.21669973093722E-15,
-12.109375));
#420197=CARTESIAN_POINT('Ctrl Pts',(1.3224756056767,0.763531646934159,-12.0677083333333));
#420198=CARTESIAN_POINT('Ctrl Pts',(0.881650403784469,1.52706329386832,
-12.0260416666667));
#420199=CARTESIAN_POINT('Ctrl Pts',(0.,1.52706329386832,-11.984375));
#420200=CARTESIAN_POINT('Ctrl Pts',(-0.881650403784468,1.52706329386832,
-11.9427083333333));
#420201=CARTESIAN_POINT('Ctrl Pts',(-1.3224756056767,0.76353164693416,-11.9010416666667));
#420202=CARTESIAN_POINT('Ctrl Pts',(-1.76330080756894,2.64858386892187E-15,
-11.859375));
#420203=CARTESIAN_POINT('Ctrl Pts',(-1.3224756056767,-0.763531646934155,
-11.8177083333333));
#420204=CARTESIAN_POINT('Ctrl Pts',(-0.881650403784469,-1.52706329386831,
-11.7760416666666));
#420205=CARTESIAN_POINT('Ctrl Pts',(-1.87011317493125E-16,-1.52706329386831,
-11.734375));
#420206=CARTESIAN_POINT('Ctrl Pts',(0.881650403784467,-1.52706329386831,
-11.6927083333333));
#420207=CARTESIAN_POINT('Ctrl Pts',(1.3224756056767,-0.763531646934156,
-11.6510416666666));
#420208=CARTESIAN_POINT('Ctrl Pts',(1.76330080756894,2.21669973093722E-15,
-11.609375));
#420209=CARTESIAN_POINT('Ctrl Pts',(1.3224756056767,0.763531646934159,-11.5677083333333));
#420210=CARTESIAN_POINT('Ctrl Pts',(0.881650403784469,1.52706329386832,
-11.5260416666666));
#420211=CARTESIAN_POINT('Ctrl Pts',(0.,1.52706329386832,-11.484375));
#420212=CARTESIAN_POINT('Ctrl Pts',(-0.881650403784468,1.52706329386832,
-11.4427083333333));
#420213=CARTESIAN_POINT('Ctrl Pts',(-1.3224756056767,0.76353164693416,-11.4010416666667));
#420214=CARTESIAN_POINT('Ctrl Pts',(-1.76330080756894,2.64858386892187E-15,
-11.359375));
#420215=CARTESIAN_POINT('Ctrl Pts',(-1.3224756056767,-0.763531646934155,
-11.3177083333333));
#420216=CARTESIAN_POINT('Ctrl Pts',(-0.881650403784469,-1.52706329386831,
-11.2760416666667));
#420217=CARTESIAN_POINT('Ctrl Pts',(-1.87011317493125E-16,-1.52706329386831,
-11.234375));
#420218=CARTESIAN_POINT('Ctrl Pts',(0.881650403784467,-1.52706329386831,
-11.1927083333333));
#420219=CARTESIAN_POINT('Ctrl Pts',(1.3224756056767,-0.763531646934156,
-11.1510416666666));
#420220=CARTESIAN_POINT('Ctrl Pts',(1.76330080756894,2.21669973093722E-15,
-11.109375));
#420221=CARTESIAN_POINT('Ctrl Pts',(1.3224756056767,0.763531646934159,-11.0677083333333));
#420222=CARTESIAN_POINT('Ctrl Pts',(0.881650403784469,1.52706329386832,
-11.0260416666666));
#420223=CARTESIAN_POINT('Ctrl Pts',(0.,1.52706329386832,-10.984375));
#420224=CARTESIAN_POINT('Ctrl Pts',(-0.881650403784468,1.52706329386832,
-10.9427083333333));
#420225=CARTESIAN_POINT('Ctrl Pts',(-1.3224756056767,0.76353164693416,-10.9010416666666));
#420226=CARTESIAN_POINT('Ctrl Pts',(-1.76330080756894,2.64858386892187E-15,
-10.859375));
#420227=CARTESIAN_POINT('Ctrl Pts',(-1.3224756056767,-0.763531646934155,
-10.8177083333333));
#420228=CARTESIAN_POINT('Ctrl Pts',(-0.881650403784469,-1.52706329386831,
-10.7760416666666));
#420229=CARTESIAN_POINT('Ctrl Pts',(-1.87011317493125E-16,-1.52706329386831,
-10.734375));
#420230=CARTESIAN_POINT('Ctrl Pts',(0.881650403784467,-1.52706329386831,
-10.6927083333333));
#420231=CARTESIAN_POINT('Ctrl Pts',(1.3224756056767,-0.763531646934156,
-10.6510416666667));
#420232=CARTESIAN_POINT('Ctrl Pts',(1.76330080756894,2.21669973093722E-15,
-10.609375));
#420233=CARTESIAN_POINT('Ctrl Pts',(1.3224756056767,0.763531646934159,-10.5677083333333));
#420234=CARTESIAN_POINT('Ctrl Pts',(0.881650403784469,1.52706329386832,
-10.5260416666667));
#420235=CARTESIAN_POINT('Ctrl Pts',(0.,1.52706329386832,-10.484375));
#420236=CARTESIAN_POINT('Ctrl Pts',(-0.881650403784468,1.52706329386832,
-10.4427083333333));
#420237=CARTESIAN_POINT('Ctrl Pts',(-1.3224756056767,0.76353164693416,-10.4010416666666));
#420238=CARTESIAN_POINT('Ctrl Pts',(-1.76330080756894,2.64858386892187E-15,
-10.359375));
#420239=CARTESIAN_POINT('Ctrl Pts',(-1.3224756056767,-0.763531646934155,
-10.3177083333333));
#420240=CARTESIAN_POINT('Ctrl Pts',(-0.881650403784469,-1.52706329386831,
-10.2760416666667));
#420241=CARTESIAN_POINT('Ctrl Pts',(-1.87011317493125E-16,-1.52706329386831,
-10.234375));
#420242=CARTESIAN_POINT('Ctrl Pts',(0.881650403784467,-1.52706329386831,
-10.1927083333333));
#420243=CARTESIAN_POINT('Ctrl Pts',(1.3224756056767,-0.763531646934156,
-10.1510416666667));
#420244=CARTESIAN_POINT('Ctrl Pts',(1.76330080756894,2.21669973093722E-15,
-10.109375));
#420245=CARTESIAN_POINT('Ctrl Pts',(1.3224756056767,0.763531646934159,-10.0677083333333));
#420246=CARTESIAN_POINT('Ctrl Pts',(0.881650403784469,1.52706329386832,
-10.0260416666666));
#420247=CARTESIAN_POINT('Ctrl Pts',(0.,1.52706329386832,-9.98437499999998));
#420248=CARTESIAN_POINT('Ctrl Pts',(-0.881650403784468,1.52706329386832,
-9.94270833333331));
#420249=CARTESIAN_POINT('Ctrl Pts',(-1.3224756056767,0.76353164693416,-9.90104166666665));
#420250=CARTESIAN_POINT('Ctrl Pts',(-1.76330080756894,2.64858386892187E-15,
-9.85937499999998));
#420251=CARTESIAN_POINT('Ctrl Pts',(-1.3224756056767,-0.763531646934155,
-9.81770833333331));
#420252=CARTESIAN_POINT('Ctrl Pts',(-0.881650403784469,-1.52706329386831,
-9.77604166666665));
#420253=CARTESIAN_POINT('Ctrl Pts',(-1.87011317493125E-16,-1.52706329386831,
-9.73437499999998));
#420254=CARTESIAN_POINT('Ctrl Pts',(0.881650403784467,-1.52706329386831,
-9.69270833333331));
#420255=CARTESIAN_POINT('Ctrl Pts',(1.3224756056767,-0.763531646934156,
-9.65104166666665));
#420256=CARTESIAN_POINT('Ctrl Pts',(1.76330080756894,2.21669973093722E-15,
-9.60937499999998));
#420257=CARTESIAN_POINT('Ctrl Pts',(1.3224756056767,0.763531646934159,-9.56770833333331));
#420258=CARTESIAN_POINT('Ctrl Pts',(0.881650403784469,1.52706329386832,
-9.52604166666665));
#420259=CARTESIAN_POINT('Ctrl Pts',(0.,1.52706329386832,-9.48437499999998));
#420260=CARTESIAN_POINT('Ctrl Pts',(-0.881650403784468,1.52706329386832,
-9.44270833333331));
#420261=CARTESIAN_POINT('Ctrl Pts',(-1.3224756056767,0.76353164693416,-9.40104166666665));
#420262=CARTESIAN_POINT('Ctrl Pts',(-1.76330080756894,2.64858386892187E-15,
-9.35937499999998));
#420263=CARTESIAN_POINT('Ctrl Pts',(-1.3224756056767,-0.763531646934155,
-9.31770833333331));
#420264=CARTESIAN_POINT('Ctrl Pts',(-0.881650403784469,-1.52706329386831,
-9.27604166666665));
#420265=CARTESIAN_POINT('Ctrl Pts',(-1.87011317493125E-16,-1.52706329386831,
-9.23437499999998));
#420266=CARTESIAN_POINT('Ctrl Pts',(0.881650403784467,-1.52706329386831,
-9.19270833333332));
#420267=CARTESIAN_POINT('Ctrl Pts',(1.3224756056767,-0.763531646934156,
-9.15104166666665));
#420268=CARTESIAN_POINT('Ctrl Pts',(1.76330080756894,2.21669973093722E-15,
-9.10937499999998));
#420269=CARTESIAN_POINT('Ctrl Pts',(1.3224756056767,0.763531646934159,-9.06770833333331));
#420270=CARTESIAN_POINT('Ctrl Pts',(0.881650403784469,1.52706329386832,
-9.02604166666665));
#420271=CARTESIAN_POINT('Ctrl Pts',(0.,1.52706329386832,-8.98437499999998));
#420272=CARTESIAN_POINT('Ctrl Pts',(-0.881650403784468,1.52706329386832,
-8.94270833333331));
#420273=CARTESIAN_POINT('Ctrl Pts',(-1.3224756056767,0.76353164693416,-8.90104166666665));
#420274=CARTESIAN_POINT('Ctrl Pts',(-1.76330080756894,2.64858386892187E-15,
-8.85937499999998));
#420275=CARTESIAN_POINT('Ctrl Pts',(-1.3224756056767,-0.763531646934155,
-8.81770833333331));
#420276=CARTESIAN_POINT('Ctrl Pts',(-0.881650403784469,-1.52706329386831,
-8.77604166666665));
#420277=CARTESIAN_POINT('Ctrl Pts',(-1.87011317493125E-16,-1.52706329386831,
-8.73437499999998));
#420278=CARTESIAN_POINT('Ctrl Pts',(0.881650403784467,-1.52706329386831,
-8.69270833333331));
#420279=CARTESIAN_POINT('Ctrl Pts',(1.3224756056767,-0.763531646934156,
-8.65104166666665));
#420280=CARTESIAN_POINT('Ctrl Pts',(1.76330080756894,2.21669973093722E-15,
-8.60937499999998));
#420281=CARTESIAN_POINT('Ctrl Pts',(1.3224756056767,0.763531646934159,-8.56770833333331));
#420282=CARTESIAN_POINT('Ctrl Pts',(0.881650403784469,1.52706329386832,
-8.52604166666665));
#420283=CARTESIAN_POINT('Ctrl Pts',(0.,1.52706329386832,-8.48437499999998));
#420284=CARTESIAN_POINT('Ctrl Pts',(-0.881650403784468,1.52706329386832,
-8.44270833333332));
#420285=CARTESIAN_POINT('Ctrl Pts',(-1.3224756056767,0.76353164693416,-8.40104166666665));
#420286=CARTESIAN_POINT('Ctrl Pts',(-1.76330080756894,2.64858386892187E-15,
-8.35937499999998));
#420287=CARTESIAN_POINT('Ctrl Pts',(-1.3224756056767,-0.763531646934155,
-8.31770833333332));
#420288=CARTESIAN_POINT('Ctrl Pts',(-0.881650403784469,-1.52706329386831,
-8.27604166666665));
#420289=CARTESIAN_POINT('Ctrl Pts',(-1.87011317493125E-16,-1.52706329386831,
-8.23437499999998));
#420290=CARTESIAN_POINT('Ctrl Pts',(0.881650403784467,-1.52706329386831,
-8.19270833333332));
#420291=CARTESIAN_POINT('Ctrl Pts',(1.3224756056767,-0.763531646934156,
-8.15104166666665));
#420292=CARTESIAN_POINT('Ctrl Pts',(1.76330080756894,2.21669973093722E-15,
-8.10937499999998));
#420293=CARTESIAN_POINT('Ctrl Pts',(1.3224756056767,0.763531646934159,-8.06770833333332));
#420294=CARTESIAN_POINT('Ctrl Pts',(0.881650403784469,1.52706329386832,
-8.02604166666665));
#420295=CARTESIAN_POINT('Ctrl Pts',(0.,1.52706329386832,-7.98437499999998));
#420296=CARTESIAN_POINT('Ctrl Pts',(-0.881650403784468,1.52706329386832,
-7.94270833333332));
#420297=CARTESIAN_POINT('Ctrl Pts',(-1.3224756056767,0.76353164693416,-7.90104166666665));
#420298=CARTESIAN_POINT('Ctrl Pts',(-1.76330080756894,2.64858386892187E-15,
-7.85937499999998));
#420299=CARTESIAN_POINT('Ctrl Pts',(-1.3224756056767,-0.763531646934155,
-7.81770833333332));
#420300=CARTESIAN_POINT('Ctrl Pts',(-0.881650403784469,-1.52706329386831,
-7.77604166666665));
#420301=CARTESIAN_POINT('Ctrl Pts',(-1.87011317493125E-16,-1.52706329386831,
-7.73437499999998));
#420302=CARTESIAN_POINT('Ctrl Pts',(0.881650403784467,-1.52706329386831,
-7.69270833333331));
#420303=CARTESIAN_POINT('Ctrl Pts',(1.3224756056767,-0.763531646934156,
-7.65104166666665));
#420304=CARTESIAN_POINT('Ctrl Pts',(1.76330080756894,2.21669973093722E-15,
-7.60937499999998));
#420305=CARTESIAN_POINT('Ctrl Pts',(1.3224756056767,0.763531646934159,-7.56770833333332));
#420306=CARTESIAN_POINT('Ctrl Pts',(0.881650403784469,1.52706329386832,
-7.52604166666665));
#420307=CARTESIAN_POINT('Ctrl Pts',(0.,1.52706329386832,-7.48437499999998));
#420308=CARTESIAN_POINT('Ctrl Pts',(-0.881650403784468,1.52706329386832,
-7.44270833333332));
#420309=CARTESIAN_POINT('Ctrl Pts',(-1.3224756056767,0.76353164693416,-7.40104166666665));
#420310=CARTESIAN_POINT('Ctrl Pts',(-1.76330080756894,2.64858386892187E-15,
-7.35937499999998));
#420311=CARTESIAN_POINT('Ctrl Pts',(-1.3224756056767,-0.763531646934155,
-7.31770833333332));
#420312=CARTESIAN_POINT('Ctrl Pts',(-0.881650403784469,-1.52706329386831,
-7.27604166666665));
#420313=CARTESIAN_POINT('Ctrl Pts',(-1.87011317493125E-16,-1.52706329386831,
-7.23437499999998));
#420314=CARTESIAN_POINT('Ctrl Pts',(0.881650403784467,-1.52706329386831,
-7.19270833333332));
#420315=CARTESIAN_POINT('Ctrl Pts',(1.3224756056767,-0.763531646934156,
-7.15104166666665));
#420316=CARTESIAN_POINT('Ctrl Pts',(1.76330080756894,2.21669973093722E-15,
-7.10937499999998));
#420317=CARTESIAN_POINT('Ctrl Pts',(1.3224756056767,0.763531646934159,-7.06770833333331));
#420318=CARTESIAN_POINT('Ctrl Pts',(0.881650403784469,1.52706329386832,
-7.02604166666665));
#420319=CARTESIAN_POINT('Ctrl Pts',(0.,1.52706329386832,-6.98437499999998));
#420320=CARTESIAN_POINT('Ctrl Pts',(-0.881650403784468,1.52706329386832,
-6.94270833333332));
#420321=CARTESIAN_POINT('Ctrl Pts',(-1.3224756056767,0.76353164693416,-6.90104166666665));
#420322=CARTESIAN_POINT('Ctrl Pts',(-1.76330080756894,2.64858386892187E-15,
-6.85937499999998));
#420323=CARTESIAN_POINT('Ctrl Pts',(-1.3224756056767,-0.763531646934155,
-6.81770833333331));
#420324=CARTESIAN_POINT('Ctrl Pts',(-0.881650403784469,-1.52706329386831,
-6.77604166666665));
#420325=CARTESIAN_POINT('Ctrl Pts',(-1.87011317493125E-16,-1.52706329386831,
-6.73437499999998));
#420326=CARTESIAN_POINT('Ctrl Pts',(0.881650403784467,-1.52706329386831,
-6.69270833333332));
#420327=CARTESIAN_POINT('Ctrl Pts',(1.3224756056767,-0.763531646934156,
-6.65104166666665));
#420328=CARTESIAN_POINT('Ctrl Pts',(1.76330080756894,2.21669973093722E-15,
-6.60937499999998));
#420329=CARTESIAN_POINT('Ctrl Pts',(1.3224756056767,0.763531646934159,-6.56770833333332));
#420330=CARTESIAN_POINT('Ctrl Pts',(0.881650403784469,1.52706329386832,
-6.52604166666665));
#420331=CARTESIAN_POINT('Ctrl Pts',(0.,1.52706329386832,-6.48437499999998));
#420332=CARTESIAN_POINT('Ctrl Pts',(-0.881650403784468,1.52706329386832,
-6.44270833333332));
#420333=CARTESIAN_POINT('Ctrl Pts',(-1.3224756056767,0.76353164693416,-6.40104166666665));
#420334=CARTESIAN_POINT('Ctrl Pts',(-1.76330080756894,2.64858386892187E-15,
-6.35937499999998));
#420335=CARTESIAN_POINT('Ctrl Pts',(-1.3224756056767,-0.763531646934155,
-6.31770833333332));
#420336=CARTESIAN_POINT('Ctrl Pts',(-0.881650403784469,-1.52706329386831,
-6.27604166666665));
#420337=CARTESIAN_POINT('Ctrl Pts',(-1.87011317493125E-16,-1.52706329386831,
-6.23437499999998));
#420338=CARTESIAN_POINT('Ctrl Pts',(0.881650403784467,-1.52706329386831,
-6.19270833333332));
#420339=CARTESIAN_POINT('Ctrl Pts',(1.3224756056767,-0.763531646934156,
-6.15104166666665));
#420340=CARTESIAN_POINT('Ctrl Pts',(1.76330080756894,2.21669973093722E-15,
-6.10937499999998));
#420341=CARTESIAN_POINT('Ctrl Pts',(1.3224756056767,0.763531646934159,-6.06770833333332));
#420342=CARTESIAN_POINT('Ctrl Pts',(0.881650403784469,1.52706329386832,
-6.02604166666665));
#420343=CARTESIAN_POINT('Ctrl Pts',(0.,1.52706329386832,-5.98437499999998));
#420344=CARTESIAN_POINT('Ctrl Pts',(-0.881650403784468,1.52706329386832,
-5.94270833333331));
#420345=CARTESIAN_POINT('Ctrl Pts',(-1.3224756056767,0.76353164693416,-5.90104166666665));
#420346=CARTESIAN_POINT('Ctrl Pts',(-1.76330080756894,2.64858386892187E-15,
-5.85937499999998));
#420347=CARTESIAN_POINT('Ctrl Pts',(-1.3224756056767,-0.763531646934155,
-5.81770833333332));
#420348=CARTESIAN_POINT('Ctrl Pts',(-0.881650403784469,-1.52706329386831,
-5.77604166666665));
#420349=CARTESIAN_POINT('Ctrl Pts',(-1.87011317493125E-16,-1.52706329386831,
-5.73437499999998));
#420350=CARTESIAN_POINT('Ctrl Pts',(0.881650403784467,-1.52706329386831,
-5.69270833333332));
#420351=CARTESIAN_POINT('Ctrl Pts',(1.3224756056767,-0.763531646934156,
-5.65104166666665));
#420352=CARTESIAN_POINT('Ctrl Pts',(1.76330080756894,2.21669973093722E-15,
-5.60937499999998));
#420353=CARTESIAN_POINT('Ctrl Pts',(1.3224756056767,0.763531646934159,-5.56770833333332));
#420354=CARTESIAN_POINT('Ctrl Pts',(0.881650403784469,1.52706329386832,
-5.52604166666665));
#420355=CARTESIAN_POINT('Ctrl Pts',(0.,1.52706329386832,-5.48437499999998));
#420356=CARTESIAN_POINT('Ctrl Pts',(-0.881650403784468,1.52706329386832,
-5.44270833333332));
#420357=CARTESIAN_POINT('Ctrl Pts',(-1.3224756056767,0.76353164693416,-5.40104166666665));
#420358=CARTESIAN_POINT('Ctrl Pts',(-1.76330080756894,2.64858386892187E-15,
-5.35937499999998));
#420359=CARTESIAN_POINT('Ctrl Pts',(-1.3224756056767,-0.763531646934155,
-5.31770833333332));
#420360=CARTESIAN_POINT('Ctrl Pts',(-0.881650403784469,-1.52706329386831,
-5.27604166666665));
#420361=CARTESIAN_POINT('Ctrl Pts',(-1.87011317493125E-16,-1.52706329386831,
-5.23437499999998));
#420362=CARTESIAN_POINT('Ctrl Pts',(0.881650403784467,-1.52706329386831,
-5.19270833333331));
#420363=CARTESIAN_POINT('Ctrl Pts',(1.3224756056767,-0.763531646934156,
-5.15104166666665));
#420364=CARTESIAN_POINT('Ctrl Pts',(1.76330080756894,2.21669973093722E-15,
-5.10937499999998));
#420365=CARTESIAN_POINT('Ctrl Pts',(1.3224756056767,0.763531646934159,-5.06770833333332));
#420366=CARTESIAN_POINT('Ctrl Pts',(0.881650403784469,1.52706329386832,
-5.02604166666665));
#420367=CARTESIAN_POINT('Ctrl Pts',(0.,1.52706329386832,-4.98437499999998));
#420368=CARTESIAN_POINT('Ctrl Pts',(-0.881650403784468,1.52706329386832,
-4.94270833333331));
#420369=CARTESIAN_POINT('Ctrl Pts',(-1.3224756056767,0.76353164693416,-4.90104166666665));
#420370=CARTESIAN_POINT('Ctrl Pts',(-1.76330080756894,2.64858386892187E-15,
-4.85937499999998));
#420371=CARTESIAN_POINT('Ctrl Pts',(-1.3224756056767,-0.763531646934155,
-4.81770833333331));
#420372=CARTESIAN_POINT('Ctrl Pts',(-0.881650403784469,-1.52706329386831,
-4.77604166666665));
#420373=CARTESIAN_POINT('Ctrl Pts',(-1.87011317493125E-16,-1.52706329386831,
-4.73437499999998));
#420374=CARTESIAN_POINT('Ctrl Pts',(0.881650403784467,-1.52706329386831,
-4.69270833333331));
#420375=CARTESIAN_POINT('Ctrl Pts',(1.3224756056767,-0.763531646934156,
-4.65104166666665));
#420376=CARTESIAN_POINT('Ctrl Pts',(1.76330080756894,2.21669973093722E-15,
-4.60937499999998));
#420377=CARTESIAN_POINT('Ctrl Pts',(1.3224756056767,0.763531646934159,-4.56770833333331));
#420378=CARTESIAN_POINT('Ctrl Pts',(0.881650403784469,1.52706329386832,
-4.52604166666665));
#420379=CARTESIAN_POINT('Ctrl Pts',(0.,1.52706329386832,-4.48437499999998));
#420380=CARTESIAN_POINT('Ctrl Pts',(-0.881650403784468,1.52706329386832,
-4.44270833333331));
#420381=CARTESIAN_POINT('Ctrl Pts',(-1.3224756056767,0.76353164693416,-4.40104166666665));
#420382=CARTESIAN_POINT('Ctrl Pts',(-1.76330080756894,2.64858386892187E-15,
-4.35937499999998));
#420383=CARTESIAN_POINT('Ctrl Pts',(-1.3224756056767,-0.763531646934155,
-4.31770833333331));
#420384=CARTESIAN_POINT('Ctrl Pts',(-0.881650403784469,-1.52706329386831,
-4.27604166666665));
#420385=CARTESIAN_POINT('Ctrl Pts',(-1.87011317493125E-16,-1.52706329386831,
-4.23437499999998));
#420386=CARTESIAN_POINT('Ctrl Pts',(0.881650403784467,-1.52706329386831,
-4.19270833333332));
#420387=CARTESIAN_POINT('Ctrl Pts',(1.3224756056767,-0.763531646934156,
-4.15104166666665));
#420388=CARTESIAN_POINT('Ctrl Pts',(1.76330080756894,2.21669973093722E-15,
-4.10937499999998));
#420389=CARTESIAN_POINT('Ctrl Pts',(1.3224756056767,0.763531646934159,-4.06770833333332));
#420390=CARTESIAN_POINT('Ctrl Pts',(0.881650403784469,1.52706329386832,
-4.02604166666665));
#420391=CARTESIAN_POINT('Ctrl Pts',(0.,1.52706329386832,-3.98437499999998));
#420392=CARTESIAN_POINT('Ctrl Pts',(-0.881650403784468,1.52706329386832,
-3.94270833333332));
#420393=CARTESIAN_POINT('Ctrl Pts',(-1.3224756056767,0.76353164693416,-3.90104166666665));
#420394=CARTESIAN_POINT('Ctrl Pts',(-1.76330080756894,2.64858386892187E-15,
-3.85937499999998));
#420395=CARTESIAN_POINT('Ctrl Pts',(-1.3224756056767,-0.763531646934155,
-3.81770833333332));
#420396=CARTESIAN_POINT('Ctrl Pts',(-0.881650403784469,-1.52706329386831,
-3.77604166666665));
#420397=CARTESIAN_POINT('Ctrl Pts',(-1.87011317493125E-16,-1.52706329386831,
-3.73437499999998));
#420398=CARTESIAN_POINT('Ctrl Pts',(0.881650403784467,-1.52706329386831,
-3.69270833333332));
#420399=CARTESIAN_POINT('Ctrl Pts',(1.3224756056767,-0.763531646934156,
-3.65104166666665));
#420400=CARTESIAN_POINT('Ctrl Pts',(1.76330080756894,2.21669973093722E-15,
-3.60937499999998));
#420401=CARTESIAN_POINT('Ctrl Pts',(1.3224756056767,0.763531646934159,-3.56770833333332));
#420402=CARTESIAN_POINT('Ctrl Pts',(0.881650403784469,1.52706329386832,
-3.52604166666665));
#420403=CARTESIAN_POINT('Ctrl Pts',(0.,1.52706329386832,-3.48437499999998));
#420404=CARTESIAN_POINT('Ctrl Pts',(-0.881650403784468,1.52706329386832,
-3.44270833333332));
#420405=CARTESIAN_POINT('Ctrl Pts',(-1.3224756056767,0.76353164693416,-3.40104166666665));
#420406=CARTESIAN_POINT('Ctrl Pts',(-1.76330080756894,2.64858386892187E-15,
-3.35937499999998));
#420407=CARTESIAN_POINT('Ctrl Pts',(-1.3224756056767,-0.763531646934155,
-3.31770833333332));
#420408=CARTESIAN_POINT('Ctrl Pts',(-0.881650403784469,-1.52706329386831,
-3.27604166666665));
#420409=CARTESIAN_POINT('Ctrl Pts',(-1.87011317493125E-16,-1.52706329386831,
-3.23437499999998));
#420410=CARTESIAN_POINT('Ctrl Pts',(0.881650403784467,-1.52706329386831,
-3.19270833333331));
#420411=CARTESIAN_POINT('Ctrl Pts',(1.3224756056767,-0.763531646934156,
-3.15104166666665));
#420412=CARTESIAN_POINT('Ctrl Pts',(1.76330080756894,2.21669973093722E-15,
-3.10937499999998));
#420413=CARTESIAN_POINT('Ctrl Pts',(1.3224756056767,0.763531646934159,-3.06770833333331));
#420414=CARTESIAN_POINT('Ctrl Pts',(0.881650403784469,1.52706329386832,
-3.02604166666665));
#420415=CARTESIAN_POINT('Ctrl Pts',(0.,1.52706329386832,-2.98437499999998));
#420416=CARTESIAN_POINT('Ctrl Pts',(-0.881650403784468,1.52706329386832,
-2.94270833333331));
#420417=CARTESIAN_POINT('Ctrl Pts',(-1.3224756056767,0.76353164693416,-2.90104166666665));
#420418=CARTESIAN_POINT('Ctrl Pts',(-1.76330080756894,2.64858386892187E-15,
-2.85937499999998));
#420419=CARTESIAN_POINT('Ctrl Pts',(-1.3224756056767,-0.763531646934155,
-2.81770833333331));
#420420=CARTESIAN_POINT('Ctrl Pts',(-0.881650403784469,-1.52706329386831,
-2.77604166666665));
#420421=CARTESIAN_POINT('Ctrl Pts',(-1.87011317493125E-16,-1.52706329386831,
-2.73437499999998));
#420422=CARTESIAN_POINT('Ctrl Pts',(0.881650403784467,-1.52706329386831,
-2.69270833333331));
#420423=CARTESIAN_POINT('Ctrl Pts',(1.3224756056767,-0.763531646934156,
-2.65104166666665));
#420424=CARTESIAN_POINT('Ctrl Pts',(1.76330080756894,2.21669973093722E-15,
-2.60937499999998));
#420425=CARTESIAN_POINT('Ctrl Pts',(1.3224756056767,0.763531646934159,-2.56770833333331));
#420426=CARTESIAN_POINT('Ctrl Pts',(0.881650403784469,1.52706329386832,
-2.52604166666665));
#420427=CARTESIAN_POINT('Ctrl Pts',(0.,1.52706329386832,-2.48437499999998));
#420428=CARTESIAN_POINT('Ctrl Pts',(-0.881650403784468,1.52706329386832,
-2.44270833333331));
#420429=CARTESIAN_POINT('Ctrl Pts',(-1.3224756056767,0.76353164693416,-2.40104166666665));
#420430=CARTESIAN_POINT('Ctrl Pts',(-1.76330080756894,2.64858386892187E-15,
-2.35937499999998));
#420431=CARTESIAN_POINT('Ctrl Pts',(-1.3224756056767,-0.763531646934155,
-2.31770833333332));
#420432=CARTESIAN_POINT('Ctrl Pts',(-0.881650403784469,-1.52706329386831,
-2.27604166666665));
#420433=CARTESIAN_POINT('Ctrl Pts',(-1.87011317493125E-16,-1.52706329386831,
-2.23437499999998));
#420434=CARTESIAN_POINT('Ctrl Pts',(0.881650403784467,-1.52706329386831,
-2.19270833333332));
#420435=CARTESIAN_POINT('Ctrl Pts',(1.3224756056767,-0.763531646934156,
-2.15104166666665));
#420436=CARTESIAN_POINT('Ctrl Pts',(1.76330080756894,2.21669973093722E-15,
-2.10937499999998));
#420437=CARTESIAN_POINT('Ctrl Pts',(1.3224756056767,0.763531646934159,-2.06770833333332));
#420438=CARTESIAN_POINT('Ctrl Pts',(0.881650403784469,1.52706329386832,
-2.02604166666665));
#420439=CARTESIAN_POINT('Ctrl Pts',(0.,1.52706329386832,-1.98437499999998));
#420440=CARTESIAN_POINT('Ctrl Pts',(-0.881650403784468,1.52706329386832,
-1.94270833333332));
#420441=CARTESIAN_POINT('Ctrl Pts',(-1.3224756056767,0.76353164693416,-1.90104166666665));
#420442=CARTESIAN_POINT('Ctrl Pts',(-1.76330080756894,2.64858386892187E-15,
-1.85937499999998));
#420443=CARTESIAN_POINT('Ctrl Pts',(-1.3224756056767,-0.763531646934155,
-1.81770833333332));
#420444=CARTESIAN_POINT('Ctrl Pts',(-0.881650403784469,-1.52706329386831,
-1.77604166666665));
#420445=CARTESIAN_POINT('Ctrl Pts',(-1.87011317493125E-16,-1.52706329386831,
-1.73437499999998));
#420446=CARTESIAN_POINT('Ctrl Pts',(0.881650403784467,-1.52706329386831,
-1.69270833333332));
#420447=CARTESIAN_POINT('Ctrl Pts',(1.3224756056767,-0.763531646934156,
-1.65104166666665));
#420448=CARTESIAN_POINT('Ctrl Pts',(1.76330080756894,2.21669973093722E-15,
-1.60937499999998));
#420449=CARTESIAN_POINT('Ctrl Pts',(1.3224756056767,0.763531646934159,-1.56770833333332));
#420450=CARTESIAN_POINT('Ctrl Pts',(0.881650403784469,1.52706329386832,
-1.52604166666665));
#420451=CARTESIAN_POINT('Ctrl Pts',(0.,1.52706329386832,-1.48437499999998));
#420452=CARTESIAN_POINT('Ctrl Pts',(-0.881650403784468,1.52706329386832,
-1.44270833333332));
#420453=CARTESIAN_POINT('Ctrl Pts',(-1.3224756056767,0.76353164693416,-1.40104166666665));
#420454=CARTESIAN_POINT('Ctrl Pts',(-1.76330080756894,2.64858386892187E-15,
-1.35937499999998));
#420455=CARTESIAN_POINT('Ctrl Pts',(-1.3224756056767,-0.763531646934155,
-1.31770833333331));
#420456=CARTESIAN_POINT('Ctrl Pts',(-0.881650403784469,-1.52706329386831,
-1.27604166666665));
#420457=CARTESIAN_POINT('Ctrl Pts',(-1.87011317493125E-16,-1.52706329386831,
-1.23437499999998));
#420458=CARTESIAN_POINT('Ctrl Pts',(0.881650403784467,-1.52706329386831,
-1.19270833333331));
#420459=CARTESIAN_POINT('Ctrl Pts',(1.3224756056767,-0.763531646934156,
-1.15104166666665));
#420460=CARTESIAN_POINT('Ctrl Pts',(1.76330080756894,2.21669973093722E-15,
-1.10937499999998));
#420461=CARTESIAN_POINT('Ctrl Pts',(1.3224756056767,0.763531646934159,-1.06770833333331));
#420462=CARTESIAN_POINT('Ctrl Pts',(0.881650403784469,1.52706329386832,
-1.02604166666665));
#420463=CARTESIAN_POINT('Ctrl Pts',(0.,1.52706329386832,-0.984374999999982));
#420464=CARTESIAN_POINT('Ctrl Pts',(-0.881650403784468,1.52706329386832,
-0.942708333333315));
#420465=CARTESIAN_POINT('Ctrl Pts',(-1.3224756056767,0.76353164693416,-0.901041666666649));
#420466=CARTESIAN_POINT('Ctrl Pts',(-1.76330080756894,2.64858386892187E-15,
-0.859374999999982));
#420467=CARTESIAN_POINT('Ctrl Pts',(-1.3224756056767,-0.763531646934155,
-0.817708333333314));
#420468=CARTESIAN_POINT('Ctrl Pts',(-0.881650403784469,-1.52706329386831,
-0.776041666666649));
#420469=CARTESIAN_POINT('Ctrl Pts',(-1.87011317493125E-16,-1.52706329386831,
-0.734374999999982));
#420470=CARTESIAN_POINT('Ctrl Pts',(0.881650403784467,-1.52706329386831,
-0.692708333333314));
#420471=CARTESIAN_POINT('Ctrl Pts',(1.3224756056767,-0.763531646934156,
-0.651041666666649));
#420472=CARTESIAN_POINT('Ctrl Pts',(1.76330080756894,2.21669973093722E-15,
-0.609374999999982));
#420473=CARTESIAN_POINT('Ctrl Pts',(1.3224756056767,0.763531646934159,-0.567708333333314));
#420474=CARTESIAN_POINT('Ctrl Pts',(0.881650403784469,1.52706329386832,
-0.526041666666649));
#420475=CARTESIAN_POINT('Ctrl Pts',(0.,1.52706329386832,-0.484374999999981));
#420476=CARTESIAN_POINT('Ctrl Pts',(-0.881650403784468,1.52706329386832,
-0.442708333333316));
#420477=CARTESIAN_POINT('Ctrl Pts',(-1.3224756056767,0.76353164693416,-0.401041666666649));
#420478=CARTESIAN_POINT('Ctrl Pts',(-1.76330080756894,2.64858386892187E-15,
-0.359374999999981));
#420479=CARTESIAN_POINT('Ctrl Pts',(-1.3224756056767,-0.763531646934155,
-0.317708333333316));
#420480=CARTESIAN_POINT('Ctrl Pts',(-0.881650403784469,-1.52706329386831,
-0.276041666666648));
#420481=CARTESIAN_POINT('Ctrl Pts',(-1.87011317493125E-16,-1.52706329386831,
-0.234374999999981));
#420482=CARTESIAN_POINT('Ctrl Pts',(0.881650403784467,-1.52706329386831,
-0.192708333333316));
#420483=CARTESIAN_POINT('Ctrl Pts',(1.3224756056767,-0.763531646934156,
-0.151041666666648));
#420484=CARTESIAN_POINT('Ctrl Pts',(1.76330080756894,2.21669973093722E-15,
-0.109374999999981));
#420485=CARTESIAN_POINT('Ctrl Pts',(1.3224756056767,0.763531646934159,-0.0677083333333155));
#420486=CARTESIAN_POINT('Ctrl Pts',(0.881650403784469,1.52706329386832,
-0.0260416666666482));
#420487=CARTESIAN_POINT('Ctrl Pts',(0.,1.52706329386832,0.0156250000000191));
#420488=CARTESIAN_POINT('Ctrl Pts',(-0.881650403784468,1.52706329386832,
0.0572916666666846));
#420489=CARTESIAN_POINT('Ctrl Pts',(-1.3224756056767,0.76353164693416,0.0989583333333519));
#420490=CARTESIAN_POINT('Ctrl Pts',(-1.76330080756894,2.64858386892187E-15,
0.140625000000017));
#420491=CARTESIAN_POINT('Ctrl Pts',(-1.3224756056767,-0.763531646934155,
0.182291666666685));
#420492=CARTESIAN_POINT('Ctrl Pts',(-0.881650403784469,-1.52706329386831,
0.223958333333352));
#420493=CARTESIAN_POINT('Ctrl Pts',(-1.87011317493125E-16,-1.52706329386831,
0.265625000000018));
#420494=CARTESIAN_POINT('Ctrl Pts',(0.881650403784467,-1.52706329386831,
0.307291666666685));
#420495=CARTESIAN_POINT('Ctrl Pts',(1.3224756056767,-0.763531646934156,
0.348958333333352));
#420496=CARTESIAN_POINT('Ctrl Pts',(1.76330080756894,2.21669973093722E-15,
0.390625000000018));
#420497=CARTESIAN_POINT('Ctrl Pts',(1.3224756056767,0.763531646934159,0.432291666666685));
#420498=CARTESIAN_POINT('Ctrl Pts',(0.881650403784469,1.52706329386832,
0.473958333333352));
#420499=CARTESIAN_POINT('Ctrl Pts',(0.,1.52706329386832,0.515625000000018));
#420500=CARTESIAN_POINT('Ctrl Pts',(-0.881650403784468,1.52706329386832,
0.557291666666685));
#420501=CARTESIAN_POINT('Ctrl Pts',(-1.3224756056767,0.76353164693416,0.598958333333352));
#420502=CARTESIAN_POINT('Ctrl Pts',(-1.76330080756894,2.64858386892187E-15,
0.640625000000018));
#420503=CARTESIAN_POINT('Ctrl Pts',(-1.3224756056767,-0.763531646934155,
0.682291666666685));
#420504=CARTESIAN_POINT('Ctrl Pts',(-0.881650403784469,-1.52706329386831,
0.723958333333353));
#420505=CARTESIAN_POINT('Ctrl Pts',(-1.87011317493125E-16,-1.52706329386831,
0.765625000000018));
#420506=CARTESIAN_POINT('Ctrl Pts',(0.881650403784467,-1.52706329386831,
0.807291666666685));
#420507=CARTESIAN_POINT('Ctrl Pts',(1.3224756056767,-0.763531646934156,
0.848958333333351));
#420508=CARTESIAN_POINT('Ctrl Pts',(1.76330080756894,2.21669973093722E-15,
0.890625000000018));
#420509=CARTESIAN_POINT('Ctrl Pts',(1.3224756056767,0.763531646934159,0.932291666666685));
#420510=CARTESIAN_POINT('Ctrl Pts',(0.881650403784469,1.52706329386832,
0.973958333333351));
#420511=CARTESIAN_POINT('Ctrl Pts',(0.,1.52706329386832,1.01562500000002));
#420512=CARTESIAN_POINT('Ctrl Pts',(-0.881650403784468,1.52706329386832,
1.05729166666669));
#420513=CARTESIAN_POINT('Ctrl Pts',(-1.3224756056767,0.76353164693416,1.09895833333335));
#420514=CARTESIAN_POINT('Ctrl Pts',(-1.76330080756894,2.64858386892187E-15,
1.14062500000002));
#420515=CARTESIAN_POINT('Ctrl Pts',(-1.3224756056767,-0.763531646934155,
1.18229166666669));
#420516=CARTESIAN_POINT('Ctrl Pts',(-0.881650403784469,-1.52706329386831,
1.22395833333335));
#420517=CARTESIAN_POINT('Ctrl Pts',(-1.87011317493125E-16,-1.52706329386831,
1.26562500000002));
#420518=CARTESIAN_POINT('Ctrl Pts',(0.881650403784467,-1.52706329386831,
1.30729166666669));
#420519=CARTESIAN_POINT('Ctrl Pts',(1.3224756056767,-0.763531646934156,
1.34895833333335));
#420520=CARTESIAN_POINT('Ctrl Pts',(1.76330080756894,2.21669973093722E-15,
1.39062500000002));
#420521=CARTESIAN_POINT('Ctrl Pts',(1.3224756056767,0.763531646934159,1.43229166666668));
#420522=CARTESIAN_POINT('Ctrl Pts',(0.881650403784469,1.52706329386832,
1.47395833333335));
#420523=CARTESIAN_POINT('Ctrl Pts',(0.,1.52706329386832,1.51562500000002));
#420524=CARTESIAN_POINT('Ctrl Pts',(-0.881650403784468,1.52706329386832,
1.55729166666668));
#420525=CARTESIAN_POINT('Ctrl Pts',(-1.3224756056767,0.76353164693416,1.59895833333335));
#420526=CARTESIAN_POINT('Ctrl Pts',(-1.76330080756894,2.64858386892187E-15,
1.64062500000002));
#420527=CARTESIAN_POINT('Ctrl Pts',(-1.3224756056767,-0.763531646934155,
1.68229166666668));
#420528=CARTESIAN_POINT('Ctrl Pts',(-0.881650403784469,-1.52706329386831,
1.72395833333335));
#420529=CARTESIAN_POINT('Ctrl Pts',(-1.87011317493125E-16,-1.52706329386831,
1.76562500000002));
#420530=CARTESIAN_POINT('Ctrl Pts',(0.881650403784467,-1.52706329386831,
1.80729166666668));
#420531=CARTESIAN_POINT('Ctrl Pts',(1.3224756056767,-0.763531646934156,
1.84895833333335));
#420532=CARTESIAN_POINT('Ctrl Pts',(1.76330080756894,2.21669973093722E-15,
1.89062500000002));
#420533=CARTESIAN_POINT('Ctrl Pts',(1.3224756056767,0.763531646934159,1.93229166666668));
#420534=CARTESIAN_POINT('Ctrl Pts',(0.881650403784469,1.52706329386832,
1.97395833333335));
#420535=CARTESIAN_POINT('Ctrl Pts',(0.,1.52706329386832,2.01562500000002));
#420536=CARTESIAN_POINT('Ctrl Pts',(-0.881650403784468,1.52706329386832,
2.05729166666668));
#420537=CARTESIAN_POINT('Ctrl Pts',(-1.3224756056767,0.76353164693416,2.09895833333335));
#420538=CARTESIAN_POINT('Ctrl Pts',(-1.76330080756894,2.64858386892187E-15,
2.14062500000002));
#420539=CARTESIAN_POINT('Ctrl Pts',(-1.3224756056767,-0.763531646934155,
2.18229166666668));
#420540=CARTESIAN_POINT('Ctrl Pts',(-0.881650403784469,-1.52706329386831,
2.22395833333335));
#420541=CARTESIAN_POINT('Ctrl Pts',(-1.87011317493125E-16,-1.52706329386831,
2.26562500000002));
#420542=CARTESIAN_POINT('Ctrl Pts',(0.881650403784467,-1.52706329386831,
2.30729166666669));
#420543=CARTESIAN_POINT('Ctrl Pts',(1.3224756056767,-0.763531646934156,
2.34895833333335));
#420544=CARTESIAN_POINT('Ctrl Pts',(1.76330080756894,2.21669973093722E-15,
2.39062500000002));
#420545=CARTESIAN_POINT('Ctrl Pts',(1.3224756056767,0.763531646934159,2.43229166666669));
#420546=CARTESIAN_POINT('Ctrl Pts',(0.881650403784469,1.52706329386832,
2.47395833333335));
#420547=CARTESIAN_POINT('Ctrl Pts',(0.,1.52706329386832,2.51562500000002));
#420548=CARTESIAN_POINT('Ctrl Pts',(-0.881650403784468,1.52706329386832,
2.55729166666669));
#420549=CARTESIAN_POINT('Ctrl Pts',(-1.3224756056767,0.76353164693416,2.59895833333335));
#420550=CARTESIAN_POINT('Ctrl Pts',(-1.76330080756894,2.64858386892187E-15,
2.64062500000002));
#420551=CARTESIAN_POINT('Ctrl Pts',(-1.3224756056767,-0.763531646934155,
2.68229166666669));
#420552=CARTESIAN_POINT('Ctrl Pts',(-0.881650403784469,-1.52706329386831,
2.72395833333335));
#420553=CARTESIAN_POINT('Ctrl Pts',(-1.87011317493125E-16,-1.52706329386831,
2.76562500000002));
#420554=CARTESIAN_POINT('Ctrl Pts',(0.881650403784467,-1.52706329386831,
2.80729166666669));
#420555=CARTESIAN_POINT('Ctrl Pts',(1.3224756056767,-0.763531646934156,
2.84895833333335));
#420556=CARTESIAN_POINT('Ctrl Pts',(1.76330080756894,2.21669973093722E-15,
2.89062500000002));
#420557=CARTESIAN_POINT('Ctrl Pts',(1.3224756056767,0.763531646934159,2.93229166666669));
#420558=CARTESIAN_POINT('Ctrl Pts',(0.881650403784469,1.52706329386832,
2.97395833333335));
#420559=CARTESIAN_POINT('Ctrl Pts',(0.,1.52706329386832,3.01562500000002));
#420560=CARTESIAN_POINT('Ctrl Pts',(-0.881650403784468,1.52706329386832,
3.05729166666669));
#420561=CARTESIAN_POINT('Ctrl Pts',(-1.3224756056767,0.76353164693416,3.09895833333335));
#420562=CARTESIAN_POINT('Ctrl Pts',(-1.76330080756894,2.64858386892187E-15,
3.14062500000002));
#420563=CARTESIAN_POINT('Ctrl Pts',(-1.3224756056767,-0.763531646934155,
3.18229166666669));
#420564=CARTESIAN_POINT('Ctrl Pts',(-0.881650403784469,-1.52706329386831,
3.22395833333335));
#420565=CARTESIAN_POINT('Ctrl Pts',(-1.87011317493125E-16,-1.52706329386831,
3.26562500000002));
#420566=CARTESIAN_POINT('Ctrl Pts',(0.881650403784467,-1.52706329386831,
3.30729166666669));
#420567=CARTESIAN_POINT('Ctrl Pts',(1.3224756056767,-0.763531646934156,
3.34895833333335));
#420568=CARTESIAN_POINT('Ctrl Pts',(1.76330080756894,2.21669973093722E-15,
3.39062500000002));
#420569=CARTESIAN_POINT('Ctrl Pts',(1.3224756056767,0.763531646934159,3.43229166666669));
#420570=CARTESIAN_POINT('Ctrl Pts',(0.881650403784469,1.52706329386832,
3.47395833333335));
#420571=CARTESIAN_POINT('Ctrl Pts',(0.,1.52706329386832,3.51562500000002));
#420572=CARTESIAN_POINT('Ctrl Pts',(-0.881650403784468,1.52706329386832,
3.55729166666669));
#420573=CARTESIAN_POINT('Ctrl Pts',(-1.3224756056767,0.76353164693416,3.59895833333335));
#420574=CARTESIAN_POINT('Ctrl Pts',(-1.76330080756894,2.64858386892187E-15,
3.64062500000002));
#420575=CARTESIAN_POINT('Ctrl Pts',(-1.3224756056767,-0.763531646934155,
3.68229166666669));
#420576=CARTESIAN_POINT('Ctrl Pts',(-0.881650403784469,-1.52706329386831,
3.72395833333335));
#420577=CARTESIAN_POINT('Ctrl Pts',(-1.87011317493125E-16,-1.52706329386831,
3.76562500000002));
#420578=CARTESIAN_POINT('Ctrl Pts',(0.881650403784467,-1.52706329386831,
3.80729166666669));
#420579=CARTESIAN_POINT('Ctrl Pts',(1.3224756056767,-0.763531646934156,
3.84895833333335));
#420580=CARTESIAN_POINT('Ctrl Pts',(1.76330080756894,2.21669973093722E-15,
3.89062500000002));
#420581=CARTESIAN_POINT('Ctrl Pts',(1.3224756056767,0.763531646934159,3.93229166666669));
#420582=CARTESIAN_POINT('Ctrl Pts',(0.881650403784469,1.52706329386832,
3.97395833333335));
#420583=CARTESIAN_POINT('Ctrl Pts',(0.,1.52706329386832,4.01562500000002));
#420584=CARTESIAN_POINT('Ctrl Pts',(-0.881650403784468,1.52706329386832,
4.05729166666669));
#420585=CARTESIAN_POINT('Ctrl Pts',(-1.3224756056767,0.76353164693416,4.09895833333335));
#420586=CARTESIAN_POINT('Ctrl Pts',(-1.76330080756894,2.64858386892187E-15,
4.14062500000002));
#420587=CARTESIAN_POINT('Ctrl Pts',(-1.3224756056767,-0.763531646934155,
4.18229166666669));
#420588=CARTESIAN_POINT('Ctrl Pts',(-0.881650403784469,-1.52706329386831,
4.22395833333335));
#420589=CARTESIAN_POINT('Ctrl Pts',(-1.87011317493125E-16,-1.52706329386831,
4.26562500000002));
#420590=CARTESIAN_POINT('Ctrl Pts',(0.881650403784467,-1.52706329386831,
4.30729166666668));
#420591=CARTESIAN_POINT('Ctrl Pts',(1.3224756056767,-0.763531646934156,
4.34895833333335));
#420592=CARTESIAN_POINT('Ctrl Pts',(1.76330080756894,2.21669973093722E-15,
4.39062500000002));
#420593=CARTESIAN_POINT('Ctrl Pts',(1.3224756056767,0.763531646934159,4.43229166666668));
#420594=CARTESIAN_POINT('Ctrl Pts',(0.881650403784469,1.52706329386832,
4.47395833333335));
#420595=CARTESIAN_POINT('Ctrl Pts',(0.,1.52706329386832,4.51562500000002));
#420596=CARTESIAN_POINT('Ctrl Pts',(-0.881650403784468,1.52706329386832,
4.55729166666668));
#420597=CARTESIAN_POINT('Ctrl Pts',(-1.3224756056767,0.76353164693416,4.59895833333335));
#420598=CARTESIAN_POINT('Ctrl Pts',(-1.76330080756894,2.64858386892187E-15,
4.64062500000002));
#420599=CARTESIAN_POINT('Ctrl Pts',(-1.3224756056767,-0.763531646934155,
4.68229166666668));
#420600=CARTESIAN_POINT('Ctrl Pts',(-0.881650403784469,-1.52706329386831,
4.72395833333335));
#420601=CARTESIAN_POINT('Ctrl Pts',(-1.87011317493125E-16,-1.52706329386831,
4.76562500000002));
#420602=CARTESIAN_POINT('Ctrl Pts',(0.881650403784467,-1.52706329386831,
4.80729166666668));
#420603=CARTESIAN_POINT('Ctrl Pts',(1.3224756056767,-0.763531646934156,
4.84895833333335));
#420604=CARTESIAN_POINT('Ctrl Pts',(1.76330080756894,2.21669973093722E-15,
4.89062500000002));
#420605=CARTESIAN_POINT('Ctrl Pts',(1.3224756056767,0.763531646934159,4.93229166666668));
#420606=CARTESIAN_POINT('Ctrl Pts',(0.881650403784469,1.52706329386832,
4.97395833333335));
#420607=CARTESIAN_POINT('Ctrl Pts',(0.,1.52706329386832,5.01562500000002));
#420608=CARTESIAN_POINT('Ctrl Pts',(-0.881650403784468,1.52706329386832,
5.05729166666668));
#420609=CARTESIAN_POINT('Ctrl Pts',(-1.3224756056767,0.76353164693416,5.09895833333335));
#420610=CARTESIAN_POINT('Ctrl Pts',(-1.76330080756894,2.64858386892187E-15,
5.14062500000002));
#420611=CARTESIAN_POINT('Ctrl Pts',(-1.3224756056767,-0.763531646934155,
5.18229166666668));
#420612=CARTESIAN_POINT('Ctrl Pts',(-0.881650403784469,-1.52706329386831,
5.22395833333335));
#420613=CARTESIAN_POINT('Ctrl Pts',(-1.87011317493125E-16,-1.52706329386831,
5.26562500000002));
#420614=CARTESIAN_POINT('Ctrl Pts',(0.881650403784467,-1.52706329386831,
5.30729166666668));
#420615=CARTESIAN_POINT('Ctrl Pts',(1.3224756056767,-0.763531646934156,
5.34895833333335));
#420616=CARTESIAN_POINT('Ctrl Pts',(1.76330080756894,2.21669973093722E-15,
5.39062500000002));
#420617=CARTESIAN_POINT('Ctrl Pts',(1.3224756056767,0.763531646934159,5.43229166666668));
#420618=CARTESIAN_POINT('Ctrl Pts',(0.881650403784469,1.52706329386832,
5.47395833333335));
#420619=CARTESIAN_POINT('Ctrl Pts',(0.,1.52706329386832,5.51562500000002));
#420620=CARTESIAN_POINT('Ctrl Pts',(-0.881650403784468,1.52706329386832,
5.55729166666668));
#420621=CARTESIAN_POINT('Ctrl Pts',(-1.3224756056767,0.76353164693416,5.59895833333335));
#420622=CARTESIAN_POINT('Ctrl Pts',(-1.76330080756894,2.64858386892187E-15,
5.64062500000002));
#420623=CARTESIAN_POINT('Ctrl Pts',(-1.3224756056767,-0.763531646934155,
5.68229166666668));
#420624=CARTESIAN_POINT('Ctrl Pts',(-0.881650403784469,-1.52706329386831,
5.72395833333335));
#420625=CARTESIAN_POINT('Ctrl Pts',(-1.87011317493125E-16,-1.52706329386831,
5.76562500000002));
#420626=CARTESIAN_POINT('Ctrl Pts',(0.881650403784467,-1.52706329386831,
5.80729166666669));
#420627=CARTESIAN_POINT('Ctrl Pts',(1.3224756056767,-0.763531646934156,
5.84895833333335));
#420628=CARTESIAN_POINT('Ctrl Pts',(1.76330080756894,2.21669973093722E-15,
5.89062500000002));
#420629=CARTESIAN_POINT('Ctrl Pts',(1.3224756056767,0.763531646934159,5.93229166666668));
#420630=CARTESIAN_POINT('Ctrl Pts',(0.881650403784469,1.52706329386832,
5.97395833333335));
#420631=CARTESIAN_POINT('Ctrl Pts',(0.,1.52706329386832,6.01562500000002));
#420632=CARTESIAN_POINT('Ctrl Pts',(-0.881650403784468,1.52706329386832,
6.05729166666669));
#420633=CARTESIAN_POINT('Ctrl Pts',(-1.3224756056767,0.76353164693416,6.09895833333335));
#420634=CARTESIAN_POINT('Ctrl Pts',(-1.76330080756894,2.64858386892187E-15,
6.14062500000002));
#420635=CARTESIAN_POINT('Ctrl Pts',(-1.3224756056767,-0.763531646934155,
6.18229166666668));
#420636=CARTESIAN_POINT('Ctrl Pts',(-0.881650403784469,-1.52706329386831,
6.22395833333335));
#420637=CARTESIAN_POINT('Ctrl Pts',(-1.87011317493125E-16,-1.52706329386831,
6.26562500000002));
#420638=CARTESIAN_POINT('Ctrl Pts',(0.881650403784467,-1.52706329386831,
6.30729166666669));
#420639=CARTESIAN_POINT('Ctrl Pts',(1.3224756056767,-0.763531646934156,
6.34895833333335));
#420640=CARTESIAN_POINT('Ctrl Pts',(1.76330080756894,2.21669973093722E-15,
6.39062500000002));
#420641=CARTESIAN_POINT('Ctrl Pts',(1.3224756056767,0.763531646934159,6.43229166666669));
#420642=CARTESIAN_POINT('Ctrl Pts',(0.881650403784469,1.52706329386832,
6.47395833333335));
#420643=CARTESIAN_POINT('Ctrl Pts',(0.,1.52706329386832,6.51562500000002));
#420644=CARTESIAN_POINT('Ctrl Pts',(-0.881650403784468,1.52706329386832,
6.55729166666668));
#420645=CARTESIAN_POINT('Ctrl Pts',(-1.3224756056767,0.76353164693416,6.59895833333335));
#420646=CARTESIAN_POINT('Ctrl Pts',(-1.76330080756894,2.64858386892187E-15,
6.64062500000002));
#420647=CARTESIAN_POINT('Ctrl Pts',(-1.3224756056767,-0.763531646934155,
6.68229166666669));
#420648=CARTESIAN_POINT('Ctrl Pts',(-0.881650403784469,-1.52706329386831,
6.72395833333335));
#420649=CARTESIAN_POINT('Ctrl Pts',(-1.87011317493125E-16,-1.52706329386831,
6.76562500000002));
#420650=CARTESIAN_POINT('Ctrl Pts',(0.881650403784467,-1.52706329386831,
6.80729166666669));
#420651=CARTESIAN_POINT('Ctrl Pts',(1.3224756056767,-0.763531646934156,
6.84895833333335));
#420652=CARTESIAN_POINT('Ctrl Pts',(1.76330080756894,2.21669973093722E-15,
6.89062500000002));
#420653=CARTESIAN_POINT('Ctrl Pts',(1.3224756056767,0.763531646934159,6.93229166666669));
#420654=CARTESIAN_POINT('Ctrl Pts',(0.881650403784469,1.52706329386832,
6.97395833333335));
#420655=CARTESIAN_POINT('Ctrl Pts',(0.,1.52706329386832,7.01562500000002));
#420656=CARTESIAN_POINT('Ctrl Pts',(-0.881650403784468,1.52706329386832,
7.05729166666669));
#420657=CARTESIAN_POINT('Ctrl Pts',(-1.3224756056767,0.76353164693416,7.09895833333335));
#420658=CARTESIAN_POINT('Ctrl Pts',(-1.76330080756894,2.64858386892187E-15,
7.14062500000002));
#420659=CARTESIAN_POINT('Ctrl Pts',(-1.3224756056767,-0.763531646934155,
7.18229166666669));
#420660=CARTESIAN_POINT('Ctrl Pts',(-0.881650403784469,-1.52706329386831,
7.22395833333335));
#420661=CARTESIAN_POINT('Ctrl Pts',(-1.87011317493125E-16,-1.52706329386831,
7.26562500000002));
#420662=CARTESIAN_POINT('Ctrl Pts',(0.881650403784467,-1.52706329386831,
7.30729166666669));
#420663=CARTESIAN_POINT('Ctrl Pts',(1.3224756056767,-0.763531646934156,
7.34895833333335));
#420664=CARTESIAN_POINT('Ctrl Pts',(1.76330080756894,2.21669973093722E-15,
7.39062500000002));
#420665=CARTESIAN_POINT('Ctrl Pts',(1.3224756056767,0.763531646934159,7.43229166666669));
#420666=CARTESIAN_POINT('Ctrl Pts',(0.881650403784469,1.52706329386832,
7.47395833333335));
#420667=CARTESIAN_POINT('Ctrl Pts',(0.,1.52706329386832,7.51562500000002));
#420668=CARTESIAN_POINT('Ctrl Pts',(-0.881650403784468,1.52706329386832,
7.55729166666669));
#420669=CARTESIAN_POINT('Ctrl Pts',(-1.3224756056767,0.76353164693416,7.59895833333335));
#420670=CARTESIAN_POINT('Ctrl Pts',(-1.76330080756894,2.64858386892187E-15,
7.64062500000002));
#420671=CARTESIAN_POINT('Ctrl Pts',(-1.3224756056767,-0.763531646934155,
7.68229166666669));
#420672=CARTESIAN_POINT('Ctrl Pts',(-0.881650403784469,-1.52706329386831,
7.72395833333335));
#420673=CARTESIAN_POINT('Ctrl Pts',(-1.87011317493125E-16,-1.52706329386831,
7.76562500000002));
#420674=CARTESIAN_POINT('Ctrl Pts',(0.881650403784467,-1.52706329386831,
7.80729166666669));
#420675=CARTESIAN_POINT('Ctrl Pts',(1.3224756056767,-0.763531646934156,
7.84895833333335));
#420676=CARTESIAN_POINT('Ctrl Pts',(1.76330080756894,2.21669973093722E-15,
7.89062500000002));
#420677=CARTESIAN_POINT('Ctrl Pts',(1.3224756056767,0.763531646934159,7.93229166666669));
#420678=CARTESIAN_POINT('Ctrl Pts',(0.881650403784469,1.52706329386832,
7.97395833333335));
#420679=CARTESIAN_POINT('Ctrl Pts',(0.,1.52706329386832,8.01562500000002));
#420680=CARTESIAN_POINT('Ctrl Pts',(-0.881650403784468,1.52706329386832,
8.05729166666668));
#420681=CARTESIAN_POINT('Ctrl Pts',(-1.3224756056767,0.76353164693416,8.09895833333335));
#420682=CARTESIAN_POINT('Ctrl Pts',(-1.76330080756894,2.64858386892187E-15,
8.14062500000002));
#420683=CARTESIAN_POINT('Ctrl Pts',(-1.3224756056767,-0.763531646934155,
8.18229166666668));
#420684=CARTESIAN_POINT('Ctrl Pts',(-0.881650403784469,-1.52706329386831,
8.22395833333335));
#420685=CARTESIAN_POINT('Ctrl Pts',(-1.87011317493125E-16,-1.52706329386831,
8.26562500000002));
#420686=CARTESIAN_POINT('Ctrl Pts',(0.881650403784467,-1.52706329386831,
8.30729166666668));
#420687=CARTESIAN_POINT('Ctrl Pts',(1.3224756056767,-0.763531646934156,
8.34895833333335));
#420688=CARTESIAN_POINT('Ctrl Pts',(1.76330080756894,2.21669973093722E-15,
8.39062500000002));
#420689=CARTESIAN_POINT('Ctrl Pts',(1.3224756056767,0.763531646934159,8.43229166666669));
#420690=CARTESIAN_POINT('Ctrl Pts',(0.881650403784469,1.52706329386832,
8.47395833333335));
#420691=CARTESIAN_POINT('Ctrl Pts',(0.,1.52706329386832,8.51562500000002));
#420692=CARTESIAN_POINT('Ctrl Pts',(-0.881650403784468,1.52706329386832,
8.55729166666669));
#420693=CARTESIAN_POINT('Ctrl Pts',(-1.3224756056767,0.76353164693416,8.59895833333335));
#420694=CARTESIAN_POINT('Ctrl Pts',(-1.76330080756894,2.64858386892187E-15,
8.64062500000002));
#420695=CARTESIAN_POINT('Ctrl Pts',(-1.3224756056767,-0.763531646934155,
8.68229166666668));
#420696=CARTESIAN_POINT('Ctrl Pts',(-0.881650403784469,-1.52706329386831,
8.72395833333335));
#420697=CARTESIAN_POINT('Ctrl Pts',(-1.87011317493125E-16,-1.52706329386831,
8.76562500000002));
#420698=CARTESIAN_POINT('Ctrl Pts',(0.881650403784467,-1.52706329386831,
8.80729166666668));
#420699=CARTESIAN_POINT('Ctrl Pts',(1.3224756056767,-0.763531646934156,
8.84895833333335));
#420700=CARTESIAN_POINT('Ctrl Pts',(1.76330080756894,2.21669973093722E-15,
8.89062500000002));
#420701=CARTESIAN_POINT('Ctrl Pts',(1.3224756056767,0.763531646934159,8.93229166666668));
#420702=CARTESIAN_POINT('Ctrl Pts',(0.881650403784469,1.52706329386832,
8.97395833333335));
#420703=CARTESIAN_POINT('Ctrl Pts',(0.,1.52706329386832,9.01562500000002));
#420704=CARTESIAN_POINT('Ctrl Pts',(-0.881650403784468,1.52706329386832,
9.05729166666669));
#420705=CARTESIAN_POINT('Ctrl Pts',(-1.3224756056767,0.76353164693416,9.09895833333335));
#420706=CARTESIAN_POINT('Ctrl Pts',(-1.76330080756894,2.64858386892187E-15,
9.14062500000002));
#420707=CARTESIAN_POINT('Ctrl Pts',(-1.3224756056767,-0.763531646934155,
9.18229166666668));
#420708=CARTESIAN_POINT('Ctrl Pts',(-0.881650403784469,-1.52706329386831,
9.22395833333335));
#420709=CARTESIAN_POINT('Ctrl Pts',(-1.87011317493125E-16,-1.52706329386831,
9.26562500000002));
#420710=CARTESIAN_POINT('Ctrl Pts',(0.881650403784467,-1.52706329386831,
9.30729166666669));
#420711=CARTESIAN_POINT('Ctrl Pts',(1.3224756056767,-0.763531646934156,
9.34895833333335));
#420712=CARTESIAN_POINT('Ctrl Pts',(1.76330080756894,2.21669973093722E-15,
9.39062500000002));
#420713=CARTESIAN_POINT('Ctrl Pts',(1.3224756056767,0.763531646934159,9.43229166666668));
#420714=CARTESIAN_POINT('Ctrl Pts',(0.881650403784469,1.52706329386832,
9.47395833333335));
#420715=CARTESIAN_POINT('Ctrl Pts',(0.,1.52706329386832,9.51562500000002));
#420716=CARTESIAN_POINT('Ctrl Pts',(-0.881650403784468,1.52706329386832,
9.55729166666669));
#420717=CARTESIAN_POINT('Ctrl Pts',(-1.3224756056767,0.76353164693416,9.59895833333335));
#420718=CARTESIAN_POINT('Ctrl Pts',(-1.76330080756894,2.64858386892187E-15,
9.64062500000002));
#420719=CARTESIAN_POINT('Ctrl Pts',(-1.3224756056767,-0.763531646934155,
9.68229166666669));
#420720=CARTESIAN_POINT('Ctrl Pts',(-0.881650403784469,-1.52706329386831,
9.72395833333335));
#420721=CARTESIAN_POINT('Ctrl Pts',(-1.87011317493125E-16,-1.52706329386831,
9.76562500000002));
#420722=CARTESIAN_POINT('Ctrl Pts',(0.881650403784467,-1.52706329386831,
9.80729166666668));
#420723=CARTESIAN_POINT('Ctrl Pts',(1.3224756056767,-0.763531646934156,
9.84895833333335));
#420724=CARTESIAN_POINT('Ctrl Pts',(1.76330080756894,2.21669973093722E-15,
9.89062500000002));
#420725=CARTESIAN_POINT('Ctrl Pts',(1.3224756056767,0.763531646934159,9.93229166666669));
#420726=CARTESIAN_POINT('Ctrl Pts',(0.881650403784469,1.52706329386832,
9.97395833333335));
#420727=CARTESIAN_POINT('Ctrl Pts',(0.,1.52706329386832,10.015625));
#420728=CARTESIAN_POINT('Ctrl Pts',(-0.881650403784468,1.52706329386832,
10.0572916666667));
#420729=CARTESIAN_POINT('Ctrl Pts',(-1.3224756056767,0.76353164693416,10.0989583333333));
#420730=CARTESIAN_POINT('Ctrl Pts',(-1.76330080756894,2.64858386892187E-15,
10.140625));
#420731=CARTESIAN_POINT('Ctrl Pts',(-1.3224756056767,-0.763531646934155,
10.1822916666667));
#420732=CARTESIAN_POINT('Ctrl Pts',(-0.881650403784469,-1.52706329386831,
10.2239583333333));
#420733=CARTESIAN_POINT('Ctrl Pts',(-1.87011317493125E-16,-1.52706329386831,
10.265625));
#420734=CARTESIAN_POINT('Ctrl Pts',(0.881650403784467,-1.52706329386831,
10.3072916666667));
#420735=CARTESIAN_POINT('Ctrl Pts',(1.3224756056767,-0.763531646934156,
10.3489583333334));
#420736=CARTESIAN_POINT('Ctrl Pts',(1.76330080756894,2.21669973093722E-15,
10.390625));
#420737=CARTESIAN_POINT('Ctrl Pts',(1.3224756056767,0.763531646934159,10.4322916666667));
#420738=CARTESIAN_POINT('Ctrl Pts',(0.881650403784469,1.52706329386832,
10.4739583333334));
#420739=CARTESIAN_POINT('Ctrl Pts',(0.,1.52706329386832,10.515625));
#420740=CARTESIAN_POINT('Ctrl Pts',(-0.881650403784468,1.52706329386832,
10.5572916666667));
#420741=CARTESIAN_POINT('Ctrl Pts',(-1.3224756056767,0.76353164693416,10.5989583333334));
#420742=CARTESIAN_POINT('Ctrl Pts',(-1.76330080756894,2.64858386892187E-15,
10.640625));
#420743=CARTESIAN_POINT('Ctrl Pts',(-1.3224756056767,-0.763531646934155,
10.6822916666667));
#420744=CARTESIAN_POINT('Ctrl Pts',(-0.881650403784469,-1.52706329386831,
10.7239583333333));
#420745=CARTESIAN_POINT('Ctrl Pts',(-1.87011317493125E-16,-1.52706329386831,
10.765625));
#420746=CARTESIAN_POINT('Ctrl Pts',(0.881650403784467,-1.52706329386831,
10.8072916666667));
#420747=CARTESIAN_POINT('Ctrl Pts',(1.3224756056767,-0.763531646934156,
10.8489583333334));
#420748=CARTESIAN_POINT('Ctrl Pts',(1.76330080756894,2.21669973093722E-15,
10.890625));
#420749=CARTESIAN_POINT('Ctrl Pts',(1.3224756056767,0.763531646934159,10.9322916666667));
#420750=CARTESIAN_POINT('Ctrl Pts',(0.881650403784469,1.52706329386832,
10.9739583333334));
#420751=CARTESIAN_POINT('Ctrl Pts',(0.,1.52706329386832,11.015625));
#420752=CARTESIAN_POINT('Ctrl Pts',(-0.881650403784468,1.52706329386832,
11.0572916666667));
#420753=CARTESIAN_POINT('Ctrl Pts',(-1.3224756056767,0.76353164693416,11.0989583333334));
#420754=CARTESIAN_POINT('Ctrl Pts',(-1.76330080756894,2.64858386892187E-15,
11.140625));
#420755=CARTESIAN_POINT('Ctrl Pts',(-1.3224756056767,-0.763531646934155,
11.1822916666667));
#420756=CARTESIAN_POINT('Ctrl Pts',(-0.881650403784469,-1.52706329386831,
11.2239583333334));
#420757=CARTESIAN_POINT('Ctrl Pts',(-1.87011317493125E-16,-1.52706329386831,
11.265625));
#420758=CARTESIAN_POINT('Ctrl Pts',(0.881650403784467,-1.52706329386831,
11.3072916666667));
#420759=CARTESIAN_POINT('Ctrl Pts',(1.3224756056767,-0.763531646934156,
11.3489583333334));
#420760=CARTESIAN_POINT('Ctrl Pts',(1.76330080756894,2.21669973093722E-15,
11.390625));
#420761=CARTESIAN_POINT('Ctrl Pts',(1.3224756056767,0.763531646934159,11.4322916666667));
#420762=CARTESIAN_POINT('Ctrl Pts',(0.881650403784469,1.52706329386832,
11.4739583333334));
#420763=CARTESIAN_POINT('Ctrl Pts',(0.,1.52706329386832,11.515625));
#420764=CARTESIAN_POINT('Ctrl Pts',(0.,1.17523522336992,-14.1875030312107));
#420765=CARTESIAN_POINT('Ctrl Pts',(-0.678522372573754,1.17523522336992,
-14.145836364544));
#420766=CARTESIAN_POINT('Ctrl Pts',(-1.01778355886063,0.587617611684963,
-14.1041696978774));
#420767=CARTESIAN_POINT('Ctrl Pts',(-1.35704474514751,2.62370785959794E-15,
-14.0625030312107));
#420768=CARTESIAN_POINT('Ctrl Pts',(-1.01778355886063,-0.587617611684958,
-14.020836364544));
#420769=CARTESIAN_POINT('Ctrl Pts',(-0.678522372573755,-1.17523522336992,
-13.9791696978774));
#420770=CARTESIAN_POINT('Ctrl Pts',(-1.4392480545452E-16,-1.17523522336992,
-13.9375030312107));
#420771=CARTESIAN_POINT('Ctrl Pts',(0.678522372573754,-1.17523522336992,
-13.895836364544));
#420772=CARTESIAN_POINT('Ctrl Pts',(1.01778355886063,-0.587617611684959,
-13.8541696978774));
#420773=CARTESIAN_POINT('Ctrl Pts',(1.35704474514751,2.29132775890901E-15,
-13.8125030312107));
#420774=CARTESIAN_POINT('Ctrl Pts',(1.01778355886063,0.587617611684963,
-13.770836364544));
#420775=CARTESIAN_POINT('Ctrl Pts',(0.678522372573755,1.17523522336992,
-13.7291696978774));
#420776=CARTESIAN_POINT('Ctrl Pts',(0.,1.17523522336992,-13.6875030312107));
#420777=CARTESIAN_POINT('Ctrl Pts',(-0.678522372573754,1.17523522336992,
-13.645836364544));
#420778=CARTESIAN_POINT('Ctrl Pts',(-1.01778355886063,0.587617611684963,
-13.6041696978774));
#420779=CARTESIAN_POINT('Ctrl Pts',(-1.35704474514751,2.62370785959794E-15,
-13.5625030312107));
#420780=CARTESIAN_POINT('Ctrl Pts',(-1.01778355886063,-0.587617611684958,
-13.520836364544));
#420781=CARTESIAN_POINT('Ctrl Pts',(-0.678522372573755,-1.17523522336992,
-13.4791696978774));
#420782=CARTESIAN_POINT('Ctrl Pts',(-1.4392480545452E-16,-1.17523522336992,
-13.4375030312107));
#420783=CARTESIAN_POINT('Ctrl Pts',(0.678522372573754,-1.17523522336992,
-13.395836364544));
#420784=CARTESIAN_POINT('Ctrl Pts',(1.01778355886063,-0.587617611684959,
-13.3541696978774));
#420785=CARTESIAN_POINT('Ctrl Pts',(1.35704474514751,2.29132775890901E-15,
-13.3125030312107));
#420786=CARTESIAN_POINT('Ctrl Pts',(1.01778355886063,0.587617611684963,
-13.270836364544));
#420787=CARTESIAN_POINT('Ctrl Pts',(0.678522372573755,1.17523522336992,
-13.2291696978774));
#420788=CARTESIAN_POINT('Ctrl Pts',(0.,1.17523522336992,-13.1875030312107));
#420789=CARTESIAN_POINT('Ctrl Pts',(-0.678522372573754,1.17523522336992,
-13.145836364544));
#420790=CARTESIAN_POINT('Ctrl Pts',(-1.01778355886063,0.587617611684963,
-13.1041696978774));
#420791=CARTESIAN_POINT('Ctrl Pts',(-1.35704474514751,2.62370785959794E-15,
-13.0625030312107));
#420792=CARTESIAN_POINT('Ctrl Pts',(-1.01778355886063,-0.587617611684958,
-13.020836364544));
#420793=CARTESIAN_POINT('Ctrl Pts',(-0.678522372573755,-1.17523522336992,
-12.9791696978774));
#420794=CARTESIAN_POINT('Ctrl Pts',(-1.4392480545452E-16,-1.17523522336992,
-12.9375030312107));
#420795=CARTESIAN_POINT('Ctrl Pts',(0.678522372573754,-1.17523522336992,
-12.895836364544));
#420796=CARTESIAN_POINT('Ctrl Pts',(1.01778355886063,-0.587617611684959,
-12.8541696978774));
#420797=CARTESIAN_POINT('Ctrl Pts',(1.35704474514751,2.29132775890901E-15,
-12.8125030312107));
#420798=CARTESIAN_POINT('Ctrl Pts',(1.01778355886063,0.587617611684963,
-12.770836364544));
#420799=CARTESIAN_POINT('Ctrl Pts',(0.678522372573755,1.17523522336992,
-12.7291696978774));
#420800=CARTESIAN_POINT('Ctrl Pts',(0.,1.17523522336992,-12.6875030312107));
#420801=CARTESIAN_POINT('Ctrl Pts',(-0.678522372573754,1.17523522336992,
-12.645836364544));
#420802=CARTESIAN_POINT('Ctrl Pts',(-1.01778355886063,0.587617611684963,
-12.6041696978774));
#420803=CARTESIAN_POINT('Ctrl Pts',(-1.35704474514751,2.62370785959794E-15,
-12.5625030312107));
#420804=CARTESIAN_POINT('Ctrl Pts',(-1.01778355886063,-0.587617611684958,
-12.520836364544));
#420805=CARTESIAN_POINT('Ctrl Pts',(-0.678522372573755,-1.17523522336992,
-12.4791696978774));
#420806=CARTESIAN_POINT('Ctrl Pts',(-1.4392480545452E-16,-1.17523522336992,
-12.4375030312107));
#420807=CARTESIAN_POINT('Ctrl Pts',(0.678522372573754,-1.17523522336992,
-12.395836364544));
#420808=CARTESIAN_POINT('Ctrl Pts',(1.01778355886063,-0.587617611684959,
-12.3541696978774));
#420809=CARTESIAN_POINT('Ctrl Pts',(1.35704474514751,2.29132775890901E-15,
-12.3125030312107));
#420810=CARTESIAN_POINT('Ctrl Pts',(1.01778355886063,0.587617611684963,
-12.270836364544));
#420811=CARTESIAN_POINT('Ctrl Pts',(0.678522372573755,1.17523522336992,
-12.2291696978774));
#420812=CARTESIAN_POINT('Ctrl Pts',(0.,1.17523522336992,-12.1875030312107));
#420813=CARTESIAN_POINT('Ctrl Pts',(-0.678522372573754,1.17523522336992,
-12.145836364544));
#420814=CARTESIAN_POINT('Ctrl Pts',(-1.01778355886063,0.587617611684963,
-12.1041696978774));
#420815=CARTESIAN_POINT('Ctrl Pts',(-1.35704474514751,2.62370785959794E-15,
-12.0625030312107));
#420816=CARTESIAN_POINT('Ctrl Pts',(-1.01778355886063,-0.587617611684958,
-12.020836364544));
#420817=CARTESIAN_POINT('Ctrl Pts',(-0.678522372573755,-1.17523522336992,
-11.9791696978774));
#420818=CARTESIAN_POINT('Ctrl Pts',(-1.4392480545452E-16,-1.17523522336992,
-11.9375030312107));
#420819=CARTESIAN_POINT('Ctrl Pts',(0.678522372573754,-1.17523522336992,
-11.895836364544));
#420820=CARTESIAN_POINT('Ctrl Pts',(1.01778355886063,-0.587617611684959,
-11.8541696978774));
#420821=CARTESIAN_POINT('Ctrl Pts',(1.35704474514751,2.29132775890901E-15,
-11.8125030312107));
#420822=CARTESIAN_POINT('Ctrl Pts',(1.01778355886063,0.587617611684963,
-11.770836364544));
#420823=CARTESIAN_POINT('Ctrl Pts',(0.678522372573755,1.17523522336992,
-11.7291696978774));
#420824=CARTESIAN_POINT('Ctrl Pts',(0.,1.17523522336992,-11.6875030312107));
#420825=CARTESIAN_POINT('Ctrl Pts',(-0.678522372573754,1.17523522336992,
-11.645836364544));
#420826=CARTESIAN_POINT('Ctrl Pts',(-1.01778355886063,0.587617611684963,
-11.6041696978774));
#420827=CARTESIAN_POINT('Ctrl Pts',(-1.35704474514751,2.62370785959794E-15,
-11.5625030312107));
#420828=CARTESIAN_POINT('Ctrl Pts',(-1.01778355886063,-0.587617611684958,
-11.520836364544));
#420829=CARTESIAN_POINT('Ctrl Pts',(-0.678522372573755,-1.17523522336992,
-11.4791696978774));
#420830=CARTESIAN_POINT('Ctrl Pts',(-1.4392480545452E-16,-1.17523522336992,
-11.4375030312107));
#420831=CARTESIAN_POINT('Ctrl Pts',(0.678522372573754,-1.17523522336992,
-11.395836364544));
#420832=CARTESIAN_POINT('Ctrl Pts',(1.01778355886063,-0.587617611684959,
-11.3541696978774));
#420833=CARTESIAN_POINT('Ctrl Pts',(1.35704474514751,2.29132775890901E-15,
-11.3125030312107));
#420834=CARTESIAN_POINT('Ctrl Pts',(1.01778355886063,0.587617611684963,
-11.270836364544));
#420835=CARTESIAN_POINT('Ctrl Pts',(0.678522372573755,1.17523522336992,
-11.2291696978774));
#420836=CARTESIAN_POINT('Ctrl Pts',(0.,1.17523522336992,-11.1875030312107));
#420837=CARTESIAN_POINT('Ctrl Pts',(-0.678522372573754,1.17523522336992,
-11.145836364544));
#420838=CARTESIAN_POINT('Ctrl Pts',(-1.01778355886063,0.587617611684963,
-11.1041696978774));
#420839=CARTESIAN_POINT('Ctrl Pts',(-1.35704474514751,2.62370785959794E-15,
-11.0625030312107));
#420840=CARTESIAN_POINT('Ctrl Pts',(-1.01778355886063,-0.587617611684958,
-11.020836364544));
#420841=CARTESIAN_POINT('Ctrl Pts',(-0.678522372573755,-1.17523522336992,
-10.9791696978774));
#420842=CARTESIAN_POINT('Ctrl Pts',(-1.4392480545452E-16,-1.17523522336992,
-10.9375030312107));
#420843=CARTESIAN_POINT('Ctrl Pts',(0.678522372573754,-1.17523522336992,
-10.895836364544));
#420844=CARTESIAN_POINT('Ctrl Pts',(1.01778355886063,-0.587617611684959,
-10.8541696978774));
#420845=CARTESIAN_POINT('Ctrl Pts',(1.35704474514751,2.29132775890901E-15,
-10.8125030312107));
#420846=CARTESIAN_POINT('Ctrl Pts',(1.01778355886063,0.587617611684963,
-10.770836364544));
#420847=CARTESIAN_POINT('Ctrl Pts',(0.678522372573755,1.17523522336992,
-10.7291696978774));
#420848=CARTESIAN_POINT('Ctrl Pts',(0.,1.17523522336992,-10.6875030312107));
#420849=CARTESIAN_POINT('Ctrl Pts',(-0.678522372573754,1.17523522336992,
-10.645836364544));
#420850=CARTESIAN_POINT('Ctrl Pts',(-1.01778355886063,0.587617611684963,
-10.6041696978774));
#420851=CARTESIAN_POINT('Ctrl Pts',(-1.35704474514751,2.62370785959794E-15,
-10.5625030312107));
#420852=CARTESIAN_POINT('Ctrl Pts',(-1.01778355886063,-0.587617611684958,
-10.520836364544));
#420853=CARTESIAN_POINT('Ctrl Pts',(-0.678522372573755,-1.17523522336992,
-10.4791696978774));
#420854=CARTESIAN_POINT('Ctrl Pts',(-1.4392480545452E-16,-1.17523522336992,
-10.4375030312107));
#420855=CARTESIAN_POINT('Ctrl Pts',(0.678522372573754,-1.17523522336992,
-10.395836364544));
#420856=CARTESIAN_POINT('Ctrl Pts',(1.01778355886063,-0.587617611684959,
-10.3541696978774));
#420857=CARTESIAN_POINT('Ctrl Pts',(1.35704474514751,2.29132775890901E-15,
-10.3125030312107));
#420858=CARTESIAN_POINT('Ctrl Pts',(1.01778355886063,0.587617611684963,
-10.270836364544));
#420859=CARTESIAN_POINT('Ctrl Pts',(0.678522372573755,1.17523522336992,
-10.2291696978774));
#420860=CARTESIAN_POINT('Ctrl Pts',(0.,1.17523522336992,-10.1875030312107));
#420861=CARTESIAN_POINT('Ctrl Pts',(-0.678522372573754,1.17523522336992,
-10.145836364544));
#420862=CARTESIAN_POINT('Ctrl Pts',(-1.01778355886063,0.587617611684963,
-10.1041696978774));
#420863=CARTESIAN_POINT('Ctrl Pts',(-1.35704474514751,2.62370785959794E-15,
-10.0625030312107));
#420864=CARTESIAN_POINT('Ctrl Pts',(-1.01778355886063,-0.587617611684958,
-10.020836364544));
#420865=CARTESIAN_POINT('Ctrl Pts',(-0.678522372573755,-1.17523522336992,
-9.97916969787736));
#420866=CARTESIAN_POINT('Ctrl Pts',(-1.4392480545452E-16,-1.17523522336992,
-9.9375030312107));
#420867=CARTESIAN_POINT('Ctrl Pts',(0.678522372573754,-1.17523522336992,
-9.89583636454403));
#420868=CARTESIAN_POINT('Ctrl Pts',(1.01778355886063,-0.587617611684959,
-9.85416969787736));
#420869=CARTESIAN_POINT('Ctrl Pts',(1.35704474514751,2.29132775890901E-15,
-9.8125030312107));
#420870=CARTESIAN_POINT('Ctrl Pts',(1.01778355886063,0.587617611684963,
-9.77083636454403));
#420871=CARTESIAN_POINT('Ctrl Pts',(0.678522372573755,1.17523522336992,
-9.72916969787736));
#420872=CARTESIAN_POINT('Ctrl Pts',(0.,1.17523522336992,-9.6875030312107));
#420873=CARTESIAN_POINT('Ctrl Pts',(-0.678522372573754,1.17523522336992,
-9.64583636454403));
#420874=CARTESIAN_POINT('Ctrl Pts',(-1.01778355886063,0.587617611684963,
-9.60416969787736));
#420875=CARTESIAN_POINT('Ctrl Pts',(-1.35704474514751,2.62370785959794E-15,
-9.5625030312107));
#420876=CARTESIAN_POINT('Ctrl Pts',(-1.01778355886063,-0.587617611684958,
-9.52083636454403));
#420877=CARTESIAN_POINT('Ctrl Pts',(-0.678522372573755,-1.17523522336992,
-9.47916969787736));
#420878=CARTESIAN_POINT('Ctrl Pts',(-1.4392480545452E-16,-1.17523522336992,
-9.4375030312107));
#420879=CARTESIAN_POINT('Ctrl Pts',(0.678522372573754,-1.17523522336992,
-9.39583636454403));
#420880=CARTESIAN_POINT('Ctrl Pts',(1.01778355886063,-0.587617611684959,
-9.35416969787736));
#420881=CARTESIAN_POINT('Ctrl Pts',(1.35704474514751,2.29132775890901E-15,
-9.3125030312107));
#420882=CARTESIAN_POINT('Ctrl Pts',(1.01778355886063,0.587617611684963,
-9.27083636454403));
#420883=CARTESIAN_POINT('Ctrl Pts',(0.678522372573755,1.17523522336992,
-9.22916969787736));
#420884=CARTESIAN_POINT('Ctrl Pts',(0.,1.17523522336992,-9.1875030312107));
#420885=CARTESIAN_POINT('Ctrl Pts',(-0.678522372573754,1.17523522336992,
-9.14583636454403));
#420886=CARTESIAN_POINT('Ctrl Pts',(-1.01778355886063,0.587617611684963,
-9.10416969787736));
#420887=CARTESIAN_POINT('Ctrl Pts',(-1.35704474514751,2.62370785959794E-15,
-9.0625030312107));
#420888=CARTESIAN_POINT('Ctrl Pts',(-1.01778355886063,-0.587617611684958,
-9.02083636454403));
#420889=CARTESIAN_POINT('Ctrl Pts',(-0.678522372573755,-1.17523522336992,
-8.97916969787736));
#420890=CARTESIAN_POINT('Ctrl Pts',(-1.4392480545452E-16,-1.17523522336992,
-8.9375030312107));
#420891=CARTESIAN_POINT('Ctrl Pts',(0.678522372573754,-1.17523522336992,
-8.89583636454403));
#420892=CARTESIAN_POINT('Ctrl Pts',(1.01778355886063,-0.587617611684959,
-8.85416969787736));
#420893=CARTESIAN_POINT('Ctrl Pts',(1.35704474514751,2.29132775890901E-15,
-8.8125030312107));
#420894=CARTESIAN_POINT('Ctrl Pts',(1.01778355886063,0.587617611684963,
-8.77083636454403));
#420895=CARTESIAN_POINT('Ctrl Pts',(0.678522372573755,1.17523522336992,
-8.72916969787736));
#420896=CARTESIAN_POINT('Ctrl Pts',(0.,1.17523522336992,-8.6875030312107));
#420897=CARTESIAN_POINT('Ctrl Pts',(-0.678522372573754,1.17523522336992,
-8.64583636454403));
#420898=CARTESIAN_POINT('Ctrl Pts',(-1.01778355886063,0.587617611684963,
-8.60416969787736));
#420899=CARTESIAN_POINT('Ctrl Pts',(-1.35704474514751,2.62370785959794E-15,
-8.5625030312107));
#420900=CARTESIAN_POINT('Ctrl Pts',(-1.01778355886063,-0.587617611684958,
-8.52083636454403));
#420901=CARTESIAN_POINT('Ctrl Pts',(-0.678522372573755,-1.17523522336992,
-8.47916969787736));
#420902=CARTESIAN_POINT('Ctrl Pts',(-1.4392480545452E-16,-1.17523522336992,
-8.43750303121069));
#420903=CARTESIAN_POINT('Ctrl Pts',(0.678522372573754,-1.17523522336992,
-8.39583636454403));
#420904=CARTESIAN_POINT('Ctrl Pts',(1.01778355886063,-0.587617611684959,
-8.35416969787736));
#420905=CARTESIAN_POINT('Ctrl Pts',(1.35704474514751,2.29132775890901E-15,
-8.31250303121069));
#420906=CARTESIAN_POINT('Ctrl Pts',(1.01778355886063,0.587617611684963,
-8.27083636454403));
#420907=CARTESIAN_POINT('Ctrl Pts',(0.678522372573755,1.17523522336992,
-8.22916969787736));
#420908=CARTESIAN_POINT('Ctrl Pts',(0.,1.17523522336992,-8.1875030312107));
#420909=CARTESIAN_POINT('Ctrl Pts',(-0.678522372573754,1.17523522336992,
-8.14583636454403));
#420910=CARTESIAN_POINT('Ctrl Pts',(-1.01778355886063,0.587617611684963,
-8.10416969787736));
#420911=CARTESIAN_POINT('Ctrl Pts',(-1.35704474514751,2.62370785959794E-15,
-8.0625030312107));
#420912=CARTESIAN_POINT('Ctrl Pts',(-1.01778355886063,-0.587617611684958,
-8.02083636454403));
#420913=CARTESIAN_POINT('Ctrl Pts',(-0.678522372573755,-1.17523522336992,
-7.97916969787736));
#420914=CARTESIAN_POINT('Ctrl Pts',(-1.4392480545452E-16,-1.17523522336992,
-7.9375030312107));
#420915=CARTESIAN_POINT('Ctrl Pts',(0.678522372573754,-1.17523522336992,
-7.89583636454403));
#420916=CARTESIAN_POINT('Ctrl Pts',(1.01778355886063,-0.587617611684959,
-7.85416969787736));
#420917=CARTESIAN_POINT('Ctrl Pts',(1.35704474514751,2.29132775890901E-15,
-7.8125030312107));
#420918=CARTESIAN_POINT('Ctrl Pts',(1.01778355886063,0.587617611684963,
-7.77083636454403));
#420919=CARTESIAN_POINT('Ctrl Pts',(0.678522372573755,1.17523522336992,
-7.72916969787736));
#420920=CARTESIAN_POINT('Ctrl Pts',(0.,1.17523522336992,-7.68750303121069));
#420921=CARTESIAN_POINT('Ctrl Pts',(-0.678522372573754,1.17523522336992,
-7.64583636454403));
#420922=CARTESIAN_POINT('Ctrl Pts',(-1.01778355886063,0.587617611684963,
-7.60416969787736));
#420923=CARTESIAN_POINT('Ctrl Pts',(-1.35704474514751,2.62370785959794E-15,
-7.5625030312107));
#420924=CARTESIAN_POINT('Ctrl Pts',(-1.01778355886063,-0.587617611684958,
-7.52083636454403));
#420925=CARTESIAN_POINT('Ctrl Pts',(-0.678522372573755,-1.17523522336992,
-7.47916969787736));
#420926=CARTESIAN_POINT('Ctrl Pts',(-1.4392480545452E-16,-1.17523522336992,
-7.4375030312107));
#420927=CARTESIAN_POINT('Ctrl Pts',(0.678522372573754,-1.17523522336992,
-7.39583636454403));
#420928=CARTESIAN_POINT('Ctrl Pts',(1.01778355886063,-0.587617611684959,
-7.35416969787736));
#420929=CARTESIAN_POINT('Ctrl Pts',(1.35704474514751,2.29132775890901E-15,
-7.31250303121069));
#420930=CARTESIAN_POINT('Ctrl Pts',(1.01778355886063,0.587617611684963,
-7.27083636454403));
#420931=CARTESIAN_POINT('Ctrl Pts',(0.678522372573755,1.17523522336992,
-7.22916969787736));
#420932=CARTESIAN_POINT('Ctrl Pts',(0.,1.17523522336992,-7.1875030312107));
#420933=CARTESIAN_POINT('Ctrl Pts',(-0.678522372573754,1.17523522336992,
-7.14583636454403));
#420934=CARTESIAN_POINT('Ctrl Pts',(-1.01778355886063,0.587617611684963,
-7.10416969787736));
#420935=CARTESIAN_POINT('Ctrl Pts',(-1.35704474514751,2.62370785959794E-15,
-7.0625030312107));
#420936=CARTESIAN_POINT('Ctrl Pts',(-1.01778355886063,-0.587617611684958,
-7.02083636454403));
#420937=CARTESIAN_POINT('Ctrl Pts',(-0.678522372573755,-1.17523522336992,
-6.97916969787736));
#420938=CARTESIAN_POINT('Ctrl Pts',(-1.4392480545452E-16,-1.17523522336992,
-6.9375030312107));
#420939=CARTESIAN_POINT('Ctrl Pts',(0.678522372573754,-1.17523522336992,
-6.89583636454403));
#420940=CARTESIAN_POINT('Ctrl Pts',(1.01778355886063,-0.587617611684959,
-6.85416969787736));
#420941=CARTESIAN_POINT('Ctrl Pts',(1.35704474514751,2.29132775890901E-15,
-6.8125030312107));
#420942=CARTESIAN_POINT('Ctrl Pts',(1.01778355886063,0.587617611684963,
-6.77083636454403));
#420943=CARTESIAN_POINT('Ctrl Pts',(0.678522372573755,1.17523522336992,
-6.72916969787736));
#420944=CARTESIAN_POINT('Ctrl Pts',(0.,1.17523522336992,-6.6875030312107));
#420945=CARTESIAN_POINT('Ctrl Pts',(-0.678522372573754,1.17523522336992,
-6.64583636454403));
#420946=CARTESIAN_POINT('Ctrl Pts',(-1.01778355886063,0.587617611684963,
-6.60416969787736));
#420947=CARTESIAN_POINT('Ctrl Pts',(-1.35704474514751,2.62370785959794E-15,
-6.5625030312107));
#420948=CARTESIAN_POINT('Ctrl Pts',(-1.01778355886063,-0.587617611684958,
-6.52083636454403));
#420949=CARTESIAN_POINT('Ctrl Pts',(-0.678522372573755,-1.17523522336992,
-6.47916969787736));
#420950=CARTESIAN_POINT('Ctrl Pts',(-1.4392480545452E-16,-1.17523522336992,
-6.4375030312107));
#420951=CARTESIAN_POINT('Ctrl Pts',(0.678522372573754,-1.17523522336992,
-6.39583636454403));
#420952=CARTESIAN_POINT('Ctrl Pts',(1.01778355886063,-0.587617611684959,
-6.35416969787736));
#420953=CARTESIAN_POINT('Ctrl Pts',(1.35704474514751,2.29132775890901E-15,
-6.3125030312107));
#420954=CARTESIAN_POINT('Ctrl Pts',(1.01778355886063,0.587617611684963,
-6.27083636454403));
#420955=CARTESIAN_POINT('Ctrl Pts',(0.678522372573755,1.17523522336992,
-6.22916969787736));
#420956=CARTESIAN_POINT('Ctrl Pts',(0.,1.17523522336992,-6.18750303121069));
#420957=CARTESIAN_POINT('Ctrl Pts',(-0.678522372573754,1.17523522336992,
-6.14583636454403));
#420958=CARTESIAN_POINT('Ctrl Pts',(-1.01778355886063,0.587617611684963,
-6.10416969787736));
#420959=CARTESIAN_POINT('Ctrl Pts',(-1.35704474514751,2.62370785959794E-15,
-6.0625030312107));
#420960=CARTESIAN_POINT('Ctrl Pts',(-1.01778355886063,-0.587617611684958,
-6.02083636454403));
#420961=CARTESIAN_POINT('Ctrl Pts',(-0.678522372573755,-1.17523522336992,
-5.97916969787736));
#420962=CARTESIAN_POINT('Ctrl Pts',(-1.4392480545452E-16,-1.17523522336992,
-5.9375030312107));
#420963=CARTESIAN_POINT('Ctrl Pts',(0.678522372573754,-1.17523522336992,
-5.89583636454403));
#420964=CARTESIAN_POINT('Ctrl Pts',(1.01778355886063,-0.587617611684959,
-5.85416969787736));
#420965=CARTESIAN_POINT('Ctrl Pts',(1.35704474514751,2.29132775890901E-15,
-5.81250303121069));
#420966=CARTESIAN_POINT('Ctrl Pts',(1.01778355886063,0.587617611684963,
-5.77083636454403));
#420967=CARTESIAN_POINT('Ctrl Pts',(0.678522372573755,1.17523522336992,
-5.72916969787736));
#420968=CARTESIAN_POINT('Ctrl Pts',(0.,1.17523522336992,-5.6875030312107));
#420969=CARTESIAN_POINT('Ctrl Pts',(-0.678522372573754,1.17523522336992,
-5.64583636454403));
#420970=CARTESIAN_POINT('Ctrl Pts',(-1.01778355886063,0.587617611684963,
-5.60416969787736));
#420971=CARTESIAN_POINT('Ctrl Pts',(-1.35704474514751,2.62370785959794E-15,
-5.5625030312107));
#420972=CARTESIAN_POINT('Ctrl Pts',(-1.01778355886063,-0.587617611684958,
-5.52083636454403));
#420973=CARTESIAN_POINT('Ctrl Pts',(-0.678522372573755,-1.17523522336992,
-5.47916969787736));
#420974=CARTESIAN_POINT('Ctrl Pts',(-1.4392480545452E-16,-1.17523522336992,
-5.4375030312107));
#420975=CARTESIAN_POINT('Ctrl Pts',(0.678522372573754,-1.17523522336992,
-5.39583636454403));
#420976=CARTESIAN_POINT('Ctrl Pts',(1.01778355886063,-0.587617611684959,
-5.35416969787736));
#420977=CARTESIAN_POINT('Ctrl Pts',(1.35704474514751,2.29132775890901E-15,
-5.3125030312107));
#420978=CARTESIAN_POINT('Ctrl Pts',(1.01778355886063,0.587617611684963,
-5.27083636454403));
#420979=CARTESIAN_POINT('Ctrl Pts',(0.678522372573755,1.17523522336992,
-5.22916969787736));
#420980=CARTESIAN_POINT('Ctrl Pts',(0.,1.17523522336992,-5.1875030312107));
#420981=CARTESIAN_POINT('Ctrl Pts',(-0.678522372573754,1.17523522336992,
-5.14583636454403));
#420982=CARTESIAN_POINT('Ctrl Pts',(-1.01778355886063,0.587617611684963,
-5.10416969787736));
#420983=CARTESIAN_POINT('Ctrl Pts',(-1.35704474514751,2.62370785959794E-15,
-5.0625030312107));
#420984=CARTESIAN_POINT('Ctrl Pts',(-1.01778355886063,-0.587617611684958,
-5.02083636454403));
#420985=CARTESIAN_POINT('Ctrl Pts',(-0.678522372573755,-1.17523522336992,
-4.97916969787736));
#420986=CARTESIAN_POINT('Ctrl Pts',(-1.4392480545452E-16,-1.17523522336992,
-4.9375030312107));
#420987=CARTESIAN_POINT('Ctrl Pts',(0.678522372573754,-1.17523522336992,
-4.89583636454403));
#420988=CARTESIAN_POINT('Ctrl Pts',(1.01778355886063,-0.587617611684959,
-4.85416969787736));
#420989=CARTESIAN_POINT('Ctrl Pts',(1.35704474514751,2.29132775890901E-15,
-4.8125030312107));
#420990=CARTESIAN_POINT('Ctrl Pts',(1.01778355886063,0.587617611684963,
-4.77083636454403));
#420991=CARTESIAN_POINT('Ctrl Pts',(0.678522372573755,1.17523522336992,
-4.72916969787736));
#420992=CARTESIAN_POINT('Ctrl Pts',(0.,1.17523522336992,-4.6875030312107));
#420993=CARTESIAN_POINT('Ctrl Pts',(-0.678522372573754,1.17523522336992,
-4.64583636454403));
#420994=CARTESIAN_POINT('Ctrl Pts',(-1.01778355886063,0.587617611684963,
-4.60416969787736));
#420995=CARTESIAN_POINT('Ctrl Pts',(-1.35704474514751,2.62370785959794E-15,
-4.5625030312107));
#420996=CARTESIAN_POINT('Ctrl Pts',(-1.01778355886063,-0.587617611684958,
-4.52083636454403));
#420997=CARTESIAN_POINT('Ctrl Pts',(-0.678522372573755,-1.17523522336992,
-4.47916969787736));
#420998=CARTESIAN_POINT('Ctrl Pts',(-1.4392480545452E-16,-1.17523522336992,
-4.4375030312107));
#420999=CARTESIAN_POINT('Ctrl Pts',(0.678522372573754,-1.17523522336992,
-4.39583636454403));
#421000=CARTESIAN_POINT('Ctrl Pts',(1.01778355886063,-0.587617611684959,
-4.35416969787736));
#421001=CARTESIAN_POINT('Ctrl Pts',(1.35704474514751,2.29132775890901E-15,
-4.3125030312107));
#421002=CARTESIAN_POINT('Ctrl Pts',(1.01778355886063,0.587617611684963,
-4.27083636454403));
#421003=CARTESIAN_POINT('Ctrl Pts',(0.678522372573755,1.17523522336992,
-4.22916969787736));
#421004=CARTESIAN_POINT('Ctrl Pts',(0.,1.17523522336992,-4.1875030312107));
#421005=CARTESIAN_POINT('Ctrl Pts',(-0.678522372573754,1.17523522336992,
-4.14583636454403));
#421006=CARTESIAN_POINT('Ctrl Pts',(-1.01778355886063,0.587617611684963,
-4.10416969787736));
#421007=CARTESIAN_POINT('Ctrl Pts',(-1.35704474514751,2.62370785959794E-15,
-4.0625030312107));
#421008=CARTESIAN_POINT('Ctrl Pts',(-1.01778355886063,-0.587617611684958,
-4.02083636454403));
#421009=CARTESIAN_POINT('Ctrl Pts',(-0.678522372573755,-1.17523522336992,
-3.97916969787736));
#421010=CARTESIAN_POINT('Ctrl Pts',(-1.4392480545452E-16,-1.17523522336992,
-3.93750303121069));
#421011=CARTESIAN_POINT('Ctrl Pts',(0.678522372573754,-1.17523522336992,
-3.89583636454403));
#421012=CARTESIAN_POINT('Ctrl Pts',(1.01778355886063,-0.587617611684959,
-3.85416969787736));
#421013=CARTESIAN_POINT('Ctrl Pts',(1.35704474514751,2.29132775890901E-15,
-3.8125030312107));
#421014=CARTESIAN_POINT('Ctrl Pts',(1.01778355886063,0.587617611684963,
-3.77083636454403));
#421015=CARTESIAN_POINT('Ctrl Pts',(0.678522372573755,1.17523522336992,
-3.72916969787736));
#421016=CARTESIAN_POINT('Ctrl Pts',(0.,1.17523522336992,-3.6875030312107));
#421017=CARTESIAN_POINT('Ctrl Pts',(-0.678522372573754,1.17523522336992,
-3.64583636454403));
#421018=CARTESIAN_POINT('Ctrl Pts',(-1.01778355886063,0.587617611684963,
-3.60416969787736));
#421019=CARTESIAN_POINT('Ctrl Pts',(-1.35704474514751,2.62370785959794E-15,
-3.5625030312107));
#421020=CARTESIAN_POINT('Ctrl Pts',(-1.01778355886063,-0.587617611684958,
-3.52083636454403));
#421021=CARTESIAN_POINT('Ctrl Pts',(-0.678522372573755,-1.17523522336992,
-3.47916969787736));
#421022=CARTESIAN_POINT('Ctrl Pts',(-1.4392480545452E-16,-1.17523522336992,
-3.4375030312107));
#421023=CARTESIAN_POINT('Ctrl Pts',(0.678522372573754,-1.17523522336992,
-3.39583636454403));
#421024=CARTESIAN_POINT('Ctrl Pts',(1.01778355886063,-0.587617611684959,
-3.35416969787736));
#421025=CARTESIAN_POINT('Ctrl Pts',(1.35704474514751,2.29132775890901E-15,
-3.3125030312107));
#421026=CARTESIAN_POINT('Ctrl Pts',(1.01778355886063,0.587617611684963,
-3.27083636454403));
#421027=CARTESIAN_POINT('Ctrl Pts',(0.678522372573755,1.17523522336992,
-3.22916969787736));
#421028=CARTESIAN_POINT('Ctrl Pts',(0.,1.17523522336992,-3.1875030312107));
#421029=CARTESIAN_POINT('Ctrl Pts',(-0.678522372573754,1.17523522336992,
-3.14583636454403));
#421030=CARTESIAN_POINT('Ctrl Pts',(-1.01778355886063,0.587617611684963,
-3.10416969787736));
#421031=CARTESIAN_POINT('Ctrl Pts',(-1.35704474514751,2.62370785959794E-15,
-3.0625030312107));
#421032=CARTESIAN_POINT('Ctrl Pts',(-1.01778355886063,-0.587617611684958,
-3.02083636454403));
#421033=CARTESIAN_POINT('Ctrl Pts',(-0.678522372573755,-1.17523522336992,
-2.97916969787736));
#421034=CARTESIAN_POINT('Ctrl Pts',(-1.4392480545452E-16,-1.17523522336992,
-2.9375030312107));
#421035=CARTESIAN_POINT('Ctrl Pts',(0.678522372573754,-1.17523522336992,
-2.89583636454403));
#421036=CARTESIAN_POINT('Ctrl Pts',(1.01778355886063,-0.587617611684959,
-2.85416969787736));
#421037=CARTESIAN_POINT('Ctrl Pts',(1.35704474514751,2.29132775890901E-15,
-2.8125030312107));
#421038=CARTESIAN_POINT('Ctrl Pts',(1.01778355886063,0.587617611684963,
-2.77083636454403));
#421039=CARTESIAN_POINT('Ctrl Pts',(0.678522372573755,1.17523522336992,
-2.72916969787736));
#421040=CARTESIAN_POINT('Ctrl Pts',(0.,1.17523522336992,-2.6875030312107));
#421041=CARTESIAN_POINT('Ctrl Pts',(-0.678522372573754,1.17523522336992,
-2.64583636454403));
#421042=CARTESIAN_POINT('Ctrl Pts',(-1.01778355886063,0.587617611684963,
-2.60416969787736));
#421043=CARTESIAN_POINT('Ctrl Pts',(-1.35704474514751,2.62370785959794E-15,
-2.56250303121069));
#421044=CARTESIAN_POINT('Ctrl Pts',(-1.01778355886063,-0.587617611684958,
-2.52083636454403));
#421045=CARTESIAN_POINT('Ctrl Pts',(-0.678522372573755,-1.17523522336992,
-2.47916969787736));
#421046=CARTESIAN_POINT('Ctrl Pts',(-1.4392480545452E-16,-1.17523522336992,
-2.4375030312107));
#421047=CARTESIAN_POINT('Ctrl Pts',(0.678522372573754,-1.17523522336992,
-2.39583636454403));
#421048=CARTESIAN_POINT('Ctrl Pts',(1.01778355886063,-0.587617611684959,
-2.35416969787736));
#421049=CARTESIAN_POINT('Ctrl Pts',(1.35704474514751,2.29132775890901E-15,
-2.31250303121069));
#421050=CARTESIAN_POINT('Ctrl Pts',(1.01778355886063,0.587617611684963,
-2.27083636454403));
#421051=CARTESIAN_POINT('Ctrl Pts',(0.678522372573755,1.17523522336992,
-2.22916969787736));
#421052=CARTESIAN_POINT('Ctrl Pts',(0.,1.17523522336992,-2.1875030312107));
#421053=CARTESIAN_POINT('Ctrl Pts',(-0.678522372573754,1.17523522336992,
-2.14583636454403));
#421054=CARTESIAN_POINT('Ctrl Pts',(-1.01778355886063,0.587617611684963,
-2.10416969787736));
#421055=CARTESIAN_POINT('Ctrl Pts',(-1.35704474514751,2.62370785959794E-15,
-2.0625030312107));
#421056=CARTESIAN_POINT('Ctrl Pts',(-1.01778355886063,-0.587617611684958,
-2.02083636454403));
#421057=CARTESIAN_POINT('Ctrl Pts',(-0.678522372573755,-1.17523522336992,
-1.97916969787736));
#421058=CARTESIAN_POINT('Ctrl Pts',(-1.4392480545452E-16,-1.17523522336992,
-1.9375030312107));
#421059=CARTESIAN_POINT('Ctrl Pts',(0.678522372573754,-1.17523522336992,
-1.89583636454403));
#421060=CARTESIAN_POINT('Ctrl Pts',(1.01778355886063,-0.587617611684959,
-1.85416969787736));
#421061=CARTESIAN_POINT('Ctrl Pts',(1.35704474514751,2.29132775890901E-15,
-1.8125030312107));
#421062=CARTESIAN_POINT('Ctrl Pts',(1.01778355886063,0.587617611684963,
-1.77083636454403));
#421063=CARTESIAN_POINT('Ctrl Pts',(0.678522372573755,1.17523522336992,
-1.72916969787736));
#421064=CARTESIAN_POINT('Ctrl Pts',(0.,1.17523522336992,-1.6875030312107));
#421065=CARTESIAN_POINT('Ctrl Pts',(-0.678522372573754,1.17523522336992,
-1.64583636454403));
#421066=CARTESIAN_POINT('Ctrl Pts',(-1.01778355886063,0.587617611684963,
-1.60416969787736));
#421067=CARTESIAN_POINT('Ctrl Pts',(-1.35704474514751,2.62370785959794E-15,
-1.5625030312107));
#421068=CARTESIAN_POINT('Ctrl Pts',(-1.01778355886063,-0.587617611684958,
-1.52083636454403));
#421069=CARTESIAN_POINT('Ctrl Pts',(-0.678522372573755,-1.17523522336992,
-1.47916969787736));
#421070=CARTESIAN_POINT('Ctrl Pts',(-1.4392480545452E-16,-1.17523522336992,
-1.4375030312107));
#421071=CARTESIAN_POINT('Ctrl Pts',(0.678522372573754,-1.17523522336992,
-1.39583636454403));
#421072=CARTESIAN_POINT('Ctrl Pts',(1.01778355886063,-0.587617611684959,
-1.35416969787736));
#421073=CARTESIAN_POINT('Ctrl Pts',(1.35704474514751,2.29132775890901E-15,
-1.3125030312107));
#421074=CARTESIAN_POINT('Ctrl Pts',(1.01778355886063,0.587617611684963,
-1.27083636454403));
#421075=CARTESIAN_POINT('Ctrl Pts',(0.678522372573755,1.17523522336992,
-1.22916969787736));
#421076=CARTESIAN_POINT('Ctrl Pts',(0.,1.17523522336992,-1.1875030312107));
#421077=CARTESIAN_POINT('Ctrl Pts',(-0.678522372573754,1.17523522336992,
-1.14583636454403));
#421078=CARTESIAN_POINT('Ctrl Pts',(-1.01778355886063,0.587617611684963,
-1.10416969787736));
#421079=CARTESIAN_POINT('Ctrl Pts',(-1.35704474514751,2.62370785959794E-15,
-1.0625030312107));
#421080=CARTESIAN_POINT('Ctrl Pts',(-1.01778355886063,-0.587617611684958,
-1.02083636454403));
#421081=CARTESIAN_POINT('Ctrl Pts',(-0.678522372573755,-1.17523522336992,
-0.979169697877363));
#421082=CARTESIAN_POINT('Ctrl Pts',(-1.4392480545452E-16,-1.17523522336992,
-0.937503031210696));
#421083=CARTESIAN_POINT('Ctrl Pts',(0.678522372573754,-1.17523522336992,
-0.895836364544029));
#421084=CARTESIAN_POINT('Ctrl Pts',(1.01778355886063,-0.587617611684959,
-0.854169697877363));
#421085=CARTESIAN_POINT('Ctrl Pts',(1.35704474514751,2.29132775890901E-15,
-0.812503031210696));
#421086=CARTESIAN_POINT('Ctrl Pts',(1.01778355886063,0.587617611684963,
-0.770836364544028));
#421087=CARTESIAN_POINT('Ctrl Pts',(0.678522372573755,1.17523522336992,
-0.729169697877363));
#421088=CARTESIAN_POINT('Ctrl Pts',(0.,1.17523522336992,-0.687503031210696));
#421089=CARTESIAN_POINT('Ctrl Pts',(-0.678522372573754,1.17523522336992,
-0.64583636454403));
#421090=CARTESIAN_POINT('Ctrl Pts',(-1.01778355886063,0.587617611684963,
-0.604169697877363));
#421091=CARTESIAN_POINT('Ctrl Pts',(-1.35704474514751,2.62370785959794E-15,
-0.562503031210696));
#421092=CARTESIAN_POINT('Ctrl Pts',(-1.01778355886063,-0.587617611684958,
-0.52083636454403));
#421093=CARTESIAN_POINT('Ctrl Pts',(-0.678522372573755,-1.17523522336992,
-0.479169697877363));
#421094=CARTESIAN_POINT('Ctrl Pts',(-1.4392480545452E-16,-1.17523522336992,
-0.437503031210695));
#421095=CARTESIAN_POINT('Ctrl Pts',(0.678522372573754,-1.17523522336992,
-0.39583636454403));
#421096=CARTESIAN_POINT('Ctrl Pts',(1.01778355886063,-0.587617611684959,
-0.354169697877363));
#421097=CARTESIAN_POINT('Ctrl Pts',(1.35704474514751,2.29132775890901E-15,
-0.312503031210695));
#421098=CARTESIAN_POINT('Ctrl Pts',(1.01778355886063,0.587617611684963,
-0.27083636454403));
#421099=CARTESIAN_POINT('Ctrl Pts',(0.678522372573755,1.17523522336992,
-0.229169697877362));
#421100=CARTESIAN_POINT('Ctrl Pts',(0.,1.17523522336992,-0.187503031210695));
#421101=CARTESIAN_POINT('Ctrl Pts',(-0.678522372573754,1.17523522336992,
-0.14583636454403));
#421102=CARTESIAN_POINT('Ctrl Pts',(-1.01778355886063,0.587617611684963,
-0.104169697877362));
#421103=CARTESIAN_POINT('Ctrl Pts',(-1.35704474514751,2.62370785959794E-15,
-0.0625030312106968));
#421104=CARTESIAN_POINT('Ctrl Pts',(-1.01778355886063,-0.587617611684958,
-0.0208363645440295));
#421105=CARTESIAN_POINT('Ctrl Pts',(-0.678522372573755,-1.17523522336992,
0.0208303021226378));
#421106=CARTESIAN_POINT('Ctrl Pts',(-1.4392480545452E-16,-1.17523522336992,
0.0624969687893033));
#421107=CARTESIAN_POINT('Ctrl Pts',(0.678522372573754,-1.17523522336992,
0.104163635455971));
#421108=CARTESIAN_POINT('Ctrl Pts',(1.01778355886063,-0.587617611684959,
0.145830302122638));
#421109=CARTESIAN_POINT('Ctrl Pts',(1.35704474514751,2.29132775890901E-15,
0.187496968789303));
#421110=CARTESIAN_POINT('Ctrl Pts',(1.01778355886063,0.587617611684963,
0.229163635455971));
#421111=CARTESIAN_POINT('Ctrl Pts',(0.678522372573755,1.17523522336992,
0.270830302122638));
#421112=CARTESIAN_POINT('Ctrl Pts',(0.,1.17523522336992,0.312496968789304));
#421113=CARTESIAN_POINT('Ctrl Pts',(-0.678522372573754,1.17523522336992,
0.354163635455971));
#421114=CARTESIAN_POINT('Ctrl Pts',(-1.01778355886063,0.587617611684963,
0.395830302122638));
#421115=CARTESIAN_POINT('Ctrl Pts',(-1.35704474514751,2.62370785959794E-15,
0.437496968789304));
#421116=CARTESIAN_POINT('Ctrl Pts',(-1.01778355886063,-0.587617611684958,
0.479163635455971));
#421117=CARTESIAN_POINT('Ctrl Pts',(-0.678522372573755,-1.17523522336992,
0.520830302122638));
#421118=CARTESIAN_POINT('Ctrl Pts',(-1.4392480545452E-16,-1.17523522336992,
0.562496968789304));
#421119=CARTESIAN_POINT('Ctrl Pts',(0.678522372573754,-1.17523522336992,
0.604163635455971));
#421120=CARTESIAN_POINT('Ctrl Pts',(1.01778355886063,-0.587617611684959,
0.645830302122637));
#421121=CARTESIAN_POINT('Ctrl Pts',(1.35704474514751,2.29132775890901E-15,
0.687496968789304));
#421122=CARTESIAN_POINT('Ctrl Pts',(1.01778355886063,0.587617611684963,
0.729163635455971));
#421123=CARTESIAN_POINT('Ctrl Pts',(0.678522372573755,1.17523522336992,
0.770830302122637));
#421124=CARTESIAN_POINT('Ctrl Pts',(0.,1.17523522336992,0.812496968789304));
#421125=CARTESIAN_POINT('Ctrl Pts',(-0.678522372573754,1.17523522336992,
0.854163635455971));
#421126=CARTESIAN_POINT('Ctrl Pts',(-1.01778355886063,0.587617611684963,
0.895830302122637));
#421127=CARTESIAN_POINT('Ctrl Pts',(-1.35704474514751,2.62370785959794E-15,
0.937496968789304));
#421128=CARTESIAN_POINT('Ctrl Pts',(-1.01778355886063,-0.587617611684958,
0.979163635455971));
#421129=CARTESIAN_POINT('Ctrl Pts',(-0.678522372573755,-1.17523522336992,
1.02083030212264));
#421130=CARTESIAN_POINT('Ctrl Pts',(-1.4392480545452E-16,-1.17523522336992,
1.0624969687893));
#421131=CARTESIAN_POINT('Ctrl Pts',(0.678522372573754,-1.17523522336992,
1.10416363545597));
#421132=CARTESIAN_POINT('Ctrl Pts',(1.01778355886063,-0.587617611684959,
1.14583030212264));
#421133=CARTESIAN_POINT('Ctrl Pts',(1.35704474514751,2.29132775890901E-15,
1.1874969687893));
#421134=CARTESIAN_POINT('Ctrl Pts',(1.01778355886063,0.587617611684963,
1.22916363545597));
#421135=CARTESIAN_POINT('Ctrl Pts',(0.678522372573755,1.17523522336992,
1.27083030212264));
#421136=CARTESIAN_POINT('Ctrl Pts',(0.,1.17523522336992,1.3124969687893));
#421137=CARTESIAN_POINT('Ctrl Pts',(-0.678522372573754,1.17523522336992,
1.35416363545597));
#421138=CARTESIAN_POINT('Ctrl Pts',(-1.01778355886063,0.587617611684963,
1.39583030212264));
#421139=CARTESIAN_POINT('Ctrl Pts',(-1.35704474514751,2.62370785959794E-15,
1.4374969687893));
#421140=CARTESIAN_POINT('Ctrl Pts',(-1.01778355886063,-0.587617611684958,
1.47916363545597));
#421141=CARTESIAN_POINT('Ctrl Pts',(-0.678522372573755,-1.17523522336992,
1.52083030212264));
#421142=CARTESIAN_POINT('Ctrl Pts',(-1.4392480545452E-16,-1.17523522336992,
1.5624969687893));
#421143=CARTESIAN_POINT('Ctrl Pts',(0.678522372573754,-1.17523522336992,
1.60416363545597));
#421144=CARTESIAN_POINT('Ctrl Pts',(1.01778355886063,-0.587617611684959,
1.64583030212264));
#421145=CARTESIAN_POINT('Ctrl Pts',(1.35704474514751,2.29132775890901E-15,
1.68749696878931));
#421146=CARTESIAN_POINT('Ctrl Pts',(1.01778355886063,0.587617611684963,
1.72916363545597));
#421147=CARTESIAN_POINT('Ctrl Pts',(0.678522372573755,1.17523522336992,
1.77083030212264));
#421148=CARTESIAN_POINT('Ctrl Pts',(0.,1.17523522336992,1.8124969687893));
#421149=CARTESIAN_POINT('Ctrl Pts',(-0.678522372573754,1.17523522336992,
1.85416363545597));
#421150=CARTESIAN_POINT('Ctrl Pts',(-1.01778355886063,0.587617611684963,
1.89583030212264));
#421151=CARTESIAN_POINT('Ctrl Pts',(-1.35704474514751,2.62370785959794E-15,
1.9374969687893));
#421152=CARTESIAN_POINT('Ctrl Pts',(-1.01778355886063,-0.587617611684958,
1.97916363545597));
#421153=CARTESIAN_POINT('Ctrl Pts',(-0.678522372573755,-1.17523522336992,
2.02083030212264));
#421154=CARTESIAN_POINT('Ctrl Pts',(-1.4392480545452E-16,-1.17523522336992,
2.06249696878931));
#421155=CARTESIAN_POINT('Ctrl Pts',(0.678522372573754,-1.17523522336992,
2.10416363545597));
#421156=CARTESIAN_POINT('Ctrl Pts',(1.01778355886063,-0.587617611684959,
2.14583030212264));
#421157=CARTESIAN_POINT('Ctrl Pts',(1.35704474514751,2.29132775890901E-15,
2.18749696878931));
#421158=CARTESIAN_POINT('Ctrl Pts',(1.01778355886063,0.587617611684963,
2.22916363545597));
#421159=CARTESIAN_POINT('Ctrl Pts',(0.678522372573755,1.17523522336992,
2.27083030212264));
#421160=CARTESIAN_POINT('Ctrl Pts',(0.,1.17523522336992,2.31249696878931));
#421161=CARTESIAN_POINT('Ctrl Pts',(-0.678522372573754,1.17523522336992,
2.35416363545597));
#421162=CARTESIAN_POINT('Ctrl Pts',(-1.01778355886063,0.587617611684963,
2.39583030212264));
#421163=CARTESIAN_POINT('Ctrl Pts',(-1.35704474514751,2.62370785959794E-15,
2.43749696878931));
#421164=CARTESIAN_POINT('Ctrl Pts',(-1.01778355886063,-0.587617611684958,
2.47916363545597));
#421165=CARTESIAN_POINT('Ctrl Pts',(-0.678522372573755,-1.17523522336992,
2.52083030212264));
#421166=CARTESIAN_POINT('Ctrl Pts',(-1.4392480545452E-16,-1.17523522336992,
2.56249696878931));
#421167=CARTESIAN_POINT('Ctrl Pts',(0.678522372573754,-1.17523522336992,
2.60416363545597));
#421168=CARTESIAN_POINT('Ctrl Pts',(1.01778355886063,-0.587617611684959,
2.64583030212264));
#421169=CARTESIAN_POINT('Ctrl Pts',(1.35704474514751,2.29132775890901E-15,
2.68749696878931));
#421170=CARTESIAN_POINT('Ctrl Pts',(1.01778355886063,0.587617611684963,
2.72916363545597));
#421171=CARTESIAN_POINT('Ctrl Pts',(0.678522372573755,1.17523522336992,
2.77083030212264));
#421172=CARTESIAN_POINT('Ctrl Pts',(0.,1.17523522336992,2.8124969687893));
#421173=CARTESIAN_POINT('Ctrl Pts',(-0.678522372573754,1.17523522336992,
2.85416363545597));
#421174=CARTESIAN_POINT('Ctrl Pts',(-1.01778355886063,0.587617611684963,
2.89583030212264));
#421175=CARTESIAN_POINT('Ctrl Pts',(-1.35704474514751,2.62370785959794E-15,
2.9374969687893));
#421176=CARTESIAN_POINT('Ctrl Pts',(-1.01778355886063,-0.587617611684958,
2.97916363545597));
#421177=CARTESIAN_POINT('Ctrl Pts',(-0.678522372573755,-1.17523522336992,
3.02083030212264));
#421178=CARTESIAN_POINT('Ctrl Pts',(-1.4392480545452E-16,-1.17523522336992,
3.0624969687893));
#421179=CARTESIAN_POINT('Ctrl Pts',(0.678522372573754,-1.17523522336992,
3.10416363545597));
#421180=CARTESIAN_POINT('Ctrl Pts',(1.01778355886063,-0.587617611684959,
3.14583030212264));
#421181=CARTESIAN_POINT('Ctrl Pts',(1.35704474514751,2.29132775890901E-15,
3.1874969687893));
#421182=CARTESIAN_POINT('Ctrl Pts',(1.01778355886063,0.587617611684963,
3.22916363545597));
#421183=CARTESIAN_POINT('Ctrl Pts',(0.678522372573755,1.17523522336992,
3.27083030212264));
#421184=CARTESIAN_POINT('Ctrl Pts',(0.,1.17523522336992,3.3124969687893));
#421185=CARTESIAN_POINT('Ctrl Pts',(-0.678522372573754,1.17523522336992,
3.35416363545597));
#421186=CARTESIAN_POINT('Ctrl Pts',(-1.01778355886063,0.587617611684963,
3.39583030212264));
#421187=CARTESIAN_POINT('Ctrl Pts',(-1.35704474514751,2.62370785959794E-15,
3.4374969687893));
#421188=CARTESIAN_POINT('Ctrl Pts',(-1.01778355886063,-0.587617611684958,
3.47916363545597));
#421189=CARTESIAN_POINT('Ctrl Pts',(-0.678522372573755,-1.17523522336992,
3.52083030212264));
#421190=CARTESIAN_POINT('Ctrl Pts',(-1.4392480545452E-16,-1.17523522336992,
3.5624969687893));
#421191=CARTESIAN_POINT('Ctrl Pts',(0.678522372573754,-1.17523522336992,
3.60416363545597));
#421192=CARTESIAN_POINT('Ctrl Pts',(1.01778355886063,-0.587617611684959,
3.64583030212264));
#421193=CARTESIAN_POINT('Ctrl Pts',(1.35704474514751,2.29132775890901E-15,
3.6874969687893));
#421194=CARTESIAN_POINT('Ctrl Pts',(1.01778355886063,0.587617611684963,
3.72916363545597));
#421195=CARTESIAN_POINT('Ctrl Pts',(0.678522372573755,1.17523522336992,
3.77083030212264));
#421196=CARTESIAN_POINT('Ctrl Pts',(0.,1.17523522336992,3.8124969687893));
#421197=CARTESIAN_POINT('Ctrl Pts',(-0.678522372573754,1.17523522336992,
3.85416363545597));
#421198=CARTESIAN_POINT('Ctrl Pts',(-1.01778355886063,0.587617611684963,
3.89583030212264));
#421199=CARTESIAN_POINT('Ctrl Pts',(-1.35704474514751,2.62370785959794E-15,
3.9374969687893));
#421200=CARTESIAN_POINT('Ctrl Pts',(-1.01778355886063,-0.587617611684958,
3.97916363545597));
#421201=CARTESIAN_POINT('Ctrl Pts',(-0.678522372573755,-1.17523522336992,
4.02083030212264));
#421202=CARTESIAN_POINT('Ctrl Pts',(-1.4392480545452E-16,-1.17523522336992,
4.0624969687893));
#421203=CARTESIAN_POINT('Ctrl Pts',(0.678522372573754,-1.17523522336992,
4.10416363545597));
#421204=CARTESIAN_POINT('Ctrl Pts',(1.01778355886063,-0.587617611684959,
4.14583030212264));
#421205=CARTESIAN_POINT('Ctrl Pts',(1.35704474514751,2.29132775890901E-15,
4.1874969687893));
#421206=CARTESIAN_POINT('Ctrl Pts',(1.01778355886063,0.587617611684963,
4.22916363545597));
#421207=CARTESIAN_POINT('Ctrl Pts',(0.678522372573755,1.17523522336992,
4.27083030212264));
#421208=CARTESIAN_POINT('Ctrl Pts',(0.,1.17523522336992,4.3124969687893));
#421209=CARTESIAN_POINT('Ctrl Pts',(-0.678522372573754,1.17523522336992,
4.35416363545597));
#421210=CARTESIAN_POINT('Ctrl Pts',(-1.01778355886063,0.587617611684963,
4.39583030212264));
#421211=CARTESIAN_POINT('Ctrl Pts',(-1.35704474514751,2.62370785959794E-15,
4.4374969687893));
#421212=CARTESIAN_POINT('Ctrl Pts',(-1.01778355886063,-0.587617611684958,
4.47916363545597));
#421213=CARTESIAN_POINT('Ctrl Pts',(-0.678522372573755,-1.17523522336992,
4.52083030212264));
#421214=CARTESIAN_POINT('Ctrl Pts',(-1.4392480545452E-16,-1.17523522336992,
4.5624969687893));
#421215=CARTESIAN_POINT('Ctrl Pts',(0.678522372573754,-1.17523522336992,
4.60416363545597));
#421216=CARTESIAN_POINT('Ctrl Pts',(1.01778355886063,-0.587617611684959,
4.64583030212264));
#421217=CARTESIAN_POINT('Ctrl Pts',(1.35704474514751,2.29132775890901E-15,
4.6874969687893));
#421218=CARTESIAN_POINT('Ctrl Pts',(1.01778355886063,0.587617611684963,
4.72916363545597));
#421219=CARTESIAN_POINT('Ctrl Pts',(0.678522372573755,1.17523522336992,
4.77083030212264));
#421220=CARTESIAN_POINT('Ctrl Pts',(0.,1.17523522336992,4.8124969687893));
#421221=CARTESIAN_POINT('Ctrl Pts',(-0.678522372573754,1.17523522336992,
4.85416363545597));
#421222=CARTESIAN_POINT('Ctrl Pts',(-1.01778355886063,0.587617611684963,
4.89583030212264));
#421223=CARTESIAN_POINT('Ctrl Pts',(-1.35704474514751,2.62370785959794E-15,
4.9374969687893));
#421224=CARTESIAN_POINT('Ctrl Pts',(-1.01778355886063,-0.587617611684958,
4.97916363545597));
#421225=CARTESIAN_POINT('Ctrl Pts',(-0.678522372573755,-1.17523522336992,
5.02083030212264));
#421226=CARTESIAN_POINT('Ctrl Pts',(-1.4392480545452E-16,-1.17523522336992,
5.06249696878931));
#421227=CARTESIAN_POINT('Ctrl Pts',(0.678522372573754,-1.17523522336992,
5.10416363545597));
#421228=CARTESIAN_POINT('Ctrl Pts',(1.01778355886063,-0.587617611684959,
5.14583030212264));
#421229=CARTESIAN_POINT('Ctrl Pts',(1.35704474514751,2.29132775890901E-15,
5.1874969687893));
#421230=CARTESIAN_POINT('Ctrl Pts',(1.01778355886063,0.587617611684963,
5.22916363545597));
#421231=CARTESIAN_POINT('Ctrl Pts',(0.678522372573755,1.17523522336992,
5.27083030212264));
#421232=CARTESIAN_POINT('Ctrl Pts',(0.,1.17523522336992,5.3124969687893));
#421233=CARTESIAN_POINT('Ctrl Pts',(-0.678522372573754,1.17523522336992,
5.35416363545597));
#421234=CARTESIAN_POINT('Ctrl Pts',(-1.01778355886063,0.587617611684963,
5.39583030212264));
#421235=CARTESIAN_POINT('Ctrl Pts',(-1.35704474514751,2.62370785959794E-15,
5.4374969687893));
#421236=CARTESIAN_POINT('Ctrl Pts',(-1.01778355886063,-0.587617611684958,
5.47916363545597));
#421237=CARTESIAN_POINT('Ctrl Pts',(-0.678522372573755,-1.17523522336992,
5.52083030212264));
#421238=CARTESIAN_POINT('Ctrl Pts',(-1.4392480545452E-16,-1.17523522336992,
5.5624969687893));
#421239=CARTESIAN_POINT('Ctrl Pts',(0.678522372573754,-1.17523522336992,
5.60416363545597));
#421240=CARTESIAN_POINT('Ctrl Pts',(1.01778355886063,-0.587617611684959,
5.64583030212264));
#421241=CARTESIAN_POINT('Ctrl Pts',(1.35704474514751,2.29132775890901E-15,
5.6874969687893));
#421242=CARTESIAN_POINT('Ctrl Pts',(1.01778355886063,0.587617611684963,
5.72916363545597));
#421243=CARTESIAN_POINT('Ctrl Pts',(0.678522372573755,1.17523522336992,
5.77083030212264));
#421244=CARTESIAN_POINT('Ctrl Pts',(0.,1.17523522336992,5.81249696878931));
#421245=CARTESIAN_POINT('Ctrl Pts',(-0.678522372573754,1.17523522336992,
5.85416363545597));
#421246=CARTESIAN_POINT('Ctrl Pts',(-1.01778355886063,0.587617611684963,
5.89583030212264));
#421247=CARTESIAN_POINT('Ctrl Pts',(-1.35704474514751,2.62370785959794E-15,
5.93749696878931));
#421248=CARTESIAN_POINT('Ctrl Pts',(-1.01778355886063,-0.587617611684958,
5.97916363545597));
#421249=CARTESIAN_POINT('Ctrl Pts',(-0.678522372573755,-1.17523522336992,
6.02083030212264));
#421250=CARTESIAN_POINT('Ctrl Pts',(-1.4392480545452E-16,-1.17523522336992,
6.06249696878931));
#421251=CARTESIAN_POINT('Ctrl Pts',(0.678522372573754,-1.17523522336992,
6.10416363545597));
#421252=CARTESIAN_POINT('Ctrl Pts',(1.01778355886063,-0.587617611684959,
6.14583030212264));
#421253=CARTESIAN_POINT('Ctrl Pts',(1.35704474514751,2.29132775890901E-15,
6.18749696878931));
#421254=CARTESIAN_POINT('Ctrl Pts',(1.01778355886063,0.587617611684963,
6.22916363545597));
#421255=CARTESIAN_POINT('Ctrl Pts',(0.678522372573755,1.17523522336992,
6.27083030212264));
#421256=CARTESIAN_POINT('Ctrl Pts',(0.,1.17523522336992,6.31249696878931));
#421257=CARTESIAN_POINT('Ctrl Pts',(-0.678522372573754,1.17523522336992,
6.35416363545597));
#421258=CARTESIAN_POINT('Ctrl Pts',(-1.01778355886063,0.587617611684963,
6.39583030212264));
#421259=CARTESIAN_POINT('Ctrl Pts',(-1.35704474514751,2.62370785959794E-15,
6.43749696878931));
#421260=CARTESIAN_POINT('Ctrl Pts',(-1.01778355886063,-0.587617611684958,
6.47916363545597));
#421261=CARTESIAN_POINT('Ctrl Pts',(-0.678522372573755,-1.17523522336992,
6.52083030212264));
#421262=CARTESIAN_POINT('Ctrl Pts',(-1.4392480545452E-16,-1.17523522336992,
6.5624969687893));
#421263=CARTESIAN_POINT('Ctrl Pts',(0.678522372573754,-1.17523522336992,
6.60416363545597));
#421264=CARTESIAN_POINT('Ctrl Pts',(1.01778355886063,-0.587617611684959,
6.64583030212264));
#421265=CARTESIAN_POINT('Ctrl Pts',(1.35704474514751,2.29132775890901E-15,
6.6874969687893));
#421266=CARTESIAN_POINT('Ctrl Pts',(1.01778355886063,0.587617611684963,
6.72916363545597));
#421267=CARTESIAN_POINT('Ctrl Pts',(0.678522372573755,1.17523522336992,
6.77083030212264));
#421268=CARTESIAN_POINT('Ctrl Pts',(0.,1.17523522336992,6.8124969687893));
#421269=CARTESIAN_POINT('Ctrl Pts',(-0.678522372573754,1.17523522336992,
6.85416363545597));
#421270=CARTESIAN_POINT('Ctrl Pts',(-1.01778355886063,0.587617611684963,
6.89583030212264));
#421271=CARTESIAN_POINT('Ctrl Pts',(-1.35704474514751,2.62370785959794E-15,
6.9374969687893));
#421272=CARTESIAN_POINT('Ctrl Pts',(-1.01778355886063,-0.587617611684958,
6.97916363545597));
#421273=CARTESIAN_POINT('Ctrl Pts',(-0.678522372573755,-1.17523522336992,
7.02083030212264));
#421274=CARTESIAN_POINT('Ctrl Pts',(-1.4392480545452E-16,-1.17523522336992,
7.0624969687893));
#421275=CARTESIAN_POINT('Ctrl Pts',(0.678522372573754,-1.17523522336992,
7.10416363545597));
#421276=CARTESIAN_POINT('Ctrl Pts',(1.01778355886063,-0.587617611684959,
7.14583030212264));
#421277=CARTESIAN_POINT('Ctrl Pts',(1.35704474514751,2.29132775890901E-15,
7.1874969687893));
#421278=CARTESIAN_POINT('Ctrl Pts',(1.01778355886063,0.587617611684963,
7.22916363545597));
#421279=CARTESIAN_POINT('Ctrl Pts',(0.678522372573755,1.17523522336992,
7.27083030212264));
#421280=CARTESIAN_POINT('Ctrl Pts',(0.,1.17523522336992,7.3124969687893));
#421281=CARTESIAN_POINT('Ctrl Pts',(-0.678522372573754,1.17523522336992,
7.35416363545597));
#421282=CARTESIAN_POINT('Ctrl Pts',(-1.01778355886063,0.587617611684963,
7.39583030212264));
#421283=CARTESIAN_POINT('Ctrl Pts',(-1.35704474514751,2.62370785959794E-15,
7.4374969687893));
#421284=CARTESIAN_POINT('Ctrl Pts',(-1.01778355886063,-0.587617611684958,
7.47916363545597));
#421285=CARTESIAN_POINT('Ctrl Pts',(-0.678522372573755,-1.17523522336992,
7.52083030212264));
#421286=CARTESIAN_POINT('Ctrl Pts',(-1.4392480545452E-16,-1.17523522336992,
7.5624969687893));
#421287=CARTESIAN_POINT('Ctrl Pts',(0.678522372573754,-1.17523522336992,
7.60416363545597));
#421288=CARTESIAN_POINT('Ctrl Pts',(1.01778355886063,-0.587617611684959,
7.64583030212264));
#421289=CARTESIAN_POINT('Ctrl Pts',(1.35704474514751,2.29132775890901E-15,
7.6874969687893));
#421290=CARTESIAN_POINT('Ctrl Pts',(1.01778355886063,0.587617611684963,
7.72916363545597));
#421291=CARTESIAN_POINT('Ctrl Pts',(0.678522372573755,1.17523522336992,
7.77083030212264));
#421292=CARTESIAN_POINT('Ctrl Pts',(0.,1.17523522336992,7.8124969687893));
#421293=CARTESIAN_POINT('Ctrl Pts',(-0.678522372573754,1.17523522336992,
7.85416363545597));
#421294=CARTESIAN_POINT('Ctrl Pts',(-1.01778355886063,0.587617611684963,
7.89583030212264));
#421295=CARTESIAN_POINT('Ctrl Pts',(-1.35704474514751,2.62370785959794E-15,
7.93749696878931));
#421296=CARTESIAN_POINT('Ctrl Pts',(-1.01778355886063,-0.587617611684958,
7.97916363545597));
#421297=CARTESIAN_POINT('Ctrl Pts',(-0.678522372573755,-1.17523522336992,
8.02083030212264));
#421298=CARTESIAN_POINT('Ctrl Pts',(-1.4392480545452E-16,-1.17523522336992,
8.0624969687893));
#421299=CARTESIAN_POINT('Ctrl Pts',(0.678522372573754,-1.17523522336992,
8.10416363545597));
#421300=CARTESIAN_POINT('Ctrl Pts',(1.01778355886063,-0.587617611684959,
8.14583030212264));
#421301=CARTESIAN_POINT('Ctrl Pts',(1.35704474514751,2.29132775890901E-15,
8.1874969687893));
#421302=CARTESIAN_POINT('Ctrl Pts',(1.01778355886063,0.587617611684963,
8.22916363545597));
#421303=CARTESIAN_POINT('Ctrl Pts',(0.678522372573755,1.17523522336992,
8.27083030212264));
#421304=CARTESIAN_POINT('Ctrl Pts',(0.,1.17523522336992,8.3124969687893));
#421305=CARTESIAN_POINT('Ctrl Pts',(-0.678522372573754,1.17523522336992,
8.35416363545597));
#421306=CARTESIAN_POINT('Ctrl Pts',(-1.01778355886063,0.587617611684963,
8.39583030212264));
#421307=CARTESIAN_POINT('Ctrl Pts',(-1.35704474514751,2.62370785959794E-15,
8.4374969687893));
#421308=CARTESIAN_POINT('Ctrl Pts',(-1.01778355886063,-0.587617611684958,
8.47916363545597));
#421309=CARTESIAN_POINT('Ctrl Pts',(-0.678522372573755,-1.17523522336992,
8.52083030212264));
#421310=CARTESIAN_POINT('Ctrl Pts',(-1.4392480545452E-16,-1.17523522336992,
8.5624969687893));
#421311=CARTESIAN_POINT('Ctrl Pts',(0.678522372573754,-1.17523522336992,
8.60416363545597));
#421312=CARTESIAN_POINT('Ctrl Pts',(1.01778355886063,-0.587617611684959,
8.64583030212264));
#421313=CARTESIAN_POINT('Ctrl Pts',(1.35704474514751,2.29132775890901E-15,
8.6874969687893));
#421314=CARTESIAN_POINT('Ctrl Pts',(1.01778355886063,0.587617611684963,
8.72916363545597));
#421315=CARTESIAN_POINT('Ctrl Pts',(0.678522372573755,1.17523522336992,
8.77083030212264));
#421316=CARTESIAN_POINT('Ctrl Pts',(0.,1.17523522336992,8.8124969687893));
#421317=CARTESIAN_POINT('Ctrl Pts',(-0.678522372573754,1.17523522336992,
8.85416363545597));
#421318=CARTESIAN_POINT('Ctrl Pts',(-1.01778355886063,0.587617611684963,
8.89583030212264));
#421319=CARTESIAN_POINT('Ctrl Pts',(-1.35704474514751,2.62370785959794E-15,
8.9374969687893));
#421320=CARTESIAN_POINT('Ctrl Pts',(-1.01778355886063,-0.587617611684958,
8.97916363545597));
#421321=CARTESIAN_POINT('Ctrl Pts',(-0.678522372573755,-1.17523522336992,
9.02083030212264));
#421322=CARTESIAN_POINT('Ctrl Pts',(-1.4392480545452E-16,-1.17523522336992,
9.06249696878931));
#421323=CARTESIAN_POINT('Ctrl Pts',(0.678522372573754,-1.17523522336992,
9.10416363545597));
#421324=CARTESIAN_POINT('Ctrl Pts',(1.01778355886063,-0.587617611684959,
9.14583030212264));
#421325=CARTESIAN_POINT('Ctrl Pts',(1.35704474514751,2.29132775890901E-15,
9.1874969687893));
#421326=CARTESIAN_POINT('Ctrl Pts',(1.01778355886063,0.587617611684963,
9.22916363545597));
#421327=CARTESIAN_POINT('Ctrl Pts',(0.678522372573755,1.17523522336992,
9.27083030212264));
#421328=CARTESIAN_POINT('Ctrl Pts',(0.,1.17523522336992,9.31249696878931));
#421329=CARTESIAN_POINT('Ctrl Pts',(-0.678522372573754,1.17523522336992,
9.35416363545597));
#421330=CARTESIAN_POINT('Ctrl Pts',(-1.01778355886063,0.587617611684963,
9.39583030212263));
#421331=CARTESIAN_POINT('Ctrl Pts',(-1.35704474514751,2.62370785959794E-15,
9.4374969687893));
#421332=CARTESIAN_POINT('Ctrl Pts',(-1.01778355886063,-0.587617611684958,
9.47916363545597));
#421333=CARTESIAN_POINT('Ctrl Pts',(-0.678522372573755,-1.17523522336992,
9.52083030212264));
#421334=CARTESIAN_POINT('Ctrl Pts',(-1.4392480545452E-16,-1.17523522336992,
9.56249696878931));
#421335=CARTESIAN_POINT('Ctrl Pts',(0.678522372573754,-1.17523522336992,
9.60416363545597));
#421336=CARTESIAN_POINT('Ctrl Pts',(1.01778355886063,-0.587617611684959,
9.64583030212264));
#421337=CARTESIAN_POINT('Ctrl Pts',(1.35704474514751,2.29132775890901E-15,
9.6874969687893));
#421338=CARTESIAN_POINT('Ctrl Pts',(1.01778355886063,0.587617611684963,
9.72916363545597));
#421339=CARTESIAN_POINT('Ctrl Pts',(0.678522372573755,1.17523522336992,
9.77083030212264));
#421340=CARTESIAN_POINT('Ctrl Pts',(0.,1.17523522336992,9.8124969687893));
#421341=CARTESIAN_POINT('Ctrl Pts',(-0.678522372573754,1.17523522336992,
9.85416363545597));
#421342=CARTESIAN_POINT('Ctrl Pts',(-1.01778355886063,0.587617611684963,
9.89583030212264));
#421343=CARTESIAN_POINT('Ctrl Pts',(-1.35704474514751,2.62370785959794E-15,
9.93749696878931));
#421344=CARTESIAN_POINT('Ctrl Pts',(-1.01778355886063,-0.587617611684958,
9.97916363545597));
#421345=CARTESIAN_POINT('Ctrl Pts',(-0.678522372573755,-1.17523522336992,
10.0208303021226));
#421346=CARTESIAN_POINT('Ctrl Pts',(-1.4392480545452E-16,-1.17523522336992,
10.0624969687893));
#421347=CARTESIAN_POINT('Ctrl Pts',(0.678522372573754,-1.17523522336992,
10.104163635456));
#421348=CARTESIAN_POINT('Ctrl Pts',(1.01778355886063,-0.587617611684959,
10.1458303021226));
#421349=CARTESIAN_POINT('Ctrl Pts',(1.35704474514751,2.29132775890901E-15,
10.1874969687893));
#421350=CARTESIAN_POINT('Ctrl Pts',(1.01778355886063,0.587617611684963,
10.229163635456));
#421351=CARTESIAN_POINT('Ctrl Pts',(0.678522372573755,1.17523522336992,
10.2708303021226));
#421352=CARTESIAN_POINT('Ctrl Pts',(0.,1.17523522336992,10.3124969687893));
#421353=CARTESIAN_POINT('Ctrl Pts',(-0.678522372573754,1.17523522336992,
10.354163635456));
#421354=CARTESIAN_POINT('Ctrl Pts',(-1.01778355886063,0.587617611684963,
10.3958303021226));
#421355=CARTESIAN_POINT('Ctrl Pts',(-1.35704474514751,2.62370785959794E-15,
10.4374969687893));
#421356=CARTESIAN_POINT('Ctrl Pts',(-1.01778355886063,-0.587617611684958,
10.479163635456));
#421357=CARTESIAN_POINT('Ctrl Pts',(-0.678522372573755,-1.17523522336992,
10.5208303021226));
#421358=CARTESIAN_POINT('Ctrl Pts',(-1.4392480545452E-16,-1.17523522336992,
10.5624969687893));
#421359=CARTESIAN_POINT('Ctrl Pts',(0.678522372573754,-1.17523522336992,
10.604163635456));
#421360=CARTESIAN_POINT('Ctrl Pts',(1.01778355886063,-0.587617611684959,
10.6458303021226));
#421361=CARTESIAN_POINT('Ctrl Pts',(1.35704474514751,2.29132775890901E-15,
10.6874969687893));
#421362=CARTESIAN_POINT('Ctrl Pts',(1.01778355886063,0.587617611684963,
10.729163635456));
#421363=CARTESIAN_POINT('Ctrl Pts',(0.678522372573755,1.17523522336992,
10.7708303021226));
#421364=CARTESIAN_POINT('Ctrl Pts',(0.,1.17523522336992,10.8124969687893));
#421365=CARTESIAN_POINT('Ctrl Pts',(-0.678522372573754,1.17523522336992,
10.854163635456));
#421366=CARTESIAN_POINT('Ctrl Pts',(-1.01778355886063,0.587617611684963,
10.8958303021226));
#421367=CARTESIAN_POINT('Ctrl Pts',(-1.35704474514751,2.62370785959794E-15,
10.9374969687893));
#421368=CARTESIAN_POINT('Ctrl Pts',(-1.01778355886063,-0.587617611684958,
10.979163635456));
#421369=CARTESIAN_POINT('Ctrl Pts',(-0.678522372573755,-1.17523522336992,
11.0208303021226));
#421370=CARTESIAN_POINT('Ctrl Pts',(-1.4392480545452E-16,-1.17523522336992,
11.0624969687893));
#421371=CARTESIAN_POINT('Ctrl Pts',(0.678522372573754,-1.17523522336992,
11.104163635456));
#421372=CARTESIAN_POINT('Ctrl Pts',(1.01778355886063,-0.587617611684959,
11.1458303021226));
#421373=CARTESIAN_POINT('Ctrl Pts',(1.35704474514751,2.29132775890901E-15,
11.1874969687893));
#421374=CARTESIAN_POINT('Ctrl Pts',(1.01778355886063,0.587617611684963,
11.229163635456));
#421375=CARTESIAN_POINT('Ctrl Pts',(0.678522372573755,1.17523522336992,
11.2708303021226));
#421376=CARTESIAN_POINT('Ctrl Pts',(0.,1.17523522336992,11.3124969687893));
#421377=CARTESIAN_POINT('Ctrl Pts',(-1.43925448419923E-16,-1.17524047358087,
3.56250000000001));
#421378=CARTESIAN_POINT('Ctrl Pts',(0.678525403784459,-1.17524047358087,
3.60416666666668));
#421379=CARTESIAN_POINT('Ctrl Pts',(1.01778810567669,-0.587620236790434,
3.64583333333334));
#421380=CARTESIAN_POINT('Ctrl Pts',(1.12956523348512,-0.394016572302108,
3.65956128014086));
#421381=CARTESIAN_POINT('Ctrl Pts',(1.16245326511943,-0.172894699617312,
3.67524047358081));
#421382=CARTESIAN_POINT('Origin',(0.,-1.11022302462516E-14,-14.21875));
#421383=CARTESIAN_POINT('Ctrl Pts',(-1.43925448419923E-16,-1.17524047358087,
3.50000000000001));
#421384=CARTESIAN_POINT('Ctrl Pts',(0.678525403784459,-1.17524047358087,
3.54166666666668));
#421385=CARTESIAN_POINT('Ctrl Pts',(1.01778810567669,-0.587620236790434,
3.58333333333334));
#421386=CARTESIAN_POINT('Ctrl Pts',(1.35705080756892,2.29132664526027E-15,
3.62500000000001));
#421387=CARTESIAN_POINT('Ctrl Pts',(1.01778810567669,0.587620236790438,
3.66666666666668));
#421388=CARTESIAN_POINT('Ctrl Pts',(0.98389535208559,0.646324208018635,
3.67082921698069));
#421389=CARTESIAN_POINT('Ctrl Pts',(0.943477955796025,0.700742119234707,
3.6752404735808));
#421390=CARTESIAN_POINT('Ctrl Pts',(0.,1.17524047358087,-14.25));
#421391=CARTESIAN_POINT('Ctrl Pts',(-0.678525403784459,1.17524047358087,
-14.2083333333333));
#421392=CARTESIAN_POINT('Ctrl Pts',(-1.01778810567669,0.587620236790438,
-14.1666666666667));
#421393=CARTESIAN_POINT('Ctrl Pts',(-1.35705080756892,2.62370823081419E-15,
-14.125));
#421394=CARTESIAN_POINT('Ctrl Pts',(-1.01778810567669,-0.587620236790433,
-14.0833333333333));
#421395=CARTESIAN_POINT('Ctrl Pts',(-0.67852540378446,-1.17524047358087,
-14.0416666666667));
#421396=CARTESIAN_POINT('Ctrl Pts',(-1.43925448419923E-16,-1.17524047358087,
-14.));
#421397=CARTESIAN_POINT('Ctrl Pts',(0.678525403784459,-1.17524047358087,
-13.9583333333333));
#421398=CARTESIAN_POINT('Ctrl Pts',(1.01778810567669,-0.587620236790434,
-13.9166666666667));
#421399=CARTESIAN_POINT('Ctrl Pts',(1.35705080756892,2.29132664526027E-15,
-13.875));
#421400=CARTESIAN_POINT('Ctrl Pts',(1.01778810567669,0.587620236790438,
-13.8333333333333));
#421401=CARTESIAN_POINT('Ctrl Pts',(0.67852540378446,1.17524047358087,-13.7916666666667));
#421402=CARTESIAN_POINT('Ctrl Pts',(0.,1.17524047358087,-13.75));
#421403=CARTESIAN_POINT('Ctrl Pts',(-0.678525403784459,1.17524047358087,
-13.7083333333333));
#421404=CARTESIAN_POINT('Ctrl Pts',(-1.01778810567669,0.587620236790438,
-13.6666666666667));
#421405=CARTESIAN_POINT('Ctrl Pts',(-1.35705080756892,2.62370823081419E-15,
-13.625));
#421406=CARTESIAN_POINT('Ctrl Pts',(-1.01778810567669,-0.587620236790433,
-13.5833333333333));
#421407=CARTESIAN_POINT('Ctrl Pts',(-0.67852540378446,-1.17524047358087,
-13.5416666666667));
#421408=CARTESIAN_POINT('Ctrl Pts',(-1.43925448419923E-16,-1.17524047358087,
-13.5));
#421409=CARTESIAN_POINT('Ctrl Pts',(0.678525403784459,-1.17524047358087,
-13.4583333333333));
#421410=CARTESIAN_POINT('Ctrl Pts',(1.01778810567669,-0.587620236790434,
-13.4166666666667));
#421411=CARTESIAN_POINT('Ctrl Pts',(1.35705080756892,2.29132664526027E-15,
-13.375));
#421412=CARTESIAN_POINT('Ctrl Pts',(1.01778810567669,0.587620236790438,
-13.3333333333333));
#421413=CARTESIAN_POINT('Ctrl Pts',(0.67852540378446,1.17524047358087,-13.2916666666667));
#421414=CARTESIAN_POINT('Ctrl Pts',(0.,1.17524047358087,-13.25));
#421415=CARTESIAN_POINT('Ctrl Pts',(-0.678525403784459,1.17524047358087,
-13.2083333333333));
#421416=CARTESIAN_POINT('Ctrl Pts',(-1.01778810567669,0.587620236790438,
-13.1666666666667));
#421417=CARTESIAN_POINT('Ctrl Pts',(-1.35705080756892,2.62370823081419E-15,
-13.125));
#421418=CARTESIAN_POINT('Ctrl Pts',(-1.01778810567669,-0.587620236790433,
-13.0833333333333));
#421419=CARTESIAN_POINT('Ctrl Pts',(-0.67852540378446,-1.17524047358087,
-13.0416666666667));
#421420=CARTESIAN_POINT('Ctrl Pts',(-1.43925448419923E-16,-1.17524047358087,
-13.));
#421421=CARTESIAN_POINT('Ctrl Pts',(0.678525403784459,-1.17524047358087,
-12.9583333333333));
#421422=CARTESIAN_POINT('Ctrl Pts',(1.01778810567669,-0.587620236790434,
-12.9166666666667));
#421423=CARTESIAN_POINT('Ctrl Pts',(1.35705080756892,2.29132664526027E-15,
-12.875));
#421424=CARTESIAN_POINT('Ctrl Pts',(1.01778810567669,0.587620236790438,
-12.8333333333333));
#421425=CARTESIAN_POINT('Ctrl Pts',(0.67852540378446,1.17524047358087,-12.7916666666667));
#421426=CARTESIAN_POINT('Ctrl Pts',(0.,1.17524047358087,-12.75));
#421427=CARTESIAN_POINT('Ctrl Pts',(-0.678525403784459,1.17524047358087,
-12.7083333333333));
#421428=CARTESIAN_POINT('Ctrl Pts',(-1.01778810567669,0.587620236790438,
-12.6666666666667));
#421429=CARTESIAN_POINT('Ctrl Pts',(-1.35705080756892,2.62370823081419E-15,
-12.625));
#421430=CARTESIAN_POINT('Ctrl Pts',(-1.01778810567669,-0.587620236790433,
-12.5833333333333));
#421431=CARTESIAN_POINT('Ctrl Pts',(-0.67852540378446,-1.17524047358087,
-12.5416666666667));
#421432=CARTESIAN_POINT('Ctrl Pts',(-1.43925448419923E-16,-1.17524047358087,
-12.5));
#421433=CARTESIAN_POINT('Ctrl Pts',(0.678525403784459,-1.17524047358087,
-12.4583333333333));
#421434=CARTESIAN_POINT('Ctrl Pts',(1.01778810567669,-0.587620236790434,
-12.4166666666667));
#421435=CARTESIAN_POINT('Ctrl Pts',(1.35705080756892,2.29132664526027E-15,
-12.375));
#421436=CARTESIAN_POINT('Ctrl Pts',(1.01778810567669,0.587620236790438,
-12.3333333333333));
#421437=CARTESIAN_POINT('Ctrl Pts',(0.67852540378446,1.17524047358087,-12.2916666666667));
#421438=CARTESIAN_POINT('Ctrl Pts',(0.,1.17524047358087,-12.25));
#421439=CARTESIAN_POINT('Ctrl Pts',(-0.678525403784459,1.17524047358087,
-12.2083333333333));
#421440=CARTESIAN_POINT('Ctrl Pts',(-1.01778810567669,0.587620236790438,
-12.1666666666667));
#421441=CARTESIAN_POINT('Ctrl Pts',(-1.35705080756892,2.62370823081419E-15,
-12.125));
#421442=CARTESIAN_POINT('Ctrl Pts',(-1.01778810567669,-0.587620236790433,
-12.0833333333333));
#421443=CARTESIAN_POINT('Ctrl Pts',(-0.67852540378446,-1.17524047358087,
-12.0416666666667));
#421444=CARTESIAN_POINT('Ctrl Pts',(-1.43925448419923E-16,-1.17524047358087,
-12.));
#421445=CARTESIAN_POINT('Ctrl Pts',(0.678525403784459,-1.17524047358087,
-11.9583333333333));
#421446=CARTESIAN_POINT('Ctrl Pts',(1.01778810567669,-0.587620236790434,
-11.9166666666667));
#421447=CARTESIAN_POINT('Ctrl Pts',(1.35705080756892,2.29132664526027E-15,
-11.875));
#421448=CARTESIAN_POINT('Ctrl Pts',(1.01778810567669,0.587620236790438,
-11.8333333333333));
#421449=CARTESIAN_POINT('Ctrl Pts',(0.67852540378446,1.17524047358087,-11.7916666666667));
#421450=CARTESIAN_POINT('Ctrl Pts',(0.,1.17524047358087,-11.75));
#421451=CARTESIAN_POINT('Ctrl Pts',(-0.678525403784459,1.17524047358087,
-11.7083333333333));
#421452=CARTESIAN_POINT('Ctrl Pts',(-1.01778810567669,0.587620236790438,
-11.6666666666667));
#421453=CARTESIAN_POINT('Ctrl Pts',(-1.35705080756892,2.62370823081419E-15,
-11.625));
#421454=CARTESIAN_POINT('Ctrl Pts',(-1.01778810567669,-0.587620236790433,
-11.5833333333333));
#421455=CARTESIAN_POINT('Ctrl Pts',(-0.67852540378446,-1.17524047358087,
-11.5416666666667));
#421456=CARTESIAN_POINT('Ctrl Pts',(-1.43925448419923E-16,-1.17524047358087,
-11.5));
#421457=CARTESIAN_POINT('Ctrl Pts',(0.678525403784459,-1.17524047358087,
-11.4583333333333));
#421458=CARTESIAN_POINT('Ctrl Pts',(1.01778810567669,-0.587620236790434,
-11.4166666666667));
#421459=CARTESIAN_POINT('Ctrl Pts',(1.35705080756892,2.29132664526027E-15,
-11.375));
#421460=CARTESIAN_POINT('Ctrl Pts',(1.01778810567669,0.587620236790438,
-11.3333333333333));
#421461=CARTESIAN_POINT('Ctrl Pts',(0.67852540378446,1.17524047358087,-11.2916666666667));
#421462=CARTESIAN_POINT('Ctrl Pts',(0.,1.17524047358087,-11.25));
#421463=CARTESIAN_POINT('Ctrl Pts',(-0.678525403784459,1.17524047358087,
-11.2083333333333));
#421464=CARTESIAN_POINT('Ctrl Pts',(-1.01778810567669,0.587620236790438,
-11.1666666666667));
#421465=CARTESIAN_POINT('Ctrl Pts',(-1.35705080756892,2.62370823081419E-15,
-11.125));
#421466=CARTESIAN_POINT('Ctrl Pts',(-1.01778810567669,-0.587620236790433,
-11.0833333333333));
#421467=CARTESIAN_POINT('Ctrl Pts',(-0.67852540378446,-1.17524047358087,
-11.0416666666667));
#421468=CARTESIAN_POINT('Ctrl Pts',(-1.43925448419923E-16,-1.17524047358087,
-11.));
#421469=CARTESIAN_POINT('Ctrl Pts',(0.678525403784459,-1.17524047358087,
-10.9583333333333));
#421470=CARTESIAN_POINT('Ctrl Pts',(1.01778810567669,-0.587620236790434,
-10.9166666666667));
#421471=CARTESIAN_POINT('Ctrl Pts',(1.35705080756892,2.29132664526027E-15,
-10.875));
#421472=CARTESIAN_POINT('Ctrl Pts',(1.01778810567669,0.587620236790438,
-10.8333333333333));
#421473=CARTESIAN_POINT('Ctrl Pts',(0.67852540378446,1.17524047358087,-10.7916666666667));
#421474=CARTESIAN_POINT('Ctrl Pts',(0.,1.17524047358087,-10.75));
#421475=CARTESIAN_POINT('Ctrl Pts',(-0.678525403784459,1.17524047358087,
-10.7083333333333));
#421476=CARTESIAN_POINT('Ctrl Pts',(-1.01778810567669,0.587620236790438,
-10.6666666666667));
#421477=CARTESIAN_POINT('Ctrl Pts',(-1.35705080756892,2.62370823081419E-15,
-10.625));
#421478=CARTESIAN_POINT('Ctrl Pts',(-1.01778810567669,-0.587620236790433,
-10.5833333333333));
#421479=CARTESIAN_POINT('Ctrl Pts',(-0.67852540378446,-1.17524047358087,
-10.5416666666667));
#421480=CARTESIAN_POINT('Ctrl Pts',(-1.43925448419923E-16,-1.17524047358087,
-10.5));
#421481=CARTESIAN_POINT('Ctrl Pts',(0.678525403784459,-1.17524047358087,
-10.4583333333333));
#421482=CARTESIAN_POINT('Ctrl Pts',(1.01778810567669,-0.587620236790434,
-10.4166666666667));
#421483=CARTESIAN_POINT('Ctrl Pts',(1.35705080756892,2.29132664526027E-15,
-10.375));
#421484=CARTESIAN_POINT('Ctrl Pts',(1.01778810567669,0.587620236790438,
-10.3333333333333));
#421485=CARTESIAN_POINT('Ctrl Pts',(0.67852540378446,1.17524047358087,-10.2916666666667));
#421486=CARTESIAN_POINT('Ctrl Pts',(0.,1.17524047358087,-10.25));
#421487=CARTESIAN_POINT('Ctrl Pts',(-0.678525403784459,1.17524047358087,
-10.2083333333333));
#421488=CARTESIAN_POINT('Ctrl Pts',(-1.01778810567669,0.587620236790438,
-10.1666666666667));
#421489=CARTESIAN_POINT('Ctrl Pts',(-1.35705080756892,2.62370823081419E-15,
-10.125));
#421490=CARTESIAN_POINT('Ctrl Pts',(-1.01778810567669,-0.587620236790433,
-10.0833333333333));
#421491=CARTESIAN_POINT('Ctrl Pts',(-0.67852540378446,-1.17524047358087,
-10.0416666666667));
#421492=CARTESIAN_POINT('Ctrl Pts',(-1.43925448419923E-16,-1.17524047358087,
-9.99999999999999));
#421493=CARTESIAN_POINT('Ctrl Pts',(0.678525403784459,-1.17524047358087,
-9.95833333333332));
#421494=CARTESIAN_POINT('Ctrl Pts',(1.01778810567669,-0.587620236790434,
-9.91666666666666));
#421495=CARTESIAN_POINT('Ctrl Pts',(1.35705080756892,2.29132664526027E-15,
-9.87499999999999));
#421496=CARTESIAN_POINT('Ctrl Pts',(1.01778810567669,0.587620236790438,
-9.83333333333332));
#421497=CARTESIAN_POINT('Ctrl Pts',(0.67852540378446,1.17524047358087,-9.79166666666666));
#421498=CARTESIAN_POINT('Ctrl Pts',(0.,1.17524047358087,-9.74999999999999));
#421499=CARTESIAN_POINT('Ctrl Pts',(-0.678525403784459,1.17524047358087,
-9.70833333333332));
#421500=CARTESIAN_POINT('Ctrl Pts',(-1.01778810567669,0.587620236790438,
-9.66666666666666));
#421501=CARTESIAN_POINT('Ctrl Pts',(-1.35705080756892,2.62370823081419E-15,
-9.62499999999999));
#421502=CARTESIAN_POINT('Ctrl Pts',(-1.01778810567669,-0.587620236790433,
-9.58333333333332));
#421503=CARTESIAN_POINT('Ctrl Pts',(-0.67852540378446,-1.17524047358087,
-9.54166666666666));
#421504=CARTESIAN_POINT('Ctrl Pts',(-1.43925448419923E-16,-1.17524047358087,
-9.49999999999999));
#421505=CARTESIAN_POINT('Ctrl Pts',(0.678525403784459,-1.17524047358087,
-9.45833333333333));
#421506=CARTESIAN_POINT('Ctrl Pts',(1.01778810567669,-0.587620236790434,
-9.41666666666666));
#421507=CARTESIAN_POINT('Ctrl Pts',(1.35705080756892,2.29132664526027E-15,
-9.37499999999999));
#421508=CARTESIAN_POINT('Ctrl Pts',(1.01778810567669,0.587620236790438,
-9.33333333333332));
#421509=CARTESIAN_POINT('Ctrl Pts',(0.67852540378446,1.17524047358087,-9.29166666666666));
#421510=CARTESIAN_POINT('Ctrl Pts',(0.,1.17524047358087,-9.24999999999999));
#421511=CARTESIAN_POINT('Ctrl Pts',(-0.678525403784459,1.17524047358087,
-9.20833333333332));
#421512=CARTESIAN_POINT('Ctrl Pts',(-1.01778810567669,0.587620236790438,
-9.16666666666666));
#421513=CARTESIAN_POINT('Ctrl Pts',(-1.35705080756892,2.62370823081419E-15,
-9.12499999999999));
#421514=CARTESIAN_POINT('Ctrl Pts',(-1.01778810567669,-0.587620236790433,
-9.08333333333332));
#421515=CARTESIAN_POINT('Ctrl Pts',(-0.67852540378446,-1.17524047358087,
-9.04166666666666));
#421516=CARTESIAN_POINT('Ctrl Pts',(-1.43925448419923E-16,-1.17524047358087,
-8.99999999999999));
#421517=CARTESIAN_POINT('Ctrl Pts',(0.678525403784459,-1.17524047358087,
-8.95833333333332));
#421518=CARTESIAN_POINT('Ctrl Pts',(1.01778810567669,-0.587620236790434,
-8.91666666666666));
#421519=CARTESIAN_POINT('Ctrl Pts',(1.35705080756892,2.29132664526027E-15,
-8.87499999999999));
#421520=CARTESIAN_POINT('Ctrl Pts',(1.01778810567669,0.587620236790438,
-8.83333333333333));
#421521=CARTESIAN_POINT('Ctrl Pts',(0.67852540378446,1.17524047358087,-8.79166666666666));
#421522=CARTESIAN_POINT('Ctrl Pts',(0.,1.17524047358087,-8.74999999999999));
#421523=CARTESIAN_POINT('Ctrl Pts',(-0.678525403784459,1.17524047358087,
-8.70833333333333));
#421524=CARTESIAN_POINT('Ctrl Pts',(-1.01778810567669,0.587620236790438,
-8.66666666666666));
#421525=CARTESIAN_POINT('Ctrl Pts',(-1.35705080756892,2.62370823081419E-15,
-8.62499999999999));
#421526=CARTESIAN_POINT('Ctrl Pts',(-1.01778810567669,-0.587620236790433,
-8.58333333333333));
#421527=CARTESIAN_POINT('Ctrl Pts',(-0.67852540378446,-1.17524047358087,
-8.54166666666666));
#421528=CARTESIAN_POINT('Ctrl Pts',(-1.43925448419923E-16,-1.17524047358087,
-8.49999999999999));
#421529=CARTESIAN_POINT('Ctrl Pts',(0.678525403784459,-1.17524047358087,
-8.45833333333333));
#421530=CARTESIAN_POINT('Ctrl Pts',(1.01778810567669,-0.587620236790434,
-8.41666666666666));
#421531=CARTESIAN_POINT('Ctrl Pts',(1.35705080756892,2.29132664526027E-15,
-8.37499999999999));
#421532=CARTESIAN_POINT('Ctrl Pts',(1.01778810567669,0.587620236790438,
-8.33333333333333));
#421533=CARTESIAN_POINT('Ctrl Pts',(0.67852540378446,1.17524047358087,-8.29166666666666));
#421534=CARTESIAN_POINT('Ctrl Pts',(0.,1.17524047358087,-8.24999999999999));
#421535=CARTESIAN_POINT('Ctrl Pts',(-0.678525403784459,1.17524047358087,
-8.20833333333333));
#421536=CARTESIAN_POINT('Ctrl Pts',(-1.01778810567669,0.587620236790438,
-8.16666666666666));
#421537=CARTESIAN_POINT('Ctrl Pts',(-1.35705080756892,2.62370823081419E-15,
-8.12499999999999));
#421538=CARTESIAN_POINT('Ctrl Pts',(-1.01778810567669,-0.587620236790433,
-8.08333333333333));
#421539=CARTESIAN_POINT('Ctrl Pts',(-0.67852540378446,-1.17524047358087,
-8.04166666666666));
#421540=CARTESIAN_POINT('Ctrl Pts',(-1.43925448419923E-16,-1.17524047358087,
-7.99999999999999));
#421541=CARTESIAN_POINT('Ctrl Pts',(0.678525403784459,-1.17524047358087,
-7.95833333333333));
#421542=CARTESIAN_POINT('Ctrl Pts',(1.01778810567669,-0.587620236790434,
-7.91666666666666));
#421543=CARTESIAN_POINT('Ctrl Pts',(1.35705080756892,2.29132664526027E-15,
-7.87499999999999));
#421544=CARTESIAN_POINT('Ctrl Pts',(1.01778810567669,0.587620236790438,
-7.83333333333332));
#421545=CARTESIAN_POINT('Ctrl Pts',(0.67852540378446,1.17524047358087,-7.79166666666666));
#421546=CARTESIAN_POINT('Ctrl Pts',(0.,1.17524047358087,-7.74999999999999));
#421547=CARTESIAN_POINT('Ctrl Pts',(-0.678525403784459,1.17524047358087,
-7.70833333333332));
#421548=CARTESIAN_POINT('Ctrl Pts',(-1.01778810567669,0.587620236790438,
-7.66666666666666));
#421549=CARTESIAN_POINT('Ctrl Pts',(-1.35705080756892,2.62370823081419E-15,
-7.62499999999999));
#421550=CARTESIAN_POINT('Ctrl Pts',(-1.01778810567669,-0.587620236790433,
-7.58333333333332));
#421551=CARTESIAN_POINT('Ctrl Pts',(-0.67852540378446,-1.17524047358087,
-7.54166666666666));
#421552=CARTESIAN_POINT('Ctrl Pts',(-1.43925448419923E-16,-1.17524047358087,
-7.49999999999999));
#421553=CARTESIAN_POINT('Ctrl Pts',(0.678525403784459,-1.17524047358087,
-7.45833333333332));
#421554=CARTESIAN_POINT('Ctrl Pts',(1.01778810567669,-0.587620236790434,
-7.41666666666666));
#421555=CARTESIAN_POINT('Ctrl Pts',(1.35705080756892,2.29132664526027E-15,
-7.37499999999999));
#421556=CARTESIAN_POINT('Ctrl Pts',(1.01778810567669,0.587620236790438,
-7.33333333333332));
#421557=CARTESIAN_POINT('Ctrl Pts',(0.67852540378446,1.17524047358087,-7.29166666666666));
#421558=CARTESIAN_POINT('Ctrl Pts',(0.,1.17524047358087,-7.24999999999999));
#421559=CARTESIAN_POINT('Ctrl Pts',(-0.678525403784459,1.17524047358087,
-7.20833333333332));
#421560=CARTESIAN_POINT('Ctrl Pts',(-1.01778810567669,0.587620236790438,
-7.16666666666666));
#421561=CARTESIAN_POINT('Ctrl Pts',(-1.35705080756892,2.62370823081419E-15,
-7.12499999999999));
#421562=CARTESIAN_POINT('Ctrl Pts',(-1.01778810567669,-0.587620236790433,
-7.08333333333332));
#421563=CARTESIAN_POINT('Ctrl Pts',(-0.67852540378446,-1.17524047358087,
-7.04166666666666));
#421564=CARTESIAN_POINT('Ctrl Pts',(-1.43925448419923E-16,-1.17524047358087,
-6.99999999999999));
#421565=CARTESIAN_POINT('Ctrl Pts',(0.678525403784459,-1.17524047358087,
-6.95833333333332));
#421566=CARTESIAN_POINT('Ctrl Pts',(1.01778810567669,-0.587620236790434,
-6.91666666666666));
#421567=CARTESIAN_POINT('Ctrl Pts',(1.35705080756892,2.29132664526027E-15,
-6.87499999999999));
#421568=CARTESIAN_POINT('Ctrl Pts',(1.01778810567669,0.587620236790438,
-6.83333333333333));
#421569=CARTESIAN_POINT('Ctrl Pts',(0.67852540378446,1.17524047358087,-6.79166666666666));
#421570=CARTESIAN_POINT('Ctrl Pts',(0.,1.17524047358087,-6.74999999999999));
#421571=CARTESIAN_POINT('Ctrl Pts',(-0.678525403784459,1.17524047358087,
-6.70833333333333));
#421572=CARTESIAN_POINT('Ctrl Pts',(-1.01778810567669,0.587620236790438,
-6.66666666666666));
#421573=CARTESIAN_POINT('Ctrl Pts',(-1.35705080756892,2.62370823081419E-15,
-6.62499999999999));
#421574=CARTESIAN_POINT('Ctrl Pts',(-1.01778810567669,-0.587620236790433,
-6.58333333333332));
#421575=CARTESIAN_POINT('Ctrl Pts',(-0.67852540378446,-1.17524047358087,
-6.54166666666666));
#421576=CARTESIAN_POINT('Ctrl Pts',(-1.43925448419923E-16,-1.17524047358087,
-6.49999999999999));
#421577=CARTESIAN_POINT('Ctrl Pts',(0.678525403784459,-1.17524047358087,
-6.45833333333332));
#421578=CARTESIAN_POINT('Ctrl Pts',(1.01778810567669,-0.587620236790434,
-6.41666666666666));
#421579=CARTESIAN_POINT('Ctrl Pts',(1.35705080756892,2.29132664526027E-15,
-6.37499999999999));
#421580=CARTESIAN_POINT('Ctrl Pts',(1.01778810567669,0.587620236790438,
-6.33333333333332));
#421581=CARTESIAN_POINT('Ctrl Pts',(0.67852540378446,1.17524047358087,-6.29166666666666));
#421582=CARTESIAN_POINT('Ctrl Pts',(0.,1.17524047358087,-6.24999999999999));
#421583=CARTESIAN_POINT('Ctrl Pts',(-0.678525403784459,1.17524047358087,
-6.20833333333333));
#421584=CARTESIAN_POINT('Ctrl Pts',(-1.01778810567669,0.587620236790438,
-6.16666666666666));
#421585=CARTESIAN_POINT('Ctrl Pts',(-1.35705080756892,2.62370823081419E-15,
-6.12499999999999));
#421586=CARTESIAN_POINT('Ctrl Pts',(-1.01778810567669,-0.587620236790433,
-6.08333333333333));
#421587=CARTESIAN_POINT('Ctrl Pts',(-0.67852540378446,-1.17524047358087,
-6.04166666666666));
#421588=CARTESIAN_POINT('Ctrl Pts',(-1.43925448419923E-16,-1.17524047358087,
-5.99999999999999));
#421589=CARTESIAN_POINT('Ctrl Pts',(0.678525403784459,-1.17524047358087,
-5.95833333333332));
#421590=CARTESIAN_POINT('Ctrl Pts',(1.01778810567669,-0.587620236790434,
-5.91666666666666));
#421591=CARTESIAN_POINT('Ctrl Pts',(1.35705080756892,2.29132664526027E-15,
-5.87499999999999));
#421592=CARTESIAN_POINT('Ctrl Pts',(1.01778810567669,0.587620236790438,
-5.83333333333333));
#421593=CARTESIAN_POINT('Ctrl Pts',(0.67852540378446,1.17524047358087,-5.79166666666666));
#421594=CARTESIAN_POINT('Ctrl Pts',(0.,1.17524047358087,-5.74999999999999));
#421595=CARTESIAN_POINT('Ctrl Pts',(-0.678525403784459,1.17524047358087,
-5.70833333333332));
#421596=CARTESIAN_POINT('Ctrl Pts',(-1.01778810567669,0.587620236790438,
-5.66666666666666));
#421597=CARTESIAN_POINT('Ctrl Pts',(-1.35705080756892,2.62370823081419E-15,
-5.62499999999999));
#421598=CARTESIAN_POINT('Ctrl Pts',(-1.01778810567669,-0.587620236790433,
-5.58333333333333));
#421599=CARTESIAN_POINT('Ctrl Pts',(-0.67852540378446,-1.17524047358087,
-5.54166666666666));
#421600=CARTESIAN_POINT('Ctrl Pts',(-1.43925448419923E-16,-1.17524047358087,
-5.49999999999999));
#421601=CARTESIAN_POINT('Ctrl Pts',(0.678525403784459,-1.17524047358087,
-5.45833333333332));
#421602=CARTESIAN_POINT('Ctrl Pts',(1.01778810567669,-0.587620236790434,
-5.41666666666666));
#421603=CARTESIAN_POINT('Ctrl Pts',(1.35705080756892,2.29132664526027E-15,
-5.37499999999999));
#421604=CARTESIAN_POINT('Ctrl Pts',(1.01778810567669,0.587620236790438,
-5.33333333333332));
#421605=CARTESIAN_POINT('Ctrl Pts',(0.67852540378446,1.17524047358087,-5.29166666666666));
#421606=CARTESIAN_POINT('Ctrl Pts',(0.,1.17524047358087,-5.24999999999999));
#421607=CARTESIAN_POINT('Ctrl Pts',(-0.678525403784459,1.17524047358087,
-5.20833333333333));
#421608=CARTESIAN_POINT('Ctrl Pts',(-1.01778810567669,0.587620236790438,
-5.16666666666666));
#421609=CARTESIAN_POINT('Ctrl Pts',(-1.35705080756892,2.62370823081419E-15,
-5.12499999999999));
#421610=CARTESIAN_POINT('Ctrl Pts',(-1.01778810567669,-0.587620236790433,
-5.08333333333332));
#421611=CARTESIAN_POINT('Ctrl Pts',(-0.67852540378446,-1.17524047358087,
-5.04166666666666));
#421612=CARTESIAN_POINT('Ctrl Pts',(-1.43925448419923E-16,-1.17524047358087,
-4.99999999999999));
#421613=CARTESIAN_POINT('Ctrl Pts',(0.678525403784459,-1.17524047358087,
-4.95833333333332));
#421614=CARTESIAN_POINT('Ctrl Pts',(1.01778810567669,-0.587620236790434,
-4.91666666666666));
#421615=CARTESIAN_POINT('Ctrl Pts',(1.35705080756892,2.29132664526027E-15,
-4.87499999999999));
#421616=CARTESIAN_POINT('Ctrl Pts',(1.01778810567669,0.587620236790438,
-4.83333333333332));
#421617=CARTESIAN_POINT('Ctrl Pts',(0.67852540378446,1.17524047358087,-4.79166666666666));
#421618=CARTESIAN_POINT('Ctrl Pts',(0.,1.17524047358087,-4.74999999999999));
#421619=CARTESIAN_POINT('Ctrl Pts',(-0.678525403784459,1.17524047358087,
-4.70833333333332));
#421620=CARTESIAN_POINT('Ctrl Pts',(-1.01778810567669,0.587620236790438,
-4.66666666666666));
#421621=CARTESIAN_POINT('Ctrl Pts',(-1.35705080756892,2.62370823081419E-15,
-4.62499999999999));
#421622=CARTESIAN_POINT('Ctrl Pts',(-1.01778810567669,-0.587620236790433,
-4.58333333333332));
#421623=CARTESIAN_POINT('Ctrl Pts',(-0.67852540378446,-1.17524047358087,
-4.54166666666666));
#421624=CARTESIAN_POINT('Ctrl Pts',(-1.43925448419923E-16,-1.17524047358087,
-4.49999999999999));
#421625=CARTESIAN_POINT('Ctrl Pts',(0.678525403784459,-1.17524047358087,
-4.45833333333333));
#421626=CARTESIAN_POINT('Ctrl Pts',(1.01778810567669,-0.587620236790434,
-4.41666666666666));
#421627=CARTESIAN_POINT('Ctrl Pts',(1.35705080756892,2.29132664526027E-15,
-4.37499999999999));
#421628=CARTESIAN_POINT('Ctrl Pts',(1.01778810567669,0.587620236790438,
-4.33333333333333));
#421629=CARTESIAN_POINT('Ctrl Pts',(0.67852540378446,1.17524047358087,-4.29166666666666));
#421630=CARTESIAN_POINT('Ctrl Pts',(0.,1.17524047358087,-4.24999999999999));
#421631=CARTESIAN_POINT('Ctrl Pts',(-0.678525403784459,1.17524047358087,
-4.20833333333332));
#421632=CARTESIAN_POINT('Ctrl Pts',(-1.01778810567669,0.587620236790438,
-4.16666666666666));
#421633=CARTESIAN_POINT('Ctrl Pts',(-1.35705080756892,2.62370823081419E-15,
-4.12499999999999));
#421634=CARTESIAN_POINT('Ctrl Pts',(-1.01778810567669,-0.587620236790433,
-4.08333333333332));
#421635=CARTESIAN_POINT('Ctrl Pts',(-0.67852540378446,-1.17524047358087,
-4.04166666666666));
#421636=CARTESIAN_POINT('Ctrl Pts',(-1.43925448419923E-16,-1.17524047358087,
-3.99999999999999));
#421637=CARTESIAN_POINT('Ctrl Pts',(0.678525403784459,-1.17524047358087,
-3.95833333333332));
#421638=CARTESIAN_POINT('Ctrl Pts',(1.01778810567669,-0.587620236790434,
-3.91666666666666));
#421639=CARTESIAN_POINT('Ctrl Pts',(1.35705080756892,2.29132664526027E-15,
-3.87499999999999));
#421640=CARTESIAN_POINT('Ctrl Pts',(1.01778810567669,0.587620236790438,
-3.83333333333332));
#421641=CARTESIAN_POINT('Ctrl Pts',(0.67852540378446,1.17524047358087,-3.79166666666666));
#421642=CARTESIAN_POINT('Ctrl Pts',(0.,1.17524047358087,-3.74999999999999));
#421643=CARTESIAN_POINT('Ctrl Pts',(-0.678525403784459,1.17524047358087,
-3.70833333333332));
#421644=CARTESIAN_POINT('Ctrl Pts',(-1.01778810567669,0.587620236790438,
-3.66666666666666));
#421645=CARTESIAN_POINT('Ctrl Pts',(-1.35705080756892,2.62370823081419E-15,
-3.62499999999999));
#421646=CARTESIAN_POINT('Ctrl Pts',(-1.01778810567669,-0.587620236790433,
-3.58333333333332));
#421647=CARTESIAN_POINT('Ctrl Pts',(-0.67852540378446,-1.17524047358087,
-3.54166666666666));
#421648=CARTESIAN_POINT('Ctrl Pts',(-1.43925448419923E-16,-1.17524047358087,
-3.49999999999999));
#421649=CARTESIAN_POINT('Ctrl Pts',(0.678525403784459,-1.17524047358087,
-3.45833333333333));
#421650=CARTESIAN_POINT('Ctrl Pts',(1.01778810567669,-0.587620236790434,
-3.41666666666666));
#421651=CARTESIAN_POINT('Ctrl Pts',(1.35705080756892,2.29132664526027E-15,
-3.37499999999999));
#421652=CARTESIAN_POINT('Ctrl Pts',(1.01778810567669,0.587620236790438,
-3.33333333333332));
#421653=CARTESIAN_POINT('Ctrl Pts',(0.67852540378446,1.17524047358087,-3.29166666666666));
#421654=CARTESIAN_POINT('Ctrl Pts',(0.,1.17524047358087,-3.24999999999999));
#421655=CARTESIAN_POINT('Ctrl Pts',(-0.678525403784459,1.17524047358087,
-3.20833333333332));
#421656=CARTESIAN_POINT('Ctrl Pts',(-1.01778810567669,0.587620236790438,
-3.16666666666666));
#421657=CARTESIAN_POINT('Ctrl Pts',(-1.35705080756892,2.62370823081419E-15,
-3.12499999999999));
#421658=CARTESIAN_POINT('Ctrl Pts',(-1.01778810567669,-0.587620236790433,
-3.08333333333332));
#421659=CARTESIAN_POINT('Ctrl Pts',(-0.67852540378446,-1.17524047358087,
-3.04166666666666));
#421660=CARTESIAN_POINT('Ctrl Pts',(-1.43925448419923E-16,-1.17524047358087,
-2.99999999999999));
#421661=CARTESIAN_POINT('Ctrl Pts',(0.678525403784459,-1.17524047358087,
-2.95833333333332));
#421662=CARTESIAN_POINT('Ctrl Pts',(1.01778810567669,-0.587620236790434,
-2.91666666666666));
#421663=CARTESIAN_POINT('Ctrl Pts',(1.35705080756892,2.29132664526027E-15,
-2.87499999999999));
#421664=CARTESIAN_POINT('Ctrl Pts',(1.01778810567669,0.587620236790438,
-2.83333333333332));
#421665=CARTESIAN_POINT('Ctrl Pts',(0.67852540378446,1.17524047358087,-2.79166666666666));
#421666=CARTESIAN_POINT('Ctrl Pts',(0.,1.17524047358087,-2.74999999999999));
#421667=CARTESIAN_POINT('Ctrl Pts',(-0.678525403784459,1.17524047358087,
-2.70833333333332));
#421668=CARTESIAN_POINT('Ctrl Pts',(-1.01778810567669,0.587620236790438,
-2.66666666666666));
#421669=CARTESIAN_POINT('Ctrl Pts',(-1.35705080756892,2.62370823081419E-15,
-2.62499999999999));
#421670=CARTESIAN_POINT('Ctrl Pts',(-1.01778810567669,-0.587620236790433,
-2.58333333333332));
#421671=CARTESIAN_POINT('Ctrl Pts',(-0.67852540378446,-1.17524047358087,
-2.54166666666666));
#421672=CARTESIAN_POINT('Ctrl Pts',(-1.43925448419923E-16,-1.17524047358087,
-2.49999999999999));
#421673=CARTESIAN_POINT('Ctrl Pts',(0.678525403784459,-1.17524047358087,
-2.45833333333332));
#421674=CARTESIAN_POINT('Ctrl Pts',(1.01778810567669,-0.587620236790434,
-2.41666666666666));
#421675=CARTESIAN_POINT('Ctrl Pts',(1.35705080756892,2.29132664526027E-15,
-2.37499999999999));
#421676=CARTESIAN_POINT('Ctrl Pts',(1.01778810567669,0.587620236790438,
-2.33333333333332));
#421677=CARTESIAN_POINT('Ctrl Pts',(0.67852540378446,1.17524047358087,-2.29166666666666));
#421678=CARTESIAN_POINT('Ctrl Pts',(0.,1.17524047358087,-2.24999999999999));
#421679=CARTESIAN_POINT('Ctrl Pts',(-0.678525403784459,1.17524047358087,
-2.20833333333332));
#421680=CARTESIAN_POINT('Ctrl Pts',(-1.01778810567669,0.587620236790438,
-2.16666666666666));
#421681=CARTESIAN_POINT('Ctrl Pts',(-1.35705080756892,2.62370823081419E-15,
-2.12499999999999));
#421682=CARTESIAN_POINT('Ctrl Pts',(-1.01778810567669,-0.587620236790433,
-2.08333333333332));
#421683=CARTESIAN_POINT('Ctrl Pts',(-0.67852540378446,-1.17524047358087,
-2.04166666666666));
#421684=CARTESIAN_POINT('Ctrl Pts',(-1.43925448419923E-16,-1.17524047358087,
-1.99999999999999));
#421685=CARTESIAN_POINT('Ctrl Pts',(0.678525403784459,-1.17524047358087,
-1.95833333333332));
#421686=CARTESIAN_POINT('Ctrl Pts',(1.01778810567669,-0.587620236790434,
-1.91666666666666));
#421687=CARTESIAN_POINT('Ctrl Pts',(1.35705080756892,2.29132664526027E-15,
-1.87499999999999));
#421688=CARTESIAN_POINT('Ctrl Pts',(1.01778810567669,0.587620236790438,
-1.83333333333332));
#421689=CARTESIAN_POINT('Ctrl Pts',(0.67852540378446,1.17524047358087,-1.79166666666666));
#421690=CARTESIAN_POINT('Ctrl Pts',(0.,1.17524047358087,-1.74999999999999));
#421691=CARTESIAN_POINT('Ctrl Pts',(-0.678525403784459,1.17524047358087,
-1.70833333333332));
#421692=CARTESIAN_POINT('Ctrl Pts',(-1.01778810567669,0.587620236790438,
-1.66666666666666));
#421693=CARTESIAN_POINT('Ctrl Pts',(-1.35705080756892,2.62370823081419E-15,
-1.62499999999999));
#421694=CARTESIAN_POINT('Ctrl Pts',(-1.01778810567669,-0.587620236790433,
-1.58333333333332));
#421695=CARTESIAN_POINT('Ctrl Pts',(-0.67852540378446,-1.17524047358087,
-1.54166666666666));
#421696=CARTESIAN_POINT('Ctrl Pts',(-1.43925448419923E-16,-1.17524047358087,
-1.49999999999999));
#421697=CARTESIAN_POINT('Ctrl Pts',(0.678525403784459,-1.17524047358087,
-1.45833333333332));
#421698=CARTESIAN_POINT('Ctrl Pts',(1.01778810567669,-0.587620236790434,
-1.41666666666666));
#421699=CARTESIAN_POINT('Ctrl Pts',(1.35705080756892,2.29132664526027E-15,
-1.37499999999999));
#421700=CARTESIAN_POINT('Ctrl Pts',(1.01778810567669,0.587620236790438,
-1.33333333333332));
#421701=CARTESIAN_POINT('Ctrl Pts',(0.67852540378446,1.17524047358087,-1.29166666666666));
#421702=CARTESIAN_POINT('Ctrl Pts',(0.,1.17524047358087,-1.24999999999999));
#421703=CARTESIAN_POINT('Ctrl Pts',(-0.678525403784459,1.17524047358087,
-1.20833333333332));
#421704=CARTESIAN_POINT('Ctrl Pts',(-1.01778810567669,0.587620236790438,
-1.16666666666666));
#421705=CARTESIAN_POINT('Ctrl Pts',(-1.35705080756892,2.62370823081419E-15,
-1.12499999999999));
#421706=CARTESIAN_POINT('Ctrl Pts',(-1.01778810567669,-0.587620236790433,
-1.08333333333332));
#421707=CARTESIAN_POINT('Ctrl Pts',(-0.67852540378446,-1.17524047358087,
-1.04166666666666));
#421708=CARTESIAN_POINT('Ctrl Pts',(-1.43925448419923E-16,-1.17524047358087,
-0.99999999999999));
#421709=CARTESIAN_POINT('Ctrl Pts',(0.678525403784459,-1.17524047358087,
-0.958333333333323));
#421710=CARTESIAN_POINT('Ctrl Pts',(1.01778810567669,-0.587620236790434,
-0.916666666666658));
#421711=CARTESIAN_POINT('Ctrl Pts',(1.35705080756892,2.29132664526027E-15,
-0.87499999999999));
#421712=CARTESIAN_POINT('Ctrl Pts',(1.01778810567669,0.587620236790438,
-0.833333333333323));
#421713=CARTESIAN_POINT('Ctrl Pts',(0.67852540378446,1.17524047358087,-0.791666666666657));
#421714=CARTESIAN_POINT('Ctrl Pts',(0.,1.17524047358087,-0.74999999999999));
#421715=CARTESIAN_POINT('Ctrl Pts',(-0.678525403784459,1.17524047358087,
-0.708333333333325));
#421716=CARTESIAN_POINT('Ctrl Pts',(-1.01778810567669,0.587620236790438,
-0.666666666666658));
#421717=CARTESIAN_POINT('Ctrl Pts',(-1.35705080756892,2.62370823081419E-15,
-0.62499999999999));
#421718=CARTESIAN_POINT('Ctrl Pts',(-1.01778810567669,-0.587620236790433,
-0.583333333333325));
#421719=CARTESIAN_POINT('Ctrl Pts',(-0.67852540378446,-1.17524047358087,
-0.541666666666657));
#421720=CARTESIAN_POINT('Ctrl Pts',(-1.43925448419923E-16,-1.17524047358087,
-0.49999999999999));
#421721=CARTESIAN_POINT('Ctrl Pts',(0.678525403784459,-1.17524047358087,
-0.458333333333324));
#421722=CARTESIAN_POINT('Ctrl Pts',(1.01778810567669,-0.587620236790434,
-0.416666666666657));
#421723=CARTESIAN_POINT('Ctrl Pts',(1.35705080756892,2.29132664526027E-15,
-0.37499999999999));
#421724=CARTESIAN_POINT('Ctrl Pts',(1.01778810567669,0.587620236790438,
-0.333333333333324));
#421725=CARTESIAN_POINT('Ctrl Pts',(0.67852540378446,1.17524047358087,-0.291666666666657));
#421726=CARTESIAN_POINT('Ctrl Pts',(0.,1.17524047358087,-0.24999999999999));
#421727=CARTESIAN_POINT('Ctrl Pts',(-0.678525403784459,1.17524047358087,
-0.208333333333324));
#421728=CARTESIAN_POINT('Ctrl Pts',(-1.01778810567669,0.587620236790438,
-0.166666666666657));
#421729=CARTESIAN_POINT('Ctrl Pts',(-1.35705080756892,2.62370823081419E-15,
-0.124999999999991));
#421730=CARTESIAN_POINT('Ctrl Pts',(-1.01778810567669,-0.587620236790433,
-0.0833333333333242));
#421731=CARTESIAN_POINT('Ctrl Pts',(-0.67852540378446,-1.17524047358087,
-0.0416666666666569));
#421732=CARTESIAN_POINT('Ctrl Pts',(-1.43925448419923E-16,-1.17524047358087,
8.67361737988404E-15));
#421733=CARTESIAN_POINT('Ctrl Pts',(0.678525403784459,-1.17524047358087,
0.041666666666676));
#421734=CARTESIAN_POINT('Ctrl Pts',(1.01778810567669,-0.587620236790434,
0.0833333333333432));
#421735=CARTESIAN_POINT('Ctrl Pts',(1.35705080756892,2.29132664526027E-15,
0.125000000000009));
#421736=CARTESIAN_POINT('Ctrl Pts',(1.01778810567669,0.587620236790438,
0.166666666666676));
#421737=CARTESIAN_POINT('Ctrl Pts',(0.67852540378446,1.17524047358087,0.208333333333343));
#421738=CARTESIAN_POINT('Ctrl Pts',(0.,1.17524047358087,0.250000000000009));
#421739=CARTESIAN_POINT('Ctrl Pts',(-0.678525403784459,1.17524047358087,
0.291666666666676));
#421740=CARTESIAN_POINT('Ctrl Pts',(-1.01778810567669,0.587620236790438,
0.333333333333343));
#421741=CARTESIAN_POINT('Ctrl Pts',(-1.35705080756892,2.62370823081419E-15,
0.375000000000009));
#421742=CARTESIAN_POINT('Ctrl Pts',(-1.01778810567669,-0.587620236790433,
0.416666666666676));
#421743=CARTESIAN_POINT('Ctrl Pts',(-0.67852540378446,-1.17524047358087,
0.458333333333344));
#421744=CARTESIAN_POINT('Ctrl Pts',(-1.43925448419923E-16,-1.17524047358087,
0.500000000000009));
#421745=CARTESIAN_POINT('Ctrl Pts',(0.678525403784459,-1.17524047358087,
0.541666666666676));
#421746=CARTESIAN_POINT('Ctrl Pts',(1.01778810567669,-0.587620236790434,
0.583333333333342));
#421747=CARTESIAN_POINT('Ctrl Pts',(1.35705080756892,2.29132664526027E-15,
0.625000000000009));
#421748=CARTESIAN_POINT('Ctrl Pts',(1.01778810567669,0.587620236790438,
0.666666666666677));
#421749=CARTESIAN_POINT('Ctrl Pts',(0.67852540378446,1.17524047358087,0.708333333333342));
#421750=CARTESIAN_POINT('Ctrl Pts',(0.,1.17524047358087,0.750000000000009));
#421751=CARTESIAN_POINT('Ctrl Pts',(-0.678525403784459,1.17524047358087,
0.791666666666677));
#421752=CARTESIAN_POINT('Ctrl Pts',(-1.01778810567669,0.587620236790438,
0.833333333333342));
#421753=CARTESIAN_POINT('Ctrl Pts',(-1.35705080756892,2.62370823081419E-15,
0.87500000000001));
#421754=CARTESIAN_POINT('Ctrl Pts',(-1.01778810567669,-0.587620236790433,
0.916666666666677));
#421755=CARTESIAN_POINT('Ctrl Pts',(-0.67852540378446,-1.17524047358087,
0.958333333333342));
#421756=CARTESIAN_POINT('Ctrl Pts',(-1.43925448419923E-16,-1.17524047358087,
1.00000000000001));
#421757=CARTESIAN_POINT('Ctrl Pts',(0.678525403784459,-1.17524047358087,
1.04166666666668));
#421758=CARTESIAN_POINT('Ctrl Pts',(1.01778810567669,-0.587620236790434,
1.08333333333334));
#421759=CARTESIAN_POINT('Ctrl Pts',(1.35705080756892,2.29132664526027E-15,
1.12500000000001));
#421760=CARTESIAN_POINT('Ctrl Pts',(1.01778810567669,0.587620236790438,
1.16666666666668));
#421761=CARTESIAN_POINT('Ctrl Pts',(0.67852540378446,1.17524047358087,1.20833333333334));
#421762=CARTESIAN_POINT('Ctrl Pts',(0.,1.17524047358087,1.25000000000001));
#421763=CARTESIAN_POINT('Ctrl Pts',(-0.678525403784459,1.17524047358087,
1.29166666666668));
#421764=CARTESIAN_POINT('Ctrl Pts',(-1.01778810567669,0.587620236790438,
1.33333333333334));
#421765=CARTESIAN_POINT('Ctrl Pts',(-1.35705080756892,2.62370823081419E-15,
1.37500000000001));
#421766=CARTESIAN_POINT('Ctrl Pts',(-1.01778810567669,-0.587620236790433,
1.41666666666668));
#421767=CARTESIAN_POINT('Ctrl Pts',(-0.67852540378446,-1.17524047358087,
1.45833333333334));
#421768=CARTESIAN_POINT('Ctrl Pts',(-1.43925448419923E-16,-1.17524047358087,
1.50000000000001));
#421769=CARTESIAN_POINT('Ctrl Pts',(0.678525403784459,-1.17524047358087,
1.54166666666668));
#421770=CARTESIAN_POINT('Ctrl Pts',(1.01778810567669,-0.587620236790434,
1.58333333333334));
#421771=CARTESIAN_POINT('Ctrl Pts',(1.35705080756892,2.29132664526027E-15,
1.62500000000001));
#421772=CARTESIAN_POINT('Ctrl Pts',(1.01778810567669,0.587620236790438,
1.66666666666668));
#421773=CARTESIAN_POINT('Ctrl Pts',(0.67852540378446,1.17524047358087,1.70833333333334));
#421774=CARTESIAN_POINT('Ctrl Pts',(0.,1.17524047358087,1.75000000000001));
#421775=CARTESIAN_POINT('Ctrl Pts',(-0.678525403784459,1.17524047358087,
1.79166666666668));
#421776=CARTESIAN_POINT('Ctrl Pts',(-1.01778810567669,0.587620236790438,
1.83333333333334));
#421777=CARTESIAN_POINT('Ctrl Pts',(-1.35705080756892,2.62370823081419E-15,
1.87500000000001));
#421778=CARTESIAN_POINT('Ctrl Pts',(-1.01778810567669,-0.587620236790433,
1.91666666666668));
#421779=CARTESIAN_POINT('Ctrl Pts',(-0.67852540378446,-1.17524047358087,
1.95833333333334));
#421780=CARTESIAN_POINT('Ctrl Pts',(-1.43925448419923E-16,-1.17524047358087,
2.00000000000001));
#421781=CARTESIAN_POINT('Ctrl Pts',(0.678525403784459,-1.17524047358087,
2.04166666666668));
#421782=CARTESIAN_POINT('Ctrl Pts',(1.01778810567669,-0.587620236790434,
2.08333333333334));
#421783=CARTESIAN_POINT('Ctrl Pts',(1.35705080756892,2.29132664526027E-15,
2.12500000000001));
#421784=CARTESIAN_POINT('Ctrl Pts',(1.01778810567669,0.587620236790438,
2.16666666666668));
#421785=CARTESIAN_POINT('Ctrl Pts',(0.67852540378446,1.17524047358087,2.20833333333334));
#421786=CARTESIAN_POINT('Ctrl Pts',(0.,1.17524047358087,2.25000000000001));
#421787=CARTESIAN_POINT('Ctrl Pts',(-0.678525403784459,1.17524047358087,
2.29166666666668));
#421788=CARTESIAN_POINT('Ctrl Pts',(-1.01778810567669,0.587620236790438,
2.33333333333334));
#421789=CARTESIAN_POINT('Ctrl Pts',(-1.35705080756892,2.62370823081419E-15,
2.37500000000001));
#421790=CARTESIAN_POINT('Ctrl Pts',(-1.01778810567669,-0.587620236790433,
2.41666666666668));
#421791=CARTESIAN_POINT('Ctrl Pts',(-0.67852540378446,-1.17524047358087,
2.45833333333334));
#421792=CARTESIAN_POINT('Ctrl Pts',(-1.43925448419923E-16,-1.17524047358087,
2.50000000000001));
#421793=CARTESIAN_POINT('Ctrl Pts',(0.678525403784459,-1.17524047358087,
2.54166666666668));
#421794=CARTESIAN_POINT('Ctrl Pts',(1.01778810567669,-0.587620236790434,
2.58333333333334));
#421795=CARTESIAN_POINT('Ctrl Pts',(1.35705080756892,2.29132664526027E-15,
2.62500000000001));
#421796=CARTESIAN_POINT('Ctrl Pts',(1.01778810567669,0.587620236790438,
2.66666666666668));
#421797=CARTESIAN_POINT('Ctrl Pts',(0.67852540378446,1.17524047358087,2.70833333333334));
#421798=CARTESIAN_POINT('Ctrl Pts',(0.,1.17524047358087,2.75000000000001));
#421799=CARTESIAN_POINT('Ctrl Pts',(-0.678525403784459,1.17524047358087,
2.79166666666668));
#421800=CARTESIAN_POINT('Ctrl Pts',(-1.01778810567669,0.587620236790438,
2.83333333333334));
#421801=CARTESIAN_POINT('Ctrl Pts',(-1.35705080756892,2.62370823081419E-15,
2.87500000000001));
#421802=CARTESIAN_POINT('Ctrl Pts',(-1.01778810567669,-0.587620236790433,
2.91666666666668));
#421803=CARTESIAN_POINT('Ctrl Pts',(-0.67852540378446,-1.17524047358087,
2.95833333333334));
#421804=CARTESIAN_POINT('Ctrl Pts',(-1.43925448419923E-16,-1.17524047358087,
3.00000000000001));
#421805=CARTESIAN_POINT('Ctrl Pts',(0.678525403784459,-1.17524047358087,
3.04166666666668));
#421806=CARTESIAN_POINT('Ctrl Pts',(1.01778810567669,-0.587620236790434,
3.08333333333334));
#421807=CARTESIAN_POINT('Ctrl Pts',(1.35705080756892,2.29132664526027E-15,
3.12500000000001));
#421808=CARTESIAN_POINT('Ctrl Pts',(1.01778810567669,0.587620236790438,
3.16666666666668));
#421809=CARTESIAN_POINT('Ctrl Pts',(0.67852540378446,1.17524047358087,3.20833333333334));
#421810=CARTESIAN_POINT('Ctrl Pts',(0.,1.17524047358087,3.25000000000001));
#421811=CARTESIAN_POINT('Ctrl Pts',(-0.678525403784459,1.17524047358087,
3.29166666666668));
#421812=CARTESIAN_POINT('Ctrl Pts',(-1.01778810567669,0.587620236790438,
3.33333333333334));
#421813=CARTESIAN_POINT('Ctrl Pts',(-1.35705080756892,2.62370823081419E-15,
3.37500000000001));
#421814=CARTESIAN_POINT('Ctrl Pts',(-1.01778810567669,-0.587620236790433,
3.41666666666668));
#421815=CARTESIAN_POINT('Ctrl Pts',(-0.67852540378446,-1.17524047358087,
3.45833333333334));
#421816=CARTESIAN_POINT('Ctrl Pts',(-1.43925448419923E-16,-1.17524047358087,
3.50000000000001));
#421817=CARTESIAN_POINT('Ctrl Pts',(0.678525403784459,-1.17524047358087,
3.54166666666668));
#421818=CARTESIAN_POINT('Ctrl Pts',(1.01778810567669,-0.587620236790434,
3.58333333333334));
#421819=CARTESIAN_POINT('Ctrl Pts',(1.35705080756892,2.29132664526027E-15,
3.62500000000001));
#421820=CARTESIAN_POINT('Ctrl Pts',(1.01778810567669,0.587620236790438,
3.66666666666668));
#421821=CARTESIAN_POINT('Ctrl Pts',(0.67852540378446,1.17524047358087,3.70833333333334));
#421822=CARTESIAN_POINT('Ctrl Pts',(0.,1.17524047358087,3.75000000000001));
#421823=CARTESIAN_POINT('Ctrl Pts',(-0.678525403784459,1.17524047358087,
3.79166666666668));
#421824=CARTESIAN_POINT('Ctrl Pts',(-1.01778810567669,0.587620236790438,
3.83333333333334));
#421825=CARTESIAN_POINT('Ctrl Pts',(-1.35705080756892,2.62370823081419E-15,
3.87500000000001));
#421826=CARTESIAN_POINT('Ctrl Pts',(-1.01778810567669,-0.587620236790433,
3.91666666666668));
#421827=CARTESIAN_POINT('Ctrl Pts',(-0.67852540378446,-1.17524047358087,
3.95833333333334));
#421828=CARTESIAN_POINT('Ctrl Pts',(-1.43925448419923E-16,-1.17524047358087,
4.00000000000001));
#421829=CARTESIAN_POINT('Ctrl Pts',(0.678525403784459,-1.17524047358087,
4.04166666666667));
#421830=CARTESIAN_POINT('Ctrl Pts',(1.01778810567669,-0.587620236790434,
4.08333333333334));
#421831=CARTESIAN_POINT('Ctrl Pts',(1.35705080756892,2.29132664526027E-15,
4.12500000000001));
#421832=CARTESIAN_POINT('Ctrl Pts',(1.01778810567669,0.587620236790438,
4.16666666666667));
#421833=CARTESIAN_POINT('Ctrl Pts',(0.67852540378446,1.17524047358087,4.20833333333334));
#421834=CARTESIAN_POINT('Ctrl Pts',(0.,1.17524047358087,4.25000000000001));
#421835=CARTESIAN_POINT('Ctrl Pts',(-0.678525403784459,1.17524047358087,
4.29166666666667));
#421836=CARTESIAN_POINT('Ctrl Pts',(-1.01778810567669,0.587620236790438,
4.33333333333334));
#421837=CARTESIAN_POINT('Ctrl Pts',(-1.35705080756892,2.62370823081419E-15,
4.37500000000001));
#421838=CARTESIAN_POINT('Ctrl Pts',(-1.01778810567669,-0.587620236790433,
4.41666666666667));
#421839=CARTESIAN_POINT('Ctrl Pts',(-0.67852540378446,-1.17524047358087,
4.45833333333334));
#421840=CARTESIAN_POINT('Ctrl Pts',(-1.43925448419923E-16,-1.17524047358087,
4.50000000000001));
#421841=CARTESIAN_POINT('Ctrl Pts',(0.678525403784459,-1.17524047358087,
4.54166666666667));
#421842=CARTESIAN_POINT('Ctrl Pts',(1.01778810567669,-0.587620236790434,
4.58333333333334));
#421843=CARTESIAN_POINT('Ctrl Pts',(1.35705080756892,2.29132664526027E-15,
4.62500000000001));
#421844=CARTESIAN_POINT('Ctrl Pts',(1.01778810567669,0.587620236790438,
4.66666666666667));
#421845=CARTESIAN_POINT('Ctrl Pts',(0.67852540378446,1.17524047358087,4.70833333333334));
#421846=CARTESIAN_POINT('Ctrl Pts',(0.,1.17524047358087,4.75000000000001));
#421847=CARTESIAN_POINT('Ctrl Pts',(-0.678525403784459,1.17524047358087,
4.79166666666667));
#421848=CARTESIAN_POINT('Ctrl Pts',(-1.01778810567669,0.587620236790438,
4.83333333333334));
#421849=CARTESIAN_POINT('Ctrl Pts',(-1.35705080756892,2.62370823081419E-15,
4.87500000000001));
#421850=CARTESIAN_POINT('Ctrl Pts',(-1.01778810567669,-0.587620236790433,
4.91666666666667));
#421851=CARTESIAN_POINT('Ctrl Pts',(-0.67852540378446,-1.17524047358087,
4.95833333333334));
#421852=CARTESIAN_POINT('Ctrl Pts',(-1.43925448419923E-16,-1.17524047358087,
5.00000000000001));
#421853=CARTESIAN_POINT('Ctrl Pts',(0.678525403784459,-1.17524047358087,
5.04166666666667));
#421854=CARTESIAN_POINT('Ctrl Pts',(1.01778810567669,-0.587620236790434,
5.08333333333335));
#421855=CARTESIAN_POINT('Ctrl Pts',(1.35705080756892,2.29132664526027E-15,
5.12500000000001));
#421856=CARTESIAN_POINT('Ctrl Pts',(1.01778810567669,0.587620236790438,
5.16666666666667));
#421857=CARTESIAN_POINT('Ctrl Pts',(0.67852540378446,1.17524047358087,5.20833333333334));
#421858=CARTESIAN_POINT('Ctrl Pts',(0.,1.17524047358087,5.25000000000001));
#421859=CARTESIAN_POINT('Ctrl Pts',(-0.678525403784459,1.17524047358087,
5.29166666666668));
#421860=CARTESIAN_POINT('Ctrl Pts',(-1.01778810567669,0.587620236790438,
5.33333333333334));
#421861=CARTESIAN_POINT('Ctrl Pts',(-1.35705080756892,2.62370823081419E-15,
5.37500000000001));
#421862=CARTESIAN_POINT('Ctrl Pts',(-1.01778810567669,-0.587620236790433,
5.41666666666668));
#421863=CARTESIAN_POINT('Ctrl Pts',(-0.67852540378446,-1.17524047358087,
5.45833333333334));
#421864=CARTESIAN_POINT('Ctrl Pts',(-1.43925448419923E-16,-1.17524047358087,
5.50000000000001));
#421865=CARTESIAN_POINT('Ctrl Pts',(0.678525403784459,-1.17524047358087,
5.54166666666667));
#421866=CARTESIAN_POINT('Ctrl Pts',(1.01778810567669,-0.587620236790434,
5.58333333333334));
#421867=CARTESIAN_POINT('Ctrl Pts',(1.35705080756892,2.29132664526027E-15,
5.62500000000001));
#421868=CARTESIAN_POINT('Ctrl Pts',(1.01778810567669,0.587620236790438,
5.66666666666668));
#421869=CARTESIAN_POINT('Ctrl Pts',(0.67852540378446,1.17524047358087,5.70833333333334));
#421870=CARTESIAN_POINT('Ctrl Pts',(0.,1.17524047358087,5.75000000000001));
#421871=CARTESIAN_POINT('Ctrl Pts',(-0.678525403784459,1.17524047358087,
5.79166666666668));
#421872=CARTESIAN_POINT('Ctrl Pts',(-1.01778810567669,0.587620236790438,
5.83333333333334));
#421873=CARTESIAN_POINT('Ctrl Pts',(-1.35705080756892,2.62370823081419E-15,
5.87500000000001));
#421874=CARTESIAN_POINT('Ctrl Pts',(-1.01778810567669,-0.587620236790433,
5.91666666666668));
#421875=CARTESIAN_POINT('Ctrl Pts',(-0.67852540378446,-1.17524047358087,
5.95833333333334));
#421876=CARTESIAN_POINT('Ctrl Pts',(-1.43925448419923E-16,-1.17524047358087,
6.00000000000001));
#421877=CARTESIAN_POINT('Ctrl Pts',(0.678525403784459,-1.17524047358087,
6.04166666666668));
#421878=CARTESIAN_POINT('Ctrl Pts',(1.01778810567669,-0.587620236790434,
6.08333333333334));
#421879=CARTESIAN_POINT('Ctrl Pts',(1.35705080756892,2.29132664526027E-15,
6.12500000000001));
#421880=CARTESIAN_POINT('Ctrl Pts',(1.01778810567669,0.587620236790438,
6.16666666666668));
#421881=CARTESIAN_POINT('Ctrl Pts',(0.67852540378446,1.17524047358087,6.20833333333334));
#421882=CARTESIAN_POINT('Ctrl Pts',(0.,1.17524047358087,6.25000000000001));
#421883=CARTESIAN_POINT('Ctrl Pts',(-0.678525403784459,1.17524047358087,
6.29166666666668));
#421884=CARTESIAN_POINT('Ctrl Pts',(-1.01778810567669,0.587620236790438,
6.33333333333334));
#421885=CARTESIAN_POINT('Ctrl Pts',(-1.35705080756892,2.62370823081419E-15,
6.37500000000001));
#421886=CARTESIAN_POINT('Ctrl Pts',(-1.01778810567669,-0.587620236790433,
6.41666666666668));
#421887=CARTESIAN_POINT('Ctrl Pts',(-0.67852540378446,-1.17524047358087,
6.45833333333334));
#421888=CARTESIAN_POINT('Ctrl Pts',(-1.43925448419923E-16,-1.17524047358087,
6.50000000000001));
#421889=CARTESIAN_POINT('Ctrl Pts',(0.678525403784459,-1.17524047358087,
6.54166666666668));
#421890=CARTESIAN_POINT('Ctrl Pts',(1.01778810567669,-0.587620236790434,
6.58333333333334));
#421891=CARTESIAN_POINT('Ctrl Pts',(1.35705080756892,2.29132664526027E-15,
6.62500000000001));
#421892=CARTESIAN_POINT('Ctrl Pts',(1.01778810567669,0.587620236790438,
6.66666666666668));
#421893=CARTESIAN_POINT('Ctrl Pts',(0.67852540378446,1.17524047358087,6.70833333333334));
#421894=CARTESIAN_POINT('Ctrl Pts',(0.,1.17524047358087,6.75000000000001));
#421895=CARTESIAN_POINT('Ctrl Pts',(-0.678525403784459,1.17524047358087,
6.79166666666668));
#421896=CARTESIAN_POINT('Ctrl Pts',(-1.01778810567669,0.587620236790438,
6.83333333333334));
#421897=CARTESIAN_POINT('Ctrl Pts',(-1.35705080756892,2.62370823081419E-15,
6.87500000000001));
#421898=CARTESIAN_POINT('Ctrl Pts',(-1.01778810567669,-0.587620236790433,
6.91666666666668));
#421899=CARTESIAN_POINT('Ctrl Pts',(-0.67852540378446,-1.17524047358087,
6.95833333333334));
#421900=CARTESIAN_POINT('Ctrl Pts',(-1.43925448419923E-16,-1.17524047358087,
7.00000000000001));
#421901=CARTESIAN_POINT('Ctrl Pts',(0.678525403784459,-1.17524047358087,
7.04166666666668));
#421902=CARTESIAN_POINT('Ctrl Pts',(1.01778810567669,-0.587620236790434,
7.08333333333334));
#421903=CARTESIAN_POINT('Ctrl Pts',(1.35705080756892,2.29132664526027E-15,
7.12500000000001));
#421904=CARTESIAN_POINT('Ctrl Pts',(1.01778810567669,0.587620236790438,
7.16666666666668));
#421905=CARTESIAN_POINT('Ctrl Pts',(0.67852540378446,1.17524047358087,7.20833333333334));
#421906=CARTESIAN_POINT('Ctrl Pts',(0.,1.17524047358087,7.25000000000001));
#421907=CARTESIAN_POINT('Ctrl Pts',(-0.678525403784459,1.17524047358087,
7.29166666666668));
#421908=CARTESIAN_POINT('Ctrl Pts',(-1.01778810567669,0.587620236790438,
7.33333333333334));
#421909=CARTESIAN_POINT('Ctrl Pts',(-1.35705080756892,2.62370823081419E-15,
7.37500000000001));
#421910=CARTESIAN_POINT('Ctrl Pts',(-1.01778810567669,-0.587620236790433,
7.41666666666668));
#421911=CARTESIAN_POINT('Ctrl Pts',(-0.67852540378446,-1.17524047358087,
7.45833333333334));
#421912=CARTESIAN_POINT('Ctrl Pts',(-1.43925448419923E-16,-1.17524047358087,
7.50000000000001));
#421913=CARTESIAN_POINT('Ctrl Pts',(0.678525403784459,-1.17524047358087,
7.54166666666668));
#421914=CARTESIAN_POINT('Ctrl Pts',(1.01778810567669,-0.587620236790434,
7.58333333333334));
#421915=CARTESIAN_POINT('Ctrl Pts',(1.35705080756892,2.29132664526027E-15,
7.62500000000001));
#421916=CARTESIAN_POINT('Ctrl Pts',(1.01778810567669,0.587620236790438,
7.66666666666668));
#421917=CARTESIAN_POINT('Ctrl Pts',(0.67852540378446,1.17524047358087,7.70833333333334));
#421918=CARTESIAN_POINT('Ctrl Pts',(0.,1.17524047358087,7.75000000000001));
#421919=CARTESIAN_POINT('Ctrl Pts',(-0.678525403784459,1.17524047358087,
7.79166666666667));
#421920=CARTESIAN_POINT('Ctrl Pts',(-1.01778810567669,0.587620236790438,
7.83333333333334));
#421921=CARTESIAN_POINT('Ctrl Pts',(-1.35705080756892,2.62370823081419E-15,
7.87500000000001));
#421922=CARTESIAN_POINT('Ctrl Pts',(-1.01778810567669,-0.587620236790433,
7.91666666666667));
#421923=CARTESIAN_POINT('Ctrl Pts',(-0.67852540378446,-1.17524047358087,
7.95833333333334));
#421924=CARTESIAN_POINT('Ctrl Pts',(-1.43925448419923E-16,-1.17524047358087,
8.00000000000001));
#421925=CARTESIAN_POINT('Ctrl Pts',(0.678525403784459,-1.17524047358087,
8.04166666666667));
#421926=CARTESIAN_POINT('Ctrl Pts',(1.01778810567669,-0.587620236790434,
8.08333333333334));
#421927=CARTESIAN_POINT('Ctrl Pts',(1.35705080756892,2.29132664526027E-15,
8.12500000000001));
#421928=CARTESIAN_POINT('Ctrl Pts',(1.01778810567669,0.587620236790438,
8.16666666666667));
#421929=CARTESIAN_POINT('Ctrl Pts',(0.67852540378446,1.17524047358087,8.20833333333334));
#421930=CARTESIAN_POINT('Ctrl Pts',(0.,1.17524047358087,8.25000000000001));
#421931=CARTESIAN_POINT('Ctrl Pts',(-0.678525403784459,1.17524047358087,
8.29166666666667));
#421932=CARTESIAN_POINT('Ctrl Pts',(-1.01778810567669,0.587620236790438,
8.33333333333334));
#421933=CARTESIAN_POINT('Ctrl Pts',(-1.35705080756892,2.62370823081419E-15,
8.37500000000001));
#421934=CARTESIAN_POINT('Ctrl Pts',(-1.01778810567669,-0.587620236790433,
8.41666666666667));
#421935=CARTESIAN_POINT('Ctrl Pts',(-0.67852540378446,-1.17524047358087,
8.45833333333335));
#421936=CARTESIAN_POINT('Ctrl Pts',(-1.43925448419923E-16,-1.17524047358087,
8.50000000000001));
#421937=CARTESIAN_POINT('Ctrl Pts',(0.678525403784459,-1.17524047358087,
8.54166666666667));
#421938=CARTESIAN_POINT('Ctrl Pts',(1.01778810567669,-0.587620236790434,
8.58333333333334));
#421939=CARTESIAN_POINT('Ctrl Pts',(1.35705080756892,2.29132664526027E-15,
8.62500000000001));
#421940=CARTESIAN_POINT('Ctrl Pts',(1.01778810567669,0.587620236790438,
8.66666666666667));
#421941=CARTESIAN_POINT('Ctrl Pts',(0.67852540378446,1.17524047358087,8.70833333333334));
#421942=CARTESIAN_POINT('Ctrl Pts',(0.,1.17524047358087,8.75000000000001));
#421943=CARTESIAN_POINT('Ctrl Pts',(-0.678525403784459,1.17524047358087,
8.79166666666667));
#421944=CARTESIAN_POINT('Ctrl Pts',(-1.01778810567669,0.587620236790438,
8.83333333333334));
#421945=CARTESIAN_POINT('Ctrl Pts',(-1.35705080756892,2.62370823081419E-15,
8.87500000000001));
#421946=CARTESIAN_POINT('Ctrl Pts',(-1.01778810567669,-0.587620236790433,
8.91666666666667));
#421947=CARTESIAN_POINT('Ctrl Pts',(-0.67852540378446,-1.17524047358087,
8.95833333333334));
#421948=CARTESIAN_POINT('Ctrl Pts',(-1.43925448419923E-16,-1.17524047358087,
9.00000000000001));
#421949=CARTESIAN_POINT('Ctrl Pts',(0.678525403784459,-1.17524047358087,
9.04166666666667));
#421950=CARTESIAN_POINT('Ctrl Pts',(1.01778810567669,-0.587620236790434,
9.08333333333334));
#421951=CARTESIAN_POINT('Ctrl Pts',(1.35705080756892,2.29132664526027E-15,
9.12500000000001));
#421952=CARTESIAN_POINT('Ctrl Pts',(1.01778810567669,0.587620236790438,
9.16666666666667));
#421953=CARTESIAN_POINT('Ctrl Pts',(0.67852540378446,1.17524047358087,9.20833333333334));
#421954=CARTESIAN_POINT('Ctrl Pts',(0.,1.17524047358087,9.25000000000001));
#421955=CARTESIAN_POINT('Ctrl Pts',(-0.678525403784459,1.17524047358087,
9.29166666666668));
#421956=CARTESIAN_POINT('Ctrl Pts',(-1.01778810567669,0.587620236790438,
9.33333333333334));
#421957=CARTESIAN_POINT('Ctrl Pts',(-1.35705080756892,2.62370823081419E-15,
9.37500000000001));
#421958=CARTESIAN_POINT('Ctrl Pts',(-1.01778810567669,-0.587620236790433,
9.41666666666667));
#421959=CARTESIAN_POINT('Ctrl Pts',(-0.67852540378446,-1.17524047358087,
9.45833333333334));
#421960=CARTESIAN_POINT('Ctrl Pts',(-1.43925448419923E-16,-1.17524047358087,
9.50000000000001));
#421961=CARTESIAN_POINT('Ctrl Pts',(0.678525403784459,-1.17524047358087,
9.54166666666667));
#421962=CARTESIAN_POINT('Ctrl Pts',(1.01778810567669,-0.587620236790434,
9.58333333333334));
#421963=CARTESIAN_POINT('Ctrl Pts',(1.35705080756892,2.29132664526027E-15,
9.62500000000001));
#421964=CARTESIAN_POINT('Ctrl Pts',(1.01778810567669,0.587620236790438,
9.66666666666667));
#421965=CARTESIAN_POINT('Ctrl Pts',(0.67852540378446,1.17524047358087,9.70833333333334));
#421966=CARTESIAN_POINT('Ctrl Pts',(0.,1.17524047358087,9.75000000000001));
#421967=CARTESIAN_POINT('Ctrl Pts',(-0.678525403784459,1.17524047358087,
9.79166666666668));
#421968=CARTESIAN_POINT('Ctrl Pts',(-1.01778810567669,0.587620236790438,
9.83333333333334));
#421969=CARTESIAN_POINT('Ctrl Pts',(-1.35705080756892,2.62370823081419E-15,
9.87500000000001));
#421970=CARTESIAN_POINT('Ctrl Pts',(-1.01778810567669,-0.587620236790433,
9.91666666666668));
#421971=CARTESIAN_POINT('Ctrl Pts',(-0.67852540378446,-1.17524047358087,
9.95833333333334));
#421972=CARTESIAN_POINT('Ctrl Pts',(-1.43925448419923E-16,-1.17524047358087,
10.));
#421973=CARTESIAN_POINT('Ctrl Pts',(0.678525403784459,-1.17524047358087,
10.0416666666667));
#421974=CARTESIAN_POINT('Ctrl Pts',(1.01778810567669,-0.587620236790434,
10.0833333333333));
#421975=CARTESIAN_POINT('Ctrl Pts',(1.35705080756892,2.29132664526027E-15,
10.125));
#421976=CARTESIAN_POINT('Ctrl Pts',(1.01778810567669,0.587620236790438,
10.1666666666667));
#421977=CARTESIAN_POINT('Ctrl Pts',(0.67852540378446,1.17524047358087,10.2083333333333));
#421978=CARTESIAN_POINT('Ctrl Pts',(0.,1.17524047358087,10.25));
#421979=CARTESIAN_POINT('Ctrl Pts',(-0.678525403784459,1.17524047358087,
10.2916666666667));
#421980=CARTESIAN_POINT('Ctrl Pts',(-1.01778810567669,0.587620236790438,
10.3333333333333));
#421981=CARTESIAN_POINT('Ctrl Pts',(-1.35705080756892,2.62370823081419E-15,
10.375));
#421982=CARTESIAN_POINT('Ctrl Pts',(-1.01778810567669,-0.587620236790433,
10.4166666666667));
#421983=CARTESIAN_POINT('Ctrl Pts',(-0.67852540378446,-1.17524047358087,
10.4583333333333));
#421984=CARTESIAN_POINT('Ctrl Pts',(-1.43925448419923E-16,-1.17524047358087,
10.5));
#421985=CARTESIAN_POINT('Ctrl Pts',(0.678525403784459,-1.17524047358087,
10.5416666666667));
#421986=CARTESIAN_POINT('Ctrl Pts',(1.01778810567669,-0.587620236790434,
10.5833333333333));
#421987=CARTESIAN_POINT('Ctrl Pts',(1.35705080756892,2.29132664526027E-15,
10.625));
#421988=CARTESIAN_POINT('Ctrl Pts',(1.01778810567669,0.587620236790438,
10.6666666666667));
#421989=CARTESIAN_POINT('Ctrl Pts',(0.67852540378446,1.17524047358087,10.7083333333333));
#421990=CARTESIAN_POINT('Ctrl Pts',(0.,1.17524047358087,10.75));
#421991=CARTESIAN_POINT('Ctrl Pts',(-0.678525403784459,1.17524047358087,
10.7916666666667));
#421992=CARTESIAN_POINT('Ctrl Pts',(-1.01778810567669,0.587620236790438,
10.8333333333333));
#421993=CARTESIAN_POINT('Ctrl Pts',(-1.35705080756892,2.62370823081419E-15,
10.875));
#421994=CARTESIAN_POINT('Ctrl Pts',(-1.01778810567669,-0.587620236790433,
10.9166666666667));
#421995=CARTESIAN_POINT('Ctrl Pts',(-0.67852540378446,-1.17524047358087,
10.9583333333333));
#421996=CARTESIAN_POINT('Ctrl Pts',(-1.43925448419923E-16,-1.17524047358087,
11.));
#421997=CARTESIAN_POINT('Ctrl Pts',(0.678525403784459,-1.17524047358087,
11.0416666666667));
#421998=CARTESIAN_POINT('Ctrl Pts',(1.01778810567669,-0.587620236790434,
11.0833333333333));
#421999=CARTESIAN_POINT('Ctrl Pts',(1.35705080756892,2.29132664526027E-15,
11.125));
#422000=CARTESIAN_POINT('Ctrl Pts',(1.01778810567669,0.587620236790438,
11.1666666666667));
#422001=CARTESIAN_POINT('Ctrl Pts',(0.67852540378446,1.17524047358087,11.2083333333333));
#422002=CARTESIAN_POINT('Ctrl Pts',(0.,1.17524047358087,11.25));
#422003=CARTESIAN_POINT('Ctrl Pts',(0.,1.52706329386832,-14.453125));
#422004=CARTESIAN_POINT('Ctrl Pts',(-0.881650403784468,1.52706329386832,
-14.4114583333333));
#422005=CARTESIAN_POINT('Ctrl Pts',(-1.3224756056767,0.76353164693416,-14.3697916666667));
#422006=CARTESIAN_POINT('Ctrl Pts',(-1.76330080756894,2.64858386892187E-15,
-14.328125));
#422007=CARTESIAN_POINT('Ctrl Pts',(-1.3224756056767,-0.763531646934155,
-14.2864583333333));
#422008=CARTESIAN_POINT('Ctrl Pts',(-0.881650403784469,-1.52706329386831,
-14.2447916666667));
#422009=CARTESIAN_POINT('Ctrl Pts',(-1.87011317493125E-16,-1.52706329386831,
-14.203125));
#422010=CARTESIAN_POINT('Ctrl Pts',(0.881650403784467,-1.52706329386831,
-14.1614583333333));
#422011=CARTESIAN_POINT('Ctrl Pts',(1.3224756056767,-0.763531646934156,
-14.1197916666667));
#422012=CARTESIAN_POINT('Ctrl Pts',(1.76330080756894,2.21669973093722E-15,
-14.078125));
#422013=CARTESIAN_POINT('Ctrl Pts',(1.3224756056767,0.763531646934159,-14.0364583333333));
#422014=CARTESIAN_POINT('Ctrl Pts',(0.881650403784469,1.52706329386832,
-13.9947916666667));
#422015=CARTESIAN_POINT('Ctrl Pts',(0.,1.52706329386832,-13.953125));
#422016=CARTESIAN_POINT('Ctrl Pts',(-0.881650403784468,1.52706329386832,
-13.9114583333333));
#422017=CARTESIAN_POINT('Ctrl Pts',(-1.3224756056767,0.76353164693416,-13.8697916666667));
#422018=CARTESIAN_POINT('Ctrl Pts',(-1.76330080756894,2.64858386892187E-15,
-13.828125));
#422019=CARTESIAN_POINT('Ctrl Pts',(-1.3224756056767,-0.763531646934155,
-13.7864583333333));
#422020=CARTESIAN_POINT('Ctrl Pts',(-0.881650403784469,-1.52706329386831,
-13.7447916666667));
#422021=CARTESIAN_POINT('Ctrl Pts',(-1.87011317493125E-16,-1.52706329386831,
-13.703125));
#422022=CARTESIAN_POINT('Ctrl Pts',(0.881650403784467,-1.52706329386831,
-13.6614583333333));
#422023=CARTESIAN_POINT('Ctrl Pts',(1.3224756056767,-0.763531646934156,
-13.6197916666667));
#422024=CARTESIAN_POINT('Ctrl Pts',(1.76330080756894,2.21669973093722E-15,
-13.578125));
#422025=CARTESIAN_POINT('Ctrl Pts',(1.3224756056767,0.763531646934159,-13.5364583333333));
#422026=CARTESIAN_POINT('Ctrl Pts',(0.881650403784469,1.52706329386832,
-13.4947916666667));
#422027=CARTESIAN_POINT('Ctrl Pts',(0.,1.52706329386832,-13.453125));
#422028=CARTESIAN_POINT('Ctrl Pts',(-0.881650403784468,1.52706329386832,
-13.4114583333333));
#422029=CARTESIAN_POINT('Ctrl Pts',(-1.3224756056767,0.76353164693416,-13.3697916666667));
#422030=CARTESIAN_POINT('Ctrl Pts',(-1.76330080756894,2.64858386892187E-15,
-13.328125));
#422031=CARTESIAN_POINT('Ctrl Pts',(-1.3224756056767,-0.763531646934155,
-13.2864583333333));
#422032=CARTESIAN_POINT('Ctrl Pts',(-0.881650403784469,-1.52706329386831,
-13.2447916666667));
#422033=CARTESIAN_POINT('Ctrl Pts',(-1.87011317493125E-16,-1.52706329386831,
-13.203125));
#422034=CARTESIAN_POINT('Ctrl Pts',(0.881650403784467,-1.52706329386831,
-13.1614583333333));
#422035=CARTESIAN_POINT('Ctrl Pts',(1.3224756056767,-0.763531646934156,
-13.1197916666667));
#422036=CARTESIAN_POINT('Ctrl Pts',(1.76330080756894,2.21669973093722E-15,
-13.078125));
#422037=CARTESIAN_POINT('Ctrl Pts',(1.3224756056767,0.763531646934159,-13.0364583333333));
#422038=CARTESIAN_POINT('Ctrl Pts',(0.881650403784469,1.52706329386832,
-12.9947916666667));
#422039=CARTESIAN_POINT('Ctrl Pts',(0.,1.52706329386832,-12.953125));
#422040=CARTESIAN_POINT('Ctrl Pts',(-0.881650403784468,1.52706329386832,
-12.9114583333333));
#422041=CARTESIAN_POINT('Ctrl Pts',(-1.3224756056767,0.76353164693416,-12.8697916666667));
#422042=CARTESIAN_POINT('Ctrl Pts',(-1.76330080756894,2.64858386892187E-15,
-12.828125));
#422043=CARTESIAN_POINT('Ctrl Pts',(-1.3224756056767,-0.763531646934155,
-12.7864583333333));
#422044=CARTESIAN_POINT('Ctrl Pts',(-0.881650403784469,-1.52706329386831,
-12.7447916666667));
#422045=CARTESIAN_POINT('Ctrl Pts',(-1.87011317493125E-16,-1.52706329386831,
-12.703125));
#422046=CARTESIAN_POINT('Ctrl Pts',(0.881650403784467,-1.52706329386831,
-12.6614583333333));
#422047=CARTESIAN_POINT('Ctrl Pts',(1.3224756056767,-0.763531646934156,
-12.6197916666667));
#422048=CARTESIAN_POINT('Ctrl Pts',(1.76330080756894,2.21669973093722E-15,
-12.578125));
#422049=CARTESIAN_POINT('Ctrl Pts',(1.3224756056767,0.763531646934159,-12.5364583333333));
#422050=CARTESIAN_POINT('Ctrl Pts',(0.881650403784469,1.52706329386832,
-12.4947916666667));
#422051=CARTESIAN_POINT('Ctrl Pts',(0.,1.52706329386832,-12.453125));
#422052=CARTESIAN_POINT('Ctrl Pts',(-0.881650403784468,1.52706329386832,
-12.4114583333333));
#422053=CARTESIAN_POINT('Ctrl Pts',(-1.3224756056767,0.76353164693416,-12.3697916666667));
#422054=CARTESIAN_POINT('Ctrl Pts',(-1.76330080756894,2.64858386892187E-15,
-12.328125));
#422055=CARTESIAN_POINT('Ctrl Pts',(-1.3224756056767,-0.763531646934155,
-12.2864583333333));
#422056=CARTESIAN_POINT('Ctrl Pts',(-0.881650403784469,-1.52706329386831,
-12.2447916666667));
#422057=CARTESIAN_POINT('Ctrl Pts',(-1.87011317493125E-16,-1.52706329386831,
-12.203125));
#422058=CARTESIAN_POINT('Ctrl Pts',(0.881650403784467,-1.52706329386831,
-12.1614583333333));
#422059=CARTESIAN_POINT('Ctrl Pts',(1.3224756056767,-0.763531646934156,
-12.1197916666667));
#422060=CARTESIAN_POINT('Ctrl Pts',(1.76330080756894,2.21669973093722E-15,
-12.078125));
#422061=CARTESIAN_POINT('Ctrl Pts',(1.3224756056767,0.763531646934159,-12.0364583333333));
#422062=CARTESIAN_POINT('Ctrl Pts',(0.881650403784469,1.52706329386832,
-11.9947916666667));
#422063=CARTESIAN_POINT('Ctrl Pts',(0.,1.52706329386832,-11.953125));
#422064=CARTESIAN_POINT('Ctrl Pts',(-0.881650403784468,1.52706329386832,
-11.9114583333333));
#422065=CARTESIAN_POINT('Ctrl Pts',(-1.3224756056767,0.76353164693416,-11.8697916666667));
#422066=CARTESIAN_POINT('Ctrl Pts',(-1.76330080756894,2.64858386892187E-15,
-11.828125));
#422067=CARTESIAN_POINT('Ctrl Pts',(-1.3224756056767,-0.763531646934155,
-11.7864583333333));
#422068=CARTESIAN_POINT('Ctrl Pts',(-0.881650403784469,-1.52706329386831,
-11.7447916666667));
#422069=CARTESIAN_POINT('Ctrl Pts',(-1.87011317493125E-16,-1.52706329386831,
-11.703125));
#422070=CARTESIAN_POINT('Ctrl Pts',(0.881650403784467,-1.52706329386831,
-11.6614583333333));
#422071=CARTESIAN_POINT('Ctrl Pts',(1.3224756056767,-0.763531646934156,
-11.6197916666667));
#422072=CARTESIAN_POINT('Ctrl Pts',(1.76330080756894,2.21669973093722E-15,
-11.578125));
#422073=CARTESIAN_POINT('Ctrl Pts',(1.3224756056767,0.763531646934159,-11.5364583333333));
#422074=CARTESIAN_POINT('Ctrl Pts',(0.881650403784469,1.52706329386832,
-11.4947916666667));
#422075=CARTESIAN_POINT('Ctrl Pts',(0.,1.52706329386832,-11.453125));
#422076=CARTESIAN_POINT('Ctrl Pts',(-0.881650403784468,1.52706329386832,
-11.4114583333333));
#422077=CARTESIAN_POINT('Ctrl Pts',(-1.3224756056767,0.76353164693416,-11.3697916666667));
#422078=CARTESIAN_POINT('Ctrl Pts',(-1.76330080756894,2.64858386892187E-15,
-11.328125));
#422079=CARTESIAN_POINT('Ctrl Pts',(-1.3224756056767,-0.763531646934155,
-11.2864583333333));
#422080=CARTESIAN_POINT('Ctrl Pts',(-0.881650403784469,-1.52706329386831,
-11.2447916666667));
#422081=CARTESIAN_POINT('Ctrl Pts',(-1.87011317493125E-16,-1.52706329386831,
-11.203125));
#422082=CARTESIAN_POINT('Ctrl Pts',(0.881650403784467,-1.52706329386831,
-11.1614583333333));
#422083=CARTESIAN_POINT('Ctrl Pts',(1.3224756056767,-0.763531646934156,
-11.1197916666667));
#422084=CARTESIAN_POINT('Ctrl Pts',(1.76330080756894,2.21669973093722E-15,
-11.078125));
#422085=CARTESIAN_POINT('Ctrl Pts',(1.3224756056767,0.763531646934159,-11.0364583333333));
#422086=CARTESIAN_POINT('Ctrl Pts',(0.881650403784469,1.52706329386832,
-10.9947916666667));
#422087=CARTESIAN_POINT('Ctrl Pts',(0.,1.52706329386832,-10.953125));
#422088=CARTESIAN_POINT('Ctrl Pts',(-0.881650403784468,1.52706329386832,
-10.9114583333333));
#422089=CARTESIAN_POINT('Ctrl Pts',(-1.3224756056767,0.76353164693416,-10.8697916666667));
#422090=CARTESIAN_POINT('Ctrl Pts',(-1.76330080756894,2.64858386892187E-15,
-10.828125));
#422091=CARTESIAN_POINT('Ctrl Pts',(-1.3224756056767,-0.763531646934155,
-10.7864583333333));
#422092=CARTESIAN_POINT('Ctrl Pts',(-0.881650403784469,-1.52706329386831,
-10.7447916666667));
#422093=CARTESIAN_POINT('Ctrl Pts',(-1.87011317493125E-16,-1.52706329386831,
-10.703125));
#422094=CARTESIAN_POINT('Ctrl Pts',(0.881650403784467,-1.52706329386831,
-10.6614583333333));
#422095=CARTESIAN_POINT('Ctrl Pts',(1.3224756056767,-0.763531646934156,
-10.6197916666667));
#422096=CARTESIAN_POINT('Ctrl Pts',(1.76330080756894,2.21669973093722E-15,
-10.578125));
#422097=CARTESIAN_POINT('Ctrl Pts',(1.3224756056767,0.763531646934159,-10.5364583333333));
#422098=CARTESIAN_POINT('Ctrl Pts',(0.881650403784469,1.52706329386832,
-10.4947916666667));
#422099=CARTESIAN_POINT('Ctrl Pts',(0.,1.52706329386832,-10.453125));
#422100=CARTESIAN_POINT('Ctrl Pts',(-0.881650403784468,1.52706329386832,
-10.4114583333333));
#422101=CARTESIAN_POINT('Ctrl Pts',(-1.3224756056767,0.76353164693416,-10.3697916666667));
#422102=CARTESIAN_POINT('Ctrl Pts',(-1.76330080756894,2.64858386892187E-15,
-10.328125));
#422103=CARTESIAN_POINT('Ctrl Pts',(-1.3224756056767,-0.763531646934155,
-10.2864583333333));
#422104=CARTESIAN_POINT('Ctrl Pts',(-0.881650403784469,-1.52706329386831,
-10.2447916666667));
#422105=CARTESIAN_POINT('Ctrl Pts',(-1.87011317493125E-16,-1.52706329386831,
-10.203125));
#422106=CARTESIAN_POINT('Ctrl Pts',(0.881650403784467,-1.52706329386831,
-10.1614583333333));
#422107=CARTESIAN_POINT('Ctrl Pts',(1.3224756056767,-0.763531646934156,
-10.1197916666667));
#422108=CARTESIAN_POINT('Ctrl Pts',(1.76330080756894,2.21669973093722E-15,
-10.078125));
#422109=CARTESIAN_POINT('Ctrl Pts',(1.3224756056767,0.763531646934159,-10.0364583333333));
#422110=CARTESIAN_POINT('Ctrl Pts',(0.881650403784469,1.52706329386832,
-9.99479166666667));
#422111=CARTESIAN_POINT('Ctrl Pts',(0.,1.52706329386832,-9.953125));
#422112=CARTESIAN_POINT('Ctrl Pts',(-0.881650403784468,1.52706329386832,
-9.91145833333333));
#422113=CARTESIAN_POINT('Ctrl Pts',(-1.3224756056767,0.76353164693416,-9.86979166666667));
#422114=CARTESIAN_POINT('Ctrl Pts',(-1.76330080756894,2.64858386892187E-15,
-9.828125));
#422115=CARTESIAN_POINT('Ctrl Pts',(-1.3224756056767,-0.763531646934155,
-9.78645833333333));
#422116=CARTESIAN_POINT('Ctrl Pts',(-0.881650403784469,-1.52706329386831,
-9.74479166666667));
#422117=CARTESIAN_POINT('Ctrl Pts',(-1.87011317493125E-16,-1.52706329386831,
-9.703125));
#422118=CARTESIAN_POINT('Ctrl Pts',(0.881650403784467,-1.52706329386831,
-9.66145833333333));
#422119=CARTESIAN_POINT('Ctrl Pts',(1.3224756056767,-0.763531646934156,
-9.61979166666667));
#422120=CARTESIAN_POINT('Ctrl Pts',(1.76330080756894,2.21669973093722E-15,
-9.578125));
#422121=CARTESIAN_POINT('Ctrl Pts',(1.3224756056767,0.763531646934159,-9.53645833333333));
#422122=CARTESIAN_POINT('Ctrl Pts',(0.881650403784469,1.52706329386832,
-9.49479166666666));
#422123=CARTESIAN_POINT('Ctrl Pts',(0.,1.52706329386832,-9.453125));
#422124=CARTESIAN_POINT('Ctrl Pts',(-0.881650403784468,1.52706329386832,
-9.41145833333333));
#422125=CARTESIAN_POINT('Ctrl Pts',(-1.3224756056767,0.76353164693416,-9.36979166666666));
#422126=CARTESIAN_POINT('Ctrl Pts',(-1.76330080756894,2.64858386892187E-15,
-9.328125));
#422127=CARTESIAN_POINT('Ctrl Pts',(-1.3224756056767,-0.763531646934155,
-9.28645833333333));
#422128=CARTESIAN_POINT('Ctrl Pts',(-0.881650403784469,-1.52706329386831,
-9.24479166666667));
#422129=CARTESIAN_POINT('Ctrl Pts',(-1.87011317493125E-16,-1.52706329386831,
-9.203125));
#422130=CARTESIAN_POINT('Ctrl Pts',(0.881650403784467,-1.52706329386831,
-9.16145833333333));
#422131=CARTESIAN_POINT('Ctrl Pts',(1.3224756056767,-0.763531646934156,
-9.11979166666666));
#422132=CARTESIAN_POINT('Ctrl Pts',(1.76330080756894,2.21669973093722E-15,
-9.078125));
#422133=CARTESIAN_POINT('Ctrl Pts',(1.3224756056767,0.763531646934159,-9.03645833333333));
#422134=CARTESIAN_POINT('Ctrl Pts',(0.881650403784469,1.52706329386832,
-8.99479166666666));
#422135=CARTESIAN_POINT('Ctrl Pts',(0.,1.52706329386832,-8.953125));
#422136=CARTESIAN_POINT('Ctrl Pts',(-0.881650403784468,1.52706329386832,
-8.91145833333333));
#422137=CARTESIAN_POINT('Ctrl Pts',(-1.3224756056767,0.76353164693416,-8.86979166666666));
#422138=CARTESIAN_POINT('Ctrl Pts',(-1.76330080756894,2.64858386892187E-15,
-8.828125));
#422139=CARTESIAN_POINT('Ctrl Pts',(-1.3224756056767,-0.763531646934155,
-8.78645833333333));
#422140=CARTESIAN_POINT('Ctrl Pts',(-0.881650403784469,-1.52706329386831,
-8.74479166666666));
#422141=CARTESIAN_POINT('Ctrl Pts',(-1.87011317493125E-16,-1.52706329386831,
-8.703125));
#422142=CARTESIAN_POINT('Ctrl Pts',(0.881650403784467,-1.52706329386831,
-8.66145833333333));
#422143=CARTESIAN_POINT('Ctrl Pts',(1.3224756056767,-0.763531646934156,
-8.61979166666667));
#422144=CARTESIAN_POINT('Ctrl Pts',(1.76330080756894,2.21669973093722E-15,
-8.578125));
#422145=CARTESIAN_POINT('Ctrl Pts',(1.3224756056767,0.763531646934159,-8.53645833333333));
#422146=CARTESIAN_POINT('Ctrl Pts',(0.881650403784469,1.52706329386832,
-8.49479166666667));
#422147=CARTESIAN_POINT('Ctrl Pts',(0.,1.52706329386832,-8.453125));
#422148=CARTESIAN_POINT('Ctrl Pts',(-0.881650403784468,1.52706329386832,
-8.41145833333333));
#422149=CARTESIAN_POINT('Ctrl Pts',(-1.3224756056767,0.76353164693416,-8.36979166666667));
#422150=CARTESIAN_POINT('Ctrl Pts',(-1.76330080756894,2.64858386892187E-15,
-8.328125));
#422151=CARTESIAN_POINT('Ctrl Pts',(-1.3224756056767,-0.763531646934155,
-8.28645833333333));
#422152=CARTESIAN_POINT('Ctrl Pts',(-0.881650403784469,-1.52706329386831,
-8.24479166666667));
#422153=CARTESIAN_POINT('Ctrl Pts',(-1.87011317493125E-16,-1.52706329386831,
-8.203125));
#422154=CARTESIAN_POINT('Ctrl Pts',(0.881650403784467,-1.52706329386831,
-8.16145833333333));
#422155=CARTESIAN_POINT('Ctrl Pts',(1.3224756056767,-0.763531646934156,
-8.11979166666667));
#422156=CARTESIAN_POINT('Ctrl Pts',(1.76330080756894,2.21669973093722E-15,
-8.078125));
#422157=CARTESIAN_POINT('Ctrl Pts',(1.3224756056767,0.763531646934159,-8.03645833333333));
#422158=CARTESIAN_POINT('Ctrl Pts',(0.881650403784469,1.52706329386832,
-7.99479166666667));
#422159=CARTESIAN_POINT('Ctrl Pts',(0.,1.52706329386832,-7.953125));
#422160=CARTESIAN_POINT('Ctrl Pts',(-0.881650403784468,1.52706329386832,
-7.91145833333333));
#422161=CARTESIAN_POINT('Ctrl Pts',(-1.3224756056767,0.76353164693416,-7.86979166666667));
#422162=CARTESIAN_POINT('Ctrl Pts',(-1.76330080756894,2.64858386892187E-15,
-7.828125));
#422163=CARTESIAN_POINT('Ctrl Pts',(-1.3224756056767,-0.763531646934155,
-7.78645833333333));
#422164=CARTESIAN_POINT('Ctrl Pts',(-0.881650403784469,-1.52706329386831,
-7.74479166666667));
#422165=CARTESIAN_POINT('Ctrl Pts',(-1.87011317493125E-16,-1.52706329386831,
-7.703125));
#422166=CARTESIAN_POINT('Ctrl Pts',(0.881650403784467,-1.52706329386831,
-7.66145833333333));
#422167=CARTESIAN_POINT('Ctrl Pts',(1.3224756056767,-0.763531646934156,
-7.61979166666667));
#422168=CARTESIAN_POINT('Ctrl Pts',(1.76330080756894,2.21669973093722E-15,
-7.578125));
#422169=CARTESIAN_POINT('Ctrl Pts',(1.3224756056767,0.763531646934159,-7.53645833333333));
#422170=CARTESIAN_POINT('Ctrl Pts',(0.881650403784469,1.52706329386832,
-7.49479166666667));
#422171=CARTESIAN_POINT('Ctrl Pts',(0.,1.52706329386832,-7.453125));
#422172=CARTESIAN_POINT('Ctrl Pts',(-0.881650403784468,1.52706329386832,
-7.41145833333333));
#422173=CARTESIAN_POINT('Ctrl Pts',(-1.3224756056767,0.76353164693416,-7.36979166666667));
#422174=CARTESIAN_POINT('Ctrl Pts',(-1.76330080756894,2.64858386892187E-15,
-7.328125));
#422175=CARTESIAN_POINT('Ctrl Pts',(-1.3224756056767,-0.763531646934155,
-7.28645833333333));
#422176=CARTESIAN_POINT('Ctrl Pts',(-0.881650403784469,-1.52706329386831,
-7.24479166666667));
#422177=CARTESIAN_POINT('Ctrl Pts',(-1.87011317493125E-16,-1.52706329386831,
-7.203125));
#422178=CARTESIAN_POINT('Ctrl Pts',(0.881650403784467,-1.52706329386831,
-7.16145833333333));
#422179=CARTESIAN_POINT('Ctrl Pts',(1.3224756056767,-0.763531646934156,
-7.11979166666667));
#422180=CARTESIAN_POINT('Ctrl Pts',(1.76330080756894,2.21669973093722E-15,
-7.078125));
#422181=CARTESIAN_POINT('Ctrl Pts',(1.3224756056767,0.763531646934159,-7.03645833333333));
#422182=CARTESIAN_POINT('Ctrl Pts',(0.881650403784469,1.52706329386832,
-6.99479166666667));
#422183=CARTESIAN_POINT('Ctrl Pts',(0.,1.52706329386832,-6.953125));
#422184=CARTESIAN_POINT('Ctrl Pts',(-0.881650403784468,1.52706329386832,
-6.91145833333333));
#422185=CARTESIAN_POINT('Ctrl Pts',(-1.3224756056767,0.76353164693416,-6.86979166666667));
#422186=CARTESIAN_POINT('Ctrl Pts',(-1.76330080756894,2.64858386892187E-15,
-6.828125));
#422187=CARTESIAN_POINT('Ctrl Pts',(-1.3224756056767,-0.763531646934155,
-6.78645833333333));
#422188=CARTESIAN_POINT('Ctrl Pts',(-0.881650403784469,-1.52706329386831,
-6.74479166666667));
#422189=CARTESIAN_POINT('Ctrl Pts',(-1.87011317493125E-16,-1.52706329386831,
-6.703125));
#422190=CARTESIAN_POINT('Ctrl Pts',(0.881650403784467,-1.52706329386831,
-6.66145833333333));
#422191=CARTESIAN_POINT('Ctrl Pts',(1.3224756056767,-0.763531646934156,
-6.61979166666667));
#422192=CARTESIAN_POINT('Ctrl Pts',(1.76330080756894,2.21669973093722E-15,
-6.578125));
#422193=CARTESIAN_POINT('Ctrl Pts',(1.3224756056767,0.763531646934159,-6.53645833333333));
#422194=CARTESIAN_POINT('Ctrl Pts',(0.881650403784469,1.52706329386832,
-6.49479166666667));
#422195=CARTESIAN_POINT('Ctrl Pts',(0.,1.52706329386832,-6.453125));
#422196=CARTESIAN_POINT('Ctrl Pts',(-0.881650403784468,1.52706329386832,
-6.41145833333333));
#422197=CARTESIAN_POINT('Ctrl Pts',(-1.3224756056767,0.76353164693416,-6.36979166666667));
#422198=CARTESIAN_POINT('Ctrl Pts',(-1.76330080756894,2.64858386892187E-15,
-6.328125));
#422199=CARTESIAN_POINT('Ctrl Pts',(-1.3224756056767,-0.763531646934155,
-6.28645833333333));
#422200=CARTESIAN_POINT('Ctrl Pts',(-0.881650403784469,-1.52706329386831,
-6.24479166666667));
#422201=CARTESIAN_POINT('Ctrl Pts',(-1.87011317493125E-16,-1.52706329386831,
-6.203125));
#422202=CARTESIAN_POINT('Ctrl Pts',(0.881650403784467,-1.52706329386831,
-6.16145833333333));
#422203=CARTESIAN_POINT('Ctrl Pts',(1.3224756056767,-0.763531646934156,
-6.11979166666667));
#422204=CARTESIAN_POINT('Ctrl Pts',(1.76330080756894,2.21669973093722E-15,
-6.078125));
#422205=CARTESIAN_POINT('Ctrl Pts',(1.3224756056767,0.763531646934159,-6.03645833333333));
#422206=CARTESIAN_POINT('Ctrl Pts',(0.881650403784469,1.52706329386832,
-5.99479166666667));
#422207=CARTESIAN_POINT('Ctrl Pts',(0.,1.52706329386832,-5.953125));
#422208=CARTESIAN_POINT('Ctrl Pts',(-0.881650403784468,1.52706329386832,
-5.91145833333333));
#422209=CARTESIAN_POINT('Ctrl Pts',(-1.3224756056767,0.76353164693416,-5.86979166666667));
#422210=CARTESIAN_POINT('Ctrl Pts',(-1.76330080756894,2.64858386892187E-15,
-5.828125));
#422211=CARTESIAN_POINT('Ctrl Pts',(-1.3224756056767,-0.763531646934155,
-5.78645833333333));
#422212=CARTESIAN_POINT('Ctrl Pts',(-0.881650403784469,-1.52706329386831,
-5.74479166666667));
#422213=CARTESIAN_POINT('Ctrl Pts',(-1.87011317493125E-16,-1.52706329386831,
-5.703125));
#422214=CARTESIAN_POINT('Ctrl Pts',(0.881650403784467,-1.52706329386831,
-5.66145833333333));
#422215=CARTESIAN_POINT('Ctrl Pts',(1.3224756056767,-0.763531646934156,
-5.61979166666667));
#422216=CARTESIAN_POINT('Ctrl Pts',(1.76330080756894,2.21669973093722E-15,
-5.578125));
#422217=CARTESIAN_POINT('Ctrl Pts',(1.3224756056767,0.763531646934159,-5.53645833333333));
#422218=CARTESIAN_POINT('Ctrl Pts',(0.881650403784469,1.52706329386832,
-5.49479166666667));
#422219=CARTESIAN_POINT('Ctrl Pts',(0.,1.52706329386832,-5.453125));
#422220=CARTESIAN_POINT('Ctrl Pts',(-0.881650403784468,1.52706329386832,
-5.41145833333333));
#422221=CARTESIAN_POINT('Ctrl Pts',(-1.3224756056767,0.76353164693416,-5.36979166666667));
#422222=CARTESIAN_POINT('Ctrl Pts',(-1.76330080756894,2.64858386892187E-15,
-5.328125));
#422223=CARTESIAN_POINT('Ctrl Pts',(-1.3224756056767,-0.763531646934155,
-5.28645833333333));
#422224=CARTESIAN_POINT('Ctrl Pts',(-0.881650403784469,-1.52706329386831,
-5.24479166666667));
#422225=CARTESIAN_POINT('Ctrl Pts',(-1.87011317493125E-16,-1.52706329386831,
-5.203125));
#422226=CARTESIAN_POINT('Ctrl Pts',(0.881650403784467,-1.52706329386831,
-5.16145833333333));
#422227=CARTESIAN_POINT('Ctrl Pts',(1.3224756056767,-0.763531646934156,
-5.11979166666667));
#422228=CARTESIAN_POINT('Ctrl Pts',(1.76330080756894,2.21669973093722E-15,
-5.078125));
#422229=CARTESIAN_POINT('Ctrl Pts',(1.3224756056767,0.763531646934159,-5.03645833333333));
#422230=CARTESIAN_POINT('Ctrl Pts',(0.881650403784469,1.52706329386832,
-4.99479166666667));
#422231=CARTESIAN_POINT('Ctrl Pts',(0.,1.52706329386832,-4.953125));
#422232=CARTESIAN_POINT('Ctrl Pts',(-0.881650403784468,1.52706329386832,
-4.91145833333333));
#422233=CARTESIAN_POINT('Ctrl Pts',(-1.3224756056767,0.76353164693416,-4.86979166666667));
#422234=CARTESIAN_POINT('Ctrl Pts',(-1.76330080756894,2.64858386892187E-15,
-4.828125));
#422235=CARTESIAN_POINT('Ctrl Pts',(-1.3224756056767,-0.763531646934155,
-4.78645833333333));
#422236=CARTESIAN_POINT('Ctrl Pts',(-0.881650403784469,-1.52706329386831,
-4.74479166666667));
#422237=CARTESIAN_POINT('Ctrl Pts',(-1.87011317493125E-16,-1.52706329386831,
-4.703125));
#422238=CARTESIAN_POINT('Ctrl Pts',(0.881650403784467,-1.52706329386831,
-4.66145833333333));
#422239=CARTESIAN_POINT('Ctrl Pts',(1.3224756056767,-0.763531646934156,
-4.61979166666667));
#422240=CARTESIAN_POINT('Ctrl Pts',(1.76330080756894,2.21669973093722E-15,
-4.578125));
#422241=CARTESIAN_POINT('Ctrl Pts',(1.3224756056767,0.763531646934159,-4.53645833333333));
#422242=CARTESIAN_POINT('Ctrl Pts',(0.881650403784469,1.52706329386832,
-4.49479166666667));
#422243=CARTESIAN_POINT('Ctrl Pts',(0.,1.52706329386832,-4.453125));
#422244=CARTESIAN_POINT('Ctrl Pts',(-0.881650403784468,1.52706329386832,
-4.41145833333333));
#422245=CARTESIAN_POINT('Ctrl Pts',(-1.3224756056767,0.76353164693416,-4.36979166666667));
#422246=CARTESIAN_POINT('Ctrl Pts',(-1.76330080756894,2.64858386892187E-15,
-4.328125));
#422247=CARTESIAN_POINT('Ctrl Pts',(-1.3224756056767,-0.763531646934155,
-4.28645833333333));
#422248=CARTESIAN_POINT('Ctrl Pts',(-0.881650403784469,-1.52706329386831,
-4.24479166666667));
#422249=CARTESIAN_POINT('Ctrl Pts',(-1.87011317493125E-16,-1.52706329386831,
-4.203125));
#422250=CARTESIAN_POINT('Ctrl Pts',(0.881650403784467,-1.52706329386831,
-4.16145833333333));
#422251=CARTESIAN_POINT('Ctrl Pts',(1.3224756056767,-0.763531646934156,
-4.11979166666667));
#422252=CARTESIAN_POINT('Ctrl Pts',(1.76330080756894,2.21669973093722E-15,
-4.078125));
#422253=CARTESIAN_POINT('Ctrl Pts',(1.3224756056767,0.763531646934159,-4.03645833333333));
#422254=CARTESIAN_POINT('Ctrl Pts',(0.881650403784469,1.52706329386832,
-3.99479166666667));
#422255=CARTESIAN_POINT('Ctrl Pts',(0.,1.52706329386832,-3.953125));
#422256=CARTESIAN_POINT('Ctrl Pts',(-0.881650403784468,1.52706329386832,
-3.91145833333333));
#422257=CARTESIAN_POINT('Ctrl Pts',(-1.3224756056767,0.76353164693416,-3.86979166666667));
#422258=CARTESIAN_POINT('Ctrl Pts',(-1.76330080756894,2.64858386892187E-15,
-3.828125));
#422259=CARTESIAN_POINT('Ctrl Pts',(-1.3224756056767,-0.763531646934155,
-3.78645833333333));
#422260=CARTESIAN_POINT('Ctrl Pts',(-0.881650403784469,-1.52706329386831,
-3.74479166666667));
#422261=CARTESIAN_POINT('Ctrl Pts',(-1.87011317493125E-16,-1.52706329386831,
-3.703125));
#422262=CARTESIAN_POINT('Ctrl Pts',(0.881650403784467,-1.52706329386831,
-3.66145833333333));
#422263=CARTESIAN_POINT('Ctrl Pts',(1.3224756056767,-0.763531646934156,
-3.61979166666667));
#422264=CARTESIAN_POINT('Ctrl Pts',(1.76330080756894,2.21669973093722E-15,
-3.578125));
#422265=CARTESIAN_POINT('Ctrl Pts',(1.3224756056767,0.763531646934159,-3.53645833333333));
#422266=CARTESIAN_POINT('Ctrl Pts',(0.881650403784469,1.52706329386832,
-3.49479166666667));
#422267=CARTESIAN_POINT('Ctrl Pts',(0.,1.52706329386832,-3.453125));
#422268=CARTESIAN_POINT('Ctrl Pts',(-0.881650403784468,1.52706329386832,
-3.41145833333333));
#422269=CARTESIAN_POINT('Ctrl Pts',(-1.3224756056767,0.76353164693416,-3.36979166666667));
#422270=CARTESIAN_POINT('Ctrl Pts',(-1.76330080756894,2.64858386892187E-15,
-3.328125));
#422271=CARTESIAN_POINT('Ctrl Pts',(-1.3224756056767,-0.763531646934155,
-3.28645833333333));
#422272=CARTESIAN_POINT('Ctrl Pts',(-0.881650403784469,-1.52706329386831,
-3.24479166666667));
#422273=CARTESIAN_POINT('Ctrl Pts',(-1.87011317493125E-16,-1.52706329386831,
-3.203125));
#422274=CARTESIAN_POINT('Ctrl Pts',(0.881650403784467,-1.52706329386831,
-3.16145833333333));
#422275=CARTESIAN_POINT('Ctrl Pts',(1.3224756056767,-0.763531646934156,
-3.11979166666667));
#422276=CARTESIAN_POINT('Ctrl Pts',(1.76330080756894,2.21669973093722E-15,
-3.078125));
#422277=CARTESIAN_POINT('Ctrl Pts',(1.3224756056767,0.763531646934159,-3.03645833333333));
#422278=CARTESIAN_POINT('Ctrl Pts',(0.881650403784469,1.52706329386832,
-2.99479166666667));
#422279=CARTESIAN_POINT('Ctrl Pts',(0.,1.52706329386832,-2.953125));
#422280=CARTESIAN_POINT('Ctrl Pts',(-0.881650403784468,1.52706329386832,
-2.91145833333333));
#422281=CARTESIAN_POINT('Ctrl Pts',(-1.3224756056767,0.76353164693416,-2.86979166666667));
#422282=CARTESIAN_POINT('Ctrl Pts',(-1.76330080756894,2.64858386892187E-15,
-2.828125));
#422283=CARTESIAN_POINT('Ctrl Pts',(-1.3224756056767,-0.763531646934155,
-2.78645833333333));
#422284=CARTESIAN_POINT('Ctrl Pts',(-0.881650403784469,-1.52706329386831,
-2.74479166666667));
#422285=CARTESIAN_POINT('Ctrl Pts',(-1.87011317493125E-16,-1.52706329386831,
-2.703125));
#422286=CARTESIAN_POINT('Ctrl Pts',(0.881650403784467,-1.52706329386831,
-2.66145833333333));
#422287=CARTESIAN_POINT('Ctrl Pts',(1.3224756056767,-0.763531646934156,
-2.61979166666667));
#422288=CARTESIAN_POINT('Ctrl Pts',(1.76330080756894,2.21669973093722E-15,
-2.578125));
#422289=CARTESIAN_POINT('Ctrl Pts',(1.3224756056767,0.763531646934159,-2.53645833333333));
#422290=CARTESIAN_POINT('Ctrl Pts',(0.881650403784469,1.52706329386832,
-2.49479166666667));
#422291=CARTESIAN_POINT('Ctrl Pts',(0.,1.52706329386832,-2.453125));
#422292=CARTESIAN_POINT('Ctrl Pts',(-0.881650403784468,1.52706329386832,
-2.41145833333333));
#422293=CARTESIAN_POINT('Ctrl Pts',(-1.3224756056767,0.76353164693416,-2.36979166666667));
#422294=CARTESIAN_POINT('Ctrl Pts',(-1.76330080756894,2.64858386892187E-15,
-2.328125));
#422295=CARTESIAN_POINT('Ctrl Pts',(-1.3224756056767,-0.763531646934155,
-2.28645833333333));
#422296=CARTESIAN_POINT('Ctrl Pts',(-0.881650403784469,-1.52706329386831,
-2.24479166666667));
#422297=CARTESIAN_POINT('Ctrl Pts',(-1.87011317493125E-16,-1.52706329386831,
-2.203125));
#422298=CARTESIAN_POINT('Ctrl Pts',(0.881650403784467,-1.52706329386831,
-2.16145833333333));
#422299=CARTESIAN_POINT('Ctrl Pts',(1.3224756056767,-0.763531646934156,
-2.11979166666667));
#422300=CARTESIAN_POINT('Ctrl Pts',(1.76330080756894,2.21669973093722E-15,
-2.078125));
#422301=CARTESIAN_POINT('Ctrl Pts',(1.3224756056767,0.763531646934159,-2.03645833333333));
#422302=CARTESIAN_POINT('Ctrl Pts',(0.881650403784469,1.52706329386832,
-1.99479166666667));
#422303=CARTESIAN_POINT('Ctrl Pts',(0.,1.52706329386832,-1.953125));
#422304=CARTESIAN_POINT('Ctrl Pts',(-0.881650403784468,1.52706329386832,
-1.91145833333333));
#422305=CARTESIAN_POINT('Ctrl Pts',(-1.3224756056767,0.76353164693416,-1.86979166666667));
#422306=CARTESIAN_POINT('Ctrl Pts',(-1.76330080756894,2.64858386892187E-15,
-1.828125));
#422307=CARTESIAN_POINT('Ctrl Pts',(-1.3224756056767,-0.763531646934155,
-1.78645833333333));
#422308=CARTESIAN_POINT('Ctrl Pts',(-0.881650403784469,-1.52706329386831,
-1.74479166666667));
#422309=CARTESIAN_POINT('Ctrl Pts',(-1.87011317493125E-16,-1.52706329386831,
-1.703125));
#422310=CARTESIAN_POINT('Ctrl Pts',(0.881650403784467,-1.52706329386831,
-1.66145833333333));
#422311=CARTESIAN_POINT('Ctrl Pts',(1.3224756056767,-0.763531646934156,
-1.61979166666667));
#422312=CARTESIAN_POINT('Ctrl Pts',(1.76330080756894,2.21669973093722E-15,
-1.578125));
#422313=CARTESIAN_POINT('Ctrl Pts',(1.3224756056767,0.763531646934159,-1.53645833333333));
#422314=CARTESIAN_POINT('Ctrl Pts',(0.881650403784469,1.52706329386832,
-1.49479166666667));
#422315=CARTESIAN_POINT('Ctrl Pts',(0.,1.52706329386832,-1.453125));
#422316=CARTESIAN_POINT('Ctrl Pts',(-0.881650403784468,1.52706329386832,
-1.41145833333333));
#422317=CARTESIAN_POINT('Ctrl Pts',(-1.3224756056767,0.76353164693416,-1.36979166666667));
#422318=CARTESIAN_POINT('Ctrl Pts',(-1.76330080756894,2.64858386892187E-15,
-1.328125));
#422319=CARTESIAN_POINT('Ctrl Pts',(-1.3224756056767,-0.763531646934155,
-1.28645833333333));
#422320=CARTESIAN_POINT('Ctrl Pts',(-0.881650403784469,-1.52706329386831,
-1.24479166666667));
#422321=CARTESIAN_POINT('Ctrl Pts',(-1.87011317493125E-16,-1.52706329386831,
-1.203125));
#422322=CARTESIAN_POINT('Ctrl Pts',(0.881650403784467,-1.52706329386831,
-1.16145833333333));
#422323=CARTESIAN_POINT('Ctrl Pts',(1.3224756056767,-0.763531646934156,
-1.11979166666667));
#422324=CARTESIAN_POINT('Ctrl Pts',(1.76330080756894,2.21669973093722E-15,
-1.078125));
#422325=CARTESIAN_POINT('Ctrl Pts',(1.3224756056767,0.763531646934159,-1.03645833333333));
#422326=CARTESIAN_POINT('Ctrl Pts',(0.881650403784469,1.52706329386832,
-0.994791666666666));
#422327=CARTESIAN_POINT('Ctrl Pts',(0.,1.52706329386832,-0.953124999999999));
#422328=CARTESIAN_POINT('Ctrl Pts',(-0.881650403784468,1.52706329386832,
-0.911458333333334));
#422329=CARTESIAN_POINT('Ctrl Pts',(-1.3224756056767,0.76353164693416,-0.869791666666666));
#422330=CARTESIAN_POINT('Ctrl Pts',(-1.76330080756894,2.64858386892187E-15,
-0.828124999999999));
#422331=CARTESIAN_POINT('Ctrl Pts',(-1.3224756056767,-0.763531646934155,
-0.786458333333334));
#422332=CARTESIAN_POINT('Ctrl Pts',(-0.881650403784469,-1.52706329386831,
-0.744791666666666));
#422333=CARTESIAN_POINT('Ctrl Pts',(-1.87011317493125E-16,-1.52706329386831,
-0.703124999999999));
#422334=CARTESIAN_POINT('Ctrl Pts',(0.881650403784467,-1.52706329386831,
-0.661458333333333));
#422335=CARTESIAN_POINT('Ctrl Pts',(1.3224756056767,-0.763531646934156,
-0.619791666666666));
#422336=CARTESIAN_POINT('Ctrl Pts',(1.76330080756894,2.21669973093722E-15,
-0.578124999999999));
#422337=CARTESIAN_POINT('Ctrl Pts',(1.3224756056767,0.763531646934159,-0.536458333333333));
#422338=CARTESIAN_POINT('Ctrl Pts',(0.881650403784469,1.52706329386832,
-0.494791666666666));
#422339=CARTESIAN_POINT('Ctrl Pts',(0.,1.52706329386832,-0.453124999999999));
#422340=CARTESIAN_POINT('Ctrl Pts',(-0.881650403784468,1.52706329386832,
-0.411458333333333));
#422341=CARTESIAN_POINT('Ctrl Pts',(-1.3224756056767,0.76353164693416,-0.369791666666666));
#422342=CARTESIAN_POINT('Ctrl Pts',(-1.76330080756894,2.64858386892187E-15,
-0.328125));
#422343=CARTESIAN_POINT('Ctrl Pts',(-1.3224756056767,-0.763531646934155,
-0.286458333333333));
#422344=CARTESIAN_POINT('Ctrl Pts',(-0.881650403784469,-1.52706329386831,
-0.244791666666666));
#422345=CARTESIAN_POINT('Ctrl Pts',(-1.87011317493125E-16,-1.52706329386831,
-0.203125));
#422346=CARTESIAN_POINT('Ctrl Pts',(0.881650403784467,-1.52706329386831,
-0.161458333333333));
#422347=CARTESIAN_POINT('Ctrl Pts',(1.3224756056767,-0.763531646934156,
-0.119791666666666));
#422348=CARTESIAN_POINT('Ctrl Pts',(1.76330080756894,2.21669973093722E-15,
-0.0781250000000001));
#422349=CARTESIAN_POINT('Ctrl Pts',(1.3224756056767,0.763531646934159,-0.0364583333333328));
#422350=CARTESIAN_POINT('Ctrl Pts',(0.881650403784469,1.52706329386832,
0.00520833333333449));
#422351=CARTESIAN_POINT('Ctrl Pts',(0.,1.52706329386832,0.046875));
#422352=CARTESIAN_POINT('Ctrl Pts',(-0.881650403784468,1.52706329386832,
0.0885416666666673));
#422353=CARTESIAN_POINT('Ctrl Pts',(-1.3224756056767,0.76353164693416,0.130208333333335));
#422354=CARTESIAN_POINT('Ctrl Pts',(-1.76330080756894,2.64858386892187E-15,
0.171875));
#422355=CARTESIAN_POINT('Ctrl Pts',(-1.3224756056767,-0.763531646934155,
0.213541666666667));
#422356=CARTESIAN_POINT('Ctrl Pts',(-0.881650403784469,-1.52706329386831,
0.255208333333335));
#422357=CARTESIAN_POINT('Ctrl Pts',(-1.87011317493125E-16,-1.52706329386831,
0.296875));
#422358=CARTESIAN_POINT('Ctrl Pts',(0.881650403784467,-1.52706329386831,
0.338541666666668));
#422359=CARTESIAN_POINT('Ctrl Pts',(1.3224756056767,-0.763531646934156,
0.380208333333333));
#422360=CARTESIAN_POINT('Ctrl Pts',(1.76330080756894,2.21669973093722E-15,
0.421875));
#422361=CARTESIAN_POINT('Ctrl Pts',(1.3224756056767,0.763531646934159,0.463541666666668));
#422362=CARTESIAN_POINT('Ctrl Pts',(0.881650403784469,1.52706329386832,
0.505208333333333));
#422363=CARTESIAN_POINT('Ctrl Pts',(0.,1.52706329386832,0.546875));
#422364=CARTESIAN_POINT('Ctrl Pts',(-0.881650403784468,1.52706329386832,
0.588541666666668));
#422365=CARTESIAN_POINT('Ctrl Pts',(-1.3224756056767,0.76353164693416,0.630208333333333));
#422366=CARTESIAN_POINT('Ctrl Pts',(-1.76330080756894,2.64858386892187E-15,
0.671875000000001));
#422367=CARTESIAN_POINT('Ctrl Pts',(-1.3224756056767,-0.763531646934155,
0.713541666666668));
#422368=CARTESIAN_POINT('Ctrl Pts',(-0.881650403784469,-1.52706329386831,
0.755208333333333));
#422369=CARTESIAN_POINT('Ctrl Pts',(-1.87011317493125E-16,-1.52706329386831,
0.796875000000001));
#422370=CARTESIAN_POINT('Ctrl Pts',(0.881650403784467,-1.52706329386831,
0.838541666666668));
#422371=CARTESIAN_POINT('Ctrl Pts',(1.3224756056767,-0.763531646934156,
0.880208333333333));
#422372=CARTESIAN_POINT('Ctrl Pts',(1.76330080756894,2.21669973093722E-15,
0.921875000000001));
#422373=CARTESIAN_POINT('Ctrl Pts',(1.3224756056767,0.763531646934159,0.963541666666666));
#422374=CARTESIAN_POINT('Ctrl Pts',(0.881650403784469,1.52706329386832,
1.00520833333333));
#422375=CARTESIAN_POINT('Ctrl Pts',(0.,1.52706329386832,1.046875));
#422376=CARTESIAN_POINT('Ctrl Pts',(-0.881650403784468,1.52706329386832,
1.08854166666667));
#422377=CARTESIAN_POINT('Ctrl Pts',(-1.3224756056767,0.76353164693416,1.13020833333333));
#422378=CARTESIAN_POINT('Ctrl Pts',(-1.76330080756894,2.64858386892187E-15,
1.171875));
#422379=CARTESIAN_POINT('Ctrl Pts',(-1.3224756056767,-0.763531646934155,
1.21354166666667));
#422380=CARTESIAN_POINT('Ctrl Pts',(-0.881650403784469,-1.52706329386831,
1.25520833333333));
#422381=CARTESIAN_POINT('Ctrl Pts',(-1.87011317493125E-16,-1.52706329386831,
1.296875));
#422382=CARTESIAN_POINT('Ctrl Pts',(0.881650403784467,-1.52706329386831,
1.33854166666667));
#422383=CARTESIAN_POINT('Ctrl Pts',(1.3224756056767,-0.763531646934156,
1.38020833333333));
#422384=CARTESIAN_POINT('Ctrl Pts',(1.76330080756894,2.21669973093722E-15,
1.421875));
#422385=CARTESIAN_POINT('Ctrl Pts',(1.3224756056767,0.763531646934159,1.46354166666667));
#422386=CARTESIAN_POINT('Ctrl Pts',(0.881650403784469,1.52706329386832,
1.50520833333333));
#422387=CARTESIAN_POINT('Ctrl Pts',(0.,1.52706329386832,1.546875));
#422388=CARTESIAN_POINT('Ctrl Pts',(-0.881650403784468,1.52706329386832,
1.58854166666667));
#422389=CARTESIAN_POINT('Ctrl Pts',(-1.3224756056767,0.76353164693416,1.63020833333333));
#422390=CARTESIAN_POINT('Ctrl Pts',(-1.76330080756894,2.64858386892187E-15,
1.671875));
#422391=CARTESIAN_POINT('Ctrl Pts',(-1.3224756056767,-0.763531646934155,
1.71354166666667));
#422392=CARTESIAN_POINT('Ctrl Pts',(-0.881650403784469,-1.52706329386831,
1.75520833333333));
#422393=CARTESIAN_POINT('Ctrl Pts',(-1.87011317493125E-16,-1.52706329386831,
1.796875));
#422394=CARTESIAN_POINT('Ctrl Pts',(0.881650403784467,-1.52706329386831,
1.83854166666667));
#422395=CARTESIAN_POINT('Ctrl Pts',(1.3224756056767,-0.763531646934156,
1.88020833333333));
#422396=CARTESIAN_POINT('Ctrl Pts',(1.76330080756894,2.21669973093722E-15,
1.921875));
#422397=CARTESIAN_POINT('Ctrl Pts',(1.3224756056767,0.763531646934159,1.96354166666667));
#422398=CARTESIAN_POINT('Ctrl Pts',(0.881650403784469,1.52706329386832,
2.00520833333333));
#422399=CARTESIAN_POINT('Ctrl Pts',(0.,1.52706329386832,2.046875));
#422400=CARTESIAN_POINT('Ctrl Pts',(-0.881650403784468,1.52706329386832,
2.08854166666667));
#422401=CARTESIAN_POINT('Ctrl Pts',(-1.3224756056767,0.76353164693416,2.13020833333333));
#422402=CARTESIAN_POINT('Ctrl Pts',(-1.76330080756894,2.64858386892187E-15,
2.171875));
#422403=CARTESIAN_POINT('Ctrl Pts',(-1.3224756056767,-0.763531646934155,
2.21354166666667));
#422404=CARTESIAN_POINT('Ctrl Pts',(-0.881650403784469,-1.52706329386831,
2.25520833333333));
#422405=CARTESIAN_POINT('Ctrl Pts',(-1.87011317493125E-16,-1.52706329386831,
2.296875));
#422406=CARTESIAN_POINT('Ctrl Pts',(0.881650403784467,-1.52706329386831,
2.33854166666667));
#422407=CARTESIAN_POINT('Ctrl Pts',(1.3224756056767,-0.763531646934156,
2.38020833333333));
#422408=CARTESIAN_POINT('Ctrl Pts',(1.76330080756894,2.21669973093722E-15,
2.421875));
#422409=CARTESIAN_POINT('Ctrl Pts',(1.3224756056767,0.763531646934159,2.46354166666667));
#422410=CARTESIAN_POINT('Ctrl Pts',(0.881650403784469,1.52706329386832,
2.50520833333333));
#422411=CARTESIAN_POINT('Ctrl Pts',(0.,1.52706329386832,2.546875));
#422412=CARTESIAN_POINT('Ctrl Pts',(-0.881650403784468,1.52706329386832,
2.58854166666667));
#422413=CARTESIAN_POINT('Ctrl Pts',(-1.3224756056767,0.76353164693416,2.63020833333333));
#422414=CARTESIAN_POINT('Ctrl Pts',(-1.76330080756894,2.64858386892187E-15,
2.671875));
#422415=CARTESIAN_POINT('Ctrl Pts',(-1.3224756056767,-0.763531646934155,
2.71354166666667));
#422416=CARTESIAN_POINT('Ctrl Pts',(-0.881650403784469,-1.52706329386831,
2.75520833333333));
#422417=CARTESIAN_POINT('Ctrl Pts',(-1.87011317493125E-16,-1.52706329386831,
2.796875));
#422418=CARTESIAN_POINT('Ctrl Pts',(0.881650403784467,-1.52706329386831,
2.83854166666667));
#422419=CARTESIAN_POINT('Ctrl Pts',(1.3224756056767,-0.763531646934156,
2.88020833333333));
#422420=CARTESIAN_POINT('Ctrl Pts',(1.76330080756894,2.21669973093722E-15,
2.921875));
#422421=CARTESIAN_POINT('Ctrl Pts',(1.3224756056767,0.763531646934159,2.96354166666667));
#422422=CARTESIAN_POINT('Ctrl Pts',(0.881650403784469,1.52706329386832,
3.00520833333333));
#422423=CARTESIAN_POINT('Ctrl Pts',(0.,1.52706329386832,3.046875));
#422424=CARTESIAN_POINT('Ctrl Pts',(-0.881650403784468,1.52706329386832,
3.08854166666667));
#422425=CARTESIAN_POINT('Ctrl Pts',(-1.3224756056767,0.76353164693416,3.13020833333333));
#422426=CARTESIAN_POINT('Ctrl Pts',(-1.76330080756894,2.64858386892187E-15,
3.171875));
#422427=CARTESIAN_POINT('Ctrl Pts',(-1.3224756056767,-0.763531646934155,
3.21354166666667));
#422428=CARTESIAN_POINT('Ctrl Pts',(-0.881650403784469,-1.52706329386831,
3.25520833333333));
#422429=CARTESIAN_POINT('Ctrl Pts',(-1.87011317493125E-16,-1.52706329386831,
3.296875));
#422430=CARTESIAN_POINT('Ctrl Pts',(0.881650403784467,-1.52706329386831,
3.33854166666667));
#422431=CARTESIAN_POINT('Ctrl Pts',(1.3224756056767,-0.763531646934156,
3.38020833333333));
#422432=CARTESIAN_POINT('Ctrl Pts',(1.76330080756894,2.21669973093722E-15,
3.421875));
#422433=CARTESIAN_POINT('Ctrl Pts',(1.3224756056767,0.763531646934159,3.46354166666667));
#422434=CARTESIAN_POINT('Ctrl Pts',(0.881650403784469,1.52706329386832,
3.50520833333333));
#422435=CARTESIAN_POINT('Ctrl Pts',(0.,1.52706329386832,3.546875));
#422436=CARTESIAN_POINT('Ctrl Pts',(-0.881650403784468,1.52706329386832,
3.58854166666667));
#422437=CARTESIAN_POINT('Ctrl Pts',(-1.3224756056767,0.76353164693416,3.63020833333333));
#422438=CARTESIAN_POINT('Ctrl Pts',(-1.76330080756894,2.64858386892187E-15,
3.671875));
#422439=CARTESIAN_POINT('Ctrl Pts',(-1.3224756056767,-0.763531646934155,
3.71354166666667));
#422440=CARTESIAN_POINT('Ctrl Pts',(-0.881650403784469,-1.52706329386831,
3.75520833333333));
#422441=CARTESIAN_POINT('Ctrl Pts',(-1.87011317493125E-16,-1.52706329386831,
3.796875));
#422442=CARTESIAN_POINT('Ctrl Pts',(0.881650403784467,-1.52706329386831,
3.83854166666667));
#422443=CARTESIAN_POINT('Ctrl Pts',(1.3224756056767,-0.763531646934156,
3.88020833333333));
#422444=CARTESIAN_POINT('Ctrl Pts',(1.76330080756894,2.21669973093722E-15,
3.921875));
#422445=CARTESIAN_POINT('Ctrl Pts',(1.3224756056767,0.763531646934159,3.96354166666667));
#422446=CARTESIAN_POINT('Ctrl Pts',(0.881650403784469,1.52706329386832,
4.00520833333333));
#422447=CARTESIAN_POINT('Ctrl Pts',(0.,1.52706329386832,4.046875));
#422448=CARTESIAN_POINT('Ctrl Pts',(-0.881650403784468,1.52706329386832,
4.08854166666667));
#422449=CARTESIAN_POINT('Ctrl Pts',(-1.3224756056767,0.76353164693416,4.13020833333333));
#422450=CARTESIAN_POINT('Ctrl Pts',(-1.76330080756894,2.64858386892187E-15,
4.171875));
#422451=CARTESIAN_POINT('Ctrl Pts',(-1.3224756056767,-0.763531646934155,
4.21354166666667));
#422452=CARTESIAN_POINT('Ctrl Pts',(-0.881650403784469,-1.52706329386831,
4.25520833333333));
#422453=CARTESIAN_POINT('Ctrl Pts',(-1.87011317493125E-16,-1.52706329386831,
4.296875));
#422454=CARTESIAN_POINT('Ctrl Pts',(0.881650403784467,-1.52706329386831,
4.33854166666667));
#422455=CARTESIAN_POINT('Ctrl Pts',(1.3224756056767,-0.763531646934156,
4.38020833333334));
#422456=CARTESIAN_POINT('Ctrl Pts',(1.76330080756894,2.21669973093722E-15,
4.421875));
#422457=CARTESIAN_POINT('Ctrl Pts',(1.3224756056767,0.763531646934159,4.46354166666667));
#422458=CARTESIAN_POINT('Ctrl Pts',(0.881650403784469,1.52706329386832,
4.50520833333333));
#422459=CARTESIAN_POINT('Ctrl Pts',(0.,1.52706329386832,4.546875));
#422460=CARTESIAN_POINT('Ctrl Pts',(-0.881650403784468,1.52706329386832,
4.58854166666667));
#422461=CARTESIAN_POINT('Ctrl Pts',(-1.3224756056767,0.76353164693416,4.63020833333333));
#422462=CARTESIAN_POINT('Ctrl Pts',(-1.76330080756894,2.64858386892187E-15,
4.671875));
#422463=CARTESIAN_POINT('Ctrl Pts',(-1.3224756056767,-0.763531646934155,
4.71354166666667));
#422464=CARTESIAN_POINT('Ctrl Pts',(-0.881650403784469,-1.52706329386831,
4.75520833333333));
#422465=CARTESIAN_POINT('Ctrl Pts',(-1.87011317493125E-16,-1.52706329386831,
4.796875));
#422466=CARTESIAN_POINT('Ctrl Pts',(0.881650403784467,-1.52706329386831,
4.83854166666667));
#422467=CARTESIAN_POINT('Ctrl Pts',(1.3224756056767,-0.763531646934156,
4.88020833333334));
#422468=CARTESIAN_POINT('Ctrl Pts',(1.76330080756894,2.21669973093722E-15,
4.921875));
#422469=CARTESIAN_POINT('Ctrl Pts',(1.3224756056767,0.763531646934159,4.96354166666667));
#422470=CARTESIAN_POINT('Ctrl Pts',(0.881650403784469,1.52706329386832,
5.00520833333333));
#422471=CARTESIAN_POINT('Ctrl Pts',(0.,1.52706329386832,5.046875));
#422472=CARTESIAN_POINT('Ctrl Pts',(-0.881650403784468,1.52706329386832,
5.08854166666667));
#422473=CARTESIAN_POINT('Ctrl Pts',(-1.3224756056767,0.76353164693416,5.13020833333333));
#422474=CARTESIAN_POINT('Ctrl Pts',(-1.76330080756894,2.64858386892187E-15,
5.171875));
#422475=CARTESIAN_POINT('Ctrl Pts',(-1.3224756056767,-0.763531646934155,
5.21354166666667));
#422476=CARTESIAN_POINT('Ctrl Pts',(-0.881650403784469,-1.52706329386831,
5.25520833333333));
#422477=CARTESIAN_POINT('Ctrl Pts',(-1.87011317493125E-16,-1.52706329386831,
5.296875));
#422478=CARTESIAN_POINT('Ctrl Pts',(0.881650403784467,-1.52706329386831,
5.33854166666667));
#422479=CARTESIAN_POINT('Ctrl Pts',(1.3224756056767,-0.763531646934156,
5.38020833333333));
#422480=CARTESIAN_POINT('Ctrl Pts',(1.76330080756894,2.21669973093722E-15,
5.421875));
#422481=CARTESIAN_POINT('Ctrl Pts',(1.3224756056767,0.763531646934159,5.46354166666667));
#422482=CARTESIAN_POINT('Ctrl Pts',(0.881650403784469,1.52706329386832,
5.50520833333333));
#422483=CARTESIAN_POINT('Ctrl Pts',(0.,1.52706329386832,5.546875));
#422484=CARTESIAN_POINT('Ctrl Pts',(-0.881650403784468,1.52706329386832,
5.58854166666667));
#422485=CARTESIAN_POINT('Ctrl Pts',(-1.3224756056767,0.76353164693416,5.63020833333333));
#422486=CARTESIAN_POINT('Ctrl Pts',(-1.76330080756894,2.64858386892187E-15,
5.671875));
#422487=CARTESIAN_POINT('Ctrl Pts',(-1.3224756056767,-0.763531646934155,
5.71354166666667));
#422488=CARTESIAN_POINT('Ctrl Pts',(-0.881650403784469,-1.52706329386831,
5.75520833333333));
#422489=CARTESIAN_POINT('Ctrl Pts',(-1.87011317493125E-16,-1.52706329386831,
5.796875));
#422490=CARTESIAN_POINT('Ctrl Pts',(0.881650403784467,-1.52706329386831,
5.83854166666667));
#422491=CARTESIAN_POINT('Ctrl Pts',(1.3224756056767,-0.763531646934156,
5.88020833333333));
#422492=CARTESIAN_POINT('Ctrl Pts',(1.76330080756894,2.21669973093722E-15,
5.921875));
#422493=CARTESIAN_POINT('Ctrl Pts',(1.3224756056767,0.763531646934159,5.96354166666667));
#422494=CARTESIAN_POINT('Ctrl Pts',(0.881650403784469,1.52706329386832,
6.00520833333333));
#422495=CARTESIAN_POINT('Ctrl Pts',(0.,1.52706329386832,6.046875));
#422496=CARTESIAN_POINT('Ctrl Pts',(-0.881650403784468,1.52706329386832,
6.08854166666667));
#422497=CARTESIAN_POINT('Ctrl Pts',(-1.3224756056767,0.76353164693416,6.13020833333333));
#422498=CARTESIAN_POINT('Ctrl Pts',(-1.76330080756894,2.64858386892187E-15,
6.171875));
#422499=CARTESIAN_POINT('Ctrl Pts',(-1.3224756056767,-0.763531646934155,
6.21354166666667));
#422500=CARTESIAN_POINT('Ctrl Pts',(-0.881650403784469,-1.52706329386831,
6.25520833333333));
#422501=CARTESIAN_POINT('Ctrl Pts',(-1.87011317493125E-16,-1.52706329386831,
6.296875));
#422502=CARTESIAN_POINT('Ctrl Pts',(0.881650403784467,-1.52706329386831,
6.33854166666667));
#422503=CARTESIAN_POINT('Ctrl Pts',(1.3224756056767,-0.763531646934156,
6.38020833333333));
#422504=CARTESIAN_POINT('Ctrl Pts',(1.76330080756894,2.21669973093722E-15,
6.421875));
#422505=CARTESIAN_POINT('Ctrl Pts',(1.3224756056767,0.763531646934159,6.46354166666667));
#422506=CARTESIAN_POINT('Ctrl Pts',(0.881650403784469,1.52706329386832,
6.50520833333333));
#422507=CARTESIAN_POINT('Ctrl Pts',(0.,1.52706329386832,6.546875));
#422508=CARTESIAN_POINT('Ctrl Pts',(-0.881650403784468,1.52706329386832,
6.58854166666667));
#422509=CARTESIAN_POINT('Ctrl Pts',(-1.3224756056767,0.76353164693416,6.63020833333333));
#422510=CARTESIAN_POINT('Ctrl Pts',(-1.76330080756894,2.64858386892187E-15,
6.671875));
#422511=CARTESIAN_POINT('Ctrl Pts',(-1.3224756056767,-0.763531646934155,
6.71354166666667));
#422512=CARTESIAN_POINT('Ctrl Pts',(-0.881650403784469,-1.52706329386831,
6.75520833333333));
#422513=CARTESIAN_POINT('Ctrl Pts',(-1.87011317493125E-16,-1.52706329386831,
6.796875));
#422514=CARTESIAN_POINT('Ctrl Pts',(0.881650403784467,-1.52706329386831,
6.83854166666667));
#422515=CARTESIAN_POINT('Ctrl Pts',(1.3224756056767,-0.763531646934156,
6.88020833333333));
#422516=CARTESIAN_POINT('Ctrl Pts',(1.76330080756894,2.21669973093722E-15,
6.921875));
#422517=CARTESIAN_POINT('Ctrl Pts',(1.3224756056767,0.763531646934159,6.96354166666667));
#422518=CARTESIAN_POINT('Ctrl Pts',(0.881650403784469,1.52706329386832,
7.00520833333333));
#422519=CARTESIAN_POINT('Ctrl Pts',(0.,1.52706329386832,7.046875));
#422520=CARTESIAN_POINT('Ctrl Pts',(-0.881650403784468,1.52706329386832,
7.08854166666667));
#422521=CARTESIAN_POINT('Ctrl Pts',(-1.3224756056767,0.76353164693416,7.13020833333333));
#422522=CARTESIAN_POINT('Ctrl Pts',(-1.76330080756894,2.64858386892187E-15,
7.171875));
#422523=CARTESIAN_POINT('Ctrl Pts',(-1.3224756056767,-0.763531646934155,
7.21354166666667));
#422524=CARTESIAN_POINT('Ctrl Pts',(-0.881650403784469,-1.52706329386831,
7.25520833333333));
#422525=CARTESIAN_POINT('Ctrl Pts',(-1.87011317493125E-16,-1.52706329386831,
7.296875));
#422526=CARTESIAN_POINT('Ctrl Pts',(0.881650403784467,-1.52706329386831,
7.33854166666667));
#422527=CARTESIAN_POINT('Ctrl Pts',(1.3224756056767,-0.763531646934156,
7.38020833333333));
#422528=CARTESIAN_POINT('Ctrl Pts',(1.76330080756894,2.21669973093722E-15,
7.421875));
#422529=CARTESIAN_POINT('Ctrl Pts',(1.3224756056767,0.763531646934159,7.46354166666667));
#422530=CARTESIAN_POINT('Ctrl Pts',(0.881650403784469,1.52706329386832,
7.50520833333333));
#422531=CARTESIAN_POINT('Ctrl Pts',(0.,1.52706329386832,7.546875));
#422532=CARTESIAN_POINT('Ctrl Pts',(-0.881650403784468,1.52706329386832,
7.58854166666667));
#422533=CARTESIAN_POINT('Ctrl Pts',(-1.3224756056767,0.76353164693416,7.63020833333333));
#422534=CARTESIAN_POINT('Ctrl Pts',(-1.76330080756894,2.64858386892187E-15,
7.671875));
#422535=CARTESIAN_POINT('Ctrl Pts',(-1.3224756056767,-0.763531646934155,
7.71354166666667));
#422536=CARTESIAN_POINT('Ctrl Pts',(-0.881650403784469,-1.52706329386831,
7.75520833333334));
#422537=CARTESIAN_POINT('Ctrl Pts',(-1.87011317493125E-16,-1.52706329386831,
7.796875));
#422538=CARTESIAN_POINT('Ctrl Pts',(0.881650403784467,-1.52706329386831,
7.83854166666667));
#422539=CARTESIAN_POINT('Ctrl Pts',(1.3224756056767,-0.763531646934156,
7.88020833333333));
#422540=CARTESIAN_POINT('Ctrl Pts',(1.76330080756894,2.21669973093722E-15,
7.921875));
#422541=CARTESIAN_POINT('Ctrl Pts',(1.3224756056767,0.763531646934159,7.96354166666667));
#422542=CARTESIAN_POINT('Ctrl Pts',(0.881650403784469,1.52706329386832,
8.00520833333333));
#422543=CARTESIAN_POINT('Ctrl Pts',(0.,1.52706329386832,8.046875));
#422544=CARTESIAN_POINT('Ctrl Pts',(-0.881650403784468,1.52706329386832,
8.08854166666667));
#422545=CARTESIAN_POINT('Ctrl Pts',(-1.3224756056767,0.76353164693416,8.13020833333333));
#422546=CARTESIAN_POINT('Ctrl Pts',(-1.76330080756894,2.64858386892187E-15,
8.171875));
#422547=CARTESIAN_POINT('Ctrl Pts',(-1.3224756056767,-0.763531646934155,
8.21354166666667));
#422548=CARTESIAN_POINT('Ctrl Pts',(-0.881650403784469,-1.52706329386831,
8.25520833333334));
#422549=CARTESIAN_POINT('Ctrl Pts',(-1.87011317493125E-16,-1.52706329386831,
8.296875));
#422550=CARTESIAN_POINT('Ctrl Pts',(0.881650403784467,-1.52706329386831,
8.33854166666666));
#422551=CARTESIAN_POINT('Ctrl Pts',(1.3224756056767,-0.763531646934156,
8.38020833333334));
#422552=CARTESIAN_POINT('Ctrl Pts',(1.76330080756894,2.21669973093722E-15,
8.421875));
#422553=CARTESIAN_POINT('Ctrl Pts',(1.3224756056767,0.763531646934159,8.46354166666667));
#422554=CARTESIAN_POINT('Ctrl Pts',(0.881650403784469,1.52706329386832,
8.50520833333334));
#422555=CARTESIAN_POINT('Ctrl Pts',(0.,1.52706329386832,8.546875));
#422556=CARTESIAN_POINT('Ctrl Pts',(-0.881650403784468,1.52706329386832,
8.58854166666667));
#422557=CARTESIAN_POINT('Ctrl Pts',(-1.3224756056767,0.76353164693416,8.63020833333334));
#422558=CARTESIAN_POINT('Ctrl Pts',(-1.76330080756894,2.64858386892187E-15,
8.671875));
#422559=CARTESIAN_POINT('Ctrl Pts',(-1.3224756056767,-0.763531646934155,
8.71354166666667));
#422560=CARTESIAN_POINT('Ctrl Pts',(-0.881650403784469,-1.52706329386831,
8.75520833333334));
#422561=CARTESIAN_POINT('Ctrl Pts',(-1.87011317493125E-16,-1.52706329386831,
8.796875));
#422562=CARTESIAN_POINT('Ctrl Pts',(0.881650403784467,-1.52706329386831,
8.83854166666667));
#422563=CARTESIAN_POINT('Ctrl Pts',(1.3224756056767,-0.763531646934156,
8.88020833333333));
#422564=CARTESIAN_POINT('Ctrl Pts',(1.76330080756894,2.21669973093722E-15,
8.921875));
#422565=CARTESIAN_POINT('Ctrl Pts',(1.3224756056767,0.763531646934159,8.96354166666667));
#422566=CARTESIAN_POINT('Ctrl Pts',(0.881650403784469,1.52706329386832,
9.00520833333333));
#422567=CARTESIAN_POINT('Ctrl Pts',(0.,1.52706329386832,9.046875));
#422568=CARTESIAN_POINT('Ctrl Pts',(-0.881650403784468,1.52706329386832,
9.08854166666667));
#422569=CARTESIAN_POINT('Ctrl Pts',(-1.3224756056767,0.76353164693416,9.13020833333333));
#422570=CARTESIAN_POINT('Ctrl Pts',(-1.76330080756894,2.64858386892187E-15,
9.171875));
#422571=CARTESIAN_POINT('Ctrl Pts',(-1.3224756056767,-0.763531646934155,
9.21354166666667));
#422572=CARTESIAN_POINT('Ctrl Pts',(-0.881650403784469,-1.52706329386831,
9.25520833333333));
#422573=CARTESIAN_POINT('Ctrl Pts',(-1.87011317493125E-16,-1.52706329386831,
9.296875));
#422574=CARTESIAN_POINT('Ctrl Pts',(0.881650403784467,-1.52706329386831,
9.33854166666667));
#422575=CARTESIAN_POINT('Ctrl Pts',(1.3224756056767,-0.763531646934156,
9.38020833333333));
#422576=CARTESIAN_POINT('Ctrl Pts',(1.76330080756894,2.21669973093722E-15,
9.421875));
#422577=CARTESIAN_POINT('Ctrl Pts',(1.3224756056767,0.763531646934159,9.46354166666667));
#422578=CARTESIAN_POINT('Ctrl Pts',(0.881650403784469,1.52706329386832,
9.50520833333334));
#422579=CARTESIAN_POINT('Ctrl Pts',(0.,1.52706329386832,9.546875));
#422580=CARTESIAN_POINT('Ctrl Pts',(-0.881650403784468,1.52706329386832,
9.58854166666667));
#422581=CARTESIAN_POINT('Ctrl Pts',(-1.3224756056767,0.76353164693416,9.63020833333333));
#422582=CARTESIAN_POINT('Ctrl Pts',(-1.76330080756894,2.64858386892187E-15,
9.671875));
#422583=CARTESIAN_POINT('Ctrl Pts',(-1.3224756056767,-0.763531646934155,
9.71354166666667));
#422584=CARTESIAN_POINT('Ctrl Pts',(-0.881650403784469,-1.52706329386831,
9.75520833333333));
#422585=CARTESIAN_POINT('Ctrl Pts',(-1.87011317493125E-16,-1.52706329386831,
9.796875));
#422586=CARTESIAN_POINT('Ctrl Pts',(0.881650403784467,-1.52706329386831,
9.83854166666667));
#422587=CARTESIAN_POINT('Ctrl Pts',(1.3224756056767,-0.763531646934156,
9.88020833333333));
#422588=CARTESIAN_POINT('Ctrl Pts',(1.76330080756894,2.21669973093722E-15,
9.921875));
#422589=CARTESIAN_POINT('Ctrl Pts',(1.3224756056767,0.763531646934159,9.96354166666667));
#422590=CARTESIAN_POINT('Ctrl Pts',(0.881650403784469,1.52706329386832,
10.0052083333333));
#422591=CARTESIAN_POINT('Ctrl Pts',(0.,1.52706329386832,10.046875));
#422592=CARTESIAN_POINT('Ctrl Pts',(-0.881650403784468,1.52706329386832,
10.0885416666667));
#422593=CARTESIAN_POINT('Ctrl Pts',(-1.3224756056767,0.76353164693416,10.1302083333333));
#422594=CARTESIAN_POINT('Ctrl Pts',(-1.76330080756894,2.64858386892187E-15,
10.171875));
#422595=CARTESIAN_POINT('Ctrl Pts',(-1.3224756056767,-0.763531646934155,
10.2135416666667));
#422596=CARTESIAN_POINT('Ctrl Pts',(-0.881650403784469,-1.52706329386831,
10.2552083333333));
#422597=CARTESIAN_POINT('Ctrl Pts',(-1.87011317493125E-16,-1.52706329386831,
10.296875));
#422598=CARTESIAN_POINT('Ctrl Pts',(0.881650403784467,-1.52706329386831,
10.3385416666667));
#422599=CARTESIAN_POINT('Ctrl Pts',(1.3224756056767,-0.763531646934156,
10.3802083333333));
#422600=CARTESIAN_POINT('Ctrl Pts',(1.76330080756894,2.21669973093722E-15,
10.421875));
#422601=CARTESIAN_POINT('Ctrl Pts',(1.3224756056767,0.763531646934159,10.4635416666667));
#422602=CARTESIAN_POINT('Ctrl Pts',(0.881650403784469,1.52706329386832,
10.5052083333333));
#422603=CARTESIAN_POINT('Ctrl Pts',(0.,1.52706329386832,10.546875));
#422604=CARTESIAN_POINT('Ctrl Pts',(-0.881650403784468,1.52706329386832,
10.5885416666667));
#422605=CARTESIAN_POINT('Ctrl Pts',(-1.3224756056767,0.76353164693416,10.6302083333333));
#422606=CARTESIAN_POINT('Ctrl Pts',(-1.76330080756894,2.64858386892187E-15,
10.671875));
#422607=CARTESIAN_POINT('Ctrl Pts',(-1.3224756056767,-0.763531646934155,
10.7135416666667));
#422608=CARTESIAN_POINT('Ctrl Pts',(-0.881650403784469,-1.52706329386831,
10.7552083333333));
#422609=CARTESIAN_POINT('Ctrl Pts',(-1.87011317493125E-16,-1.52706329386831,
10.796875));
#422610=CARTESIAN_POINT('Ctrl Pts',(0.881650403784467,-1.52706329386831,
10.8385416666667));
#422611=CARTESIAN_POINT('Ctrl Pts',(1.3224756056767,-0.763531646934156,
10.8802083333333));
#422612=CARTESIAN_POINT('Ctrl Pts',(1.76330080756894,2.21669973093722E-15,
10.921875));
#422613=CARTESIAN_POINT('Ctrl Pts',(1.3224756056767,0.763531646934159,10.9635416666667));
#422614=CARTESIAN_POINT('Ctrl Pts',(0.881650403784469,1.52706329386832,
11.0052083333333));
#422615=CARTESIAN_POINT('Ctrl Pts',(0.,1.52706329386832,11.046875));
#422616=CARTESIAN_POINT('Origin',(0.,0.,12.5));
#422617=CARTESIAN_POINT('',(-0.0113570611445785,2.67622108038738,12.5737548217797));
#422618=CARTESIAN_POINT('',(0.0113570611445786,2.67622108038738,12.5737548217797));
#422619=CARTESIAN_POINT('Ctrl Pts',(-0.0113570611446294,2.67622108038736,
12.5737548217797));
#422620=CARTESIAN_POINT('Ctrl Pts',(-0.0110019926948033,2.67528393257247,
12.5746934679442));
#422621=CARTESIAN_POINT('Ctrl Pts',(-0.0104377846361818,2.67431181904781,
12.5756680099006));
#422622=CARTESIAN_POINT('Ctrl Pts',(-0.00973150788946615,2.67341366715362,
12.5765688348656));
#422623=CARTESIAN_POINT('Ctrl Pts',(-0.0095445289395165,2.6731758913825,
12.5768073183026));
#422624=CARTESIAN_POINT('Ctrl Pts',(-0.00934782754285408,2.67294319438909,
12.5770407398754));
#422625=CARTESIAN_POINT('Ctrl Pts',(-0.00914308800688213,2.67271724557782,
12.5772674179684));
#422626=CARTESIAN_POINT('Ctrl Pts',(-0.00830289231515457,2.67179001275552,
12.5781976435658));
#422627=CARTESIAN_POINT('Ctrl Pts',(-0.00727124971308708,2.67093133294071,
12.5790594849312));
#422628=CARTESIAN_POINT('Ctrl Pts',(-0.00608692606376634,2.67023630041101,
12.5797571720116));
#422629=CARTESIAN_POINT('Ctrl Pts',(-0.00531529662175078,2.66978346172677,
12.580211740231));
#422630=CARTESIAN_POINT('Ctrl Pts',(-0.0044342859023428,2.66939570266161,
12.5806009430798));
#422631=CARTESIAN_POINT('Ctrl Pts',(-0.0034987762678617,2.66911653534957,
12.5808812374708));
#422632=CARTESIAN_POINT('Ctrl Pts',(-0.00269486313975067,2.66887663801573,
12.5811221033394));
#422633=CARTESIAN_POINT('Ctrl Pts',(-0.00183421434939168,2.66871212840399,
12.581287365893));
#422634=CARTESIAN_POINT('Ctrl Pts',(-0.000963840870899584,2.66864048141248,
12.581359338449));
#422635=CARTESIAN_POINT('Ctrl Pts',(-0.000842876929915767,2.66863052396011,
12.5813693411482));
#422636=CARTESIAN_POINT('Ctrl Pts',(-0.000721709896414026,2.66862230227233,
12.5813775999465));
#422637=CARTESIAN_POINT('Ctrl Pts',(-0.000600449288197464,2.66861580422801,
12.5813841266931));
#422638=CARTESIAN_POINT('Ctrl Pts',(-0.000394716000188903,2.66860477950991,
12.5813952001081));
#422639=CARTESIAN_POINT('Ctrl Pts',(-0.000187302871016306,2.6685992504993,
12.5814007534795));
#422640=CARTESIAN_POINT('Ctrl Pts',(2.17050192878445E-5,2.66859941674402,
12.5814005856065));
#422641=CARTESIAN_POINT('Ctrl Pts',(0.000978461424311802,2.66860017774733,
12.5813998171494));
#422642=CARTESIAN_POINT('Ctrl Pts',(0.00190253100785044,2.66871988992492,
12.58127954464));
#422643=CARTESIAN_POINT('Ctrl Pts',(0.00279246900606494,2.66892852948603,
12.5810700125799));
#422644=CARTESIAN_POINT('Ctrl Pts',(0.00386741278035352,2.66918054232034,
12.5808169217085));
#422645=CARTESIAN_POINT('Ctrl Pts',(0.00488883606980967,2.66957861621199,
12.5804173076348));
#422646=CARTESIAN_POINT('Ctrl Pts',(0.00577667963579214,2.67006359989213,
12.5799304713245));
#422647=CARTESIAN_POINT('Ctrl Pts',(0.00687699751361092,2.67066464745743,
12.5793271277669));
#422648=CARTESIAN_POINT('Ctrl Pts',(0.00785584128008872,2.67140820491266,
12.5785808224116));
#422649=CARTESIAN_POINT('Ctrl Pts',(0.00869113617801994,2.67223767359591,
12.5777485681082));
#422650=CARTESIAN_POINT('Ctrl Pts',(0.00993581708932545,2.67347367280903,
12.576508418016));
#422651=CARTESIAN_POINT('Ctrl Pts',(0.0108561202078293,2.67488514781087,
12.5750928681475));
#422652=CARTESIAN_POINT('Ctrl Pts',(0.0113570611445786,2.67622108038738,
12.5737548217797));
#422653=CARTESIAN_POINT('Origin',(4.96027592420657,14.4980536550356,-1.23970454698711));
#422654=CARTESIAN_POINT('Ctrl Pts',(-0.0391405672444681,2.74327713825537,
12.5064436508398));
#422655=CARTESIAN_POINT('Ctrl Pts',(-0.0350274426582294,2.73335128343629,
12.5164271754438));
#422656=CARTESIAN_POINT('Ctrl Pts',(-0.0309128806500304,2.7234214140262,
12.5264061185523));
#422657=CARTESIAN_POINT('Ctrl Pts',(-0.02679682972068,2.71348738899688,
12.536380305637));
#422658=CARTESIAN_POINT('Ctrl Pts',(-0.0216526008840716,2.70107187254761,
12.5488460165097));
#422659=CARTESIAN_POINT('Ctrl Pts',(-0.0165060448658723,2.68864986137333,
12.5613043021964));
#422660=CARTESIAN_POINT('Ctrl Pts',(-0.0113570611445786,2.67622108038738,
12.5737548217797));
#422661=CARTESIAN_POINT('Ctrl Pts',(-0.0317307692307694,2.68331575103722,
12.5893111709658));
#422662=CARTESIAN_POINT('Ctrl Pts',(-0.0273715540959461,2.67285363471365,
12.5770542771492));
#422663=CARTESIAN_POINT('Ctrl Pts',(-0.0113570611445786,2.67622108038738,
12.5737548217797));
#422664=CARTESIAN_POINT('Ctrl Pts',(-0.0412629097345479,2.70619288824629,
12.5663937883685));
#422665=CARTESIAN_POINT('Ctrl Pts',(-0.0368981338154389,2.69571742604038,
12.5540940315304));
#422666=CARTESIAN_POINT('Ctrl Pts',(-0.0208346759798513,2.69909844921069,
12.5508374392248));
#422667=CARTESIAN_POINT('Ctrl Pts',(-0.0507854324254145,2.72904694270437,
12.5434499600945));
#422668=CARTESIAN_POINT('Ctrl Pts',(-0.0464064650654964,2.71853742104045,
12.5311293540533));
#422669=CARTESIAN_POINT('Ctrl Pts',(-0.0303041210136914,2.72195301478113,
12.5278936106989));
#422670=CARTESIAN_POINT('Ctrl Pts',(-0.0602990906798147,2.75187972251493,
12.5204817579905));
#422671=CARTESIAN_POINT('Ctrl Pts',(-0.055898450424013,2.74131818590101,
12.5081597038247));
#422672=CARTESIAN_POINT('Ctrl Pts',(-0.0397660440343088,2.74478654415416,
12.5049254088044));
#422673=CARTESIAN_POINT('Ctrl Pts',(-0.0534592077666727,2.73546400352339,
12.5369868989719));
#422674=CARTESIAN_POINT('Ctrl Pts',(-0.0538174786896658,2.73632385415953,
12.5342545179733));
#422675=CARTESIAN_POINT('Ctrl Pts',(-0.0540442458867107,2.73719243561899,
12.5314872231885));
#422676=CARTESIAN_POINT('Ctrl Pts',(-0.0540726472749342,2.73803494049807,
12.5287124745063));
#422677=CARTESIAN_POINT('Ctrl Pts',(-0.0540982610565531,2.73879475321623,
12.5262100684184));
#422678=CARTESIAN_POINT('Ctrl Pts',(-0.0539615285066121,2.73953262349448,
12.5237004536639));
#422679=CARTESIAN_POINT('Ctrl Pts',(-0.053594920915001,2.74024914247203,
12.5212220730815));
#422680=CARTESIAN_POINT('Ctrl Pts',(-0.0533142510895361,2.74079769973319,
12.5193246583486));
#422681=CARTESIAN_POINT('Ctrl Pts',(-0.0528949269479518,2.74134000950387,
12.517417831369));
#422682=CARTESIAN_POINT('Ctrl Pts',(-0.0522498055207138,2.7418329426105,
12.5155812248348));
#422683=CARTESIAN_POINT('Ctrl Pts',(-0.0519749803251656,2.74204293476346,
12.5147988205793));
#422684=CARTESIAN_POINT('Ctrl Pts',(-0.0516590665142463,2.74224439930327,
12.5140295443047));
#422685=CARTESIAN_POINT('Ctrl Pts',(-0.0512954408753555,2.74243612605565,
12.5132817086137));
#422686=CARTESIAN_POINT('Ctrl Pts',(-0.0507451426610602,2.74272627855916,
12.5121499604604));
#422687=CARTESIAN_POINT('Ctrl Pts',(-0.05007035249633,2.7429940683096,12.5110494206568));
#422688=CARTESIAN_POINT('Ctrl Pts',(-0.0492469258911254,2.74321114142987,
12.5100666561695));
#422689=CARTESIAN_POINT('Ctrl Pts',(-0.0487741162306004,2.74333578431565,
12.5095023550641));
#422690=CARTESIAN_POINT('Ctrl Pts',(-0.0482466714157864,2.74344451472892,
12.5089719619137));
#422691=CARTESIAN_POINT('Ctrl Pts',(-0.047673188284389,2.74352903919257,
12.5085043804652));
#422692=CARTESIAN_POINT('Ctrl Pts',(-0.0468339704230212,2.74365272973503,
12.5078201359221));
#422693=CARTESIAN_POINT('Ctrl Pts',(-0.0458716475248564,2.7437269769725,
12.5072563000949));
#422694=CARTESIAN_POINT('Ctrl Pts',(-0.0448507996350875,2.7437383071242,
12.5068768744332));
#422695=CARTESIAN_POINT('Ctrl Pts',(-0.0441146980311557,2.74374647694355,
12.5066032824114));
#422696=CARTESIAN_POINT('Ctrl Pts',(-0.0433352353966569,2.74372213722096,
12.5064197834844));
#422697=CARTESIAN_POINT('Ctrl Pts',(-0.0425558582720206,2.74366923074806,
12.5063282718343));
#422698=CARTESIAN_POINT('Ctrl Pts',(-0.0414182089591113,2.74359200367704,
12.5061946931565));
#422699=CARTESIAN_POINT('Ctrl Pts',(-0.0402563540000962,2.74345331865916,
12.5062515701262));
#422700=CARTESIAN_POINT('Ctrl Pts',(-0.0391405672444685,2.74327713825537,
12.5064436508398));
#422701=CARTESIAN_POINT('Origin',(-0.011423076923077,2.69177728949876,12.5893111709658));
#422702=CARTESIAN_POINT('Origin',(-0.0737669000743653,2.72700246506185,
14.));
#422703=CARTESIAN_POINT('Origin',(-0.0737669000743651,2.72700246506185,
13.7435492065112));
#422704=CARTESIAN_POINT('Origin',(-0.0737669000743653,2.72700246506185,
12.5369868989719));
#422705=CARTESIAN_POINT('Ctrl Pts',(0.0317307692307692,2.68331575103722,
12.5893111709658));
#422706=CARTESIAN_POINT('Ctrl Pts',(0.0273715540959458,2.67285363471365,
12.5770542771492));
#422707=CARTESIAN_POINT('Ctrl Pts',(0.0113570611445786,2.67622108038738,
12.5737548217797));
#422708=CARTESIAN_POINT('Ctrl Pts',(0.0276636594244307,2.67355468750201,
12.5928319619712));
#422709=CARTESIAN_POINT('Ctrl Pts',(0.0217268505389381,2.66777647699801,
12.5821634970842));
#422710=CARTESIAN_POINT('Ctrl Pts',(0.00988422427522153,2.6726617308786,
12.5773203894503));
#422711=CARTESIAN_POINT('Ctrl Pts',(0.0153590491204503,2.66218892027728,
12.5969440695591));
#422712=CARTESIAN_POINT('Ctrl Pts',(0.0113393216910521,2.6621706461079,
12.5878292599214));
#422713=CARTESIAN_POINT('Ctrl Pts',(0.00549722182757579,2.66861224243907,
12.5813877129824));
#422714=CARTESIAN_POINT('Ctrl Pts',(-0.0152378843491264,2.66213499625976,
12.596957478804));
#422715=CARTESIAN_POINT('Ctrl Pts',(-0.0112478641478143,2.66215321553576,
12.5878468778671));
#422716=CARTESIAN_POINT('Ctrl Pts',(-0.00545385531034724,2.66859890739381,
12.5814011370086));
#422717=CARTESIAN_POINT('Ctrl Pts',(-0.0276577539880537,2.67354051445456,
12.5928371701607));
#422718=CARTESIAN_POINT('Ctrl Pts',(-0.0217209762404702,2.66777078866562,
12.5821692192952));
#422719=CARTESIAN_POINT('Ctrl Pts',(-0.00987974857032336,2.67265025064741,
12.5773318885715));
#422720=CARTESIAN_POINT('Ctrl Pts',(-0.0317307692308192,2.6833157510372,
12.5893111709658));
#422721=CARTESIAN_POINT('Ctrl Pts',(-0.027371554095996,2.67285363471362,
12.5770542771492));
#422722=CARTESIAN_POINT('Ctrl Pts',(-0.0113570611446294,2.67622108038736,
12.5737548217797));
#422723=CARTESIAN_POINT('Origin',(0.0114230769230771,2.69177728949876,12.5893111709658));
#422724=CARTESIAN_POINT('Ctrl Pts',(-0.0534431697003658,2.73542540894656,
12.5369868989719));
#422725=CARTESIAN_POINT('Ctrl Pts',(-0.059315855709328,2.74959561934461,
12.5369868989719));
#422726=CARTESIAN_POINT('Ctrl Pts',(-0.0746426453864402,2.74898502792764,
12.5369868989719));
#422727=CARTESIAN_POINT('Ctrl Pts',(-0.0554284284177582,2.74021546890479,
12.5218025310015));
#422728=CARTESIAN_POINT('Ctrl Pts',(-0.0628349616649562,2.74942411315693,
12.5216901060417));
#422729=CARTESIAN_POINT('Ctrl Pts',(-0.0745959249085834,2.74898690569132,
12.5161920673678));
#422730=CARTESIAN_POINT('Ctrl Pts',(-0.0522516314408065,2.74533836185331,
12.5042015548895));
#422731=CARTESIAN_POINT('Ctrl Pts',(-0.0571442744892229,2.74951441130436,
12.4980677368514));
#422732=CARTESIAN_POINT('Ctrl Pts',(-0.0639390575126279,2.74936709060421,
12.4907278922777));
#422733=CARTESIAN_POINT('Ctrl Pts',(-0.0391402818913614,2.74325713920844,
12.506463626192));
#422734=CARTESIAN_POINT('Ctrl Pts',(-0.0392336229776118,2.74979921271597,
12.4999376786891));
#422735=CARTESIAN_POINT('Ctrl Pts',(-0.0392324829519608,2.74971931080024,
12.4906970594712));
#422736=CARTESIAN_POINT('Ctrl Pts',(-0.0439361159158126,2.71260851248741,
13.793642941384));
#422737=CARTESIAN_POINT('Ctrl Pts',(-0.0480695586587779,2.72259955197769,
13.8071662555867));
#422738=CARTESIAN_POINT('Ctrl Pts',(-0.0645921377528991,2.71847356558496,
13.8103758687955));
#422739=CARTESIAN_POINT('Ctrl Pts',(-0.0503288525022281,2.72795108802607,
13.7804579775006));
#422740=CARTESIAN_POINT('Ctrl Pts',(-0.0554385177735605,2.74027525098119,
13.7901904343352));
#422741=CARTESIAN_POINT('Ctrl Pts',(-0.0711414500059975,2.73898147995502,
13.7927914348263));
#422742=CARTESIAN_POINT('Ctrl Pts',(-0.0540924971515107,2.73698383963716,
13.7597120340895));
#422743=CARTESIAN_POINT('Ctrl Pts',(-0.0600111123098007,2.7512441721922,
13.7635825532445));
#422744=CARTESIAN_POINT('Ctrl Pts',(-0.0750279227547006,2.75106719703732,
13.7651073818884));
#422745=CARTESIAN_POINT('Ctrl Pts',(-0.0533554893522594,2.73521502004488,
13.7381884353898));
#422746=CARTESIAN_POINT('Ctrl Pts',(-0.0591347381257982,2.74914190750188,
13.7368803041982));
#422747=CARTESIAN_POINT('Ctrl Pts',(-0.0742673064063059,2.74870030320526,
13.7363986145813));
#422748=CARTESIAN_POINT('Origin',(-0.0657949699454127,2.70786983275237,
13.7902182540695));
#422749=CARTESIAN_POINT('Ctrl Pts',(0.0113570611445786,2.67622108038738,
12.5737548217797));
#422750=CARTESIAN_POINT('Ctrl Pts',(0.0273715540959461,2.67285363471365,
12.5770542771492));
#422751=CARTESIAN_POINT('Ctrl Pts',(0.0317307692307694,2.68331575103722,
12.5893111709658));
#422752=CARTESIAN_POINT('Ctrl Pts',(0.0208332521184758,2.69909501224871,
12.5508408821982));
#422753=CARTESIAN_POINT('Ctrl Pts',(0.0368967013046715,2.69571398801462,
12.55409748406));
#422754=CARTESIAN_POINT('Ctrl Pts',(0.0412614776815739,2.70618945131915,
12.5663972313419));
#422755=CARTESIAN_POINT('Ctrl Pts',(0.030301275750311,2.72194614771936,
12.52790050457));
#422756=CARTESIAN_POINT('Ctrl Pts',(0.046403605589348,2.71853055829785,
12.5311362602938));
#422757=CARTESIAN_POINT('Ctrl Pts',(0.0507825712136453,2.72904007579613,
12.5434568539655));
#422758=CARTESIAN_POINT('Ctrl Pts',(0.0397617795410514,2.74477625307133,
12.5049357605811));
#422759=CARTESIAN_POINT('Ctrl Pts',(0.0558941686815425,2.74130790971908,
12.5081700652078));
#422760=CARTESIAN_POINT('Ctrl Pts',(0.0602948028693876,2.75186943176991,
12.5204921097672));
#422761=CARTESIAN_POINT('Ctrl Pts',(0.0391405672443406,2.74327713825507,
12.5064436508395));
#422762=CARTESIAN_POINT('Ctrl Pts',(0.0403458187330792,2.74346744495352,
12.5062361689309));
#422763=CARTESIAN_POINT('Ctrl Pts',(0.0416072967527669,2.74361395374604,
12.5061871075061));
#422764=CARTESIAN_POINT('Ctrl Pts',(0.042834363742733,2.7436869143056,12.5063648335164));
#422765=CARTESIAN_POINT('Ctrl Pts',(0.0433917732582066,2.74372005749215,
12.5064455676329));
#422766=CARTESIAN_POINT('Ctrl Pts',(0.0439498697112453,2.74373826608298,
12.506574497099));
#422767=CARTESIAN_POINT('Ctrl Pts',(0.0444847578701803,2.74373970895803,
12.5067492519495));
#422768=CARTESIAN_POINT('Ctrl Pts',(0.0455596363883573,2.74374260847144,
12.5071004286051));
#422769=CARTESIAN_POINT('Ctrl Pts',(0.0465803157288013,2.74367710231937,
12.5076537929612));
#422770=CARTESIAN_POINT('Ctrl Pts',(0.0474707943411653,2.74355754611012,
12.5083435010503));
#422771=CARTESIAN_POINT('Ctrl Pts',(0.0475268552914394,2.74355001933227,
12.5083869222963));
#422772=CARTESIAN_POINT('Ctrl Pts',(0.0475824047224509,2.74354226567989,
12.5084308732336));
#422773=CARTESIAN_POINT('Ctrl Pts',(0.0476374258851168,2.7435342837174,
12.5084753333615));
#422774=CARTESIAN_POINT('Ctrl Pts',(0.0480787682303327,2.74347025784312,
12.508831962269));
#422775=CARTESIAN_POINT('Ctrl Pts',(0.0484952661504182,2.74339151902502,
12.509227847131));
#422776=CARTESIAN_POINT('Ctrl Pts',(0.0488750551274305,2.74330315989752,
12.5096423454524));
#422777=CARTESIAN_POINT('Ctrl Pts',(0.0500651456938278,2.74302628149805,
12.5109411997424));
#422778=CARTESIAN_POINT('Ctrl Pts',(0.0509701735738429,2.74264732684897,
12.5124831113042));
#422779=CARTESIAN_POINT('Ctrl Pts',(0.0516586827254371,2.74223154610909,
12.5140723025008));
#422780=CARTESIAN_POINT('Ctrl Pts',(0.0517231967870444,2.74219258699837,
12.5142212114565));
#422781=CARTESIAN_POINT('Ctrl Pts',(0.0517858370895858,2.7421533161305,
12.5143705582413));
#422782=CARTESIAN_POINT('Ctrl Pts',(0.0518466749855142,2.74211379521906,
12.5145201959299));
#422783=CARTESIAN_POINT('Ctrl Pts',(0.0526282283368708,2.74160609027122,
12.5164425148273));
#422784=CARTESIAN_POINT('Ctrl Pts',(0.0531449550363651,2.7410487292595,
12.5184635205941));
#422785=CARTESIAN_POINT('Ctrl Pts',(0.0534850107690122,2.74046085777738,
12.5205025929158));
#422786=CARTESIAN_POINT('Ctrl Pts',(0.0536822565724959,2.74011986901671,
12.5216853356836));
#422787=CARTESIAN_POINT('Ctrl Pts',(0.0538201244047732,2.73976947321855,
12.5228750347131));
#422788=CARTESIAN_POINT('Ctrl Pts',(0.053914227561147,2.73941911276914,
12.5240609649613));
#422789=CARTESIAN_POINT('Ctrl Pts',(0.0541451987100069,2.73855917184226,
12.5269717671326));
#422790=CARTESIAN_POINT('Ctrl Pts',(0.054108978580863,2.73767254503778,
12.5299036066169));
#422791=CARTESIAN_POINT('Ctrl Pts',(0.0538915946618915,2.73676966278747,
12.5328133004019));
#422792=CARTESIAN_POINT('Ctrl Pts',(0.0537872377228983,2.73633622673406,
12.5342101228451));
#422793=CARTESIAN_POINT('Ctrl Pts',(0.0536407512085802,2.73589970799702,
12.5356023438238));
#422794=CARTESIAN_POINT('Ctrl Pts',(0.0534592077666729,2.73546400352339,
12.5369868989719));
#422795=CARTESIAN_POINT('Ctrl Pts',(-0.0317292560088479,2.68331211733141,
13.8235227101244));
#422796=CARTESIAN_POINT('Ctrl Pts',(-0.0361471144551244,2.69392650450487,
13.8358800583119));
#422797=CARTESIAN_POINT('Ctrl Pts',(-0.0523410482444131,2.69040761867485,
13.8390832900376));
#422798=CARTESIAN_POINT('Ctrl Pts',(-0.0363167865314177,2.69432219058271,
13.8124254819052));
#422799=CARTESIAN_POINT('Ctrl Pts',(-0.0407432246529827,2.70495719063873,
13.8247886449158));
#422800=CARTESIAN_POINT('Ctrl Pts',(-0.0569540009528031,2.70141720294675,
13.8279860620657));
#422801=CARTESIAN_POINT('Ctrl Pts',(-0.040902261072039,2.70532732947737,
13.8013225099955));
#422802=CARTESIAN_POINT('Ctrl Pts',(-0.0453351884501785,2.71597792517399,
13.8136962257787));
#422803=CARTESIAN_POINT('Ctrl Pts',(-0.0615645680923407,2.71242179507057,
13.8168830918626));
#422804=CARTESIAN_POINT('Ctrl Pts',(-0.0454857596258171,2.71632772600364,
13.7902140179785));
#422805=CARTESIAN_POINT('Ctrl Pts',(-0.0499232224687475,2.72698922801144,
13.802602731458));
#422806=CARTESIAN_POINT('Ctrl Pts',(-0.0661728417004948,2.72342159191108,
13.8057746032558));
#422807=CARTESIAN_POINT('Origin',(-0.0520384615384617,2.67485421257569,
13.8235269408515));
#422808=CARTESIAN_POINT('Ctrl Pts',(0.0391403049721299,2.74325875688934,
12.506462012331));
#422809=CARTESIAN_POINT('Ctrl Pts',(0.0392335873299004,2.74979671424555,
12.4999388158272));
#422810=CARTESIAN_POINT('Ctrl Pts',(0.0392324836772759,2.74971936163602,
12.4907030323752));
#422811=CARTESIAN_POINT('Ctrl Pts',(0.052251582889411,2.74533793329604,
12.5042014951932));
#422812=CARTESIAN_POINT('Ctrl Pts',(0.0571414622024566,2.7495128796933,
12.4980716682127));
#422813=CARTESIAN_POINT('Ctrl Pts',(0.0639314807543423,2.74936723186163,
12.4907355092743));
#422814=CARTESIAN_POINT('Ctrl Pts',(0.0554299221525007,2.74021700947567,
12.5218047446509));
#422815=CARTESIAN_POINT('Ctrl Pts',(0.0628336980936782,2.74942043127133,
12.5216906929434));
#422816=CARTESIAN_POINT('Ctrl Pts',(0.0745888263163512,2.74898717061242,
12.5161988840776));
#422817=CARTESIAN_POINT('Ctrl Pts',(0.0534444632996223,2.73542852959617,
12.5369868989719));
#422818=CARTESIAN_POINT('Ctrl Pts',(0.0593158561893107,2.74958947155127,
12.5369868989719));
#422819=CARTESIAN_POINT('Ctrl Pts',(0.0746338391269334,2.74898537698633,
12.5369868989719));
#422820=CARTESIAN_POINT('Origin',(0.0737669000743652,2.72700246506185,12.5369868989719));
#422821=CARTESIAN_POINT('Ctrl Pts',(0.0317307692307695,2.68331575103722,
13.8235269408515));
#422822=CARTESIAN_POINT('Ctrl Pts',(0.0362721082597566,2.69421496470679,
13.8362179249168));
#422823=CARTESIAN_POINT('Ctrl Pts',(0.0528913878732058,2.69028271990423,
13.8391868794938));
#422824=CARTESIAN_POINT('Ctrl Pts',(0.0275756416919826,2.67334344494414,
13.8400110824519));
#422825=CARTESIAN_POINT('Ctrl Pts',(0.0343745296800287,2.68076617927778,
13.8494522556837));
#422826=CARTESIAN_POINT('Ctrl Pts',(0.0459495068922318,2.67391433354299,
13.85569149686));
#422827=CARTESIAN_POINT('Ctrl Pts',(0.0157029524147764,2.66218831270049,
13.8586819406588));
#422828=CARTESIAN_POINT('Ctrl Pts',(0.0200567840833213,2.66220222086172,
13.868010383617));
#422829=CARTESIAN_POINT('Ctrl Pts',(0.0261406348414864,2.65550299502995,
13.8744918421245));
#422830=CARTESIAN_POINT('Ctrl Pts',(-0.0155871213907187,2.66213559464325,
13.8587686893867));
#422831=CARTESIAN_POINT('Ctrl Pts',(-0.0199022038181156,2.66212175395646,
13.8680909899357));
#422832=CARTESIAN_POINT('Ctrl Pts',(-0.0259481535750132,2.65541780787651,
13.8745789365162));
#422833=CARTESIAN_POINT('Ctrl Pts',(-0.0275688803167364,2.67332721762648,
13.8400379222776));
#422834=CARTESIAN_POINT('Ctrl Pts',(-0.0343713127316049,2.68074322377194,
13.8494748685453));
#422835=CARTESIAN_POINT('Ctrl Pts',(-0.0459415271867833,2.67389550570487,
13.8557104837033));
#422836=CARTESIAN_POINT('Ctrl Pts',(-0.0317307692368139,2.68331575103455,
13.8235269408542));
#422837=CARTESIAN_POINT('Ctrl Pts',(-0.0362721082658378,2.69421496470408,
13.8362179249195));
#422838=CARTESIAN_POINT('Ctrl Pts',(-0.0528913878792488,2.69028271990147,
13.8391868794965));
#422839=CARTESIAN_POINT('Origin',(0.0520384615384617,2.67485421257569,13.8235269408515));
#422840=CARTESIAN_POINT('Origin',(0.0737669000743654,2.72700246506185,14.));
#422841=CARTESIAN_POINT('Origin',(0.0737669000743653,2.72700246506185,13.7435492065112));
#422842=CARTESIAN_POINT('Ctrl Pts',(0.0454857618430532,2.7163277313308,
13.7902140241682));
#422843=CARTESIAN_POINT('Ctrl Pts',(0.0499232289341833,2.72698922659215,
13.8026027327198));
#422844=CARTESIAN_POINT('Ctrl Pts',(0.0661728417005767,2.72342159191127,
13.8057746032556));
#422845=CARTESIAN_POINT('Ctrl Pts',(0.0409022632877525,2.70532733480086,
13.8013225161808));
#422846=CARTESIAN_POINT('Ctrl Pts',(0.0453351949047153,2.71597792375946,
13.8136962270464));
#422847=CARTESIAN_POINT('Ctrl Pts',(0.0615645680922413,2.71242179507032,
13.8168830918628));
#422848=CARTESIAN_POINT('Ctrl Pts',(0.0363167887449816,2.69432219590103,
13.8124254880875));
#422849=CARTESIAN_POINT('Ctrl Pts',(0.0407432310975133,2.70495718923156,
13.8247886461868));
#422850=CARTESIAN_POINT('Ctrl Pts',(0.0569540009528616,2.70141720294686,
13.8279860620656));
#422851=CARTESIAN_POINT('Ctrl Pts',(0.0317292582190083,2.68331212264155,
13.8235227163065));
#422852=CARTESIAN_POINT('Ctrl Pts',(0.0361471208901607,2.69392650310656,
13.8358800595847));
#422853=CARTESIAN_POINT('Ctrl Pts',(0.0523410482444131,2.69040761867485,
13.8390832900376));
#422854=CARTESIAN_POINT('Origin',(0.0657949699454121,2.70786983275237,13.7902182540695));
#422855=CARTESIAN_POINT('Ctrl Pts',(0.0533554409592648,2.735214891466,13.7382347919292));
#422856=CARTESIAN_POINT('Ctrl Pts',(0.0591372501192909,2.74915363429203,
13.7369371795943));
#422857=CARTESIAN_POINT('Ctrl Pts',(0.0742812611866724,2.74870340567088,
13.7364597369711));
#422858=CARTESIAN_POINT('Ctrl Pts',(0.0540829631312669,2.73696094572446,
13.7595490285574));
#422859=CARTESIAN_POINT('Ctrl Pts',(0.0600036499999177,2.75123186978083,
13.7633824266926));
#422860=CARTESIAN_POINT('Ctrl Pts',(0.0750322024404344,2.75104141808081,
13.7648920890506));
#422861=CARTESIAN_POINT('Ctrl Pts',(0.0503726399036044,2.72805616466601,
13.7803806590111));
#422862=CARTESIAN_POINT('Ctrl Pts',(0.0554888357784383,2.74040207191393,
13.7901039518744));
#422863=CARTESIAN_POINT('Ctrl Pts',(0.0712002870186107,2.73912311086945,
13.7926933640891));
#422864=CARTESIAN_POINT('Ctrl Pts',(0.0439232699567853,2.71257766735968,
13.7936647693663));
#422865=CARTESIAN_POINT('Ctrl Pts',(0.0480553632782531,2.72257262292373,
13.8072068914933));
#422866=CARTESIAN_POINT('Ctrl Pts',(0.0645931722560378,2.71843195340523,
13.8104111085397));
#422867=CARTESIAN_POINT('Origin',(-0.187089956683836,2.67697359150001,12.5));
#422868=CARTESIAN_POINT('',(-0.187089956683836,2.67697359150001,12.5893111709658));
#422869=CARTESIAN_POINT('',(-0.187089956683836,2.67697359150001,13.8235269408515));
#422870=CARTESIAN_POINT('',(-0.187089956683836,2.67697359150001,12.5));
#422871=CARTESIAN_POINT('',(-0.176070301470241,2.71100063806851,13.7902182540695));
#422872=CARTESIAN_POINT('',(-0.187089956683836,2.67697359150001,13.8235269408515));
#422873=CARTESIAN_POINT('',(-0.16968438443307,2.73071939443562,13.7435492065112));
#422874=CARTESIAN_POINT('Origin',(-0.190694276985055,2.66584504699436,13.7445212918699));
#422875=CARTESIAN_POINT('',(-0.16968438443307,2.73071939443562,12.5369868989719));
#422876=CARTESIAN_POINT('',(-0.16968438443307,2.73071939443562,12.5));
#422877=CARTESIAN_POINT('Ctrl Pts',(-0.16968438443307,2.73071939443562,
12.5369868989719));
#422878=CARTESIAN_POINT('Ctrl Pts',(-0.175482010328069,2.71281719309701,
12.5544431401645));
#422879=CARTESIAN_POINT('Ctrl Pts',(-0.1812837828392,2.69490218762818,12.5718848856037));
#422880=CARTESIAN_POINT('Ctrl Pts',(-0.187089956683836,2.67697359150001,
12.5893111709658));
#422881=CARTESIAN_POINT('Origin',(-0.376448442621724,2.91618121445596,12.5));
#422882=CARTESIAN_POINT('',(-0.276247037758877,2.72200455098751,13.7435492065112));
#422883=CARTESIAN_POINT('',(-0.266742146417875,2.703585367247,13.7902182540695));
#422884=CARTESIAN_POINT('Origin',(-0.241764934750096,2.65518293585363,13.7418732680453));
#422885=CARTESIAN_POINT('',(-0.250340332111353,2.67180088696722,13.8235269408515));
#422886=CARTESIAN_POINT('',(-0.266742146417875,2.703585367247,13.7902182540695));
#422887=CARTESIAN_POINT('',(-0.250340332111353,2.67180088696722,12.5893111709658));
#422888=CARTESIAN_POINT('',(-0.250340332111353,2.67180088696722,12.5));
#422889=CARTESIAN_POINT('',(-0.276247037758877,2.72200455098751,12.5369868989719));
#422890=CARTESIAN_POINT('Ctrl Pts',(-0.250340332111353,2.67180088696722,
12.5893111709658));
#422891=CARTESIAN_POINT('Ctrl Pts',(-0.258982325294008,2.68854789170455,
12.5718848856037));
#422892=CARTESIAN_POINT('Ctrl Pts',(-0.267617767468175,2.70528220148044,
12.5544431401645));
#422893=CARTESIAN_POINT('Ctrl Pts',(-0.276247037758877,2.72200455098751,
12.5369868989719));
#422894=CARTESIAN_POINT('',(-0.276247037758877,2.72200455098751,12.5));
#422895=CARTESIAN_POINT('Origin',(-0.21979279117526,2.68756440078102,12.5));
#422896=CARTESIAN_POINT('',(-0.215876635126138,2.65341394113584,13.8587068136939));
#422897=CARTESIAN_POINT('Ctrl Pts',(-0.250340332117159,2.67180088696406,
13.8235269408542));
#422898=CARTESIAN_POINT('Ctrl Pts',(-0.249536772004133,2.67024369700394,
13.8262006681044));
#422899=CARTESIAN_POINT('Ctrl Pts',(-0.248560051181353,2.66872981310272,
13.8288634856214));
#422900=CARTESIAN_POINT('Ctrl Pts',(-0.247423382155456,2.66725743645065,
13.8314912288862));
#422901=CARTESIAN_POINT('Ctrl Pts',(-0.24625159363173,2.66573956799097,
13.8342001611531));
#422902=CARTESIAN_POINT('Ctrl Pts',(-0.244908912170735,2.66426382167543,
13.8368750301949));
#422903=CARTESIAN_POINT('Ctrl Pts',(-0.243365577123696,2.66283751664132,
13.8394886372969));
#422904=CARTESIAN_POINT('Ctrl Pts',(-0.243246381614405,2.6627273596438,
13.8396904925131));
#422905=CARTESIAN_POINT('Ctrl Pts',(-0.243125971626977,2.6626175109886,
13.8398919674349));
#422906=CARTESIAN_POINT('Ctrl Pts',(-0.243004324996858,2.66250798176036,
13.8400930404591));
#422907=CARTESIAN_POINT('Ctrl Pts',(-0.241108988659767,2.66080144269672,
13.8432258934518));
#422908=CARTESIAN_POINT('Ctrl Pts',(-0.238923872511486,2.6591803183025,
13.8462331177034));
#422909=CARTESIAN_POINT('Ctrl Pts',(-0.236462766213828,2.65777495436557,
13.8489036603661));
#422910=CARTESIAN_POINT('Ctrl Pts',(-0.235657463591899,2.65731510293036,
13.849777493004));
#422911=CARTESIAN_POINT('Ctrl Pts',(-0.234822725104269,2.65687857500021,
13.85061494757));
#422912=CARTESIAN_POINT('Ctrl Pts',(-0.23395936919549,2.65647056727925,
13.8514076489583));
#422913=CARTESIAN_POINT('Ctrl Pts',(-0.232133246933858,2.6556075721059,
13.8530843267192));
#422914=CARTESIAN_POINT('Ctrl Pts',(-0.229998457928146,2.65479007714677,
13.8546805203176));
#422915=CARTESIAN_POINT('Ctrl Pts',(-0.227630109492369,2.65419295193012,
13.8559412814274));
#422916=CARTESIAN_POINT('Ctrl Pts',(-0.227313147664311,2.65411303721091,
13.8561100121513));
#422917=CARTESIAN_POINT('Ctrl Pts',(-0.226992065096586,2.65403702499007,
13.8562727473908));
#422918=CARTESIAN_POINT('Ctrl Pts',(-0.226667097614289,2.65396528305557,
13.8564289040185));
#422919=CARTESIAN_POINT('Ctrl Pts',(-0.225193373789397,2.65363993420106,
13.8571370725437));
#422920=CARTESIAN_POINT('Ctrl Pts',(-0.223613357649691,2.65339891275393,
13.8577210840553));
#422921=CARTESIAN_POINT('Ctrl Pts',(-0.221984039041397,2.653280599691,13.8581177131616));
#422922=CARTESIAN_POINT('Ctrl Pts',(-0.221525166841861,2.65324727866026,
13.8582294175695));
#422923=CARTESIAN_POINT('Ctrl Pts',(-0.221062431392487,2.65322351941437,
13.8583265086086));
#422924=CARTESIAN_POINT('Ctrl Pts',(-0.220597197391072,2.65320974940297,
13.8584082369006));
#422925=CARTESIAN_POINT('Ctrl Pts',(-0.219928780888465,2.65318996558916,
13.8585256585398));
#422926=CARTESIAN_POINT('Ctrl Pts',(-0.219246887321347,2.65319087878083,
13.8586122832068));
#422927=CARTESIAN_POINT('Ctrl Pts',(-0.218569231365846,2.65321325494219,
13.8586682984299));
#422928=CARTESIAN_POINT('Ctrl Pts',(-0.218027173775319,2.6532311536532,
13.8587131050557));
#422929=CARTESIAN_POINT('Ctrl Pts',(-0.217481832815699,2.65326274859779,
13.8587357943552));
#422930=CARTESIAN_POINT('Ctrl Pts',(-0.216933172977939,2.65330854912843,
13.8587355499465));
#422931=CARTESIAN_POINT('Ctrl Pts',(-0.216578561044268,2.65333815110331,
13.8587353919793));
#422932=CARTESIAN_POINT('Ctrl Pts',(-0.216226394209478,2.65337332859157,
13.8587257282814));
#422933=CARTESIAN_POINT('Ctrl Pts',(-0.215876635126138,2.65341394113584,
13.8587068136939));
#422934=CARTESIAN_POINT('Ctrl Pts',(-0.215876635126138,2.65341394113584,
13.8587068136939));
#422935=CARTESIAN_POINT('Ctrl Pts',(-0.21472629656782,2.65354751357998,
13.8586446046466));
#422936=CARTESIAN_POINT('Ctrl Pts',(-0.213601970174342,2.65373980551323,
13.858482427929));
#422937=CARTESIAN_POINT('Ctrl Pts',(-0.212502602233195,2.65398647232433,
13.8582284286032));
#422938=CARTESIAN_POINT('Ctrl Pts',(-0.211374778609438,2.65423952377902,
13.8579678548414));
#422939=CARTESIAN_POINT('Ctrl Pts',(-0.210270802547482,2.65455191401367,
13.857615680862));
#422940=CARTESIAN_POINT('Ctrl Pts',(-0.209231559205508,2.65490200369315,
13.8571944833187));
#422941=CARTESIAN_POINT('Ctrl Pts',(-0.206638021160501,2.65577568829253,
13.8561433417727));
#422942=CARTESIAN_POINT('Ctrl Pts',(-0.204324791989813,2.65692048993979,
13.8546163505474));
#422943=CARTESIAN_POINT('Ctrl Pts',(-0.202344521073351,2.65813644386444,
13.8528973491086));
#422944=CARTESIAN_POINT('Ctrl Pts',(-0.201982754793105,2.65835858070673,
13.8525833129072));
#422945=CARTESIAN_POINT('Ctrl Pts',(-0.201631979407093,2.65858301952384,
13.8522628768811));
#422946=CARTESIAN_POINT('Ctrl Pts',(-0.201292350061553,2.65880847431043,
13.851937733538));
#422947=CARTESIAN_POINT('Ctrl Pts',(-0.199218280769687,2.66018529541175,
13.8499521282529));
#422948=CARTESIAN_POINT('Ctrl Pts',(-0.197356021225063,2.66174023370548,
13.847639871647));
#422949=CARTESIAN_POINT('Ctrl Pts',(-0.195751952356615,2.66332989773982,
13.8452109780794));
#422950=CARTESIAN_POINT('Ctrl Pts',(-0.195030248570126,2.66404512049328,
13.8441181685877));
#422951=CARTESIAN_POINT('Ctrl Pts',(-0.194360159582619,2.66476706910083,
13.8430021611332));
#422952=CARTESIAN_POINT('Ctrl Pts',(-0.193742625521376,2.66548228083695,
13.8418824960098));
#422953=CARTESIAN_POINT('Ctrl Pts',(-0.192287390736757,2.66716769555671,
13.8392439765549));
#422954=CARTESIAN_POINT('Ctrl Pts',(-0.191051575423354,2.66889379713922,
13.8364981347964));
#422955=CARTESIAN_POINT('Ctrl Pts',(-0.190004086953026,2.67064522939239,
13.8336931113419));
#422956=CARTESIAN_POINT('Ctrl Pts',(-0.188983899704597,2.67235101318074,
13.8309611966328));
#422957=CARTESIAN_POINT('Ctrl Pts',(-0.188141812403136,2.67408282348032,
13.8281701127185));
#422958=CARTESIAN_POINT('Ctrl Pts',(-0.187487856314965,2.67583299279055,
13.825358068512));
#422959=CARTESIAN_POINT('Ctrl Pts',(-0.187346077929281,2.67621243138584,
13.8247484142932));
#422960=CARTESIAN_POINT('Ctrl Pts',(-0.187213310689527,2.67659269278633,
13.8241378483365));
#422961=CARTESIAN_POINT('Ctrl Pts',(-0.187089956683836,2.67697359150001,
13.8235269408515));
#422962=CARTESIAN_POINT('',(-0.217112984834088,2.65329470919124,12.5969504640361));
#422963=CARTESIAN_POINT('Origin',(-0.219795292788959,2.68759739206378,12.584524458991));
#422964=CARTESIAN_POINT('Origin',(-0.219795292788959,2.68759739206378,12.584524458991));
#422965=CARTESIAN_POINT('Ctrl Pts',(-0.250340332111353,2.67180088696722,
12.5893111709658));
#422966=CARTESIAN_POINT('Ctrl Pts',(-0.245142862299359,2.66172889897511,
12.5770542771492));
#422967=CARTESIAN_POINT('Ctrl Pts',(-0.229456134336435,2.666390469598,12.5737548217797));
#422968=CARTESIAN_POINT('Ctrl Pts',(-0.261705454267471,2.69382494444632,
12.5663937883685));
#422969=CARTESIAN_POINT('Ctrl Pts',(-0.256501354360936,2.68374010823476,
12.5540940315304));
#422970=CARTESIAN_POINT('Ctrl Pts',(-0.240766931132422,2.68841920226884,
12.5508374392248));
#422971=CARTESIAN_POINT('Ctrl Pts',(-0.273059109154684,2.71582677992147,
12.5434499600945));
#422972=CARTESIAN_POINT('Ctrl Pts',(-0.267838088866063,2.70570915431606,
12.5311293540533));
#422973=CARTESIAN_POINT('Ctrl Pts',(-0.252067726634541,2.7104258734774,
12.5278936106989));
#422974=CARTESIAN_POINT('Ctrl Pts',(-0.284402195019786,2.73780813407251,
12.5204817579905));
#422975=CARTESIAN_POINT('Ctrl Pts',(-0.279155334248852,2.72764043313481,
12.5081597038247));
#422976=CARTESIAN_POINT('Ctrl Pts',(-0.263359310506878,2.7324121915987,
12.5049254088044));
#422977=CARTESIAN_POINT('Ctrl Pts',(-0.276247037758876,2.72200455098751,
12.5369868989719));
#422978=CARTESIAN_POINT('Ctrl Pts',(-0.276674202374231,2.72283233813534,
12.5342545179733));
#422979=CARTESIAN_POINT('Ctrl Pts',(-0.276971012474594,2.72367954582987,
12.5314872231885));
#422980=CARTESIAN_POINT('Ctrl Pts',(-0.277067991328621,2.72451693236666,
12.5287124745063));
#422981=CARTESIAN_POINT('Ctrl Pts',(-0.277155451672784,2.72527212910971,
12.5262100684184));
#422982=CARTESIAN_POINT('Ctrl Pts',(-0.277079317366856,2.72601868915766,
12.5237004536639));
#422983=CARTESIAN_POINT('Ctrl Pts',(-0.276772332580271,2.72676270589956,
12.5212220730815));
#422984=CARTESIAN_POINT('Ctrl Pts',(-0.276537309169838,2.72733231507807,
12.5193246583486));
#422985=CARTESIAN_POINT('Ctrl Pts',(-0.276163583575611,2.72790699916809,
12.517417831369));
#422986=CARTESIAN_POINT('Ctrl Pts',(-0.275560787361057,2.72845087546581,
12.5155812248347));
#422987=CARTESIAN_POINT('Ctrl Pts',(-0.275303992933616,2.72868256969198,
12.5147988205793));
#422988=CARTESIAN_POINT('Ctrl Pts',(-0.275005551530144,2.72890911378354,
12.5140295443047));
#422989=CARTESIAN_POINT('Ctrl Pts',(-0.274658763335797,2.72912984144627,
12.5132817086137));
#422990=CARTESIAN_POINT('Ctrl Pts',(-0.274133946316095,2.72946388290445,
12.5121499604604));
#422991=CARTESIAN_POINT('Ctrl Pts',(-0.273483228810673,2.72978578326946,
12.5110494206568));
#422992=CARTESIAN_POINT('Ctrl Pts',(-0.272680235564079,2.73006925100947,
12.5100666561695));
#422993=CARTESIAN_POINT('Ctrl Pts',(-0.272219158691014,2.73023201753301,
12.5095023550641));
#422994=CARTESIAN_POINT('Ctrl Pts',(-0.271702331443396,2.73038337780377,
12.5089719619137));
#422995=CARTESIAN_POINT('Ctrl Pts',(-0.271137646058283,2.7305143652184,
12.5085043804652));
#422996=CARTESIAN_POINT('Ctrl Pts',(-0.270311302552617,2.73070604823741,
12.5078201359221));
#422997=CARTESIAN_POINT('Ctrl Pts',(-0.26935823354364,2.73085848667329,
12.5072563000949));
#422998=CARTESIAN_POINT('Ctrl Pts',(-0.268341705953558,2.73095298770495,
12.5068768744332));
#422999=CARTESIAN_POINT('Ctrl Pts',(-0.267608719583111,2.73102112945426,
12.5066032824114));
#423000=CARTESIAN_POINT('Ctrl Pts',(-0.266829866632878,2.73106040416098,
12.5064197834844));
#423001=CARTESIAN_POINT('Ctrl Pts',(-0.266048770452628,2.73107120020104,
12.5063282718343));
#423002=CARTESIAN_POINT('Ctrl Pts',(-0.264908611850729,2.73108695907716,
12.5061946931565));
#423003=CARTESIAN_POINT('Ctrl Pts',(-0.263739318751798,2.73104343748753,
12.5062515701262));
#423004=CARTESIAN_POINT('Ctrl Pts',(-0.262612884346067,2.73095879028853,
12.5064436508398));
#423005=CARTESIAN_POINT('',(-0.229456134336435,2.666390469598,12.5737548217797));
#423006=CARTESIAN_POINT('Origin',(-0.230789905912253,2.68188953580805,12.5893111709658));
#423007=CARTESIAN_POINT('Ctrl Pts',(-0.262612884346068,2.73095879028853,
12.5064436508398));
#423008=CARTESIAN_POINT('Ctrl Pts',(-0.257704396527699,2.72140122077071,
12.5164271754438));
#423009=CARTESIAN_POINT('Ctrl Pts',(-0.252794148843822,2.71183976718331,
12.5264061185523));
#423010=CARTESIAN_POINT('Ctrl Pts',(-0.247882078471508,2.70227429316508,
12.536380305637));
#423011=CARTESIAN_POINT('Ctrl Pts',(-0.241742986781333,2.69031939072946,
12.5488460165097));
#423012=CARTESIAN_POINT('Ctrl Pts',(-0.235601046272685,2.6783582048664,
12.5613043021964));
#423013=CARTESIAN_POINT('Ctrl Pts',(-0.229456134336435,2.666390469598,12.5737548217797));
#423014=CARTESIAN_POINT('Ctrl Pts',(-0.187089956683836,2.67697359150001,
12.5893111709658));
#423015=CARTESIAN_POINT('Ctrl Pts',(-0.190581907283988,2.66619097050297,
12.5770542771492));
#423016=CARTESIAN_POINT('Ctrl Pts',(-0.206817591415412,2.66824188143219,
12.5737548217797));
#423017=CARTESIAN_POINT('Ctrl Pts',(-0.190347916222393,2.66691349989206,
12.5928319619712));
#423018=CARTESIAN_POINT('Ctrl Pts',(-0.195793993067713,2.66067061086804,
12.5821634970842));
#423019=CARTESIAN_POINT('Ctrl Pts',(-0.207995407513229,2.66457432548726,
12.5773203894503));
#423020=CARTESIAN_POINT('Ctrl Pts',(-0.201685168407197,2.65458261134995,
12.5969440695591));
#423021=CARTESIAN_POINT('Ctrl Pts',(-0.205690031010724,2.65423675288354,
12.5878292599214));
#423022=CARTESIAN_POINT('Ctrl Pts',(-0.212037741670697,2.66018072996003,
12.5813877129824));
#423023=CARTESIAN_POINT('Ctrl Pts',(-0.232175897796688,2.65203493263431,
12.596957478804));
#423024=CARTESIAN_POINT('Ctrl Pts',(-0.228200639098576,2.65237831497512,
12.5878468778671));
#423025=CARTESIAN_POINT('Ctrl Pts',(-0.222951293072859,2.65927482483445,
12.5814011370086));
#423026=CARTESIAN_POINT('Ctrl Pts',(-0.245484096960501,2.6623901652322,
12.5928371701607));
#423027=CARTESIAN_POINT('Ctrl Pts',(-0.239096787135805,2.65712354023063,
12.5821692192952));
#423028=CARTESIAN_POINT('Ctrl Pts',(-0.227692681624127,2.66295193618891,
12.5773318885715));
#423029=CARTESIAN_POINT('Ctrl Pts',(-0.2503403321114,2.67180088696719,12.5893111709658));
#423030=CARTESIAN_POINT('Ctrl Pts',(-0.245142862299407,2.66172889897508,
12.5770542771492));
#423031=CARTESIAN_POINT('Ctrl Pts',(-0.229456134336484,2.66639046959797,
12.5737548217797));
#423032=CARTESIAN_POINT('',(-0.206817591415412,2.66824188143219,12.5737548217797));
#423033=CARTESIAN_POINT('Origin',(-0.208019770758347,2.68375170943985,12.5893111709658));
#423034=CARTESIAN_POINT('Ctrl Pts',(-0.229456134336484,2.66639046959797,
12.5737548217797));
#423035=CARTESIAN_POINT('Ctrl Pts',(-0.229025861100665,2.66548538144008,
12.5746934679442));
#423036=CARTESIAN_POINT('Ctrl Pts',(-0.228384294120895,2.66456249073761,
12.5756680099006));
#423037=CARTESIAN_POINT('Ctrl Pts',(-0.227607159734381,2.66372489548137,
12.5765688348656));
#423038=CARTESIAN_POINT('Ctrl Pts',(-0.227401422008713,2.66350315140976,
12.5768073183026));
#423039=CARTESIAN_POINT('Ctrl Pts',(-0.227186408154502,2.66328726168631,
12.5770407398754));
#423040=CARTESIAN_POINT('Ctrl Pts',(-0.22696393294672,2.66307875287396,
12.5772674179684));
#423041=CARTESIAN_POINT('Ctrl Pts',(-0.226050954853818,2.66222308909126,
12.5781976435658));
#423042=CARTESIAN_POINT('Ctrl Pts',(-0.224952754580903,2.66145135491207,
12.5790594849312));
#423043=CARTESIAN_POINT('Ctrl Pts',(-0.223715720067288,2.66085516841792,
12.5797571720116));
#423044=CARTESIAN_POINT('Ctrl Pts',(-0.222909747601871,2.66046673148003,
12.580211740231));
#423045=CARTESIAN_POINT('Ctrl Pts',(-0.222000062409363,2.6601520732037,
12.5806009430798));
#423046=CARTESIAN_POINT('Ctrl Pts',(-0.221044910878422,2.65995008751792,
12.5808812374708));
#423047=CARTESIAN_POINT('Ctrl Pts',(-0.220224118845122,2.65977651480578,
12.5811221033394));
#423048=CARTESIAN_POINT('Ctrl Pts',(-0.219352924732026,2.65968270345249,
12.581287365893));
#423049=CARTESIAN_POINT('Ctrl Pts',(-0.218479607454537,2.65968223837908,
12.581359338449));
#423050=CARTESIAN_POINT('Ctrl Pts',(-0.218358234386279,2.65968217374348,
12.5813693411482));
#423051=CARTESIAN_POINT('Ctrl Pts',(-0.218236800382204,2.65968385565078,
12.5813775999465));
#423052=CARTESIAN_POINT('Ctrl Pts',(-0.21811541360772,2.65968726309347,
12.5813841266931));
#423053=CARTESIAN_POINT('Ctrl Pts',(-0.217909466263382,2.65969304423211,
12.5813952001081));
#423054=CARTESIAN_POINT('Ctrl Pts',(-0.217702292618593,2.65970443971438,
12.5814007534795));
#423055=CARTESIAN_POINT('Ctrl Pts',(-0.217493993735289,2.65972164148933,
12.5814005856065));
#423056=CARTESIAN_POINT('Ctrl Pts',(-0.216540482887111,2.65980038448957,
12.5813998171494));
#423057=CARTESIAN_POINT('Ctrl Pts',(-0.215629245722708,2.65999501858446,
12.58127954464));
#423058=CARTESIAN_POINT('Ctrl Pts',(-0.214759274980914,2.66027550212328,
12.5810700125799));
#423059=CARTESIAN_POINT('Ctrl Pts',(-0.213708449378927,2.66061429430257,
12.5808169217085));
#423060=CARTESIAN_POINT('Ctrl Pts',(-0.212722871508912,2.66109429911671,
12.5804173076348));
#423061=CARTESIAN_POINT('Ctrl Pts',(-0.211877512841454,2.66165003654662,
12.5799304713245));
#423062=CARTESIAN_POINT('Ctrl Pts',(-0.210829847137029,2.66233877029763,
12.5793271277669));
#423063=CARTESIAN_POINT('Ctrl Pts',(-0.209914867227887,2.66315963848088,
12.5785808224116));
#423064=CARTESIAN_POINT('Ctrl Pts',(-0.209149961102918,2.66405443146419,
12.5777485681082));
#423065=CARTESIAN_POINT('Ctrl Pts',(-0.208010167174992,2.66538777104121,
12.576508418016));
#423066=CARTESIAN_POINT('Ctrl Pts',(-0.20720797460534,2.66686956272427,
12.5750928681475));
#423067=CARTESIAN_POINT('Ctrl Pts',(-0.206817591415412,2.66824188143219,
12.5737548217797));
#423068=CARTESIAN_POINT('Ctrl Pts',(-0.206817591415412,2.66824188143219,
12.5737548217797));
#423069=CARTESIAN_POINT('Ctrl Pts',(-0.190581907283988,2.66619097050297,
12.5770542771492));
#423070=CARTESIAN_POINT('Ctrl Pts',(-0.187089956683836,2.67697359150001,
12.5893111709658));
#423071=CARTESIAN_POINT('Ctrl Pts',(-0.199237369483173,2.69181209970925,
12.5508408821982));
#423072=CARTESIAN_POINT('Ctrl Pts',(-0.182951785236016,2.68975164578888,
12.55409748406));
#423073=CARTESIAN_POINT('Ctrl Pts',(-0.179455379801222,2.70054802264873,
12.5663972313419));
#423074=CARTESIAN_POINT('Ctrl Pts',(-0.191663429599364,2.71535893173455,
12.52790050457));
#423075=CARTESIAN_POINT('Ctrl Pts',(-0.175336276687888,2.71326719677367,
12.5311362602938));
#423076=CARTESIAN_POINT('Ctrl Pts',(-0.17182850495217,2.72409867107017,
12.5434568539655));
#423077=CARTESIAN_POINT('Ctrl Pts',(-0.184095270385093,2.73888419068029,
12.5049357605811));
#423078=CARTESIAN_POINT('Ctrl Pts',(-0.167733858256901,2.73674232743516,
12.5081700652078));
#423079=CARTESIAN_POINT('Ctrl Pts',(-0.164208728911819,2.74762739943244,
12.5204921097672));
#423080=CARTESIAN_POINT('Ctrl Pts',(-0.184592223874505,2.73733942947567,
12.5064436508395));
#423081=CARTESIAN_POINT('Ctrl Pts',(-0.183406494523313,2.73762734212962,
12.5062361689309));
#423082=CARTESIAN_POINT('Ctrl Pts',(-0.182161155794383,2.73787618559581,
12.5061871075061));
#423083=CARTESIAN_POINT('Ctrl Pts',(-0.180944118731537,2.73804892073635,
12.5063648335164));
#423084=CARTESIAN_POINT('Ctrl Pts',(-0.180391265427633,2.73812738769193,
12.5064455676329));
#423085=CARTESIAN_POINT('Ctrl Pts',(-0.179836510163696,2.73819102573722,
12.506574497099));
#423086=CARTESIAN_POINT('Ctrl Pts',(-0.179303519408695,2.73823606216183,
12.5067492519495));
#423087=CARTESIAN_POINT('Ctrl Pts',(-0.178232453797269,2.73832656460527,
12.5071004286051));
#423088=CARTESIAN_POINT('Ctrl Pts',(-0.177209831323526,2.73834447126128,
12.5076537929613));
#423089=CARTESIAN_POINT('Ctrl Pts',(-0.176312570764263,2.73829789513915,
12.5083435010505));
#423090=CARTESIAN_POINT('Ctrl Pts',(-0.176256082849997,2.73829496289392,
12.5083869222964));
#423091=CARTESIAN_POINT('Ctrl Pts',(-0.176200086260576,2.73829176283551,
12.5084308732337));
#423092=CARTESIAN_POINT('Ctrl Pts',(-0.176144597572335,2.7382882921679,
12.5084753333615));
#423093=CARTESIAN_POINT('Ctrl Pts',(-0.175699505054222,2.73826045283278,
12.5088319622689));
#423094=CARTESIAN_POINT('Ctrl Pts',(-0.175277975051939,2.73821592445867,
12.509227847131));
#423095=CARTESIAN_POINT('Ctrl Pts',(-0.17489224770224,2.7381588156663,12.5096423454524));
#423096=CARTESIAN_POINT('Ctrl Pts',(-0.173683548904055,2.73797986198629,
12.5109411997424));
#423097=CARTESIAN_POINT('Ctrl Pts',(-0.172750644107707,2.73767593645163,
12.5124831113042));
#423098=CARTESIAN_POINT('Ctrl Pts',(-0.172030535923296,2.73731765907553,
12.5140723025008));
#423099=CARTESIAN_POINT('Ctrl Pts',(-0.171963060997705,2.73728408809298,
12.5142212114565));
#423100=CARTESIAN_POINT('Ctrl Pts',(-0.171897428185298,2.73725005366185,
12.5143705582413));
#423101=CARTESIAN_POINT('Ctrl Pts',(-0.171833571401274,2.7372156231063,
12.5145201959299));
#423102=CARTESIAN_POINT('Ctrl Pts',(-0.171013235937672,2.73677331135852,
12.5164425148273));
#423103=CARTESIAN_POINT('Ctrl Pts',(-0.170452798506902,2.73625992294265,
12.518463520594));
#423104=CARTESIAN_POINT('Ctrl Pts',(-0.170065957298328,2.73570172525353,
12.5205025929157));
#423105=CARTESIAN_POINT('Ctrl Pts',(-0.169841574064402,2.73537794846895,
12.5216853356836));
#423106=CARTESIAN_POINT('Ctrl Pts',(-0.169675604465496,2.73503995609214,
12.5228750347131));
#423107=CARTESIAN_POINT('Ctrl Pts',(-0.169553256800397,2.73469843171908,
12.5240609649613));
#423108=CARTESIAN_POINT('Ctrl Pts',(-0.169252961020137,2.73386017846754,
12.5269717671326));
#423109=CARTESIAN_POINT('Ctrl Pts',(-0.169216792314183,2.73297354956384,
12.5299036066169));
#423110=CARTESIAN_POINT('Ctrl Pts',(-0.169359859620749,2.73205595277224,
12.5328133004019));
#423111=CARTESIAN_POINT('Ctrl Pts',(-0.169428540258459,2.73161545288222,
12.5342101228451));
#423112=CARTESIAN_POINT('Ctrl Pts',(-0.169538959021474,2.73116844661443,
12.5356023438238));
#423113=CARTESIAN_POINT('Ctrl Pts',(-0.16968438443307,2.73071939443562,
12.5369868989719));
#423114=CARTESIAN_POINT('Origin',(3.76220301131683,14.8546061023375,-1.24025450174292));
#423115=CARTESIAN_POINT('Ctrl Pts',(-0.276227907241606,2.72196739208225,
12.5369868989719));
#423116=CARTESIAN_POINT('Ctrl Pts',(-0.283236056069593,2.73561177384507,
12.5369868989719));
#423117=CARTESIAN_POINT('Ctrl Pts',(-0.298462078249489,2.73375393847501,
12.5369868989719));
#423118=CARTESIAN_POINT('Ctrl Pts',(-0.27859699452973,2.7265796964954,12.5218025310015));
#423119=CARTESIAN_POINT('Ctrl Pts',(-0.286729473143964,2.7351539985249,
12.5216901060417));
#423120=CARTESIAN_POINT('Ctrl Pts',(-0.298415666285335,2.73375961814326,
12.5161920673678));
#423121=CARTESIAN_POINT('Ctrl Pts',(-0.275848331416576,2.73194448188581,
12.5042015548895));
#423122=CARTESIAN_POINT('Ctrl Pts',(-0.281065081397688,2.7357078400473,
12.4980677368514));
#423123=CARTESIAN_POINT('Ctrl Pts',(-0.287825247336383,2.73500717164852,
12.4907278922777));
#423124=CARTESIAN_POINT('Ctrl Pts',(-0.262610969834461,2.73093888104572,
12.506463626192));
#423125=CARTESIAN_POINT('Ctrl Pts',(-0.263237240060458,2.73745157817826,
12.4999376786891));
#423126=CARTESIAN_POINT('Ctrl Pts',(-0.263229591080243,2.73737203505225,
12.4906970594712));
#423127=CARTESIAN_POINT('Origin',(-0.295797463957976,2.71191590214668,12.5369868989719));
#423128=CARTESIAN_POINT('Origin',(-0.295797463957976,2.71191590214668,14.));
#423129=CARTESIAN_POINT('Origin',(-0.295797463957976,2.71191590214668,13.7435492065112));
#423130=CARTESIAN_POINT('Ctrl Pts',(-0.264892698511088,2.70000133010642,
13.793642941384));
#423131=CARTESIAN_POINT('Ctrl Pts',(-0.269826750035054,2.70962221128044,
13.8071662555867));
#423132=CARTESIAN_POINT('Ctrl Pts',(-0.285958045415463,2.70416321018274,
13.8103758687955));
#423133=CARTESIAN_POINT('Ctrl Pts',(-0.272514726133809,2.7147717871116,
13.7804579775006));
#423134=CARTESIAN_POINT('Ctrl Pts',(-0.27861192310825,2.72663845727571,
13.7901904343351));
#423135=CARTESIAN_POINT('Ctrl Pts',(-0.294157150779669,2.72406905641006,
13.7927914348262));
#423136=CARTESIAN_POINT('Ctrl Pts',(-0.277002100678258,2.72346771100792,
13.7597120340895));
#423137=CARTESIAN_POINT('Ctrl Pts',(-0.284063371622543,2.73719817140167,
13.7635825532445));
#423138=CARTESIAN_POINT('Ctrl Pts',(-0.299015789751427,2.73579777565649,
13.7651073818885));
#423139=CARTESIAN_POINT('Ctrl Pts',(-0.276123369993984,2.72176484999464,
13.7381884353898));
#423140=CARTESIAN_POINT('Ctrl Pts',(-0.283018559412648,2.73517433445553,
13.7368803041982));
#423141=CARTESIAN_POINT('Ctrl Pts',(-0.298064780470721,2.73350075476201,
13.7363986145813));
#423142=CARTESIAN_POINT('Origin',(-0.286292572616974,2.69349671840617,13.7902182540695));
#423143=CARTESIAN_POINT('Ctrl Pts',(-0.25033852774379,2.67179738869388,
13.8235227101244));
#423144=CARTESIAN_POINT('Ctrl Pts',(-0.255606857224329,2.6820163608929,
13.8358800583119));
#423145=CARTESIAN_POINT('Ctrl Pts',(-0.27146008517196,2.67718922792421,
13.8390832900376));
#423146=CARTESIAN_POINT('Ctrl Pts',(-0.25580821681952,2.6823969005086,13.8124254819053));
#423147=CARTESIAN_POINT('Ctrl Pts',(-0.261086777568463,2.69263571767931,
13.8247886449158));
#423148=CARTESIAN_POINT('Ctrl Pts',(-0.276955071986918,2.68778618024237,
13.8279860620657));
#423149=CARTESIAN_POINT('Ctrl Pts',(-0.261275454558501,2.69299166196687,
13.8013225099955));
#423150=CARTESIAN_POINT('Ctrl Pts',(-0.266561754161049,2.70324549395033,
13.8136962257787));
#423151=CARTESIAN_POINT('Ctrl Pts',(-0.282447274264371,2.69837835146943,
13.8168830918626));
#423152=CARTESIAN_POINT('Ctrl Pts',(-0.26674033633855,2.70358185789793,
13.7902140179785));
#423153=CARTESIAN_POINT('Ctrl Pts',(-0.27203204528012,2.71384619022022,
13.802602731458));
#423154=CARTESIAN_POINT('Ctrl Pts',(-0.287936799781886,2.70896593031318,
13.8057746032558));
#423155=CARTESIAN_POINT('Origin',(-0.269890758310452,2.66171223812639,13.8235269408515));
#423156=CARTESIAN_POINT('Ctrl Pts',(-0.187089956683836,2.67697359150001,
13.8235269408515));
#423157=CARTESIAN_POINT('Ctrl Pts',(-0.183452115683267,2.68820670022581,
13.8362179249168));
#423158=CARTESIAN_POINT('Ctrl Pts',(-0.166567620895153,2.68564216521781,
13.8391868794938));
#423159=CARTESIAN_POINT('Ctrl Pts',(-0.190418422853553,2.66669578596405,
13.8400110824519));
#423160=CARTESIAN_POINT('Ctrl Pts',(-0.184247179361899,2.67464799425036,
13.8494522556837));
#423161=CARTESIAN_POINT('Ctrl Pts',(-0.172152227894695,2.66876241556666,
13.85569149686));
#423162=CARTESIAN_POINT('Ctrl Pts',(-0.201342359899562,2.65461003710596,
13.8586819406588));
#423163=CARTESIAN_POINT('Ctrl Pts',(-0.197004148890986,2.65497877668892,
13.868010383617));
#423164=CARTESIAN_POINT('Ctrl Pts',(-0.19039449254647,2.64879773229496,
13.8744918421245));
#423165=CARTESIAN_POINT('Ctrl Pts',(-0.232524021554646,2.65200706296568,
13.8587686893867));
#423166=CARTESIAN_POINT('Ctrl Pts',(-0.236823617756771,2.65164154905553,
13.8680909899357));
#423167=CARTESIAN_POINT('Ctrl Pts',(-0.242303016272693,2.64446710877009,
13.8745789365163));
#423168=CARTESIAN_POINT('Ctrl Pts',(-0.245378133337349,2.66218482216098,
13.8400379222776));
#423169=CARTESIAN_POINT('Ctrl Pts',(-0.252762404567227,2.66902169076523,
13.8494748685453));
#423170=CARTESIAN_POINT('Ctrl Pts',(-0.263735967494693,2.66125367802444,
13.8557104837033));
#423171=CARTESIAN_POINT('Ctrl Pts',(-0.250340332117159,2.67180088696406,
13.8235269408542));
#423172=CARTESIAN_POINT('Ctrl Pts',(-0.255754947312626,2.68229367310862,
13.8362179249195));
#423173=CARTESIAN_POINT('Ctrl Pts',(-0.271998413187523,2.67701988695185,
13.8391868794965));
#423174=CARTESIAN_POINT('Origin',(-0.166160142609325,2.67019547356017,13.8235269408515));
#423175=CARTESIAN_POINT('Ctrl Pts',(-0.176071515536958,2.71099688674549,
13.7902140241682));
#423176=CARTESIAN_POINT('Ctrl Pts',(-0.172517824591793,2.72198460152422,
13.8026027327198));
#423177=CARTESIAN_POINT('Ctrl Pts',(-0.156031485724598,2.71975333214794,
13.8057746032556));
#423178=CARTESIAN_POINT('Ctrl Pts',(-0.17974312843904,2.69965949544416,
13.8013225161808));
#423179=CARTESIAN_POINT('Ctrl Pts',(-0.176193068911704,2.71063597052669,
13.8136962270464));
#423180=CARTESIAN_POINT('Ctrl Pts',(-0.159727840122992,2.70841451914335,
13.8168830918628));
#423181=CARTESIAN_POINT('Ctrl Pts',(-0.183416324206491,2.68831721649143,
13.8124254880875));
#423182=CARTESIAN_POINT('Ctrl Pts',(-0.179871461162618,2.69927761890379,
13.8247886461867));
#423183=CARTESIAN_POINT('Ctrl Pts',(-0.16342608956085,2.69707073986811,
13.8279860620656));
#423184=CARTESIAN_POINT('Ctrl Pts',(-0.187091166919895,2.67696985201606,
13.8235227163065));
#423185=CARTESIAN_POINT('Ctrl Pts',(-0.183553174869323,2.68790901082681,
13.8358800595848));
#423186=CARTESIAN_POINT('Ctrl Pts',(-0.167126309723535,2.68572179060922,
13.8390832900376));
#423187=CARTESIAN_POINT('Origin',(-0.15514048739573,2.70422252012867,13.7902182540695));
#423188=CARTESIAN_POINT('Ctrl Pts',(-0.169767501019668,2.73046265331991,
13.7382347919292));
#423189=CARTESIAN_POINT('Ctrl Pts',(-0.165141067293955,2.74482628725131,
13.7369371795942));
#423190=CARTESIAN_POINT('Ctrl Pts',(-0.150010748861761,2.74561193422088,
13.7364597369711));
#423191=CARTESIAN_POINT('Ctrl Pts',(-0.169184719249316,2.73226219753788,
13.7595490285574));
#423192=CARTESIAN_POINT('Ctrl Pts',(-0.164446945773195,2.74696822721648,
13.7633824266926));
#423193=CARTESIAN_POINT('Ctrl Pts',(-0.149452876019529,2.74800337577097,
13.7648920890506));
#423194=CARTESIAN_POINT('Ctrl Pts',(-0.172156874358305,2.72308462061578,
13.780380659011));
#423195=CARTESIAN_POINT('Ctrl Pts',(-0.168064008257698,2.73580646533606,
13.7901039518743));
#423196=CARTESIAN_POINT('Ctrl Pts',(-0.152300588377005,2.73581238906302,
13.7926933640892));
#423197=CARTESIAN_POINT('Ctrl Pts',(-0.177323143332834,2.70713194320866,
13.7936647693663));
#423198=CARTESIAN_POINT('Ctrl Pts',(-0.174019480878138,2.71743044534879,
13.8072068914933));
#423199=CARTESIAN_POINT('Ctrl Pts',(-0.157199197089587,2.71465153852775,
13.8104111085397));
#423200=CARTESIAN_POINT('Origin',(-0.148754570358559,2.72394127649578,13.7435492065112));
#423201=CARTESIAN_POINT('Origin',(-0.148754570358559,2.72394127649578,14.));
#423202=CARTESIAN_POINT('Origin',(-0.148754570358559,2.72394127649578,12.5369868989719));
#423203=CARTESIAN_POINT('Ctrl Pts',(-0.184590987022074,2.73732108789479,
12.506462012331));
#423204=CARTESIAN_POINT('Ctrl Pts',(-0.18503091927362,2.7438448941154,12.4999388158272));
#423205=CARTESIAN_POINT('Ctrl Pts',(-0.185025714298148,2.74376770893236,
12.4907030323752));
#423206=CARTESIAN_POINT('Ctrl Pts',(-0.171692807979739,2.74046203688297,
12.5042014951932));
#423207=CARTESIAN_POINT('Ctrl Pts',(-0.167159496226433,2.74502166204993,
12.4980716682127));
#423208=CARTESIAN_POINT('Ctrl Pts',(-0.160380199250707,2.74542994839683,
12.4907355092744));
#423209=CARTESIAN_POINT('Ctrl Pts',(-0.168107641546659,2.73561721667034,
12.5218047446509));
#423210=CARTESIAN_POINT('Ctrl Pts',(-0.161478665375871,2.74539349131174,
12.5216906929434));
#423211=CARTESIAN_POINT('Ctrl Pts',(-0.149727336606756,2.74591982437135,
12.5161988840775));
#423212=CARTESIAN_POINT('Ctrl Pts',(-0.169696188384732,2.73068283673402,
12.5369868989719));
#423213=CARTESIAN_POINT('Ctrl Pts',(-0.164998580303643,2.74527523235082,
12.5369868989719));
#423214=CARTESIAN_POINT('Ctrl Pts',(-0.149682327375411,2.74592170567534,
12.5369868989719));
#423215=CARTESIAN_POINT('Origin',(-4.19924629559645E-32,-1.71423978068635E-33,
12.5));
#423216=CARTESIAN_POINT('Origin',(0.250340332111317,2.67180088696722,12.5));
#423217=CARTESIAN_POINT('',(0.250340332111317,2.67180088696722,12.5893111709658));
#423218=CARTESIAN_POINT('',(0.250340332111317,2.67180088696722,13.8235269408515));
#423219=CARTESIAN_POINT('',(0.250340332111317,2.67180088696722,12.5));
#423220=CARTESIAN_POINT('',(0.266742146417839,2.703585367247,13.7902182540695));
#423221=CARTESIAN_POINT('',(0.250340332111317,2.67180088696722,13.8235269408515));
#423222=CARTESIAN_POINT('',(0.276247037758841,2.72200455098751,13.7435492065112));
#423223=CARTESIAN_POINT('Origin',(0.24497578139935,2.66140582933077,13.7445212918703));
#423224=CARTESIAN_POINT('',(0.276247037758841,2.72200455098751,12.5369868989719));
#423225=CARTESIAN_POINT('',(0.276247037758841,2.72200455098751,12.5));
#423226=CARTESIAN_POINT('Ctrl Pts',(0.276247037758841,2.72200455098751,
12.5369868989719));
#423227=CARTESIAN_POINT('Ctrl Pts',(0.267617767468139,2.70528220148044,
12.5544431401645));
#423228=CARTESIAN_POINT('Ctrl Pts',(0.258982325293973,2.68854789170455,
12.5718848856037));
#423229=CARTESIAN_POINT('Ctrl Pts',(0.250340332111317,2.67180088696722,
12.5893111709658));
#423230=CARTESIAN_POINT('Origin',(0.102363482435782,2.9385962674314,12.5));
#423231=CARTESIAN_POINT('',(0.169684384433034,2.73071939443562,13.7435492065112));
#423232=CARTESIAN_POINT('',(0.176070301470205,2.71100063806852,13.7902182540695));
#423233=CARTESIAN_POINT('Origin',(0.192851387736352,2.6591831544195,13.7418732680435));
#423234=CARTESIAN_POINT('',(0.187089956683801,2.67697359150002,13.8235269408515));
#423235=CARTESIAN_POINT('',(0.176070301470205,2.71100063806852,13.7902182540695));
#423236=CARTESIAN_POINT('',(0.187089956683801,2.67697359150002,12.5893111709658));
#423237=CARTESIAN_POINT('',(0.187089956683801,2.67697359150002,12.5));
#423238=CARTESIAN_POINT('',(0.169684384433034,2.73071939443562,12.5369868989719));
#423239=CARTESIAN_POINT('Ctrl Pts',(0.187089956683801,2.67697359150002,
12.5893111709658));
#423240=CARTESIAN_POINT('Ctrl Pts',(0.181283782839164,2.69490218762819,
12.5718848856037));
#423241=CARTESIAN_POINT('Ctrl Pts',(0.175482010328033,2.71281719309701,
12.5544431401645));
#423242=CARTESIAN_POINT('Ctrl Pts',(0.169684384433034,2.73071939443562,
12.5369868989719));
#423243=CARTESIAN_POINT('',(0.169684384433034,2.73071939443562,12.5));
#423244=CARTESIAN_POINT('Origin',(0.219792791175224,2.68756440078102,12.5));
#423245=CARTESIAN_POINT('',(0.2181082764625,2.6532314343732,13.8587068136939));
#423246=CARTESIAN_POINT('Ctrl Pts',(0.187089956677558,2.67697359149784,
13.8235269408542));
#423247=CARTESIAN_POINT('Ctrl Pts',(0.187629833256057,2.67530653339834,
13.8262006681044));
#423248=CARTESIAN_POINT('Ctrl Pts',(0.1883476058679,2.67365407144425,13.8288634856214));
#423249=CARTESIAN_POINT('Ctrl Pts',(0.189229945304323,2.67201657744458,
13.8314912288862));
#423250=CARTESIAN_POINT('Ctrl Pts',(0.190139546254182,2.67032849003059,
13.8342001611531));
#423251=CARTESIAN_POINT('Ctrl Pts',(0.191224613240091,2.66865419903748,
13.8368750301949));
#423252=CARTESIAN_POINT('Ctrl Pts',(0.192515700650559,2.66699609095406,
13.8394886372969));
#423253=CARTESIAN_POINT('Ctrl Pts',(0.192615414463006,2.66686803124477,
13.8396904925131));
#423254=CARTESIAN_POINT('Ctrl Pts',(0.192716376714451,2.66674007845698,
13.8398919674349));
#423255=CARTESIAN_POINT('Ctrl Pts',(0.19281861107592,2.66661223992683,13.8400930404591));
#423256=CARTESIAN_POINT('Ctrl Pts',(0.194411491207561,2.66462042962144,
13.8432258934518));
#423257=CARTESIAN_POINT('Ctrl Pts',(0.196304178538909,2.66266581673169,
13.8462331177034));
#423258=CARTESIAN_POINT('Ctrl Pts',(0.198504244718641,2.6608792555633,13.8489036603661));
#423259=CARTESIAN_POINT('Ctrl Pts',(0.199224131976106,2.66029467195774,
13.8497774930041));
#423260=CARTESIAN_POINT('Ctrl Pts',(0.199976853482409,2.65972831931982,
13.85061494757));
#423261=CARTESIAN_POINT('Ctrl Pts',(0.20076244600851,2.65918545828004,13.8514076489583));
#423262=CARTESIAN_POINT('Ctrl Pts',(0.202424087500611,2.65803722888861,
13.8530843267192));
#423263=CARTESIAN_POINT('Ctrl Pts',(0.204397687018218,2.65688374414613,
13.8546805203176));
#423264=CARTESIAN_POINT('Ctrl Pts',(0.206637547363053,2.65590975314353,
13.8559412814273));
#423265=CARTESIAN_POINT('Ctrl Pts',(0.206937313317593,2.6557794015601,13.8561100121513));
#423266=CARTESIAN_POINT('Ctrl Pts',(0.207241779320219,2.65565223109864,
13.8562727473908));
#423267=CARTESIAN_POINT('Ctrl Pts',(0.207550772436138,2.65552864297606,
13.8564289040185));
#423268=CARTESIAN_POINT('Ctrl Pts',(0.20895205269168,2.65496817225013,13.8571370725437));
#423269=CARTESIAN_POINT('Ctrl Pts',(0.210471914091406,2.65447363846428,
13.8577210840554));
#423270=CARTESIAN_POINT('Ctrl Pts',(0.212060360036008,2.65409217209711,
13.8581177131616));
#423271=CARTESIAN_POINT('Ctrl Pts',(0.212507721086649,2.65398473803844,
13.8582294175695));
#423272=CARTESIAN_POINT('Ctrl Pts',(0.21296044761595,2.65388611102624,13.8583265086086));
#423273=CARTESIAN_POINT('Ctrl Pts',(0.213417262509939,2.65379693456122,
13.8584082369006));
#423274=CARTESIAN_POINT('Ctrl Pts',(0.214073583012853,2.65366881189461,
13.8585256585398));
#423275=CARTESIAN_POINT('Ctrl Pts',(0.214746564272907,2.65355892152009,
13.8586122832068));
#423276=CARTESIAN_POINT('Ctrl Pts',(0.21541885144911,2.65347089743625,13.8586682984299));
#423277=CARTESIAN_POINT('Ctrl Pts',(0.215956614548388,2.65340048689472,
13.8587131050557));
#423278=CARTESIAN_POINT('Ctrl Pts',(0.216499842700019,2.65334305712858,
13.8587357943552));
#423279=CARTESIAN_POINT('Ctrl Pts',(0.217048653698843,2.65329910495289,
13.8587355499465));
#423280=CARTESIAN_POINT('Ctrl Pts',(0.217403363331688,2.65327069761387,
13.8587353919793));
#423281=CARTESIAN_POINT('Ctrl Pts',(0.217756566242839,2.65324818897368,
13.8587257282814));
#423282=CARTESIAN_POINT('Ctrl Pts',(0.2181082764625,2.6532314343732,13.8587068136939));
#423283=CARTESIAN_POINT('Ctrl Pts',(0.2181082764625,2.6532314343732,13.8587068136939));
#423284=CARTESIAN_POINT('Ctrl Pts',(0.219265032201073,2.65317632940561,
13.8586446046466));
#423285=CARTESIAN_POINT('Ctrl Pts',(0.220405661927858,2.65318339004639,
13.858482427929));
#423286=CARTESIAN_POINT('Ctrl Pts',(0.221530499458477,2.65324815821025,
13.8582284286032));
#423287=CARTESIAN_POINT('Ctrl Pts',(0.222684451918457,2.65331460281224,
13.8579678548414));
#423288=CARTESIAN_POINT('Ctrl Pts',(0.223824514827443,2.65344347238825,
13.857615680862));
#423289=CARTESIAN_POINT('Ctrl Pts',(0.224906830414324,2.65362005799896,
13.8571944833187));
#423290=CARTESIAN_POINT('Ctrl Pts',(0.227607859651537,2.65406074545018,
13.8561433417727));
#423291=CARTESIAN_POINT('Ctrl Pts',(0.230076354676476,2.65481449097715,
13.8546163505475));
#423292=CARTESIAN_POINT('Ctrl Pts',(0.232227876185974,2.65569254111439,
13.8528973491086));
#423293=CARTESIAN_POINT('Ctrl Pts',(0.232620927423026,2.65585294792005,
13.8525833129072));
#423294=CARTESIAN_POINT('Ctrl Pts',(0.233003507823617,2.656017411871,13.8522628768812));
#423295=CARTESIAN_POINT('Ctrl Pts',(0.23337525535784,2.6561846892573,13.851937733538));
#423296=CARTESIAN_POINT('Ctrl Pts',(0.235645465971667,2.65720622904672,
13.8499521282529));
#423297=CARTESIAN_POINT('Ctrl Pts',(0.237735621059127,2.65843793332097,
13.847639871647));
#423298=CARTESIAN_POINT('Ctrl Pts',(0.239576658290055,2.65974585174012,
13.8452109780794));
#423299=CARTESIAN_POINT('Ctrl Pts',(0.240404979047825,2.66033431130946,
13.8441181685877));
#423300=CARTESIAN_POINT('Ctrl Pts',(0.241183463630411,2.66093779353603,
13.8430021611332));
#423301=CARTESIAN_POINT('Ctrl Pts',(0.241908997030878,2.6615431673289,13.8418824960098));
#423302=CARTESIAN_POINT('Ctrl Pts',(0.243618735016232,2.66296974613057,
13.8392439765549));
#423303=CARTESIAN_POINT('Ctrl Pts',(0.245118579716688,2.66447212159511,
13.8364981347964));
#423304=CARTESIAN_POINT('Ctrl Pts',(0.246436715601507,2.66603008976617,
13.8336931113419));
#423305=CARTESIAN_POINT('Ctrl Pts',(0.247720496243951,2.66754745182466,
13.8309611966328));
#423306=CARTESIAN_POINT('Ctrl Pts',(0.248832772134196,2.66911943155766,
13.8281701127186));
#423307=CARTESIAN_POINT('Ctrl Pts',(0.249762399510772,2.67074009318812,
13.8253580685121));
#423308=CARTESIAN_POINT('Ctrl Pts',(0.2499639437293,2.67109145437867,13.8247484142933));
#423309=CARTESIAN_POINT('Ctrl Pts',(0.250156730223949,2.67144509153756,
13.8241378483365));
#423310=CARTESIAN_POINT('Ctrl Pts',(0.250340332111317,2.67180088696722,
13.8235269408515));
#423311=CARTESIAN_POINT('',(0.216868982438032,2.65331466404988,12.5969504640361));
#423312=CARTESIAN_POINT('Origin',(0.219795683097938,2.68759736014377,12.584524458991));
#423313=CARTESIAN_POINT('Origin',(0.219795683097938,2.68759736014377,12.584524458991));
#423314=CARTESIAN_POINT('Ctrl Pts',(0.187089956683801,2.67697359150002,
12.5893111709658));
#423315=CARTESIAN_POINT('Ctrl Pts',(0.190581907283952,2.66619097050298,
12.5770542771492));
#423316=CARTESIAN_POINT('Ctrl Pts',(0.206817591415377,2.66824188143219,
12.5737548217797));
#423317=CARTESIAN_POINT('Ctrl Pts',(0.179454232654721,2.70055156486539,
12.5663937883685));
#423318=CARTESIAN_POINT('Ctrl Pts',(0.182950637722834,2.68975518913778,
12.5540940315304));
#423319=CARTESIAN_POINT('Ctrl Pts',(0.199236230503856,2.69181564129295,
12.5508374392248));
#423320=CARTESIAN_POINT('Ctrl Pts',(0.171826212977586,2.72410574834465,
12.5434499600945));
#423321=CARTESIAN_POINT('Ctrl Pts',(0.175333986103709,2.71327426975484,
12.5311293540532));
#423322=CARTESIAN_POINT('Ctrl Pts',(0.191661153532608,2.71536600786211,
12.5278936106989));
#423323=CARTESIAN_POINT('Ctrl Pts',(0.164205294159946,2.74763800543221,
12.5204817579905));
#423324=CARTESIAN_POINT('Ctrl Pts',(0.167730428365766,2.73675291842571,
12.5081597038247));
#423325=CARTESIAN_POINT('Ctrl Pts',(0.184091858900337,2.73889479511617,
12.5049254088044));
#423326=CARTESIAN_POINT('Ctrl Pts',(0.169684384433034,2.73071939443562,
12.5369868989719));
#423327=CARTESIAN_POINT('Ctrl Pts',(0.169397391436294,2.73160558639595,
12.5342545179733));
#423328=CARTESIAN_POINT('Ctrl Pts',(0.169242176240853,2.73248976135401,
12.5314872231885));
#423329=CARTESIAN_POINT('Ctrl Pts',(0.169282541324984,2.73333177784442,
12.5287124745063));
#423330=CARTESIAN_POINT('Ctrl Pts',(0.169318944561396,2.73409115010943,
12.5262100684184));
#423331=CARTESIAN_POINT('Ctrl Pts',(0.169515365422786,2.73481542021301,
12.5237004536639));
#423332=CARTESIAN_POINT('Ctrl Pts',(0.169939156106387,2.73549967311065,
12.5212220730815));
#423333=CARTESIAN_POINT('Ctrl Pts',(0.170263604535504,2.73602352789638,
12.5193246583486));
#423334=CARTESIAN_POINT('Ctrl Pts',(0.170725736691472,2.73652985436569,
12.517417831369));
#423335=CARTESIAN_POINT('Ctrl Pts',(0.171408890154744,2.73696856389274,
12.5155812248347));
#423336=CARTESIAN_POINT('Ctrl Pts',(0.171699917202061,2.73715545650933,
12.5147988205793));
#423337=CARTESIAN_POINT('Ctrl Pts',(0.172031201066131,2.73733050078412,
12.5140295443047));
#423338=CARTESIAN_POINT('Ctrl Pts',(0.172409244280923,2.73749195071623,
12.5132817086137));
#423339=CARTESIAN_POINT('Ctrl Pts',(0.172981361545988,2.73773628334805,
12.5121499604604));
#423340=CARTESIAN_POINT('Ctrl Pts',(0.17367573375281,2.73794818038731,12.5110494206568));
#423341=CARTESIAN_POINT('Ctrl Pts',(0.174514113948424,2.73809741430203,
12.5100666561695));
#423342=CARTESIAN_POINT('Ctrl Pts',(0.174995509926128,2.73818310407221,
12.5095023550641));
#423343=CARTESIAN_POINT('Ctrl Pts',(0.175530062249885,2.73824848104504,
12.5089719619137));
#423344=CARTESIAN_POINT('Ctrl Pts',(0.176108526691945,2.73828598006134,
12.5085043804652));
#423345=CARTESIAN_POINT('Ctrl Pts',(0.176955034052607,2.73834085498711,
12.5078201359221));
#423346=CARTESIAN_POINT('Ctrl Pts',(0.177920206739881,2.73833641692304,
12.5072563000949));
#423347=CARTESIAN_POINT('Ctrl Pts',(0.178938581355058,2.73826450079449,
12.5068768744332));
#423348=CARTESIAN_POINT('Ctrl Pts',(0.179672899557749,2.73821264431509,
12.5066032824114));
#423349=CARTESIAN_POINT('Ctrl Pts',(0.180447784681282,2.73812485214003,
12.5064197834844));
#423350=CARTESIAN_POINT('Ctrl Pts',(0.181220256124129,2.73800859523801,
12.5063282718343));
#423351=CARTESIAN_POINT('Ctrl Pts',(0.18234782527957,2.73783889615328,12.5061946931565));
#423352=CARTESIAN_POINT('Ctrl Pts',(0.183494510145609,2.73760597063306,
12.5062515701262));
#423353=CARTESIAN_POINT('Ctrl Pts',(0.184592223874365,2.73733942947598,
12.5064436508398));
#423354=CARTESIAN_POINT('',(0.206817591415377,2.66824188143219,12.5737548217797));
#423355=CARTESIAN_POINT('Origin',(0.208019770758312,2.68375170943986,12.5893111709658));
#423356=CARTESIAN_POINT('Ctrl Pts',(0.184592223874365,2.73733942947598,
12.5064436508398));
#423357=CARTESIAN_POINT('Ctrl Pts',(0.187882613062957,2.72711134428183,
12.5164271754438));
#423358=CARTESIAN_POINT('Ctrl Pts',(0.191174107664169,2.71687914069164,
12.5264061185523));
#423359=CARTESIAN_POINT('Ctrl Pts',(0.194466747510725,2.70664267394882,
12.536380305637));
#423360=CARTESIAN_POINT('Ctrl Pts',(0.198581879499603,2.69384916669944,
12.5488460165097));
#423361=CARTESIAN_POINT('Ctrl Pts',(0.202698801546182,2.68104899664882,
12.5613043021964));
#423362=CARTESIAN_POINT('Ctrl Pts',(0.206817591415376,2.66824188143219,
12.5737548217797));
#423363=CARTESIAN_POINT('Ctrl Pts',(0.250340332111317,2.67180088696722,
12.5893111709658));
#423364=CARTESIAN_POINT('Ctrl Pts',(0.245142862299324,2.66172889897511,
12.5770542771492));
#423365=CARTESIAN_POINT('Ctrl Pts',(0.2294561343364,2.666390469598,12.5737548217797));
#423366=CARTESIAN_POINT('Ctrl Pts',(0.245491137981933,2.66240380977211,
12.5928319619712));
#423367=CARTESIAN_POINT('Ctrl Pts',(0.23910310553989,2.65712873082571,12.5821634970843));
#423368=CARTESIAN_POINT('Ctrl Pts',(0.227698078181869,2.66296301340908,
12.5773203894503));
#423369=CARTESIAN_POINT('Ctrl Pts',(0.23230105471023,2.65207880117041,12.5969440695591));
#423370=CARTESIAN_POINT('Ctrl Pts',(0.228293213077796,2.65238823290965,
12.5878292599214));
#423371=CARTESIAN_POINT('Ctrl Pts',(0.222995602221529,2.6592845807347,12.5813877129824));
#423372=CARTESIAN_POINT('Ctrl Pts',(0.20180153470467,2.65451899070645,12.596957478804));
#423373=CARTESIAN_POINT('Ctrl Pts',(0.205779763483049,2.65421192567137,
12.5878468778671));
#423374=CARTESIAN_POINT('Ctrl Pts',(0.212079876959397,2.66016390451229,
12.5814011370086));
#423375=CARTESIAN_POINT('Ctrl Pts',(0.190352646773942,2.66689889265637,
12.5928371701607));
#423376=CARTESIAN_POINT('Ctrl Pts',(0.195799384167996,2.66066446265324,
12.5821692192952));
#423377=CARTESIAN_POINT('Ctrl Pts',(0.207998932580136,2.6645625186441,12.5773318885715));
#423378=CARTESIAN_POINT('Ctrl Pts',(0.187089956683749,2.67697359149999,
12.5893111709658));
#423379=CARTESIAN_POINT('Ctrl Pts',(0.190581907283901,2.66619097050295,
12.5770542771492));
#423380=CARTESIAN_POINT('Ctrl Pts',(0.206817591415324,2.66824188143217,
12.5737548217797));
#423381=CARTESIAN_POINT('',(0.2294561343364,2.666390469598,12.5737548217797));
#423382=CARTESIAN_POINT('Origin',(0.230789905912218,2.68188953580805,12.5893111709658));
#423383=CARTESIAN_POINT('Ctrl Pts',(0.206817591415324,2.66824188143217,
12.5737548217797));
#423384=CARTESIAN_POINT('Ctrl Pts',(0.207095092157204,2.66727891052437,
12.5746934679442));
#423385=CARTESIAN_POINT('Ctrl Pts',(0.20757818658313,2.66626404343265,12.5756680099006));
#423386=CARTESIAN_POINT('Ctrl Pts',(0.208208905534819,2.66531131195319,
12.5765688348656));
#423387=CARTESIAN_POINT('Ctrl Pts',(0.208375881394991,2.66505908684108,
12.5768073183026));
#423388=CARTESIAN_POINT('Ctrl Pts',(0.208552961318769,2.66481113113779,
12.5770407398754));
#423389=CARTESIAN_POINT('Ctrl Pts',(0.208738602675104,2.66456924597966,
12.5772674179684));
#423390=CARTESIAN_POINT('Ctrl Pts',(0.209500424601951,2.66357661469922,
12.5781976435658));
#423391=CARTESIAN_POINT('Ctrl Pts',(0.210458644121863,2.66263670362128,
12.5790594849312));
#423392=CARTESIAN_POINT('Ctrl Pts',(0.211582375428402,2.66184745038285,
12.5797571720116));
#423393=CARTESIAN_POINT('Ctrl Pts',(0.21231452678039,2.66133322351899,12.580211740231));
#423394=CARTESIAN_POINT('Ctrl Pts',(0.213161000045717,2.66087494413759,
12.5806009430798));
#423395=CARTESIAN_POINT('Ctrl Pts',(0.214070642121469,2.66052045301169,
12.5808812374708));
#423396=CARTESIAN_POINT('Ctrl Pts',(0.214852326435155,2.66021582753334,
12.5811221033394));
#423397=CARTESIAN_POINT('Ctrl Pts',(0.21569670242707,2.65998171444748,12.581287365893));
#423398=CARTESIAN_POINT('Ctrl Pts',(0.216558339914664,2.65983936233677,
12.581359338449));
#423399=CARTESIAN_POINT('Ctrl Pts',(0.216678089733308,2.65981957833284,
12.5813693411482));
#423400=CARTESIAN_POINT('Ctrl Pts',(0.216798183449623,2.65980150776395,
12.5813775999465));
#423401=CARTESIAN_POINT('Ctrl Pts',(0.216918510922236,2.65978514747604,
12.5813841266931));
#423402=CARTESIAN_POINT('Ctrl Pts',(0.217122661032826,2.65975739026887,
12.5813952001081));
#423403=CARTESIAN_POINT('Ctrl Pts',(0.217328933346229,2.65973497356003,
12.5814007534795));
#423404=CARTESIAN_POINT('Ctrl Pts',(0.217537259330507,2.65971810316819,
12.5814005856065));
#423405=CARTESIAN_POINT('Ctrl Pts',(0.218490894236355,2.65964087711022,
12.5813998171494));
#423406=CARTESIAN_POINT('Ctrl Pts',(0.219421646708412,2.65968487070571,
12.58127954464));
#423407=CARTESIAN_POINT('Ctrl Pts',(0.220325629572498,2.65982027782726,
12.5810700125799));
#423408=CARTESIAN_POINT('Ctrl Pts',(0.221417537945624,2.65998383421276,
12.5808169217085));
#423409=CARTESIAN_POINT('Ctrl Pts',(0.222468009251053,2.66029732806586,
12.5804173076348));
#423410=CARTESIAN_POINT('Ctrl Pts',(0.223392429263112,2.66070833050984,
12.5799304713245));
#423411=CARTESIAN_POINT('Ctrl Pts',(0.224538076880387,2.66121769201706,
12.5793271277669));
#423412=CARTESIAN_POINT('Ctrl Pts',(0.225574270460432,2.66187899049208,
12.5785808224116));
#423413=CARTESIAN_POINT('Ctrl Pts',(0.226474395381594,2.66263761489803,
12.5777485681082));
#423414=CARTESIAN_POINT('Ctrl Pts',(0.227815680130172,2.6637680483764,12.576508418016));
#423415=CARTESIAN_POINT('Ctrl Pts',(0.228847969332114,2.66509981356379,
12.5750928681475));
#423416=CARTESIAN_POINT('Ctrl Pts',(0.2294561343364,2.666390469598,12.5737548217797));
#423417=CARTESIAN_POINT('Ctrl Pts',(0.2294561343364,2.666390469598,12.5737548217797));
#423418=CARTESIAN_POINT('Ctrl Pts',(0.245142862299325,2.66172889897512,
12.5770542771492));
#423419=CARTESIAN_POINT('Ctrl Pts',(0.250340332111317,2.67180088696722,
12.5893111709658));
#423420=CARTESIAN_POINT('Ctrl Pts',(0.24076523186447,2.68841589280098,12.5508408821982));
#423421=CARTESIAN_POINT('Ctrl Pts',(0.256499646385662,2.68373679841165,
12.5540974840599));
#423422=CARTESIAN_POINT('Ctrl Pts',(0.261703746838024,2.69382163568088,
12.5663972313419));
#423423=CARTESIAN_POINT('Ctrl Pts',(0.252064331109194,2.71041926118062,
12.52790050457));
#423424=CARTESIAN_POINT('Ctrl Pts',(0.267834679527419,2.70570254748252,
12.5311362602938));
#423425=CARTESIAN_POINT('Ctrl Pts',(0.27305569774653,2.71582016907758,12.5434568539655));
#423426=CARTESIAN_POINT('Ctrl Pts',(0.263354221384546,2.7324022823544,12.5049357605811));
#423427=CARTESIAN_POINT('Ctrl Pts',(0.279150229149263,2.72763054014779,
12.5081700652078));
#423428=CARTESIAN_POINT('Ctrl Pts',(0.284397082685404,2.73779822706545,
12.5204921097672));
#423429=CARTESIAN_POINT('Ctrl Pts',(0.262612884345878,2.73095879028825,
12.5064436508395));
#423430=CARTESIAN_POINT('Ctrl Pts',(0.263829637222359,2.73105022457152,
12.5062361689309));
#423431=CARTESIAN_POINT('Ctrl Pts',(0.265098859604712,2.73109342369852,
12.5061871075062));
#423432=CARTESIAN_POINT('Ctrl Pts',(0.266327790593432,2.73106612413663,
12.5063648335164));
#423433=CARTESIAN_POINT('Ctrl Pts',(0.266886046852116,2.73105372299171,
12.5064455676329));
#423434=CARTESIAN_POINT('Ctrl Pts',(0.26744377045444,2.73102638095292,12.506574497099));
#423435=CARTESIAN_POINT('Ctrl Pts',(0.267976996424862,2.7309842206763,12.5067492519495));
#423436=CARTESIAN_POINT('Ctrl Pts',(0.269048534710697,2.7308994979639,12.5071004286051));
#423437=CARTESIAN_POINT('Ctrl Pts',(0.270060478465309,2.73075101493638,
12.5076537929612));
#423438=CARTESIAN_POINT('Ctrl Pts',(0.270938249142587,2.73055927426686,
12.5083435010503));
#423439=CARTESIAN_POINT('Ctrl Pts',(0.270993510052408,2.73054720304584,
12.5083869222963));
#423440=CARTESIAN_POINT('Ctrl Pts',(0.271048242652624,2.73053494739878,
12.5084308732336));
#423441=CARTESIAN_POINT('Ctrl Pts',(0.27110243013287,2.73052250726006,12.5084753333615));
#423442=CARTESIAN_POINT('Ctrl Pts',(0.271537085244699,2.73042272092823,
12.508831962269));
#423443=CARTESIAN_POINT('Ctrl Pts',(0.271945779357663,2.73031029565999,
12.509227847131));
#423444=CARTESIAN_POINT('Ctrl Pts',(0.272317102529008,2.73019127421278,
12.5096423454524));
#423445=CARTESIAN_POINT('Ctrl Pts',(0.273480665007251,2.72981831367392,
12.5109411997424));
#423446=CARTESIAN_POINT('Ctrl Pts',(0.274351793159712,2.72936685179109,
12.5124831113042));
#423447=CARTESIAN_POINT('Ctrl Pts',(0.275004121363683,2.72889633463966,
12.5140723025008));
#423448=CARTESIAN_POINT('Ctrl Pts',(0.27506524523087,2.72885224666723,12.5142212114565));
#423449=CARTESIAN_POINT('Ctrl Pts',(0.275124476162666,2.72880800070374,
12.5143705582413));
#423450=CARTESIAN_POINT('Ctrl Pts',(0.275181890304338,2.72876365244157,
12.5145201959299));
#423451=CARTESIAN_POINT('Ctrl Pts',(0.275919460434837,2.72819393298635,
12.5164425148273));
#423452=CARTESIAN_POINT('Ctrl Pts',(0.276389037672122,2.72759630852435,
12.518463520594));
#423453=CARTESIAN_POINT('Ctrl Pts',(0.276680044914046,2.72698267543696,
12.5205025929157));
#423454=CARTESIAN_POINT('Ctrl Pts',(0.276848840648812,2.72662674392413,
12.5216853356836));
#423455=CARTESIAN_POINT('Ctrl Pts',(0.276957689226786,2.72626627653085,
12.5228750347131));
#423456=CARTESIAN_POINT('Ctrl Pts',(0.277022921633456,2.72590941159608,
12.5240609649613));
#423457=CARTESIAN_POINT('Ctrl Pts',(0.27718303107603,2.72503350575881,12.5269717671327));
#423458=CARTESIAN_POINT('Ctrl Pts',(0.27707466315077,2.72415278140866,12.5299036066169));
#423459=CARTESIAN_POINT('Ctrl Pts',(0.276784409273502,2.72327062223204,
12.532813300402));
#423460=CARTESIAN_POINT('Ctrl Pts',(0.276645070511438,2.72284713446068,
12.5342101228452));
#423461=CARTESIAN_POINT('Ctrl Pts',(0.276463491089403,2.72242400821456,
12.5356023438238));
#423462=CARTESIAN_POINT('Ctrl Pts',(0.276247037758841,2.72200455098751,
12.5369868989719));
#423463=CARTESIAN_POINT('Origin',(6.12570493509179,14.0459053753743,-1.24019187649867));
#423464=CARTESIAN_POINT('Ctrl Pts',(0.1696972233177,2.73067962102774,12.5369868989719));
#423465=CARTESIAN_POINT('Ctrl Pts',(0.164999081884238,2.74528135964877,
12.5369868989719));
#423466=CARTESIAN_POINT('Ctrl Pts',(0.149673521966447,2.74592207557002,
12.5369868989719));
#423467=CARTESIAN_POINT('Ctrl Pts',(0.168109004740274,2.7356155594723,12.5218025310016));
#423468=CARTESIAN_POINT('Ctrl Pts',(0.161477706116907,2.74539726393894,
12.5216901060418));
#423469=CARTESIAN_POINT('Ctrl Pts',(0.149720240040939,2.74592013893292,
12.5161920673678));
#423470=CARTESIAN_POINT('Ctrl Pts',(0.171692794521266,2.74046246797167,
12.5042015548894));
#423471=CARTESIAN_POINT('Ctrl Pts',(0.167156818137774,2.74502341779219,
12.4980677368513));
#423472=CARTESIAN_POINT('Ctrl Pts',(0.160372636189632,2.74543042518558,
12.4907278922777));
#423473=CARTESIAN_POINT('Ctrl Pts',(0.184590878169996,2.7373194737153,12.506463626192));
#423474=CARTESIAN_POINT('Ctrl Pts',(0.185031087393022,2.74384738717799,
12.4999376786891));
#423475=CARTESIAN_POINT('Ctrl Pts',(0.185025710877426,2.74376765820662,
12.4906970594712));
#423476=CARTESIAN_POINT('Origin',(0.148754570358523,2.72394127649578,12.5369868989719));
#423477=CARTESIAN_POINT('Origin',(0.148754570358523,2.72394127649578,14.));
#423478=CARTESIAN_POINT('Origin',(0.148754570358523,2.72394127649578,13.7435492065112));
#423479=CARTESIAN_POINT('Ctrl Pts',(0.177312854281905,2.7071637327667,13.793642941384));
#423480=CARTESIAN_POINT('Ctrl Pts',(0.174007527699429,2.71745844185384,
13.8071662555867));
#423481=CARTESIAN_POINT('Ctrl Pts',(0.157203619929424,2.71469292792477,
13.8103758687955));
#423482=CARTESIAN_POINT('Ctrl Pts',(0.172191951339028,2.72297632453001,
13.7804579775006));
#423483=CARTESIAN_POINT('Ctrl Pts',(0.16810382175015,2.735675965005,13.7901904343351));
#423484=CARTESIAN_POINT('Ctrl Pts',(0.152347685379907,2.73566643365103,
13.7927914348263));
#423485=CARTESIAN_POINT('Ctrl Pts',(0.169177083019134,2.7322857923841,13.7597120340895));
#423486=CARTESIAN_POINT('Ctrl Pts',(0.164440511054253,2.7469810969401,13.7635825532445));
#423487=CARTESIAN_POINT('Ctrl Pts',(0.149459242689212,2.74802872011601,
13.7651073818884));
#423488=CARTESIAN_POINT('Ctrl Pts',(0.16976746326803,2.73046278541545,13.7381884353898));
#423489=CARTESIAN_POINT('Ctrl Pts',(0.165142615086688,2.74481439473029,
13.7368803041982));
#423490=CARTESIAN_POINT('Ctrl Pts',(0.150024404328957,2.7456077046343,13.7363986145813));
#423491=CARTESIAN_POINT('Origin',(0.155140487395694,2.70422252012868,13.7902182540695));
#423492=CARTESIAN_POINT('Ctrl Pts',(0.187091168689846,2.67696984654341,
13.8235227101244));
#423493=CARTESIAN_POINT('Ctrl Pts',(0.183553181396909,2.68790901169596,
13.8358800583119));
#423494=CARTESIAN_POINT('Ctrl Pts',(0.1671263097235,2.68572179060922,13.8390832900376));
#423495=CARTESIAN_POINT('Ctrl Pts',(0.18341632597915,2.68831721101041,13.8124254819053));
#423496=CARTESIAN_POINT('Ctrl Pts',(0.179871467700373,2.69927761978102,
13.8247886449158));
#423497=CARTESIAN_POINT('Ctrl Pts',(0.163426089560844,2.69707073986799,
13.8279860620657));
#423498=CARTESIAN_POINT('Ctrl Pts',(0.179743130213438,2.69965948995776,
13.8013225099955));
#423499=CARTESIAN_POINT('Ctrl Pts',(0.176193075460045,2.71063597141044,
13.8136962257787));
#423500=CARTESIAN_POINT('Ctrl Pts',(0.159727840122876,2.7084145191436,13.8168830918626));
#423501=CARTESIAN_POINT('Ctrl Pts',(0.176071517312574,2.71099688125532,
13.7902140179785));
#423502=CARTESIAN_POINT('Ctrl Pts',(0.172517831151386,2.7219846024118,13.802602731458));
#423503=CARTESIAN_POINT('Ctrl Pts',(0.156031485724627,2.71975333214774,
13.8057746032558));
#423504=CARTESIAN_POINT('Origin',(0.16616014260929,2.67019547356017,13.8235269408515));
#423505=CARTESIAN_POINT('Ctrl Pts',(0.250340332111317,2.67180088696722,
13.8235269408515));
#423506=CARTESIAN_POINT('Ctrl Pts',(0.255754947306752,2.68229367311183,
13.8362179249168));
#423507=CARTESIAN_POINT('Ctrl Pts',(0.271998413181692,2.6770198869551,13.8391868794938));
#423508=CARTESIAN_POINT('Ctrl Pts',(0.245386194891663,2.6622004443687,13.8400110824519));
#423509=CARTESIAN_POINT('Ctrl Pts',(0.252767481898282,2.66904430767732,
13.8494522556836));
#423510=CARTESIAN_POINT('Ctrl Pts',(0.263745455291886,2.66127179279442,
13.85569149686));
#423511=CARTESIAN_POINT('Ctrl Pts',(0.232643764171567,2.65205016430416,
13.8586819406588));
#423512=CARTESIAN_POINT('Ctrl Pts',(0.236984242468656,2.65170914848714,
13.868010383617));
#423513=CARTESIAN_POINT('Ctrl Pts',(0.242501800617441,2.64453632346018,
13.8744918421245));
#423514=CARTESIAN_POINT('Ctrl Pts',(0.201453508494333,2.65454805315992,
13.8587686893867));
#423515=CARTESIAN_POINT('Ctrl Pts',(0.197151656003279,2.65488597780398,
13.8680909899357));
#423516=CARTESIAN_POINT('Ctrl Pts',(0.190579389803528,2.64869713958462,
13.8745789365163));
#423517=CARTESIAN_POINT('Ctrl Pts',(0.190423839053807,2.66667906152662,
13.8400379222776));
#423518=CARTESIAN_POINT('Ctrl Pts',(0.184248514519325,2.67462485291589,
13.8494748685453));
#423519=CARTESIAN_POINT('Ctrl Pts',(0.172158646404701,2.66874299995655,
13.8557104837033));
#423520=CARTESIAN_POINT('Ctrl Pts',(0.187089956677558,2.67697359149784,
13.8235269408542));
#423521=CARTESIAN_POINT('Ctrl Pts',(0.18345211567695,2.68820670022361,13.8362179249195));
#423522=CARTESIAN_POINT('Ctrl Pts',(0.166567620888867,2.68564216521555,
13.8391868794965));
#423523=CARTESIAN_POINT('Origin',(0.269890758310417,2.66171223812639,13.8235269408515));
#423524=CARTESIAN_POINT('Ctrl Pts',(0.266740338982597,2.70358186302666,
13.7902140241683));
#423525=CARTESIAN_POINT('Ctrl Pts',(0.27203205160835,2.71384618827866,13.8026027327198));
#423526=CARTESIAN_POINT('Ctrl Pts',(0.287936799781948,2.70896593031337,
13.8057746032556));
#423527=CARTESIAN_POINT('Ctrl Pts',(0.26127545720074,2.69299166709209,13.8013225161808));
#423528=CARTESIAN_POINT('Ctrl Pts',(0.26656176047881,2.7032454920144,13.8136962270464));
#423529=CARTESIAN_POINT('Ctrl Pts',(0.282447274264215,2.69837835146919,
13.8168830918628));
#423530=CARTESIAN_POINT('Ctrl Pts',(0.255808219459156,2.68239690562876,
13.8124254880875));
#423531=CARTESIAN_POINT('Ctrl Pts',(0.261086783876821,2.69263571575147,
13.8247886461868));
#423532=CARTESIAN_POINT('Ctrl Pts',(0.27695507198693,2.68778618024249,13.8279860620656));
#423533=CARTESIAN_POINT('Ctrl Pts',(0.250338530379399,2.67179739380624,
13.8235227163066));
#423534=CARTESIAN_POINT('Ctrl Pts',(0.25560686352397,2.68201635897472,13.8358800595847));
#423535=CARTESIAN_POINT('Ctrl Pts',(0.271460085171925,2.67718922792421,
13.8390832900376));
#423536=CARTESIAN_POINT('Origin',(0.286292572616938,2.69349671840617,13.7902182540695));
#423537=CARTESIAN_POINT('Ctrl Pts',(0.276123311281598,2.72176472578806,
13.7382347919292));
#423538=CARTESIAN_POINT('Ctrl Pts',(0.283022018889911,2.73518581747498,
13.7369371795942));
#423539=CARTESIAN_POINT('Ctrl Pts',(0.298078941697422,2.73350270946029,
13.7364597369711));
#423540=CARTESIAN_POINT('Ctrl Pts',(0.27699073231523,2.72344567038401,13.7595490285574));
#423541=CARTESIAN_POINT('Ctrl Pts',(0.284054931382105,2.73718651817309,
13.7633824266926));
#423542=CARTESIAN_POINT('Ctrl Pts',(0.299017953972554,2.73577173364322,
13.7648920890506));
#423543=CARTESIAN_POINT('Ctrl Pts',(0.272566932557813,2.71487294503796,
13.7803806590111));
#423544=CARTESIAN_POINT('Ctrl Pts',(0.278672410767457,2.72676075483776,
13.7901039518744));
#423545=CARTESIAN_POINT('Ctrl Pts',(0.29422733625131,2.72420542029655,13.7926933640892));
#423546=CARTESIAN_POINT('Ctrl Pts',(0.264877381131631,2.69997163467822,
13.7936647693663));
#423547=CARTESIAN_POINT('Ctrl Pts',(0.269810406920547,2.70959652888598,
13.8072068914933));
#423548=CARTESIAN_POINT('Ctrl Pts',(0.285955684697386,2.70412165214251,
13.8104111085397));
#423549=CARTESIAN_POINT('Origin',(0.29579746395794,2.71191590214668,13.7435492065112));
#423550=CARTESIAN_POINT('Origin',(0.29579746395794,2.71191590214668,14.));
#423551=CARTESIAN_POINT('Origin',(0.29579746395794,2.71191590214668,12.5369868989719));
#423552=CARTESIAN_POINT('Ctrl Pts',(0.262611124694406,2.73094049146263,
12.506462012331));
#423553=CARTESIAN_POINT('Ctrl Pts',(0.263237000882791,2.73744909092692,
12.4999388158272));
#423554=CARTESIAN_POINT('Ctrl Pts',(0.263229595946696,2.73737208565975,
12.4907030323752));
#423555=CARTESIAN_POINT('Ctrl Pts',(0.275848248095312,2.73194405871191,
12.5042014951932));
#423556=CARTESIAN_POINT('Ctrl Pts',(0.281062153627983,2.73570654276002,
12.4980716682129));
#423557=CARTESIAN_POINT('Ctrl Pts',(0.287817707302887,2.73500793001206,
12.4907355092744));
#423558=CARTESIAN_POINT('Ctrl Pts',(0.278598608864998,2.72658111018693,
12.5218047446509));
#423559=CARTESIAN_POINT('Ctrl Pts',(0.28672791366929,2.73515043188327,12.5216906929433));
#423560=CARTESIAN_POINT('Ctrl Pts',(0.298408612906582,2.73376046078403,
12.5161988840775));
#423561=CARTESIAN_POINT('Ctrl Pts',(0.276229450898405,2.72197039690782,
12.5369868989719));
#423562=CARTESIAN_POINT('Ctrl Pts',(0.283235555445726,2.73560564646888,
12.5369868989719));
#423563=CARTESIAN_POINT('Ctrl Pts',(0.298453329743572,2.73375500416414,
12.5369868989719));
#423564=CARTESIAN_POINT('Origin',(4.19924629559577E-32,-1.71423978068577E-33,
12.5));
#423565=CARTESIAN_POINT('Origin',(0.467283921384947,2.64250562881057,12.5));
#423566=CARTESIAN_POINT('',(0.467283921384947,2.64250562881057,12.5893111709658));
#423567=CARTESIAN_POINT('',(0.467283921384947,2.64250562881057,13.8235269408515));
#423568=CARTESIAN_POINT('',(0.467283921384947,2.64250562881057,12.5));
#423569=CARTESIAN_POINT('',(0.486221890222939,2.67284744872126,13.7902182540695));
#423570=CARTESIAN_POINT('',(0.467283921384947,2.64250562881057,13.8235269408515));
#423571=CARTESIAN_POINT('',(0.497196489292313,2.69043060726395,13.7435492065112));
#423572=CARTESIAN_POINT('Origin',(0.461089927072368,2.63258242055567,13.7445212918703));
#423573=CARTESIAN_POINT('',(0.497196489292313,2.69043060726395,12.5369868989719));
#423574=CARTESIAN_POINT('',(0.497196489292313,2.69043060726395,12.5));
#423575=CARTESIAN_POINT('Ctrl Pts',(0.497196489292313,2.69043060726395,
12.5369868989719));
#423576=CARTESIAN_POINT('Ctrl Pts',(0.487232905459094,2.6744672656343,12.5544431401645));
#423577=CARTESIAN_POINT('Ctrl Pts',(0.477262195405901,2.65849250659843,
12.5718848856037));
#423578=CARTESIAN_POINT('Ctrl Pts',(0.467283921384947,2.64250562881057,
12.5893111709658));
#423579=CARTESIAN_POINT('Origin',(0.341545752784778,2.92047475665393,12.5));
#423580=CARTESIAN_POINT('',(0.391698755050327,2.70780229831487,13.7435492065112));
#423581=CARTESIAN_POINT('',(0.396456161771436,2.6876286429604,13.7902182540695));
#423582=CARTESIAN_POINT('Origin',(0.40895780438952,2.63461576339665,13.7418732680443));
#423583=CARTESIAN_POINT('',(0.404665629804346,2.65281661438093,13.8235269408515));
#423584=CARTESIAN_POINT('',(0.396456161771436,2.6876286429604,13.7902182540695));
#423585=CARTESIAN_POINT('',(0.404665629804346,2.65281661438093,12.5893111709658));
#423586=CARTESIAN_POINT('',(0.404665629804346,2.65281661438093,12.5));
#423587=CARTESIAN_POINT('',(0.391698755050327,2.70780229831487,12.5369868989719));
#423588=CARTESIAN_POINT('Ctrl Pts',(0.404665629804346,2.65281661438093,
12.5893111709658));
#423589=CARTESIAN_POINT('Ctrl Pts',(0.400340122549613,2.67115881165471,
12.5718848856037));
#423590=CARTESIAN_POINT('Ctrl Pts',(0.396017894218406,2.68948710474141,
12.5544431401645));
#423591=CARTESIAN_POINT('Ctrl Pts',(0.391698755050327,2.70780229831487,
12.5369868989719));
#423592=CARTESIAN_POINT('',(0.391698755050327,2.70780229831487,12.5));
#423593=CARTESIAN_POINT('Origin',(0.438122897588471,2.66070659900838,12.5));
#423594=CARTESIAN_POINT('',(0.433645532464802,2.62662517630146,13.8587068136939));
#423595=CARTESIAN_POINT('Ctrl Pts',(0.404665629797947,2.65281661437927,
13.8235269408542));
#423596=CARTESIAN_POINT('Ctrl Pts',(0.405067829270345,2.65111109832496,
13.8262006681044));
#423597=CARTESIAN_POINT('Ctrl Pts',(0.405648522563066,2.64940562967036,
13.8288634856214));
#423598=CARTESIAN_POINT('Ctrl Pts',(0.406394455125075,2.64770166544159,
13.8314912288862));
#423599=CARTESIAN_POINT('Ctrl Pts',(0.40716343465713,2.64594505407748,13.8342001611531));
#423600=CARTESIAN_POINT('Ctrl Pts',(0.408108420912855,2.6441878911169,13.8368750301949));
#423601=CARTESIAN_POINT('Ctrl Pts',(0.409260061134546,2.64243006464152,
13.8394886372969));
#423602=CARTESIAN_POINT('Ctrl Pts',(0.409349005102356,2.64229430343894,
13.8396904925131));
#423603=CARTESIAN_POINT('Ctrl Pts',(0.40943920207018,2.64215854704271,13.8398919674349));
#423604=CARTESIAN_POINT('Ctrl Pts',(0.409530676228246,2.64202280083516,
13.8400930404591));
#423605=CARTESIAN_POINT('Ctrl Pts',(0.410955905151698,2.63990778359594,
13.8432258934518));
#423606=CARTESIAN_POINT('Ctrl Pts',(0.412682975625832,2.63780540293098,
13.8462331177034));
#423607=CARTESIAN_POINT('Ctrl Pts',(0.414730099945994,2.63584546057943,
13.8489036603661));
#423608=CARTESIAN_POINT('Ctrl Pts',(0.415399942847134,2.63520414463301,
13.8497774930041));
#423609=CARTESIAN_POINT('Ctrl Pts',(0.416103996736968,2.63457832269608,
13.85061494757));
#423610=CARTESIAN_POINT('Ctrl Pts',(0.416842727054327,2.63397323489766,
13.8514076489583));
#423611=CARTESIAN_POINT('Ctrl Pts',(0.418405248216396,2.63269338693728,
13.8530843267192));
#423612=CARTESIAN_POINT('Ctrl Pts',(0.420278261029477,2.63138287363743,
13.8546805203176));
#423613=CARTESIAN_POINT('Ctrl Pts',(0.422431279114987,2.63022955409759,
13.8559412814273));
#423614=CARTESIAN_POINT('Ctrl Pts',(0.422719422758868,2.63007520254012,
13.8561100121513));
#423615=CARTESIAN_POINT('Ctrl Pts',(0.423012510102785,2.62992363842213,
13.8562727473908));
#423616=CARTESIAN_POINT('Ctrl Pts',(0.423310401490274,2.62977527572134,
13.8564289040185));
#423617=CARTESIAN_POINT('Ctrl Pts',(0.424661335534045,2.62910245256584,
13.8571370725437));
#423618=CARTESIAN_POINT('Ctrl Pts',(0.42613583062577,2.62848568148658,13.8577210840554));
#423619=CARTESIAN_POINT('Ctrl Pts',(0.427687898097245,2.62797601132638,
13.8581177131616));
#423620=CARTESIAN_POINT('Ctrl Pts',(0.428125013717743,2.62783247066695,
13.8582294175695));
#423621=CARTESIAN_POINT('Ctrl Pts',(0.428568194819761,2.62769727041296,
13.8583265086086));
#423622=CARTESIAN_POINT('Ctrl Pts',(0.4290162209901,2.62757115602055,13.8584082369006));
#423623=CARTESIAN_POINT('Ctrl Pts',(0.429659914453921,2.62738996345757,
13.8585256585398));
#423624=CARTESIAN_POINT('Ctrl Pts',(0.430321699338655,2.62722558451386,
13.8586122832068));
#423625=CARTESIAN_POINT('Ctrl Pts',(0.430984574754729,2.62708305567682,
13.8586682984299));
#423626=CARTESIAN_POINT('Ctrl Pts',(0.431514809378862,2.62696904673562,
13.8587131050557));
#423627=CARTESIAN_POINT('Ctrl Pts',(0.43205154892454,2.62686752992485,13.8587357943552));
#423628=CARTESIAN_POINT('Ctrl Pts',(0.432594951289688,2.62677899080508,
13.8587355499465));
#423629=CARTESIAN_POINT('Ctrl Pts',(0.432946165193391,2.62672176586114,
13.8587353919793));
#423630=CARTESIAN_POINT('Ctrl Pts',(0.43329635818761,2.62667054280039,13.8587257282814));
#423631=CARTESIAN_POINT('Ctrl Pts',(0.433645532464802,2.62662517630146,
13.8587068136939));
#423632=CARTESIAN_POINT('Ctrl Pts',(0.433645532464802,2.62662517630146,
13.8587068136939));
#423633=CARTESIAN_POINT('Ctrl Pts',(0.434793947627904,2.62647596835956,
13.8586446046467));
#423634=CARTESIAN_POINT('Ctrl Pts',(0.435931357511387,2.62639003359478,
13.858482427929));
#423635=CARTESIAN_POINT('Ctrl Pts',(0.43705773144479,2.62636290154669,13.8582284286032));
#423636=CARTESIAN_POINT('Ctrl Pts',(0.438213260075057,2.62633506722148,
13.8579678548414));
#423637=CARTESIAN_POINT('Ctrl Pts',(0.439360033585576,2.62637058228371,
13.857615680862));
#423638=CARTESIAN_POINT('Ctrl Pts',(0.44045314122324,2.6264583615523,13.8571944833187));
#423639=CARTESIAN_POINT('Ctrl Pts',(0.443181103126918,2.62667742369442,
13.8561433417727));
#423640=CARTESIAN_POINT('Ctrl Pts',(0.445702821696192,2.62722745593441,
13.8546163505474));
#423641=CARTESIAN_POINT('Ctrl Pts',(0.447918753432971,2.62792721545549,
13.8528973491086));
#423642=CARTESIAN_POINT('Ctrl Pts',(0.448323571468247,2.62805505119599,
13.8525833129072));
#423643=CARTESIAN_POINT('Ctrl Pts',(0.448718284202914,2.62818778405236,
13.8522628768812));
#423644=CARTESIAN_POINT('Ctrl Pts',(0.449102429437782,2.62832420396178,
13.851937733538));
#423645=CARTESIAN_POINT('Ctrl Pts',(0.45144835108942,2.62915730142119,13.8499521282529));
#423646=CARTESIAN_POINT('Ctrl Pts',(0.453631946691186,2.63021454025739,
13.847639871647));
#423647=CARTESIAN_POINT('Ctrl Pts',(0.455573465515885,2.63136804506022,
13.8452109780794));
#423648=CARTESIAN_POINT('Ctrl Pts',(0.456446995022561,2.63188703074737,
13.8441181685877));
#423649=CARTESIAN_POINT('Ctrl Pts',(0.457272078665843,2.63242505121604,
13.8430021611332));
#423650=CARTESIAN_POINT('Ctrl Pts',(0.458044541497908,2.63296927296989,
13.8418824960098));
#423651=CARTESIAN_POINT('Ctrl Pts',(0.459864869887205,2.63425174543004,
13.8392439765549));
#423652=CARTESIAN_POINT('Ctrl Pts',(0.461482181525879,2.6356268705972,13.8364981347964));
#423653=CARTESIAN_POINT('Ctrl Pts',(0.462922920291689,2.6370722144461,13.8336931113419));
#423654=CARTESIAN_POINT('Ctrl Pts',(0.464326108354215,2.63847988756711,
13.8309611966328));
#423655=CARTESIAN_POINT('Ctrl Pts',(0.465562814179977,2.63995597585631,
13.8281701127186));
#423656=CARTESIAN_POINT('Ctrl Pts',(0.466621447266517,2.64149547160745,
13.8253580685121));
#423657=CARTESIAN_POINT('Ctrl Pts',(0.466850960062196,2.64182923594778,
13.8247484142933));
#423658=CARTESIAN_POINT('Ctrl Pts',(0.467071929787148,2.64216598251914,
13.8241378483365));
#423659=CARTESIAN_POINT('Ctrl Pts',(0.467283921384947,2.64250562881057,
13.8235269408515));
#423660=CARTESIAN_POINT('',(0.432417146080976,2.62680914300621,12.5969504640361));
#423661=CARTESIAN_POINT('Origin',(0.438128466382594,2.66073921298301,12.584524458991));
#423662=CARTESIAN_POINT('Origin',(0.438128466382594,2.66073921298301,12.584524458991));
#423663=CARTESIAN_POINT('Ctrl Pts',(0.404665629804346,2.65281661438093,
12.5893111709658));
#423664=CARTESIAN_POINT('Ctrl Pts',(0.407267077514713,2.64178524527415,
12.5770542771492));
#423665=CARTESIAN_POINT('Ctrl Pts',(0.423615907026998,2.64250597298499,
12.5737548217797));
#423666=CARTESIAN_POINT('Ctrl Pts',(0.398977136733573,2.67693851637994,
12.5663937883685));
#423667=CARTESIAN_POINT('Ctrl Pts',(0.401581902951781,2.66589307522986,
12.5540940315304));
#423668=CARTESIAN_POINT('Ctrl Pts',(0.417981252745244,2.66661924440073,
12.5508374392248));
#423669=CARTESIAN_POINT('Ctrl Pts',(0.39329438328257,2.70103607967557,12.5434499600945));
#423670=CARTESIAN_POINT('Ctrl Pts',(0.39590761852335,2.6899547258629,12.5311293540533));
#423671=CARTESIAN_POINT('Ctrl Pts',(0.412350954724039,2.69070868816462,
12.5278936106989));
#423672=CARTESIAN_POINT('Ctrl Pts',(0.387616919859073,2.72511121075171,
12.5204817579905));
#423673=CARTESIAN_POINT('Ctrl Pts',(0.39024308882838,2.71397501181074,12.5081597038247));
#423674=CARTESIAN_POINT('Ctrl Pts',(0.406724660887055,2.71477615310253,
12.5049254088044));
#423675=CARTESIAN_POINT('Ctrl Pts',(0.391698755050328,2.70780229831487,
12.5369868989719));
#423676=CARTESIAN_POINT('Ctrl Pts',(0.391484949870882,2.7087089341381,12.5342545179733));
#423677=CARTESIAN_POINT('Ctrl Pts',(0.391402319608562,2.70960281855631,
12.5314872231885));
#423678=CARTESIAN_POINT('Ctrl Pts',(0.391511182542072,2.71043874317721,
12.5287124745063));
#423679=CARTESIAN_POINT('Ctrl Pts',(0.391609360538986,2.71119262149194,
12.5262100684184));
#423680=CARTESIAN_POINT('Ctrl Pts',(0.3918641625634,2.71189847152282,12.5237004536639));
#423681=CARTESIAN_POINT('Ctrl Pts',(0.392342316081914,2.71254590475039,
12.5212220730815));
#423682=CARTESIAN_POINT('Ctrl Pts',(0.392708383963915,2.71304157089353,
12.5193246583486));
#423683=CARTESIAN_POINT('Ctrl Pts',(0.393210248721006,2.71350854454234,
12.517417831369));
#423684=CARTESIAN_POINT('Ctrl Pts',(0.393926887946714,2.71389011095029,
12.5155812248348));
#423685=CARTESIAN_POINT('Ctrl Pts',(0.39423218010882,2.714052660291,12.5147988205793));
#423686=CARTESIAN_POINT('Ctrl Pts',(0.394576629386592,2.71420011940999,
12.5140295443047));
#423687=CARTESIAN_POINT('Ctrl Pts',(0.394966574362074,2.71433021809919,
12.5132817086137));
#423688=CARTESIAN_POINT('Ctrl Pts',(0.395556703331901,2.71452710486594,
12.5121499604604));
#423689=CARTESIAN_POINT('Ctrl Pts',(0.396266036648342,2.7146816990542,12.5110494206568));
#423690=CARTESIAN_POINT('Ctrl Pts',(0.397113791152486,2.71476210063629,
12.5100666561695));
#423691=CARTESIAN_POINT('Ctrl Pts',(0.397600569836561,2.71480826703958,
12.5095023550641));
#423692=CARTESIAN_POINT('Ctrl Pts',(0.398138672311807,2.71482985549899,
12.5089719619137));
#423693=CARTESIAN_POINT('Ctrl Pts',(0.398718268479109,2.71482007951818,
12.5085043804652));
#423694=CARTESIAN_POINT('Ctrl Pts',(0.399566431972245,2.71480577364368,
12.5078201359221));
#423695=CARTESIAN_POINT('Ctrl Pts',(0.400528031383566,2.71472267981267,
12.5072563000949));
#423696=CARTESIAN_POINT('Ctrl Pts',(0.401537155609109,2.71456799599384,
12.5068768744332));
#423697=CARTESIAN_POINT('Ctrl Pts',(0.402264803644073,2.714456458312,12.5066032824114));
#423698=CARTESIAN_POINT('Ctrl Pts',(0.403029954523992,2.71430579792691,
12.5064197834844));
#423699=CARTESIAN_POINT('Ctrl Pts',(0.403790379615045,2.71412696426627,
12.5063282718343));
#423700=CARTESIAN_POINT('Ctrl Pts',(0.404900364826325,2.71386592248724,
12.5061946931565));
#423701=CARTESIAN_POINT('Ctrl Pts',(0.406024248600795,2.71354030654559,
12.5062515701262));
#423702=CARTESIAN_POINT('Ctrl Pts',(0.407096584198923,2.71318517842265,
12.5064436508398));
#423703=CARTESIAN_POINT('',(0.423615907026998,2.64250597298499,12.5737548217797));
#423704=CARTESIAN_POINT('Origin',(0.426078281186186,2.65786620454249,12.5893111709658));
#423705=CARTESIAN_POINT('Ctrl Pts',(0.407096584198923,2.71318517842265,
12.5064436508398));
#423706=CARTESIAN_POINT('Ctrl Pts',(0.409542340992688,2.70272292907287,
12.5164271754438));
#423707=CARTESIAN_POINT('Ctrl Pts',(0.411988863833398,2.69225648492929,
12.5264061185523));
#423708=CARTESIAN_POINT('Ctrl Pts',(0.414436180622228,2.68178569847023,
12.536380305637));
#423709=CARTESIAN_POINT('Ctrl Pts',(0.417494830238938,2.66869933910072,
12.5488460165097));
#423710=CARTESIAN_POINT('Ctrl Pts',(0.420554720876929,2.65560619319357,
12.5613043021964));
#423711=CARTESIAN_POINT('Ctrl Pts',(0.423615907026998,2.64250597298499,
12.5737548217797));
#423712=CARTESIAN_POINT('Ctrl Pts',(0.467283921384947,2.64250562881057,
12.5893111709658));
#423713=CARTESIAN_POINT('Ctrl Pts',(0.46128278519986,2.63289079656826,12.5770542771492));
#423714=CARTESIAN_POINT('Ctrl Pts',(0.446028214811845,2.63881547015691,
12.5737548217797));
#423715=CARTESIAN_POINT('Ctrl Pts',(0.461684913519388,2.63353507395389,
12.5928319619712));
#423716=CARTESIAN_POINT('Ctrl Pts',(0.454888168822745,2.62879823134515,
12.5821634970842));
#423717=CARTESIAN_POINT('Ctrl Pts',(0.443996638945792,2.63554271644331,
12.5773203894503));
#423718=CARTESIAN_POINT('Ctrl Pts',(0.447697135107924,2.62431953520396,
12.5969440695591));
#423719=CARTESIAN_POINT('Ctrl Pts',(0.443727850797269,2.62495461363464,
12.5878292599214));
#423720=CARTESIAN_POINT('Ctrl Pts',(0.439009983674417,2.63225981889662,
12.5813877129824));
#423721=CARTESIAN_POINT('Ctrl Pts',(0.417497997839952,2.62923759923481,
12.596957478804));
#423722=CARTESIAN_POINT('Ctrl Pts',(0.42143796073924,2.62860729335578,12.5878468778671));
#423723=CARTESIAN_POINT('Ctrl Pts',(0.428202252638728,2.63402594974239,
12.5814011370086));
#423724=CARTESIAN_POINT('Ctrl Pts',(0.407096282077668,2.64250949873489,
12.5928371701607));
#423725=CARTESIAN_POINT('Ctrl Pts',(0.412016731979506,2.63585185362063,
12.5821692192951));
#423726=CARTESIAN_POINT('Ctrl Pts',(0.424493415151723,2.63874256270109,
12.5773318885715));
#423727=CARTESIAN_POINT('Ctrl Pts',(0.404665629804292,2.65281661438091,
12.5893111709658));
#423728=CARTESIAN_POINT('Ctrl Pts',(0.40726707751466,2.64178524527414,12.5770542771492));
#423729=CARTESIAN_POINT('Ctrl Pts',(0.423615907026944,2.64250597298498,
12.5737548217797));
#423730=CARTESIAN_POINT('',(0.446028214811845,2.63881547015691,12.5737548217797));
#423731=CARTESIAN_POINT('Origin',(0.448620866155203,2.65415424973717,12.5893111709658));
#423732=CARTESIAN_POINT('Ctrl Pts',(0.423615907026944,2.64250597298498,
12.5737548217797));
#423733=CARTESIAN_POINT('Ctrl Pts',(0.423813993339227,2.64152358739678,
12.5746934679442));
#423734=CARTESIAN_POINT('Ctrl Pts',(0.424212759218763,2.64047272051103,
12.5756680099006));
#423735=CARTESIAN_POINT('Ctrl Pts',(0.424763723044868,2.6394717497171,12.5765688348656));
#423736=CARTESIAN_POINT('Ctrl Pts',(0.424909584618459,2.63920675378052,
12.5768073183026));
#423737=CARTESIAN_POINT('Ctrl Pts',(0.425065864631672,2.63894518947167,
12.5770407398754));
#423738=CARTESIAN_POINT('Ctrl Pts',(0.425231172395766,2.6386889776725,12.5772674179684));
#423739=CARTESIAN_POINT('Ctrl Pts',(0.425909550758503,2.6376375537313,12.5781976435658));
#423740=CARTESIAN_POINT('Ctrl Pts',(0.426787970403449,2.63662266634339,
12.5790594849312));
#423741=CARTESIAN_POINT('Ctrl Pts',(0.427843631120765,2.6357444447463,12.5797571720116));
#423742=CARTESIAN_POINT('Ctrl Pts',(0.428531432036273,2.63517225179777,
12.580211740231));
#423743=CARTESIAN_POINT('Ctrl Pts',(0.429337734707596,2.63464650187381,
12.5806009430798));
#423744=CARTESIAN_POINT('Ctrl Pts',(0.430215455706686,2.63421904601401,
12.5808812374708));
#423745=CARTESIAN_POINT('Ctrl Pts',(0.430969709225813,2.63385171962343,
12.5811221033394));
#423746=CARTESIAN_POINT('Ctrl Pts',(0.431792193236375,2.6335495610474,12.581287365893));
#423747=CARTESIAN_POINT('Ctrl Pts',(0.432639360677754,2.63333745114731,
12.581359338449));
#423748=CARTESIAN_POINT('Ctrl Pts',(0.432757099458768,2.6333079722511,12.5813693411482));
#423749=CARTESIAN_POINT('Ctrl Pts',(0.432875320654025,2.63328017305776,
12.5813775999465));
#423750=CARTESIAN_POINT('Ctrl Pts',(0.432993914231552,2.63325405940128,
12.5813841266931));
#423751=CARTESIAN_POINT('Ctrl Pts',(0.43319512257942,2.63320975442467,12.5813952001081));
#423752=CARTESIAN_POINT('Ctrl Pts',(0.433398881368839,2.6331705991971,12.5814007534795));
#423753=CARTESIAN_POINT('Ctrl Pts',(0.433605139072039,2.63313680443837,
12.5814005856065));
#423754=CARTESIAN_POINT('Ctrl Pts',(0.434549306195751,2.63298210524581,
12.5813998171494));
#423755=CARTESIAN_POINT('Ctrl Pts',(0.435480547552188,2.63295008748908,
12.58127954464));
#423756=CARTESIAN_POINT('Ctrl Pts',(0.436392559425332,2.63301136105901,
12.5810700125799));
#423757=CARTESIAN_POINT('Ctrl Pts',(0.437494165927224,2.63308537255494,
12.5808169217085));
#423758=CARTESIAN_POINT('Ctrl Pts',(0.438566694535404,2.6333122001196,12.5804173076348));
#423759=CARTESIAN_POINT('Ctrl Pts',(0.439521539130877,2.63364648617398,
12.5799304713245));
#423760=CARTESIAN_POINT('Ctrl Pts',(0.440704892391735,2.63406077190632,
12.5793271277669));
#423761=CARTESIAN_POINT('Ctrl Pts',(0.441791540088032,2.6346354105689,12.5785808224116));
#423762=CARTESIAN_POINT('Ctrl Pts',(0.442750504849584,2.63531814217729,
12.5777485681082));
#423763=CARTESIAN_POINT('Ctrl Pts',(0.44417946740673,2.63633548707263,12.576508418016));
#423764=CARTESIAN_POINT('Ctrl Pts',(0.445316872977787,2.63757867976795,
12.5750928681475));
#423765=CARTESIAN_POINT('Ctrl Pts',(0.446028214811845,2.63881547015691,
12.5737548217797));
#423766=CARTESIAN_POINT('Ctrl Pts',(0.446028214811845,2.63881547015691,
12.5737548217797));
#423767=CARTESIAN_POINT('Ctrl Pts',(0.461282785199861,2.63289079656826,
12.5770542771492));
#423768=CARTESIAN_POINT('Ctrl Pts',(0.467283921384947,2.64250562881057,
12.5893111709658));
#423769=CARTESIAN_POINT('Ctrl Pts',(0.459094958715932,2.65984580914408,
12.5508408821982));
#423770=CARTESIAN_POINT('Ctrl Pts',(0.474395628639503,2.65389978320067,
12.55409748406));
#423771=CARTESIAN_POINT('Ctrl Pts',(0.480404420737386,2.66352688150644,
12.5663972313419));
#423772=CARTESIAN_POINT('Ctrl Pts',(0.472149939932253,2.6808549816464,12.52790050457));
#423773=CARTESIAN_POINT('Ctrl Pts',(0.487483357862869,2.6748685326232,12.5311362602938));
#423774=CARTESIAN_POINT('Ctrl Pts',(0.49351168366197,2.68452692721261,12.5434568539655));
#423775=CARTESIAN_POINT('Ctrl Pts',(0.48519408433515,2.70184462526304,12.5049357605811));
#423776=CARTESIAN_POINT('Ctrl Pts',(0.500548590898578,2.69580123935917,
12.5081700652078));
#423777=CARTESIAN_POINT('Ctrl Pts',(0.506606746838401,2.70550742686479,
12.5204921097672));
#423778=CARTESIAN_POINT('Ctrl Pts',(0.484337556030204,2.70046636214855,
12.5064436508395));
#423779=CARTESIAN_POINT('Ctrl Pts',(0.485557713004785,2.70045831553657,
12.5062361689309));
#423780=CARTESIAN_POINT('Ctrl Pts',(0.486826233284257,2.70039791751499,
12.5061871075061));
#423781=CARTESIAN_POINT('Ctrl Pts',(0.48804884993876,2.70027053950571,12.5063648335164));
#423782=CARTESIAN_POINT('Ctrl Pts',(0.488604237837358,2.7002126765569,12.5064455676329));
#423783=CARTESIAN_POINT('Ctrl Pts',(0.489157877030412,2.70013996584525,
12.506574497099));
#423784=CARTESIAN_POINT('Ctrl Pts',(0.489685892281465,2.70005448298666,
12.5067492519495));
#423785=CARTESIAN_POINT('Ctrl Pts',(0.490746959424457,2.69988270186413,
12.5071004286051));
#423786=CARTESIAN_POINT('Ctrl Pts',(0.491743433274509,2.6996522300912,12.5076537929612));
#423787=CARTESIAN_POINT('Ctrl Pts',(0.492602654597667,2.69938958096391,
12.5083435010503));
#423788=CARTESIAN_POINT('Ctrl Pts',(0.492656747714796,2.69937304563172,
12.5083869222963));
#423789=CARTESIAN_POINT('Ctrl Pts',(0.492710299247793,2.69935636954928,
12.5084308732336));
#423790=CARTESIAN_POINT('Ctrl Pts',(0.492763292436878,2.69933955402141,
12.5084753333615));
#423791=CARTESIAN_POINT('Ctrl Pts',(0.493188367757264,2.69920467129361,
12.508831962269));
#423792=CARTESIAN_POINT('Ctrl Pts',(0.493586538271215,2.69905930774684,
12.509227847131));
#423793=CARTESIAN_POINT('Ctrl Pts',(0.49394692454245,2.69891041604802,12.5096423454524));
#423794=CARTESIAN_POINT('Ctrl Pts',(0.495076215616221,2.69844385536062,
12.5109411997424));
#423795=CARTESIAN_POINT('Ctrl Pts',(0.495907646827,2.69792289064837,12.5124831113042));
#423796=CARTESIAN_POINT('Ctrl Pts',(0.496519452946775,2.6974007682994,12.5140723025008));
#423797=CARTESIAN_POINT('Ctrl Pts',(0.49657677985029,2.69735184486344,12.5142212114565));
#423798=CARTESIAN_POINT('Ctrl Pts',(0.496632207239263,2.69730291825394,
12.5143705582413));
#423799=CARTESIAN_POINT('Ctrl Pts',(0.496685815545039,2.6972540377714,12.5145201959299));
#423800=CARTESIAN_POINT('Ctrl Pts',(0.497374494047155,2.69662609519776,
12.5164425148273));
#423801=CARTESIAN_POINT('Ctrl Pts',(0.497793796863192,2.69599218437767,
12.518463520594));
#423802=CARTESIAN_POINT('Ctrl Pts',(0.498033819009212,2.69535687331197,
12.5205025929157));
#423803=CARTESIAN_POINT('Ctrl Pts',(0.498173041367493,2.69498836771248,
12.5216853356836));
#423804=CARTESIAN_POINT('Ctrl Pts',(0.498252146321835,2.69462022757511,
12.5228750347131));
#423805=CARTESIAN_POINT('Ctrl Pts',(0.498288073867896,2.69425923303223,
12.5240609649613));
#423806=CARTESIAN_POINT('Ctrl Pts',(0.498376256102257,2.69337319129344,
12.5269717671326));
#423807=CARTESIAN_POINT('Ctrl Pts',(0.498196461551548,2.69250423047285,
12.5299036066169));
#423808=CARTESIAN_POINT('Ctrl Pts',(0.497835269307655,2.69164866499371,
12.5328133004019));
#423809=CARTESIAN_POINT('Ctrl Pts',(0.497661875998992,2.69123794374564,
12.5342101228451));
#423810=CARTESIAN_POINT('Ctrl Pts',(0.497446412050331,2.69083102582579,
12.5356023438238));
#423811=CARTESIAN_POINT('Ctrl Pts',(0.497196489292312,2.69043060726395,
12.5369868989719));
#423812=CARTESIAN_POINT('Origin',(7.25027860668965,13.5000022643794,-1.24036406790302));
#423813=CARTESIAN_POINT('Ctrl Pts',(0.391708309312677,2.70776161076147,
12.5369868989719));
#423814=CARTESIAN_POINT('Ctrl Pts',(0.388215977810789,2.72269770544401,
12.5369868989719));
#423815=CARTESIAN_POINT('Ctrl Pts',(0.372993636725075,2.72458546484474,
12.5369868989719));
#423816=CARTESIAN_POINT('Ctrl Pts',(0.390527700207791,2.71281057983639,
12.5218025310015));
#423817=CARTESIAN_POINT('Ctrl Pts',(0.384715766406483,2.72310024888808,
12.5216901060417));
#423818=CARTESIAN_POINT('Ctrl Pts',(0.373040041495134,2.72457972669485,
12.5161920673678));
#423819=CARTESIAN_POINT('Ctrl Pts',(0.394494633263108,2.71734924851006,
12.5042015548895));
#423820=CARTESIAN_POINT('Ctrl Pts',(0.390345509719021,2.72226474633153,
12.4980677368514));
#423821=CARTESIAN_POINT('Ctrl Pts',(0.3836170764577,2.72322337325147,12.4907278922777));
#423822=CARTESIAN_POINT('Ctrl Pts',(0.407093616392521,2.71316539875053,
12.506463626192));
#423823=CARTESIAN_POINT('Ctrl Pts',(0.408064446405071,2.71963570998129,
12.4999376786891));
#423824=CARTESIAN_POINT('Ctrl Pts',(0.408052589128054,2.71955668453743,
12.4906970594712));
#423825=CARTESIAN_POINT('Origin',(0.370286103668487,2.7027527081533,12.5369868989719));
#423826=CARTESIAN_POINT('Origin',(0.370286103668487,2.7027527081533,14.));
#423827=CARTESIAN_POINT('Origin',(0.370286103668487,2.7027527081533,13.7435492065112));
#423828=CARTESIAN_POINT('Ctrl Pts',(0.39738183668897,2.683703225055,13.793642941384));
#423829=CARTESIAN_POINT('Ctrl Pts',(0.394926622670047,2.69423309414853,
13.8071662555867));
#423830=CARTESIAN_POINT('Ctrl Pts',(0.377953213457921,2.69284645672205,
13.8103758687955));
#423831=CARTESIAN_POINT('Ctrl Pts',(0.393566846153838,2.69988060285367,
13.7804579775006));
#423832=CARTESIAN_POINT('Ctrl Pts',(0.390527458075338,2.71287120683648,
13.7901904343351));
#423833=CARTESIAN_POINT('Ctrl Pts',(0.37482297205525,2.71414597858428,13.7927914348262));
#423834=CARTESIAN_POINT('Ctrl Pts',(0.391320817614566,2.70940483397817,
13.7597120340895));
#423835=CARTESIAN_POINT('Ctrl Pts',(0.38779780994803,2.72443731570785,13.7635825532445));
#423836=CARTESIAN_POINT('Ctrl Pts',(0.372951781532102,2.72670256545515,
13.7651073818884));
#423837=CARTESIAN_POINT('Ctrl Pts',(0.391760641429967,2.70753977144373,
13.7381884353898));
#423838=CARTESIAN_POINT('Ctrl Pts',(0.388320971442423,2.72222059502428,
13.7368803041982));
#423839=CARTESIAN_POINT('Ctrl Pts',(0.373317727405731,2.7242435397824,13.7363986145813));
#423840=CARTESIAN_POINT('Origin',(0.375043510389596,2.68257905279884,13.7902182540695));
#423841=CARTESIAN_POINT('Ctrl Pts',(0.404666532528808,2.65281278309563,
13.8235227101244));
#423842=CARTESIAN_POINT('Ctrl Pts',(0.402031961110901,2.66400392788798,
13.8358800583119));
#423843=CARTESIAN_POINT('Ctrl Pts',(0.385481469674138,2.66316292713999,
13.8390832900376));
#423844=CARTESIAN_POINT('Ctrl Pts',(0.401928833101939,2.66442192393992,
13.8124254819052));
#423845=CARTESIAN_POINT('Ctrl Pts',(0.39928914511293,2.67563480171307,13.8247886449158));
#423846=CARTESIAN_POINT('Ctrl Pts',(0.382718606411933,2.67477571600075,
13.8279860620657));
#423847=CARTESIAN_POINT('Ctrl Pts',(0.399192360622903,2.67602586194496,
13.8013225099955));
#423848=CARTESIAN_POINT('Ctrl Pts',(0.396548803522908,2.68725518248059,
13.8136962257787));
#423849=CARTESIAN_POINT('Ctrl Pts',(0.379957285915346,2.68638319144869,
13.8168830918626));
#423850=CARTESIAN_POINT('Ctrl Pts',(0.396457067353036,2.68762479954526,
13.7902140179785));
#423851=CARTESIAN_POINT('Ctrl Pts',(0.393810807068658,2.69886561837895,
13.802602731458));
#423852=CARTESIAN_POINT('Ctrl Pts',(0.377197449355671,2.69798556268668,
13.8057746032558));
#423853=CARTESIAN_POINT('Origin',(0.383252978422506,2.64776702421936,13.8235269408515));
#423854=CARTESIAN_POINT('Ctrl Pts',(0.467283921384947,2.64250562881057,
13.8235269408515));
#423855=CARTESIAN_POINT('Ctrl Pts',(0.473535779376053,2.65252215966961,
13.8362179249168));
#423856=CARTESIAN_POINT('Ctrl Pts',(0.489295333927072,2.64594192833548,
13.8391868794938));
#423857=CARTESIAN_POINT('Ctrl Pts',(0.461563743450256,2.63334093906817,
13.8400110824519));
#423858=CARTESIAN_POINT('Ctrl Pts',(0.469478308228246,2.63956038657065,
13.8494522556836));
#423859=CARTESIAN_POINT('Ctrl Pts',(0.479786221201546,2.63091892734374,
13.85569149686));
#423860=CARTESIAN_POINT('Ctrl Pts',(0.448036370061348,2.62426305962186,
13.8586819406588));
#423861=CARTESIAN_POINT('Ctrl Pts',(0.452334609820048,2.6235693892306,13.868010383617));
#423862=CARTESIAN_POINT('Ctrl Pts',(0.457249156920298,2.61597069897555,
13.8744918421245));
#423863=CARTESIAN_POINT('Ctrl Pts',(0.417153498517881,2.62929493235242,
13.8587686893867));
#423864=CARTESIAN_POINT('Ctrl Pts',(0.412893504081745,2.62998237349456,
13.8680909899357));
#423865=CARTESIAN_POINT('Ctrl Pts',(0.40583865878635,2.62434982883307,13.8745789365163));
#423866=CARTESIAN_POINT('Ctrl Pts',(0.407149319193208,2.64228459624337,
13.8400379222776));
#423867=CARTESIAN_POINT('Ctrl Pts',(0.401642198305064,2.65070729494577,
13.8494748685453));
#423868=CARTESIAN_POINT('Ctrl Pts',(0.389113132608578,2.64583044985511,
13.8557104837033));
#423869=CARTESIAN_POINT('Ctrl Pts',(0.404665629797947,2.65281661437927,
13.8235269408542));
#423870=CARTESIAN_POINT('Ctrl Pts',(0.401955496057409,2.66430886367604,
13.8362179249195));
#423871=CARTESIAN_POINT('Ctrl Pts',(0.384918149621722,2.66312910501989,
13.8391868794965));
#423872=CARTESIAN_POINT('Origin',(0.485946976614692,2.63085700788398,13.8235269408515));
#423873=CARTESIAN_POINT('Ctrl Pts',(0.4862198031753,2.67284410348367,13.7902140241683));
#423874=CARTESIAN_POINT('Ctrl Pts',(0.492330545861212,2.68264295133528,
13.8026027327198));
#423875=CARTESIAN_POINT('Ctrl Pts',(0.507784585967035,2.67648254739715,
13.8057746032556));
#423876=CARTESIAN_POINT('Ctrl Pts',(0.479909906053499,2.66273458415115,
13.8013225161808));
#423877=CARTESIAN_POINT('Ctrl Pts',(0.486014401516539,2.67252340752409,
13.8136962270464));
#423878=CARTESIAN_POINT('Ctrl Pts',(0.501450340426531,2.66637764514013,
13.8168830918628));
#423879=CARTESIAN_POINT('Ctrl Pts',(0.47359728867826,2.65262070651389,13.8124254880875));
#423880=CARTESIAN_POINT('Ctrl Pts',(0.479692847185781,2.66239519583671,
13.8247886461867));
#423881=CARTESIAN_POINT('Ctrl Pts',(0.495113052711343,2.6562683839621,13.8279860620656));
#423882=CARTESIAN_POINT('Ctrl Pts',(0.467281840923095,2.64250229413067,
13.8235227163066));
#423883=CARTESIAN_POINT('Ctrl Pts',(0.473365584653211,2.65225783847546,
13.8358800595847));
#423884=CARTESIAN_POINT('Ctrl Pts',(0.488772600020414,2.64615458456687,
13.8390832900376));
#423885=CARTESIAN_POINT('Origin',(0.504884945452683,2.66119882779466,13.7902182540695));
#423886=CARTESIAN_POINT('Ctrl Pts',(0.497053626524536,2.69020166491958,
13.7382347919292));
#423887=CARTESIAN_POINT('Ctrl Pts',(0.505023322820197,2.70301579031652,
13.7369371795943));
#423888=CARTESIAN_POINT('Ctrl Pts',(0.519892956030771,2.70011100371444,
13.7364597369712));
#423889=CARTESIAN_POINT('Ctrl Pts',(0.498055173875918,2.69180631344405,
13.7595490285574));
#423890=CARTESIAN_POINT('Ctrl Pts',(0.506215874061809,2.70492564189087,
13.7633824266926));
#423891=CARTESIAN_POINT('Ctrl Pts',(0.521013790355526,2.70229593968879,
13.7648920890506));
#423892=CARTESIAN_POINT('Ctrl Pts',(0.49294733724627,2.6836226938832,13.780380659011));
#423893=CARTESIAN_POINT('Ctrl Pts',(0.500001466840538,2.69497329482198,
13.7901039518744));
#423894=CARTESIAN_POINT('Ctrl Pts',(0.515296351105374,2.69115859211384,
13.7926933640892));
#423895=CARTESIAN_POINT('Ctrl Pts',(0.484068777036776,2.66939773623195,
13.7936647693663));
#423896=CARTESIAN_POINT('Ctrl Pts',(0.489769906820424,2.67858851700046,
13.8072068914933));
#423897=CARTESIAN_POINT('Ctrl Pts',(0.50541520923648,2.67181586743344,13.8104111085397));
#423898=CARTESIAN_POINT('Origin',(0.515859544522057,2.67878198633736,13.7435492065112));
#423899=CARTESIAN_POINT('Origin',(0.515859544522058,2.67878198633736,14.));
#423900=CARTESIAN_POINT('Origin',(0.515859544522057,2.67878198633736,12.5369868989719));
#423901=CARTESIAN_POINT('Ctrl Pts',(0.48433431070966,2.70044826763868,12.506462012331));
#423902=CARTESIAN_POINT('Ctrl Pts',(0.48548861562589,2.70688419555548,12.4999388158272));
#423903=CARTESIAN_POINT('Ctrl Pts',(0.485474958684953,2.70680805008802,
12.4907030323752));
#423904=CARTESIAN_POINT('Ctrl Pts',(0.497609188721907,2.70036954715612,
12.5042014951932));
#423905=CARTESIAN_POINT('Ctrl Pts',(0.503112422793168,2.70369453014448,
12.4980716682127));
#423906=CARTESIAN_POINT('Ctrl Pts',(0.509788554495942,2.7024476016328,12.4907355092743));
#423907=CARTESIAN_POINT('Ctrl Pts',(0.499913267801054,2.69480026346409,
12.5218047446509));
#423908=CARTESIAN_POINT('Ctrl Pts',(0.508714002286156,2.70267845763908,
12.5216906929434));
#423909=CARTESIAN_POINT('Ctrl Pts',(0.520242539411905,2.70034102612785,
12.5161988840776));
#423910=CARTESIAN_POINT('Ctrl Pts',(0.49717617707613,2.69039800032153,12.5369868989719));
#423911=CARTESIAN_POINT('Ctrl Pts',(0.505270368811235,2.7034168171524,12.5369868989719));
#423912=CARTESIAN_POINT('Ctrl Pts',(0.520286662692129,2.70033194282706,
12.5369868989719));
#423913=CARTESIAN_POINT('Origin',(8.3705472999219E-32,-6.84555113983343E-33,
12.5));
#423914=CARTESIAN_POINT('Origin',(0.68111781325818,2.59562493167692,12.5));
#423915=CARTESIAN_POINT('',(0.68111781325818,2.59562493167692,12.5893111709658));
#423916=CARTESIAN_POINT('',(0.68111781325818,2.59562493167692,13.8235269408515));
#423917=CARTESIAN_POINT('',(0.68111781325818,2.59562493167692,12.5));
#423918=CARTESIAN_POINT('',(0.702465907569571,2.62432217141306,13.7902182540695));
#423919=CARTESIAN_POINT('',(0.68111781325818,2.59562493167692,13.8235269408515));
#423920=CARTESIAN_POINT('',(0.714837180221191,2.64095229173885,13.7435492065112));
#423921=CARTESIAN_POINT('Origin',(0.674135595355062,2.58623961011718,13.74452129187));
#423922=CARTESIAN_POINT('',(0.714837180221191,2.64095229173885,12.5369868989719));
#423923=CARTESIAN_POINT('',(0.714837180221191,2.64095229173885,12.5));
#423924=CARTESIAN_POINT('Ctrl Pts',(0.714837180221191,2.64095229173885,
12.5369868989719));
#423925=CARTESIAN_POINT('Ctrl Pts',(0.703605588851989,2.62585419139139,
12.5544431401645));
#423926=CARTESIAN_POINT('Ctrl Pts',(0.692365964350122,2.61074529248129,
12.5718848856037));
#423927=CARTESIAN_POINT('Ctrl Pts',(0.68111781325818,2.59562493167692,12.5893111709658));
#423928=CARTESIAN_POINT('Origin',(0.578455092500073,2.88291796821534,12.5));
#423929=CARTESIAN_POINT('',(0.611106435078506,2.66686522465476,13.7435492065112));
#423930=CARTESIAN_POINT('',(0.614203671726741,2.6463709226609,13.7902182540695));
#423931=CARTESIAN_POINT('Origin',(0.622342674328417,2.59251543914704,13.741873268044));
#423932=CARTESIAN_POINT('',(0.619548319923672,2.61100558037707,13.8235269408515));
#423933=CARTESIAN_POINT('',(0.614203671726741,2.6463709226609,13.7902182540695));
#423934=CARTESIAN_POINT('',(0.619548319923672,2.61100558037707,12.5893111709658));
#423935=CARTESIAN_POINT('',(0.619548319923672,2.61100558037707,12.5));
#423936=CARTESIAN_POINT('',(0.611106435078506,2.66686522465476,12.5369868989719));
#423937=CARTESIAN_POINT('Ctrl Pts',(0.619548319923672,2.61100558037707,
12.5893111709658));
#423938=CARTESIAN_POINT('Ctrl Pts',(0.616732264795966,2.62963931449986,
12.5718848856037));
#423939=CARTESIAN_POINT('Ctrl Pts',(0.613918344361108,2.64825892343789,
12.5544431401645));
#423940=CARTESIAN_POINT('Ctrl Pts',(0.611106435078506,2.66686522465476,
12.5369868989719));
#423941=CARTESIAN_POINT('',(0.611106435078506,2.66686522465476,12.5));
#423942=CARTESIAN_POINT('Origin',(0.653537368403456,2.61614223380502,12.5));
#423943=CARTESIAN_POINT('',(0.646296948995977,2.58253916104401,13.8587068136939));
#423944=CARTESIAN_POINT('Ctrl Pts',(0.619548319917159,2.61100558037594,
13.8235269408542));
#423945=CARTESIAN_POINT('Ctrl Pts',(0.619810165712327,2.60927295629476,
13.8262006681044));
#423946=CARTESIAN_POINT('Ctrl Pts',(0.620249915267873,2.60752583055217,
13.8288634856214));
#423947=CARTESIAN_POINT('Ctrl Pts',(0.620854476897341,2.60576673569509,
13.8314912288862));
#423948=CARTESIAN_POINT('Ctrl Pts',(0.621477717579682,2.60395329033967,
13.8342001611531));
#423949=CARTESIAN_POINT('Ctrl Pts',(0.622276334377607,2.60212494904122,
13.8368750301949));
#423950=CARTESIAN_POINT('Ctrl Pts',(0.623280863434857,2.60027910221905,
13.8394886372969));
#423951=CARTESIAN_POINT('Ctrl Pts',(0.623358445650594,2.60013654299158,
13.8396904925131));
#423952=CARTESIAN_POINT('Ctrl Pts',(0.623437277088852,2.59999388642334,
13.8398919674349));
#423953=CARTESIAN_POINT('Ctrl Pts',(0.623517382298079,2.59985113590701,
13.8400930404591));
#423954=CARTESIAN_POINT('Ctrl Pts',(0.624765475350002,2.59762698682474,
13.8432258934518));
#423955=CARTESIAN_POINT('Ctrl Pts',(0.626315435597862,2.59539082938103,
13.8462331177034));
#423956=CARTESIAN_POINT('Ctrl Pts',(0.628195994783854,2.5932705489393,13.8489036603661));
#423957=CARTESIAN_POINT('Ctrl Pts',(0.62881133563468,2.59257676850382,13.849777493004));
#423958=CARTESIAN_POINT('Ctrl Pts',(0.62946203654557,2.59189564200963,13.85061494757));
#423959=CARTESIAN_POINT('Ctrl Pts',(0.630148988525808,2.59123235421203,
13.8514076489583));
#423960=CARTESIAN_POINT('Ctrl Pts',(0.631601991037305,2.58982940485971,
13.8530843267192));
#423961=CARTESIAN_POINT('Ctrl Pts',(0.63336195255461,2.5883705842523,13.8546805203176));
#423962=CARTESIAN_POINT('Ctrl Pts',(0.635413800400653,2.58704561132647,
13.8559412814273));
#423963=CARTESIAN_POINT('Ctrl Pts',(0.635688404185469,2.5868682869791,13.8561100121513));
#423964=CARTESIAN_POINT('Ctrl Pts',(0.635968162422763,2.58669333783879,
13.8562727473908));
#423965=CARTESIAN_POINT('Ctrl Pts',(0.636252969663793,2.58652118788908,
13.8564289040185));
#423966=CARTESIAN_POINT('Ctrl Pts',(0.637544567252616,2.5857404898311,13.8571370725437));
#423967=CARTESIAN_POINT('Ctrl Pts',(0.638963883514774,2.58500558596821,
13.8577210840554));
#423968=CARTESIAN_POINT('Ctrl Pts',(0.640469243760167,2.5843711037858,13.8581177131616));
#423969=CARTESIAN_POINT('Ctrl Pts',(0.640893205018191,2.58419241176502,
13.8582294175695));
#423970=CARTESIAN_POINT('Ctrl Pts',(0.641323891395816,2.58402153800461,
13.8583265086086));
#423971=CARTESIAN_POINT('Ctrl Pts',(0.641760147302266,2.58385932495528,
13.8584082369006));
#423972=CARTESIAN_POINT('Ctrl Pts',(0.642386930053195,2.58362626830254,
13.8585256585398));
#423973=CARTESIAN_POINT('Ctrl Pts',(0.643033114493385,2.5834084947044,13.8586122832068));
#423974=CARTESIAN_POINT('Ctrl Pts',(0.643682166822805,2.58321240962006,
13.8586682984299));
#423975=CARTESIAN_POINT('Ctrl Pts',(0.644201344347852,2.58305556098988,
13.8587131050557));
#423976=CARTESIAN_POINT('Ctrl Pts',(0.644728023374455,2.5829106327121,13.8587357943552));
#423977=CARTESIAN_POINT('Ctrl Pts',(0.645262400852843,2.58277809586149,
13.8587355499465));
#423978=CARTESIAN_POINT('Ctrl Pts',(0.645607781757141,2.58269243413515,
13.8587353919793));
#423979=CARTESIAN_POINT('Ctrl Pts',(0.645952634358145,2.58261283753483,
13.8587257282814));
#423980=CARTESIAN_POINT('Ctrl Pts',(0.646296948995977,2.58253916104401,
13.8587068136939));
#423981=CARTESIAN_POINT('Ctrl Pts',(0.646296948995977,2.58253916104401,
13.8587068136939));
#423982=CARTESIAN_POINT('Ctrl Pts',(0.647429381069848,2.58229684308209,
13.8586446046467));
#423983=CARTESIAN_POINT('Ctrl Pts',(0.648556001834598,2.58211848479346,
13.858482427929));
#423984=CARTESIAN_POINT('Ctrl Pts',(0.649676416337789,2.58199963309271,
13.8582284286032));
#423985=CARTESIAN_POINT('Ctrl Pts',(0.650825831285958,2.58187770507316,
13.8579678548414));
#423986=CARTESIAN_POINT('Ctrl Pts',(0.6519716838095,2.58181962927471,13.857615680862));
#423987=CARTESIAN_POINT('Ctrl Pts',(0.653068309046968,2.58181801804464,
13.8571944833187));
#423988=CARTESIAN_POINT('Ctrl Pts',(0.655805049480698,2.58181399705524,
13.8561433417727));
#423989=CARTESIAN_POINT('Ctrl Pts',(0.658363209973259,2.58215665563443,
13.8546163505474));
#423990=CARTESIAN_POINT('Ctrl Pts',(0.660628805277197,2.58267346775518,
13.8528973491086));
#423991=CARTESIAN_POINT('Ctrl Pts',(0.661042696113486,2.58276788170478,
13.8525833129072));
#423992=CARTESIAN_POINT('Ctrl Pts',(0.661446914434123,2.58286800015131,
13.8522628768812));
#423993=CARTESIAN_POINT('Ctrl Pts',(0.661840900946499,2.58297265473186,
13.851937733538));
#423994=CARTESIAN_POINT('Ctrl Pts',(0.664246921914411,2.58361176573513,
13.8499521282529));
#423995=CARTESIAN_POINT('Ctrl Pts',(0.666509426562027,2.58448750338326,
13.847639871647));
#423996=CARTESIAN_POINT('Ctrl Pts',(0.66853850649305,2.58547891818562,13.8452109780794));
#423997=CARTESIAN_POINT('Ctrl Pts',(0.66945143155388,2.58592497622647,13.8441181685877));
#423998=CARTESIAN_POINT('Ctrl Pts',(0.670317623462334,2.58639395449978,
13.8430021611332));
#423999=CARTESIAN_POINT('Ctrl Pts',(0.671131875113294,2.58687340250863,
13.8418824960098));
#424000=CARTESIAN_POINT('Ctrl Pts',(0.673050679921444,2.58800323398464,
13.8392439765549));
#424001=CARTESIAN_POINT('Ctrl Pts',(0.674774695556229,2.5892419576233,13.8364981347964));
#424002=CARTESIAN_POINT('Ctrl Pts',(0.676328449324258,2.59056505862521,
13.8336931113419));
#424003=CARTESIAN_POINT('Ctrl Pts',(0.67784170682183,2.59185367497638,13.8309611966328));
#424004=CARTESIAN_POINT('Ctrl Pts',(0.679194612509888,2.59322404869775,
13.8281701127185));
#424005=CARTESIAN_POINT('Ctrl Pts',(0.680375206277863,2.59467213347936,
13.825358068512));
#424006=CARTESIAN_POINT('Ctrl Pts',(0.680631160280891,2.59498607982283,
13.8247484142932));
#424007=CARTESIAN_POINT('Ctrl Pts',(0.680878842719071,2.59530369481378,
13.8241378483365));
#424008=CARTESIAN_POINT('Ctrl Pts',(0.68111781325818,2.59562493167692,13.8235269408515));
#424009=CARTESIAN_POINT('',(0.645087644960638,2.58282264050882,12.5969504640361));
#424010=CARTESIAN_POINT('Origin',(0.653545577009588,2.61617428535095,12.584524458991));
#424011=CARTESIAN_POINT('Origin',(0.653545577009588,2.61617428535095,12.584524458991));
#424012=CARTESIAN_POINT('Ctrl Pts',(0.619548319923672,2.61100558037707,
12.5893111709658));
#424013=CARTESIAN_POINT('Ctrl Pts',(0.62124195253895,2.59979887510191,12.5770542771492));
#424014=CARTESIAN_POINT('Ctrl Pts',(0.63759512866906,2.59918462327037,12.5737548217797));
#424015=CARTESIAN_POINT('Ctrl Pts',(0.615844913794055,2.63551088373177,
12.5663937883685));
#424016=CARTESIAN_POINT('Ctrl Pts',(0.617540706872934,2.62428988274767,
12.5540940315304));
#424017=CARTESIAN_POINT('Ctrl Pts',(0.633944678711678,2.6236769363982,12.5508374392248));
#424018=CARTESIAN_POINT('Ctrl Pts',(0.612145244355821,2.65999146153581,
12.5434499600945));
#424019=CARTESIAN_POINT('Ctrl Pts',(0.613846551061904,2.64873397708158,
12.5311293540533));
#424020=CARTESIAN_POINT('Ctrl Pts',(0.630296628344904,2.64814514608311,
12.5278936106989));
#424021=CARTESIAN_POINT('Ctrl Pts',(0.608449018908829,2.68444925057535,
12.5204817579905));
#424022=CARTESIAN_POINT('Ctrl Pts',(0.610158745920418,2.67313604926652,
12.5081597038247));
#424023=CARTESIAN_POINT('Ctrl Pts',(0.626650777360416,2.67259112369652,
12.5049254088044));
#424024=CARTESIAN_POINT('Ctrl Pts',(0.611106435078507,2.66686522465476,
12.5369868989719));
#424025=CARTESIAN_POINT('Ctrl Pts',(0.610967240554547,2.66778627082908,
12.5342545179733));
#424026=CARTESIAN_POINT('Ctrl Pts',(0.610957745116111,2.66868391605411,
12.5314872231885));
#424027=CARTESIAN_POINT('Ctrl Pts',(0.611134381434141,2.66950818586508,
12.5287124745063));
#424028=CARTESIAN_POINT('Ctrl Pts',(0.611293680833185,2.67025155329372,
12.5262100684184));
#424029=CARTESIAN_POINT('Ctrl Pts',(0.611605168355191,2.67093428593639,
12.5237004536639));
#424030=CARTESIAN_POINT('Ctrl Pts',(0.612134502675841,2.67154059093258,
12.5212220730815));
#424031=CARTESIAN_POINT('Ctrl Pts',(0.612539753889369,2.67200476985674,
12.5193246583486));
#424032=CARTESIAN_POINT('Ctrl Pts',(0.613078011420432,2.67242928305247,
12.517417831369));
#424033=CARTESIAN_POINT('Ctrl Pts',(0.613823367292772,2.67275116707981,
12.5155812248347));
#424034=CARTESIAN_POINT('Ctrl Pts',(0.614140892900696,2.6728882914056,12.5147988205793));
#424035=CARTESIAN_POINT('Ctrl Pts',(0.614496215339052,2.67300718405268,
12.5140295443047));
#424036=CARTESIAN_POINT('Ctrl Pts',(0.614895467055743,2.67310506571365,
12.5132817086137));
#424037=CARTESIAN_POINT('Ctrl Pts',(0.615499680519403,2.6732531963664,12.5121499604604));
#424038=CARTESIAN_POINT('Ctrl Pts',(0.616219254449275,2.67334945890483,
12.5110494206568));
#424039=CARTESIAN_POINT('Ctrl Pts',(0.617070741595595,2.67336049309504,
12.5100666561695));
#424040=CARTESIAN_POINT('Ctrl Pts',(0.61755966355421,2.67336682890164,12.5095023550641));
#424041=CARTESIAN_POINT('Ctrl Pts',(0.618097735197687,2.67334448518002,
12.5089719619137));
#424042=CARTESIAN_POINT('Ctrl Pts',(0.618674605973363,2.67328749925963,
12.5085043804652));
#424043=CARTESIAN_POINT('Ctrl Pts',(0.619518781210861,2.67320410778808,
12.5078201359221));
#424044=CARTESIAN_POINT('Ctrl Pts',(0.62047040806087,2.67304291116586,12.5072563000949));
#424045=CARTESIAN_POINT('Ctrl Pts',(0.621463566341549,2.67280648905205,
12.5068768744332));
#424046=CARTESIAN_POINT('Ctrl Pts',(0.622179701831168,2.67263601243263,
12.5066032824114));
#424047=CARTESIAN_POINT('Ctrl Pts',(0.622930026514607,2.67242348645752,
12.5064197834844));
#424048=CARTESIAN_POINT('Ctrl Pts',(0.623673344750348,2.67218326614677,
12.5063282718343));
#424049=CARTESIAN_POINT('Ctrl Pts',(0.624758359249019,2.6718326188634,12.5061946931565));
#424050=CARTESIAN_POINT('Ctrl Pts',(0.625851962670828,2.67141647942069,
12.5062515701262));
#424051=CARTESIAN_POINT('Ctrl Pts',(0.626891783921846,2.67097512765096,
12.5064436508398));
#424052=CARTESIAN_POINT('',(0.63759512866906,2.59918462327037,12.5737548217797));
#424053=CARTESIAN_POINT('Origin',(0.641301310950734,2.61429303857096,12.5893111709658));
#424054=CARTESIAN_POINT('Ctrl Pts',(0.626891783921846,2.67097512765096,
12.5064436508398));
#424055=CARTESIAN_POINT('Ctrl Pts',(0.628476632212847,2.66034833868883,
12.5164271754438));
#424056=CARTESIAN_POINT('Ctrl Pts',(0.6300619020872,2.64971730645078,12.5264061185523));
#424057=CARTESIAN_POINT('Ctrl Pts',(0.631647609328853,2.63908188163182,
12.536380305637));
#424058=CARTESIAN_POINT('Ctrl Pts',(0.633629421764836,2.62578975770468,
12.5488460165097));
#424059=CARTESIAN_POINT('Ctrl Pts',(0.635611917926886,2.6124907686668,12.5613043021964));
#424060=CARTESIAN_POINT('Ctrl Pts',(0.63759512866906,2.59918462327037,12.5737548217797));
#424061=CARTESIAN_POINT('Ctrl Pts',(0.68111781325818,2.59562493167692,12.5893111709658));
#424062=CARTESIAN_POINT('Ctrl Pts',(0.674352947271195,2.58653124030665,
12.5770542771492));
#424063=CARTESIAN_POINT('Ctrl Pts',(0.659632051107192,2.59367958913582,
12.5737548217797));
#424064=CARTESIAN_POINT('Ctrl Pts',(0.67480625213002,2.58714059672121,12.5928319619712));
#424065=CARTESIAN_POINT('Ctrl Pts',(0.66764602639335,2.58297351335615,12.5821634970842));
#424066=CARTESIAN_POINT('Ctrl Pts',(0.657340475331822,2.59058331753354,
12.5773203894503));
#424067=CARTESIAN_POINT('Ctrl Pts',(0.660113864936306,2.57909585571297,
12.5969440695591));
#424068=CARTESIAN_POINT('Ctrl Pts',(0.656209552879632,2.58005235449292,
12.5878292599214));
#424069=CARTESIAN_POINT('Ctrl Pts',(0.652102826117502,2.58771780225609,
12.5813877129824));
#424070=CARTESIAN_POINT('Ctrl Pts',(0.630416080681929,2.58645906533392,
12.596957478804));
#424071=CARTESIAN_POINT('Ctrl Pts',(0.634291557899078,2.58550971319259,
12.5878468778671));
#424072=CARTESIAN_POINT('Ctrl Pts',(0.641475012975146,2.59035898686064,
12.5814011370086));
#424073=CARTESIAN_POINT('Ctrl Pts',(0.621130758790323,2.60053464008273,
12.5928371701607));
#424074=CARTESIAN_POINT('Ctrl Pts',(0.625492176417632,2.59349808538714,
12.5821692192952));
#424075=CARTESIAN_POINT('Ctrl Pts',(0.63816296408195,2.59536221036517,12.5773318885715));
#424076=CARTESIAN_POINT('Ctrl Pts',(0.619548319923617,2.61100558037706,
12.5893111709658));
#424077=CARTESIAN_POINT('Ctrl Pts',(0.621241952538896,2.5997988751019,12.5770542771492));
#424078=CARTESIAN_POINT('Ctrl Pts',(0.637595128669005,2.59918462327036,
12.5737548217797));
#424079=CARTESIAN_POINT('',(0.659632051107192,2.59367958913582,12.5737548217797));
#424080=CARTESIAN_POINT('Origin',(0.663466328551157,2.6087560050389,12.5893111709658));
#424081=CARTESIAN_POINT('Ctrl Pts',(0.637595128669005,2.59918462327036,
12.5737548217797));
#424082=CARTESIAN_POINT('Ctrl Pts',(0.637712482319963,2.59818936061577,
12.5746934679442));
#424083=CARTESIAN_POINT('Ctrl Pts',(0.638024265931971,2.59710948728175,
12.5756680099006));
#424084=CARTESIAN_POINT('Ctrl Pts',(0.638491808059133,2.59606693846884,
12.5765688348656));
#424085=CARTESIAN_POINT('Ctrl Pts',(0.638615584661436,2.59579093521201,
12.5768073183026));
#424086=CARTESIAN_POINT('Ctrl Pts',(0.63875002474638,2.59551750296491,12.5770407398754));
#424087=CARTESIAN_POINT('Ctrl Pts',(0.638893898822339,2.59524866957195,
12.5772674179684));
#424088=CARTESIAN_POINT('Ctrl Pts',(0.639484319124885,2.59414545002286,
12.5781976435658));
#424089=CARTESIAN_POINT('Ctrl Pts',(0.640277093157057,2.5930623402331,12.5790594849312));
#424090=CARTESIAN_POINT('Ctrl Pts',(0.641257658037249,2.59210099469719,
12.5797571720116));
#424091=CARTESIAN_POINT('Ctrl Pts',(0.641896531314664,2.59147464351364,
12.580211740231));
#424092=CARTESIAN_POINT('Ctrl Pts',(0.642657297580737,2.59088492182612,
12.5806009430798));
#424093=CARTESIAN_POINT('Ctrl Pts',(0.643497256414729,2.59038734588064,
12.5808812374708));
#424094=CARTESIAN_POINT('Ctrl Pts',(0.64421905970657,2.58995976307438,12.5811221033394));
#424095=CARTESIAN_POINT('Ctrl Pts',(0.645014178240386,2.58959156982365,
12.581287365893));
#424096=CARTESIAN_POINT('Ctrl Pts',(0.645841237876002,2.58931111369056,
12.581359338449));
#424097=CARTESIAN_POINT('Ctrl Pts',(0.645956182087224,2.58927213607926,
12.5813693411482));
#424098=CARTESIAN_POINT('Ctrl Pts',(0.646071744018875,2.58923479326052,
12.5813775999465));
#424099=CARTESIAN_POINT('Ctrl Pts',(0.646187814480624,2.58919910001754,
12.5813841266931));
#424100=CARTESIAN_POINT('Ctrl Pts',(0.646384742057413,2.58913854211381,
12.5813952001081));
#424101=CARTESIAN_POINT('Ctrl Pts',(0.646584631341723,2.58908290893908,
12.5814007534795));
#424102=CARTESIAN_POINT('Ctrl Pts',(0.646787448152858,2.58903241471201,
12.5814005856065));
#424103=CARTESIAN_POINT('Ctrl Pts',(0.647715864218004,2.58880127188245,
12.5813998171494));
#424104=CARTESIAN_POINT('Ctrl Pts',(0.648641397201237,2.58869345584639,
12.58127954464));
#424105=CARTESIAN_POINT('Ctrl Pts',(0.649555368794894,2.58868018809921,
12.5810700125799));
#424106=CARTESIAN_POINT('Ctrl Pts',(0.650659342416034,2.58866416217127,
12.5808169217085));
#424107=CARTESIAN_POINT('Ctrl Pts',(0.651746790826033,2.58880281394749,
12.5804173076348));
#424108=CARTESIAN_POINT('Ctrl Pts',(0.652725705671675,2.58905815899372,
12.5799304713245));
#424109=CARTESIAN_POINT('Ctrl Pts',(0.653938889555404,2.58937461194798,
12.5793271277669));
#424110=CARTESIAN_POINT('Ctrl Pts',(0.655068759906819,2.58985876667262,
12.5785808224116));
#424111=CARTESIAN_POINT('Ctrl Pts',(0.656080182756492,2.59046106201725,
12.5777485681082));
#424112=CARTESIAN_POINT('Ctrl Pts',(0.65758731361215,2.59135854806713,12.576508418016));
#424113=CARTESIAN_POINT('Ctrl Pts',(0.658822266305905,2.59250489502811,
12.5750928681475));
#424114=CARTESIAN_POINT('Ctrl Pts',(0.659632051107192,2.59367958913582,
12.5737548217797));
#424115=CARTESIAN_POINT('Ctrl Pts',(0.659632051107192,2.59367958913582,
12.5737548217797));
#424116=CARTESIAN_POINT('Ctrl Pts',(0.674352947271195,2.58653124030665,
12.5770542771492));
#424117=CARTESIAN_POINT('Ctrl Pts',(0.68111781325818,2.59562493167692,12.5893111709658));
#424118=CARTESIAN_POINT('Ctrl Pts',(0.674369484362452,2.61357489047098,
12.5508408821982));
#424119=CARTESIAN_POINT('Ctrl Pts',(0.689134586254481,2.60640150279514,
12.55409748406));
#424120=CARTESIAN_POINT('Ctrl Pts',(0.695908082477892,2.61550679538659,
12.5663972313419));
#424121=CARTESIAN_POINT('Ctrl Pts',(0.689093468804328,2.63345005451928,
12.52790050457));
#424122=CARTESIAN_POINT('Ctrl Pts',(0.703887914880779,2.62623370900147,
12.5311362602938));
#424123=CARTESIAN_POINT('Ctrl Pts',(0.710683430746334,2.6353686015628,12.5434568539655));
#424124=CARTESIAN_POINT('Ctrl Pts',(0.703805060705893,2.65330663796353,
12.5049357605811));
#424125=CARTESIAN_POINT('Ctrl Pts',(0.718615884360165,2.64603182609852,
12.5081700652078));
#424126=CARTESIAN_POINT('Ctrl Pts',(0.725445026675419,2.65521192111564,
12.5204921097672));
#424127=CARTESIAN_POINT('Ctrl Pts',(0.702839041189222,2.65200277591434,
12.5064436508395));
#424128=CARTESIAN_POINT('Ctrl Pts',(0.704054482318549,2.65189530195598,
12.5062361689309));
#424129=CARTESIAN_POINT('Ctrl Pts',(0.705313858701969,2.65173170872469,
12.5061871075061));
#424130=CARTESIAN_POINT('Ctrl Pts',(0.706522024710137,2.65150509994767,
12.5063648335164));
#424131=CARTESIAN_POINT('Ctrl Pts',(0.707070848233817,2.65140216026334,
12.5064455676329));
#424132=CARTESIAN_POINT('Ctrl Pts',(0.707616718640117,2.65128456475662,
12.506574497099));
#424133=CARTESIAN_POINT('Ctrl Pts',(0.70813600931742,2.65115632819037,12.5067492519495));
#424134=CARTESIAN_POINT('Ctrl Pts',(0.709179544090808,2.65089863183273,
12.5071004286051));
#424135=CARTESIAN_POINT('Ctrl Pts',(0.710153916667244,2.65058770506602,
12.5076537929612));
#424136=CARTESIAN_POINT('Ctrl Pts',(0.710988870660144,2.65025589536758,
12.5083435010503));
#424137=CARTESIAN_POINT('Ctrl Pts',(0.711041436003802,2.65023500596412,
12.5083869222963));
#424138=CARTESIAN_POINT('Ctrl Pts',(0.711093450092954,2.65021402042289,
12.5084308732336));
#424139=CARTESIAN_POINT('Ctrl Pts',(0.711144896329939,2.65019294141042,
12.5084753333615));
#424140=CARTESIAN_POINT('Ctrl Pts',(0.711557563052756,2.65002385990895,
12.508831962269));
#424141=CARTESIAN_POINT('Ctrl Pts',(0.711942560208617,2.64984652545407,
12.509227847131));
#424142=CARTESIAN_POINT('Ctrl Pts',(0.712289611268568,2.64966875435332,
12.5096423454524));
#424143=CARTESIAN_POINT('Ctrl Pts',(0.713377115692091,2.64911169840178,
12.5109411997424));
#424144=CARTESIAN_POINT('Ctrl Pts',(0.714163316923655,2.64852469779433,
12.5124831113042));
#424145=CARTESIAN_POINT('Ctrl Pts',(0.71473052949045,2.64795444488592,12.5140723025008));
#424146=CARTESIAN_POINT('Ctrl Pts',(0.714783677929208,2.64790101156382,
12.5142212114565));
#424147=CARTESIAN_POINT('Ctrl Pts',(0.714834932915229,2.6478477299068,12.5143705582413));
#424148=CARTESIAN_POINT('Ctrl Pts',(0.714884378630678,2.64779464249544,
12.5145201959299));
#424149=CARTESIAN_POINT('Ctrl Pts',(0.715519582462606,2.64711265565761,
12.5164425148273));
#424150=CARTESIAN_POINT('Ctrl Pts',(0.715885820466335,2.64644667705136,
12.5184635205941));
#424151=CARTESIAN_POINT('Ctrl Pts',(0.716073260208669,2.64579391589766,
12.5205025929158));
#424152=CARTESIAN_POINT('Ctrl Pts',(0.71618198268864,2.64541528855548,12.5216853356836));
#424153=CARTESIAN_POINT('Ctrl Pts',(0.716230817588929,2.64504192558589,
12.5228750347131));
#424154=CARTESIAN_POINT('Ctrl Pts',(0.71623720118249,2.64467920379404,12.5240609649613));
#424155=CARTESIAN_POINT('Ctrl Pts',(0.716252869370419,2.6437889226153,12.5269717671326));
#424156=CARTESIAN_POINT('Ctrl Pts',(0.716002844697329,2.64293750811518,
12.5299036066169));
#424157=CARTESIAN_POINT('Ctrl Pts',(0.715573117761601,2.64211422998061,
12.5328133004019));
#424158=CARTESIAN_POINT('Ctrl Pts',(0.7153668238102,2.64171900853796,12.5342101228451));
#424159=CARTESIAN_POINT('Ctrl Pts',(0.715118909211944,2.64133100691601,
12.5356023438238));
#424160=CARTESIAN_POINT('Ctrl Pts',(0.714837180221191,2.64095229173885,
12.5369868989719));
#424161=CARTESIAN_POINT('Origin',(8.32709028079248,12.8648684166111,-1.24137497597455));
#424162=CARTESIAN_POINT('Ctrl Pts',(0.611112641136512,2.66682389372473,
12.5369868989719));
#424163=CARTESIAN_POINT('Ctrl Pts',(0.608849360456181,2.68199494722301,
12.5369868989719));
#424164=CARTESIAN_POINT('Ctrl Pts',(0.593831540370921,2.68511718737588,
12.5369868989719));
#424165=CARTESIAN_POINT('Ctrl Pts',(0.610347498262984,2.67195229337386,
12.5218025310016));
#424166=CARTESIAN_POINT('Ctrl Pts',(0.605393606744313,2.68268145096083,
12.5216901060418));
#424167=CARTESIAN_POINT('Ctrl Pts',(0.593877323020444,2.68510768589965,
12.5161920673678));
#424168=CARTESIAN_POINT('Ctrl Pts',(0.614671175307676,2.67615251813078,
12.5042015548894));
#424169=CARTESIAN_POINT('Ctrl Pts',(0.61093651633559,2.68138985212617,12.4980677368513));
#424170=CARTESIAN_POINT('Ctrl Pts',(0.604308608374317,2.68289371906861,
12.4907278922777));
#424171=CARTESIAN_POINT('Ctrl Pts',(0.626887213763669,2.67095565569782,
12.506463626192));
#424172=CARTESIAN_POINT('Ctrl Pts',(0.628382203852189,2.67732530584298,
12.4999376786891));
#424173=CARTESIAN_POINT('Ctrl Pts',(0.628363944721972,2.67724750982792,
12.4906970594712));
#424174=CARTESIAN_POINT('Origin',(0.589353444051444,2.66357776646088,12.5369868989719));
#424175=CARTESIAN_POINT('Origin',(0.589353444051444,2.66357776646088,14.));
#424176=CARTESIAN_POINT('Origin',(0.589353444051445,2.66357776646088,13.7435492065112));
#424177=CARTESIAN_POINT('Ctrl Pts',(0.614806308536257,2.64238311516042,
13.793642941384));
#424178=CARTESIAN_POINT('Ctrl Pts',(0.613217546125108,2.65307806971884,
13.8071662555867));
#424179=CARTESIAN_POINT('Ctrl Pts',(0.596187590708747,2.65307953663824,
13.8103758687955));
#424180=CARTESIAN_POINT('Ctrl Pts',(0.612322618541459,2.65881762121425,
13.7804579775005));
#424181=CARTESIAN_POINT('Ctrl Pts',(0.610352198599527,2.67201273837864,
13.7901904343351));
#424182=CARTESIAN_POINT('Ctrl Pts',(0.594803873693005,2.67456332983262,
13.7927914348263));
#424183=CARTESIAN_POINT('Ctrl Pts',(0.61086037673216,2.66849323342245,13.7597120340895));
#424184=CARTESIAN_POINT('Ctrl Pts',(0.608574378398752,2.68376285364013,
13.7635825532445));
#424185=CARTESIAN_POINT('Ctrl Pts',(0.593962387801594,2.68723065509545,
13.7651073818884));
#424186=CARTESIAN_POINT('Ctrl Pts',(0.611146717159145,2.66659852700566,
13.7381884353898));
#424187=CARTESIAN_POINT('Ctrl Pts',(0.608915115801662,2.68151086639315,
13.7368803041982));
#424188=CARTESIAN_POINT('Ctrl Pts',(0.594126682599713,2.68474998364179,
13.7363986145813));
#424189=CARTESIAN_POINT('Origin',(0.592450680699679,2.64308346446701,13.7902182540695));
#424190=CARTESIAN_POINT('Ctrl Pts',(0.619548907359073,2.61100168825963,
13.8235227101244));
#424191=CARTESIAN_POINT('Ctrl Pts',(0.617835284454321,2.62237033746962,
13.8358800583119));
#424192=CARTESIAN_POINT('Ctrl Pts',(0.601271314044061,2.6228811537816,13.8390832900376));
#424193=CARTESIAN_POINT('Ctrl Pts',(0.617766570154019,2.6227953485643,13.8124254819053));
#424194=CARTESIAN_POINT('Ctrl Pts',(0.61604961914282,2.63418607548845,13.8247886449158));
#424195=CARTESIAN_POINT('Ctrl Pts',(0.599464194081463,2.63468050105046,
13.8279860620657));
#424196=CARTESIAN_POINT('Ctrl Pts',(0.615985031734527,2.63458372333411,
13.8013225099955));
#424197=CARTESIAN_POINT('Ctrl Pts',(0.61426556472429,2.64599115367724,13.8136962257787));
#424198=CARTESIAN_POINT('Ctrl Pts',(0.597658178658591,2.6464744268367,13.8168830918626));
#424199=CARTESIAN_POINT('Ctrl Pts',(0.614204261021079,2.6463670182211,13.7902140179785));
#424200=CARTESIAN_POINT('Ctrl Pts',(0.612483037039116,2.65778612893728,
13.802602731458));
#424201=CARTESIAN_POINT('Ctrl Pts',(0.595853226194451,2.65826314444222,
13.8057746032558));
#424202=CARTESIAN_POINT('Origin',(0.59779532889661,2.60771812218318,13.8235269408515));
#424203=CARTESIAN_POINT('Ctrl Pts',(0.68111781325818,2.59562493167692,13.8235269408515));
#424204=CARTESIAN_POINT('Ctrl Pts',(0.688165308961509,2.60509854889014,
13.8362179249168));
#424205=CARTESIAN_POINT('Ctrl Pts',(0.70333607495321,2.59725566273247,13.8391868794938));
#424206=CARTESIAN_POINT('Ctrl Pts',(0.674669661448873,2.58695698428885,
13.8400110824519));
#424207=CARTESIAN_POINT('Ctrl Pts',(0.683064833875491,2.59251062658824,
13.8494522556837));
#424208=CARTESIAN_POINT('Ctrl Pts',(0.692634088968283,2.58305773050263,
13.85569149686));
#424209=CARTESIAN_POINT('Ctrl Pts',(0.660447367829172,2.57901191725071,
13.8586819406588));
#424210=CARTESIAN_POINT('Ctrl Pts',(0.664674764973042,2.5779702085472,13.868010383617));
#424211=CARTESIAN_POINT('Ctrl Pts',(0.668953595524655,2.56999622109403,
13.8744918421245));
#424212=CARTESIAN_POINT('Ctrl Pts',(0.630077400834271,2.58654428757324,
13.8587686893867));
#424213=CARTESIAN_POINT('Ctrl Pts',(0.625887614013172,2.5875766704061,13.8680909899357));
#424214=CARTESIAN_POINT('Ctrl Pts',(0.618397138453611,2.58253790295787,
13.8745789365163));
#424215=CARTESIAN_POINT('Ctrl Pts',(0.621165287788283,2.6003061629184,13.8400379222776));
#424216=CARTESIAN_POINT('Ctrl Pts',(0.616363019527336,2.60914971726367,
13.8494748685453));
#424217=CARTESIAN_POINT('Ctrl Pts',(0.603478135114092,2.60531033464119,
13.8557104837033));
#424218=CARTESIAN_POINT('Ctrl Pts',(0.619548319917159,2.61100558037594,
13.8235269408542));
#424219=CARTESIAN_POINT('Ctrl Pts',(0.617783928929597,2.62268049122072,
13.8362179249195));
#424220=CARTESIAN_POINT('Ctrl Pts',(0.600707111575873,2.62289336001569,
13.8391868794965));
#424221=CARTESIAN_POINT('Origin',(0.698769297965203,2.58249385831494,13.8235269408515));
#424222=CARTESIAN_POINT('Ctrl Pts',(0.702463554798479,2.62431900742022,
13.7902140241682));
#424223=CARTESIAN_POINT('Ctrl Pts',(0.709352661560167,2.63358716815571,
13.8026027327198));
#424224=CARTESIAN_POINT('Ctrl Pts',(0.72425314951107,2.62618761471654,13.8057746032556));
#424225=CARTESIAN_POINT('Ctrl Pts',(0.695350633661023,2.61475744187296,
13.8013225161808));
#424226=CARTESIAN_POINT('Ctrl Pts',(0.702232696898884,2.62401612069207,
13.8136962270464));
#424227=CARTESIAN_POINT('Ctrl Pts',(0.717116337306784,2.61663263550401,
13.8168830918628));
#424228=CARTESIAN_POINT('Ctrl Pts',(0.688234646079274,2.60519175424879,
13.8124254880875));
#424229=CARTESIAN_POINT('Ctrl Pts',(0.695106633740426,2.61443687515799,
13.8247886461868));
#424230=CARTESIAN_POINT('Ctrl Pts',(0.709976137757868,2.60707355983987,
13.8279860620656));
#424231=CARTESIAN_POINT('Ctrl Pts',(0.681115467911512,2.59562177766984,
13.8235227163065));
#424232=CARTESIAN_POINT('Ctrl Pts',(0.687974135916385,2.60484897965289,
13.8358800595847));
#424233=CARTESIAN_POINT('Ctrl Pts',(0.702832413857569,2.59751021903401,
13.8390832900376));
#424234=CARTESIAN_POINT('Origin',(0.720117392276593,2.61119109805108,13.7902182540695));
#424235=CARTESIAN_POINT('Ctrl Pts',(0.714676131891023,2.64073575582309,
13.7382347919292));
#424236=CARTESIAN_POINT('Ctrl Pts',(0.723663779860099,2.65285763903972,
13.7369371795942));
#424237=CARTESIAN_POINT('Ctrl Pts',(0.738247168518024,2.64875050472583,
13.7364597369711));
#424238=CARTESIAN_POINT('Ctrl Pts',(0.715805140427811,2.64225342960495,
13.7595490285574));
#424239=CARTESIAN_POINT('Ctrl Pts',(0.725008033619357,2.65466393174321,
13.7633824266926));
#424240=CARTESIAN_POINT('Ctrl Pts',(0.739542365924913,2.65083681210318,
13.7648920890506));
#424241=CARTESIAN_POINT('Ctrl Pts',(0.710047258735931,2.63451337646721,
13.780380659011));
#424242=CARTESIAN_POINT('Ctrl Pts',(0.718003095646263,2.64525123216844,
13.7901039518744));
#424243=CARTESIAN_POINT('Ctrl Pts',(0.732936153760743,2.64020254751053,
13.7926933640891));
#424244=CARTESIAN_POINT('Ctrl Pts',(0.70003877509647,2.62105943627068,13.7936647693663));
#424245=CARTESIAN_POINT('Ctrl Pts',(0.706470068796747,2.62975494047029,
13.8072068914933));
#424246=CARTESIAN_POINT('Ctrl Pts',(0.721511278945734,2.6217295889452,13.8104111085397));
#424247=CARTESIAN_POINT('Origin',(0.732488664928214,2.62782121837687,13.7435492065112));
#424248=CARTESIAN_POINT('Origin',(0.732488664928214,2.62782121837687,14.));
#424249=CARTESIAN_POINT('Origin',(0.732488664928214,2.62782121837687,12.5369868989719));
#424250=CARTESIAN_POINT('Ctrl Pts',(0.702834331796678,2.6519850061362,12.506462012331));
#424251=CARTESIAN_POINT('Ctrl Pts',(0.704509383731982,2.65830543246707,
12.4999388158272));
#424252=CARTESIAN_POINT('Ctrl Pts',(0.704489565670892,2.65823065353485,
12.4907030323752));
#424253=CARTESIAN_POINT('Ctrl Pts',(0.716058622297308,2.65082452179361,
12.5042014951932));
#424254=CARTESIAN_POINT('Ctrl Pts',(0.721814561792379,2.65368987650902,
12.4980716682127));
#424255=CARTESIAN_POINT('Ctrl Pts',(0.72836684296802,2.65190293033714,12.4907355092743));
#424256=CARTESIAN_POINT('Ctrl Pts',(0.717901086419768,2.64508596559864,
12.5218047446509));
#424257=CARTESIAN_POINT('Ctrl Pts',(0.727314683149728,2.65222060416988,
12.5216906929434));
#424258=CARTESIAN_POINT('Ctrl Pts',(0.738614337651426,2.64895126746769,
12.5161988840776));
#424259=CARTESIAN_POINT('Ctrl Pts',(0.714814277823711,2.64092144892752,
12.5369868989719));
#424260=CARTESIAN_POINT('Ctrl Pts',(0.723942691236055,2.65323719495015,
12.5369868989719));
#424261=CARTESIAN_POINT('Ctrl Pts',(0.738657573741734,2.64893861793388,
12.5369868989719));
#424262=CARTESIAN_POINT('Origin',(1.24861436930101E-31,-1.53597860469545E-32,
12.5));
#424263=CARTESIAN_POINT('Origin',(0.890418978460709,2.53147077887094,12.5));
#424264=CARTESIAN_POINT('',(0.890418978460709,2.53147077887094,12.5893111709658));
#424265=CARTESIAN_POINT('',(0.890418978460709,2.53147077887094,13.8235269408515));
#424266=CARTESIAN_POINT('',(0.890418978460709,2.53147077887094,12.5));
#424267=CARTESIAN_POINT('',(0.914035130200043,2.55833246303679,13.7902182540695));
#424268=CARTESIAN_POINT('',(0.890418978460709,2.53147077887094,13.8235269408515));
#424269=CARTESIAN_POINT('',(0.92772074765553,2.57389887443869,13.7435492065112));
#424270=CARTESIAN_POINT('Origin',(0.882695002474742,2.52268580177247,13.7445212918696));
#424271=CARTESIAN_POINT('',(0.92772074765553,2.57389887443869,12.5369868989719));
#424272=CARTESIAN_POINT('',(0.92772074765553,2.57389887443869,12.5));
#424273=CARTESIAN_POINT('Ctrl Pts',(0.92772074765553,2.57389887443869,12.5369868989719));
#424274=CARTESIAN_POINT('Ctrl Pts',(0.915295893137825,2.55976649074023,
12.5544431401645));
#424275=CARTESIAN_POINT('Ctrl Pts',(0.902862152033936,2.54562399918533,
12.5718848856037));
#424276=CARTESIAN_POINT('Ctrl Pts',(0.890418978460709,2.53147077887094,
12.5893111709658));
#424277=CARTESIAN_POINT('Origin',(0.811514909013153,2.82617583634627,12.5));
#424278=CARTESIAN_POINT('',(0.826447302606703,2.60818060292637,13.7435492065112));
#424279=CARTESIAN_POINT('',(0.827863757583178,2.58750204049156,13.7902182540695));
#424280=CARTESIAN_POINT('Origin',(0.831585956448851,2.53316235238502,13.7418732680438));
#424281=CARTESIAN_POINT('',(0.830308018192183,2.5518187350214,13.8235269408515));
#424282=CARTESIAN_POINT('',(0.827863757583178,2.58750204049156,13.7902182540695));
#424283=CARTESIAN_POINT('',(0.830308018192183,2.5518187350214,12.5893111709658));
#424284=CARTESIAN_POINT('',(0.830308018192183,2.5518187350214,12.5));
#424285=CARTESIAN_POINT('',(0.826447302606703,2.60818060292637,12.5369868989719));
#424286=CARTESIAN_POINT('Ctrl Pts',(0.830308018192183,2.5518187350214,12.5893111709658));
#424287=CARTESIAN_POINT('Ctrl Pts',(0.829020155573762,2.57062000156696,
12.5718848856037));
#424288=CARTESIAN_POINT('Ctrl Pts',(0.827733269211485,2.58940701593086,
12.5544431401645));
#424289=CARTESIAN_POINT('Ctrl Pts',(0.826447302606703,2.60818060292637,
12.5369868989719));
#424290=CARTESIAN_POINT('',(0.826447302606703,2.60818060292637,12.5));
#424291=CARTESIAN_POINT('Origin',(0.864602655857793,2.55416787366878,12.5));
#424292=CARTESIAN_POINT('',(0.854647365963043,2.52126677375875,13.8587068136939));
#424293=CARTESIAN_POINT('Ctrl Pts',(0.830308018185601,2.5518187350208,13.8235269408542));
#424294=CARTESIAN_POINT('Ctrl Pts',(0.830427767762972,2.55007053324016,
13.8262006681044));
#424295=CARTESIAN_POINT('Ctrl Pts',(0.830723647120603,2.54829337724314,
13.8288634856214));
#424296=CARTESIAN_POINT('Ctrl Pts',(0.831182814559629,2.54649085824381,
13.8314912288862));
#424297=CARTESIAN_POINT('Ctrl Pts',(0.831656168828339,2.54463264707671,
13.8342001611531));
#424298=CARTESIAN_POINT('Ctrl Pts',(0.832303101505432,2.54274529475008,
13.8368750301949));
#424299=CARTESIAN_POINT('Ctrl Pts',(0.833153834423097,2.54082371138719,
13.8394886372969));
#424300=CARTESIAN_POINT('Ctrl Pts',(0.833219538589919,2.54067530284296,
13.8396904925131));
#424301=CARTESIAN_POINT('Ctrl Pts',(0.833286479888402,2.54052669545863,
13.8398919674349));
#424302=CARTESIAN_POINT('Ctrl Pts',(0.833354683061843,2.54037789061465,
13.8400930404591));
#424303=CARTESIAN_POINT('Ctrl Pts',(0.834417334388897,2.5380594110345,13.8432258934518));
#424304=CARTESIAN_POINT('Ctrl Pts',(0.835779869680757,2.53570435807089,
13.8462331177034));
#424305=CARTESIAN_POINT('Ctrl Pts',(0.837481348921467,2.53343784965551,
13.8489036603661));
#424306=CARTESIAN_POINT('Ctrl Pts',(0.83803809273014,2.53269622172531,13.849777493004));
#424307=CARTESIAN_POINT('Ctrl Pts',(0.838631110354884,2.53196432345828,
13.85061494757));
#424308=CARTESIAN_POINT('Ctrl Pts',(0.839261712445912,2.53124724973237,
13.8514076489583));
#424309=CARTESIAN_POINT('Ctrl Pts',(0.840595526814868,2.52973053538457,
13.8530843267192));
#424310=CARTESIAN_POINT('Ctrl Pts',(0.842230724782893,2.52813311568002,
13.8546805203176));
#424311=CARTESIAN_POINT('Ctrl Pts',(0.844167747680612,2.52664530684441,
13.8559412814274));
#424312=CARTESIAN_POINT('Ctrl Pts',(0.844426984163462,2.52644618977143,
13.8561100121513));
#424313=CARTESIAN_POINT('Ctrl Pts',(0.8446915515492,2.52624901986648,13.8562727473908));
#424314=CARTESIAN_POINT('Ctrl Pts',(0.844961379298549,2.52605422829737,
13.8564289040185));
#424315=CARTESIAN_POINT('Ctrl Pts',(0.846185045063571,2.52517085075368,
13.8571370725437));
#424316=CARTESIAN_POINT('Ctrl Pts',(0.847539737180612,2.52432270477111,
13.8577210840554));
#424317=CARTESIAN_POINT('Ctrl Pts',(0.848988372275861,2.52356763294074,
13.8581177131616));
#424318=CARTESIAN_POINT('Ctrl Pts',(0.849396357779184,2.52335497872453,
13.8582294175695));
#424319=CARTESIAN_POINT('Ctrl Pts',(0.849811683285629,2.52314956859438,
13.8583265086086));
#424320=CARTESIAN_POINT('Ctrl Pts',(0.850233265717106,2.52295233638922,
13.8584082369006));
#424321=CARTESIAN_POINT('Ctrl Pts',(0.850838966619347,2.5226689666003,13.8585256585398));
#424322=CARTESIAN_POINT('Ctrl Pts',(0.851465250364158,2.52239924759507,
13.8586122832068));
#424323=CARTESIAN_POINT('Ctrl Pts',(0.852096160270757,2.52215091117732,
13.8586682984299));
#424324=CARTESIAN_POINT('Ctrl Pts',(0.852600825655947,2.52195226665992,
13.8587131050557));
#424325=CARTESIAN_POINT('Ctrl Pts',(0.85311393920145,2.52176489138891,13.8587357943552));
#424326=CARTESIAN_POINT('Ctrl Pts',(0.853635735599124,2.52158923881833,
13.8587355499465));
#424327=CARTESIAN_POINT('Ctrl Pts',(0.853972985051072,2.52147571037424,
13.8587353919793));
#424328=CARTESIAN_POINT('Ctrl Pts',(0.854310202321688,2.52136826993659,
13.8587257282814));
#424329=CARTESIAN_POINT('Ctrl Pts',(0.854647365963043,2.52126677375875,
13.8587068136939));
#424330=CARTESIAN_POINT('Ctrl Pts',(0.854647365963043,2.52126677375875,
13.8587068136939));
#424331=CARTESIAN_POINT('Ctrl Pts',(0.855756278799083,2.52093295836288,
13.8586446046466));
#424332=CARTESIAN_POINT('Ctrl Pts',(0.856864612969799,2.5206633634954,13.858482427929));
#424333=CARTESIAN_POINT('Ctrl Pts',(0.857971611869124,2.52045358308046,
13.8582284286032));
#424334=CARTESIAN_POINT('Ctrl Pts',(0.859107263968355,2.5202383727774,13.8579678548414));
#424335=CARTESIAN_POINT('Ctrl Pts',(0.860244570045428,2.52008709260314,
13.857615680862));
#424336=CARTESIAN_POINT('Ctrl Pts',(0.861337415022675,2.51999610159688,
13.8571944833187));
#424337=CARTESIAN_POINT('Ctrl Pts',(0.864064721430431,2.51976902423498,
13.8561433417727));
#424338=CARTESIAN_POINT('Ctrl Pts',(0.866642299710296,2.51990202881707,
13.8546163505474));
#424339=CARTESIAN_POINT('Ctrl Pts',(0.86894248141846,2.52023245423809,13.8528973491086));
#424340=CARTESIAN_POINT('Ctrl Pts',(0.869362690680508,2.52029281808754,
13.8525833129072));
#424341=CARTESIAN_POINT('Ctrl Pts',(0.869773724580859,2.52035965585248,
13.8522628768812));
#424342=CARTESIAN_POINT('Ctrl Pts',(0.870174930455481,2.52043184864519,
13.851937733538));
#424343=CARTESIAN_POINT('Ctrl Pts',(0.872625039067083,2.52087272001402,
13.8499521282529));
#424344=CARTESIAN_POINT('Ctrl Pts',(0.874951396165398,2.52156112858452,
13.847639871647));
#424345=CARTESIAN_POINT('Ctrl Pts',(0.877054534010571,2.52238385568447,
13.8452109780794));
#424346=CARTESIAN_POINT('Ctrl Pts',(0.878000779259908,2.52275401763635,
13.8441181685877));
#424347=CARTESIAN_POINT('Ctrl Pts',(0.878902315069305,2.52315083274127,
13.8430021611332));
#424348=CARTESIAN_POINT('Ctrl Pts',(0.879752936828771,2.52356231635773,
13.8418824960098));
#424349=CARTESIAN_POINT('Ctrl Pts',(0.881757448726344,2.52453198800752,
13.8392439765549));
#424350=CARTESIAN_POINT('Ctrl Pts',(0.88357669531762,2.52562606661625,13.8364981347964));
#424351=CARTESIAN_POINT('Ctrl Pts',(0.885233124112882,2.52681811975228,
13.8336931113419));
#424352=CARTESIAN_POINT('Ctrl Pts',(0.886846380566513,2.52797910380439,
13.8309611966328));
#424353=CARTESIAN_POINT('Ctrl Pts',(0.888306482752718,2.52923464334691,
13.8281701127186));
#424354=CARTESIAN_POINT('Ctrl Pts',(0.889601180545386,2.53058168039367,
13.8253580685121));
#424355=CARTESIAN_POINT('Ctrl Pts',(0.88988187242412,2.53087371947918,13.8247484142933));
#424356=CARTESIAN_POINT('Ctrl Pts',(0.890154619289783,2.53117008921438,
13.8241378483365));
#424357=CARTESIAN_POINT('Ctrl Pts',(0.890418978460709,2.53147077887094,
13.8235269408515));
#424358=CARTESIAN_POINT('',(0.853465191995009,2.5216478794746,12.5969504640361));
#424359=CARTESIAN_POINT('Origin',(0.864613449649006,2.55419914948822,12.584524458991));
#424360=CARTESIAN_POINT('Origin',(0.864613449649006,2.55419914948822,12.584524458991));
#424361=CARTESIAN_POINT('Ctrl Pts',(0.830308018192183,2.5518187350214,12.5893111709658));
#424362=CARTESIAN_POINT('Ctrl Pts',(0.831082564866749,2.5405112723525,12.5770542771492));
#424363=CARTESIAN_POINT('Ctrl Pts',(0.847331259925621,2.53856612872316,
12.5737548217797));
#424364=CARTESIAN_POINT('Ctrl Pts',(0.828614344560504,2.57654436098097,
12.5663937883685));
#424365=CARTESIAN_POINT('Ctrl Pts',(0.829389879276917,2.56522247407308,
12.5540940315303));
#424366=CARTESIAN_POINT('Ctrl Pts',(0.845689307434817,2.56327449126019,
12.5508374392248));
#424367=CARTESIAN_POINT('Ctrl Pts',(0.826922379824748,2.60124503908716,
12.5434499600944));
#424368=CARTESIAN_POINT('Ctrl Pts',(0.827700436080648,2.58988634069314,
12.5311293540533));
#424369=CARTESIAN_POINT('Ctrl Pts',(0.844047781895784,2.58795863496758,
12.5278936106989));
#424370=CARTESIAN_POINT('Ctrl Pts',(0.825231990124768,2.62592272353936,
12.5204817579905));
#424371=CARTESIAN_POINT('Ctrl Pts',(0.826013897227463,2.61450780735084,
12.5081597038247));
#424372=CARTESIAN_POINT('Ctrl Pts',(0.842406636300544,2.61262044130881,
12.5049254088044));
#424373=CARTESIAN_POINT('Ctrl Pts',(0.826447302606703,2.60818060292637,
12.5369868989719));
#424374=CARTESIAN_POINT('Ctrl Pts',(0.826383645054817,2.60910993004145,
12.5342545179733));
#424375=CARTESIAN_POINT('Ctrl Pts',(0.826447347630837,2.61000536239243,
12.5314872231885));
#424376=CARTESIAN_POINT('Ctrl Pts',(0.826690581847834,2.61081249201388,
12.5287124745062));
#424377=CARTESIAN_POINT('Ctrl Pts',(0.826909942537789,2.61154040156883,
12.5262100684184));
#424378=CARTESIAN_POINT('Ctrl Pts',(0.827276042659319,2.61219547335019,
12.5237004536639));
#424379=CARTESIAN_POINT('Ctrl Pts',(0.827853035149533,2.61275661525529,
12.5212220730815));
#424380=CARTESIAN_POINT('Ctrl Pts',(0.828294772814625,2.6131862179263,12.5193246583486));
#424381=CARTESIAN_POINT('Ctrl Pts',(0.828865841104599,2.61356544560367,
12.517417831369));
#424382=CARTESIAN_POINT('Ctrl Pts',(0.829634953403218,2.61382550516533,
12.5155812248348));
#424383=CARTESIAN_POINT('Ctrl Pts',(0.829962599376427,2.61393629193642,
12.5147988205793));
#424384=CARTESIAN_POINT('Ctrl Pts',(0.830326430363164,2.61402582690065,
12.5140295443047));
#424385=CARTESIAN_POINT('Ctrl Pts',(0.830732331866762,2.61409084014709,
12.5132817086137));
#424386=CARTESIAN_POINT('Ctrl Pts',(0.831346608883344,2.61418922890078,
12.5121499604604));
#424387=CARTESIAN_POINT('Ctrl Pts',(0.832071634780866,2.61422651917806,
12.5110494206568));
#424388=CARTESIAN_POINT('Ctrl Pts',(0.832921188062887,2.61416811254567,
12.5100666561695));
#424389=CARTESIAN_POINT('Ctrl Pts',(0.833408999601075,2.61413457559184,
12.5095023550641));
#424390=CARTESIAN_POINT('Ctrl Pts',(0.833943459634806,2.61406844838295,
12.5089719619137));
#424391=CARTESIAN_POINT('Ctrl Pts',(0.834513766039022,2.61396463175489,
12.5085043804652));
#424392=CARTESIAN_POINT('Ctrl Pts',(0.835348335173957,2.61381270964279,
12.5078201359221));
#424393=CARTESIAN_POINT('Ctrl Pts',(0.836283656542937,2.61357448296628,
12.5072563000949));
#424394=CARTESIAN_POINT('Ctrl Pts',(0.837254239574256,2.61325789590764,
12.5068768744332));
#424395=CARTESIAN_POINT('Ctrl Pts',(0.837954096755,2.61302961484443,12.5066032824114));
#424396=CARTESIAN_POINT('Ctrl Pts',(0.838684601954986,2.61275663760459,
12.5064197834844));
#424397=CARTESIAN_POINT('Ctrl Pts',(0.839405866675194,2.61245662927027,
12.5063282718343));
#424398=CARTESIAN_POINT('Ctrl Pts',(0.840458689868784,2.61201870998238,
12.5061946931565));
#424399=CARTESIAN_POINT('Ctrl Pts',(0.841514735187592,2.61151481637794,
12.5062515701262));
#424400=CARTESIAN_POINT('Ctrl Pts',(0.842515122252634,2.61099017808463,
12.5064436508398));
#424401=CARTESIAN_POINT('',(0.847331259925621,2.53856612872316,12.5737548217797));
#424402=CARTESIAN_POINT('Origin',(0.852256586298173,2.55332218375572,12.5893111709658));
#424403=CARTESIAN_POINT('Ctrl Pts',(0.842515122252634,2.61099017808463,
12.5064436508398));
#424404=CARTESIAN_POINT('Ctrl Pts',(0.843228515136987,2.60026956903739,
12.5164271754438));
#424405=CARTESIAN_POINT('Ctrl Pts',(0.843941982335526,2.58954469647043,
12.5264061185523));
#424406=CARTESIAN_POINT('Ctrl Pts',(0.844655527409933,2.57881541028901,
12.536380305637));
#424407=CARTESIAN_POINT('Ctrl Pts',(0.845547314030407,2.56540597869594,
12.5488460165097));
#424408=CARTESIAN_POINT('Ctrl Pts',(0.846439222531624,2.55198964910518,
12.5613043021964));
#424409=CARTESIAN_POINT('Ctrl Pts',(0.847331259925621,2.53856612872316,
12.5737548217797));
#424410=CARTESIAN_POINT('Ctrl Pts',(0.890418978460709,2.53147077887094,
12.5893111709658));
#424411=CARTESIAN_POINT('Ctrl Pts',(0.882935401738845,2.52295874538841,
12.5770542771492));
#424412=CARTESIAN_POINT('Ctrl Pts',(0.868846144934049,2.53128319837605,
12.5737548217797));
#424413=CARTESIAN_POINT('Ctrl Pts',(0.883436866467923,2.5235291256655,12.5928319619712));
#424414=CARTESIAN_POINT('Ctrl Pts',(0.875960809812146,2.51995953279641,
12.5821634970842));
#424415=CARTESIAN_POINT('Ctrl Pts',(0.86630981930806,2.52838401406174,12.5773203894503));
#424416=CARTESIAN_POINT('Ctrl Pts',(0.868137645904655,2.51670871882308,
12.5969440695591));
#424417=CARTESIAN_POINT('Ctrl Pts',(0.864324288654534,2.51798027261073,
12.5878292599214));
#424418=CARTESIAN_POINT('Ctrl Pts',(0.860856031842167,2.52595495058492,
12.5813877129824));
#424419=CARTESIAN_POINT('Ctrl Pts',(0.839138848518301,2.52646807308894,
12.596957478804));
#424420=CARTESIAN_POINT('Ctrl Pts',(0.842924049391841,2.52520599246717,
12.5878468778671));
#424421=CARTESIAN_POINT('Ctrl Pts',(0.850478862936143,2.52945361230049,
12.5814011370086));
#424422=CARTESIAN_POINT('Ctrl Pts',(0.831031712782593,2.54125365245881,
12.5928371701607));
#424423=CARTESIAN_POINT('Ctrl Pts',(0.834805073620663,2.53388501529245,
12.5821692192952));
#424424=CARTESIAN_POINT('Ctrl Pts',(0.847585643775695,2.5347101507239,12.5773318885715));
#424425=CARTESIAN_POINT('Ctrl Pts',(0.830308018192128,2.55181873502139,
12.5893111709658));
#424426=CARTESIAN_POINT('Ctrl Pts',(0.831082564866694,2.54051127235249,
12.5770542771492));
#424427=CARTESIAN_POINT('Ctrl Pts',(0.847331259925566,2.53856612872316,
12.5737548217797));
#424428=CARTESIAN_POINT('',(0.868846144934049,2.53128319837605,12.5737548217797));
#424429=CARTESIAN_POINT('Origin',(0.873896531994843,2.54599691954156,12.5893111709658));
#424430=CARTESIAN_POINT('Ctrl Pts',(0.847331259925566,2.53856612872316,
12.5737548217797));
#424431=CARTESIAN_POINT('Ctrl Pts',(0.847367099946014,2.53756461231094,
12.5746934679442));
#424432=CARTESIAN_POINT('Ctrl Pts',(0.847589826421995,2.53646291890752,
12.5756680099006));
#424433=CARTESIAN_POINT('Ctrl Pts',(0.847970835434494,2.53538573006596,
12.5765688348656));
#424434=CARTESIAN_POINT('Ctrl Pts',(0.848071703352644,2.53510055624503,
12.5768073183026));
#424435=CARTESIAN_POINT('Ctrl Pts',(0.848183408832736,2.53481707570617,
12.5770407398754));
#424436=CARTESIAN_POINT('Ctrl Pts',(0.848304891762323,2.5345374097613,12.5772674179684));
#424437=CARTESIAN_POINT('Ctrl Pts',(0.848803424854977,2.5333897363484,12.5781976435658));
#424438=CARTESIAN_POINT('Ctrl Pts',(0.849505277493991,2.53224561207373,
12.5790594849312));
#424439=CARTESIAN_POINT('Ctrl Pts',(0.850404221039561,2.53120754019494,
12.5797571720116));
#424440=CARTESIAN_POINT('Ctrl Pts',(0.850989915082629,2.53053119904016,
12.580211740231));
#424441=CARTESIAN_POINT('Ctrl Pts',(0.851700082169469,2.52988143008961,
12.5806009430798));
#424442=CARTESIAN_POINT('Ctrl Pts',(0.852496689050906,2.52931704534428,
12.5808812374708));
#424443=CARTESIAN_POINT('Ctrl Pts',(0.853181238633642,2.52883205161534,
12.5811221033394));
#424444=CARTESIAN_POINT('Ctrl Pts',(0.853943700308057,2.52840027395526,
12.581287365893));
#424445=CARTESIAN_POINT('Ctrl Pts',(0.854745148192489,2.52805333797847,
12.581359338449));
#424446=CARTESIAN_POINT('Ctrl Pts',(0.854856532899159,2.52800512104164,
12.5813693411482));
#424447=CARTESIAN_POINT('Ctrl Pts',(0.854968666521613,2.5279584831078,12.5813775999465));
#424448=CARTESIAN_POINT('Ctrl Pts',(0.855081441437813,2.52791344781096,
12.5813841266931));
#424449=CARTESIAN_POINT('Ctrl Pts',(0.855272777722989,2.52783703998297,
12.5813952001081));
#424450=CARTESIAN_POINT('Ctrl Pts',(0.855467467271982,2.52776529909069,
12.5814007534795));
#424451=CARTESIAN_POINT('Ctrl Pts',(0.855665493478638,2.52769844142603,
12.5814005856065));
#424452=CARTESIAN_POINT('Ctrl Pts',(0.85657198002948,2.52739239317685,12.5813998171494));
#424453=CARTESIAN_POINT('Ctrl Pts',(0.857485645370209,2.5272094963594,12.58127954464));
#424454=CARTESIAN_POINT('Ctrl Pts',(0.858395494354219,2.52712177558977,
12.5810700125799));
#424455=CARTESIAN_POINT('Ctrl Pts',(0.8594944883323,2.52701581888787,12.5808169217085));
#424456=CARTESIAN_POINT('Ctrl Pts',(0.860589619754366,2.52706537217095,
12.5804173076348));
#424457=CARTESIAN_POINT('Ctrl Pts',(0.86158609033339,2.52724007692988,12.5799304713245));
#424458=CARTESIAN_POINT('Ctrl Pts',(0.862821031301405,2.52745659116387,
12.5793271277669));
#424459=CARTESIAN_POINT('Ctrl Pts',(0.863986605207165,2.52784703998076,
12.5785808224116));
#424460=CARTESIAN_POINT('Ctrl Pts',(0.865043755292766,2.52836489088548,
12.5777485681082));
#424461=CARTESIAN_POINT('Ctrl Pts',(0.86661902473975,2.5291365454683,12.576508418016));
#424462=CARTESIAN_POINT('Ctrl Pts',(0.867943306149779,2.53017841794506,
12.5750928681475));
#424463=CARTESIAN_POINT('Ctrl Pts',(0.868846144934049,2.53128319837605,
12.5737548217797));
#424464=CARTESIAN_POINT('Ctrl Pts',(0.868846144934049,2.53128319837605,
12.5737548217797));
#424465=CARTESIAN_POINT('Ctrl Pts',(0.882935401738845,2.52295874538841,
12.5770542771492));
#424466=CARTESIAN_POINT('Ctrl Pts',(0.890418978460709,2.53147077887094,
12.5893111709658));
#424467=CARTESIAN_POINT('Ctrl Pts',(0.885156192353693,2.54991106211131,
12.5508408821982));
#424468=CARTESIAN_POINT('Ctrl Pts',(0.899287466897137,2.54155805041447,
12.55409748406));
#424469=CARTESIAN_POINT('Ctrl Pts',(0.906780590746262,2.55008094307168,
12.5663972313419));
#424470=CARTESIAN_POINT('Ctrl Pts',(0.901451194333948,2.56851995176799,
12.52790050457));
#424471=CARTESIAN_POINT('Ctrl Pts',(0.915608213958567,2.56012173334445,
12.5311362602938));
#424472=CARTESIAN_POINT('Ctrl Pts',(0.923125696853579,2.56867233267479,
12.5434568539655));
#424473=CARTESIAN_POINT('Ctrl Pts',(0.9177323305173,2.58711133275317,12.5049357605811));
#424474=CARTESIAN_POINT('Ctrl Pts',(0.931900907674612,2.5786535075997,12.5081700652078));
#424475=CARTESIAN_POINT('Ctrl Pts',(0.939455589549916,2.5872464181106,12.5204921097672));
#424476=CARTESIAN_POINT('Ctrl Pts',(0.916663248489405,2.58589054875607,
12.5064436508395));
#424477=CARTESIAN_POINT('Ctrl Pts',(0.917865885213295,2.5856843626728,12.5062361689309));
#424478=CARTESIAN_POINT('Ctrl Pts',(0.919107736758615,2.58541866291777,
12.5061871075061));
#424479=CARTESIAN_POINT('Ctrl Pts',(0.920293411974997,2.58509433141703,
12.5063648335164));
#424480=CARTESIAN_POINT('Ctrl Pts',(0.920832018793759,2.58494700004379,
12.5064455676329));
#424481=CARTESIAN_POINT('Ctrl Pts',(0.921366487735811,2.58478530232069,
12.506574497099));
#424482=CARTESIAN_POINT('Ctrl Pts',(0.921873598045585,2.58461516543998,
12.5067492519495));
#424483=CARTESIAN_POINT('Ctrl Pts',(0.922892655897611,2.58427326877398,
12.5071004286051));
#424484=CARTESIAN_POINT('Ctrl Pts',(0.923838442911685,2.58388395617983,
12.5076537929612));
#424485=CARTESIAN_POINT('Ctrl Pts',(0.924643573093256,2.58348519404902,
12.5083435010503));
#424486=CARTESIAN_POINT('Ctrl Pts',(0.924694260849764,2.58346008958983,
12.5083869222963));
#424487=CARTESIAN_POINT('Ctrl Pts',(0.924744391349898,2.58343493424511,
12.5084308732336));
#424488=CARTESIAN_POINT('Ctrl Pts',(0.924793948268574,2.5834097320254,12.5084753333616));
#424489=CARTESIAN_POINT('Ctrl Pts',(0.925191460164867,2.58320757695976,
12.508831962269));
#424490=CARTESIAN_POINT('Ctrl Pts',(0.925560721870087,2.58299945172831,
12.509227847131));
#424491=CARTESIAN_POINT('Ctrl Pts',(0.925892128151208,2.58279398426298,
12.5096423454524));
#424492=CARTESIAN_POINT('Ctrl Pts',(0.926930608761967,2.58215014016275,
12.5109411997424));
#424493=CARTESIAN_POINT('Ctrl Pts',(0.927666347974835,2.58150101005229,
12.5124831113042));
#424494=CARTESIAN_POINT('Ctrl Pts',(0.9281851922826,2.58088642152345,12.5140723025008));
#424495=CARTESIAN_POINT('Ctrl Pts',(0.928233808562511,2.58082883390516,
12.5142212114565));
#424496=CARTESIAN_POINT('Ctrl Pts',(0.928280550052106,2.58077155178127,
12.5143705582413));
#424497=CARTESIAN_POINT('Ctrl Pts',(0.928325504124151,2.58071461072905,
12.5145201959299));
#424498=CARTESIAN_POINT('Ctrl Pts',(0.928903006109187,2.57998311813691,
12.5164425148273));
#424499=CARTESIAN_POINT('Ctrl Pts',(0.929213742047119,2.57928950372225,
12.5184635205941));
#424500=CARTESIAN_POINT('Ctrl Pts',(0.929347352005207,2.57862363649833,
12.5205025929157));
#424501=CARTESIAN_POINT('Ctrl Pts',(0.929424851076703,2.57823740711595,
12.5216853356836));
#424502=CARTESIAN_POINT('Ctrl Pts',(0.929443090934737,2.57786130598311,
12.5228750347131));
#424503=CARTESIAN_POINT('Ctrl Pts',(0.929419888094036,2.57749927079595,
12.5240609649613));
#424504=CARTESIAN_POINT('Ctrl Pts',(0.929362937966327,2.57661067485162,
12.5269717671326));
#424505=CARTESIAN_POINT('Ctrl Pts',(0.929044347043804,2.57578247269498,
12.5299036066169));
#424506=CARTESIAN_POINT('Ctrl Pts',(0.928548945178096,2.57499696068514,
12.5328133004019));
#424507=CARTESIAN_POINT('Ctrl Pts',(0.928311123436168,2.57461986918142,
12.5342101228451));
#424508=CARTESIAN_POINT('Ctrl Pts',(0.928032408019065,2.57425336594414,
12.5356023438238));
#424509=CARTESIAN_POINT('Ctrl Pts',(0.927720747655529,2.57389887443869,
12.5369868989719));
#424510=CARTESIAN_POINT('Origin',(9.34773057027711,12.1430337570218,-1.24095417635099));
#424511=CARTESIAN_POINT('Ctrl Pts',(0.826450119160066,2.60813890367028,
12.5369868989719));
#424512=CARTESIAN_POINT('Ctrl Pts',(0.825430951060778,2.62344395512627,
12.5369868989719));
#424513=CARTESIAN_POINT('Ctrl Pts',(0.8107175930909,2.62777989803818,12.5369868989719));
#424514=CARTESIAN_POINT('Ctrl Pts',(0.826105534417468,2.61331260524006,
12.5218025310015));
#424515=CARTESIAN_POINT('Ctrl Pts',(0.822042652512112,2.62440985058867,
12.5216901060418));
#424516=CARTESIAN_POINT('Ctrl Pts',(0.810762448943919,2.62776669646636,
12.5161920673677));
#424517=CARTESIAN_POINT('Ctrl Pts',(0.83075718209413,2.61714643427736,12.5042015548895));
#424518=CARTESIAN_POINT('Ctrl Pts',(0.827461841233387,2.62267075085312,
12.4980677368513));
#424519=CARTESIAN_POINT('Ctrl Pts',(0.820978566206095,2.62470984983164,
12.4907278922778));
#424520=CARTESIAN_POINT('Ctrl Pts',(0.842508980156334,2.61097114343314,
12.506463626192));
#424521=CARTESIAN_POINT('Ctrl Pts',(0.844518181408437,2.61719774352186,
12.4999376786891));
#424522=CARTESIAN_POINT('Ctrl Pts',(0.844493641936519,2.61712169465524,
12.4906970594712));
#424523=CARTESIAN_POINT('Origin',(0.804498734500713,2.60667715419205,12.5369868989719));
#424524=CARTESIAN_POINT('Origin',(0.804498734500713,2.60667715419205,14.));
#424525=CARTESIAN_POINT('Origin',(0.804498734500713,2.60667715419205,13.7435492065112));
#424526=CARTESIAN_POINT('Ctrl Pts',(0.828139345836136,2.58347838159699,
13.793642941384));
#424527=CARTESIAN_POINT('Ctrl Pts',(0.827427607984465,2.59426724846225,
13.8071662555867));
#424528=CARTESIAN_POINT('Ctrl Pts',(0.810454437907433,2.59565680996541,
13.8103758687955));
#424529=CARTESIAN_POINT('Ctrl Pts',(0.827003484928802,2.60006064697971,
13.7804579775005));
#424530=CARTESIAN_POINT('Ctrl Pts',(0.826115145943083,2.61337246599799,
13.790190434335));
#424531=CARTESIAN_POINT('Ctrl Pts',(0.810826453687069,2.61718190339281,
13.7927914348263));
#424532=CARTESIAN_POINT('Ctrl Pts',(0.826334760827468,2.60982325066871,
13.7597120340895));
#424533=CARTESIAN_POINT('Ctrl Pts',(0.825300984768903,2.6252283925711,13.7635825532445));
#424534=CARTESIAN_POINT('Ctrl Pts',(0.811020272377169,2.62987566808793,
13.7651073818884));
#424535=CARTESIAN_POINT('Ctrl Pts',(0.826465712317739,2.60791150932817,
13.7381884353898));
#424536=CARTESIAN_POINT('Ctrl Pts',(0.825457030529163,2.62295612536434,
13.7368803041981));
#424537=CARTESIAN_POINT('Ctrl Pts',(0.810981822744995,2.62738985931261,
13.7363986145813));
#424538=CARTESIAN_POINT('Origin',(0.805915189477188,2.58599859175724,13.7902182540695));
#424539=CARTESIAN_POINT('Ctrl Pts',(0.830308286429238,2.55181480797322,
13.8235227101244));
#424540=CARTESIAN_POINT('Ctrl Pts',(0.829527015915338,2.56328530511605,
13.8358800583119));
#424541=CARTESIAN_POINT('Ctrl Pts',(0.813059797021804,2.56514453908973,
13.8390832900376));
#424542=CARTESIAN_POINT('Ctrl Pts',(0.829493172606032,2.56371450287475,
13.8124254819052));
#424543=CARTESIAN_POINT('Ctrl Pts',(0.828710384598348,2.57520727554153,
13.8247886449157));
#424544=CARTESIAN_POINT('Ctrl Pts',(0.812220446444013,2.57705192205735,
13.8279860620657));
#424545=CARTESIAN_POINT('Ctrl Pts',(0.828678424090336,2.57560886472017,
13.8013225099955));
#424546=CARTESIAN_POINT('Ctrl Pts',(0.827894489939108,2.58711849030397,
13.8136962257787));
#424547=CARTESIAN_POINT('Ctrl Pts',(0.811381754829519,2.58895381155168,
13.8168830918626));
#424548=CARTESIAN_POINT('Ctrl Pts',(0.827864026668595,2.5874981010105,13.7902140179785));
#424549=CARTESIAN_POINT('Ctrl Pts',(0.827079293450659,2.59901951131138,
13.802602731458));
#424550=CARTESIAN_POINT('Ctrl Pts',(0.810543698121769,2.60085042355405,
13.8057746032558));
#424551=CARTESIAN_POINT('Origin',(0.808359450086194,2.55031528628708,13.8235269408515));
#424552=CARTESIAN_POINT('Ctrl Pts',(0.890418978460709,2.53147077887094,
13.8235269408515));
#424553=CARTESIAN_POINT('Ctrl Pts',(0.898215211955112,2.54033843707882,
13.8362179249168));
#424554=CARTESIAN_POINT('Ctrl Pts',(0.912696230442824,2.531285089211,13.8391868794938));
#424555=CARTESIAN_POINT('Ctrl Pts',(0.883285764163169,2.5233572575969,13.8400110824519));
#424556=CARTESIAN_POINT('Ctrl Pts',(0.892105675750976,2.52820813611993,
13.8494522556837));
#424557=CARTESIAN_POINT('Ctrl Pts',(0.90087259114951,2.51800671063957,13.85569149686));
#424558=CARTESIAN_POINT('Ctrl Pts',(0.868463197330234,2.51659787607726,
13.8586819406588));
#424559=CARTESIAN_POINT('Ctrl Pts',(0.872591619228754,2.51521506146106,
13.868010383617));
#424560=CARTESIAN_POINT('Ctrl Pts',(0.876206258320368,2.50691884238066,
13.8744918421245));
#424561=CARTESIAN_POINT('Ctrl Pts',(0.838808242003569,2.52658061731002,
13.8587686893867));
#424562=CARTESIAN_POINT('Ctrl Pts',(0.834716545137537,2.52795107149618,
13.8680909899357));
#424563=CARTESIAN_POINT('Ctrl Pts',(0.826840287192812,2.52353961342725,
13.8745789365163));
#424564=CARTESIAN_POINT('Ctrl Pts',(0.83104750387819,2.54102312109951,13.8400379222776));
#424565=CARTESIAN_POINT('Ctrl Pts',(0.826982046547405,2.5502286786926,13.8494748685453));
#424566=CARTESIAN_POINT('Ctrl Pts',(0.813827090197301,2.54745230899619,
13.8557104837033));
#424567=CARTESIAN_POINT('Ctrl Pts',(0.830308018185601,2.5518187350208,13.8235269408542));
#424568=CARTESIAN_POINT('Ctrl Pts',(0.829501111681931,2.56359861280815,
13.8362179249195));
#424569=CARTESIAN_POINT('Ctrl Pts',(0.812498466812179,2.56520269244754,
13.8391868794965));
#424570=CARTESIAN_POINT('Origin',(0.906941424926576,2.51694463820032,13.8235269408515));
#424571=CARTESIAN_POINT('Ctrl Pts',(0.914032527362825,2.55832950134457,
13.7902140241683));
#424572=CARTESIAN_POINT('Ctrl Pts',(0.92165415233143,2.56700529688334,13.8026027327198));
#424573=CARTESIAN_POINT('Ctrl Pts',(0.935901927838467,2.55841583675045,
13.8057746032556));
#424574=CARTESIAN_POINT('Ctrl Pts',(0.906163917526332,2.54937952022373,
13.8013225161808));
#424575=CARTESIAN_POINT('Ctrl Pts',(0.913777749543641,2.558046439509,13.8136962270464));
#424576=CARTESIAN_POINT('Ctrl Pts',(0.928010043278109,2.54947436739259,
13.8168830918628));
#424577=CARTESIAN_POINT('Ctrl Pts',(0.898291915461332,2.54042568068552,
13.8124254880875));
#424578=CARTESIAN_POINT('Ctrl Pts',(0.905894600332056,2.54907990842673,
13.8247886461867));
#424579=CARTESIAN_POINT('Ctrl Pts',(0.920114448745435,2.5405290913138,13.8279860620656));
#424580=CARTESIAN_POINT('Ctrl Pts',(0.890416383837143,2.53146782652609,
13.8235227163066));
#424581=CARTESIAN_POINT('Ctrl Pts',(0.898004332812819,2.54010528064054,
13.8358800595847));
#424582=CARTESIAN_POINT('Ctrl Pts',(0.912214993939689,2.5315798515525,13.8390832900376));
#424583=CARTESIAN_POINT('Origin',(0.930557576665909,2.54380632236618,13.7902182540695));
#424584=CARTESIAN_POINT('Ctrl Pts',(0.927542585513044,2.57369618596234,
13.7382347919292));
#424585=CARTESIAN_POINT('Ctrl Pts',(0.937488373841171,2.58504515786582,
13.7369371795942));
#424586=CARTESIAN_POINT('Ctrl Pts',(0.951688467901028,2.57976300814133,
13.7364597369711));
#424587=CARTESIAN_POINT('Ctrl Pts',(0.928791541869654,2.5751167851329,13.7595490285574));
#424588=CARTESIAN_POINT('Ctrl Pts',(0.938975384331029,2.58673587111851,
13.7633824266926));
#424589=CARTESIAN_POINT('Ctrl Pts',(0.953149409064946,2.58173680289031,
13.7648920890506));
#424590=CARTESIAN_POINT('Ctrl Pts',(0.922421932868273,2.56787180719496,
13.780380659011));
#424591=CARTESIAN_POINT('Ctrl Pts',(0.93122653231263,2.5779254590006,13.7901039518744));
#424592=CARTESIAN_POINT('Ctrl Pts',(0.945698387238799,2.57167639055629,
13.7926933640892));
#424593=CARTESIAN_POINT('Ctrl Pts',(0.911350130606159,2.55527841820539,
13.7936647693663));
#424594=CARTESIAN_POINT('Ctrl Pts',(0.918468789024592,2.56342077869032,
13.8072068914933));
#424595=CARTESIAN_POINT('Ctrl Pts',(0.932805810134608,2.55419613259745,
13.8104111085397));
#424596=CARTESIAN_POINT('Origin',(0.944243194121396,2.55937273376807,13.7435492065112));
#424597=CARTESIAN_POINT('Origin',(0.944243194121396,2.55937273376807,14.));
#424598=CARTESIAN_POINT('Origin',(0.944243194121396,2.55937273376807,12.5369868989719));
#424599=CARTESIAN_POINT('Ctrl Pts',(0.916657106365097,2.58587322196464,
12.506462012331));
#424600=CARTESIAN_POINT('Ctrl Pts',(0.918841758125204,2.59203608531513,
12.4999388158272));
#424601=CARTESIAN_POINT('Ctrl Pts',(0.918815910829888,2.59196317055959,
12.4907030323752));
#424602=CARTESIAN_POINT('Ctrl Pts',(0.929742803882678,2.58363869659378,
12.5042014951932));
#424603=CARTESIAN_POINT('Ctrl Pts',(0.93571314397386,2.58602535457338,12.4980716682128));
#424604=CARTESIAN_POINT('Ctrl Pts',(0.942097970272217,2.58371028257328,
12.4907355092744));
#424605=CARTESIAN_POINT('Ctrl Pts',(0.931111391753753,2.57776905704064,
12.5218047446509));
#424606=CARTESIAN_POINT('Ctrl Pts',(0.941075204795464,2.58411266016551,
12.5216906929433));
#424607=CARTESIAN_POINT('Ctrl Pts',(0.952070779336664,2.57993317516873,
12.5161988840775));
#424608=CARTESIAN_POINT('Ctrl Pts',(0.927695407488456,2.5738700010123,12.5369868989719));
#424609=CARTESIAN_POINT('Ctrl Pts',(0.937797294492868,2.58540071696883,
12.5369868989719));
#424610=CARTESIAN_POINT('Ctrl Pts',(0.952112840508009,2.57991704358246,
12.5369868989719));
#424611=CARTESIAN_POINT('Origin',(1.65186468598901E-31,-2.72002836734922E-32,
12.5));
#424612=CARTESIAN_POINT('Origin',(1.09379455227037,2.45047010569484,12.5));
#424613=CARTESIAN_POINT('',(1.09379455227037,2.45047010569484,12.5893111709658));
#424614=CARTESIAN_POINT('',(1.09379455227037,2.45047010569484,13.8235269408515));
#424615=CARTESIAN_POINT('',(1.09379455227037,2.45047010569484,12.5));
#424616=CARTESIAN_POINT('',(1.11952159984422,2.47531747421416,13.7902182540695));
#424617=CARTESIAN_POINT('',(1.09379455227037,2.45047010569484,13.8235269408515));
#424618=CARTESIAN_POINT('',(1.13443048657737,2.48971658479255,13.7435492065112));
#424619=CARTESIAN_POINT('Origin',(1.08538021998782,2.4423439356315,13.7445212918694));
#424620=CARTESIAN_POINT('',(1.13443048657737,2.48971658479255,12.5369868989719));
#424621=CARTESIAN_POINT('',(1.13443048657737,2.48971658479255,12.5));
#424622=CARTESIAN_POINT('Ctrl Pts',(1.13443048657737,2.48971658479255,12.5369868989719));
#424623=CARTESIAN_POINT('Ctrl Pts',(1.12089505426802,2.47664396642493,12.5544431401645));
#424624=CARTESIAN_POINT('Ctrl Pts',(1.10734994105773,2.46356199817319,12.5718848856037));
#424625=CARTESIAN_POINT('Ctrl Pts',(1.09379455227037,2.45047010569484,12.5893111709658));
#424626=CARTESIAN_POINT('Origin',(1.03917422769729,2.7506259705725,12.5));
#424627=CARTESIAN_POINT('',(1.03628829969026,2.53213896960501,13.7435492065112));
#424628=CARTESIAN_POINT('',(1.0360145467208,2.51141375915053,13.7902182540695));
#424629=CARTESIAN_POINT('Origin',(1.03529517123111,2.45695148811307,13.7418732680447));
#424630=CARTESIAN_POINT('',(1.03554215359081,2.47564995700462,13.8235269408515));
#424631=CARTESIAN_POINT('',(1.0360145467208,2.51141375915053,13.7902182540695));
#424632=CARTESIAN_POINT('',(1.03554215359081,2.47564995700462,12.5893111709658));
#424633=CARTESIAN_POINT('',(1.03554215359081,2.47564995700462,12.5));
#424634=CARTESIAN_POINT('',(1.03628829969026,2.53213896960501,12.5369868989719));
#424635=CARTESIAN_POINT('Ctrl Pts',(1.03554215359081,2.47564995700462,12.5893111709658));
#424636=CARTESIAN_POINT('Ctrl Pts',(1.03579105399491,2.49449363664608,12.5718848856037));
#424637=CARTESIAN_POINT('Ctrl Pts',(1.03603976572164,2.5133230319549,12.5544431401645));
#424638=CARTESIAN_POINT('Ctrl Pts',(1.03628829969026,2.53213896960501,12.5369868989719));
#424639=CARTESIAN_POINT('',(1.03628829969026,2.53213896960501,12.5));
#424640=CARTESIAN_POINT('Origin',(1.06991415528679,2.47519594774131,12.5));
#424641=CARTESIAN_POINT('',(1.05731024571616,2.44321577207398,13.8587068136939));
#424642=CARTESIAN_POINT('Ctrl Pts',(1.0355421535842,2.47564995700456,13.8235269408542));
#424643=CARTESIAN_POINT('Ctrl Pts',(1.03551901003009,2.47389781151887,13.8262006681044));
#424644=CARTESIAN_POINT('Ctrl Pts',(1.0356690501615,2.47210245194736,13.8288634856214));
#424645=CARTESIAN_POINT('Ctrl Pts',(1.03597976772654,2.47026850427233,13.8314912288862));
#424646=CARTESIAN_POINT('Ctrl Pts',(1.03630008548706,2.46837789338229,13.8342001611531));
#424647=CARTESIAN_POINT('Ctrl Pts',(1.03679102881309,2.46644409004582,13.8368750301949));
#424648=CARTESIAN_POINT('Ctrl Pts',(1.03748230410397,2.46445955796243,13.8394886372968));
#424649=CARTESIAN_POINT('Ctrl Pts',(1.03753569297148,2.46430628773583,13.8396904925131));
#424650=CARTESIAN_POINT('Ctrl Pts',(1.03759029864689,2.46415271849303,13.8398919674349));
#424651=CARTESIAN_POINT('Ctrl Pts',(1.03764614590368,2.46399884959309,13.8400930404591));
#424652=CARTESIAN_POINT('Ctrl Pts',(1.03851628373661,2.46160146861416,13.8432258934518));
#424653=CARTESIAN_POINT('Ctrl Pts',(1.03968232662491,2.45914319261956,13.8462331177034));
#424654=CARTESIAN_POINT('Ctrl Pts',(1.04119340285672,2.45674553947007,13.8489036603661));
#424655=CARTESIAN_POINT('Ctrl Pts',(1.04168784458504,2.45596099945666,13.849777493004));
#424656=CARTESIAN_POINT('Ctrl Pts',(1.04221923248918,2.45518320007902,13.85061494757));
#424657=CARTESIAN_POINT('Ctrl Pts',(1.04278928813813,2.45441711243214,13.8514076489583));
#424658=CARTESIAN_POINT('Ctrl Pts',(1.04399503804997,2.4527967265726,13.8530843267192));
#424659=CARTESIAN_POINT('Ctrl Pts',(1.04549459049601,2.45107133833551,13.8546805203176));
#424660=CARTESIAN_POINT('Ctrl Pts',(1.04730389787759,2.44943059471246,13.8559412814274));
#424661=CARTESIAN_POINT('Ctrl Pts',(1.04754604188247,2.44921101000513,13.8561100121513));
#424662=CARTESIAN_POINT('Ctrl Pts',(1.04779365776436,2.44899293146871,13.8562727473908));
#424663=CARTESIAN_POINT('Ctrl Pts',(1.04804671036289,2.44877679458595,13.8564289040185));
#424664=CARTESIAN_POINT('Ctrl Pts',(1.04919430101033,2.44779661628836,13.8571370725437));
#424665=CARTESIAN_POINT('Ctrl Pts',(1.05047535372972,2.4468408724577,13.8577210840553));
#424666=CARTESIAN_POINT('Ctrl Pts',(1.05185762324726,2.44597023585783,13.8581177131616));
#424667=CARTESIAN_POINT('Ctrl Pts',(1.05224691791968,2.4457250346249,13.8582294175695));
#424668=CARTESIAN_POINT('Ctrl Pts',(1.05264411863223,2.44548645509554,13.8583265086086));
#424669=CARTESIAN_POINT('Ctrl Pts',(1.05304822202721,2.44525551628232,13.8584082369006));
#424670=CARTESIAN_POINT('Ctrl Pts',(1.0536288102412,2.44492371913641,13.8585256585398));
#424671=CARTESIAN_POINT('Ctrl Pts',(1.05423102547564,2.44460384965959,13.8586122832068));
#424672=CARTESIAN_POINT('Ctrl Pts',(1.05483959435808,2.44430491454631,13.8586682984299));
#424673=CARTESIAN_POINT('Ctrl Pts',(1.05532638913854,2.44406579608818,13.8587131050557));
#424674=CARTESIAN_POINT('Ctrl Pts',(1.05582252251695,2.44383722077545,13.8587357943552));
#424675=CARTESIAN_POINT('Ctrl Pts',(1.05632826536498,2.44361962142378,13.8587355499465));
#424676=CARTESIAN_POINT('Ctrl Pts',(1.05665513902499,2.44347898177504,13.8587353919793));
#424677=CARTESIAN_POINT('Ctrl Pts',(1.0569824768398,2.44334441249848,13.8587257282814));
#424678=CARTESIAN_POINT('Ctrl Pts',(1.05731024571616,2.44321577207398,13.8587068136939));
#424679=CARTESIAN_POINT('Ctrl Pts',(1.05731024571616,2.44321577207398,13.8587068136939));
#424680=CARTESIAN_POINT('Ctrl Pts',(1.05838825968252,2.44279268073048,13.8586446046466));
#424681=CARTESIAN_POINT('Ctrl Pts',(1.05947093147828,2.44243364339347,13.858482427929));
#424682=CARTESIAN_POINT('Ctrl Pts',(1.06055714787882,2.44213433031837,13.8582284286032));
#424683=CARTESIAN_POINT('Ctrl Pts',(1.06167147955176,2.44182726992088,13.8579678548414));
#424684=CARTESIAN_POINT('Ctrl Pts',(1.06279267059807,2.4415837921154,13.857615680862));
#424685=CARTESIAN_POINT('Ctrl Pts',(1.06387446261208,2.44140402686309,13.8571944833187));
#424686=CARTESIAN_POINT('Ctrl Pts',(1.06657418521963,2.44095540429107,13.8561433417727));
#424687=CARTESIAN_POINT('Ctrl Pts',(1.06915402792857,2.44087786975251,13.8546163505475));
#424688=CARTESIAN_POINT('Ctrl Pts',(1.07147348871116,2.44101970954713,13.8528973491086));
#424689=CARTESIAN_POINT('Ctrl Pts',(1.07189721997571,2.44104562158495,13.8525833129073));
#424690=CARTESIAN_POINT('Ctrl Pts',(1.07231233409303,2.44107873387402,13.8522628768812));
#424691=CARTESIAN_POINT('Ctrl Pts',(1.07271808937104,2.44111798444778,13.851937733538));
#424692=CARTESIAN_POINT('Ctrl Pts',(1.07519598055777,2.44135768225595,13.8499521282529));
#424693=CARTESIAN_POINT('Ctrl Pts',(1.07757070858412,2.44185418050337,13.847639871647));
#424694=CARTESIAN_POINT('Ctrl Pts',(1.07973390830809,2.4425027447878,13.8452109780794));
#424695=CARTESIAN_POINT('Ctrl Pts',(1.08070717663991,2.44279454728398,13.8441181685877));
#424696=CARTESIAN_POINT('Ctrl Pts',(1.08163805677817,2.44311655848146,13.8430021611332));
#424697=CARTESIAN_POINT('Ctrl Pts',(1.08251938789867,2.44345733934995,13.8418824960098));
#424698=CARTESIAN_POINT('Ctrl Pts',(1.08459626718971,2.44426039816869,13.8392439765549));
#424699=CARTESIAN_POINT('Ctrl Pts',(1.08649863795158,2.44520255083485,13.8364981347964));
#424700=CARTESIAN_POINT('Ctrl Pts',(1.08824671851374,2.44625562318806,13.8336931113419));
#424701=CARTESIAN_POINT('Ctrl Pts',(1.0899492379679,2.4472812487838,13.8309611966328));
#424702=CARTESIAN_POINT('Ctrl Pts',(1.09150681991311,2.44841359873896,13.8281701127186));
#424703=CARTESIAN_POINT('Ctrl Pts',(1.09290700573027,2.44965062374159,13.8253580685121));
#424704=CARTESIAN_POINT('Ctrl Pts',(1.09321056752656,2.4499188120972,13.8247484142933));
#424705=CARTESIAN_POINT('Ctrl Pts',(1.0935065637343,2.45019196428493,13.8241378483365));
#424706=CARTESIAN_POINT('Ctrl Pts',(1.09379455227037,2.45047010569484,13.8235269408515));
#424707=CARTESIAN_POINT('',(1.05616306898853,2.44369196784508,12.5969504640361));
#424708=CARTESIAN_POINT('Origin',(1.06992746243219,2.47522623969885,12.584524458991));
#424709=CARTESIAN_POINT('Origin',(1.06992746243219,2.47522623969885,12.584524458991));
#424710=CARTESIAN_POINT('Ctrl Pts',(1.03554215359081,2.47564995700462,12.5893111709658));
#424711=CARTESIAN_POINT('Ctrl Pts',(1.03539245984433,2.46431698624043,12.5770542771492));
#424712=CARTESIAN_POINT('Ctrl Pts',(1.05142854144719,2.46105389542323,12.5737548217797));
#424713=CARTESIAN_POINT('Ctrl Pts',(1.03586948357564,2.50043136060788,12.5663937883685));
#424714=CARTESIAN_POINT('Ctrl Pts',(1.03571959887401,2.48908393306558,12.5540940315304));
#424715=CARTESIAN_POINT('Ctrl Pts',(1.05180601334584,2.48581387729336,12.5508374392248));
#424716=CARTESIAN_POINT('Ctrl Pts',(1.03619648328852,2.52518776007868,12.5434499600945));
#424717=CARTESIAN_POINT('Ctrl Pts',(1.03604611125831,2.51380343800857,12.5311293540533));
#424718=CARTESIAN_POINT('Ctrl Pts',(1.0521819367162,2.51054968611948,12.5278936106989));
#424719=CARTESIAN_POINT('Ctrl Pts',(1.03652317860012,2.54992111402498,12.5204817579905));
#424720=CARTESIAN_POINT('Ctrl Pts',(1.03637206233116,2.53848044734067,12.5081597038247));
#424721=CARTESIAN_POINT('Ctrl Pts',(1.0525564180634,2.53526320093622,12.5049254088044));
#424722=CARTESIAN_POINT('Ctrl Pts',(1.03628829969026,2.53213896960501,12.5369868989719));
#424723=CARTESIAN_POINT('Ctrl Pts',(1.03630060274096,2.53307039314223,12.5342545179733));
#424724=CARTESIAN_POINT('Ctrl Pts',(1.03643707940131,2.53395765366459,12.5314872231885));
#424725=CARTESIAN_POINT('Ctrl Pts',(1.03674529283368,2.53474227178204,12.5287124745063));
#424726=CARTESIAN_POINT('Ctrl Pts',(1.03702325500535,2.53544987934533,12.5262100684184));
#424727=CARTESIAN_POINT('Ctrl Pts',(1.0374415313905,2.53607293087077,12.5237004536639));
#424728=CARTESIAN_POINT('Ctrl Pts',(1.03806234226045,2.53658517537798,12.5212220730815));
#424729=CARTESIAN_POINT('Ctrl Pts',(1.03853762668583,2.53697734286094,12.5193246583486));
#424730=CARTESIAN_POINT('Ctrl Pts',(1.03913770536946,2.53730876132232,12.517417831369));
#424731=CARTESIAN_POINT('Ctrl Pts',(1.0399254557789,2.53750526576482,12.5155812248348));
#424732=CARTESIAN_POINT('Ctrl Pts',(1.0402610416875,2.53758897771353,12.5147988205793));
#424733=CARTESIAN_POINT('Ctrl Pts',(1.04063095998743,2.5376485591545,12.5140295443047));
#424734=CARTESIAN_POINT('Ctrl Pts',(1.0410408100704,2.53768027133397,12.5132817086137));
#424735=CARTESIAN_POINT('Ctrl Pts',(1.04166106272771,2.53772826342768,12.5121499604604));
#424736=CARTESIAN_POINT('Ctrl Pts',(1.04238671566515,2.53770633328319,12.5110494206568));
#424737=CARTESIAN_POINT('Ctrl Pts',(1.04322868144594,2.53757887451469,12.5100666561695));
#424738=CARTESIAN_POINT('Ctrl Pts',(1.0437121362584,2.53750568798333,12.5095023550641));
#424739=CARTESIAN_POINT('Ctrl Pts',(1.04423942793907,2.53739621735281,12.5089719619137));
#424740=CARTESIAN_POINT('Ctrl Pts',(1.0447993746768,2.53724626089961,12.5085043804652));
#424741=CARTESIAN_POINT('Ctrl Pts',(1.04561878378927,2.53702681916354,12.5078201359221));
#424742=CARTESIAN_POINT('Ctrl Pts',(1.0465315752678,2.536713147792,12.5072563000949));
#424743=CARTESIAN_POINT('Ctrl Pts',(1.04747312397982,2.53631850262317,12.5068768744332));
#424744=CARTESIAN_POINT('Ctrl Pts',(1.04815204541762,2.53603393628898,12.5066032824114));
#424745=CARTESIAN_POINT('Ctrl Pts',(1.04885786974257,2.53570232440291,12.5064197834844));
#424746=CARTESIAN_POINT('Ctrl Pts',(1.04955228104954,2.53534452455097,12.5063282718343));
#424747=CARTESIAN_POINT('Ctrl Pts',(1.0505659065734,2.53482224753919,12.5061946931565));
#424748=CARTESIAN_POINT('Ctrl Pts',(1.05157736598184,2.53423395310182,12.5062515701262));
#424749=CARTESIAN_POINT('Ctrl Pts',(1.05253166145004,2.5336295196662,12.5064436508398));
#424750=CARTESIAN_POINT('',(1.05142854144719,2.46105389542323,12.5737548217797));
#424751=CARTESIAN_POINT('Origin',(1.05754023467624,2.4753593910761,12.5893111709658));
#424752=CARTESIAN_POINT('Ctrl Pts',(1.05253166145004,2.5336295196662,12.5064436508398));
#424753=CARTESIAN_POINT('Ctrl Pts',(1.05236885141579,2.52288643441829,12.5164271754438));
#424754=CARTESIAN_POINT('Ctrl Pts',(1.05220576793201,2.51213909377987,12.5264061185523));
#424755=CARTESIAN_POINT('Ctrl Pts',(1.05204240231442,2.50138734786532,12.536380305637));
#424756=CARTESIAN_POINT('Ctrl Pts',(1.05183822842656,2.48794984616116,12.5488460165097));
#424757=CARTESIAN_POINT('Ctrl Pts',(1.05163361376306,2.47450545947743,12.5613043021964));
#424758=CARTESIAN_POINT('Ctrl Pts',(1.05142854144719,2.46105389542323,12.5737548217797));
#424759=CARTESIAN_POINT('Ctrl Pts',(1.09379455227037,2.45047010569484,12.5893111709658));
#424760=CARTESIAN_POINT('Ctrl Pts',(1.08564206678201,2.4425963762785,12.5770542771492));
#424761=CARTESIAN_POINT('Ctrl Pts',(1.07227821101589,2.45204153556342,12.5737548217797));
#424762=CARTESIAN_POINT('Ctrl Pts',(1.0861883542163,2.44312398463148,12.5928319619712));
#424763=CARTESIAN_POINT('Ctrl Pts',(1.07844621856501,2.44017563730997,12.5821634970843));
#424764=CARTESIAN_POINT('Ctrl Pts',(1.06951401436786,2.44935873213036,12.5773203894503));
#424765=CARTESIAN_POINT('Ctrl Pts',(1.07038411407214,2.43757330063713,12.5969440695591));
#424766=CARTESIAN_POINT('Ctrl Pts',(1.06668708889191,2.43915144745181,12.5878292599214));
#424767=CARTESIAN_POINT('Ctrl Pts',(1.06388038270617,2.44738228547084,12.5813877129824));
#424768=CARTESIAN_POINT('Ctrl Pts',(1.04227728576595,2.44966385265545,12.596957478804));
#424769=CARTESIAN_POINT('Ctrl Pts',(1.04594702040858,2.44809744249155,12.5878468778671));
#424770=CARTESIAN_POINT('Ctrl Pts',(1.05382291638343,2.45171514128095,12.5814011370086));
#424771=CARTESIAN_POINT('Ctrl Pts',(1.03540228783687,2.46506104105513,12.5928371701607));
#424772=CARTESIAN_POINT('Ctrl Pts',(1.03856248079188,2.45740935848259,12.5821692192952));
#424773=CARTESIAN_POINT('Ctrl Pts',(1.0513677808519,2.45719001322731,12.5773318885715));
#424774=CARTESIAN_POINT('Ctrl Pts',(1.03554215359075,2.47564995700461,12.5893111709658));
#424775=CARTESIAN_POINT('Ctrl Pts',(1.03539245984427,2.46431698624042,12.5770542771492));
#424776=CARTESIAN_POINT('Ctrl Pts',(1.05142854144714,2.46105389542323,12.5737548217797));
#424777=CARTESIAN_POINT('',(1.07227821101589,2.45204153556342,12.5737548217797));
#424778=CARTESIAN_POINT('Origin',(1.07851109820088,2.46629464460458,12.5893111709658));
#424779=CARTESIAN_POINT('Ctrl Pts',(1.05142854144714,2.46105389542323,12.5737548217797));
#424780=CARTESIAN_POINT('Ctrl Pts',(1.05138262932765,2.46005279017987,12.5746934679442));
#424781=CARTESIAN_POINT('Ctrl Pts',(1.05151481645966,2.45893660829488,12.5756680099006));
#424782=CARTESIAN_POINT('Ctrl Pts',(1.05180675680538,2.4578319479387,12.5765688348656));
#424783=CARTESIAN_POINT('Ctrl Pts',(1.05188404478002,2.45753950133839,12.5768073183026));
#424784=CARTESIAN_POINT('Ctrl Pts',(1.05197227227372,2.45724785902399,12.5770407398754));
#424785=CARTESIAN_POINT('Ctrl Pts',(1.05207055560808,2.45695922165792,12.5772674179684));
#424786=CARTESIAN_POINT('Ctrl Pts',(1.05247388383537,2.45577473195842,12.5781976435658));
#424787=CARTESIAN_POINT('Ctrl Pts',(1.05308014436771,2.45457720715713,12.5790594849312));
#424788=CARTESIAN_POINT('Ctrl Pts',(1.05389148425767,2.45346931713253,12.5797571720116));
#424789=CARTESIAN_POINT('Ctrl Pts',(1.05442010136917,2.45274748694532,12.580211740231));
#424790=CARTESIAN_POINT('Ctrl Pts',(1.05507494323198,2.45204199483691,12.5806009430798));
#424791=CARTESIAN_POINT('Ctrl Pts',(1.0558228968735,2.45141455717908,12.5808812374708));
#424792=CARTESIAN_POINT('Ctrl Pts',(1.0564656371826,2.45087538008073,12.5811221033394));
#424793=CARTESIAN_POINT('Ctrl Pts',(1.05719036794097,2.45038289142037,12.581287365893));
#424794=CARTESIAN_POINT('Ctrl Pts',(1.05796087057078,2.44997178440156,12.581359338449));
#424795=CARTESIAN_POINT('Ctrl Pts',(1.05806795452605,2.44991464901498,12.5813693411482));
#424796=CARTESIAN_POINT('Ctrl Pts',(1.05817591360855,2.44985902633379,12.5813775999465));
#424797=CARTESIAN_POINT('Ctrl Pts',(1.05828464248074,2.44980494868556,12.5813841266931));
#424798=CARTESIAN_POINT('Ctrl Pts',(1.05846911416289,2.44971319941479,12.5813952001081));
#424799=CARTESIAN_POINT('Ctrl Pts',(1.05865730834974,2.44962582822876,12.5814007534795));
#424800=CARTESIAN_POINT('Ctrl Pts',(1.05884922612019,2.44954305205324,12.5814005856065));
#424801=CARTESIAN_POINT('Ctrl Pts',(1.05972775063829,2.44916413508506,12.5813998171494));
#424802=CARTESIAN_POINT('Ctrl Pts',(1.06062346804441,2.44890737463436,12.58127954464));
#424803=CARTESIAN_POINT('Ctrl Pts',(1.0615231395239,2.44874578460953,12.5810700125799));
#424804=CARTESIAN_POINT('Ctrl Pts',(1.06260984023532,2.44855060225803,12.5808169217085));
#424805=CARTESIAN_POINT('Ctrl Pts',(1.06370536675053,2.44851072727905,12.5804173076348));
#424806=CARTESIAN_POINT('Ctrl Pts',(1.06471276171563,2.44860362911934,12.5799304713245));
#424807=CARTESIAN_POINT('Ctrl Pts',(1.06596124143954,2.44871876376655,12.5793271277669));
#424808=CARTESIAN_POINT('Ctrl Pts',(1.06715476219761,2.44901290830323,12.5785808224116));
#424809=CARTESIAN_POINT('Ctrl Pts',(1.06825060435974,2.4494428685557,12.5777485681082));
#424810=CARTESIAN_POINT('Ctrl Pts',(1.06988352923978,2.45008355643754,12.576508418016));
#424811=CARTESIAN_POINT('Ctrl Pts',(1.07128832649179,2.45101402094063,12.5750928681475));
#424812=CARTESIAN_POINT('Ctrl Pts',(1.07227821101589,2.45204153556342,12.5737548217797));
#424813=CARTESIAN_POINT('Ctrl Pts',(1.07227821101589,2.45204153556342,12.5737548217797));
#424814=CARTESIAN_POINT('Ctrl Pts',(1.08564206678201,2.4425963762785,12.5770542771492));
#424815=CARTESIAN_POINT('Ctrl Pts',(1.09379455227037,2.45047010569484,12.5893111709658));
#424816=CARTESIAN_POINT('Ctrl Pts',(1.0900523319253,2.46927799633899,12.5508408821982));
#424817=CARTESIAN_POINT('Ctrl Pts',(1.10345573781959,2.45980094853584,12.55409748406));
#424818=CARTESIAN_POINT('Ctrl Pts',(1.11161862379148,2.46768472281437,12.5663972313419));
#424819=CARTESIAN_POINT('Ctrl Pts',(1.10780991089423,2.48649677251367,12.52790050457));
#424820=CARTESIAN_POINT('Ctrl Pts',(1.12123529143713,2.47697256994233,12.5311362602938));
#424821=CARTESIAN_POINT('Ctrl Pts',(1.1294247137533,2.48488197321396,12.5434568539655));
#424822=CARTESIAN_POINT('Ctrl Pts',(1.12555224308429,2.50369922846665,12.5049357605811));
#424823=CARTESIAN_POINT('Ctrl Pts',(1.13898428420131,2.49411467545568,12.5081700652078));
#424824=CARTESIAN_POINT('Ctrl Pts',(1.14721423047522,2.50206321705864,12.5204921097672));
#424825=CARTESIAN_POINT('Ctrl Pts',(1.12438721310968,2.50256964663775,12.5064436508395));
#424826=CARTESIAN_POINT('Ctrl Pts',(1.12556904207916,2.50226612056393,12.5062361689309));
#424827=CARTESIAN_POINT('Ctrl Pts',(1.12678510446924,2.50190008247318,12.5061871075061));
#424828=CARTESIAN_POINT('Ctrl Pts',(1.12794039842089,2.50148018662134,12.5063648335164));
#424829=CARTESIAN_POINT('Ctrl Pts',(1.12846520419522,2.50128944402519,12.5064455676329));
#424830=CARTESIAN_POINT('Ctrl Pts',(1.12898471487039,2.50108472015738,12.506574497099));
#424831=CARTESIAN_POINT('Ctrl Pts',(1.12947627007719,2.50087381519507,12.5067492519495));
#424832=CARTESIAN_POINT('Ctrl Pts',(1.1304640693461,2.50044999348656,12.5071004286051));
#424833=CARTESIAN_POINT('Ctrl Pts',(1.13137497674137,2.49998488587599,12.5076537929613));
#424834=CARTESIAN_POINT('Ctrl Pts',(1.13214492510314,2.49952182500897,12.5083435010505));
#424835=CARTESIAN_POINT('Ctrl Pts',(1.13219339795375,2.49949267256013,12.5083869222964));
#424836=CARTESIAN_POINT('Ctrl Pts',(1.13224131125456,2.49946351481665,12.5084308732337));
#424837=CARTESIAN_POINT('Ctrl Pts',(1.13228864906172,2.49943435710636,12.5084753333615));
#424838=CARTESIAN_POINT('Ctrl Pts',(1.13266836075541,2.49920047378516,12.5088319622689));
#424839=CARTESIAN_POINT('Ctrl Pts',(1.13301942963428,2.4989629428162,12.509227847131));
#424840=CARTESIAN_POINT('Ctrl Pts',(1.13333298568245,2.49873114633838,12.5096423454524));
#424841=CARTESIAN_POINT('Ctrl Pts',(1.13431553156332,2.49800479876572,12.5109411997424));
#424842=CARTESIAN_POINT('Ctrl Pts',(1.13499591253442,2.49729785900603,12.5124831113042));
#424843=CARTESIAN_POINT('Ctrl Pts',(1.13546293575989,2.49664302484202,12.5140723025008));
#424844=CARTESIAN_POINT('Ctrl Pts',(1.13550669634763,2.49658166616364,12.5142212114565));
#424845=CARTESIAN_POINT('Ctrl Pts',(1.1355486132839,2.49652076477596,12.5143705582413));
#424846=CARTESIAN_POINT('Ctrl Pts',(1.1355887765506,2.49646034901619,12.5145201959299));
#424847=CARTESIAN_POINT('Ctrl Pts',(1.13610473350832,2.49568421863226,12.5164425148273));
#424848=CARTESIAN_POINT('Ctrl Pts',(1.13635789948406,2.49496758429867,12.5184635205941));
#424849=CARTESIAN_POINT('Ctrl Pts',(1.13643679050567,2.49429304224105,12.5205025929158));
#424850=CARTESIAN_POINT('Ctrl Pts',(1.13648255042516,2.49390178111128,12.5216853356836));
#424851=CARTESIAN_POINT('Ctrl Pts',(1.13647007385769,2.49352544470617,12.5228750347131));
#424852=CARTESIAN_POINT('Ctrl Pts',(1.1364174389938,2.49316650540816,12.5240609649613));
#424853=CARTESIAN_POINT('Ctrl Pts',(1.13628824954416,2.49228550815763,12.5269717671326));
#424854=CARTESIAN_POINT('Ctrl Pts',(1.13590321254223,2.49148602989319,12.5299036066169));
#424855=CARTESIAN_POINT('Ctrl Pts',(1.13534543256422,2.4907435114609,12.5328133004019));
#424856=CARTESIAN_POINT('Ctrl Pts',(1.13507766569622,2.49038705937785,12.5342101228451));
#424857=CARTESIAN_POINT('Ctrl Pts',(1.13477000426539,2.49004449354382,12.5356023438238));
#424858=CARTESIAN_POINT('Ctrl Pts',(1.13443048657737,2.48971658479255,12.5369868989719));
#424859=CARTESIAN_POINT('Origin',(10.3056869474636,11.3400187595675,-1.23989184831316));
#424860=CARTESIAN_POINT('Ctrl Pts',(1.03628770799528,2.53209717952451,12.5369868989719));
#424861=CARTESIAN_POINT('Ctrl Pts',(1.0365194348726,2.54743437634594,12.5369868989719));
#424862=CARTESIAN_POINT('Ctrl Pts',(1.02220845398785,2.5529551670322,12.5369868989719));
#424863=CARTESIAN_POINT('Ctrl Pts',(1.03636597453823,2.53728175288462,12.5218025310015));
#424864=CARTESIAN_POINT('Ctrl Pts',(1.03322114005496,2.54867323565804,12.5216901060417));
#424865=CARTESIAN_POINT('Ctrl Pts',(1.02225208453606,2.55293835321908,12.5161920673678));
#424866=CARTESIAN_POINT('Ctrl Pts',(1.04131463689905,2.54072367270261,12.5042015548895));
#424867=CARTESIAN_POINT('Ctrl Pts',(1.03848054409933,2.54649820844322,12.4980677368514));
#424868=CARTESIAN_POINT('Ctrl Pts',(1.03218504713171,2.5490589695907,12.4907278922777));
#424869=CARTESIAN_POINT('Ctrl Pts',(1.05252398829026,2.53361104898882,12.506463626192));
#424870=CARTESIAN_POINT('Ctrl Pts',(1.0550340298031,2.53965316202484,12.4999376786891));
#424871=CARTESIAN_POINT('Ctrl Pts',(1.05500337329562,2.53957936639933,12.4906970594712));
#424872=CARTESIAN_POINT('Origin',(1.01429021860483,2.53242953553353,12.5369868989719));
#424873=CARTESIAN_POINT('Origin',(1.01429021860483,2.53242953553353,14.));
#424874=CARTESIAN_POINT('Origin',(1.01429021860483,2.53242953553353,13.7435492065112));
#424875=CARTESIAN_POINT('Ctrl Pts',(1.03596125242285,2.50738102564795,13.793642941384));
#424876=CARTESIAN_POINT('Ctrl Pts',(1.03613127562864,2.5181920066911,13.8071662555867));
#424877=CARTESIAN_POINT('Ctrl Pts',(1.01932784453742,2.52096041547549,13.8103758687955));
#424878=CARTESIAN_POINT('Ctrl Pts',(1.03618077956992,2.5240006981193,13.7804579775006));
#424879=CARTESIAN_POINT('Ctrl Pts',(1.03638043328978,2.53734063103223,13.7901904343351));
#424880=CARTESIAN_POINT('Ctrl Pts',(1.02145311740879,2.54238356319055,13.7927914348262));
#424881=CARTESIAN_POINT('Ctrl Pts',(1.03631002342511,2.53378532477233,13.7597120340895));
#424882=CARTESIAN_POINT('Ctrl Pts',(1.03653534925048,2.54922346968174,13.7635825532445));
#424883=CARTESIAN_POINT('Ctrl Pts',(1.02268095084899,2.55501929240823,13.7651073818885));
#424884=CARTESIAN_POINT('Ctrl Pts',(1.0362847145181,2.5318692708312,13.7381884353898));
#424885=CARTESIAN_POINT('Ctrl Pts',(1.03650566490932,2.54694604407851,13.7368803041982));
#424886=CARTESIAN_POINT('Ctrl Pts',(1.02244001266249,2.55254488895851,13.7363986145813));
#424887=CARTESIAN_POINT('Origin',(1.01401646563537,2.51170432507905,13.7902182540695));
#424888=CARTESIAN_POINT('Ctrl Pts',(1.03554210084444,2.47564602115955,13.8235227101244));
#424889=CARTESIAN_POINT('Ctrl Pts',(1.03569838194778,2.48714203196923,13.8358800583119));
#424890=CARTESIAN_POINT('Ctrl Pts',(1.01943750119579,2.49033731070927,13.8390832900376));
#424891=CARTESIAN_POINT('Ctrl Pts',(1.03569963485109,2.48757256015172,13.8124254819053));
#424892=CARTESIAN_POINT('Ctrl Pts',(1.03585621917197,2.49909089605522,13.8247886449158));
#424893=CARTESIAN_POINT('Ctrl Pts',(1.01957150574241,2.5022734877066,13.8279860620657));
#424894=CARTESIAN_POINT('Ctrl Pts',(1.03585709825614,2.49949375405706,13.8013225099955));
#424895=CARTESIAN_POINT('Ctrl Pts',(1.03601391391637,2.51102898022224,13.8136962257787));
#424896=CARTESIAN_POINT('Ctrl Pts',(1.01970571929062,2.51420413579808,13.8168830918626));
#424897=CARTESIAN_POINT('Ctrl Pts',(1.03601449380658,2.5114098108448,13.7902140179785));
#424898=CARTESIAN_POINT('Ctrl Pts',(1.03617147362278,2.52295684764573,13.802602731458));
#424899=CARTESIAN_POINT('Ctrl Pts',(1.01984013546838,2.52612947220724,13.8057746032558));
#424900=CARTESIAN_POINT('Origin',(1.01354407250538,2.47594052293313,13.8235269408515));
#424901=CARTESIAN_POINT('Ctrl Pts',(1.09379455227037,2.45047010569484,13.8235269408515));
#424902=CARTESIAN_POINT('Ctrl Pts',(1.10228764090823,2.45867279209507,13.8362179249168));
#424903=CARTESIAN_POINT('Ctrl Pts',(1.11598254310312,2.44846923105347,13.8391868794938));
#424904=CARTESIAN_POINT('Ctrl Pts',(1.08602374584887,2.44296500468032,13.8400110824519));
#424905=CARTESIAN_POINT('Ctrl Pts',(1.09520970154143,2.44708083763075,13.8494522556837));
#424906=CARTESIAN_POINT('Ctrl Pts',(1.10311593487012,2.43619877155908,13.85569149686));
#424907=CARTESIAN_POINT('Ctrl Pts',(1.07069954753941,2.43743629124795,13.8586819406588));
#424908=CARTESIAN_POINT('Ctrl Pts',(1.07470152022599,2.43572157312218,13.868010383617));
#424909=CARTESIAN_POINT('Ctrl Pts',(1.07762791303082,2.42715833238374,13.8744918421245));
#424910=CARTESIAN_POINT('Ctrl Pts',(1.04195695271595,2.44980296989507,13.8587686893867));
#424911=CARTESIAN_POINT('Ctrl Pts',(1.03799057537254,2.45150237528801,13.8680909899357));
#424912=CARTESIAN_POINT('Ctrl Pts',(1.02978095023979,2.447747584124,13.8745789365163));
#424913=CARTESIAN_POINT('Ctrl Pts',(1.03539923594297,2.46482998964901,13.8400379222776));
#424914=CARTESIAN_POINT('Ctrl Pts',(1.03209764449017,2.47433628902295,13.8494748685453));
#424915=CARTESIAN_POINT('Ctrl Pts',(1.01876016026727,2.47264140853484,13.8557104837033));
#424916=CARTESIAN_POINT('Ctrl Pts',(1.0355421535842,2.47564995700456,13.8235269408542));
#424917=CARTESIAN_POINT('Ctrl Pts',(1.03569810139407,2.48745640859135,13.8362179249195));
#424918=CARTESIAN_POINT('Ctrl Pts',(1.01888277880466,2.4904410241898,13.8391868794965));
#424919=CARTESIAN_POINT('Origin',(1.10907800633986,2.43464556678511,13.8235269408515));
#424920=CARTESIAN_POINT('Ctrl Pts',(1.11951876426231,2.47531473453212,13.7902140241682));
#424921=CARTESIAN_POINT('Ctrl Pts',(1.12782218678114,2.48334042888628,13.8026027327198));
#424922=CARTESIAN_POINT('Ctrl Pts',(1.14132243324905,2.47361822349969,13.8057746032556));
#424923=CARTESIAN_POINT('Ctrl Pts',(1.11094683002701,2.46703589848542,13.8013225161808));
#424924=CARTESIAN_POINT('Ctrl Pts',(1.11924176202788,2.47505338131897,13.8136962270464));
#424925=CARTESIAN_POINT('Ctrl Pts',(1.13272799552232,2.46534976799986,13.8168830918628));
#424926=CARTESIAN_POINT('Ctrl Pts',(1.10237120035374,2.45875349335803,13.8124254880875));
#424927=CARTESIAN_POINT('Ctrl Pts',(1.11065398782056,2.46675923547352,13.8247886461867));
#424928=CARTESIAN_POINT('Ctrl Pts',(1.12412954988478,2.4570778208428,13.8279860620656));
#424929=CARTESIAN_POINT('Ctrl Pts',(1.09379172563669,2.45046737465958,13.8235227163065));
#424930=CARTESIAN_POINT('Ctrl Pts',(1.10205845903465,2.45845760007342,13.8358800595848));
#424931=CARTESIAN_POINT('Ctrl Pts',(1.11552693374202,2.44880223784019,13.8390832900376));
#424932=CARTESIAN_POINT('Origin',(1.13480505391371,2.45949293530442,13.7902182540695));
#424933=CARTESIAN_POINT('Ctrl Pts',(1.13423639626223,2.48952909261398,13.7382347919292));
#424934=CARTESIAN_POINT('Ctrl Pts',(1.145074137369,2.50002962766872,13.7369371795943));
#424935=CARTESIAN_POINT('Ctrl Pts',(1.15879643754766,2.4936076143686,13.7364597369711));
#424936=CARTESIAN_POINT('Ctrl Pts',(1.13559698884022,2.49084316332022,13.7595490285573));
#424937=CARTESIAN_POINT('Ctrl Pts',(1.14669400878008,2.50159351005293,13.7633824266925));
#424938=CARTESIAN_POINT('Ctrl Pts',(1.16041340014625,2.4954557612108,13.7648920890506));
#424939=CARTESIAN_POINT('Ctrl Pts',(1.12865804122628,2.48414147471485,13.7803806590111));
#424940=CARTESIAN_POINT('Ctrl Pts',(1.13825281004802,2.49344401723081,13.7901039518744));
#424941=CARTESIAN_POINT('Ctrl Pts',(1.15216715397904,2.48603615151962,13.7926933640892));
#424942=CARTESIAN_POINT('Ctrl Pts',(1.11659660135886,2.47249244385822,13.7936647693663));
#424943=CARTESIAN_POINT('Ctrl Pts',(1.12435525099816,2.48002747456282,13.8072068914933));
#424944=CARTESIAN_POINT('Ctrl Pts',(1.13789267255913,2.46966492239998,13.8104111085397));
#424945=CARTESIAN_POINT('Origin',(1.14971394064686,2.47389204588282,13.7435492065112));
#424946=CARTESIAN_POINT('Origin',(1.14971394064686,2.47389204588282,14.));
#424947=CARTESIAN_POINT('Origin',(1.14971394064686,2.47389204588282,12.5369868989719));
#424948=CARTESIAN_POINT('Ctrl Pts',(1.12437967912842,2.50255287813992,12.506462012331));
#424949=CARTESIAN_POINT('Ctrl Pts',(1.12705939221632,2.50851716567126,12.4999388158272));
#424950=CARTESIAN_POINT('Ctrl Pts',(1.12702768769627,2.50844660032808,12.4907030323752));
#424951=CARTESIAN_POINT('Ctrl Pts',(1.13723970050497,2.49925918213859,12.5042014951932));
#424952=CARTESIAN_POINT('Ctrl Pts',(1.14338470956401,2.50115126056727,12.4980716682127));
#424953=CARTESIAN_POINT('Ctrl Pts',(1.14955959101947,2.49832346916108,12.4907355092743));
#424954=CARTESIAN_POINT('Ctrl Pts',(1.13812530439812,2.49329752070994,12.5218047446509));
#424955=CARTESIAN_POINT('Ctrl Pts',(1.14857302621971,2.49880787275631,12.5216906929434));
#424956=CARTESIAN_POINT('Ctrl Pts',(1.15919134706604,2.49374605324804,12.5161988840776));
#424957=CARTESIAN_POINT('Ctrl Pts',(1.13440287727529,2.48968987289895,12.5369868989719));
#424958=CARTESIAN_POINT('Ctrl Pts',(1.14541101148044,2.50035882377718,12.5369868989719));
#424959=CARTESIAN_POINT('Ctrl Pts',(1.15923195340826,2.49372654696235,12.5369868989719));
#424960=CARTESIAN_POINT('Origin',(2.04412211573024E-31,-4.22882474612863E-32,
12.5));
#424961=CARTESIAN_POINT('Origin',(1.28989110379808,2.35316195826446,12.5));
#424962=CARTESIAN_POINT('',(1.28989110379808,2.35316195826446,12.5893111709658));
#424963=CARTESIAN_POINT('',(1.28989110379808,2.35316195826446,13.8235269408515));
#424964=CARTESIAN_POINT('',(1.28989110379808,2.35316195826446,12.5));
#424965=CARTESIAN_POINT('',(1.31755783794949,2.37582965599927,13.7902182540695));
#424966=CARTESIAN_POINT('',(1.28989110379808,2.35316195826446,13.8235269408515));
#424967=CARTESIAN_POINT('',(1.33359077777889,2.38896564204895,13.7435492065112));
#424968=CARTESIAN_POINT('Origin',(1.28084241121639,2.34574867356094,13.7445212918716));
#424969=CARTESIAN_POINT('',(1.33359077777889,2.38896564204895,12.5369868989719));
#424970=CARTESIAN_POINT('',(1.33359077777889,2.38896564204895,12.5));
#424971=CARTESIAN_POINT('Ctrl Pts',(1.33359077777889,2.38896564204895,12.5369868989719));
#424972=CARTESIAN_POINT('Ctrl Pts',(1.31903484374673,2.37703978513056,12.5544431401645));
#424973=CARTESIAN_POINT('Ctrl Pts',(1.30446849892367,2.36510539852233,12.5718848856037));
#424974=CARTESIAN_POINT('Ctrl Pts',(1.28989110379808,2.35316195826446,12.5893111709658));
#424975=CARTESIAN_POINT('Origin',(1.25991801334777,2.65677114278591,12.5));
#424976=CARTESIAN_POINT('',(1.23923296911491,2.43924636921446,13.7435492065112));
#424977=CARTESIAN_POINT('',(1.23727082998037,2.41861243359646,13.7902182540695));
#424978=CARTESIAN_POINT('Origin',(1.23211466746072,2.3643900170544,13.7418732680449));
#424979=CARTESIAN_POINT('',(1.23388492680971,2.38300613697746,13.8235269408515));
#424980=CARTESIAN_POINT('',(1.23727082998037,2.41861243359646,13.7902182540695));
#424981=CARTESIAN_POINT('',(1.23388492680971,2.38300613697746,12.5893111709658));
#424982=CARTESIAN_POINT('',(1.23388492680971,2.38300613697746,12.5));
#424983=CARTESIAN_POINT('',(1.23923296911491,2.43924636921446,12.5369868989719));
#424984=CARTESIAN_POINT('Ctrl Pts',(1.23388492680971,2.38300613697746,12.5893111709658));
#424985=CARTESIAN_POINT('Ctrl Pts',(1.23566893384522,2.4017668281358,12.5718848856037));
#424986=CARTESIAN_POINT('Ctrl Pts',(1.23745158852544,2.42051329787039,12.5544431401645));
#424987=CARTESIAN_POINT('Ctrl Pts',(1.23923296911491,2.43924636921446,12.5369868989719));
#424988=CARTESIAN_POINT('',(1.23923296911491,2.43924636921446,12.5));
#424989=CARTESIAN_POINT('Origin',(1.26810555253577,2.3797520011602,12.5));
#424990=CARTESIAN_POINT('',(1.25293690022837,2.3489055725281,13.8587068136939));
#424991=CARTESIAN_POINT('Ctrl Pts',(1.23388492680312,2.38300613697794,13.8235269408542));
#424992=CARTESIAN_POINT('Ctrl Pts',(1.23371904413407,2.38126170802633,13.8262006681044));
#424993=CARTESIAN_POINT('Ctrl Pts',(1.23372224654694,2.37946009270208,13.8288634856214));
#424994=CARTESIAN_POINT('Ctrl Pts',(1.23388244646385,2.37760692097054,13.8314912288862));
#424995=CARTESIAN_POINT('Ctrl Pts',(1.23404759605434,2.37569649206111,13.834200161153));
#424996=CARTESIAN_POINT('Ctrl Pts',(1.23437928288247,2.37372910685695,13.8368750301949));
#424997=CARTESIAN_POINT('Ctrl Pts',(1.23490650022355,2.37169483278667,13.8394886372968));
#424998=CARTESIAN_POINT('Ctrl Pts',(1.23494721849766,2.37153772086575,13.839690492513));
#424999=CARTESIAN_POINT('Ctrl Pts',(1.23498912515823,2.37138021174245,13.8398919674349));
#425000=CARTESIAN_POINT('Ctrl Pts',(1.23503224484409,2.37122230275869,13.8400930404591));
#425001=CARTESIAN_POINT('Ctrl Pts',(1.23570407855918,2.36876197455584,13.8432258934518));
#425002=CARTESIAN_POINT('Ctrl Pts',(1.23666586922088,2.36621683495141,13.8462331177034));
#425003=CARTESIAN_POINT('Ctrl Pts',(1.23797648648077,2.36370399305394,13.8489036603661));
#425004=CARTESIAN_POINT('Ctrl Pts',(1.23840533570063,2.36288176194168,13.849777493004));
#425005=CARTESIAN_POINT('Ctrl Pts',(1.23887155758534,2.36206323757994,13.85061494757));
#425006=CARTESIAN_POINT('Ctrl Pts',(1.2393772731659,2.36125323419899,13.8514076489583));
#425007=CARTESIAN_POINT('Ctrl Pts',(1.24044693455389,2.3595399602283,13.8530843267192));
#425008=CARTESIAN_POINT('Ctrl Pts',(1.24180086220381,2.35769808563273,13.8546805203176));
#425009=CARTESIAN_POINT('Ctrl Pts',(1.24347041342712,2.35591532610035,13.8559412814273));
#425010=CARTESIAN_POINT('Ctrl Pts',(1.24369385352563,2.35567673505865,13.8561100121513));
#425011=CARTESIAN_POINT('Ctrl Pts',(1.24392287006086,2.35543919916743,13.8562727473908));
#425012=CARTESIAN_POINT('Ctrl Pts',(1.2441574634853,2.35520315532629,13.8564289040185));
#425013=CARTESIAN_POINT('Ctrl Pts',(1.24522134198875,2.35413269919965,13.8571370725437));
#425014=CARTESIAN_POINT('Ctrl Pts',(1.246420230116,2.3530757178384,13.8577210840554));
#425015=CARTESIAN_POINT('Ctrl Pts',(1.24772693528028,2.35209531041194,13.8581177131616));
#425016=CARTESIAN_POINT('Ctrl Pts',(1.24809494842996,2.35181919393605,13.8582294175695));
#425017=CARTESIAN_POINT('Ctrl Pts',(1.2484713810434,2.3515490327149,13.8583265086086));
#425018=CARTESIAN_POINT('Ctrl Pts',(1.24885531616046,2.35128592415332,13.8584082369006));
#425019=CARTESIAN_POINT('Ctrl Pts',(1.24940692796741,2.35090790770569,13.8585256585398));
#425020=CARTESIAN_POINT('Ctrl Pts',(1.24998106704845,2.35054001643586,13.8586122832068));
#425021=CARTESIAN_POINT('Ctrl Pts',(1.25056324498123,2.35019247199092,13.8586682984299));
#425022=CARTESIAN_POINT('Ctrl Pts',(1.25102892961801,2.34991447088594,13.8587131050557));
#425023=CARTESIAN_POINT('Ctrl Pts',(1.25150478114356,2.34964621666249,13.8587357943552));
#425024=CARTESIAN_POINT('Ctrl Pts',(1.25199110480672,2.34938811861751,13.8587355499465));
#425025=CARTESIAN_POINT('Ctrl Pts',(1.25230542738467,2.34922130369772,13.8587353919793));
#425026=CARTESIAN_POINT('Ctrl Pts',(1.25262070736467,2.34906050111852,13.8587257282814));
#425027=CARTESIAN_POINT('Ctrl Pts',(1.25293690022837,2.3489055725281,13.8587068136939));
#425028=CARTESIAN_POINT('Ctrl Pts',(1.25293690022837,2.3489055725281,13.8587068136939));
#425029=CARTESIAN_POINT('Ctrl Pts',(1.25397684131982,2.34839602084015,13.8586446046466));
#425030=CARTESIAN_POINT('Ctrl Pts',(1.25502664573831,2.34794993036791,13.858482427929));
#425031=CARTESIAN_POINT('Ctrl Pts',(1.256084851049,2.34756307651182,13.8582284286032));
#425032=CARTESIAN_POINT('Ctrl Pts',(1.25717044660222,2.34716620945617,13.8579678548414));
#425033=CARTESIAN_POINT('Ctrl Pts',(1.25826806127632,2.3468321543241,13.857615680862));
#425034=CARTESIAN_POINT('Ctrl Pts',(1.25933160117973,2.34656481113383,13.8571944833187));
#425035=CARTESIAN_POINT('Ctrl Pts',(1.26198577377861,2.34589762886089,13.8561433417727));
#425036=CARTESIAN_POINT('Ctrl Pts',(1.26455071248909,2.34561007118124,13.8546163505474));
#425037=CARTESIAN_POINT('Ctrl Pts',(1.26687401671733,2.34556238142904,13.8528973491086));
#425038=CARTESIAN_POINT('Ctrl Pts',(1.26729845012266,2.34555366921491,13.8525833129072));
#425039=CARTESIAN_POINT('Ctrl Pts',(1.26771488194094,2.34555283567127,13.8522628768812));
#425040=CARTESIAN_POINT('Ctrl Pts',(1.26812248638786,2.34555888281998,13.851937733538));
#425041=CARTESIAN_POINT('Ctrl Pts',(1.27061167019269,2.34559581191813,13.8499521282529));
#425042=CARTESIAN_POINT('Ctrl Pts',(1.27301896572387,2.34589709572854,13.847639871647));
#425043=CARTESIAN_POINT('Ctrl Pts',(1.27522783158936,2.34636718110915,13.8452109780794));
#425044=CARTESIAN_POINT('Ctrl Pts',(1.2762216460635,2.34657868225217,13.8441181685877));
#425045=CARTESIAN_POINT('Ctrl Pts',(1.27717567567689,2.34682374661082,13.8430021611332));
#425046=CARTESIAN_POINT('Ctrl Pts',(1.27808185104523,2.34709155689088,13.8418824960098));
#425047=CARTESIAN_POINT('Ctrl Pts',(1.28021727644072,2.34772265865462,13.8392439765549));
#425048=CARTESIAN_POINT('Ctrl Pts',(1.28219011140962,2.34850661550767,13.8364981347964));
#425049=CARTESIAN_POINT('Ctrl Pts',(1.28401821055095,2.34941369905528,13.8336931113419));
#425050=CARTESIAN_POINT('Ctrl Pts',(1.28579866301958,2.35029714082553,13.8309611966328));
#425051=CARTESIAN_POINT('Ctrl Pts',(1.28744335927292,2.35129876559121,13.8281701127186));
#425052=CARTESIAN_POINT('Ctrl Pts',(1.28893971510898,2.3524175463524,13.8253580685121));
#425053=CARTESIAN_POINT('Ctrl Pts',(1.28926412666915,2.35266009922885,13.8247484142933));
#425054=CARTESIAN_POINT('Ctrl Pts',(1.28958140241306,2.35290821608639,13.8241378483365));
#425055=CARTESIAN_POINT('Ctrl Pts',(1.28989110379808,2.35316195826446,13.8235269408515));
#425056=CARTESIAN_POINT('',(1.25183235501256,2.34947368935035,12.5969504640361));
#425057=CARTESIAN_POINT('Origin',(1.2681212844785,2.37978110766788,12.584524458991));
#425058=CARTESIAN_POINT('Origin',(1.2681212844785,2.37978110766788,12.584524458991));
#425059=CARTESIAN_POINT('Ctrl Pts',(1.23388492680971,2.38300613697746,12.5893111709658));
#425060=CARTESIAN_POINT('Ctrl Pts',(1.23281198882938,2.37172307716861,12.5770542771492));
#425061=CARTESIAN_POINT('Ctrl Pts',(1.24852873949894,2.36716375449457,12.5737548217797));
#425062=CARTESIAN_POINT('Ctrl Pts',(1.23623108208401,2.40767840207199,12.5663937883685));
#425063=CARTESIAN_POINT('Ctrl Pts',(1.23515677542226,2.3963809491534,12.5540940315304));
#425064=CARTESIAN_POINT('Ctrl Pts',(1.25092312377384,2.39181058210357,12.5508374392248));
#425065=CARTESIAN_POINT('Ctrl Pts',(1.2385748701164,2.4323257731535,12.5434499600944));
#425066=CARTESIAN_POINT('Ctrl Pts',(1.23749707050107,2.42099158819238,12.5311293540533));
#425067=CARTESIAN_POINT('Ctrl Pts',(1.25331399434559,2.41643344332179,12.5278936106989));
#425068=CARTESIAN_POINT('Ctrl Pts',(1.24091647633618,2.45695020020412,12.5204817579905));
#425069=CARTESIAN_POINT('Ctrl Pts',(1.2398333423494,2.44555991877323,12.5081597038247));
#425070=CARTESIAN_POINT('Ctrl Pts',(1.25570161052364,2.44103420225039,12.5049254088044));
#425071=CARTESIAN_POINT('Ctrl Pts',(1.23923296911491,2.43924636921446,12.5369868989719));
#425072=CARTESIAN_POINT('Ctrl Pts',(1.23932115089342,2.44017369070384,12.5342545179733));
#425073=CARTESIAN_POINT('Ctrl Pts',(1.23952949340843,2.4410468748252,12.5314872231885));
#425074=CARTESIAN_POINT('Ctrl Pts',(1.23990063494665,2.44180375993454,12.5287124745063));
#425075=CARTESIAN_POINT('Ctrl Pts',(1.24023534880764,2.44248635649457,12.5262100684184));
#425076=CARTESIAN_POINT('Ctrl Pts',(1.24070301789607,2.44307324145897,12.5237004536639));
#425077=CARTESIAN_POINT('Ctrl Pts',(1.24136351575186,2.44353317966562,12.5212220730815));
#425078=CARTESIAN_POINT('Ctrl Pts',(1.24186918399808,2.44388530215064,12.5193246583486));
#425079=CARTESIAN_POINT('Ctrl Pts',(1.24249427965073,2.44416670586086,12.517417831369));
#425080=CARTESIAN_POINT('Ctrl Pts',(1.24329542582199,2.44429834747954,12.5155812248348));
#425081=CARTESIAN_POINT('Ctrl Pts',(1.24363671839713,2.44435442751668,12.5147988205793));
#425082=CARTESIAN_POINT('Ctrl Pts',(1.244010262265,2.44438365892971,12.5140295443047));
#425083=CARTESIAN_POINT('Ctrl Pts',(1.24442133344266,2.4443818590029,12.5132817086137));
#425084=CARTESIAN_POINT('Ctrl Pts',(1.24504343406159,2.44437913505716,12.5121499604604));
#425085=CARTESIAN_POINT('Ctrl Pts',(1.24576488493838,2.44429813043238,12.5110494206568));
#425086=CARTESIAN_POINT('Ctrl Pts',(1.2465936600746,2.44410246774485,12.5100666561695));
#425087=CARTESIAN_POINT('Ctrl Pts',(1.24706954084931,2.44399011868025,12.5095023550641));
#425088=CARTESIAN_POINT('Ctrl Pts',(1.24758615513775,2.44383803313712,12.5089719619137));
#425089=CARTESIAN_POINT('Ctrl Pts',(1.24813201585584,2.44364293479422,12.5085043804652));
#425090=CARTESIAN_POINT('Ctrl Pts',(1.2489308119134,2.44335743378275,12.5078201359221));
#425091=CARTESIAN_POINT('Ctrl Pts',(1.24981499902482,2.44297040514737,12.5072563000949));
#425092=CARTESIAN_POINT('Ctrl Pts',(1.25072124756621,2.44250032816684,12.5068768744332));
#425093=CARTESIAN_POINT('Ctrl Pts',(1.25137471515091,2.44216137030367,12.5066032824114));
#425094=CARTESIAN_POINT('Ctrl Pts',(1.25205116145639,2.44177333059376,12.5064197834844));
#425095=CARTESIAN_POINT('Ctrl Pts',(1.25271409815743,2.4413601203232,12.5063282718343));
#425096=CARTESIAN_POINT('Ctrl Pts',(1.25368178050094,2.44075696125485,12.5061946931565));
#425097=CARTESIAN_POINT('Ctrl Pts',(1.25464192290353,2.44008818098697,12.5062515701262));
#425098=CARTESIAN_POINT('Ctrl Pts',(1.255543776096,2.43940797481384,12.5064436508398));
#425099=CARTESIAN_POINT('',(1.24852873949894,2.36716375449457,12.5737548217797));
#425100=CARTESIAN_POINT('Origin',(1.25578612727439,2.38092349005441,12.5893111709658));
#425101=CARTESIAN_POINT('Ctrl Pts',(1.255543776096,2.43940797481384,12.5064436508398));
#425102=CARTESIAN_POINT('Ctrl Pts',(1.25450584661706,2.4287139068251,12.5164271754438));
#425103=CARTESIAN_POINT('Ctrl Pts',(1.25346729774465,2.41801561989398,12.5264061185523));
#425104=CARTESIAN_POINT('Ctrl Pts',(1.2524281086063,2.40731296534145,12.536380305637));
#425105=CARTESIAN_POINT('Ctrl Pts',(1.25112933295363,2.39393681788302,12.5488460165097));
#425106=CARTESIAN_POINT('Ctrl Pts',(1.24982955680223,2.38055384428151,12.5613043021964));
#425107=CARTESIAN_POINT('Ctrl Pts',(1.24852873949894,2.36716375449458,12.5737548217797));
#425108=CARTESIAN_POINT('Ctrl Pts',(1.28989110379807,2.35316195826446,12.5893111709658));
#425109=CARTESIAN_POINT('Ctrl Pts',(1.28112396298907,2.3459789312845,12.5770542771492));
#425110=CARTESIAN_POINT('Ctrl Pts',(1.26857444251688,2.35648194088999,12.5737548217797));
#425111=CARTESIAN_POINT('Ctrl Pts',(1.28171143767584,2.34646025656683,12.5928319619712));
#425112=CARTESIAN_POINT('Ctrl Pts',(1.27375474566441,2.34415277555787,12.5821634970843));
#425113=CARTESIAN_POINT('Ctrl Pts',(1.26560077011944,2.3540333719524,12.5773203894503));
#425114=CARTESIAN_POINT('Ctrl Pts',(1.26550735256142,2.34221623430672,12.5969440695591));
#425115=CARTESIAN_POINT('Ctrl Pts',(1.26195126254369,2.34409047184176,12.5878292599214));
#425116=CARTESIAN_POINT('Ctrl Pts',(1.25982478515117,2.35252269503661,12.5813877129824));
#425117=CARTESIAN_POINT('Ctrl Pts',(1.23847953964047,2.35655752344862,12.596957478804));
#425118=CARTESIAN_POINT('Ctrl Pts',(1.24200938657361,2.35469720794379,12.5878468778671));
#425119=CARTESIAN_POINT('Ctrl Pts',(1.25015395219074,2.35766091050071,12.5814011370086));
#425120=CARTESIAN_POINT('Ctrl Pts',(1.23288243149495,2.37246385512966,12.5928371701607));
#425121=CARTESIAN_POINT('Ctrl Pts',(1.2354084260042,2.36458004783603,12.5821692192951));
#425122=CARTESIAN_POINT('Ctrl Pts',(1.24815323881001,2.3633176816005,12.5773318885715));
#425123=CARTESIAN_POINT('Ctrl Pts',(1.23388492680966,2.38300613697746,12.5893111709658));
#425124=CARTESIAN_POINT('Ctrl Pts',(1.23281198882932,2.37172307716861,12.5770542771492));
#425125=CARTESIAN_POINT('Ctrl Pts',(1.24852873949888,2.36716375449458,12.5737548217797));
#425126=CARTESIAN_POINT('',(1.26857444251688,2.35648194088999,12.5737548217797));
#425127=CARTESIAN_POINT('Origin',(1.2759483509902,2.37017958571773,12.5893111709658));
#425128=CARTESIAN_POINT('Ctrl Pts',(1.24852873949888,2.36716375449458,12.5737548217797));
#425129=CARTESIAN_POINT('Ctrl Pts',(1.24840138077704,2.36616972261029,12.5746934679442));
#425130=CARTESIAN_POINT('Ctrl Pts',(1.24844214888152,2.36504648025003,12.5756680099006));
#425131=CARTESIAN_POINT('Ctrl Pts',(1.24864307774563,2.36392169971164,12.5765688348656));
#425132=CARTESIAN_POINT('Ctrl Pts',(1.24869627143804,2.36362392651583,12.5768073183026));
#425133=CARTESIAN_POINT('Ctrl Pts',(1.24876043380594,2.36332606325736,12.5770407398754));
#425134=CARTESIAN_POINT('Ctrl Pts',(1.2488348634857,2.36303037530415,12.5772674179684));
#425135=CARTESIAN_POINT('Ctrl Pts',(1.2491403027648,2.36181695190157,12.5781976435658));
#425136=CARTESIAN_POINT('Ctrl Pts',(1.24964693662665,2.36057399590364,12.5790594849312));
#425137=CARTESIAN_POINT('Ctrl Pts',(1.25036527352791,2.35940366055855,12.5797571720116));
#425138=CARTESIAN_POINT('Ctrl Pts',(1.25083329584817,2.35864114499971,12.580211740231));
#425139=CARTESIAN_POINT('Ctrl Pts',(1.25142845462241,2.35788462466702,12.5806009430798));
#425140=CARTESIAN_POINT('Ctrl Pts',(1.25212277751592,2.35719830959079,12.5808812374708));
#425141=CARTESIAN_POINT('Ctrl Pts',(1.25271943122067,2.35660853725765,12.5811221033394));
#425142=CARTESIAN_POINT('Ctrl Pts',(1.25340160809937,2.35605861502781,12.581287365893));
#425143=CARTESIAN_POINT('Ctrl Pts',(1.25413603790667,2.35558607281637,12.581359338449));
#425144=CARTESIAN_POINT('Ctrl Pts',(1.25423810848449,2.3555203992066,12.5813693411482));
#425145=CARTESIAN_POINT('Ctrl Pts',(1.25434117457716,2.35545616193782,12.5813775999465));
#425146=CARTESIAN_POINT('Ctrl Pts',(1.25444513383263,2.35539340181603,12.5813841266931));
#425147=CARTESIAN_POINT('Ctrl Pts',(1.25462151328316,2.35528692167874,12.5813952001081));
#425148=CARTESIAN_POINT('Ctrl Pts',(1.2548019597066,2.35518450163979,12.5814007534795));
#425149=CARTESIAN_POINT('Ctrl Pts',(1.25498649185973,2.35508635781519,12.5814005856065));
#425150=CARTESIAN_POINT('Ctrl Pts',(1.25583120790937,2.35463709375792,12.5813998171494));
#425151=CARTESIAN_POINT('Ctrl Pts',(1.25670301652934,2.3543081783724,12.58127954464));
#425152=CARTESIAN_POINT('Ctrl Pts',(1.25758652333905,2.35407379444733,12.5810700125799));
#425153=CARTESIAN_POINT('Ctrl Pts',(1.25865369896987,2.35379068535259,12.5808169217085));
#425154=CARTESIAN_POINT('Ctrl Pts',(1.25974233003,2.35366164747295,12.5804173076348));
#425155=CARTESIAN_POINT('Ctrl Pts',(1.2607539453339,2.35367212814817,12.5799304713245));
#425156=CARTESIAN_POINT('Ctrl Pts',(1.26200765538713,2.35368511700652,12.5793271277669));
#425157=CARTESIAN_POINT('Ctrl Pts',(1.26322118031378,2.35388099977963,12.5785808224116));
#425158=CARTESIAN_POINT('Ctrl Pts',(1.26434842190364,2.35422020806532,12.5777485681082));
#425159=CARTESIAN_POINT('Ctrl Pts',(1.26602813537108,2.35472566557403,12.576508418016));
#425160=CARTESIAN_POINT('Ctrl Pts',(1.26750409977113,2.3555385300157,12.5750928681475));
#425161=CARTESIAN_POINT('Ctrl Pts',(1.26857444251688,2.35648194088999,12.5737548217797));
#425162=CARTESIAN_POINT('Ctrl Pts',(1.26857444251688,2.35648194088999,12.5737548217797));
#425163=CARTESIAN_POINT('Ctrl Pts',(1.28112396298907,2.3459789312845,12.5770542771492));
#425164=CARTESIAN_POINT('Ctrl Pts',(1.28989110379808,2.35316195826446,12.5893111709658));
#425165=CARTESIAN_POINT('Ctrl Pts',(1.28769435307392,2.37221229290324,12.5508408821982));
#425166=CARTESIAN_POINT('Ctrl Pts',(1.30028069286421,2.36167427718335,12.55409748406));
#425167=CARTESIAN_POINT('Ctrl Pts',(1.30905901829952,2.36886646786604,12.5663972313419));
#425168=CARTESIAN_POINT('Ctrl Pts',(1.30679633527328,2.38792636748136,12.52790050457));
#425169=CARTESIAN_POINT('Ctrl Pts',(1.31940073304203,2.37733956275899,12.5311362602938));
#425170=CARTESIAN_POINT('Ctrl Pts',(1.32820759552495,2.38455513419804,12.5434568539655));
#425171=CARTESIAN_POINT('Ctrl Pts',(1.3258817911766,2.40362541889598,12.5049357605811));
#425172=CARTESIAN_POINT('Ctrl Pts',(1.33848790823583,2.39297792164647,12.5081700652078));
#425173=CARTESIAN_POINT('Ctrl Pts',(1.34733834997374,2.40022919810854,12.5204921097672));
#425174=CARTESIAN_POINT('Ctrl Pts',(1.32462856633754,2.40259455641597,12.5064436508395));
#425175=CARTESIAN_POINT('Ctrl Pts',(1.3257817226758,2.40219571026755,12.5062361689309));
#425176=CARTESIAN_POINT('Ctrl Pts',(1.32696390321607,2.40173176976419,12.5061871075061));
#425177=CARTESIAN_POINT('Ctrl Pts',(1.32808112761236,2.40121910389888,12.5063648335164));
#425178=CARTESIAN_POINT('Ctrl Pts',(1.32858863984641,2.40098621944031,12.5064455676329));
#425179=CARTESIAN_POINT('Ctrl Pts',(1.32908973499688,2.40073983183135,12.506574497099));
#425180=CARTESIAN_POINT('Ctrl Pts',(1.32956246388191,2.40048956232518,12.5067492519495));
#425181=CARTESIAN_POINT('Ctrl Pts',(1.33051243092642,2.39998663603774,12.5071004286051));
#425182=CARTESIAN_POINT('Ctrl Pts',(1.33138239676436,2.39944882862522,12.5076537929613));
#425183=CARTESIAN_POINT('Ctrl Pts',(1.33211203942697,2.39892455061569,12.5083435010505));
#425184=CARTESIAN_POINT('Ctrl Pts',(1.33215797479295,2.39889154418189,12.5083869222964));
#425185=CARTESIAN_POINT('Ctrl Pts',(1.33220335203943,2.39885857807958,12.5084308732337));
#425186=CARTESIAN_POINT('Ctrl Pts',(1.33224815570986,2.39882565891842,12.5084753333615));
#425187=CARTESIAN_POINT('Ctrl Pts',(1.33260754028227,2.39856160379656,12.5088319622689));
#425188=CARTESIAN_POINT('Ctrl Pts',(1.33293808002931,2.39829624781952,12.509227847131));
#425189=CARTESIAN_POINT('Ctrl Pts',(1.33323169918076,2.39803966489652,12.5096423454524));
#425190=CARTESIAN_POINT('Ctrl Pts',(1.33415177165101,2.39723564757469,12.5109411997424));
#425191=CARTESIAN_POINT('Ctrl Pts',(1.33477226655723,2.39647560273324,12.5124831113042));
#425192=CARTESIAN_POINT('Ctrl Pts',(1.33518436073789,2.39578488074739,12.5140723025007));
#425193=CARTESIAN_POINT('Ctrl Pts',(1.33522297441397,2.39572015934078,12.5142212114565));
#425194=CARTESIAN_POINT('Ctrl Pts',(1.33525978784662,2.39565604397801,12.5143705582413));
#425195=CARTESIAN_POINT('Ctrl Pts',(1.33529489302807,2.3955925555676,12.5145201959299));
#425196=CARTESIAN_POINT('Ctrl Pts',(1.33574587135004,2.39477695241153,12.5164425148273));
#425197=CARTESIAN_POINT('Ctrl Pts',(1.33593978258578,2.39404206724226,12.518463520594));
#425198=CARTESIAN_POINT('Ctrl Pts',(1.33596342966419,2.39336333931705,12.5205025929157));
#425199=CARTESIAN_POINT('Ctrl Pts',(1.33597714590695,2.39296965021816,12.5216853356836));
#425200=CARTESIAN_POINT('Ctrl Pts',(1.33593403594348,2.39259558299747,12.5228750347131));
#425201=CARTESIAN_POINT('Ctrl Pts',(1.33585231933275,2.39224212827041,12.5240609649613));
#425202=CARTESIAN_POINT('Ctrl Pts',(1.33565175029564,2.39137459260503,12.5269717671327));
#425203=CARTESIAN_POINT('Ctrl Pts',(1.33520282957202,2.39060915862872,12.5299036066169));
#425204=CARTESIAN_POINT('Ctrl Pts',(1.33458638341544,2.38991457511165,12.532813300402));
#425205=CARTESIAN_POINT('Ctrl Pts',(1.33429045336569,2.38958113457907,12.5342101228452));
#425206=CARTESIAN_POINT('Ctrl Pts',(1.3339558933572,2.3892647858674,12.5356023438238));
#425207=CARTESIAN_POINT('Ctrl Pts',(1.33359077777889,2.38896564204895,12.5369868989719));
#425208=CARTESIAN_POINT('Origin',(11.1950251471808,10.4617154507776,-1.23893508993275));
#425209=CARTESIAN_POINT('Ctrl Pts',(1.23922897310923,2.4392047664156,12.5369868989719));
#425210=CARTESIAN_POINT('Ctrl Pts',(1.24071005285903,2.45447204208811,12.5369868989719));
#425211=CARTESIAN_POINT('Ctrl Pts',(1.22689668627604,2.46114094059758,12.5369868989719));
#425212=CARTESIAN_POINT('Ctrl Pts',(1.23972957008679,2.44436570908569,12.5218025310016));
#425213=CARTESIAN_POINT('Ctrl Pts',(1.23752371138027,2.45597562084555,12.5216901060418));
#425214=CARTESIAN_POINT('Ctrl Pts',(1.22693880116534,2.46112062643631,12.5161920673678));
#425215=CARTESIAN_POINT('Ctrl Pts',(1.24494231460027,2.44739281427596,12.5042015548894));
#425216=CARTESIAN_POINT('Ctrl Pts',(1.24258833028154,2.45337914059885,12.4980677368513));
#425217=CARTESIAN_POINT('Ctrl Pts',(1.2365225068672,2.45644452247225,12.4907278922777));
#425218=CARTESIAN_POINT('Ctrl Pts',(1.25553462293633,2.43939019102985,12.506463626192));
#425219=CARTESIAN_POINT('Ctrl Pts',(1.25852880079779,2.44520760774782,12.4999376786891));
#425220=CARTESIAN_POINT('Ctrl Pts',(1.25849223126875,2.44513655646112,12.4906970594712));
#425221=CARTESIAN_POINT('Origin',(1.21733176865023,2.4413290161375,12.5369868989719));
#425222=CARTESIAN_POINT('Origin',(1.21733176865023,2.4413290161375,14.));
#425223=CARTESIAN_POINT('Origin',(1.21733176865023,2.4413290161375,13.7435492065112));
#425224=CARTESIAN_POINT('Ctrl Pts',(1.23688900779627,2.41459746266198,13.793642941384));
#425225=CARTESIAN_POINT('Ctrl Pts',(1.23793966058313,2.42535861258785,13.8071662555867));
#425226=CARTESIAN_POINT('Ctrl Pts',(1.22141779253926,2.42948744534977,13.8103758687955));
#425227=CARTESIAN_POINT('Ctrl Pts',(1.23846246208079,2.43114394104373,13.7804579775006));
#425228=CARTESIAN_POINT('Ctrl Pts',(1.23974877984366,2.44442321279872,13.7901904343351));
#425229=CARTESIAN_POINT('Ctrl Pts',(1.22528217916204,2.45066607983901,13.7927914348262));
#425230=CARTESIAN_POINT('Ctrl Pts',(1.23938881379597,2.44088547558468,13.7597120340895));
#425231=CARTESIAN_POINT('Ctrl Pts',(1.24087174199913,2.45625388519388,13.7635825532445));
#425232=CARTESIAN_POINT('Ctrl Pts',(1.22753585632341,2.46315968488607,13.7651073818884));
#425233=CARTESIAN_POINT('Ctrl Pts',(1.23920741291829,2.43897786006587,13.7381884353898));
#425234=CARTESIAN_POINT('Ctrl Pts',(1.2406565251009,2.45398645708587,13.7368803041982));
#425235=CARTESIAN_POINT('Ctrl Pts',(1.22709403298645,2.46071315350867,13.7363986145813));
#425236=CARTESIAN_POINT('Origin',(1.2153696295157,2.42069508051951,13.7902182540695));
#425237=CARTESIAN_POINT('Ctrl Pts',(1.23388455343094,2.38300221852792,13.8235227101244));
#425238=CARTESIAN_POINT('Ctrl Pts',(1.23497734612654,2.39444723894921,13.8358800583119));
#425239=CARTESIAN_POINT('Ctrl Pts',(1.21903101699467,2.39895729840277,13.8390832900376));
#425240=CARTESIAN_POINT('Ctrl Pts',(1.23501368690463,2.39487623246143,13.8124254819052));
#425241=CARTESIAN_POINT('Ctrl Pts',(1.23610860151124,2.40634347897658,13.8247886449157));
#425242=CARTESIAN_POINT('Ctrl Pts',(1.22013748488756,2.41084283614122,13.8279860620657));
#425243=CARTESIAN_POINT('Ctrl Pts',(1.23614231433744,2.40674492484817,13.8013225099955));
#425244=CARTESIAN_POINT('Ctrl Pts',(1.23723883622677,2.41822898656775,13.8136962257787));
#425245=CARTESIAN_POINT('Ctrl Pts',(1.22124371042945,2.42272284633523,13.8168830918626));
#425246=CARTESIAN_POINT('Ctrl Pts',(1.23727045541865,2.4186085027414,13.7902140179785));
#425247=CARTESIAN_POINT('Ctrl Pts',(1.23836810359418,2.43010432241759,13.802602731458));
#425248=CARTESIAN_POINT('Ctrl Pts',(1.22234970497524,2.43459754600491,13.8057746032558));
#425249=CARTESIAN_POINT('Origin',(1.21198372634504,2.3850887839005,13.8235269408515));
#425250=CARTESIAN_POINT('Ctrl Pts',(1.28989110379808,2.35316195826446,13.8235269408515));
#425251=CARTESIAN_POINT('Ctrl Pts',(1.29902452747577,2.36064508533239,13.8362179249168));
#425252=CARTESIAN_POINT('Ctrl Pts',(1.31184217606322,2.34935921413227,13.8391868794938));
#425253=CARTESIAN_POINT('Ctrl Pts',(1.28153441868724,2.34631522271842,13.8400110824519));
#425254=CARTESIAN_POINT('Ctrl Pts',(1.29102528746501,2.34966861990706,13.8494522556837));
#425255=CARTESIAN_POINT('Ctrl Pts',(1.29801822404552,2.33817833159836,13.85569149686));
#425256=CARTESIAN_POINT('Ctrl Pts',(1.2658105689127,2.34205397004906,13.8586819406588));
#425257=CARTESIAN_POINT('Ctrl Pts',(1.26965945991938,2.34001875957994,13.868010383617));
#425258=CARTESIAN_POINT('Ctrl Pts',(1.27187813177613,2.33124548413774,13.8744918421245));
#425259=CARTESIAN_POINT('Ctrl Pts',(1.2381716118188,2.3567222879045,13.8587686893867));
#425260=CARTESIAN_POINT('Ctrl Pts',(1.23435694958484,2.35873933524174,13.8680909899357));
#425261=CARTESIAN_POINT('Ctrl Pts',(1.22586859096482,2.35566619849833,13.8745789365163));
#425262=CARTESIAN_POINT('Ctrl Pts',(1.2328605569214,2.37223382128573,13.8400379222776));
#425263=CARTESIAN_POINT('Ctrl Pts',(1.23034480289294,2.38197759958659,13.8494748685453));
#425264=CARTESIAN_POINT('Ctrl Pts',(1.21691354955425,2.38137548745683,13.8557104837033));
#425265=CARTESIAN_POINT('Ctrl Pts',(1.23388492680312,2.38300613697794,13.8235269408542));
#425266=CARTESIAN_POINT('Ctrl Pts',(1.23500269111959,2.39476059237678,13.8362179249195));
#425267=CARTESIAN_POINT('Ctrl Pts',(1.21848659400803,2.39910588180992,13.8391868794965));
#425268=CARTESIAN_POINT('Origin',(1.30383385660595,2.33614433081118,13.8235269408515));
#425269=CARTESIAN_POINT('Ctrl Pts',(1.31755478849323,2.37582715655954,13.7902140241682));
#425270=CARTESIAN_POINT('Ctrl Pts',(1.32648475065538,2.38314934005731,13.8026027327198));
#425271=CARTESIAN_POINT('Ctrl Pts',(1.33914762617131,2.37235908908981,13.8057746032556));
#425272=CARTESIAN_POINT('Ctrl Pts',(1.3083365746672,2.36827455987497,13.8013225161808));
#425273=CARTESIAN_POINT('Ctrl Pts',(1.31725740524774,2.37558925123131,13.8136962270464));
#425274=CARTESIAN_POINT('Ctrl Pts',(1.32990782984329,2.36481867265513,13.8168830918628));
#425275=CARTESIAN_POINT('Ctrl Pts',(1.29911438678623,2.36071870719801,13.8124254880875));
#425276=CARTESIAN_POINT('Ctrl Pts',(1.30802215626515,2.36802268679485,13.8247886461868));
#425277=CARTESIAN_POINT('Ctrl Pts',(1.32066375433798,2.35727510286342,13.8279860620656));
#425278=CARTESIAN_POINT('Ctrl Pts',(1.28988806396505,2.35315946671338,13.8235227163065));
#425279=CARTESIAN_POINT('Ctrl Pts',(1.29877856803845,2.36044928979476,13.8358800595847));
#425280=CARTESIAN_POINT('Ctrl Pts',(1.31141522584929,2.34972824925897,13.8390832900376));
#425281=CARTESIAN_POINT('Origin',(1.33150059075736,2.35881202854599,13.7902182540695));
#425282=CARTESIAN_POINT('Ctrl Pts',(1.33338205093011,2.38879459389766,13.7382347919292));
#425283=CARTESIAN_POINT('Ctrl Pts',(1.34503962143658,2.39837681277536,13.7369371795943));
#425284=CARTESIAN_POINT('Ctrl Pts',(1.35819280809039,2.39085767333853,13.7364597369711));
#425285=CARTESIAN_POINT('Ctrl Pts',(1.33484522521034,2.38999339121579,13.7595490285574));
#425286=CARTESIAN_POINT('Ctrl Pts',(1.34678157379184,2.3998034569118,13.7633824266926));
#425287=CARTESIAN_POINT('Ctrl Pts',(1.35995503150433,2.39256787316164,13.7648920890506));
#425288=CARTESIAN_POINT('Ctrl Pts',(1.32738311653536,2.38387959057498,13.780380659011));
#425289=CARTESIAN_POINT('Ctrl Pts',(1.33770420313101,2.39236911691569,13.7901039518744));
#425290=CARTESIAN_POINT('Ctrl Pts',(1.35096843840372,2.38385175206171,13.7926933640892));
#425291=CARTESIAN_POINT('Ctrl Pts',(1.31441230595499,2.37325244022971,13.7936647693663));
#425292=CARTESIAN_POINT('Ctrl Pts',(1.32275931428189,2.38012999676785,13.8072068914933));
#425293=CARTESIAN_POINT('Ctrl Pts',(1.33540704698687,2.36869849960996,13.8104111085397));
#425294=CARTESIAN_POINT('Origin',(1.34753353058677,2.37194801459568,13.7435492065112));
#425295=CARTESIAN_POINT('Origin',(1.34753353058677,2.37194801459568,14.));
#425296=CARTESIAN_POINT('Origin',(1.34753353058677,2.37194801459568,12.5369868989719));
#425297=CARTESIAN_POINT('Ctrl Pts',(1.32461969063675,2.40257845780336,12.506462012331));
#425298=CARTESIAN_POINT('Ctrl Pts',(1.32777663200395,2.40830447816604,12.4999388158272));
#425299=CARTESIAN_POINT('Ctrl Pts',(1.3277392812475,2.40823673183594,12.4907030323752));
#425300=CARTESIAN_POINT('Ctrl Pts',(1.33716845455174,2.39824751017493,12.5042014951932));
#425301=CARTESIAN_POINT('Ctrl Pts',(1.3434472385572,2.39963241758292,12.4980716682127));
#425302=CARTESIAN_POINT('Ctrl Pts',(1.34937108235248,2.39631072525598,12.4907355092744));
#425303=CARTESIAN_POINT('Ctrl Pts',(1.33756518091922,2.39223350074408,12.5218047446509));
#425304=CARTESIAN_POINT('Ctrl Pts',(1.3484272836557,2.39687393122821,12.5216906929434));
#425305=CARTESIAN_POINT('Ctrl Pts',(1.35859768763379,2.39096346278212,12.5161988840775));
#425306=CARTESIAN_POINT('Ctrl Pts',(1.33356108307719,2.38894126945141,12.5369868989719));
#425307=CARTESIAN_POINT('Ctrl Pts',(1.34540220716617,2.39867745514345,12.5369868989719));
#425308=CARTESIAN_POINT('Ctrl Pts',(1.35863656891839,2.39094071160812,12.5369868989719));
#425309=CARTESIAN_POINT('Origin',(2.42277625004769E-31,-6.05232695006679E-32,
12.5));
#425310=CARTESIAN_POINT('Origin',(1.47740364284705,2.24019390624622,12.5));
#425311=CARTESIAN_POINT('',(1.47740364284705,2.24019390624622,12.5893111709658));
#425312=CARTESIAN_POINT('',(1.47740364284705,2.24019390624622,13.8235269408515));
#425313=CARTESIAN_POINT('',(1.47740364284705,2.24019390624622,12.5));
#425314=CARTESIAN_POINT('',(1.50682594602495,2.260531083408,13.7902182540695));
#425315=CARTESIAN_POINT('',(1.47740364284705,2.24019390624622,13.8235269408515));
#425316=CARTESIAN_POINT('',(1.52387624238129,2.2723165271091,13.7435492065112));
#425317=CARTESIAN_POINT('Origin',(1.46778080751396,2.2335428410822,13.7445212918695));
#425318=CARTESIAN_POINT('',(1.52387624238129,2.2723165271091,12.5369868989719));
#425319=CARTESIAN_POINT('',(1.52387624238129,2.2723165271091,12.5));
#425320=CARTESIAN_POINT('Ctrl Pts',(1.52387624238129,2.2723165271091,12.5369868989719));
#425321=CARTESIAN_POINT('Ctrl Pts',(1.50839667396574,2.26161679625011,12.5544431401645));
#425322=CARTESIAN_POINT('Ctrl Pts',(1.49290603415143,2.25090941265923,12.5718848856037));
#425323=CARTESIAN_POINT('Ctrl Pts',(1.47740364284705,2.24019390624622,12.5893111709658));
#425324=CARTESIAN_POINT('Origin',(1.47227725249127,2.54523594138047,12.5));
#425325=CARTESIAN_POINT('',(1.43393074758915,2.3301209866841,13.7435492065112));
#425326=CARTESIAN_POINT('',(1.43029328000174,2.30971564133977,13.7902182540695));
#425327=CARTESIAN_POINT('Origin',(1.4207346438628,2.25609392052757,13.7418732680446));
#425328=CARTESIAN_POINT('',(1.42401639941738,2.27450380427705,13.8235269408515));
#425329=CARTESIAN_POINT('',(1.43029328000174,2.30971564133977,13.7902182540695));
#425330=CARTESIAN_POINT('',(1.42401639941738,2.27450380427705,12.5893111709658));
#425331=CARTESIAN_POINT('',(1.42401639941738,2.27450380427705,12.5));
#425332=CARTESIAN_POINT('',(1.43393074758915,2.3301209866841,12.5369868989719));
#425333=CARTESIAN_POINT('Ctrl Pts',(1.42401639941738,2.27450380427705,12.5893111709658));
#425334=CARTESIAN_POINT('Ctrl Pts',(1.42732364081181,2.2930566576479,12.5718848856037));
#425335=CARTESIAN_POINT('Ctrl Pts',(1.43062837517274,2.31159544714513,12.5544431401645));
#425336=CARTESIAN_POINT('Ctrl Pts',(1.43393074758915,2.3301209866841,12.5369868989719));
#425337=CARTESIAN_POINT('',(1.43393074758915,2.3301209866841,12.5));
#425338=CARTESIAN_POINT('Origin',(1.45785791655531,2.26847119764282,12.5));
#425339=CARTESIAN_POINT('',(1.44022546638962,2.23896379393913,13.8587068136939));
#425340=CARTESIAN_POINT('Ctrl Pts',(1.42401639941085,2.27450380427807,13.8235269408542));
#425341=CARTESIAN_POINT('Ctrl Pts',(1.42370888154866,2.27277870074739,13.8262006681044));
#425342=CARTESIAN_POINT('Ctrl Pts',(1.42356522493145,2.27098281912313,13.8288634856214));
#425343=CARTESIAN_POINT('Ctrl Pts',(1.42357384109623,2.26912275588719,13.8314912288862));
#425344=CARTESIAN_POINT('Ctrl Pts',(1.4235827234734,2.26720522254756,13.8342001611531));
#425345=CARTESIAN_POINT('Ctrl Pts',(1.42375294648253,2.26521734809964,13.8368750301949));
#425346=CARTESIAN_POINT('Ctrl Pts',(1.42411259732939,2.26314686980077,13.8394886372968));
#425347=CARTESIAN_POINT('Ctrl Pts',(1.42414037403668,2.26298696173946,13.8396904925131));
#425348=CARTESIAN_POINT('Ctrl Pts',(1.42416930280051,2.26282656093291,13.8398919674349));
#425349=CARTESIAN_POINT('Ctrl Pts',(1.42419940796103,2.26266566272357,13.8400930404591));
#425350=CARTESIAN_POINT('Ctrl Pts',(1.42466846661575,2.26015876037508,13.8432258934518));
#425351=CARTESIAN_POINT('Ctrl Pts',(1.42541960449268,2.25754369464496,13.8462331177034));
#425352=CARTESIAN_POINT('Ctrl Pts',(1.42652104083903,2.25493238654776,13.8489036603661));
#425353=CARTESIAN_POINT('Ctrl Pts',(1.42688144362962,2.25407793614903,13.849777493004));
#425354=CARTESIAN_POINT('Ctrl Pts',(1.42727939686518,2.25322413394779,13.85061494757));
#425355=CARTESIAN_POINT('Ctrl Pts',(1.42771740692362,2.2523756052716,13.8514076489583));
#425356=CARTESIAN_POINT('Ctrl Pts',(1.42864386136771,2.25058084474533,13.8530843267192));
#425357=CARTESIAN_POINT('Ctrl Pts',(1.42984315405642,2.24863474116279,13.8546805203176));
#425358=CARTESIAN_POINT('Ctrl Pts',(1.43136183853355,2.24672182969162,13.8559412814274));
#425359=CARTESIAN_POINT('Ctrl Pts',(1.43156508776869,2.2464658200996,13.8561100121513));
#425360=CARTESIAN_POINT('Ctrl Pts',(1.43177398088997,2.24621040761577,13.8562727473908));
#425361=CARTESIAN_POINT('Ctrl Pts',(1.43198855395975,2.24595602764911,13.8564289040185));
#425362=CARTESIAN_POINT('Ctrl Pts',(1.43296164038328,2.24480241740233,13.8571370725437));
#425363=CARTESIAN_POINT('Ctrl Pts',(1.43407038551572,2.24365123254706,13.8577210840554));
#425364=CARTESIAN_POINT('Ctrl Pts',(1.43529283041943,2.24256757874369,13.8581177131616));
#425365=CARTESIAN_POINT('Ctrl Pts',(1.4356371129796,2.24226238453443,13.8582294175695));
#425366=CARTESIAN_POINT('Ctrl Pts',(1.43599027239699,2.24196243949982,13.8583265086086));
#425367=CARTESIAN_POINT('Ctrl Pts',(1.43635148421128,2.24166891213396,13.8584082369006));
#425368=CARTESIAN_POINT('Ctrl Pts',(1.43687044872563,2.24124719202169,13.8585256585398));
#425369=CARTESIAN_POINT('Ctrl Pts',(1.43741269085242,2.24083372721456,13.8586122832068));
#425370=CARTESIAN_POINT('Ctrl Pts',(1.43796460353744,2.24043988628889,13.8586682984299));
#425371=CARTESIAN_POINT('Ctrl Pts',(1.43840607897612,2.24012485258855,13.8587131050557));
#425372=CARTESIAN_POINT('Ctrl Pts',(1.43885848193541,2.23981870464198,13.8587357943552));
#425373=CARTESIAN_POINT('Ctrl Pts',(1.43932215000997,2.2395218255036,13.8587355499465));
#425374=CARTESIAN_POINT('Ctrl Pts',(1.43962182974097,2.2393299454385,13.8587353919793));
#425375=CARTESIAN_POINT('Ctrl Pts',(1.4399229537499,2.23914397967128,13.8587257282814));
#425376=CARTESIAN_POINT('Ctrl Pts',(1.44022546638962,2.23896379393913,13.8587068136939));
#425377=CARTESIAN_POINT('Ctrl Pts',(1.44022546638962,2.23896379393913,13.8587068136939));
#425378=CARTESIAN_POINT('Ctrl Pts',(1.44122041396978,2.23837117288915,13.8586446046466));
#425379=CARTESIAN_POINT('Ctrl Pts',(1.44223036473579,2.2378409979402,13.858482427929));
#425380=CARTESIAN_POINT('Ctrl Pts',(1.44325351677486,2.23736917775172,13.8582284286032));
#425381=CARTESIAN_POINT('Ctrl Pts',(1.44430315174906,2.2368851451227,13.8579678548414));
#425382=CARTESIAN_POINT('Ctrl Pts',(1.4453698856064,2.23646273574583,13.857615680862));
#425383=CARTESIAN_POINT('Ctrl Pts',(1.44640809571661,2.23610959374242,13.8571944833187));
#425384=CARTESIAN_POINT('Ctrl Pts',(1.44899905522606,2.23522829175651,13.8561433417727));
#425385=CARTESIAN_POINT('Ctrl Pts',(1.45153202069412,2.23473262458468,13.8546163505474));
#425386=CARTESIAN_POINT('Ctrl Pts',(1.45384370716165,2.23449572265309,13.8528973491086));
#425387=CARTESIAN_POINT('Ctrl Pts',(1.45426601817352,2.23445244416535,13.8525833129072));
#425388=CARTESIAN_POINT('Ctrl Pts',(1.45468099640773,2.23441767033611,13.8522628768812));
#425389=CARTESIAN_POINT('Ctrl Pts',(1.45508773748325,2.23439047381699,13.851937733538));
#425390=CARTESIAN_POINT('Ctrl Pts',(1.45757164879865,2.23422438844806,13.8499521282529));
#425391=CARTESIAN_POINT('Ctrl Pts',(1.45999549168006,2.23432845282741,13.847639871647));
#425392=CARTESIAN_POINT('Ctrl Pts',(1.46223532404918,2.23461693096355,13.8452109780794));
#425393=CARTESIAN_POINT('Ctrl Pts',(1.46324307099428,2.2347467232482,13.8441181685877));
#425394=CARTESIAN_POINT('Ctrl Pts',(1.46421390117313,2.23491320990514,13.8430021611332));
#425395=CARTESIAN_POINT('Ctrl Pts',(1.46513889034174,2.23510626736355,13.8418824960098));
#425396=CARTESIAN_POINT('Ctrl Pts',(1.467318650938,2.23556121219418,13.8392439765549));
#425397=CARTESIAN_POINT('Ctrl Pts',(1.46934882122271,2.23618175613059,13.8364981347964));
#425398=CARTESIAN_POINT('Ctrl Pts',(1.47124477324504,2.23693681438127,13.8336931113419));
#425399=CARTESIAN_POINT('Ctrl Pts',(1.4730913101107,2.2376721931668,13.8309611966328));
#425400=CARTESIAN_POINT('Ctrl Pts',(1.47481217548998,2.23853642709544,13.8281701127186));
#425401=CARTESIAN_POINT('Ctrl Pts',(1.47639474334372,2.23952951831381,13.8253580685121));
#425402=CARTESIAN_POINT('Ctrl Pts',(1.47673784576237,2.23974482156173,13.8247484142933));
#425403=CARTESIAN_POINT('Ctrl Pts',(1.47707428962471,2.23996625191232,13.8241378483365));
#425404=CARTESIAN_POINT('Ctrl Pts',(1.47740364284705,2.24019390624622,13.8235269408515));
#425405=CARTESIAN_POINT('',(1.43917090325177,2.23962005108887,12.5969504640361));
#425406=CARTESIAN_POINT('Origin',(1.45787596860187,2.26849892500159,12.584524458991));
#425407=CARTESIAN_POINT('Origin',(1.45787596860187,2.26849892500159,12.584524458991));
#425408=CARTESIAN_POINT('Ctrl Pts',(1.42401639941738,2.27450380427705,12.5893111709658));
#425409=CARTESIAN_POINT('Ctrl Pts',(1.42202735742843,2.263345742325,12.5770542771492));
#425410=CARTESIAN_POINT('Ctrl Pts',(1.43732018478205,2.25752052933428,12.5737548217797));
#425411=CARTESIAN_POINT('Ctrl Pts',(1.42836576670489,2.29890274100932,12.5663937883685));
#425412=CARTESIAN_POINT('Ctrl Pts',(1.42637418741666,2.28773044539962,12.5540940315304));
#425413=CARTESIAN_POINT('Ctrl Pts',(1.44171554720094,2.28189018211084,12.5508374392248));
#425414=CARTESIAN_POINT('Ctrl Pts',(1.43271074553412,2.32327705951349,12.5434499600945));
#425415=CARTESIAN_POINT('Ctrl Pts',(1.43071269091247,2.31206843879219,12.5311293540532));
#425416=CARTESIAN_POINT('Ctrl Pts',(1.44610545412486,2.30623623464224,12.5278936106989));
#425417=CARTESIAN_POINT('Ctrl Pts',(1.43705167965902,2.34762868816916,12.5204817579905));
#425418=CARTESIAN_POINT('Ctrl Pts',(1.4350437360324,2.33636459243535,12.5081597038247));
#425419=CARTESIAN_POINT('Ctrl Pts',(1.45049031594202,2.33056052369087,12.5049254088044));
#425420=CARTESIAN_POINT('Ctrl Pts',(1.43393074758915,2.3301209866841,12.5369868989719));
#425421=CARTESIAN_POINT('Ctrl Pts',(1.43409422126029,2.33103803495414,12.5342545179733));
#425422=CARTESIAN_POINT('Ctrl Pts',(1.43437304314491,2.33189133177823,12.5314872231885));
#425423=CARTESIAN_POINT('Ctrl Pts',(1.43480464290327,2.33261544693394,12.5287124745063));
#425424=CARTESIAN_POINT('Ctrl Pts',(1.43519388098805,2.33326848992322,12.5262100684184));
#425425=CARTESIAN_POINT('Ctrl Pts',(1.43570783051915,2.33381530270399,12.5237004536639));
#425426=CARTESIAN_POINT('Ctrl Pts',(1.4364036198565,2.33421987379719,12.5212220730815));
#425427=CARTESIAN_POINT('Ctrl Pts',(1.43693630678483,2.33452960796722,12.5193246583486));
#425428=CARTESIAN_POINT('Ctrl Pts',(1.43758225949808,2.33475912423101,12.517417831369));
#425429=CARTESIAN_POINT('Ctrl Pts',(1.43839146993557,2.33482502697263,12.5155812248347));
#425430=CARTESIAN_POINT('Ctrl Pts',(1.43873619793146,2.33485310189479,12.5147988205793));
#425431=CARTESIAN_POINT('Ctrl Pts',(1.43911088149446,2.33485178874967,12.5140295443047));
#425432=CARTESIAN_POINT('Ctrl Pts',(1.43952043815593,2.33481648869479,12.5132817086137));
#425433=CARTESIAN_POINT('Ctrl Pts',(1.44014024675951,2.33476306683701,12.5121499604604));
#425434=CARTESIAN_POINT('Ctrl Pts',(1.44085269443909,2.33462352680435,12.5110494206568));
#425435=CARTESIAN_POINT('Ctrl Pts',(1.44166276356893,2.3343609623007,12.5100666561695));
#425436=CARTESIAN_POINT('Ctrl Pts',(1.44212790339786,2.33421019836734,12.5095023550641));
#425437=CARTESIAN_POINT('Ctrl Pts',(1.44263040231119,2.33401651001581,12.5089719619137));
#425438=CARTESIAN_POINT('Ctrl Pts',(1.44315854439662,2.33377756813051,12.5085043804652));
#425439=CARTESIAN_POINT('Ctrl Pts',(1.44393141154329,2.33342790780574,12.5078201359221));
#425440=CARTESIAN_POINT('Ctrl Pts',(1.44478111016828,2.33297009751822,12.5072563000949));
#425441=CARTESIAN_POINT('Ctrl Pts',(1.44564602760451,2.33242771701075,12.5068768744332));
#425442=CARTESIAN_POINT('Ctrl Pts',(1.44626969261716,2.33203662332726,12.5066032824114));
#425443=CARTESIAN_POINT('Ctrl Pts',(1.44691225926462,2.33159473813375,12.5064197834844));
#425444=CARTESIAN_POINT('Ctrl Pts',(1.44753930962537,2.33112886729074,12.5063282718343));
#425445=CARTESIAN_POINT('Ctrl Pts',(1.44845460902218,2.33044884008991,12.5061946931565));
#425446=CARTESIAN_POINT('Ctrl Pts',(1.44935704482965,2.32970402461386,12.5062515701262));
#425447=CARTESIAN_POINT('Ctrl Pts',(1.45020045406218,2.32895257236308,12.5064436508398));
#425448=CARTESIAN_POINT('',(1.43732018478205,2.25752052933428,12.5737548217797));
#425449=CARTESIAN_POINT('Origin',(1.44567497038565,2.27064293603114,12.5893111709658));
#425450=CARTESIAN_POINT('Ctrl Pts',(1.45020045406218,2.32895257236308,12.5064436508398));
#425451=CARTESIAN_POINT('Ctrl Pts',(1.448294312388,2.31837868889157,12.5164271754438));
#425452=CARTESIAN_POINT('Ctrl Pts',(1.44638720949835,2.30780065100219,12.5264061185523));
#425453=CARTESIAN_POINT('Ctrl Pts',(1.4444791124715,2.29721831221191,12.536380305637));
#425454=CARTESIAN_POINT('Ctrl Pts',(1.44209437819172,2.28399253505363,12.5488460165097));
#425455=CARTESIAN_POINT('Ctrl Pts',(1.43970809034824,2.27076003601564,12.5613043021964));
#425456=CARTESIAN_POINT('Ctrl Pts',(1.43732018478205,2.25752052933428,12.5737548217797));
#425457=CARTESIAN_POINT('Ctrl Pts',(1.47740364284705,2.24019390624622,12.5893111709658));
#425458=CARTESIAN_POINT('Ctrl Pts',(1.46808019059302,2.23374938356208,12.5770542771492));
#425459=CARTESIAN_POINT('Ctrl Pts',(1.45642852040297,2.24524034769209,12.5737548217797));
#425460=CARTESIAN_POINT('Ctrl Pts',(1.46870494298515,2.23418122263341,12.5928319619712));
#425461=CARTESIAN_POINT('Ctrl Pts',(1.46058664508617,2.23252996384242,12.5821634970842));
#425462=CARTESIAN_POINT('Ctrl Pts',(1.45326516155529,2.24304230807227,12.5773203894503));
#425463=CARTESIAN_POINT('Ctrl Pts',(1.45220884841342,2.23127210537548,12.5969440695591));
#425464=CARTESIAN_POINT('Ctrl Pts',(1.44881735875055,2.23342996088931,12.5878292599214));
#425465=CARTESIAN_POINT('Ctrl Pts',(1.44738526150745,2.24200745420583,12.5813877129824));
#425466=CARTESIAN_POINT('Ctrl Pts',(1.42643991651343,2.24776869272787,12.596957478804));
#425467=CARTESIAN_POINT('Ctrl Pts',(1.42980638518812,2.24562685197486,12.5878468778671));
#425468=CARTESIAN_POINT('Ctrl Pts',(1.43816541970709,2.24791683534776,12.5814011370086));
#425469=CARTESIAN_POINT('Ctrl Pts',(1.42215794598272,2.2640783136773,12.5928371701607));
#425470=CARTESIAN_POINT('Ctrl Pts',(1.42403293196948,2.25601484709938,12.5821692192952));
#425471=CARTESIAN_POINT('Ctrl Pts',(1.43663244289462,2.25371786072261,12.5773318885715));
#425472=CARTESIAN_POINT('Ctrl Pts',(1.42401639941733,2.27450380427706,12.5893111709658));
#425473=CARTESIAN_POINT('Ctrl Pts',(1.42202735742837,2.26334574232501,12.5770542771492));
#425474=CARTESIAN_POINT('Ctrl Pts',(1.437320184782,2.25752052933429,12.5737548217797));
#425475=CARTESIAN_POINT('',(1.45642852040297,2.24524034769209,12.5737548217797));
#425476=CARTESIAN_POINT('Origin',(1.46489437802034,2.25829137274004,12.5893111709658));
#425477=CARTESIAN_POINT('Ctrl Pts',(1.437320184782,2.25752052933429,12.5737548217797));
#425478=CARTESIAN_POINT('Ctrl Pts',(1.43711222700909,2.25654018592726,12.5746934679442));
#425479=CARTESIAN_POINT('Ctrl Pts',(1.43706130478103,2.2554173580843,12.5756680099006));
#425480=CARTESIAN_POINT('Ctrl Pts',(1.43716988501508,2.25427994259259,12.5765688348656));
#425481=CARTESIAN_POINT('Ctrl Pts',(1.43719863043003,2.25397882443277,12.5768073183026));
#425482=CARTESIAN_POINT('Ctrl Pts',(1.43723830068214,2.2536767224611,12.5770407398754));
#425483=CARTESIAN_POINT('Ctrl Pts',(1.43728838139006,2.25337595167529,12.5772674179684));
#425484=CARTESIAN_POINT('Ctrl Pts',(1.43749389907298,2.25214166970218,12.5781976435658));
#425485=CARTESIAN_POINT('Ctrl Pts',(1.43789753469957,2.25086155417469,12.5790594849312));
#425486=CARTESIAN_POINT('Ctrl Pts',(1.43851808819857,2.24963656189775,12.5797571720116));
#425487=CARTESIAN_POINT('Ctrl Pts',(1.43892240111627,2.24883843538253,12.580211740231));
#425488=CARTESIAN_POINT('Ctrl Pts',(1.43945391611847,2.24803592134354,12.5806009430798));
#425489=CARTESIAN_POINT('Ctrl Pts',(1.44008998765969,2.24729529616251,12.5808812374708));
#425490=CARTESIAN_POINT('Ctrl Pts',(1.44063658412813,2.24665885343216,12.5811221033394));
#425491=CARTESIAN_POINT('Ctrl Pts',(1.44127166735258,2.24605515727454,12.581287365893));
#425492=CARTESIAN_POINT('Ctrl Pts',(1.44196513682819,2.24552432456091,12.581359338449));
#425493=CARTESIAN_POINT('Ctrl Pts',(1.4420615147657,2.24545054977499,12.5813693411482));
#425494=CARTESIAN_POINT('Ctrl Pts',(1.44215900198069,2.24537812540706,12.5813775999465));
#425495=CARTESIAN_POINT('Ctrl Pts',(1.44225749978775,2.24530710046997,12.5813841266931));
#425496=CARTESIAN_POINT('Ctrl Pts',(1.4424246132305,2.24518659807391,12.5813952001081));
#425497=CARTESIAN_POINT('Ctrl Pts',(1.44259611104936,2.24506981077049,12.5814007534795));
#425498=CARTESIAN_POINT('Ctrl Pts',(1.44277202955414,2.24495695242778,12.5814005856065));
#425499=CARTESIAN_POINT('Ctrl Pts',(1.44357731568938,2.24444033105959,12.5813998171494));
#425500=CARTESIAN_POINT('Ctrl Pts',(1.44441941378067,2.24404144961688,12.58127954464));
#425501=CARTESIAN_POINT('Ctrl Pts',(1.44528087632854,2.24373583157791,12.5810700125799));
#425502=CARTESIAN_POINT('Ctrl Pts',(1.446321425001,2.24336667978424,12.5808169217085));
#425503=CARTESIAN_POINT('Ctrl Pts',(1.44739591594597,2.24314933772975,12.5804173076348));
#425504=CARTESIAN_POINT('Ctrl Pts',(1.44840501945573,2.24307732749274,12.5799304713245));
#425505=CARTESIAN_POINT('Ctrl Pts',(1.44965561660472,2.24298808412352,12.5793271277669));
#425506=CARTESIAN_POINT('Ctrl Pts',(1.45088106989178,2.24308440156553,12.5785808224116));
#425507=CARTESIAN_POINT('Ctrl Pts',(1.45203220930258,2.24333060050925,12.5777485681082));
#425508=CARTESIAN_POINT('Ctrl Pts',(1.45374753314142,2.2436974639085,12.576508418016));
#425509=CARTESIAN_POINT('Ctrl Pts',(1.45528484238996,2.24438731881001,12.5750928681475));
#425510=CARTESIAN_POINT('Ctrl Pts',(1.45642852040297,2.24524034769209,12.5737548217797));
#425511=CARTESIAN_POINT('Ctrl Pts',(1.45642852040297,2.24524034769209,12.5737548217797));
#425512=CARTESIAN_POINT('Ctrl Pts',(1.46808019059302,2.23374938356208,12.5770542771492));
#425513=CARTESIAN_POINT('Ctrl Pts',(1.47740364284705,2.24019390624622,12.5893111709658));
#425514=CARTESIAN_POINT('Ctrl Pts',(1.47676698075747,2.25935990804567,12.5508408821982));
#425515=CARTESIAN_POINT('Ctrl Pts',(1.48845249442907,2.24783105316495,12.55409748406));
#425516=CARTESIAN_POINT('Ctrl Pts',(1.49778784102034,2.25428379740954,12.5663972313419));
#425517=CARTESIAN_POINT('Ctrl Pts',(1.49708624564732,2.27346470645356,12.52790050457));
#425518=CARTESIAN_POINT('Ctrl Pts',(1.50878578045427,2.26188575301888,12.5311362602938));
#425519=CARTESIAN_POINT('Ctrl Pts',(1.51815147488721,2.26835947418794,12.5434568539655));
#425520=CARTESIAN_POINT('Ctrl Pts',(1.51738781470373,2.28755587873285,12.5049357605811));
#425521=CARTESIAN_POINT('Ctrl Pts',(1.529084116076,2.27591629458227,12.5081700652078));
#425522=CARTESIAN_POINT('Ctrl Pts',(1.53849615504836,2.28242204985496,12.5204921097672));
#425523=CARTESIAN_POINT('Ctrl Pts',(1.51605473500476,2.28663059582145,12.5064436508395));
#425524=CARTESIAN_POINT('Ctrl Pts',(1.51717154464663,2.28613908385374,12.5062361689309));
#425525=CARTESIAN_POINT('Ctrl Pts',(1.51831197612063,2.28558032838526,12.5061871075061));
#425526=CARTESIAN_POINT('Ctrl Pts',(1.51938369601753,2.28497830421322,12.5063648335164));
#425527=CARTESIAN_POINT('Ctrl Pts',(1.51987053730112,2.28470482769989,12.5064455676329));
#425528=CARTESIAN_POINT('Ctrl Pts',(1.52034988222133,2.28441841601867,12.506574497099));
#425529=CARTESIAN_POINT('Ctrl Pts',(1.52080063885185,2.28413044747091,12.5067492519495));
#425530=CARTESIAN_POINT('Ctrl Pts',(1.52170645179803,2.28355176349601,12.5071004286051));
#425531=CARTESIAN_POINT('Ctrl Pts',(1.52252968659954,2.28294483530112,12.5076537929613));
#425532=CARTESIAN_POINT('Ctrl Pts',(1.52321416791145,2.28236282913274,12.5083435010505));
#425533=CARTESIAN_POINT('Ctrl Pts',(1.5232572601005,2.28232618836636,12.5083869222964));
#425534=CARTESIAN_POINT('Ctrl Pts',(1.52329979931455,2.28228963328919,12.5084308732337));
#425535=CARTESIAN_POINT('Ctrl Pts',(1.52334177068723,2.28225317174875,12.5084753333615));
#425536=CARTESIAN_POINT('Ctrl Pts',(1.52367843649331,2.28196070206952,12.5088319622689));
#425537=CARTESIAN_POINT('Ctrl Pts',(1.52398624742104,2.28166928698463,12.509227847131));
#425538=CARTESIAN_POINT('Ctrl Pts',(1.52425797568876,2.28138962513347,12.5096423454524));
#425539=CARTESIAN_POINT('Ctrl Pts',(1.5251094518179,2.28051328866509,12.5109411997424));
#425540=CARTESIAN_POINT('Ctrl Pts',(1.52566593136802,2.27970519671489,12.5124831113042));
#425541=CARTESIAN_POINT('Ctrl Pts',(1.5260203540851,2.27898318354805,12.5140723025008));
#425542=CARTESIAN_POINT('Ctrl Pts',(1.52605356388188,2.27891553012351,12.5142212114565));
#425543=CARTESIAN_POINT('Ctrl Pts',(1.52608502882357,2.2788486274628,12.5143705582413));
#425544=CARTESIAN_POINT('Ctrl Pts',(1.52611484230059,2.27878248890665,12.5145201959299));
#425545=CARTESIAN_POINT('Ctrl Pts',(1.52649784080049,2.27793284068288,12.5164425148273));
#425546=CARTESIAN_POINT('Ctrl Pts',(1.52663120684895,2.2771845952175,12.5184635205941));
#425547=CARTESIAN_POINT('Ctrl Pts',(1.52659945261675,2.27650619824704,12.5205025929157));
#425548=CARTESIAN_POINT('Ctrl Pts',(1.52658103390345,2.27611270111503,12.5216853356836));
#425549=CARTESIAN_POINT('Ctrl Pts',(1.52650757743367,2.27574339243439,12.5228750347131));
#425550=CARTESIAN_POINT('Ctrl Pts',(1.52639732288665,2.27539777446118,12.5240609649613));
#425551=CARTESIAN_POINT('Ctrl Pts',(1.52612670901593,2.27454947368767,12.5269717671327));
#425552=CARTESIAN_POINT('Ctrl Pts',(1.52561689206398,2.27382317783633,12.5299036066169));
#425553=CARTESIAN_POINT('Ctrl Pts',(1.52494588207629,2.27318115157318,12.5328133004019));
#425554=CARTESIAN_POINT('Ctrl Pts',(1.52462375821045,2.2728729415828,12.5342101228451));
#425555=CARTESIAN_POINT('Ctrl Pts',(1.52426452606594,2.27258491524197,12.5356023438238));
#425556=CARTESIAN_POINT('Ctrl Pts',(1.52387624238129,2.2723165271091,12.5369868989719));
#425557=CARTESIAN_POINT('Origin',(12.0106235946827,9.5144905286836,-1.23909490405968));
#425558=CARTESIAN_POINT('Ctrl Pts',(1.43392337386552,2.33007984802669,12.5369868989719));
#425559=CARTESIAN_POINT('Ctrl Pts',(1.43664395014642,2.34517560134957,12.5369868989719));
#425560=CARTESIAN_POINT('Ctrl Pts',(1.42342012354076,2.35294822726294,12.5369868989719));
#425561=CARTESIAN_POINT('Ctrl Pts',(1.43484296988741,2.33518281478483,12.5218025310016));
#425562=CARTESIAN_POINT('Ctrl Pts',(1.43359076658335,2.34693389348384,12.5216901060418));
#425563=CARTESIAN_POINT('Ctrl Pts',(1.4234604425035,2.35292454794093,12.5161920673678));
#425564=CARTESIAN_POINT('Ctrl Pts',(1.44028510659882,2.33777496046166,12.5042015548894));
#425565=CARTESIAN_POINT('Ctrl Pts',(1.43842689613838,2.34393323935284,12.4980677368514));
#425566=CARTESIAN_POINT('Ctrl Pts',(1.43263111333136,2.34748284234156,12.4907278922777));
#425567=CARTESIAN_POINT('Ctrl Pts',(1.4501898818154,2.32893559382066,12.506463626192));
#425568=CARTESIAN_POINT('Ctrl Pts',(1.45364827026581,2.33448960027209,12.4999376786891));
#425569=CARTESIAN_POINT('Ctrl Pts',(1.45360603107938,2.3344217661588,12.4906970594712));
#425570=CARTESIAN_POINT('Origin',(1.41227217662088,2.33398185493001,12.5369868989719));
#425571=CARTESIAN_POINT('Origin',(1.41227217662088,2.33398185493001,14.));
#425572=CARTESIAN_POINT('Origin',(1.41227217662088,2.33398185493001,13.7435492065112));
#425573=CARTESIAN_POINT('Ctrl Pts',(1.42958547089512,2.30574515194253,13.793642941384));
#425574=CARTESIAN_POINT('Ctrl Pts',(1.43150976134211,2.31638485707385,13.8071662555867));
#425575=CARTESIAN_POINT('Ctrl Pts',(1.41537940665151,2.32184663711247,13.8103758687955));
#425576=CARTESIAN_POINT('Ctrl Pts',(1.43250238123844,2.32210832215104,13.7804579775005));
#425577=CARTESIAN_POINT('Ctrl Pts',(1.43486680281184,2.33523856138542,13.7901904343351));
#425578=CARTESIAN_POINT('Ctrl Pts',(1.42095719017033,2.34263981805758,13.7927914348262));
#425579=CARTESIAN_POINT('Ctrl Pts',(1.43421967609579,2.33174193627479,13.7597120340895));
#425580=CARTESIAN_POINT('Ctrl Pts',(1.43695033803418,2.34693833635346,13.7635825532446));
#425581=CARTESIAN_POINT('Ctrl Pts',(1.42422171320313,2.35490815605373,13.7651073818884));
#425582=CARTESIAN_POINT('Ctrl Pts',(1.43388339044034,2.32985545404484,13.7381884353898));
#425583=CARTESIAN_POINT('Ctrl Pts',(1.43655102081185,2.34469599510058,13.7368803041981));
#425584=CARTESIAN_POINT('Ctrl Pts',(1.42358194497715,2.35250577801131,13.7363986145813));
#425585=CARTESIAN_POINT('Origin',(1.40863470903346,2.31357650958568,13.7902182540695));
#425586=CARTESIAN_POINT('Ctrl Pts',(1.42401570789099,2.27449992929967,13.8235227101244));
#425587=CARTESIAN_POINT('Ctrl Pts',(1.42603773982375,2.28581779460998,13.8358800583119));
#425588=CARTESIAN_POINT('Ctrl Pts',(1.41051208250141,2.2916126210755,13.8390832900376));
#425589=CARTESIAN_POINT('Ctrl Pts',(1.42610892663473,2.28624239857086,13.8124254819053));
#425590=CARTESIAN_POINT('Ctrl Pts',(1.42813488505102,2.2975822430641,13.8247886449157));
#425591=CARTESIAN_POINT('Ctrl Pts',(1.4125836503793,2.30336842326239,13.8279860620657));
#425592=CARTESIAN_POINT('Ctrl Pts',(1.42820120726595,2.29797960524938,13.8013225099955));
#425593=CARTESIAN_POINT('Ctrl Pts',(1.43023013821212,2.30933607798735,13.8136962257787));
#425594=CARTESIAN_POINT('Ctrl Pts',(1.4146545261664,2.31511873605116,13.8168830918626));
#425595=CARTESIAN_POINT('Ctrl Pts',(1.43029258628516,2.30971175409457,13.7902140179785));
#425596=CARTESIAN_POINT('Ctrl Pts',(1.43232359815253,2.32107985386274,13.802602731458));
#425597=CARTESIAN_POINT('Ctrl Pts',(1.41672473886898,2.32686377481425,13.8057746032558));
#425598=CARTESIAN_POINT('Origin',(1.40235782844911,2.27836467252297,13.8235269408515));
#425599=CARTESIAN_POINT('Ctrl Pts',(1.47740364284705,2.24019390624622,13.8235269408515));
#425600=CARTESIAN_POINT('Ctrl Pts',(1.48711662013691,2.24690767500585,13.8362179249168));
#425601=CARTESIAN_POINT('Ctrl Pts',(1.49897171578034,2.23461459925801,13.8391868794938));
#425602=CARTESIAN_POINT('Ctrl Pts',(1.46851669140757,2.23405110006411,13.8400110824519));
#425603=CARTESIAN_POINT('Ctrl Pts',(1.4782493131047,2.23661974518589,13.8494522556836));
#425604=CARTESIAN_POINT('Ctrl Pts',(1.48428241609783,2.2245977006131,13.85569149686));
#425605=CARTESIAN_POINT('Ctrl Pts',(1.45249782979392,2.2310856660912,13.8586819406588));
#425606=CARTESIAN_POINT('Ctrl Pts',(1.45616802538609,2.22874350726861,13.868010383617));
#425607=CARTESIAN_POINT('Ctrl Pts',(1.45766421139961,2.21981858182324,13.8744918421245));
#425608=CARTESIAN_POINT('Ctrl Pts',(1.42614644312893,2.24795800791975,13.8587686893867));
#425609=CARTESIAN_POINT('Ctrl Pts',(1.4225088819522,2.25027927408403,13.8680909899357));
#425610=CARTESIAN_POINT('Ctrl Pts',(1.41379827847105,2.24790824297923,13.8745789365163));
#425611=CARTESIAN_POINT('Ctrl Pts',(1.4221173943012,2.26385082823282,13.8400379222776));
#425612=CARTESIAN_POINT('Ctrl Pts',(1.42040421962509,2.27376724222361,13.8494748685453));
#425613=CARTESIAN_POINT('Ctrl Pts',(1.40696857994555,2.27426190540908,13.8557104837033));
#425614=CARTESIAN_POINT('Ctrl Pts',(1.42401639941085,2.27450380427807,13.8235269408542));
#425615=CARTESIAN_POINT('Ctrl Pts',(1.42608854169682,2.28612803952764,13.8362179249195));
#425616=CARTESIAN_POINT('Ctrl Pts',(1.40998158196441,2.2918050856112,13.8391868794965));
#425617=CARTESIAN_POINT('Origin',(1.48991290767377,2.2220964397524,13.8235269408515));
#425618=CARTESIAN_POINT('Ctrl Pts',(1.50682270298796,2.26052884084395,13.7902140241682));
#425619=CARTESIAN_POINT('Ctrl Pts',(1.51631977736859,2.26709878556223,13.8026027327198));
#425620=CARTESIAN_POINT('Ctrl Pts',(1.5280610125852,2.25531229635374,13.8057746032556));
#425621=CARTESIAN_POINT('Ctrl Pts',(1.4970195552633,2.25375274480634,13.8013225161808));
#425622=CARTESIAN_POINT('Ctrl Pts',(1.50650691776783,2.26031596662135,13.8136962270464));
#425623=CARTESIAN_POINT('Ctrl Pts',(1.51823734697599,2.24855009921154,13.8168830918628));
#425624=CARTESIAN_POINT('Ctrl Pts',(1.48721218131346,2.24697372753278,13.8124254880875));
#425625=CARTESIAN_POINT('Ctrl Pts',(1.49668565306825,2.25352733783179,13.8247886461867));
#425626=CARTESIAN_POINT('Ctrl Pts',(1.50840915940023,2.24178510799748,13.8279860620656));
#425627=CARTESIAN_POINT('Ctrl Pts',(1.47740041004428,2.24019167076019,13.8235227163065));
#425628=CARTESIAN_POINT('Ctrl Pts',(1.48685551995534,2.24673257893923,13.8358800595847));
#425629=CARTESIAN_POINT('Ctrl Pts',(1.49857626599681,2.23501720685682,13.8390832900376));
#425630=CARTESIAN_POINT('Origin',(1.51933521085166,2.24243361691417,13.7902182540695));
#425631=CARTESIAN_POINT('Ctrl Pts',(1.52365426804161,2.27216306128232,13.7382347919292));
#425632=CARTESIAN_POINT('Ctrl Pts',(1.53605408873942,2.28076319589732,13.7369371795942));
#425633=CARTESIAN_POINT('Ctrl Pts',(1.54855062958131,2.27219696895615,13.7364597369711));
#425634=CARTESIAN_POINT('Ctrl Pts',(1.52521028684062,2.27323860741397,13.7595490285574));
#425635=CARTESIAN_POINT('Ctrl Pts',(1.53790652963333,2.28204310770456,13.7633824266926));
#425636=CARTESIAN_POINT('Ctrl Pts',(1.55044638650451,2.27375784066251,13.7648920890506));
#425637=CARTESIAN_POINT('Ctrl Pts',(1.51727467620672,2.2677533810723,13.780380659011));
#425638=CARTESIAN_POINT('Ctrl Pts',(1.52825339544785,2.27537339484063,13.7901039518744));
#425639=CARTESIAN_POINT('Ctrl Pts',(1.54077925076494,2.26580321250166,13.7926933640892));
#425640=CARTESIAN_POINT('Ctrl Pts',(1.50348081351774,2.25821883317055,13.7936647693663));
#425641=CARTESIAN_POINT('Ctrl Pts',(1.51236063256899,2.26439314653818,13.8072068914933));
#425642=CARTESIAN_POINT('Ctrl Pts',(1.52403450784357,2.25196877911278,13.8104111085397));
#425643=CARTESIAN_POINT('Origin',(1.53638550720801,2.25421906061527,13.7435492065112));
#425644=CARTESIAN_POINT('Origin',(1.53638550720801,2.25421906061527,14.));
#425645=CARTESIAN_POINT('Origin',(1.53638550720801,2.25421906061527,12.5369868989719));
#425646=CARTESIAN_POINT('Ctrl Pts',(1.51604457665074,2.28661527422765,12.506462012331));
#425647=CARTESIAN_POINT('Ctrl Pts',(1.51965773737332,2.29206492170091,12.4999388158272));
#425648=CARTESIAN_POINT('Ctrl Pts',(1.5196149889436,2.29200044522452,12.4907030323752));
#425649=CARTESIAN_POINT('Ctrl Pts',(1.52819857315075,2.28127589671409,12.5042014951932));
#425650=CARTESIAN_POINT('Ctrl Pts',(1.534569347831,2.28214441677112,12.4980716682127));
#425651=CARTESIAN_POINT('Ctrl Pts',(1.54020273176299,2.27835092883773,12.4907355092743));
#425652=CARTESIAN_POINT('Ctrl Pts',(1.52810378184397,2.27524956152149,12.5218047446509));
#425653=CARTESIAN_POINT('Ctrl Pts',(1.53930797999379,2.27898918914412,12.5216906929434));
#425654=CARTESIAN_POINT('Ctrl Pts',(1.54896278474319,2.27226940495258,12.5161988840776));
#425655=CARTESIAN_POINT('Ctrl Pts',(1.52384465989328,2.27229465600322,12.5369868989719));
#425656=CARTESIAN_POINT('Ctrl Pts',(1.53643997313891,2.28103328379968,12.5369868989719));
#425657=CARTESIAN_POINT('Ctrl Pts',(1.54899968222163,2.27224356029559,12.5369868989719));
#425658=CARTESIAN_POINT('Origin',(2.78530720815102E-31,-8.17839987285318E-32,
12.5));
#425659=CARTESIAN_POINT('Origin',(1.65508430440733,2.11231773338789,12.5));
#425660=CARTESIAN_POINT('',(1.65508430440733,2.11231773338789,12.5893111709658));
#425661=CARTESIAN_POINT('',(1.65508430440733,2.11231773338789,13.8235269408515));
#425662=CARTESIAN_POINT('',(1.65508430440733,2.11231773338789,12.5));
#425663=CARTESIAN_POINT('',(1.68606637603839,2.13018904941803,13.7902182540695));
#425664=CARTESIAN_POINT('',(1.65508430440733,2.11231773338789,13.8235269408515));
#425665=CARTESIAN_POINT('',(1.70402056201252,2.14054552058717,13.7435492065112));
#425666=CARTESIAN_POINT('Origin',(1.64495136471449,2.10647314951159,13.7445212918719));
#425667=CARTESIAN_POINT('',(1.70402056201252,2.14054552058717,12.5369868989719));
#425668=CARTESIAN_POINT('',(1.70402056201252,2.14054552058717,12.5));
#425669=CARTESIAN_POINT('Ctrl Pts',(1.70402056201252,2.14054552058717,12.5369868989719));
#425670=CARTESIAN_POINT('Ctrl Pts',(1.68772037318743,2.13114312073112,12.5544431401645));
#425671=CARTESIAN_POINT('Ctrl Pts',(1.67140852603406,2.12173399602879,12.5718848856037));
#425672=CARTESIAN_POINT('Ctrl Pts',(1.65508430440733,2.11231773338789,12.5893111709658));
#425673=CARTESIAN_POINT('Origin',(1.67483872942809,2.41676261471951,12.5));
#425674=CARTESIAN_POINT('',(1.6190859535201,2.20548903343026,13.7435492065112));
#425675=CARTESIAN_POINT('',(1.61379736422647,2.18544807256622,13.7902182540695));
#425676=CARTESIAN_POINT('Origin',(1.59989986561444,2.13278389118854,13.7418732680441));
#425677=CARTESIAN_POINT('',(1.6046712778331,2.1508650240259,13.8235269408515));
#425678=CARTESIAN_POINT('',(1.61379736422647,2.18544807256622,13.7902182540695));
#425679=CARTESIAN_POINT('',(1.6046712778331,2.1508650240259,12.5893111709658));
#425680=CARTESIAN_POINT('',(1.6046712778331,2.1508650240259,12.5));
#425681=CARTESIAN_POINT('',(1.6190859535201,2.20548903343026,12.5369868989719));
#425682=CARTESIAN_POINT('Ctrl Pts',(1.6046712778331,2.1508650240259,12.5893111709658));
#425683=CARTESIAN_POINT('Ctrl Pts',(1.60947974444063,2.16908657343108,12.5718848856037));
#425684=CARTESIAN_POINT('Ctrl Pts',(1.61428456602034,2.18729431010553,12.5544431401645));
#425685=CARTESIAN_POINT('Ctrl Pts',(1.6190859535201,2.20548903343026,12.5369868989719));
#425686=CARTESIAN_POINT('',(1.6190859535201,2.20548903343026,12.5));
#425687=CARTESIAN_POINT('Origin',(1.6379084766698,2.14209409257653,12.5));
#425688=CARTESIAN_POINT('',(1.61792956969214,2.11412208070473,13.8587068136939));
#425689=CARTESIAN_POINT('Ctrl Pts',(1.60467127782667,2.15086502402745,13.8235269408542));
#425690=CARTESIAN_POINT('Ctrl Pts',(1.60422417125196,2.14917072619708,13.8262006681044));
#425691=CARTESIAN_POINT('Ctrl Pts',(1.60393461161577,2.14739252956872,13.8288634856214));
#425692=CARTESIAN_POINT('Ctrl Pts',(1.60379158668926,2.14553795324233,13.8314912288862));
#425693=CARTESIAN_POINT('Ctrl Pts',(1.60364414274236,2.1436260763405,13.8342001611531));
#425694=CARTESIAN_POINT('Ctrl Pts',(1.60365176912644,2.14163094162529,13.8368750301949));
#425695=CARTESIAN_POINT('Ctrl Pts',(1.60384146006204,2.1395380377893,13.8394886372969));
#425696=CARTESIAN_POINT('Ctrl Pts',(1.60385611035312,2.13937639774937,13.8396904925131));
#425697=CARTESIAN_POINT('Ctrl Pts',(1.60387186870404,2.13921417270046,13.8398919674349));
#425698=CARTESIAN_POINT('Ctrl Pts',(1.60388875899436,2.13905135601658,13.8400930404591));
#425699=CARTESIAN_POINT('Ctrl Pts',(1.60415192108076,2.13651456254395,13.8432258934518));
#425700=CARTESIAN_POINT('Ctrl Pts',(1.60468740747428,2.13384697351913,13.8462331177034));
#425701=CARTESIAN_POINT('Ctrl Pts',(1.60557233302992,2.13115457704674,13.8489036603661));
#425702=CARTESIAN_POINT('Ctrl Pts',(1.60586189097013,2.13027359358798,13.8497774930041));
#425703=CARTESIAN_POINT('Ctrl Pts',(1.60618892724341,2.12939019546001,13.85061494757));
#425704=CARTESIAN_POINT('Ctrl Pts',(1.60655631689504,2.12850878830696,13.8514076489583));
#425705=CARTESIAN_POINT('Ctrl Pts',(1.60733339899377,2.12664448506031,13.8530843267192));
#425706=CARTESIAN_POINT('Ctrl Pts',(1.60837007562625,2.12460710348909,13.8546805203176));
#425707=CARTESIAN_POINT('Ctrl Pts',(1.60972778676256,2.12257677018939,13.8559412814273));
#425708=CARTESIAN_POINT('Ctrl Pts',(1.60990949254421,2.12230504574861,13.8561100121513));
#425709=CARTESIAN_POINT('Ctrl Pts',(1.61009687210231,2.12203345640009,13.8562727473908));
#425710=CARTESIAN_POINT('Ctrl Pts',(1.61028999686907,2.12176243316459,13.8564289040185));
#425711=CARTESIAN_POINT('Ctrl Pts',(1.61116581548311,2.12053334588351,13.8571370725437));
#425712=CARTESIAN_POINT('Ctrl Pts',(1.6121770391048,2.11929561847949,13.8577210840554));
#425713=CARTESIAN_POINT('Ctrl Pts',(1.61330708857883,2.11811592983647,13.8581177131616));
#425714=CARTESIAN_POINT('Ctrl Pts',(1.61362534940583,2.11778368891096,13.8582294175695));
#425715=CARTESIAN_POINT('Ctrl Pts',(1.61395288540951,2.11745595614763,13.8583265086086));
#425716=CARTESIAN_POINT('Ctrl Pts',(1.61428897011599,2.11713396335368,13.8584082369006));
#425717=CARTESIAN_POINT('Ctrl Pts',(1.61477183371452,2.11667134605454,13.8585256585398));
#425718=CARTESIAN_POINT('Ctrl Pts',(1.61527857035516,2.11621505925019,13.8586122832068));
#425719=CARTESIAN_POINT('Ctrl Pts',(1.61579654490457,2.11577754279017,13.8586682984299));
#425720=CARTESIAN_POINT('Ctrl Pts',(1.61621087319893,2.11542757299177,13.8587131050557));
#425721=CARTESIAN_POINT('Ctrl Pts',(1.61663681692492,2.11508556868615,13.8587357943552));
#425722=CARTESIAN_POINT('Ctrl Pts',(1.61707474377634,2.11475188413605,13.8587355499465));
#425723=CARTESIAN_POINT('Ctrl Pts',(1.61735778634109,2.1145362158559,13.8587353919793));
#425724=CARTESIAN_POINT('Ctrl Pts',(1.61764275044824,2.11432632447222,13.8587257282814));
#425725=CARTESIAN_POINT('Ctrl Pts',(1.61792956969214,2.11412208070473,13.8587068136939));
#425726=CARTESIAN_POINT('Ctrl Pts',(1.61792956969214,2.11412208070473,13.8587068136939));
#425727=CARTESIAN_POINT('Ctrl Pts',(1.61887290254913,2.11345033408795,13.8586446046466));
#425728=CARTESIAN_POINT('Ctrl Pts',(1.61983627860707,2.11283960288903,13.858482427929));
#425729=CARTESIAN_POINT('Ctrl Pts',(1.62081756846665,2.11228595625362,13.8582284286032));
#425730=CARTESIAN_POINT('Ctrl Pts',(1.62182425771426,2.11171797920851,13.8579678548414));
#425731=CARTESIAN_POINT('Ctrl Pts',(1.62285301181702,2.11121002665154,13.857615680862));
#425732=CARTESIAN_POINT('Ctrl Pts',(1.62385898301704,2.11077343593676,13.8571944833187));
#425733=CARTESIAN_POINT('Ctrl Pts',(1.62636948702899,2.1096838791572,13.8561433417727));
#425734=CARTESIAN_POINT('Ctrl Pts',(1.62885362278733,2.10898340107645,13.8546163505475));
#425735=CARTESIAN_POINT('Ctrl Pts',(1.63113830760212,2.10855886350875,13.8528973491086));
#425736=CARTESIAN_POINT('Ctrl Pts',(1.63155568581042,2.10848130675859,13.8525833129073));
#425737=CARTESIAN_POINT('Ctrl Pts',(1.6319664488489,2.10841282405783,13.8522628768812));
#425738=CARTESIAN_POINT('Ctrl Pts',(1.63236961975827,2.10835256485923,13.851937733538));
#425739=CARTESIAN_POINT('Ctrl Pts',(1.63483172856425,2.10798457029395,13.8499521282529));
#425740=CARTESIAN_POINT('Ctrl Pts',(1.63725598852144,2.10789072271098,13.847639871647));
#425741=CARTESIAN_POINT('Ctrl Pts',(1.63951188167932,2.10799567382824,13.8452109780794));
#425742=CARTESIAN_POINT('Ctrl Pts',(1.64052685470572,2.10804289350828,13.8441181685877));
#425743=CARTESIAN_POINT('Ctrl Pts',(1.64150802473536,2.10812969452228,13.8430021611332));
#425744=CARTESIAN_POINT('Ctrl Pts',(1.64244567205393,2.10824671439349,13.8418824960098));
#425745=CARTESIAN_POINT('Ctrl Pts',(1.64465526190383,2.10852247470822,13.8392439765549));
#425746=CARTESIAN_POINT('Ctrl Pts',(1.64672925705608,2.1089754761105,13.8364981347964));
#425747=CARTESIAN_POINT('Ctrl Pts',(1.64868044471151,2.10957348427616,13.8336931113419));
#425748=CARTESIAN_POINT('Ctrl Pts',(1.65058077757604,2.11015590625249,13.8309611966327));
#425749=CARTESIAN_POINT('Ctrl Pts',(1.65236636000607,2.11087699800988,13.8281701127185));
#425750=CARTESIAN_POINT('Ctrl Pts',(1.65402460814955,2.11173779082723,13.825358068512));
#425751=CARTESIAN_POINT('Ctrl Pts',(1.65438411813667,2.11192441163902,13.8247484142932));
#425752=CARTESIAN_POINT('Ctrl Pts',(1.65473749113902,2.11211768190021,13.8241378483365));
#425753=CARTESIAN_POINT('Ctrl Pts',(1.65508430440733,2.11231773338789,13.8235269408515));
#425754=CARTESIAN_POINT('',(1.61693200657635,2.11486211089867,12.5969504640361));
#425755=CARTESIAN_POINT('Origin',(1.63792872868682,2.14212025626543,12.584524458991));
#425756=CARTESIAN_POINT('Origin',(1.63792872868682,2.14212025626543,12.584524458991));
#425757=CARTESIAN_POINT('Ctrl Pts',(1.6046712778331,2.1508650240259,12.5893111709658));
#425758=CARTESIAN_POINT('Ctrl Pts',(1.60177936858179,2.13990621499198,12.5770542771492));
#425759=CARTESIAN_POINT('Ctrl Pts',(1.61654650137658,2.13285387751594,12.5737548217797));
#425760=CARTESIAN_POINT('Ctrl Pts',(1.61099491281211,2.17482826149746,12.5663937883686));
#425761=CARTESIAN_POINT('Ctrl Pts',(1.60809931452895,2.1638554729807,12.5540940315304));
#425762=CARTESIAN_POINT('Ctrl Pts',(1.62291359152771,2.15678417944156,12.5508374392248));
#425763=CARTESIAN_POINT('Ctrl Pts',(1.61731216732095,2.19876732035617,12.5434499600944));
#425764=CARTESIAN_POINT('Ctrl Pts',(1.61440715441655,2.18775885539644,12.5311293540533));
#425765=CARTESIAN_POINT('Ctrl Pts',(1.62927332069752,2.18069140432334,12.5278936106989));
#425766=CARTESIAN_POINT('Ctrl Pts',(1.62362354115058,2.2226840945459,12.5204817579905));
#425767=CARTESIAN_POINT('Ctrl Pts',(1.62070415041766,2.21162114520783,12.5081597038247));
#425768=CARTESIAN_POINT('Ctrl Pts',(1.63562624762186,2.20457734936162,12.5049254088044));
#425769=CARTESIAN_POINT('Ctrl Pts',(1.6190859535201,2.20548903343026,12.5369868989719));
#425770=CARTESIAN_POINT('Ctrl Pts',(1.61932363119355,2.20638970567602,12.5342545179733));
#425771=CARTESIAN_POINT('Ctrl Pts',(1.61967107693414,2.20721743665328,12.5314872231885));
#425772=CARTESIAN_POINT('Ctrl Pts',(1.62016026268745,2.20790396298846,12.5287124745063));
#425773=CARTESIAN_POINT('Ctrl Pts',(1.6206014346808,2.20852310651364,12.5262100684184));
#425774=CARTESIAN_POINT('Ctrl Pts',(1.62115824440522,2.20902620816193,12.5237004536639));
#425775=CARTESIAN_POINT('Ctrl Pts',(1.6218846948609,2.2093727197878,12.5212220730815));
#425776=CARTESIAN_POINT('Ctrl Pts',(1.62244085552771,2.20963800441305,12.5193246583486));
#425777=CARTESIAN_POINT('Ctrl Pts',(1.62310336659281,2.20981410583755,12.517417831369));
#425778=CARTESIAN_POINT('Ctrl Pts',(1.62391525613458,2.20981383113023,12.5155812248348));
#425779=CARTESIAN_POINT('Ctrl Pts',(1.6242611254433,2.20981371410344,12.5147988205793));
#425780=CARTESIAN_POINT('Ctrl Pts',(1.62463445524413,2.20978186513892,12.5140295443047));
#425781=CARTESIAN_POINT('Ctrl Pts',(1.62503977185742,2.20971329987201,12.5132817086137));
#425782=CARTESIAN_POINT('Ctrl Pts',(1.62565316372165,2.20960953561584,12.5121499604604));
#425783=CARTESIAN_POINT('Ctrl Pts',(1.62635186698226,2.20941238879121,12.5110494206568));
#425784=CARTESIAN_POINT('Ctrl Pts',(1.62713783922933,2.20908466979489,12.5100666561695));
#425785=CARTESIAN_POINT('Ctrl Pts',(1.62758914268366,2.20889649430187,12.5095023550641));
#425786=CARTESIAN_POINT('Ctrl Pts',(1.62807418217456,2.20866249210592,12.5089719619137));
#425787=CARTESIAN_POINT('Ctrl Pts',(1.62858109092889,2.20838129679704,12.5085043804652));
#425788=CARTESIAN_POINT('Ctrl Pts',(1.62932288586133,2.20796980409075,12.5078201359221));
#425789=CARTESIAN_POINT('Ctrl Pts',(1.63013244139569,2.20744425880307,12.5072563000949));
#425790=CARTESIAN_POINT('Ctrl Pts',(1.63095027184392,2.20683318422143,12.5068768744332));
#425791=CARTESIAN_POINT('Ctrl Pts',(1.63153998389674,2.20639255738156,12.5066032824114));
#425792=CARTESIAN_POINT('Ctrl Pts',(1.63214439471116,2.20589976737752,12.5064197834844));
#425793=CARTESIAN_POINT('Ctrl Pts',(1.63273138581492,2.20538433625565,12.5063282718343));
#425794=CARTESIAN_POINT('Ctrl Pts',(1.63358821109856,2.20463196639117,12.5061946931565));
#425795=CARTESIAN_POINT('Ctrl Pts',(1.63442693474951,2.20381607233106,12.5062515701262));
#425796=CARTESIAN_POINT('Ctrl Pts',(1.63520628727281,2.20299837479338,12.5064436508398));
#425797=CARTESIAN_POINT('',(1.61654650137658,2.13285387751594,12.5737548217797));
#425798=CARTESIAN_POINT('Origin',(1.62594308508859,2.1452516278983,12.5893111709658));
#425799=CARTESIAN_POINT('Ctrl Pts',(1.63520628727281,2.20299837479338,12.5064436508398));
#425800=CARTESIAN_POINT('Ctrl Pts',(1.63244461846173,2.19261504328903,12.5164271754438));
#425801=CARTESIAN_POINT('Ctrl Pts',(1.62968165300992,2.18222764953829,12.5264061185523));
#425802=CARTESIAN_POINT('Ctrl Pts',(1.62691734616548,2.17183605022895,12.536380305637));
#425803=CARTESIAN_POINT('Ctrl Pts',(1.62346252327176,2.15884865873571,12.5488460165097));
#425804=CARTESIAN_POINT('Ctrl Pts',(1.6200056040881,2.14585469435912,12.5613043021964));
#425805=CARTESIAN_POINT('Ctrl Pts',(1.61654650137658,2.13285387751594,12.5737548217797));
#425806=CARTESIAN_POINT('Ctrl Pts',(1.65508430440733,2.11231773338789,12.5893111709658));
#425807=CARTESIAN_POINT('Ctrl Pts',(1.64526658674475,2.10665460223475,12.5770542771492));
#425808=CARTESIAN_POINT('Ctrl Pts',(1.63459030677956,2.11905705041888,12.5737548217797));
#425809=CARTESIAN_POINT('Ctrl Pts',(1.64592445921814,2.10703408127733,12.5928319619712));
#425810=CARTESIAN_POINT('Ctrl Pts',(1.63769858136471,2.1060500335591,12.5821634970842));
#425811=CARTESIAN_POINT('Ctrl Pts',(1.63125831311288,2.11712416770785,12.5773203894503));
#425812=CARTESIAN_POINT('Ctrl Pts',(1.62924613397682,2.10547922871696,12.5969440695591));
#425813=CARTESIAN_POINT('Ctrl Pts',(1.62604181447296,2.10790634203715,12.5878292599214));
#425814=CARTESIAN_POINT('Ctrl Pts',(1.62531362775016,2.1165720236725,12.5813877129824));
#425815=CARTESIAN_POINT('Ctrl Pts',(1.604907571088,2.12402133221274,12.596957478804));
#425816=CARTESIAN_POINT('Ctrl Pts',(1.60808825821064,2.12161221980839,12.5878468778671));
#425817=CARTESIAN_POINT('Ctrl Pts',(1.61660613363589,2.12321324453574,12.5814011370086));
#425818=CARTESIAN_POINT('Ctrl Pts',(1.60196923397952,2.14062570459404,12.5928371701607));
#425819=CARTESIAN_POINT('Ctrl Pts',(1.60318073372141,2.13243623977153,12.5821692192952));
#425820=CARTESIAN_POINT('Ctrl Pts',(1.61555109509945,2.12911991931888,12.5773318885715));
#425821=CARTESIAN_POINT('Ctrl Pts',(1.60467127783304,2.15086502402591,12.5893111709658));
#425822=CARTESIAN_POINT('Ctrl Pts',(1.60177936858174,2.13990621499199,12.5770542771492));
#425823=CARTESIAN_POINT('Ctrl Pts',(1.61654650137653,2.13285387751595,12.5737548217797));
#425824=CARTESIAN_POINT('',(1.63459030677956,2.11905705041888,12.5737548217797));
#425825=CARTESIAN_POINT('Origin',(1.64409177465531,2.13137460326862,12.5893111709658));
#425826=CARTESIAN_POINT('Ctrl Pts',(1.61654650137653,2.13285387751595,12.5737548217797));
#425827=CARTESIAN_POINT('Ctrl Pts',(1.61625932847722,2.13189374660982,12.5746934679442));
#425828=CARTESIAN_POINT('Ctrl Pts',(1.61611705479564,2.13077880551821,12.5756680099006));
#425829=CARTESIAN_POINT('Ctrl Pts',(1.6161325638161,2.12963632438565,12.5765688348656));
#425830=CARTESIAN_POINT('Ctrl Pts',(1.61613666965758,2.12933386515348,12.5768073183026));
#425831=CARTESIAN_POINT('Ctrl Pts',(1.61615158379493,2.12902953490736,12.5770407398754));
#425832=CARTESIAN_POINT('Ctrl Pts',(1.61617698225217,2.1287256828689,12.5772674179684));
#425833=CARTESIAN_POINT('Ctrl Pts',(1.61628121065262,2.12747875626814,12.5781976435658));
#425834=CARTESIAN_POINT('Ctrl Pts',(1.61657916191547,2.12617000016873,12.5790594849312));
#425835=CARTESIAN_POINT('Ctrl Pts',(1.61709780233104,2.12489850308143,12.5797571720116));
#425836=CARTESIAN_POINT('Ctrl Pts',(1.61743571521043,2.1240700770101,12.580211740231));
#425837=CARTESIAN_POINT('Ctrl Pts',(1.61790004929595,2.12322690986335,12.5806009430798));
#425838=CARTESIAN_POINT('Ctrl Pts',(1.61847363653371,2.12243690331591,12.5808812374708));
#425839=CARTESIAN_POINT('Ctrl Pts',(1.61896653825652,2.12175802560971,12.5811221033394));
#425840=CARTESIAN_POINT('Ctrl Pts',(1.61955030145264,2.12110457302263,12.581287365893));
#425841=CARTESIAN_POINT('Ctrl Pts',(1.62019819567159,2.12051898241095,12.581359338449));
#425842=CARTESIAN_POINT('Ctrl Pts',(1.62028823958953,2.12043759740791,12.5813693411482));
#425843=CARTESIAN_POINT('Ctrl Pts',(1.62037949916551,2.12035746791303,12.5813775999465));
#425844=CARTESIAN_POINT('Ctrl Pts',(1.62047188003752,2.12027865081987,12.5813841266931));
#425845=CARTESIAN_POINT('Ctrl Pts',(1.6206286153601,2.12014492808861,12.5813952001081));
#425846=CARTESIAN_POINT('Ctrl Pts',(1.62079002328469,2.12001455072096,12.5814007534795));
#425847=CARTESIAN_POINT('Ctrl Pts',(1.6209561574325,2.11988772891379,12.5814005856065));
#425848=CARTESIAN_POINT('Ctrl Pts',(1.62171665460697,2.11930718826465,12.5813998171494));
#425849=CARTESIAN_POINT('Ctrl Pts',(1.62252343814571,2.11884099525493,12.58127954464));
#425850=CARTESIAN_POINT('Ctrl Pts',(1.62335712354063,2.1184661769397,12.5810700125799));
#425851=CARTESIAN_POINT('Ctrl Pts',(1.624364120575,2.11801343909139,12.5808169217085));
#425852=CARTESIAN_POINT('Ctrl Pts',(1.62541732084484,2.11770923923754,12.5804173076348));
#425853=CARTESIAN_POINT('Ctrl Pts',(1.62641719714309,2.11755521730455,12.5799304713245));
#425854=CARTESIAN_POINT('Ctrl Pts',(1.62765635887015,2.11736433560767,12.5793271277669));
#425855=CARTESIAN_POINT('Ctrl Pts',(1.62888558532817,2.11736044674188,12.5785808224116));
#425856=CARTESIAN_POINT('Ctrl Pts',(1.63005296191707,2.11751199793029,12.5777485681082));
#425857=CARTESIAN_POINT('Ctrl Pts',(1.63179248093017,2.11773782580469,12.576508418016));
#425858=CARTESIAN_POINT('Ctrl Pts',(1.63338090448777,2.11830008029549,12.5750928681475));
#425859=CARTESIAN_POINT('Ctrl Pts',(1.63459030677956,2.11905705041888,12.5737548217797));
#425860=CARTESIAN_POINT('Ctrl Pts',(1.63459030677956,2.11905705041888,12.5737548217797));
#425861=CARTESIAN_POINT('Ctrl Pts',(1.64526658674475,2.10665460223475,12.5770542771492));
#425862=CARTESIAN_POINT('Ctrl Pts',(1.65508430440733,2.11231773338789,12.5893111709658));
#425863=CARTESIAN_POINT('Ctrl Pts',(1.65601196783346,2.13147185576822,12.5508408821982));
#425864=CARTESIAN_POINT('Ctrl Pts',(1.66671889022083,2.11902888435382,12.5540974840599));
#425865=CARTESIAN_POINT('Ctrl Pts',(1.67654913277672,2.1246992402119,12.5663972313419));
#425866=CARTESIAN_POINT('Ctrl Pts',(1.67741329405842,2.1438735128996,12.52790050457));
#425867=CARTESIAN_POINT('Ctrl Pts',(1.68813010742981,2.13137946677734,12.5311362602938));
#425868=CARTESIAN_POINT('Ctrl Pts',(1.69799230666146,2.1370682561301,12.5434568539655));
#425869=CARTESIAN_POINT('Ctrl Pts',(1.69879587267538,2.15626303161689,12.5049357605811));
#425870=CARTESIAN_POINT('Ctrl Pts',(1.70950452140481,2.14370882007737,12.5081700652078));
#425871=CARTESIAN_POINT('Ctrl Pts',(1.71941552204513,2.14942575943273,12.5204921097672));
#425872=CARTESIAN_POINT('Ctrl Pts',(1.69739180954195,2.15544948587923,12.5064436508395));
#425873=CARTESIAN_POINT('Ctrl Pts',(1.69846484030352,2.15486857902327,12.5062361689309));
#425874=CARTESIAN_POINT('Ctrl Pts',(1.69955593332796,2.15421872701515,12.5061871075061));
#425875=CARTESIAN_POINT('Ctrl Pts',(1.70057501660636,2.15353135090792,12.5063648335164));
#425876=CARTESIAN_POINT('Ctrl Pts',(1.70103794709108,2.1532191022809,12.5064455676329));
#425877=CARTESIAN_POINT('Ctrl Pts',(1.70149235181968,2.1528945725499,12.506574497099));
#425878=CARTESIAN_POINT('Ctrl Pts',(1.70191813648468,2.15257082134372,12.5067492519495));
#425879=CARTESIAN_POINT('Ctrl Pts',(1.70277376729671,2.15192023072781,12.5071004286051));
#425880=CARTESIAN_POINT('Ctrl Pts',(1.70354479256992,2.15124822075764,12.5076537929612));
#425881=CARTESIAN_POINT('Ctrl Pts',(1.70417955742088,2.15061235958551,12.5083435010503));
#425882=CARTESIAN_POINT('Ctrl Pts',(1.7042195196617,2.15057232832472,12.5083869222963));
#425883=CARTESIAN_POINT('Ctrl Pts',(1.70425893775195,2.15053242754061,12.5084308732336));
#425884=CARTESIAN_POINT('Ctrl Pts',(1.70429779751439,2.15049266626635,12.5084753333615));
#425885=CARTESIAN_POINT('Ctrl Pts',(1.70460950409876,2.15017372836719,12.508831962269));
#425886=CARTESIAN_POINT('Ctrl Pts',(1.70489253777622,2.14985819349379,12.509227847131));
#425887=CARTESIAN_POINT('Ctrl Pts',(1.70514056685342,2.14955731381794,12.5096423454524));
#425888=CARTESIAN_POINT('Ctrl Pts',(1.7059177802083,2.14861449007762,12.5109411997424));
#425889=CARTESIAN_POINT('Ctrl Pts',(1.70640654112272,2.14776372873729,12.5124831113042));
#425890=CARTESIAN_POINT('Ctrl Pts',(1.70670093375151,2.14701522926795,12.5140723025008));
#425891=CARTESIAN_POINT('Ctrl Pts',(1.70672851866326,2.14694509404787,12.5142212114565));
#425892=CARTESIAN_POINT('Ctrl Pts',(1.70675442572002,2.14687584931539,12.5143705582413));
#425893=CARTESIAN_POINT('Ctrl Pts',(1.70677874908882,2.14680750075468,12.5145201959299));
#425894=CARTESIAN_POINT('Ctrl Pts',(1.70709121897482,2.14592946173196,12.5164425148273));
#425895=CARTESIAN_POINT('Ctrl Pts',(1.70716315230696,2.14517283542057,12.5184635205941));
#425896=CARTESIAN_POINT('Ctrl Pts',(1.70707620808332,2.14449928402478,12.5205025929157));
#425897=CARTESIAN_POINT('Ctrl Pts',(1.70702577698747,2.14410859751815,12.5216853356836));
#425898=CARTESIAN_POINT('Ctrl Pts',(1.70692246285206,2.1437465050659,12.5228750347131));
#425899=CARTESIAN_POINT('Ctrl Pts',(1.70678440409457,2.14341102387711,12.5240609649613));
#425900=CARTESIAN_POINT('Ctrl Pts',(1.70644554628091,2.14258760329718,12.5269717671326));
#425901=CARTESIAN_POINT('Ctrl Pts',(1.70587822584832,2.14190527894986,12.5299036066169));
#425902=CARTESIAN_POINT('Ctrl Pts',(1.70515711749028,2.14132008251949,12.5328133004019));
#425903=CARTESIAN_POINT('Ctrl Pts',(1.70481094348954,2.14103915415795,12.5342101228451));
#425904=CARTESIAN_POINT('Ctrl Pts',(1.70442942983967,2.14078136695572,12.5356023438238));
#425905=CARTESIAN_POINT('Ctrl Pts',(1.70402056201252,2.14054552058717,12.5369868989719));
#425906=CARTESIAN_POINT('Origin',(12.7471961618985,8.5044392418344,-1.24036033660154));
#425907=CARTESIAN_POINT('Ctrl Pts',(1.61907525114944,2.20544863268529,12.5369868989719));
#425908=CARTESIAN_POINT('Ctrl Pts',(1.62301721897513,2.2202724039108,12.5369868989719));
#425909=CARTESIAN_POINT('Ctrl Pts',(1.61047093473111,2.22909703168501,12.5369868989719));
#425910=CARTESIAN_POINT('Ctrl Pts',(1.62040772645585,2.2104596641296,12.5218025310015));
#425911=CARTESIAN_POINT('Ctrl Pts',(1.62011751176063,2.22227370827781,12.5216901060417));
#425912=CARTESIAN_POINT('Ctrl Pts',(1.61050918945125,2.22907014478422,12.5161920673677));
#425913=CARTESIAN_POINT('Ctrl Pts',(1.62604303884323,2.21259959999119,12.5042015548895));
#425914=CARTESIAN_POINT('Ctrl Pts',(1.62469296832513,2.2188888491207,12.4980677368514));
#425915=CARTESIAN_POINT('Ctrl Pts',(1.61920579610378,2.22289905120251,12.4907278922778));
#425916=CARTESIAN_POINT('Ctrl Pts',(1.63519436629549,2.20298231448191,12.506463626192));
#425917=CARTESIAN_POINT('Ctrl Pts',(1.63909395033029,2.20823594967023,12.4999376786891));
#425918=CARTESIAN_POINT('Ctrl Pts',(1.6390463225813,2.20817178415518,12.4906970594712));
#425919=CARTESIAN_POINT('Origin',(1.59781414626462,2.21110242955786,12.5369868989719));
#425920=CARTESIAN_POINT('Origin',(1.59781414626462,2.21110242955786,14.));
#425921=CARTESIAN_POINT('Origin',(1.59781414626462,2.21110242955786,13.7435492065112));
#425922=CARTESIAN_POINT('Ctrl Pts',(1.61276827855017,2.18154848765808,13.793642941384));
#425923=CARTESIAN_POINT('Ctrl Pts',(1.61555340082184,2.19199594251261,13.8071662555867));
#425924=CARTESIAN_POINT('Ctrl Pts',(1.59992190433366,2.19875432258291,13.8103758687955));
#425925=CARTESIAN_POINT('Ctrl Pts',(1.61700923339519,2.1976194554953,13.7804579775006));
#425926=CARTESIAN_POINT('Ctrl Pts',(1.62043602394366,2.21051328263337,13.7901904343352));
#425927=CARTESIAN_POINT('Ctrl Pts',(1.60717596551943,2.21902367479535,13.7927914348262));
#425928=CARTESIAN_POINT('Ctrl Pts',(1.61950604308078,2.20708103908937,13.7597120340895));
#425929=CARTESIAN_POINT('Ctrl Pts',(1.62346626664974,2.22200430010217,13.7635825532445));
#425930=CARTESIAN_POINT('Ctrl Pts',(1.61142960956155,2.23098510197535,13.7651073818884));
#425931=CARTESIAN_POINT('Ctrl Pts',(1.61901711057312,2.20522824437622,13.7381884353898));
#425932=CARTESIAN_POINT('Ctrl Pts',(1.62288550649353,2.21980196811551,13.7368803041982));
#425933=CARTESIAN_POINT('Ctrl Pts',(1.61059615399851,2.22864286469742,13.7363986145813));
#425934=CARTESIAN_POINT('Origin',(1.59252555697098,2.19106146869382,13.7902182540695));
#425935=CARTESIAN_POINT('Ctrl Pts',(1.60467027276106,2.15086121830799,13.8235227101244));
#425936=CARTESIAN_POINT('Ctrl Pts',(1.60760808764213,2.16197660998099,13.8358800583119));
#425937=CARTESIAN_POINT('Ctrl Pts',(1.59260642281721,2.16901763984444,13.8390832900376));
#425938=CARTESIAN_POINT('Ctrl Pts',(1.6077136467495,2.1623939987213,13.8124254819053));
#425939=CARTESIAN_POINT('Ctrl Pts',(1.61065716655649,2.17353097639845,13.8247886449158));
#425940=CARTESIAN_POINT('Ctrl Pts',(1.59562930473764,2.18056547355579,13.8279860620657));
#425941=CARTESIAN_POINT('Ctrl Pts',(1.61075565679672,2.17392161051757,13.8013225099955));
#425942=CARTESIAN_POINT('Ctrl Pts',(1.61370349459905,2.18507491882158,13.8136962257787));
#425943=CARTESIAN_POINT('Ctrl Pts',(1.59865104943327,2.19210789254638,13.8168830918626));
#425944=CARTESIAN_POINT('Ctrl Pts',(1.6137963559716,2.18544425479983,13.7902140179785));
#425945=CARTESIAN_POINT('Ctrl Pts',(1.61674721548195,2.19660898183165,13.802602731458));
#425946=CARTESIAN_POINT('Ctrl Pts',(1.60167170336868,2.20364510910769,13.8057746032558));
#425947=CARTESIAN_POINT('Origin',(1.58339947057761,2.1564784201535,13.8235269408515));
#425948=CARTESIAN_POINT('Ctrl Pts',(1.65508430440733,2.11231773338789,13.8235269408515));
#425949=CARTESIAN_POINT('Ctrl Pts',(1.66531219704801,2.11821746481581,13.8362179249168));
#425950=CARTESIAN_POINT('Ctrl Pts',(1.67612584604187,2.10499899291114,13.8391868794938));
#425951=CARTESIAN_POINT('Ctrl Pts',(1.6457262278348,2.10691973593138,13.8400110824519));
#425952=CARTESIAN_POINT('Ctrl Pts',(1.65563583345973,2.10868653507685,13.8494522556837));
#425953=CARTESIAN_POINT('Ctrl Pts',(1.66066895356037,2.09621273896306,13.85569149686));
#425954=CARTESIAN_POINT('Ctrl Pts',(1.62951895726314,2.10526985512872,13.8586819406588));
#425955=CARTESIAN_POINT('Ctrl Pts',(1.63298603289465,2.10263633463321,13.868010383617));
#425956=CARTESIAN_POINT('Ctrl Pts',(1.63374977619388,2.09361915309099,13.8744918421245));
#425957=CARTESIAN_POINT('Ctrl Pts',(1.60463050515763,2.12423393827925,13.8587686893867));
#425958=CARTESIAN_POINT('Ctrl Pts',(1.60119425240762,2.12684397562723,13.8680909899357));
#425959=CARTESIAN_POINT('Ctrl Pts',(1.59231937169436,2.12519082898184,13.8745789365163));
#425960=CARTESIAN_POINT('Ctrl Pts',(1.60191027505477,2.14040228142712,13.8400379222776));
#425961=CARTESIAN_POINT('Ctrl Pts',(1.60101108062577,2.15042533900887,13.8494748685453));
#425962=CARTESIAN_POINT('Ctrl Pts',(1.5876604665708,2.15201348560764,13.8557104837033));
#425963=CARTESIAN_POINT('Ctrl Pts',(1.60467127782667,2.15086502402745,13.8235269408542));
#425964=CARTESIAN_POINT('Ctrl Pts',(1.60768400831709,2.16228168176001,13.8362179249195));
#425965=CARTESIAN_POINT('Ctrl Pts',(1.5920933751234,2.16925270468897,13.8391868794965));
#425966=CARTESIAN_POINT('Origin',(1.66607683415935,2.09326086350716,13.8235269408515));
#425967=CARTESIAN_POINT('Ctrl Pts',(1.68606296100254,2.13018707865354,13.7902140241682));
#425968=CARTESIAN_POINT('Ctrl Pts',(1.69606394613856,2.13596106269421,13.8026027327198));
#425969=CARTESIAN_POINT('Ctrl Pts',(1.70680540507266,2.12325677238577,13.8057746032556));
#425970=CARTESIAN_POINT('Ctrl Pts',(1.67574011770996,2.12423257706404,13.8013225161808));
#425971=CARTESIAN_POINT('Ctrl Pts',(1.68573087530632,2.13000065217942,13.8136962270464));
#425972=CARTESIAN_POINT('Ctrl Pts',(1.6964632450561,2.11731779584232,13.8168830918628));
#425973=CARTESIAN_POINT('Ctrl Pts',(1.6654128241468,2.11827550843538,13.8124254880875));
#425974=CARTESIAN_POINT('Ctrl Pts',(1.67538895378594,2.12403513624135,13.8247886461868));
#425975=CARTESIAN_POINT('Ctrl Pts',(1.68611635037669,2.11137640310633,13.8279860620656));
#425976=CARTESIAN_POINT('Ctrl Pts',(1.65508090014856,2.11231576884368,13.8235227163065));
#425977=CARTESIAN_POINT('Ctrl Pts',(1.6650376937008,2.11806423345566,13.8358800595847));
#425978=CARTESIAN_POINT('Ctrl Pts',(1.6757645283418,2.10543249369491,13.8390832900376));
#425979=CARTESIAN_POINT('Origin',(1.69705890579041,2.1111321795373,13.7902182540695));
#425980=CARTESIAN_POINT('Ctrl Pts',(1.70378681738456,2.14041065837467,13.7382347919292));
#425981=CARTESIAN_POINT('Ctrl Pts',(1.71684636951277,2.14797147624999,13.7369371795943));
#425982=CARTESIAN_POINT('Ctrl Pts',(1.72860310212523,2.13841516863148,13.7364597369711));
#425983=CARTESIAN_POINT('Ctrl Pts',(1.70542532565402,2.14135579573781,13.7595490285574));
#425984=CARTESIAN_POINT('Ctrl Pts',(1.71879697125689,2.14909613812624,13.7633824266925));
#425985=CARTESIAN_POINT('Ctrl Pts',(1.73061977660815,2.13981632487743,13.7648920890506));
#425986=CARTESIAN_POINT('Ctrl Pts',(1.69706902324063,2.13653564697155,13.7803806590111));
#425987=CARTESIAN_POINT('Ctrl Pts',(1.70863231356203,2.14323543823304,13.7901039518745));
#425988=CARTESIAN_POINT('Ctrl Pts',(1.72033643142302,2.13267612639362,13.7926933640892));
#425989=CARTESIAN_POINT('Ctrl Pts',(1.68254390432342,2.12815715235653,13.7936647693663));
#425990=CARTESIAN_POINT('Ctrl Pts',(1.6918974403683,2.13358713351688,13.8072068914932));
#425991=CARTESIAN_POINT('Ctrl Pts',(1.70251977049854,2.12025257793931,13.8104111085397));
#425992=CARTESIAN_POINT('Origin',(1.71501309176454,2.12148865070644,13.7435492065112));
#425993=CARTESIAN_POINT('Origin',(1.71501309176454,2.12148865070644,14.));
#425994=CARTESIAN_POINT('Origin',(1.71501309176454,2.12148865070644,12.5369868989719));
#425995=CARTESIAN_POINT('Ctrl Pts',(1.69738043613688,2.15543504326693,12.506462012331));
#425996=CARTESIAN_POINT('Ctrl Pts',(1.70142577122634,2.16057205134594,12.4999388158272));
#425997=CARTESIAN_POINT('Ctrl Pts',(1.70137790960711,2.1605112738036,12.4907030323752));
#425998=CARTESIAN_POINT('Ctrl Pts',(1.70905878238044,2.14912276854463,12.5042014951932));
#425999=CARTESIAN_POINT('Ctrl Pts',(1.71547915128111,2.14946912139297,12.4980716682127));
#426000=CARTESIAN_POINT('Ctrl Pts',(1.72078458610918,2.14522908288952,12.4907355092743));
#426001=CARTESIAN_POINT('Ctrl Pts',(1.70847310421998,2.14312421185675,12.5218047446509));
#426002=CARTESIAN_POINT('Ctrl Pts',(1.71994483569297,2.14593815001309,12.5216906929434));
#426003=CARTESIAN_POINT('Ctrl Pts',(1.72901979008099,2.13845376913115,12.5161988840776));
#426004=CARTESIAN_POINT('Ctrl Pts',(1.70398730191446,2.14052629652156,12.5369868989719));
#426005=CARTESIAN_POINT('Ctrl Pts',(1.71725298458519,2.14820921229621,12.5369868989719));
#426006=CARTESIAN_POINT('Ctrl Pts',(1.72905445820664,2.13842500298309,12.5369868989719));
#426007=CARTESIAN_POINT('Origin',(3.12930240632745E-31,-1.0592894849964E-31,
12.5));
#426008=CARTESIAN_POINT('Origin',(1.82175065299146,1.97038443452176,12.5));
#426009=CARTESIAN_POINT('',(1.82175065299146,1.97038443452176,12.5893111709658));
#426010=CARTESIAN_POINT('',(1.82175065299146,1.97038443452176,13.8235269408515));
#426011=CARTESIAN_POINT('',(1.82175065299146,1.97038443452176,12.5));
#426012=CARTESIAN_POINT('',(1.85408631250068,1.98567095876063,13.7902182540695));
#426013=CARTESIAN_POINT('',(1.82175065299146,1.97038443452176,13.8235269408515));
#426014=CARTESIAN_POINT('',(1.87282490594716,1.99452953679089,13.7435492065112));
#426015=CARTESIAN_POINT('Origin',(1.81117504197252,1.96538522666951,13.7445212918709));
#426016=CARTESIAN_POINT('',(1.87282490594716,1.99452953679089,12.5369868989719));
#426017=CARTESIAN_POINT('',(1.87282490594716,1.99452953679089,12.5));
#426018=CARTESIAN_POINT('Ctrl Pts',(1.87282490594716,1.99452953679089,12.5369868989719));
#426019=CARTESIAN_POINT('Ctrl Pts',(1.85581257177983,1.98648703935753,12.5544431401645));
#426020=CARTESIAN_POINT('Ctrl Pts',(1.83878806993894,1.97843878971625,12.5718848856037));
#426021=CARTESIAN_POINT('Ctrl Pts',(1.82175065299146,1.97038443452176,12.5893111709658));
#426022=CARTESIAN_POINT('Origin',(1.8662544309495,2.27220613159535,12.5));
#426023=CARTESIAN_POINT('',(1.79346640956076,2.06617991453902,13.7435492065112));
#426024=CARTESIAN_POINT('',(1.7865618932501,2.04663670744329,13.7902182540695));
#426025=CARTESIAN_POINT('Origin',(1.76841801772587,1.99528053694052,13.7418732680445));
#426026=CARTESIAN_POINT('',(1.77464733364696,2.0129125919076,13.8235269408515));
#426027=CARTESIAN_POINT('',(1.7865618932501,2.04663670744329,13.7902182540695));
#426028=CARTESIAN_POINT('',(1.77464733364696,2.0129125919076,12.5893111709658));
#426029=CARTESIAN_POINT('',(1.77464733364696,2.0129125919076,12.5));
#426030=CARTESIAN_POINT('',(1.79346640956076,2.06617991453902,12.5369868989719));
#426031=CARTESIAN_POINT('Ctrl Pts',(1.77464733364696,2.0129125919076,12.5893111709658));
#426032=CARTESIAN_POINT('Ctrl Pts',(1.78092502591566,2.03068157594217,12.5718848856037));
#426033=CARTESIAN_POINT('Ctrl Pts',(1.78719795941929,2.04843709031033,12.5544431401645));
#426034=CARTESIAN_POINT('Ctrl Pts',(1.79346640956076,2.06617991453902,12.5369868989719));
#426035=CARTESIAN_POINT('',(1.79346640956076,2.06617991453902,12.5));
#426036=CARTESIAN_POINT('Origin',(1.80705902610793,2.00146170474478,12.5));
#426037=CARTESIAN_POINT('',(1.78486661864788,1.97521123382891,13.8587068136939));
#426038=CARTESIAN_POINT('Ctrl Pts',(1.77464733364068,2.01291259190967,13.8235269408542));
#426039=CARTESIAN_POINT('Ctrl Pts',(1.77406361377395,2.01126037505213,13.8262006681044));
#426040=CARTESIAN_POINT('Ctrl Pts',(1.77363007809038,2.00951169702485,13.8288634856214));
#426041=CARTESIAN_POINT('Ctrl Pts',(1.77333636387986,2.00767494950749,13.8314912288862));
#426042=CARTESIAN_POINT('Ctrl Pts',(1.77303357482403,2.00578145226881,13.8342001611531));
#426043=CARTESIAN_POINT('Ctrl Pts',(1.77287855383073,2.00379233457868,13.8368750301949));
#426044=CARTESIAN_POINT('Ctrl Pts',(1.77289702249318,2.00169093313529,13.8394886372969));
#426045=CARTESIAN_POINT('Ctrl Pts',(1.77289844887278,2.00152863680453,13.8396904925131));
#426046=CARTESIAN_POINT('Ctrl Pts',(1.77290093194159,2.00136566709419,13.8398919674349));
#426047=CARTESIAN_POINT('Ctrl Pts',(1.7729044949596,2.00120201545393,13.8400930404591));
#426048=CARTESIAN_POINT('Ctrl Pts',(1.7729600091774,1.99865221279919,13.8432258934518));
#426049=CARTESIAN_POINT('Ctrl Pts',(1.77327628051391,1.9959498528445,13.8462331177034));
#426050=CARTESIAN_POINT('Ctrl Pts',(1.77393880624529,1.99319428545123,13.8489036603661));
#426051=CARTESIAN_POINT('Ctrl Pts',(1.77415559237479,1.992292631732,13.8497774930041));
#426052=CARTESIAN_POINT('Ctrl Pts',(1.77440953531336,1.99138551654611,13.85061494757));
#426053=CARTESIAN_POINT('Ctrl Pts',(1.77470385964067,1.99047709653535,13.8514076489583));
#426054=CARTESIAN_POINT('Ctrl Pts',(1.77532639804086,1.98855565719886,13.8530843267192));
#426055=CARTESIAN_POINT('Ctrl Pts',(1.77619355970518,1.98644055607719,13.8546805203176));
#426056=CARTESIAN_POINT('Ctrl Pts',(1.77738126215705,1.98430631248208,13.8559412814273));
#426057=CARTESIAN_POINT('Ctrl Pts',(1.77754021526322,1.98402068147387,13.8561100121513));
#426058=CARTESIAN_POINT('Ctrl Pts',(1.77770483427809,1.98373472264295,13.8562727473908));
#426059=CARTESIAN_POINT('Ctrl Pts',(1.77787522552839,1.98344885975351,13.8564289040185));
#426060=CARTESIAN_POINT('Ctrl Pts',(1.77864794790453,1.98215247481122,13.8571370725437));
#426061=CARTESIAN_POINT('Ctrl Pts',(1.77955492048912,1.98083644173013,13.8577210840554));
#426062=CARTESIAN_POINT('Ctrl Pts',(1.78058505424064,1.97956856888076,13.8581177131616));
#426063=CARTESIAN_POINT('Ctrl Pts',(1.78087517536119,1.97921149224752,13.8582294175695));
#426064=CARTESIAN_POINT('Ctrl Pts',(1.78117490825311,1.97885815276292,13.8583265086086));
#426065=CARTESIAN_POINT('Ctrl Pts',(1.7814836292635,1.97850983734979,13.8584082369006));
#426066=CARTESIAN_POINT('Ctrl Pts',(1.78192717856864,1.97800940150559,13.8585256585398));
#426067=CARTESIAN_POINT('Ctrl Pts',(1.78239503747439,1.97751332921741,13.8586122832068));
#426068=CARTESIAN_POINT('Ctrl Pts',(1.78287562685303,1.97703504882291,13.8586682984299));
#426069=CARTESIAN_POINT('Ctrl Pts',(1.78326005071664,1.97665247191771,13.8587131050557));
#426070=CARTESIAN_POINT('Ctrl Pts',(1.78365670062409,1.97627688723527,13.8587357943552));
#426071=CARTESIAN_POINT('Ctrl Pts',(1.78406597192143,1.97590861788907,13.8587355499465));
#426072=CARTESIAN_POINT('Ctrl Pts',(1.78433049371834,1.97567059663072,13.8587353919793));
#426073=CARTESIAN_POINT('Ctrl Pts',(1.78459740153457,1.97543817642315,13.8587257282814));
#426074=CARTESIAN_POINT('Ctrl Pts',(1.78486661864788,1.97521123382891,13.8587068136939));
#426075=CARTESIAN_POINT('Ctrl Pts',(1.78486661864788,1.97521123382891,13.8587068136939));
#426076=CARTESIAN_POINT('Ctrl Pts',(1.78575205905721,1.97446483200821,13.8586446046466));
#426077=CARTESIAN_POINT('Ctrl Pts',(1.78666244929838,1.97377760887465,13.858482427929));
#426078=CARTESIAN_POINT('Ctrl Pts',(1.78759534665637,1.9731458202193,13.8582284286032));
#426079=CARTESIAN_POINT('Ctrl Pts',(1.78855239082654,1.97249767855163,13.8579678548414));
#426080=CARTESIAN_POINT('Ctrl Pts',(1.78953631898589,1.97190756315503,13.857615680862));
#426081=CARTESIAN_POINT('Ctrl Pts',(1.79050335670337,1.97139042916805,13.8571944833187));
#426082=CARTESIAN_POINT('Ctrl Pts',(1.79291669822787,1.97009986841542,13.8561433417727));
#426083=CARTESIAN_POINT('Ctrl Pts',(1.79533547276294,1.96919924099179,13.8546163505474));
#426084=CARTESIAN_POINT('Ctrl Pts',(1.79757795172452,1.96858989301544,13.8528973491086));
#426085=CARTESIAN_POINT('Ctrl Pts',(1.79798761954609,1.96847857413025,13.8525833129072));
#426086=CARTESIAN_POINT('Ctrl Pts',(1.79839143382854,1.96837683829907,13.8522628768811));
#426087=CARTESIAN_POINT('Ctrl Pts',(1.79878835153583,1.96828391743601,13.851937733538));
#426088=CARTESIAN_POINT('Ctrl Pts',(1.8012122729045,1.96771646261751,13.8499521282529));
#426089=CARTESIAN_POINT('Ctrl Pts',(1.80362081688741,1.96742532761238,13.847639871647));
#426090=CARTESIAN_POINT('Ctrl Pts',(1.80587775823729,1.9673460532784,13.8452109780794));
#426091=CARTESIAN_POINT('Ctrl Pts',(1.80689320286696,1.96731038611465,13.8441181685877));
#426092=CARTESIAN_POINT('Ctrl Pts',(1.80787818322274,1.96731692383928,13.8430021611332));
#426093=CARTESIAN_POINT('Ctrl Pts',(1.80882224880307,1.96735712737537,13.8418824960098));
#426094=CARTESIAN_POINT('Ctrl Pts',(1.81104696345071,1.9674518680348,13.8392439765549));
#426095=CARTESIAN_POINT('Ctrl Pts',(1.81315098137492,1.96773431225335,13.8364981347964));
#426096=CARTESIAN_POINT('Ctrl Pts',(1.81514441983153,1.96817129068831,13.8336931113419));
#426097=CARTESIAN_POINT('Ctrl Pts',(1.81708590229323,1.96859687993326,13.8309611966327));
#426098=CARTESIAN_POINT('Ctrl Pts',(1.81892431901754,1.96917003077274,13.8281701127185));
#426099=CARTESIAN_POINT('Ctrl Pts',(1.82064721208293,1.96989279675487,13.825358068512));
#426100=CARTESIAN_POINT('Ctrl Pts',(1.8210207371589,1.97004949319983,13.8247484142932));
#426101=CARTESIAN_POINT('Ctrl Pts',(1.82138868766226,1.97021331718992,13.8241378483365));
#426102=CARTESIAN_POINT('Ctrl Pts',(1.82175065299146,1.97038443452176,13.8235269408515));
#426103=CARTESIAN_POINT('',(1.78393269417216,1.97603011228814,12.5969504640361));
#426104=CARTESIAN_POINT('Origin',(1.80708134332157,2.00148613064876,12.584524458991));
#426105=CARTESIAN_POINT('Origin',(1.80708134332157,2.00148613064876,12.584524458991));
#426106=CARTESIAN_POINT('Ctrl Pts',(1.77464733364696,2.0129125919076,12.5893111709658));
#426107=CARTESIAN_POINT('Ctrl Pts',(1.77087180231224,2.00222596485786,12.5770542771492));
#426108=CARTESIAN_POINT('Ctrl Pts',(1.78501496771585,1.99399343503885,12.5737548217797));
#426109=CARTESIAN_POINT('Ctrl Pts',(1.78290315357002,2.03628065872676,12.5663937883685));
#426110=CARTESIAN_POINT('Ctrl Pts',(1.77912280602073,2.02558039940009,12.5540940315304));
#426111=CARTESIAN_POINT('Ctrl Pts',(1.79331141366479,2.0173251339024,12.5508374392248));
#426112=CARTESIAN_POINT('Ctrl Pts',(1.79115064347199,2.05962514745298,12.5434499600945));
#426113=CARTESIAN_POINT('Ctrl Pts',(1.78735800466664,2.04889009777273,12.5311293540533));
#426114=CARTESIAN_POINT('Ctrl Pts',(1.80159864213211,2.04063443249746,12.5278936106989));
#426115=CARTESIAN_POINT('Ctrl Pts',(1.79939045585481,2.0829479049905,12.5204817579905));
#426116=CARTESIAN_POINT('Ctrl Pts',(1.79557904607925,2.07215972415076,12.5081597038247));
#426117=CARTESIAN_POINT('Ctrl Pts',(1.80987735648312,2.06392307650201,12.5049254088044));
#426118=CARTESIAN_POINT('Ctrl Pts',(1.79346640956076,2.06617991453902,12.5369868989719));
#426119=CARTESIAN_POINT('Ctrl Pts',(1.79377670953082,2.0670582169353,12.5342545179733));
#426120=CARTESIAN_POINT('Ctrl Pts',(1.7941904669333,2.06785487365262,12.5314872231885));
#426121=CARTESIAN_POINT('Ctrl Pts',(1.79473398323109,2.06849924244778,12.5287124745063));
#426122=CARTESIAN_POINT('Ctrl Pts',(1.79522415320617,2.06908036621086,12.5262100684184));
#426123=CARTESIAN_POINT('Ctrl Pts',(1.79582011764708,2.06953640866822,12.5237004536639));
#426124=CARTESIAN_POINT('Ctrl Pts',(1.79657239481317,2.06982255484906,12.5212220730815));
#426125=CARTESIAN_POINT('Ctrl Pts',(1.79714832806097,2.07004162450412,12.5193246583486));
#426126=CARTESIAN_POINT('Ctrl Pts',(1.7978229885761,2.0701631391634,12.517417831369));
#426127=CARTESIAN_POINT('Ctrl Pts',(1.7986321542312,2.07009668883528,12.5155812248348));
#426128=CARTESIAN_POINT('Ctrl Pts',(1.79897686314955,2.07006838063833,12.5147988205793));
#426129=CARTESIAN_POINT('Ctrl Pts',(1.79934635473999,2.07000620780402,12.5140295443047));
#426130=CARTESIAN_POINT('Ctrl Pts',(1.7997447339899,2.06990483361562,12.5132817086137));
#426131=CARTESIAN_POINT('Ctrl Pts',(1.80034762709312,2.06975141749507,12.5121499604604));
#426132=CARTESIAN_POINT('Ctrl Pts',(1.80102793617984,2.06949797585804,12.5110494206568));
#426133=CARTESIAN_POINT('Ctrl Pts',(1.8017845810285,2.0691072832849,12.5100666561695));
#426134=CARTESIAN_POINT('Ctrl Pts',(1.8022190447582,2.06888294850909,12.5095023550641));
#426135=CARTESIAN_POINT('Ctrl Pts',(1.80268339696886,2.06861018971475,12.5089719619137));
#426136=CARTESIAN_POINT('Ctrl Pts',(1.80316569899797,2.06828861229067,12.5085043804652));
#426137=CARTESIAN_POINT('Ctrl Pts',(1.8038714851933,2.06781802561894,12.5078201359221));
#426138=CARTESIAN_POINT('Ctrl Pts',(1.80463551017852,2.06722824274825,12.5072563000949));
#426139=CARTESIAN_POINT('Ctrl Pts',(1.80540081111206,2.06655254069297,12.5068768744332));
#426140=CARTESIAN_POINT('Ctrl Pts',(1.80595264576864,2.06606531299563,12.5066032824114));
#426141=CARTESIAN_POINT('Ctrl Pts',(1.80651487849577,2.06552489761722,12.5064197834844));
#426142=CARTESIAN_POINT('Ctrl Pts',(1.8070579040136,2.06496333632558,12.5063282718343));
#426143=CARTESIAN_POINT('Ctrl Pts',(1.80785055315317,2.06414363069476,12.5061946931565));
#426144=CARTESIAN_POINT('Ctrl Pts',(1.80861998308007,2.06326208769095,12.5062515701262));
#426145=CARTESIAN_POINT('Ctrl Pts',(1.80933009243168,2.06238358650856,12.5064436508398));
#426146=CARTESIAN_POINT('',(1.78501496771585,1.99399343503885,12.5737548217797));
#426147=CARTESIAN_POINT('Origin',(1.79539081682198,2.0055840241234,12.5893111709658));
#426148=CARTESIAN_POINT('Ctrl Pts',(1.80933009243168,2.06238358650856,12.5064436508398));
#426149=CARTESIAN_POINT('Ctrl Pts',(1.80573127493399,2.05225990632942,12.5164271754438));
#426150=CARTESIAN_POINT('Ctrl Pts',(1.80213083399926,2.04213228310893,12.5264061185523));
#426151=CARTESIAN_POINT('Ctrl Pts',(1.79852871334319,2.03200057765943,12.536380305637));
#426152=CARTESIAN_POINT('Ctrl Pts',(1.79402679311189,2.01933800077885,12.5488460165097));
#426153=CARTESIAN_POINT('Ctrl Pts',(1.78952224781487,2.00666904375274,12.5613043021964));
#426154=CARTESIAN_POINT('Ctrl Pts',(1.78501496771585,1.99399343503885,12.5737548217797));
#426155=CARTESIAN_POINT('Ctrl Pts',(1.82175065299146,1.97038443452176,12.5893111709658));
#426156=CARTESIAN_POINT('Ctrl Pts',(1.81150400521158,1.9655403821031,12.5770542771492));
#426157=CARTESIAN_POINT('Ctrl Pts',(1.80187416435296,1.97877177809493,12.5737548217797));
#426158=CARTESIAN_POINT('Ctrl Pts',(1.81219061973347,1.96586497574649,12.5928319619712));
#426159=CARTESIAN_POINT('Ctrl Pts',(1.80391190378551,1.96555468777625,12.5821634970843));
#426160=CARTESIAN_POINT('Ctrl Pts',(1.79839570973538,1.97711691530823,12.5773203894503));
#426161=CARTESIAN_POINT('Ctrl Pts',(1.79544105532531,1.96567473517094,12.5969440695591));
#426162=CARTESIAN_POINT('Ctrl Pts',(1.79244523019807,1.96835495425879,12.5878292599214));
#426163=CARTESIAN_POINT('Ctrl Pts',(1.79242579995806,1.97705115553144,12.5813877129824));
#426164=CARTESIAN_POINT('Ctrl Pts',(1.7726948305681,1.98613896017059,12.596957478804));
#426165=CARTESIAN_POINT('Ctrl Pts',(1.77566856919067,1.98347860836047,12.5878468778671));
#426166=CARTESIAN_POINT('Ctrl Pts',(1.78428860046658,1.98438001988686,12.5814011370086));
#426167=CARTESIAN_POINT('Ctrl Pts',(1.7711196810305,2.00292758462508,12.5928371701607));
#426168=CARTESIAN_POINT('Ctrl Pts',(1.77165963219662,1.9946666210952,12.5821692192952));
#426169=CARTESIAN_POINT('Ctrl Pts',(1.78371852131355,1.99035303613215,12.5773318885715));
#426170=CARTESIAN_POINT('Ctrl Pts',(1.7746473336469,2.01291259190762,12.5893111709658));
#426171=CARTESIAN_POINT('Ctrl Pts',(1.77087180231219,2.00222596485788,12.5770542771492));
#426172=CARTESIAN_POINT('Ctrl Pts',(1.7850149677158,1.99399343503886,12.5737548217797));
#426173=CARTESIAN_POINT('',(1.80187416435296,1.97877177809493,12.5737548217797));
#426174=CARTESIAN_POINT('Origin',(1.812348011786,1.99027388746449,12.5893111709658));
#426175=CARTESIAN_POINT('Ctrl Pts',(1.7850149677158,1.99399343503886,12.5737548217797));
#426176=CARTESIAN_POINT('Ctrl Pts',(1.78465049077835,1.99305990614639,12.5746934679442));
#426177=CARTESIAN_POINT('Ctrl Pts',(1.78441781245114,1.99196027155514,12.5756680099006));
#426178=CARTESIAN_POINT('Ctrl Pts',(1.78434014704803,1.99082032780515,12.5765688348656));
#426179=CARTESIAN_POINT('Ctrl Pts',(1.78431958599235,1.99051854031693,12.5768073183026));
#426180=CARTESIAN_POINT('Ctrl Pts',(1.78430964476381,1.99021400706395,12.5770407398754));
#426181=CARTESIAN_POINT('Ctrl Pts',(1.78431019194782,1.98990909585803,12.5772674179684));
#426182=CARTESIAN_POINT('Ctrl Pts',(1.78431243744301,1.98865782272043,12.5781976435658));
#426183=CARTESIAN_POINT('Ctrl Pts',(1.7845027215256,1.98732913560501,12.5790594849312));
#426184=CARTESIAN_POINT('Ctrl Pts',(1.78491599739136,1.98601959531068,12.5797571720116));
#426185=CARTESIAN_POINT('Ctrl Pts',(1.78518526147797,1.98516638272206,12.580211740231));
#426186=CARTESIAN_POINT('Ctrl Pts',(1.78557932458009,1.9842881736058,12.5806009430798));
#426187=CARTESIAN_POINT('Ctrl Pts',(1.78608661038595,1.98345404305517,12.5808812374708));
#426188=CARTESIAN_POINT('Ctrl Pts',(1.78652253718349,1.98273724819225,12.5811221033394));
#426189=CARTESIAN_POINT('Ctrl Pts',(1.78705109550353,1.98203838779487,12.581287365893));
#426190=CARTESIAN_POINT('Ctrl Pts',(1.78764910283671,1.98140193629404,12.581359338449));
#426191=CARTESIAN_POINT('Ctrl Pts',(1.78773221350764,1.98131348267764,12.5813693411482));
#426192=CARTESIAN_POINT('Ctrl Pts',(1.7878166381272,1.9812261813044,12.5813775999465));
#426193=CARTESIAN_POINT('Ctrl Pts',(1.78790228728468,1.98114009656993,12.5813841266931));
#426194=CARTESIAN_POINT('Ctrl Pts',(1.78804760143938,1.98099404340616,12.5813952001081));
#426195=CARTESIAN_POINT('Ctrl Pts',(1.78819784532659,1.98085094361417,12.5814007534795));
#426196=CARTESIAN_POINT('Ctrl Pts',(1.78835308952209,1.98071100232073,12.5814005856065));
#426197=CARTESIAN_POINT('Ctrl Pts',(1.78906373675257,1.98007040579288,12.5813998171494));
#426198=CARTESIAN_POINT('Ctrl Pts',(1.78982983672742,1.97954000365373,12.58127954464));
#426199=CARTESIAN_POINT('Ctrl Pts',(1.79063019693062,1.97909847941628,12.5810700125799));
#426200=CARTESIAN_POINT('Ctrl Pts',(1.79159694092779,1.978565168409,12.5808169217085));
#426201=CARTESIAN_POINT('Ctrl Pts',(1.79262184164847,1.97817613515564,12.5804173076348));
#426202=CARTESIAN_POINT('Ctrl Pts',(1.79360583672341,1.97794112651723,12.5799304713245));
#426203=CARTESIAN_POINT('Ctrl Pts',(1.79482531661169,1.97764987677887,12.5793271277669));
#426204=CARTESIAN_POINT('Ctrl Pts',(1.79605013594142,1.97754580748505,12.5785808224116));
#426205=CARTESIAN_POINT('Ctrl Pts',(1.7972259810098,1.97760170236999,12.5777485681082));
#426206=CARTESIAN_POINT('Ctrl Pts',(1.79897811898514,1.97768499187229,12.576508418016));
#426207=CARTESIAN_POINT('Ctrl Pts',(1.8006070861551,1.97811590424151,12.5750928681475));
#426208=CARTESIAN_POINT('Ctrl Pts',(1.80187416435296,1.97877177809493,12.5737548217797));
#426209=CARTESIAN_POINT('Ctrl Pts',(1.80187416435296,1.97877177809493,12.5737548217797));
#426210=CARTESIAN_POINT('Ctrl Pts',(1.81150400521158,1.9655403821031,12.5770542771492));
#426211=CARTESIAN_POINT('Ctrl Pts',(1.82175065299146,1.97038443452176,12.5893111709658));
#426212=CARTESIAN_POINT('Ctrl Pts',(1.82423646848627,1.98939920995872,12.5508408821982));
#426213=CARTESIAN_POINT('Ctrl Pts',(1.83389354678749,1.97612492793244,12.55409748406));
#426214=CARTESIAN_POINT('Ctrl Pts',(1.84415326666565,1.98097516012137,12.5663972313419));
#426215=CARTESIAN_POINT('Ctrl Pts',(1.84657743375127,2.00001519483152,12.52790050457));
#426216=CARTESIAN_POINT('Ctrl Pts',(1.8562402070622,1.98668920183727,12.5311362602938));
#426217=CARTESIAN_POINT('Ctrl Pts',(1.86653327978389,1.99155520141915,12.5434568539655));
#426218=CARTESIAN_POINT('Ctrl Pts',(1.86889872439596,2.01062060978389,12.5049357605811));
#426219=CARTESIAN_POINT('Ctrl Pts',(1.87854845619206,1.99723531706192,12.5081700652078));
#426220=CARTESIAN_POINT('Ctrl Pts',(1.88889246242629,2.00212539521176,12.5204921097672));
#426221=CARTESIAN_POINT('Ctrl Pts',(1.86743302163657,2.00992421523262,12.5064436508395));
#426222=CARTESIAN_POINT('Ctrl Pts',(1.86845513267516,2.0092577793277,12.5062361689309));
#426223=CARTESIAN_POINT('Ctrl Pts',(1.86948962620598,2.00852115543782,12.5061871075061));
#426224=CARTESIAN_POINT('Ctrl Pts',(1.87044929103482,2.00775300176998,12.5063648335164));
#426225=CARTESIAN_POINT('Ctrl Pts',(1.87088522999466,2.00740405899237,12.5064455676329));
#426226=CARTESIAN_POINT('Ctrl Pts',(1.87131167054314,2.00704357090341,12.506574497099));
#426227=CARTESIAN_POINT('Ctrl Pts',(1.87170964971593,2.00668619154967,12.5067492519495));
#426228=CARTESIAN_POINT('Ctrl Pts',(1.87250940431204,2.00596802386589,12.5071004286051));
#426229=CARTESIAN_POINT('Ctrl Pts',(1.87322308901106,2.00523540423583,12.5076537929612));
#426230=CARTESIAN_POINT('Ctrl Pts',(1.87380391314577,2.00454991961107,12.5083435010503));
#426231=CARTESIAN_POINT('Ctrl Pts',(1.87384047949614,2.00450676425739,12.5083869222963));
#426232=CARTESIAN_POINT('Ctrl Pts',(1.87387651414162,2.00446378329956,12.5084308732336));
#426233=CARTESIAN_POINT('Ctrl Pts',(1.87391200368841,2.00442098689627,12.5084753333615));
#426234=CARTESIAN_POINT('Ctrl Pts',(1.87419667669519,2.0040777032563,12.508831962269));
#426235=CARTESIAN_POINT('Ctrl Pts',(1.87445304957996,2.00374014842688,12.509227847131));
#426236=CARTESIAN_POINT('Ctrl Pts',(1.87467572887406,2.00342005323096,12.5096423454524));
#426237=CARTESIAN_POINT('Ctrl Pts',(1.87537350722804,2.00241701655513,12.5109411997424));
#426238=CARTESIAN_POINT('Ctrl Pts',(1.87579129688352,2.00152924750102,12.5124831113042));
#426239=CARTESIAN_POINT('Ctrl Pts',(1.87602370028963,2.00075924286967,12.5140723025008));
#426240=CARTESIAN_POINT('Ctrl Pts',(1.87604547674333,2.00068709259235,12.5142212114565));
#426241=CARTESIAN_POINT('Ctrl Pts',(1.87606565350796,2.00061596660036,12.5143705582413));
#426242=CARTESIAN_POINT('Ctrl Pts',(1.87608432490054,2.00054586288349,12.5145201959299));
#426243=CARTESIAN_POINT('Ctrl Pts',(1.8763241867371,1.99964527626665,12.5164425148273));
#426244=CARTESIAN_POINT('Ctrl Pts',(1.87633420864846,1.99888530433253,12.518463520594));
#426245=CARTESIAN_POINT('Ctrl Pts',(1.87619265303285,1.99822108088482,12.5205025929157));
#426246=CARTESIAN_POINT('Ctrl Pts',(1.87611054516506,1.9978358049578,12.5216853356836));
#426247=CARTESIAN_POINT('Ctrl Pts',(1.87597806090256,1.99748333839948,12.5228750347131));
#426248=CARTESIAN_POINT('Ctrl Pts',(1.87581311669285,1.99716022656708,12.5240609649613));
#426249=CARTESIAN_POINT('Ctrl Pts',(1.87540826997908,1.99636716590881,12.5269717671327));
#426250=CARTESIAN_POINT('Ctrl Pts',(1.87478722148973,1.99573335382147,12.5299036066169));
#426251=CARTESIAN_POINT('Ctrl Pts',(1.87402081361849,1.99520888160956,12.532813300402));
#426252=CARTESIAN_POINT('Ctrl Pts',(1.8736528932137,1.99495710440875,12.5342101228452));
#426253=CARTESIAN_POINT('Ctrl Pts',(1.87325163696887,1.99473127187644,12.5356023438238));
#426254=CARTESIAN_POINT('Ctrl Pts',(1.87282490594716,1.99452953679089,12.5369868989719));
#426255=CARTESIAN_POINT('Origin',(13.3982603696714,7.43726248417796,-1.24070444298747));
#426256=CARTESIAN_POINT('Ctrl Pts',(1.79345244976558,2.06614052056676,12.5369868989719));
#426257=CARTESIAN_POINT('Ctrl Pts',(1.79858957599058,2.08059365994316,12.5369868989719));
#426258=CARTESIAN_POINT('Ctrl Pts',(1.78680432755982,2.09041156313634,12.5369868989719));
#426259=CARTESIAN_POINT('Ctrl Pts',(1.79518893695318,2.07102626910976,12.5218025310015));
#426260=CARTESIAN_POINT('Ctrl Pts',(1.79586264219775,2.08282465819253,12.5216901060418));
#426261=CARTESIAN_POINT('Ctrl Pts',(1.78684026345852,2.09038164758466,12.5161920673677));
#426262=CARTESIAN_POINT('Ctrl Pts',(1.8009799229424,2.07269975423603,12.5042015548895));
#426263=CARTESIAN_POINT('Ctrl Pts',(1.8001469768632,2.07907811968861,12.4980677368513));
#426264=CARTESIAN_POINT('Ctrl Pts',(1.79500493145329,2.08352223363022,12.4907278922778));
#426265=CARTESIAN_POINT('Ctrl Pts',(1.80931690205595,2.06236855130678,12.506463626192));
#426266=CARTESIAN_POINT('Ctrl Pts',(1.81363173058679,2.06728685315659,12.4999376786891));
#426267=CARTESIAN_POINT('Ctrl Pts',(1.81357903123004,2.0672267832507,12.4906970594712));
#426268=CARTESIAN_POINT('Origin',(1.77272292638574,2.07350848232323,12.5369868989719));
#426269=CARTESIAN_POINT('Origin',(1.77272292638574,2.07350848232323,14.));
#426270=CARTESIAN_POINT('Origin',(1.77272292638574,2.07350848232323,13.7435492065112));
#426271=CARTESIAN_POINT('Ctrl Pts',(1.7852183793995,2.04283397811842,13.793642941384));
#426272=CARTESIAN_POINT('Ctrl Pts',(1.78884579896665,2.05301965660783,13.8071662555867));
#426273=CARTESIAN_POINT('Ctrl Pts',(1.77381718571099,2.06102966080549,13.8103758687955));
#426274=CARTESIAN_POINT('Ctrl Pts',(1.79075515589145,2.05850579394497,13.7804579775006));
#426275=CARTESIAN_POINT('Ctrl Pts',(1.79522151068929,2.07107740269442,13.7901904343351));
#426276=CARTESIAN_POINT('Ctrl Pts',(1.78269924998341,2.08064029509048,13.7927914348262));
#426277=CARTESIAN_POINT('Ctrl Pts',(1.79401486454876,2.06773238173152,13.7597120340895));
#426278=CARTESIAN_POINT('Ctrl Pts',(1.79917829511383,2.08228319183858,13.7635825532445));
#426279=CARTESIAN_POINT('Ctrl Pts',(1.7879137077355,2.09221521012996,13.7651073818885));
#426280=CARTESIAN_POINT('Ctrl Pts',(1.79337653895405,2.06592560457833,13.7381884353898));
#426281=CARTESIAN_POINT('Ctrl Pts',(1.79841995688676,2.08013552527418,13.7368803041982));
#426282=CARTESIAN_POINT('Ctrl Pts',(1.78689211134467,2.08994870081916,13.7363986145813));
#426283=CARTESIAN_POINT('Origin',(1.76581841007508,2.05396527522749,13.7902182540695));
#426284=CARTESIAN_POINT('Ctrl Pts',(1.77464602171788,2.01290888077561,13.8235227101244));
#426285=CARTESIAN_POINT('Ctrl Pts',(1.77848006887388,2.02374782771363,13.8358800583119));
#426286=CARTESIAN_POINT('Ctrl Pts',(1.76410223015073,2.03198820408293,13.8390832900376));
#426287=CARTESIAN_POINT('Ctrl Pts',(1.77861929779921,2.02415522358009,13.8124254819052));
#426288=CARTESIAN_POINT('Ctrl Pts',(1.78246079035821,2.03501521969218,13.8247886449157));
#426289=CARTESIAN_POINT('Ctrl Pts',(1.7680563093333,2.04325122039067,13.8279860620657));
#426290=CARTESIAN_POINT('Ctrl Pts',(1.78259079318749,2.03539652613963,13.8013225099955));
#426291=CARTESIAN_POINT('Ctrl Pts',(1.78643792047172,2.04627244658305,13.8136962257787));
#426292=CARTESIAN_POINT('Ctrl Pts',(1.77200881372502,2.05450893268902,13.8168830918626));
#426293=CARTESIAN_POINT('Ctrl Pts',(1.78656057716672,2.04663298456234,13.7902140179785));
#426294=CARTESIAN_POINT('Ctrl Pts',(1.79041164683682,2.05752003944145,13.802602731458));
#426295=CARTESIAN_POINT('Ctrl Pts',(1.7759598069397,2.06576154877587,13.8057746032558));
#426296=CARTESIAN_POINT('Origin',(1.75390385047194,2.0202411596918,13.8235269408515));
#426297=CARTESIAN_POINT('Ctrl Pts',(1.82175065299146,1.97038443452176,13.8235269408515));
#426298=CARTESIAN_POINT('Ctrl Pts',(1.83242539604493,1.97543086687871,13.8362179249168));
#426299=CARTESIAN_POINT('Ctrl Pts',(1.84212563533929,1.96137496556683,13.8391868794938));
#426300=CARTESIAN_POINT('Ctrl Pts',(1.81198372774147,1.96576716857329,13.8400110824519));
#426301=CARTESIAN_POINT('Ctrl Pts',(1.82200437050368,1.96672036398564,13.8494522556837));
#426302=CARTESIAN_POINT('Ctrl Pts',(1.82600401312805,1.95387782738599,13.85569149686));
#426303=CARTESIAN_POINT('Ctrl Pts',(1.79569590492346,1.96544382062545,13.8586819406588));
#426304=CARTESIAN_POINT('Ctrl Pts',(1.79893678777804,1.96253646410141,13.868010383617));
#426305=CARTESIAN_POINT('Ctrl Pts',(1.79896300577732,1.95348703431776,13.8744918421245));
#426306=CARTESIAN_POINT('Ctrl Pts',(1.77243601591992,1.98637344225342,13.8587686893867));
#426307=CARTESIAN_POINT('Ctrl Pts',(1.76922393929173,1.98925488141718,13.8680909899357));
#426308=CARTESIAN_POINT('Ctrl Pts',(1.76024384221326,1.98833062064939,13.8745789365163));
#426309=CARTESIAN_POINT('Ctrl Pts',(1.77104270722445,2.00270971058003,13.8400379222776));
#426310=CARTESIAN_POINT('Ctrl Pts',(1.77096347703319,2.01277270995821,13.8494748685453));
#426311=CARTESIAN_POINT('Ctrl Pts',(1.75778673473655,2.01544377111672,13.8557104837033));
#426312=CARTESIAN_POINT('Ctrl Pts',(1.77464733364068,2.01291259190967,13.8235269408542));
#426313=CARTESIAN_POINT('Ctrl Pts',(1.77858060311121,2.02404569615164,13.8362179249195));
#426314=CARTESIAN_POINT('Ctrl Pts',(1.76361004954787,2.03226430491853,13.8391868794965));
#426315=CARTESIAN_POINT('Origin',(1.83115329419692,1.95049498157902,13.8235269408515));
#426316=CARTESIAN_POINT('Ctrl Pts',(1.85408274819248,1.98566927291083,13.7902140241682));
#426317=CARTESIAN_POINT('Ctrl Pts',(1.86452108917785,1.99060887136271,13.8026027327198));
#426318=CARTESIAN_POINT('Ctrl Pts',(1.87419128919243,1.97707132491028,13.8057746032556));
#426319=CARTESIAN_POINT('Ctrl Pts',(1.84330890615097,1.98057599199512,13.8013225161807));
#426320=CARTESIAN_POINT('Ctrl Pts',(1.85373657199566,1.98551053482259,13.8136962270464));
#426321=CARTESIAN_POINT('Ctrl Pts',(1.86339946013712,1.97199509187463,13.8168830918628));
#426322=CARTESIAN_POINT('Ctrl Pts',(1.83253041940917,1.97548051532018,13.8124254880875));
#426323=CARTESIAN_POINT('Ctrl Pts',(1.8429428174359,1.98040783126028,13.8247886461867));
#426324=CARTESIAN_POINT('Ctrl Pts',(1.85260271523098,1.96691683660509,13.8279860620656));
#426325=CARTESIAN_POINT('Ctrl Pts',(1.82174709993151,1.9703827539931,13.8235227163065));
#426326=CARTESIAN_POINT('Ctrl Pts',(1.8321393163066,1.97530051995441,13.8358800595847));
#426327=CARTESIAN_POINT('Ctrl Pts',(1.84180085423237,1.96183647465937,13.8390832900376));
#426328=CARTESIAN_POINT('Origin',(1.86348895370614,1.96578150581789,13.7902182540695));
#426329=CARTESIAN_POINT('Ctrl Pts',(1.87258094656285,1.99441417567843,13.7382347919292));
#426330=CARTESIAN_POINT('Ctrl Pts',(1.88621332095675,2.00088536081857,13.7369371795943));
#426331=CARTESIAN_POINT('Ctrl Pts',(1.89715200622395,1.99040256817324,13.7364597369711));
#426332=CARTESIAN_POINT('Ctrl Pts',(1.87429104030055,1.99522261453984,13.7595490285573));
#426333=CARTESIAN_POINT('Ctrl Pts',(1.88824910261822,2.00184728832458,13.7633824266925));
#426334=CARTESIAN_POINT('Ctrl Pts',(1.89927617763065,1.9916346844951,13.7648920890506));
#426335=CARTESIAN_POINT('Ctrl Pts',(1.86556965592157,1.99109962064379,13.7803806590111));
#426336=CARTESIAN_POINT('Ctrl Pts',(1.87764056553396,1.99683460339297,13.7901039518744));
#426337=CARTESIAN_POINT('Ctrl Pts',(1.88844505696549,1.98535643253125,13.7926933640892));
#426338=CARTESIAN_POINT('Ctrl Pts',(1.85040994304603,1.98393293681479,13.7936647693663));
#426339=CARTESIAN_POINT('Ctrl Pts',(1.86017494984539,1.98858245013912,13.8072068914933));
#426340=CARTESIAN_POINT('Ctrl Pts',(1.86967504497685,1.97442644567669,13.8104111085397));
#426341=CARTESIAN_POINT('Origin',(1.88222754715262,1.97464008384815,13.7435492065112));
#426342=CARTESIAN_POINT('Origin',(1.88222754715262,1.97464008384815,14.));
#426343=CARTESIAN_POINT('Origin',(1.88222754715262,1.97464008384815,12.5369868989719));
#426344=CARTESIAN_POINT('Ctrl Pts',(1.86742050886859,2.00991074771501,12.506462012331));
#426345=CARTESIAN_POINT('Ctrl Pts',(1.87187109728735,2.01470093045857,12.4999388158272));
#426346=CARTESIAN_POINT('Ctrl Pts',(1.87181844098977,2.01464425631477,12.4907030323752));
#426347=CARTESIAN_POINT('Ctrl Pts',(1.87854548738825,2.00266758293081,12.5042014951932));
#426348=CARTESIAN_POINT('Ctrl Pts',(1.88497272401356,2.00248946364943,12.4980716682127));
#426349=CARTESIAN_POINT('Ctrl Pts',(1.88991490294428,1.99783109133255,12.4907355092743));
#426350=CARTESIAN_POINT('Ctrl Pts',(1.87747281996563,1.99673672415271,12.5218047446509));
#426351=CARTESIAN_POINT('Ctrl Pts',(1.88913574228157,1.99860624654853,12.5216906929434));
#426352=CARTESIAN_POINT('Ctrl Pts',(1.89757045398399,1.99040707629619,12.5161988840776));
#426353=CARTESIAN_POINT('Ctrl Pts',(1.87279018957953,1.99451308769853,12.5369868989719));
#426354=CARTESIAN_POINT('Ctrl Pts',(1.88663796074585,2.00108916291449,12.5369868989719));
#426355=CARTESIAN_POINT('Ctrl Pts',(1.89760266204618,1.99037558009103,12.5369868989719));
#426356=CARTESIAN_POINT('Origin',(3.45247261328832E-31,-1.32797438156902E-31,
12.5));
#426357=CARTESIAN_POINT('Origin',(1.97629355154764,1.81533855233443,12.5));
#426358=CARTESIAN_POINT('',(1.97629355154764,1.81533855233443,12.5893111709658));
#426359=CARTESIAN_POINT('',(1.97629355154764,1.81533855233443,13.8235269408515));
#426360=CARTESIAN_POINT('',(1.97629355154764,1.81533855233443,12.5));
#426361=CARTESIAN_POINT('',(2.00976761045597,1.82793855548533,13.7902182540695));
#426362=CARTESIAN_POINT('',(1.97629355154764,1.81533855233443,13.8235269408515));
#426363=CARTESIAN_POINT('',(2.02916590912708,1.83524028800147,13.7435492065112));
#426364=CARTESIAN_POINT('Origin',(1.96534564815276,1.81121798941157,13.7445212918713));
#426365=CARTESIAN_POINT('',(2.02916590912708,1.83524028800147,12.5369868989719));
#426366=CARTESIAN_POINT('',(2.02916590912708,1.83524028800147,12.5));
#426367=CARTESIAN_POINT('Ctrl Pts',(2.02916590912708,1.83524028800147,12.5369868989719));
#426368=CARTESIAN_POINT('Ctrl Pts',(2.01155464389455,1.82861121448431,12.5544431401645));
#426369=CARTESIAN_POINT('Ctrl Pts',(1.99393078261705,1.82197739967757,12.5718848856037));
#426370=CARTESIAN_POINT('Ctrl Pts',(1.97629355154764,1.81533855233443,12.5893111709658));
#426371=CARTESIAN_POINT('Origin',(2.04525051714325,2.11252849155305,12.5));
#426372=CARTESIAN_POINT('',(1.95591164254692,1.91312070921222,13.7435492065112));
#426373=CARTESIAN_POINT('',(1.94743714763612,1.89420531270362,13.7902182540695));
#426374=CARTESIAN_POINT('Origin',(1.92516763969895,1.84449891991954,13.7418732680457));
#426375=CARTESIAN_POINT('',(1.9328134042516,1.86156455859736,13.8235269408515));
#426376=CARTESIAN_POINT('',(1.94743714763612,1.89420531270362,13.7902182540695));
#426377=CARTESIAN_POINT('',(1.9328134042516,1.86156455859736,12.5893111709658));
#426378=CARTESIAN_POINT('',(1.9328134042516,1.86156455859736,12.5));
#426379=CARTESIAN_POINT('',(1.95591164254692,1.91312070921222,12.5369868989719));
#426380=CARTESIAN_POINT('Ctrl Pts',(1.9328134042516,1.86156455859736,12.5893111709658));
#426381=CARTESIAN_POINT('Ctrl Pts',(1.94051854517517,1.87876272760424,12.5718848856037));
#426382=CARTESIAN_POINT('Ctrl Pts',(1.9482178452652,1.89594785964745,12.5544431401645));
#426383=CARTESIAN_POINT('Ctrl Pts',(1.95591164254692,1.91312070921222,12.5369868989719));
#426384=CARTESIAN_POINT('',(1.95591164254692,1.91312070921222,12.5));
#426385=CARTESIAN_POINT('Origin',(1.96418389587106,1.8475099194859,12.5));
#426386=CARTESIAN_POINT('',(1.93992567473915,1.82315568207856,13.8587068136939));
#426387=CARTESIAN_POINT('Ctrl Pts',(1.93281340424551,1.86156455859993,13.8235269408542));
#426388=CARTESIAN_POINT('Ctrl Pts',(1.93209695564616,1.85996541794582,13.8262006681044));
#426389=CARTESIAN_POINT('Ctrl Pts',(1.93152232902365,1.85825789568338,13.8288634856214));
#426390=CARTESIAN_POINT('Ctrl Pts',(1.93107988014874,1.85645120022672,13.8314912288862));
#426391=CARTESIAN_POINT('Ctrl Pts',(1.9306237609952,1.85458868356291,13.8342001611531));
#426392=CARTESIAN_POINT('Ctrl Pts',(1.93030712426365,1.85261882014791,13.8368750301949));
#426393=CARTESIAN_POINT('Ctrl Pts',(1.93015424774706,1.85052290557702,13.8394886372969));
#426394=CARTESIAN_POINT('Ctrl Pts',(1.93014244072286,1.85036103301074,13.8396904925131));
#426395=CARTESIAN_POINT('Ctrl Pts',(1.93013163198512,1.8501984031755,13.8398919674349));
#426396=CARTESIAN_POINT('Ctrl Pts',(1.93012184401954,1.85003500565352,13.8400930404591));
#426397=CARTESIAN_POINT('Ctrl Pts',(1.92996934093079,1.84748916233266,13.8432258934518));
#426398=CARTESIAN_POINT('Ctrl Pts',(1.93006429247672,1.84477001520775,13.8462331177034));
#426399=CARTESIAN_POINT('Ctrl Pts',(1.93050000938439,1.84196961473997,13.8489036603661));
#426400=CARTESIAN_POINT('Ctrl Pts',(1.93064258102727,1.84105329111701,13.849777493004));
#426401=CARTESIAN_POINT('Ctrl Pts',(1.93082174068276,1.84012849557507,13.85061494757));
#426402=CARTESIAN_POINT('Ctrl Pts',(1.93104104100592,1.83919910809192,13.8514076489583));
#426403=CARTESIAN_POINT('Ctrl Pts',(1.93150489281725,1.83723331952729,13.8530843267192));
#426404=CARTESIAN_POINT('Ctrl Pts',(1.93219676869563,1.83505457450409,13.8546805203176));
#426405=CARTESIAN_POINT('Ctrl Pts',(1.93320655849924,1.83283062365253,13.8559412814274));
#426406=CARTESIAN_POINT('Ctrl Pts',(1.93334170112321,1.83253298690417,13.8561100121513));
#426407=CARTESIAN_POINT('Ctrl Pts',(1.93348246408243,1.83223456159975,13.8562727473908));
#426408=CARTESIAN_POINT('Ctrl Pts',(1.93362898789057,1.8319357614268,13.8564289040185));
#426409=CARTESIAN_POINT('Ctrl Pts',(1.93429347168891,1.8305807060512,13.8571370725437));
#426410=CARTESIAN_POINT('Ctrl Pts',(1.93509015748347,1.82919512527606,13.8577210840553));
#426411=CARTESIAN_POINT('Ctrl Pts',(1.93601352014234,1.82784750570495,13.8581177131616));
#426412=CARTESIAN_POINT('Ctrl Pts',(1.93627357084825,1.82746796965008,13.8582294175695));
#426413=CARTESIAN_POINT('Ctrl Pts',(1.93654350595545,1.82709137486019,13.8583265086086));
#426414=CARTESIAN_POINT('Ctrl Pts',(1.93682280878238,1.82671905480949,13.8584082369006));
#426415=CARTESIAN_POINT('Ctrl Pts',(1.93722409204667,1.8261841307382,13.8585256585398));
#426416=CARTESIAN_POINT('Ctrl Pts',(1.93764995969372,1.82565157424543,13.8586122832068));
#426417=CARTESIAN_POINT('Ctrl Pts',(1.93808996565855,1.82513571279355,13.8586682984299));
#426418=CARTESIAN_POINT('Ctrl Pts',(1.93844192681403,1.82472307476775,13.8587131050557));
#426419=CARTESIAN_POINT('Ctrl Pts',(1.93880664326325,1.82431640916258,13.8587357943552));
#426420=CARTESIAN_POINT('Ctrl Pts',(1.93918453537355,1.82391600579203,13.8587355499465));
#426421=CARTESIAN_POINT('Ctrl Pts',(1.93942877605383,1.82365721554756,13.8587353919793));
#426422=CARTESIAN_POINT('Ctrl Pts',(1.93967585135178,1.82340381323412,13.8587257282814));
#426423=CARTESIAN_POINT('Ctrl Pts',(1.93992567473915,1.82315568207856,13.8587068136939));
#426424=CARTESIAN_POINT('Ctrl Pts',(1.93992567473915,1.82315568207856,13.8587068136939));
#426425=CARTESIAN_POINT('Ctrl Pts',(1.94074733024086,1.82233959223502,13.8586446046466));
#426426=CARTESIAN_POINT('Ctrl Pts',(1.94159867616829,1.82158045052351,13.858482427929));
#426427=CARTESIAN_POINT('Ctrl Pts',(1.94247697274657,1.82087472429757,13.8582284286032));
#426428=CARTESIAN_POINT('Ctrl Pts',(1.94337800286824,1.82015073128319,13.8579678548414));
#426429=CARTESIAN_POINT('Ctrl Pts',(1.94431055720462,1.81948238016756,13.857615680862));
#426430=CARTESIAN_POINT('Ctrl Pts',(1.9452322259631,1.81888814434975,13.8571944833187));
#426431=CARTESIAN_POINT('Ctrl Pts',(1.9475323446104,1.81740516809297,13.8561433417727));
#426432=CARTESIAN_POINT('Ctrl Pts',(1.94986966137666,1.81631038485339,13.8546163505475));
#426433=CARTESIAN_POINT('Ctrl Pts',(1.95205501115748,1.81552028157863,13.8528973491087));
#426434=CARTESIAN_POINT('Ctrl Pts',(1.95245424232062,1.81537594136721,13.8525833129073));
#426435=CARTESIAN_POINT('Ctrl Pts',(1.95284842052968,1.81524162944075,13.8522628768812));
#426436=CARTESIAN_POINT('Ctrl Pts',(1.9532364436131,1.81511666528624,13.851937733538));
#426437=CARTESIAN_POINT('Ctrl Pts',(1.95560604674767,1.8143535265327,13.8499521282529));
#426438=CARTESIAN_POINT('Ctrl Pts',(1.95798284629349,1.81386704156084,13.847639871647));
#426439=CARTESIAN_POINT('Ctrl Pts',(1.96022581626304,1.81360406933324,13.8452109780794));
#426440=CARTESIAN_POINT('Ctrl Pts',(1.96123497487951,1.81348575268478,13.8441181685877));
#426441=CARTESIAN_POINT('Ctrl Pts',(1.96221721067966,1.81341198361257,13.8430021611332));
#426442=CARTESIAN_POINT('Ctrl Pts',(1.96316141192108,1.81337510326563,13.8418824960098));
#426443=CARTESIAN_POINT('Ctrl Pts',(1.96538644625752,1.81328819378631,13.8392439765549));
#426444=CARTESIAN_POINT('Ctrl Pts',(1.96750648506154,1.81339820120145,13.8364981347964));
#426445=CARTESIAN_POINT('Ctrl Pts',(1.96952890831528,1.81367124188632,13.833693111342));
#426446=CARTESIAN_POINT('Ctrl Pts',(1.97149862012867,1.8139371661737,13.8309611966328));
#426447=CARTESIAN_POINT('Ctrl Pts',(1.97337763678728,1.81435856187097,13.8281701127186));
#426448=CARTESIAN_POINT('Ctrl Pts',(1.9751537092055,1.81493849112953,13.8253580685121));
#426449=CARTESIAN_POINT('Ctrl Pts',(1.97553876362257,1.81506422041867,13.8247484142933));
#426450=CARTESIAN_POINT('Ctrl Pts',(1.97591884297707,1.81519750791604,13.8241378483365));
#426451=CARTESIAN_POINT('Ctrl Pts',(1.97629355154764,1.81533855233443,13.8235269408515));
#426452=CARTESIAN_POINT('',(1.93906160401641,1.82404795930237,12.5969504640361));
#426453=CARTESIAN_POINT('Origin',(1.96420812976395,1.84753244505461,12.584524458991));
#426454=CARTESIAN_POINT('Origin',(1.96420812976395,1.84753244505461,12.584524458991));
#426455=CARTESIAN_POINT('Ctrl Pts',(1.9328134042516,1.86156455859736,12.5893111709658));
#426456=CARTESIAN_POINT('Ctrl Pts',(1.92817937637158,1.85122123127164,12.5770542771492));
#426457=CARTESIAN_POINT('Ctrl Pts',(1.94160445395171,1.84186329523733,12.5737548217797));
#426458=CARTESIAN_POINT('Ctrl Pts',(1.94294646799923,1.88418194413488,12.5663937883685));
#426459=CARTESIAN_POINT('Ctrl Pts',(1.93830652877308,1.8738254224587,12.5540940315304));
#426460=CARTESIAN_POINT('Ctrl Pts',(1.95177504421946,1.86444112243238,12.5508374392248));
#426461=CARTESIAN_POINT('Ctrl Pts',(1.95306930760976,1.90677650900767,12.5434499600945));
#426462=CARTESIAN_POINT('Ctrl Pts',(1.94841428228888,1.89638631459144,12.5311293540533));
#426463=CARTESIAN_POINT('Ctrl Pts',(1.96193462184618,1.88699737520424,12.5278936106989));
#426464=CARTESIAN_POINT('Ctrl Pts',(1.96318272395384,1.9293500407896,12.5204817579905));
#426465=CARTESIAN_POINT('Ctrl Pts',(1.95850465943888,1.91890842201175,12.5081597038247));
#426466=CARTESIAN_POINT('Ctrl Pts',(1.97208403014572,1.90953373609163,12.5049254088044));
#426467=CARTESIAN_POINT('Ctrl Pts',(1.95591164254692,1.91312070921222,12.5369868989719));
#426468=CARTESIAN_POINT('Ctrl Pts',(1.95629249981849,1.91397079680149,12.5342545179733));
#426469=CARTESIAN_POINT('Ctrl Pts',(1.9567698153956,1.91473107763987,12.5314872231885));
#426470=CARTESIAN_POINT('Ctrl Pts',(1.95736404522658,1.91532900072698,12.5287124745063));
#426471=CARTESIAN_POINT('Ctrl Pts',(1.95789995118309,1.9158682374452,12.5262100684184));
#426472=CARTESIAN_POINT('Ctrl Pts',(1.95853110429545,1.91627418582429,12.5237004536639));
#426473=CARTESIAN_POINT('Ctrl Pts',(1.95930420189151,1.91649806230449,12.5212220730815));
#426474=CARTESIAN_POINT('Ctrl Pts',(1.95989607497958,1.91666945911695,12.5193246583486));
#426475=CARTESIAN_POINT('Ctrl Pts',(1.96057839519032,1.91673557835099,12.517417831369));
#426476=CARTESIAN_POINT('Ctrl Pts',(1.96137945209482,1.91660339461804,12.5155812248347));
#426477=CARTESIAN_POINT('Ctrl Pts',(1.96172070664183,1.91654708363731,12.5147988205793));
#426478=CARTESIAN_POINT('Ctrl Pts',(1.9620839011163,1.91645500068317,12.5140295443047));
#426479=CARTESIAN_POINT('Ctrl Pts',(1.96247269185465,1.91632149220178,12.5132817086137));
#426480=CARTESIAN_POINT('Ctrl Pts',(1.96306107404274,1.91611944517581,12.5121499604604));
#426481=CARTESIAN_POINT('Ctrl Pts',(1.96371846161084,1.91581139533868,12.5110494206568));
#426482=CARTESIAN_POINT('Ctrl Pts',(1.96444074371445,1.91536032918333,12.5100666561695));
#426483=CARTESIAN_POINT('Ctrl Pts',(1.96485547643508,1.91510132803565,12.5095023550641));
#426484=CARTESIAN_POINT('Ctrl Pts',(1.96529605117817,1.91479162780768,12.5089719619137));
#426485=CARTESIAN_POINT('Ctrl Pts',(1.96575053684161,1.91443180831311,12.5085043804652));
#426486=CARTESIAN_POINT('Ctrl Pts',(1.96641561740914,1.91390525935259,12.5078201359221));
#426487=CARTESIAN_POINT('Ctrl Pts',(1.96712902738502,1.91325516380659,12.5072563000949));
#426488=CARTESIAN_POINT('Ctrl Pts',(1.96783670585242,1.91251933096337,12.5068768744332));
#426489=CARTESIAN_POINT('Ctrl Pts',(1.96834699074417,1.91198874482851,12.5066032824114));
#426490=CARTESIAN_POINT('Ctrl Pts',(1.96886330381797,1.91140430045091,12.5064197834844));
#426491=CARTESIAN_POINT('Ctrl Pts',(1.96935875000463,1.91080034608724,12.5063282718343));
#426492=CARTESIAN_POINT('Ctrl Pts',(1.97008194805089,1.90991875969581,12.5061946931565));
#426493=CARTESIAN_POINT('Ctrl Pts',(1.97077696382452,1.90897743427154,12.5062515701262));
#426494=CARTESIAN_POINT('Ctrl Pts',(1.97141310434388,1.90804397572488,12.5064436508398));
#426495=CARTESIAN_POINT('',(1.94160445395171,1.84186329523733,12.5737548217797));
#426496=CARTESIAN_POINT('Origin',(1.95289051888806,1.85256958956603,12.5893111709658));
#426497=CARTESIAN_POINT('Ctrl Pts',(1.97141310434388,1.90804397572488,12.5064436508398));
#426498=CARTESIAN_POINT('Ctrl Pts',(1.96700108769627,1.89824731829224,12.5164271754438));
#426499=CARTESIAN_POINT('Ctrl Pts',(1.96258713161899,1.88844686326359,12.5264061185523));
#426500=CARTESIAN_POINT('Ctrl Pts',(1.95817116866995,1.8786424765021,12.536380305637));
#426501=CARTESIAN_POINT('Ctrl Pts',(1.95265211063745,1.86638898159414,12.5488460165097));
#426502=CARTESIAN_POINT('Ctrl Pts',(1.94712991623282,1.85412934173728,12.5613043021964));
#426503=CARTESIAN_POINT('Ctrl Pts',(1.94160445395171,1.84186329523733,12.5737548217797));
#426504=CARTESIAN_POINT('Ctrl Pts',(1.97629355154764,1.81533855233443,12.5893111709658));
#426505=CARTESIAN_POINT('Ctrl Pts',(1.96568616340084,1.81134581501989,12.5770542771492));
#426506=CARTESIAN_POINT('Ctrl Pts',(1.9571668466509,1.82531810606213,12.5737548217797));
#426507=CARTESIAN_POINT('Ctrl Pts',(1.96639695066487,1.81161336314696,12.5928319619712));
#426508=CARTESIAN_POINT('Ctrl Pts',(1.95812049011114,1.81197889983995,12.5821634970843));
#426509=CARTESIAN_POINT('Ctrl Pts',(1.95356507962399,1.82395227603856,12.5773203894503));
#426510=CARTESIAN_POINT('Ctrl Pts',(1.94968761267752,1.81278900057586,12.5969440695591));
#426511=CARTESIAN_POINT('Ctrl Pts',(1.94692021864885,1.81570448901556,12.5878292599214));
#426512=CARTESIAN_POINT('Ctrl Pts',(1.94760967419668,1.8243733381408,12.5813877129824));
#426513=CARTESIAN_POINT('Ctrl Pts',(1.92868509842483,1.83503916103836,12.596957478804));
#426514=CARTESIAN_POINT('Ctrl Pts',(1.93143209880742,1.83214527402485,12.5878468778671));
#426515=CARTESIAN_POINT('Ctrl Pts',(1.94009692104806,1.83234107360529,12.5814011370086));
#426516=CARTESIAN_POINT('Ctrl Pts',(1.9284836188184,1.85190031204024,12.5928371701607));
#426517=CARTESIAN_POINT('Ctrl Pts',(1.92834842812283,1.84362282515232,12.5821692192952));
#426518=CARTESIAN_POINT('Ctrl Pts',(1.94001559506115,1.83834068187509,12.5773318885715));
#426519=CARTESIAN_POINT('Ctrl Pts',(1.93281340425155,1.86156455859738,12.5893111709658));
#426520=CARTESIAN_POINT('Ctrl Pts',(1.92817937637153,1.85122123127166,12.5770542771492));
#426521=CARTESIAN_POINT('Ctrl Pts',(1.94160445395166,1.84186329523735,12.5737548217797));
#426522=CARTESIAN_POINT('',(1.9571668466509,1.82531810606213,12.5737548217797));
#426523=CARTESIAN_POINT('Origin',(1.96854337191463,1.83592822731137,12.5893111709658));
#426524=CARTESIAN_POINT('Ctrl Pts',(1.94160445395166,1.84186329523735,12.5737548217797));
#426525=CARTESIAN_POINT('Ctrl Pts',(1.94116509850996,1.8409625808393,12.5746934679442));
#426526=CARTESIAN_POINT('Ctrl Pts',(1.94084356397299,1.83988557063518,12.5756680099006));
#426527=CARTESIAN_POINT('Ctrl Pts',(1.94067324099676,1.83875575040534,12.5765688348656));
#426528=CARTESIAN_POINT('Ctrl Pts',(1.94062814987434,1.83845664300701,12.5768073183026));
#426529=CARTESIAN_POINT('Ctrl Pts',(1.94059341943716,1.83815393336573,12.5770407398754));
#426530=CARTESIAN_POINT('Ctrl Pts',(1.94056911170652,1.83784999212612,12.5772674179684));
#426531=CARTESIAN_POINT('Ctrl Pts',(1.94046935935304,1.83660269946795,12.5781976435658));
#426532=CARTESIAN_POINT('Ctrl Pts',(1.94055070994621,1.83526292353006,12.5790594849312));
#426533=CARTESIAN_POINT('Ctrl Pts',(1.94085587097945,1.83392405480331,12.5797571720116));
#426534=CARTESIAN_POINT('Ctrl Pts',(1.94105469436521,1.8330517336864,12.580211740231));
#426535=CARTESIAN_POINT('Ctrl Pts',(1.941375864059,1.83214432693741,12.5806009430798));
#426536=CARTESIAN_POINT('Ctrl Pts',(1.94181347252961,1.83127162338478,12.5808812374708));
#426537=CARTESIAN_POINT('Ctrl Pts',(1.94218952338097,1.83052168151669,12.5811221033394));
#426538=CARTESIAN_POINT('Ctrl Pts',(1.94265935935651,1.82978206410965,12.581287365893));
#426539=CARTESIAN_POINT('Ctrl Pts',(1.94320350016378,1.8290989871994,12.581359338449));
#426540=CARTESIAN_POINT('Ctrl Pts',(1.94327912449992,1.82900405361388,12.5813693411482));
#426541=CARTESIAN_POINT('Ctrl Pts',(1.94335615233113,1.8289101613385,12.5813775999465));
#426542=CARTESIAN_POINT('Ctrl Pts',(1.94343449979307,1.82881738184242,12.5813841266931));
#426543=CARTESIAN_POINT('Ctrl Pts',(1.94356742573818,1.82865997020587,12.5813952001081));
#426544=CARTESIAN_POINT('Ctrl Pts',(1.94370550573972,1.82850510029502,12.5814007534795));
#426545=CARTESIAN_POINT('Ctrl Pts',(1.9438488268584,1.82835297080154,12.5814005856065));
#426546=CARTESIAN_POINT('Ctrl Pts',(1.94450489490482,1.82765658145918,12.5813998171494));
#426547=CARTESIAN_POINT('Ctrl Pts',(1.94522521304684,1.82706549992931,12.58127954464));
#426548=CARTESIAN_POINT('Ctrl Pts',(1.94598692179323,1.8265602080406,12.5810700125799));
#426549=CARTESIAN_POINT('Ctrl Pts',(1.94690697923139,1.82594987297112,12.5808169217085));
#426550=CARTESIAN_POINT('Ctrl Pts',(1.94789675985771,1.82547859527038,12.5804173076348));
#426551=CARTESIAN_POINT('Ctrl Pts',(1.94885832538448,1.82516416387024,12.5799304713245));
#426552=CARTESIAN_POINT('Ctrl Pts',(1.95005000799652,1.82477448430937,12.5793271277669));
#426553=CARTESIAN_POINT('Ctrl Pts',(1.95126226922739,1.8245709271515,12.5785808224116));
#426554=CARTESIAN_POINT('Ctrl Pts',(1.95243875772033,1.82453079376174,12.5777485681082));
#426555=CARTESIAN_POINT('Ctrl Pts',(1.95419185446875,1.82447099061405,12.576508418016));
#426556=CARTESIAN_POINT('Ctrl Pts',(1.95585052474333,1.82476769321095,12.5750928681475));
#426557=CARTESIAN_POINT('Ctrl Pts',(1.9571668466509,1.82531810606213,12.5737548217797));
#426558=CARTESIAN_POINT('Ctrl Pts',(1.9571668466509,1.82531810606213,12.5737548217797));
#426559=CARTESIAN_POINT('Ctrl Pts',(1.96568616340084,1.81134581501989,12.5770542771492));
#426560=CARTESIAN_POINT('Ctrl Pts',(1.97629355154764,1.81533855233443,12.5893111709658));
#426561=CARTESIAN_POINT('Ctrl Pts',(1.98032097641911,1.83408744063474,12.5508408821982));
#426562=CARTESIAN_POINT('Ctrl Pts',(1.98886394437141,1.82007018615336,12.55409748406));
#426563=CARTESIAN_POINT('Ctrl Pts',(1.99948486482878,1.82406801717812,12.5663972313419));
#426564=CARTESIAN_POINT('Ctrl Pts',(2.00345290528634,1.84284710562112,12.52790050457));
#426565=CARTESIAN_POINT('Ctrl Pts',(2.01199733437468,1.82877784803957,12.5311362602938));
#426566=CARTESIAN_POINT('Ctrl Pts',(2.02265278188567,1.83278867542623,12.5434568539655));
#426567=CARTESIAN_POINT('Ctrl Pts',(2.02656436345227,1.85159783952182,12.5049357605811));
#426568=CARTESIAN_POINT('Ctrl Pts',(2.03509096094202,1.83747054253206,12.5081700652078));
#426569=CARTESIAN_POINT('Ctrl Pts',(2.04579913511532,1.8415012168131,12.5204921097672));
#426570=CARTESIAN_POINT('Ctrl Pts',(2.02504677507696,1.85102323054778,12.5064436508395));
#426571=CARTESIAN_POINT('Ctrl Pts',(2.02601116441225,1.8502757006149,12.5062361689309));
#426572=CARTESIAN_POINT('Ctrl Pts',(2.02698217406567,1.84945720695371,12.5061871075061));
#426573=CARTESIAN_POINT('Ctrl Pts',(2.02787603403384,1.8486133876612,12.5063648335164));
#426574=CARTESIAN_POINT('Ctrl Pts',(2.02828208036695,1.8482300728896,12.5064455676329));
#426575=CARTESIAN_POINT('Ctrl Pts',(2.02867771884383,1.84783602543144,12.506574497099));
#426576=CARTESIAN_POINT('Ctrl Pts',(2.02904524403868,1.84744739623077,12.5067492519495));
#426577=CARTESIAN_POINT('Ctrl Pts',(2.02978380018397,1.84666643076658,12.5071004286051));
#426578=CARTESIAN_POINT('Ctrl Pts',(2.03043539485487,1.84587807693941,12.5076537929612));
#426579=CARTESIAN_POINT('Ctrl Pts',(2.03095841298454,1.8451475306491,12.5083435010503));
#426580=CARTESIAN_POINT('Ctrl Pts',(2.03099134010144,1.84510153839428,12.5083869222963));
#426581=CARTESIAN_POINT('Ctrl Pts',(2.03102375149753,1.8450557632939,12.5084308732336));
#426582=CARTESIAN_POINT('Ctrl Pts',(2.03105563465161,1.84501021656458,12.5084753333615));
#426583=CARTESIAN_POINT('Ctrl Pts',(2.03131137962889,1.84464487167977,12.508831962269));
#426584=CARTESIAN_POINT('Ctrl Pts',(2.03153938560174,1.84428754326604,12.509227847131));
#426585=CARTESIAN_POINT('Ctrl Pts',(2.03173523321877,1.84395036273076,12.5096423454524));
#426586=CARTESIAN_POINT('Ctrl Pts',(2.03234893297202,1.84289378816302,12.5109411997424));
#426587=CARTESIAN_POINT('Ctrl Pts',(2.03269297104733,1.84197491935171,12.5124831113042));
#426588=CARTESIAN_POINT('Ctrl Pts',(2.03286183862445,1.84118853381212,12.5140723025008));
#426589=CARTESIAN_POINT('Ctrl Pts',(2.03287766170138,1.84111484862576,12.5142212114565));
#426590=CARTESIAN_POINT('Ctrl Pts',(2.03289197390084,1.84104231470602,12.5143705582413));
#426591=CARTESIAN_POINT('Ctrl Pts',(2.03290486906217,1.84097092236164,12.5145201959299));
#426592=CARTESIAN_POINT('Ctrl Pts',(2.03307052660835,1.84005378140603,12.5164425148273));
#426593=CARTESIAN_POINT('Ctrl Pts',(2.03301857040475,1.83929552133701,12.518463520594));
#426594=CARTESIAN_POINT('Ctrl Pts',(2.03282334542645,1.83864504613485,12.5205025929157));
#426595=CARTESIAN_POINT('Ctrl Pts',(2.03271010720103,1.83826774473516,12.5216853356836));
#426596=CARTESIAN_POINT('Ctrl Pts',(2.03254933447234,1.83792724967755,12.5228750347131));
#426597=CARTESIAN_POINT('Ctrl Pts',(2.03235860248692,1.83761865745748,12.5240609649613));
#426598=CARTESIAN_POINT('Ctrl Pts',(2.03189046106112,1.83686123440871,12.5269717671326));
#426599=CARTESIAN_POINT('Ctrl Pts',(2.03121981749025,1.83628015249623,12.5299036066169));
#426600=CARTESIAN_POINT('Ctrl Pts',(2.03041321042375,1.83581989477883,12.5328133004019));
#426601=CARTESIAN_POINT('Ctrl Pts',(2.0300259920645,1.83559894427448,12.5342101228451));
#426602=CARTESIAN_POINT('Ctrl Pts',(2.02960766351881,1.83540656929033,12.5356023438238));
#426603=CARTESIAN_POINT('Ctrl Pts',(2.02916590912708,1.83524028800147,12.5369868989719));
#426604=CARTESIAN_POINT('Origin',(13.9600593447379,6.32049840735972,-1.24090551502508));
#426605=CARTESIAN_POINT('Ctrl Pts',(1.95589451822736,1.91308258417306,12.5369868989719));
#426606=CARTESIAN_POINT('Ctrl Pts',(1.96219261612419,1.9270689084424,12.5369868989719));
#426607=CARTESIAN_POINT('Ctrl Pts',(1.95124683239059,1.93781475052863,12.5369868989719));
#426608=CARTESIAN_POINT('Ctrl Pts',(1.95802346126042,1.91781053596428,12.5218025310015));
#426609=CARTESIAN_POINT('Ctrl Pts',(1.95965660304747,1.92951475364883,12.5216901060418));
#426610=CARTESIAN_POINT('Ctrl Pts',(1.95128021032037,1.93778200540912,12.5161920673677));
#426611=CARTESIAN_POINT('Ctrl Pts',(1.96393158279513,1.91900643358783,12.5042015548895));
#426612=CARTESIAN_POINT('Ctrl Pts',(1.96362130427354,1.92543146839368,12.4980677368512));
#426613=CARTESIAN_POINT('Ctrl Pts',(1.95885860513893,1.93027991935011,12.4907278922778));
#426614=CARTESIAN_POINT('Ctrl Pts',(1.97139873234952,1.90803006568957,12.506463626192));
#426615=CARTESIAN_POINT('Ctrl Pts',(1.97610009090441,1.91258030371353,12.4999376786891));
#426616=CARTESIAN_POINT('Ctrl Pts',(1.97604267064543,1.9125247291721,12.4906970594712));
#426617=CARTESIAN_POINT('Origin',(1.93583452791047,1.92211567824355,12.5369868989719));
#426618=CARTESIAN_POINT('Origin',(1.93583452791047,1.92211567824355,14.));
#426619=CARTESIAN_POINT('Origin',(1.93583452791047,1.92211567824355,13.7435492065112));
#426620=CARTESIAN_POINT('Ctrl Pts',(1.94578814647423,1.89052474549827,13.793642941384));
#426621=CARTESIAN_POINT('Ctrl Pts',(1.95023372345813,1.90038086361272,13.8071662555867));
#426622=CARTESIAN_POINT('Ctrl Pts',(1.93590800637666,1.90958918668137,13.8103758687955));
#426623=CARTESIAN_POINT('Ctrl Pts',(1.95258389827906,1.90569311596547,13.7804579775006));
#426624=CARTESIAN_POINT('Ctrl Pts',(1.95806009447194,1.91785884434426,13.7901904343351));
#426625=CARTESIAN_POINT('Ctrl Pts',(1.94635896506339,1.92841059750327,13.7927914348263));
#426626=CARTESIAN_POINT('Ctrl Pts',(1.95658481308477,1.91462330652505,13.7597120340895));
#426627=CARTESIAN_POINT('Ctrl Pts',(1.96291708886745,1.92870483248585,13.7635825532445));
#426628=CARTESIAN_POINT('Ctrl Pts',(1.95249953516948,1.93952197125236,13.7651073818884));
#426629=CARTESIAN_POINT('Ctrl Pts',(1.95580134235455,1.91287457073571,13.7381884353898));
#426630=CARTESIAN_POINT('Ctrl Pts',(1.96198621918532,1.92662612371035,13.7368803041982));
#426631=CARTESIAN_POINT('Ctrl Pts',(1.95129659650628,1.93734627315421,13.7363986145813));
#426632=CARTESIAN_POINT('Origin',(1.92736003299966,1.90320028173495,13.7902182540695));
#426633=CARTESIAN_POINT('Ctrl Pts',(1.93281179419615,1.86156096674826,13.8235227101244));
#426634=CARTESIAN_POINT('Ctrl Pts',(1.93751655867584,1.87205133754772,13.8358800583119));
#426635=CARTESIAN_POINT('Ctrl Pts',(1.92385822819898,1.88143622207771,13.8390832900376));
#426636=CARTESIAN_POINT('Ctrl Pts',(1.93768853087362,1.8724460293881,13.8124254819052));
#426637=CARTESIAN_POINT('Ctrl Pts',(1.94240243168542,1.88295677245277,13.8247886449158));
#426638=CARTESIAN_POINT('Ctrl Pts',(1.92871719089907,1.89233946746655,13.8279860620657));
#426639=CARTESIAN_POINT('Ctrl Pts',(1.94256308195636,1.88332621369697,13.8013225099955));
#426640=CARTESIAN_POINT('Ctrl Pts',(1.94728389672519,1.89385236882366,13.8136962257787));
#426641=CARTESIAN_POINT('Ctrl Pts',(1.93357415172232,1.90323755485475,13.8168830918626));
#426642=CARTESIAN_POINT('Ctrl Pts',(1.94743553248254,1.89420170948327,13.7902140179785));
#426643=CARTESIAN_POINT('Ctrl Pts',(1.95216118407913,1.90473864065568,13.802602731458));
#426644=CARTESIAN_POINT('Ctrl Pts',(1.93842919100827,1.91413068616362,13.8057746032558));
#426645=CARTESIAN_POINT('Origin',(1.91273628961514,1.87055952762869,13.8235269408515));
#426646=CARTESIAN_POINT('Ctrl Pts',(1.97629355154764,1.81533855233443,13.8235269408515));
#426647=CARTESIAN_POINT('Ctrl Pts',(1.98734410636009,1.81949810244568,13.8362179249168));
#426648=CARTESIAN_POINT('Ctrl Pts',(1.99586638246287,1.80469831143077,13.8391868794938));
#426649=CARTESIAN_POINT('Ctrl Pts',(1.96618277489624,1.81153274503707,13.8400110824519));
#426650=CARTESIAN_POINT('Ctrl Pts',(1.97624776907141,1.81166599335812,13.8494522556836));
#426651=CARTESIAN_POINT('Ctrl Pts',(1.97918731725781,1.79854018123482,13.85569149686));
#426652=CARTESIAN_POINT('Ctrl Pts',(1.9499227926055,1.81253808177131,13.8586819406588));
#426653=CARTESIAN_POINT('Ctrl Pts',(1.95291591514243,1.80937623719673,13.868010383617));
#426654=CARTESIAN_POINT('Ctrl Pts',(1.95220443336531,1.80035478163383,13.8744918421245));
#426655=CARTESIAN_POINT('Ctrl Pts',(1.92844625742762,1.83529395869795,13.8587686893867));
#426656=CARTESIAN_POINT('Ctrl Pts',(1.92547973276126,1.83842762417526,13.8680909899357));
#426657=CARTESIAN_POINT('Ctrl Pts',(1.91645418038201,1.83823840008797,13.8745789365162));
#426658=CARTESIAN_POINT('Ctrl Pts',(1.92838914237902,1.85168943703289,13.8400379222776));
#426659=CARTESIAN_POINT('Ctrl Pts',(1.92913040368935,1.86172541060687,13.8494748685453));
#426660=CARTESIAN_POINT('Ctrl Pts',(1.91621522219703,1.86546161085383,13.8557104837033));
#426661=CARTESIAN_POINT('Ctrl Pts',(1.93281340424551,1.86156455859993,13.8235269408542));
#426662=CARTESIAN_POINT('Ctrl Pts',(1.93764103743677,1.87234002037941,13.8362179249195));
#426663=CARTESIAN_POINT('Ctrl Pts',(1.92339019006777,1.88175152149887,13.8391868794965));
#426664=CARTESIAN_POINT('Origin',(1.98404373118065,1.79474887735749,13.8235269408515));
#426665=CARTESIAN_POINT('Ctrl Pts',(2.00976392059532,1.82793716576927,13.7902140241683));
#426666=CARTESIAN_POINT('Ctrl Pts',(2.02057015199298,1.83200950641964,13.8026027327198));
#426667=CARTESIAN_POINT('Ctrl Pts',(2.02910473950242,1.81772879396133,13.8057746032556));
#426668=CARTESIAN_POINT('Ctrl Pts',(1.99861077794605,1.82373900047149,13.8013225161808));
#426669=CARTESIAN_POINT('Ctrl Pts',(2.0094059576434,1.8278071724427,13.8136962270464));
#426670=CARTESIAN_POINT('Ctrl Pts',(2.01793505925016,1.8135490859268,13.8168830918628));
#426671=CARTESIAN_POINT('Ctrl Pts',(1.98745282707664,1.81953902530688,13.8124254880875));
#426672=CARTESIAN_POINT('Ctrl Pts',(1.99823220069998,1.82360123890651,13.8247886461867));
#426673=CARTESIAN_POINT('Ctrl Pts',(2.00676031467335,1.80936776307468,13.8279860620656));
#426674=CARTESIAN_POINT('Ctrl Pts',(1.97628987333152,1.81533716700497,13.8235227163066));
#426675=CARTESIAN_POINT('Ctrl Pts',(1.98704835404407,1.81939150739452,13.8358800595847));
#426676=CARTESIAN_POINT('Ctrl Pts',(1.99558029931377,1.80518475756521,13.8390832900376));
#426677=CARTESIAN_POINT('Origin',(2.01751779008898,1.80734888050839,13.7902182540695));
#426678=CARTESIAN_POINT('Ctrl Pts',(2.02891335849587,1.83514519569823,13.7382347919292));
#426679=CARTESIAN_POINT('Ctrl Pts',(2.04302783395304,1.84048368343377,13.7369371795943));
#426680=CARTESIAN_POINT('Ctrl Pts',(2.05307567672931,1.8291441670171,13.7364597369711));
#426681=CARTESIAN_POINT('Ctrl Pts',(2.03068365731009,1.83581155603065,13.7595490285574));
#426682=CARTESIAN_POINT('Ctrl Pts',(2.0451352477408,1.84127647510066,13.7633824266926));
#426683=CARTESIAN_POINT('Ctrl Pts',(2.0552932090495,1.83019904388407,13.7648920890506));
#426684=CARTESIAN_POINT('Ctrl Pts',(2.02165523033963,1.83241315484894,13.7803806590111));
#426685=CARTESIAN_POINT('Ctrl Pts',(2.03415342933113,1.83714516372188,13.7901039518744));
#426686=CARTESIAN_POINT('Ctrl Pts',(2.04398639222538,1.82482451917112,13.7926933640891));
#426687=CARTESIAN_POINT('Ctrl Pts',(2.00596180889381,1.82650597490444,13.7936647693663));
#426688=CARTESIAN_POINT('Ctrl Pts',(2.01607330193851,1.8303440786487,13.8072068914933));
#426689=CARTESIAN_POINT('Ctrl Pts',(2.0243879405055,1.81546083117553,13.8104111085397));
#426690=CARTESIAN_POINT('Origin',(2.03691608876009,1.81465061302453,13.7435492065112));
#426691=CARTESIAN_POINT('Origin',(2.03691608876009,1.81465061302453,14.));
#426692=CARTESIAN_POINT('Origin',(2.03691608876009,1.81465061302453,12.5369868989719));
#426693=CARTESIAN_POINT('Ctrl Pts',(2.02503320621647,1.85101082774899,12.506462012331));
#426694=CARTESIAN_POINT('Ctrl Pts',(2.02985943003291,1.85542230728125,12.4999388158272));
#426695=CARTESIAN_POINT('Ctrl Pts',(2.02980232947595,1.85537011369308,12.4907030323752));
#426696=CARTESIAN_POINT('Ctrl Pts',(2.03553078211568,1.84288497496945,12.5042014951932));
#426697=CARTESIAN_POINT('Ctrl Pts',(2.04192211426631,1.84218356891276,12.4980716682127));
#426698=CARTESIAN_POINT('Ctrl Pts',(2.04646814791431,1.8371378634817,12.4907355092744));
#426699=CARTESIAN_POINT('Ctrl Pts',(2.03397826385555,1.83706128298778,12.5218047446509));
#426700=CARTESIAN_POINT('Ctrl Pts',(2.04575476219069,1.83797394826004,12.5216906929434));
#426701=CARTESIAN_POINT('Ctrl Pts',(2.0534930995928,1.82911455276253,12.5161988840775));
#426702=CARTESIAN_POINT('Ctrl Pts',(2.02912996752156,1.83522672334837,12.5369868989719));
#426703=CARTESIAN_POINT('Ctrl Pts',(2.0434676725511,1.84065219531004,12.5369868989719));
#426704=CARTESIAN_POINT('Ctrl Pts',(2.05352263325222,1.82908053610232,12.5369868989719));
#426705=CARTESIAN_POINT('Origin',(3.75266718462565E-31,-1.62210662334638E-31,
12.5));
#426706=CARTESIAN_POINT('Origin',(2.11768454258375,1.6482118915911,12.5));
#426707=CARTESIAN_POINT('',(2.11768454258375,1.6482118915911,12.5893111709658));
#426708=CARTESIAN_POINT('',(2.11768454258375,1.6482118915911,13.8235269408515));
#426709=CARTESIAN_POINT('',(2.11768454258375,1.6482118915911,12.5));
#426710=CARTESIAN_POINT('',(2.152074236552,1.65804152271191,13.7902182540695));
#426711=CARTESIAN_POINT('',(2.11768454258375,1.6482118915911,13.8235269408515));
#426712=CARTESIAN_POINT('',(2.17200314797058,1.66373781788874,13.7435492065112));
#426713=CARTESIAN_POINT('Origin',(2.10643720329692,1.64499739526187,13.7445212918691));
#426714=CARTESIAN_POINT('',(2.17200314797058,1.66373781788874,12.5369868989719));
#426715=CARTESIAN_POINT('',(2.17200314797058,1.66373781788874,12.5));
#426716=CARTESIAN_POINT('Ctrl Pts',(2.17200314797058,1.66373781788874,12.5369868989719));
#426717=CARTESIAN_POINT('Ctrl Pts',(2.15391015173731,1.6585662836783,12.5544431401645));
#426718=CARTESIAN_POINT('Ctrl Pts',(2.13580421491226,1.65339105064915,12.5718848856037));
#426719=CARTESIAN_POINT('Ctrl Pts',(2.11768454258375,1.6482118915911,12.5893111709658));
#426720=CARTESIAN_POINT('Origin',(2.210635798588,1.93879232294214,12.5));
#426721=CARTESIAN_POINT('',(2.10534060625464,1.74733000120831,13.7435492065112));
#426722=CARTESIAN_POINT('',(2.09535252910913,1.72916829412978,13.7902182540695));
#426723=CARTESIAN_POINT('Origin',(2.06910558865603,1.68144246689875,13.7418732680435));
#426724=CARTESIAN_POINT('',(2.07811692054271,1.69782812028618,13.8235269408515));
#426725=CARTESIAN_POINT('',(2.09535252910913,1.72916829412978,13.7902182540695));
#426726=CARTESIAN_POINT('',(2.07811692054271,1.69782812028618,12.5893111709658));
#426727=CARTESIAN_POINT('',(2.07811692054271,1.69782812028618,12.5));
#426728=CARTESIAN_POINT('',(2.10534060625464,1.74733000120831,12.5369868989719));
#426729=CARTESIAN_POINT('Ctrl Pts',(2.07811692054271,1.69782812028618,12.5893111709658));
#426730=CARTESIAN_POINT('Ctrl Pts',(2.08719823367956,1.71434102328813,12.5718848856037));
#426731=CARTESIAN_POINT('Ctrl Pts',(2.09627266278419,1.73084140878799,12.5544431401645));
#426732=CARTESIAN_POINT('Ctrl Pts',(2.10534060625464,1.74733000120831,12.5369868989719));
#426733=CARTESIAN_POINT('',(2.10534060625464,1.74733000120831,12.5));
#426734=CARTESIAN_POINT('Origin',(2.10823744587471,1.68126326053052,12.5));
#426735=CARTESIAN_POINT('',(2.08207484552998,1.65896733006374,13.8587068136939));
#426736=CARTESIAN_POINT('Ctrl Pts',(2.07811692053685,1.69782812028924,13.8235269408542));
#426737=CARTESIAN_POINT('Ctrl Pts',(2.07727251105211,1.69629269785577,13.8262006681044));
#426738=CARTESIAN_POINT('Ctrl Pts',(2.07656061753603,1.69463769463711,13.8288634856214));
#426739=CARTESIAN_POINT('Ctrl Pts',(2.07597237842099,1.69287307450134,13.8314912288862));
#426740=CARTESIAN_POINT('Ctrl Pts',(2.07536596456744,1.69105393315349,13.8342001611531));
#426741=CARTESIAN_POINT('Ctrl Pts',(2.07488981926285,1.68911643312964,13.8368750301949));
#426742=CARTESIAN_POINT('Ctrl Pts',(2.07456661493521,1.68703995339693,13.8394886372969));
#426743=CARTESIAN_POINT('Ctrl Pts',(2.074541653081,1.68687958183033,13.8396904925131));
#426744=CARTESIAN_POINT('Ctrl Pts',(2.0745176244671,1.68671837414493,13.8398919674349));
#426745=CARTESIAN_POINT('Ctrl Pts',(2.07449455065522,1.68655631812479,13.8400930404591));
#426746=CARTESIAN_POINT('Ctrl Pts',(2.0741350451428,1.68403137630506,13.8432258934518));
#426747=CARTESIAN_POINT('Ctrl Pts',(2.07400804501129,1.68131353748541,13.8462331177034));
#426748=CARTESIAN_POINT('Ctrl Pts',(2.07421405347112,1.67848694014619,13.8489036603661));
#426749=CARTESIAN_POINT('Ctrl Pts',(2.07428146183661,1.67756204460203,13.8497774930041));
#426750=CARTESIAN_POINT('Ctrl Pts',(2.07438464593108,1.67662572306582,13.85061494757));
#426751=CARTESIAN_POINT('Ctrl Pts',(2.07452746284261,1.67568155303062,13.8514076489583));
#426752=CARTESIAN_POINT('Ctrl Pts',(2.0748295412078,1.67368449723647,13.8530843267192));
#426753=CARTESIAN_POINT('Ctrl Pts',(2.07534152698039,1.67145660750048,13.8546805203176));
#426754=CARTESIAN_POINT('Ctrl Pts',(2.07616668415117,1.6691577494185,13.8559412814273));
#426755=CARTESIAN_POINT('Ctrl Pts',(2.0762771169411,1.6688500876534,13.8561100121513));
#426756=CARTESIAN_POINT('Ctrl Pts',(2.07639308709043,1.66854118184659,13.8562727473908));
#426757=CARTESIAN_POINT('Ctrl Pts',(2.07651476836467,1.66823143285592,13.8564289040185));
#426758=CARTESIAN_POINT('Ctrl Pts',(2.07706659155516,1.66682672471698,13.8571370725437));
#426759=CARTESIAN_POINT('Ctrl Pts',(2.07774768874718,1.66538081705924,13.8577210840554));
#426760=CARTESIAN_POINT('Ctrl Pts',(2.07855813548723,1.66396241895231,13.8581177131616));
#426761=CARTESIAN_POINT('Ctrl Pts',(2.07878638518395,1.66356294922562,13.8582294175695));
#426762=CARTESIAN_POINT('Ctrl Pts',(2.07902472613285,1.66316560530663,13.8583265086086));
#426763=CARTESIAN_POINT('Ctrl Pts',(2.07927275206209,1.66277175834687,13.8584082369006));
#426764=CARTESIAN_POINT('Ctrl Pts',(2.07962909881161,1.66220590587992,13.8585256585398));
#426765=CARTESIAN_POINT('Ctrl Pts',(2.08001014112102,1.66164040925815,13.8586122832068));
#426766=CARTESIAN_POINT('Ctrl Pts',(2.08040663550495,1.66109039972175,13.8586682984299));
#426767=CARTESIAN_POINT('Ctrl Pts',(2.08072379170887,1.66065044661331,13.8587131050557));
#426768=CARTESIAN_POINT('Ctrl Pts',(2.08105414757208,1.66021540637792,13.8587357943552));
#426769=CARTESIAN_POINT('Ctrl Pts',(2.08139814568569,1.65978553360139,13.8587355499465));
#426770=CARTESIAN_POINT('Ctrl Pts',(2.08162047986781,1.65950769657728,13.8587353919793));
#426771=CARTESIAN_POINT('Ctrl Pts',(2.08184607840205,1.65923499850864,13.8587257282814));
#426772=CARTESIAN_POINT('Ctrl Pts',(2.08207484552998,1.65896733006374,13.8587068136939));
#426773=CARTESIAN_POINT('Ctrl Pts',(2.08207484552998,1.65896733006374,13.8587068136939));
#426774=CARTESIAN_POINT('Ctrl Pts',(2.08282724814235,1.65808698314053,13.8586446046466));
#426775=CARTESIAN_POINT('Ctrl Pts',(2.08361388418944,1.65726097481382,13.858482427929));
#426776=CARTESIAN_POINT('Ctrl Pts',(2.08443173506927,1.65648600750882,13.8582284286032));
#426777=CARTESIAN_POINT('Ctrl Pts',(2.08527075493565,1.6556909812018,13.8579678548414));
#426778=CARTESIAN_POINT('Ctrl Pts',(2.08614572945382,1.65494884213355,13.857615680862));
#426779=CARTESIAN_POINT('Ctrl Pts',(2.08701589569976,1.65428145902623,13.8571944833187));
#426780=CARTESIAN_POINT('Ctrl Pts',(2.08918748455982,1.65261593622757,13.8561433417727));
#426781=CARTESIAN_POINT('Ctrl Pts',(2.09142778909988,1.65133428277386,13.8546163505474));
#426782=CARTESIAN_POINT('Ctrl Pts',(2.09354146655774,1.65036868220764,13.8528973491086));
#426783=CARTESIAN_POINT('Ctrl Pts',(2.09392760424489,1.65019228123029,13.8525833129072));
#426784=CARTESIAN_POINT('Ctrl Pts',(2.09430952318956,1.65002628703228,13.8522628768812));
#426785=CARTESIAN_POINT('Ctrl Pts',(2.09468606941946,1.64987011120217,13.851937733538));
#426786=CARTESIAN_POINT('Ctrl Pts',(2.09698558500203,1.64891636707609,13.8499521282529));
#426787=CARTESIAN_POINT('Ctrl Pts',(2.09931482290192,1.64823776961473,13.847639871647));
#426788=CARTESIAN_POINT('Ctrl Pts',(2.10152889489607,1.64779284953028,13.8452109780794));
#426789=CARTESIAN_POINT('Ctrl Pts',(2.10252505171524,1.6475926707749,13.8441181685877));
#426790=CARTESIAN_POINT('Ctrl Pts',(2.10349800634257,1.64743908582684,13.8430021611332));
#426791=CARTESIAN_POINT('Ctrl Pts',(2.1044360597416,1.64732536702951,13.8418824960098));
#426792=CARTESIAN_POINT('Ctrl Pts',(2.10664660653044,1.64705738577968,13.8392439765549));
#426793=CARTESIAN_POINT('Ctrl Pts',(2.10876855770583,1.6469942243102,13.8364981347964));
#426794=CARTESIAN_POINT('Ctrl Pts',(2.11080650686364,1.64710151020428,13.8336931113419));
#426795=CARTESIAN_POINT('Ctrl Pts',(2.11279133992161,1.64720599985183,13.8309611966328));
#426796=CARTESIAN_POINT('Ctrl Pts',(2.11469845196866,1.64747283608806,13.8281701127186));
#426797=CARTESIAN_POINT('Ctrl Pts',(2.1165158842708,1.64790606928952,13.8253580685121));
#426798=CARTESIAN_POINT('Ctrl Pts',(2.11690990555534,1.64799999471516,13.8247484142933));
#426799=CARTESIAN_POINT('Ctrl Pts',(2.11729958439555,1.6481018587135,13.8241378483365));
#426800=CARTESIAN_POINT('Ctrl Pts',(2.11768454258375,1.6482118915911,13.8235269408515));
#426801=CARTESIAN_POINT('',(2.08128637880857,1.65992706809418,12.5969504640361));
#426802=CARTESIAN_POINT('Origin',(2.10826343517428,1.68128373586001,12.584524458991));
#426803=CARTESIAN_POINT('Origin',(2.10826343517428,1.68128373586001,12.584524458991));
#426804=CARTESIAN_POINT('Ctrl Pts',(2.07811692054271,1.69782812028618,12.5893111709658));
#426805=CARTESIAN_POINT('Ctrl Pts',(2.07265523480837,1.68789692582132,12.5770542771492));
#426806=CARTESIAN_POINT('Ctrl Pts',(2.08527288288871,1.67747585909206,12.5737548217797));
#426807=CARTESIAN_POINT('Ctrl Pts',(2.09005979424748,1.71954430957288,12.5663937883685));
#426808=CARTESIAN_POINT('Ctrl Pts',(2.08459114137447,1.70960044649025,12.5540940315303));
#426809=CARTESIAN_POINT('Ctrl Pts',(2.09724993387507,1.69914956290367,12.5508374392248));
#426810=CARTESIAN_POINT('Ctrl Pts',(2.10199061773916,1.74123858749091,12.5434499600945));
#426811=CARTESIAN_POINT('Ctrl Pts',(2.09650418432823,1.73126239336826,12.5311293540533));
#426812=CARTESIAN_POINT('Ctrl Pts',(2.1092142503483,1.72080266171172,12.5278936106989));
#426813=CARTESIAN_POINT('Ctrl Pts',(2.11391033492732,1.7629126703876,12.5204817579905));
#426814=CARTESIAN_POINT('Ctrl Pts',(2.10839674742046,1.75288710092186,12.5081597038247));
#426815=CARTESIAN_POINT('Ctrl Pts',(2.12116680995867,1.74243676371845,12.5049254088044));
#426816=CARTESIAN_POINT('Ctrl Pts',(2.10534060625464,1.74733000120831,12.5369868989719));
#426817=CARTESIAN_POINT('Ctrl Pts',(2.10578948628541,1.74814621679791,12.5342545179733));
#426818=CARTESIAN_POINT('Ctrl Pts',(2.10632718358074,1.7488650622138,12.5314872231885));
#426819=CARTESIAN_POINT('Ctrl Pts',(2.10696817244343,1.74941256051339,12.5287124745063));
#426820=CARTESIAN_POINT('Ctrl Pts',(2.10754624801564,1.74990632165534,12.5262100684184));
#426821=CARTESIAN_POINT('Ctrl Pts',(2.10820838957962,1.7502594744367,12.5237004536639));
#426822=CARTESIAN_POINT('Ctrl Pts',(2.10899716276871,1.75041959135521,12.5212220730815));
#426823=CARTESIAN_POINT('Ctrl Pts',(2.10960103687929,1.75054217470755,12.5193246583486));
#426824=CARTESIAN_POINT('Ctrl Pts',(2.1102864760572,1.75055245850377,12.5174178313691));
#426825=CARTESIAN_POINT('Ctrl Pts',(2.11107409330956,1.75035542102692,12.5155812248348));
#426826=CARTESIAN_POINT('Ctrl Pts',(2.11140962249253,1.7502714820027,12.5147988205794));
#426827=CARTESIAN_POINT('Ctrl Pts',(2.11176410285173,1.75015010172559,12.5140295443047));
#426828=CARTESIAN_POINT('Ctrl Pts',(2.11214071774031,1.74998534742812,12.5132817086137));
#426829=CARTESIAN_POINT('Ctrl Pts',(2.11271067342687,1.74973601408637,12.5121499604604));
#426830=CARTESIAN_POINT('Ctrl Pts',(2.11334076467055,1.74937540606996,12.5110494206568));
#426831=CARTESIAN_POINT('Ctrl Pts',(2.1140238773609,1.74886696810325,12.5100666561695));
#426832=CARTESIAN_POINT('Ctrl Pts',(2.11441611909463,1.7485750241936,12.5095023550641));
#426833=CARTESIAN_POINT('Ctrl Pts',(2.1148299844179,1.74823044353594,12.5089719619137));
#426834=CARTESIAN_POINT('Ctrl Pts',(2.11525362918859,1.74783477651024,12.5085043804652));
#426835=CARTESIAN_POINT('Ctrl Pts',(2.11587357812687,1.74725576935739,12.5078201359221));
#426836=CARTESIAN_POINT('Ctrl Pts',(2.11653162546771,1.74654968741468,12.5072563000949));
#426837=CARTESIAN_POINT('Ctrl Pts',(2.11717697198553,1.74575862062969,12.5068768744332));
#426838=CARTESIAN_POINT('Ctrl Pts',(2.11764231125069,1.74518820702048,12.5066032824114));
#426839=CARTESIAN_POINT('Ctrl Pts',(2.11810926869283,1.74456362302461,12.5064197834844));
#426840=CARTESIAN_POINT('Ctrl Pts',(2.1185538384357,1.74392129480555,12.5063282718343));
#426841=CARTESIAN_POINT('Ctrl Pts',(2.11920277262498,1.7429836944655,12.5061946931565));
#426842=CARTESIAN_POINT('Ctrl Pts',(2.11981874903004,1.74198885098616,12.5062515701262));
#426843=CARTESIAN_POINT('Ctrl Pts',(2.12037668730694,1.74100664708784,12.5064436508398));
#426844=CARTESIAN_POINT('',(2.08527288288871,1.67747585909206,12.5737548217797));
#426845=CARTESIAN_POINT('Origin',(2.09739405675519,1.68722661004256,12.5893111709658));
#426846=CARTESIAN_POINT('Ctrl Pts',(2.12037668730694,1.74100664708784,12.5064436508398));
#426847=CARTESIAN_POINT('Ctrl Pts',(2.11518083275227,1.73160220754059,12.5164271754438));
#426848=CARTESIAN_POINT('Ctrl Pts',(2.10998273568189,1.72219414111502,12.5264061185523));
#426849=CARTESIAN_POINT('Ctrl Pts',(2.10478231794473,1.71278231961782,12.536380305637));
#426850=CARTESIAN_POINT('Ctrl Pts',(2.09828285053164,1.70101945166941,12.5488460165097));
#426851=CARTESIAN_POINT('Ctrl Pts',(2.09177975631206,1.68925071486236,12.5613043021964));
#426852=CARTESIAN_POINT('Ctrl Pts',(2.08527288288871,1.67747585909206,12.5737548217797));
#426853=CARTESIAN_POINT('Ctrl Pts',(2.11768454258375,1.6482118915911,12.5893111709658));
#426854=CARTESIAN_POINT('Ctrl Pts',(2.10678700448806,1.64509704038874,12.5770542771492));
#426855=CARTESIAN_POINT('Ctrl Pts',(2.09943490649417,1.65971724318977,12.5737548217797));
#426856=CARTESIAN_POINT('Ctrl Pts',(2.10751723432225,1.64530576251085,12.5928319619712));
#426857=CARTESIAN_POINT('Ctrl Pts',(2.09929810764222,1.64634469128069,12.5821634970843));
#426858=CARTESIAN_POINT('Ctrl Pts',(2.09573379622326,1.6586495353028,12.5773203894503));
#426859=CARTESIAN_POINT('Ctrl Pts',(2.09095932064318,1.64783945427108,12.5969440695591));
#426860=CARTESIAN_POINT('Ctrl Pts',(2.08843877426376,1.65097080996808,12.5878292599214));
#426861=CARTESIAN_POINT('Ctrl Pts',(2.0898325273865,1.65955461718524,12.5813877129824));
#426862=CARTESIAN_POINT('Ctrl Pts',(2.07184028516219,1.67172747904958,12.596957478804));
#426863=CARTESIAN_POINT('Ctrl Pts',(2.07434226647048,1.66861931517329,12.5878468778671));
#426864=CARTESIAN_POINT('Ctrl Pts',(2.08299421671343,1.66810819979388,12.5814011370086));
#426865=CARTESIAN_POINT('Ctrl Pts',(2.07301381630046,1.68854894842081,12.5928371701607));
#426866=CARTESIAN_POINT('Ctrl Pts',(2.07220438341499,1.68031002348439,12.5821692192951));
#426867=CARTESIAN_POINT('Ctrl Pts',(2.08340218510367,1.67409447368502,12.5773318885715));
#426868=CARTESIAN_POINT('Ctrl Pts',(2.07811692054266,1.69782812028621,12.5893111709658));
#426869=CARTESIAN_POINT('Ctrl Pts',(2.07265523480832,1.68789692582134,12.5770542771492));
#426870=CARTESIAN_POINT('Ctrl Pts',(2.08527288288866,1.67747585909209,12.5737548217797));
#426871=CARTESIAN_POINT('',(2.09943490649417,1.65971724318977,12.5737548217797));
#426872=CARTESIAN_POINT('Origin',(2.11163840068996,1.66936476771233,12.5893111709658));
#426873=CARTESIAN_POINT('Ctrl Pts',(2.08527288288866,1.67747585909209,12.5737548217797));
#426874=CARTESIAN_POINT('Ctrl Pts',(2.08476157278068,1.67661395329417,12.5746934679442));
#426875=CARTESIAN_POINT('Ctrl Pts',(2.08435332179325,1.6755667348024,12.5756680099006));
#426876=CARTESIAN_POINT('Ctrl Pts',(2.0840914747152,1.67445455685994,12.5765688348656));
#426877=CARTESIAN_POINT('Ctrl Pts',(2.08402215360003,1.67416012006189,12.5768073183026));
#426878=CARTESIAN_POINT('Ctrl Pts',(2.08396286507953,1.67386124851501,12.5770407398754));
#426879=CARTESIAN_POINT('Ctrl Pts',(2.08391386419817,1.67356029992052,12.5772674179684));
#426880=CARTESIAN_POINT('Ctrl Pts',(2.08371277783148,1.67232528826864,12.5781976435658));
#426881=CARTESIAN_POINT('Ctrl Pts',(2.08368465356045,1.67098333949609,12.5790594849312));
#426882=CARTESIAN_POINT('Ctrl Pts',(2.08387966896484,1.66962405228739,12.5797571720116));
#426883=CARTESIAN_POINT('Ctrl Pts',(2.08400672851294,1.66873842779531,12.580211740231));
#426884=CARTESIAN_POINT('Ctrl Pts',(2.08425286746706,1.66780786205578,12.5806009430798));
#426885=CARTESIAN_POINT('Ctrl Pts',(2.08461788639027,1.66690239319932,12.5808812374708));
#426886=CARTESIAN_POINT('Ctrl Pts',(2.08493155873907,1.66612429506545,12.5811221033394));
#426887=CARTESIAN_POINT('Ctrl Pts',(2.08533954568921,1.66534884268058,12.581287365893));
#426888=CARTESIAN_POINT('Ctrl Pts',(2.08582619880327,1.66462368612505,12.581359338449));
#426889=CARTESIAN_POINT('Ctrl Pts',(2.08589383353713,1.66452290433774,12.5813693411482));
#426890=CARTESIAN_POINT('Ctrl Pts',(2.08596295197249,1.66442304599782,12.5813775999465));
#426891=CARTESIAN_POINT('Ctrl Pts',(2.08603347634946,1.66432418917237,12.5813841266931));
#426892=CARTESIAN_POINT('Ctrl Pts',(2.08615312948473,1.66415646661151,12.5813952001081));
#426893=CARTESIAN_POINT('Ctrl Pts',(2.08627812670098,1.66399085721551,12.5814007534795));
#426894=CARTESIAN_POINT('Ctrl Pts',(2.08640857096445,1.66382755191868,12.5814005856065));
#426895=CARTESIAN_POINT('Ctrl Pts',(2.0870056938022,1.66308000411798,12.5813998171494));
#426896=CARTESIAN_POINT('Ctrl Pts',(2.08767543651301,1.66243217674746,12.58127954464));
#426897=CARTESIAN_POINT('Ctrl Pts',(2.08839342475655,1.66186647984163,12.5810700125799));
#426898=CARTESIAN_POINT('Ctrl Pts',(2.08926067280524,1.66118318238914,12.5808169217085));
#426899=CARTESIAN_POINT('Ctrl Pts',(2.09020874651044,1.66063279651635,12.5804173076348));
#426900=CARTESIAN_POINT('Ctrl Pts',(2.09114148342909,1.66024103484359,12.5799304713245));
#426901=CARTESIAN_POINT('Ctrl Pts',(2.09229743831373,1.65975551871339,12.5793271277669));
#426902=CARTESIAN_POINT('Ctrl Pts',(2.09348907404726,1.65945382833077,12.5785808224116));
#426903=CARTESIAN_POINT('Ctrl Pts',(2.09465837662795,1.65931793374739,12.5777485681082));
#426904=CARTESIAN_POINT('Ctrl Pts',(2.09640076557984,1.65911543592979,12.576508418016));
#426905=CARTESIAN_POINT('Ctrl Pts',(2.09807810078201,1.65927595424756,12.5750928681475));
#426906=CARTESIAN_POINT('Ctrl Pts',(2.09943490649417,1.65971724318977,12.5737548217797));
#426907=CARTESIAN_POINT('Ctrl Pts',(2.09943490649417,1.65971724318977,12.5737548217797));
#426908=CARTESIAN_POINT('Ctrl Pts',(2.10678700448806,1.64509704038875,12.5770542771492));
#426909=CARTESIAN_POINT('Ctrl Pts',(2.11768454258375,1.6482118915911,12.5893111709658));
#426910=CARTESIAN_POINT('Ctrl Pts',(2.12322677498387,1.66657012199645,12.5508408821982));
#426911=CARTESIAN_POINT('Ctrl Pts',(2.13059878054495,1.65190317757585,12.55409748406));
#426912=CARTESIAN_POINT('Ctrl Pts',(2.14151022110824,1.65502200253059,12.5663972313419));
#426913=CARTESIAN_POINT('Ctrl Pts',(2.14699572828318,1.67341517297119,12.52790050457));
#426914=CARTESIAN_POINT('Ctrl Pts',(2.15436495138303,1.65869627939029,12.5311362602937));
#426915=CARTESIAN_POINT('Ctrl Pts',(2.16531186343821,1.66182524318719,12.5434568539655));
#426916=CARTESIAN_POINT('Ctrl Pts',(2.17074355102939,1.68025299112988,12.5049357605811));
#426917=CARTESIAN_POINT('Ctrl Pts',(2.1780902711133,1.66547770470294,12.5081700652078));
#426918=CARTESIAN_POINT('Ctrl Pts',(2.18909135209325,1.66862215164286,12.5204921097672));
#426919=CARTESIAN_POINT('Ctrl Pts',(2.16918417633841,1.67980399166099,12.5064436508395));
#426920=CARTESIAN_POINT('Ctrl Pts',(2.17008442611849,1.67898034238851,12.5062361689309));
#426921=CARTESIAN_POINT('Ctrl Pts',(2.17098548998548,1.67808542589629,12.5061871075061));
#426922=CARTESIAN_POINT('Ctrl Pts',(2.17180759660236,1.67717155645727,12.5063648335164));
#426923=CARTESIAN_POINT('Ctrl Pts',(2.17218104813739,1.67675642058825,12.5064455676329));
#426924=CARTESIAN_POINT('Ctrl Pts',(2.17254325163388,1.67633143608171,12.506574497099));
#426925=CARTESIAN_POINT('Ctrl Pts',(2.17287787703125,1.67591414329733,12.5067492519495));
#426926=CARTESIAN_POINT('Ctrl Pts',(2.1735503197565,1.67507557724895,12.5071004286051));
#426927=CARTESIAN_POINT('Ctrl Pts',(2.17413548814429,1.67423673558925,12.5076537929613));
#426928=CARTESIAN_POINT('Ctrl Pts',(2.17459721966958,1.67346598929836,12.5083435010505));
#426929=CARTESIAN_POINT('Ctrl Pts',(2.17462628842842,1.67341746621334,12.5083869222964));
#426930=CARTESIAN_POINT('Ctrl Pts',(2.17465486088258,1.67336920159624,12.5084308732337));
#426931=CARTESIAN_POINT('Ctrl Pts',(2.17468292546678,1.67332120764692,12.5084753333615));
#426932=CARTESIAN_POINT('Ctrl Pts',(2.17490804047394,1.67293623282721,12.5088319622689));
#426933=CARTESIAN_POINT('Ctrl Pts',(2.17510616219274,1.6725615087908,12.509227847131));
#426934=CARTESIAN_POINT('Ctrl Pts',(2.17527387479912,1.67220948679698,12.5096423454524));
#426935=CARTESIAN_POINT('Ctrl Pts',(2.17579941188104,1.67110640566676,12.5109411997424));
#426936=CARTESIAN_POINT('Ctrl Pts',(2.17606740885955,1.67016255201858,12.5124831113042));
#426937=CARTESIAN_POINT('Ctrl Pts',(2.17617161682182,1.66936501883677,12.5140723025008));
#426938=CARTESIAN_POINT('Ctrl Pts',(2.17618138122202,1.66929028910413,12.5142212114565));
#426939=CARTESIAN_POINT('Ctrl Pts',(2.17618973361099,1.6692168299579,12.5143705582413));
#426940=CARTESIAN_POINT('Ctrl Pts',(2.17619676672589,1.66914462409029,12.5145201959299));
#426941=CARTESIAN_POINT('Ctrl Pts',(2.17628711755804,1.66821703221765,12.5164425148273));
#426942=CARTESIAN_POINT('Ctrl Pts',(2.17617352899946,1.66746553010939,12.5184635205941));
#426943=CARTESIAN_POINT('Ctrl Pts',(2.17592593384847,1.66683313195791,12.5205025929157));
#426944=CARTESIAN_POINT('Ctrl Pts',(2.17578231884714,1.66646631596413,12.5216853356836));
#426945=CARTESIAN_POINT('Ctrl Pts',(2.17559432756824,1.66614005834567,12.5228750347131));
#426946=CARTESIAN_POINT('Ctrl Pts',(2.175379077097,1.66584803936824,12.5240609649613));
#426947=CARTESIAN_POINT('Ctrl Pts',(2.17485075636314,1.6651312944544,12.5269717671326));
#426948=CARTESIAN_POINT('Ctrl Pts',(2.17413498073306,1.66460680972102,12.5299036066169));
#426949=CARTESIAN_POINT('Ctrl Pts',(2.17329354230824,1.66421382943731,12.5328133004019));
#426950=CARTESIAN_POINT('Ctrl Pts',(2.17288960286883,1.66402517601857,12.5342101228451));
#426951=CARTESIAN_POINT('Ctrl Pts',(2.17245698592973,1.66386753880635,12.5356023438238));
#426952=CARTESIAN_POINT('Ctrl Pts',(2.17200314797057,1.66373781788874,12.5369868989719));
#426953=CARTESIAN_POINT('Origin',(14.4283934060731,5.16148105026723,-1.24046354638259));
#426954=CARTESIAN_POINT('Ctrl Pts',(2.10532043137021,1.74729339881809,12.5369868989719));
#426955=CARTESIAN_POINT('Ctrl Pts',(2.11273758813649,1.76071983129993,12.5369868989719));
#426956=CARTESIAN_POINT('Ctrl Pts',(2.10270411148486,1.77232210047308,12.5369868989719));
#426957=CARTESIAN_POINT('Ctrl Pts',(2.1078276624841,1.75183209011841,12.5218025310015));
#426958=CARTESIAN_POINT('Ctrl Pts',(2.11040937252457,1.76336424676715,12.5216901060418));
#426959=CARTESIAN_POINT('Ctrl Pts',(2.10273470932111,1.7722867436991,12.5161920673677));
#426960=CARTESIAN_POINT('Ctrl Pts',(2.11381360199028,1.75254244173787,12.5042015548895));
#426961=CARTESIAN_POINT('Ctrl Pts',(2.11402805587868,1.75897138835048,12.4980677368513));
#426962=CARTESIAN_POINT('Ctrl Pts',(2.10967639799629,1.76419191068048,12.4907278922778));
#426963=CARTESIAN_POINT('Ctrl Pts',(2.12036122933718,1.74099395478799,12.506463626192));
#426964=CARTESIAN_POINT('Ctrl Pts',(2.12541783115062,1.74514584790279,12.4999376786891));
#426965=CARTESIAN_POINT('Ctrl Pts',(2.12535607211176,1.74509513856523,12.4906970594712));
#426966=CARTESIAN_POINT('Origin',(2.08606347004216,1.75793151145193,12.5369868989719));
#426967=CARTESIAN_POINT('Origin',(2.08606347004216,1.75793151145193,14.));
#426968=CARTESIAN_POINT('Origin',(2.08606347004216,1.75793151145193,13.7435492065112));
#426969=CARTESIAN_POINT('Ctrl Pts',(2.09340901446662,1.72563438261146,13.793642941384));
#426970=CARTESIAN_POINT('Ctrl Pts',(2.0986431642859,1.73509534951103,13.8071662555867));
#426971=CARTESIAN_POINT('Ctrl Pts',(2.08511567866223,1.74544071157992,13.8103758687955));
#426972=CARTESIAN_POINT('Ctrl Pts',(2.10141851697729,1.74019836471646,13.7804579775006));
#426973=CARTESIAN_POINT('Ctrl Pts',(2.10786811138308,1.75187725180944,13.7901904343352));
#426974=CARTESIAN_POINT('Ctrl Pts',(2.0970659823575,1.76334764555504,13.7927914348263));
#426975=CARTESIAN_POINT('Ctrl Pts',(2.10613401250348,1.74877272910428,13.7597120340895));
#426976=CARTESIAN_POINT('Ctrl Pts',(2.11359299325318,1.76229126068683,13.7635825532444));
#426977=CARTESIAN_POINT('Ctrl Pts',(2.10409180033665,1.77392153365468,13.7651073818884));
#426978=CARTESIAN_POINT('Ctrl Pts',(2.10521061050618,1.74709367222693,13.7381884353898));
#426979=CARTESIAN_POINT('Ctrl Pts',(2.11249578690014,1.76029534316416,13.7368803041982));
#426980=CARTESIAN_POINT('Ctrl Pts',(2.10271552475942,1.77185112568106,13.7363986145813));
#426981=CARTESIAN_POINT('Origin',(2.07607539289665,1.7397698043734,13.7902182540695));
#426982=CARTESIAN_POINT('Ctrl Pts',(2.07811502307555,1.69782467162314,13.8235227101244));
#426983=CARTESIAN_POINT('Ctrl Pts',(2.08365919544754,1.70789665459716,13.8358800583119));
#426984=CARTESIAN_POINT('Ctrl Pts',(2.07081126715283,1.71836359242969,13.8390832900376));
#426985=CARTESIAN_POINT('Ctrl Pts',(2.08386276647115,1.70827601580236,13.8124254819053));
#426986=CARTESIAN_POINT('Ctrl Pts',(2.08941770530363,1.71836755855869,13.8247886449157));
#426987=CARTESIAN_POINT('Ctrl Pts',(2.07654277777535,1.72883450760048,13.8279860620657));
#426988=CARTESIAN_POINT('Ctrl Pts',(2.08960793391517,1.71872267602913,13.8013225099955));
#426989=CARTESIAN_POINT('Ctrl Pts',(2.09517101992517,1.7288290160134,13.8136962257787));
#426990=CARTESIAN_POINT('Ctrl Pts',(2.0822718727572,1.73930044510501,13.8168830918626));
#426991=CARTESIAN_POINT('Ctrl Pts',(2.09535062563393,1.72916483454887,13.7902140179785));
#426992=CARTESIAN_POINT('Ctrl Pts',(2.10091941072531,1.73928152047611,13.802602731458));
#426993=CARTESIAN_POINT('Ctrl Pts',(2.08799864862899,1.74976159964428,13.8057746032558));
#426994=CARTESIAN_POINT('Origin',(2.05883978433024,1.70842963052981,13.8235269408515));
#426995=CARTESIAN_POINT('Ctrl Pts',(2.11768454258375,1.6482118915911,13.8235269408515));
#426996=CARTESIAN_POINT('Ctrl Pts',(2.12903736953611,1.65145687833693,13.8362179249168));
#426997=CARTESIAN_POINT('Ctrl Pts',(2.13632496810593,1.6360116877864,13.8391868794938));
#426998=CARTESIAN_POINT('Ctrl Pts',(2.10729720008146,1.64524286996452,13.8400110824519));
#426999=CARTESIAN_POINT('Ctrl Pts',(2.11733956479398,1.64455528444865,13.8494522556836));
#427000=CARTESIAN_POINT('Ctrl Pts',(2.11919945633416,1.63123354691577,13.85569149686));
#427001=CARTESIAN_POINT('Ctrl Pts',(2.09117326581736,1.64757020103072,13.8586819406588));
#427002=CARTESIAN_POINT('Ctrl Pts',(2.09389870930001,1.64417490995957,13.868010383617));
#427003=CARTESIAN_POINT('Ctrl Pts',(2.09245426254032,1.63524146491575,13.8744918421245));
#427004=CARTESIAN_POINT('Ctrl Pts',(2.07162300726337,1.67200089664954,13.8587686893867));
#427005=CARTESIAN_POINT('Ctrl Pts',(2.06892177629104,1.67536593441366,13.8680909899357));
#427006=CARTESIAN_POINT('Ctrl Pts',(2.059910832173,1.67591300626196,13.8745789365163));
#427007=CARTESIAN_POINT('Ctrl Pts',(2.07290246595287,1.68834647578953,13.8400379222776));
#427008=CARTESIAN_POINT('Ctrl Pts',(2.07445928579305,1.69828863581103,13.8494748685453));
#427009=CARTESIAN_POINT('Ctrl Pts',(2.06189161350704,1.70306511135021,13.8557104837033));
#427010=CARTESIAN_POINT('Ctrl Pts',(2.07811692053685,1.69782812028924,13.8235269408542));
#427011=CARTESIAN_POINT('Ctrl Pts',(2.08380679034645,1.70817423068592,13.8362179249195));
#427012=CARTESIAN_POINT('Ctrl Pts',(2.07037048620981,1.71871599217078,13.8391868794965));
#427013=CARTESIAN_POINT('Origin',(2.12373068447753,1.62705901546987,13.8235269408515));
#427014=CARTESIAN_POINT('Ctrl Pts',(2.15207044569429,1.65804043837791,13.7902140241683));
#427015=CARTESIAN_POINT('Ctrl Pts',(2.1631726538172,1.66121842047165,13.8026027327198));
#427016=CARTESIAN_POINT('Ctrl Pts',(2.17051483254974,1.6462895777927,13.8057746032556));
#427017=CARTESIAN_POINT('Ctrl Pts',(2.14061222476149,1.65476532679547,13.8013225161808));
#427018=CARTESIAN_POINT('Ctrl Pts',(2.15170307817164,1.65794005489717,13.8136962270464));
#427019=CARTESIAN_POINT('Ctrl Pts',(2.15904163347975,1.64303421002668,13.8168830918628));
#427020=CARTESIAN_POINT('Ctrl Pts',(2.12914906408654,1.65148880328298,13.8124254880875));
#427021=CARTESIAN_POINT('Ctrl Pts',(2.1402236783535,1.65465888118083,13.8247886461868));
#427022=CARTESIAN_POINT('Ctrl Pts',(2.14756325531373,1.6397776456057,13.8279860620656));
#427023=CARTESIAN_POINT('Ctrl Pts',(2.11768076368937,1.64821081067997,13.8235227163066));
#427024=CARTESIAN_POINT('Ctrl Pts',(2.12873391282528,1.6513747445314,13.8358800595848));
#427025=CARTESIAN_POINT('Ctrl Pts',(2.13607948675081,1.63651983374397,13.8390832900376));
#427026=CARTESIAN_POINT('Origin',(2.15812037844579,1.63688864659068,13.7902182540695));
#427027=CARTESIAN_POINT('Ctrl Pts',(2.17174368677524,1.6636636272183,13.7382347919292));
#427028=CARTESIAN_POINT('Ctrl Pts',(2.18624633379024,1.66783389079414,13.7369371795942));
#427029=CARTESIAN_POINT('Ctrl Pts',(2.19533646733967,1.65571311321701,13.7364597369711));
#427030=CARTESIAN_POINT('Ctrl Pts',(2.17356240961947,1.66418347450367,13.7595490285574));
#427031=CARTESIAN_POINT('Ctrl Pts',(2.18841135521326,1.66845227072419,13.7633824266926));
#427032=CARTESIAN_POINT('Ctrl Pts',(2.19763260326166,1.65658373059756,13.7648920890506));
#427033=CARTESIAN_POINT('Ctrl Pts',(2.16428702274945,1.66153228183547,13.780380659011));
#427034=CARTESIAN_POINT('Ctrl Pts',(2.17712933766779,1.66522982609384,13.7901039518744));
#427035=CARTESIAN_POINT('Ctrl Pts',(2.185925335279,1.65214869971078,13.7926933640892));
#427036=CARTESIAN_POINT('Ctrl Pts',(2.14816432986381,1.65692391708338,13.7936647693663));
#427037=CARTESIAN_POINT('Ctrl Pts',(2.15855501883592,1.65992506930038,13.8072068914933));
#427038=CARTESIAN_POINT('Ctrl Pts',(2.1656288682906,1.64441362437285,13.8104111085397));
#427039=CARTESIAN_POINT('Origin',(2.17804928986436,1.64258494176751,13.7435492065112));
#427040=CARTESIAN_POINT('Origin',(2.17804928986436,1.64258494176751,14.));
#427041=CARTESIAN_POINT('Origin',(2.17804928986436,1.64258494176751,12.5369868989719));
#427042=CARTESIAN_POINT('Ctrl Pts',(2.16916964168394,1.67979273611958,12.506462012331));
#427043=CARTESIAN_POINT('Ctrl Pts',(2.17433938317482,1.6837961547721,12.4999388158272));
#427044=CARTESIAN_POINT('Ctrl Pts',(2.17427821835328,1.68374878907928,12.4907030323752));
#427045=CARTESIAN_POINT('Ctrl Pts',(2.17896995532707,1.67083827155431,12.5042014951932));
#427046=CARTESIAN_POINT('Ctrl Pts',(2.18528284974206,1.66961824646391,12.4980716682127));
#427047=CARTESIAN_POINT('Ctrl Pts',(2.18940248500344,1.66421878625579,12.4907355092743));
#427048=CARTESIAN_POINT('Ctrl Pts',(2.17694791798238,1.66516050207837,12.5218047446509));
#427049=CARTESIAN_POINT('Ctrl Pts',(2.18875962168325,1.66511023659022,12.5216906929434));
#427050=CARTESIAN_POINT('Ctrl Pts',(2.19575008742635,1.65564957366289,12.5161988840776));
#427051=CARTESIAN_POINT('Ctrl Pts',(2.17196622031264,1.66372722794542,12.5369868989719));
#427052=CARTESIAN_POINT('Ctrl Pts',(2.18669844414395,1.66796599103203,12.5369868989719));
#427053=CARTESIAN_POINT('Ctrl Pts',(2.19577675014134,1.6556132629229,12.5369868989719));
#427054=CARTESIAN_POINT('Origin',(4.02788837499579E-31,-1.93972880878785E-31,
12.5));
#427055=CARTESIAN_POINT('Origin',(-0.404665629804381,2.65281661438092,12.5));
#427056=CARTESIAN_POINT('',(-0.404665629804381,2.65281661438092,12.5893111709658));
#427057=CARTESIAN_POINT('',(-0.404665629804381,2.65281661438092,13.8235269408515));
#427058=CARTESIAN_POINT('',(-0.404665629804381,2.65281661438092,12.5));
#427059=CARTESIAN_POINT('',(-0.396456161771472,2.6876286429604,13.7902182540695));
#427060=CARTESIAN_POINT('',(-0.404665629804381,2.65281661438092,13.8235269408515));
#427061=CARTESIAN_POINT('',(-0.391698755050363,2.70780229831486,13.7435492065112));
#427062=CARTESIAN_POINT('Origin',(-0.407350877337861,2.64143131362234,13.7445212918694));
#427063=CARTESIAN_POINT('',(-0.391698755050363,2.70780229831486,12.5369868989719));
#427064=CARTESIAN_POINT('',(-0.391698755050363,2.70780229831486,12.5));
#427065=CARTESIAN_POINT('Ctrl Pts',(-0.391698755050363,2.70780229831486,
12.5369868989719));
#427066=CARTESIAN_POINT('Ctrl Pts',(-0.396017894218442,2.6894871047414,
12.5544431401645));
#427067=CARTESIAN_POINT('Ctrl Pts',(-0.400340122549649,2.67115881165471,
12.5718848856037));
#427068=CARTESIAN_POINT('Ctrl Pts',(-0.404665629804381,2.65281661438092,
12.5893111709658));
#427069=CARTESIAN_POINT('Origin',(-0.612891682967421,2.87579381918237,12.5));
#427070=CARTESIAN_POINT('',(-0.497196489292348,2.69043060726394,13.7435492065112));
#427071=CARTESIAN_POINT('',(-0.486221890222975,2.67284744872125,13.7902182540695));
#427072=CARTESIAN_POINT('Origin',(-0.45738254066051,2.62664194705149,13.7418732680444));
#427073=CARTESIAN_POINT('',(-0.467283921384982,2.64250562881056,13.8235269408515));
#427074=CARTESIAN_POINT('',(-0.486221890222975,2.67284744872125,13.7902182540695));
#427075=CARTESIAN_POINT('',(-0.467283921384982,2.64250562881056,12.5893111709658));
#427076=CARTESIAN_POINT('',(-0.467283921384982,2.64250562881056,12.5));
#427077=CARTESIAN_POINT('',(-0.497196489292348,2.69043060726394,12.5369868989719));
#427078=CARTESIAN_POINT('Ctrl Pts',(-0.467283921384982,2.64250562881056,
12.5893111709658));
#427079=CARTESIAN_POINT('Ctrl Pts',(-0.477262195405936,2.65849250659842,
12.5718848856037));
#427080=CARTESIAN_POINT('Ctrl Pts',(-0.487232905459129,2.67446726563429,
12.5544431401645));
#427081=CARTESIAN_POINT('Ctrl Pts',(-0.497196489292348,2.69043060726394,
12.5369868989719));
#427082=CARTESIAN_POINT('',(-0.497196489292348,2.69043060726394,12.5));
#427083=CARTESIAN_POINT('Origin',(-0.438122897588506,2.66070659900837,12.5));
#427084=CARTESIAN_POINT('',(-0.431436192726697,2.62698897527435,13.8587068136939));
#427085=CARTESIAN_POINT('Ctrl Pts',(-0.467283921390512,2.64250562880694,
13.8235269408542));
#427086=CARTESIAN_POINT('Ctrl Pts',(-0.466356109619478,2.64101911787706,
13.8262006681044));
#427087=CARTESIAN_POINT('Ctrl Pts',(-0.465259243162499,2.63958988311412,
13.8288634856214));
#427088=CARTESIAN_POINT('Ctrl Pts',(-0.464006343942995,2.63821505475183,
13.8314912288862));
#427089=CARTESIAN_POINT('Ctrl Pts',(-0.462714734078248,2.63679774851727,
13.8342001611531));
#427090=CARTESIAN_POINT('Ctrl Pts',(-0.461256233254173,2.63543635362977,
13.8368750301949));
#427091=CARTESIAN_POINT('Ctrl Pts',(-0.459601776425736,2.63414059064196,
13.8394886372969));
#427092=CARTESIAN_POINT('Ctrl Pts',(-0.459473998711725,2.63404051572332,
13.8396904925131));
#427093=CARTESIAN_POINT('Ctrl Pts',(-0.459345035693413,2.63394084711228,
13.8398919674349));
#427094=CARTESIAN_POINT('Ctrl Pts',(-0.4592148661835,2.63384159766317,13.8400930404591));
#427095=CARTESIAN_POINT('Ctrl Pts',(-0.457186737645295,2.6322952244744,
13.8432258934518));
#427096=CARTESIAN_POINT('Ctrl Pts',(-0.454876755602826,2.63085760148959,
13.8462331177034));
#427097=CARTESIAN_POINT('Ctrl Pts',(-0.452309288225724,2.62965751679628,
13.8489036603661));
#427098=CARTESIAN_POINT('Ctrl Pts',(-0.451469183020814,2.62926483511854,
13.8497774930041));
#427099=CARTESIAN_POINT('Ctrl Pts',(-0.450601640977806,2.62889779863514,
13.85061494757));
#427100=CARTESIAN_POINT('Ctrl Pts',(-0.449707901397574,2.62856152004778,
13.8514076489583));
#427101=CARTESIAN_POINT('Ctrl Pts',(-0.447817513288837,2.62785024233689,
13.8530843267192));
#427102=CARTESIAN_POINT('Ctrl Pts',(-0.445623194189009,2.62720947264718,
13.8546805203176));
#427103=CARTESIAN_POINT('Ctrl Pts',(-0.443214054988678,2.62680737669962,
13.8559412814274));
#427104=CARTESIAN_POINT('Ctrl Pts',(-0.442891634033449,2.62675356322156,
13.8561100121513));
#427105=CARTESIAN_POINT('Ctrl Pts',(-0.442565424139822,2.62670397513517,
13.8562727473908));
#427106=CARTESIAN_POINT('Ctrl Pts',(-0.442235690326336,2.62665895978269,
13.8564289040185));
#427107=CARTESIAN_POINT('Ctrl Pts',(-0.440740351243861,2.62645481567278,
13.8571370725437));
#427108=CARTESIAN_POINT('Ctrl Pts',(-0.439145946992039,2.62634338218817,
13.8577210840554));
#427109=CARTESIAN_POINT('Ctrl Pts',(-0.437512406194008,2.62635826739462,
13.8581177131616));
#427110=CARTESIAN_POINT('Ctrl Pts',(-0.437052344880522,2.62636245958109,
13.8582294175695));
#427111=CARTESIAN_POINT('Ctrl Pts',(-0.436589212546076,2.62637649662708,
13.8583265086086));
#427112=CARTESIAN_POINT('Ctrl Pts',(-0.43612440418866,2.6264006933244,13.8584082369006));
#427113=CARTESIAN_POINT('Ctrl Pts',(-0.435456599222336,2.62643545748983,
13.8585256585398));
#427114=CARTESIAN_POINT('Ctrl Pts',(-0.434777049033409,2.62649194829904,
13.8586122832068));
#427115=CARTESIAN_POINT('Ctrl Pts',(-0.434103471787078,2.62656948525699,
13.8586682984299));
#427116=CARTESIAN_POINT('Ctrl Pts',(-0.433564676759578,2.62663150713736,
13.8587131050557));
#427117=CARTESIAN_POINT('Ctrl Pts',(-0.433023725658311,2.62670744730329,
13.8587357943552));
#427118=CARTESIAN_POINT('Ctrl Pts',(-0.432480624609339,2.62679781630673,
13.8587355499465));
#427119=CARTESIAN_POINT('Ctrl Pts',(-0.432129605453252,2.62685622394815,
13.8587353919793));
#427120=CARTESIAN_POINT('Ctrl Pts',(-0.431781477716286,2.62691998925264,
13.8587257282814));
#427121=CARTESIAN_POINT('Ctrl Pts',(-0.431436192726697,2.62698897527435,
13.8587068136939));
#427122=CARTESIAN_POINT('Ctrl Pts',(-0.431436192726697,2.62698897527435,
13.8587068136939));
#427123=CARTESIAN_POINT('Ctrl Pts',(-0.4303005692194,2.62721586653891,13.8586446046466));
#427124=CARTESIAN_POINT('Ctrl Pts',(-0.42919565750709,2.6274991616754,13.858482427929));
#427125=CARTESIAN_POINT('Ctrl Pts',(-0.428120053257249,2.62783461641623,
13.8582284286032));
#427126=CARTESIAN_POINT('Ctrl Pts',(-0.427016608416334,2.62817875395862,
13.8579678548414));
#427127=CARTESIAN_POINT('Ctrl Pts',(-0.425941768447865,2.62858008903839,
13.857615680862));
#427128=CARTESIAN_POINT('Ctrl Pts',(-0.424934518661332,2.62901372180358,
13.8571944833187));
#427129=CARTESIAN_POINT('Ctrl Pts',(-0.422420823805986,2.63009589671742,
13.8561433417727));
#427130=CARTESIAN_POINT('Ctrl Pts',(-0.420208603676628,2.63142543878401,
13.8546163505474));
#427131=CARTESIAN_POINT('Ctrl Pts',(-0.418334033481517,2.63279875718589,
13.8528973491086));
#427132=CARTESIAN_POINT('Ctrl Pts',(-0.417991577163569,2.6330496421965,
13.8525833129072));
#427133=CARTESIAN_POINT('Ctrl Pts',(-0.417660262800879,2.63330192566237,
13.8522628768812));
#427134=CARTESIAN_POINT('Ctrl Pts',(-0.417340140202077,2.6335543132114,
13.851937733538));
#427135=CARTESIAN_POINT('Ctrl Pts',(-0.41538519590622,2.6350956089561,13.8499521282529));
#427136=CARTESIAN_POINT('Ctrl Pts',(-0.413655874782884,2.63679716476219,
13.847639871647));
#427137=CARTESIAN_POINT('Ctrl Pts',(-0.412186715697788,2.63851228582483,
13.8452109780794));
#427138=CARTESIAN_POINT('Ctrl Pts',(-0.411525710615326,2.63928395429214,
13.8441181685877));
#427139=CARTESIAN_POINT('Ctrl Pts',(-0.410916696807409,2.64005811914853,
13.8430021611332));
#427140=CARTESIAN_POINT('Ctrl Pts',(-0.410359513936009,2.6408212858355,
13.8418824960098));
#427141=CARTESIAN_POINT('Ctrl Pts',(-0.409046498271374,2.64261970762151,
13.8392439765549));
#427142=CARTESIAN_POINT('Ctrl Pts',(-0.407955488334797,2.64444079616419,
13.8364981347964));
#427143=CARTESIAN_POINT('Ctrl Pts',(-0.407054243284078,2.64627178070576,
13.8336931113419));
#427144=CARTESIAN_POINT('Ctrl Pts',(-0.406176487839031,2.64805504337099,
13.8309611966327));
#427145=CARTESIAN_POINT('Ctrl Pts',(-0.405478361130355,2.64984972914729,
13.8281701127185));
#427146=CARTESIAN_POINT('Ctrl Pts',(-0.404969236073682,2.65164737840573,
13.825358068512));
#427147=CARTESIAN_POINT('Ctrl Pts',(-0.404858857211935,2.65203711070503,
13.8247484142932));
#427148=CARTESIAN_POINT('Ctrl Pts',(-0.404757526578536,2.65242692857967,
13.8241378483365));
#427149=CARTESIAN_POINT('Ctrl Pts',(-0.404665629804381,2.65281661438092,
13.8235269408515));
#427150=CARTESIAN_POINT('',(-0.432658710073015,2.62676936608522,12.5969504640361));
#427151=CARTESIAN_POINT('Origin',(-0.438128079974114,2.66073927661063,12.584524458991));
#427152=CARTESIAN_POINT('Origin',(-0.438128079974114,2.66073927661063,12.584524458991));
#427153=CARTESIAN_POINT('Ctrl Pts',(-0.467283921384982,2.64250562881056,
12.5893111709658));
#427154=CARTESIAN_POINT('Ctrl Pts',(-0.461282785199896,2.63289079656825,
12.5770542771492));
#427155=CARTESIAN_POINT('Ctrl Pts',(-0.44602821481188,2.6388154701569,12.5737548217797));
#427156=CARTESIAN_POINT('Ctrl Pts',(-0.480406392180606,2.6635300400909,
12.5663937883685));
#427157=CARTESIAN_POINT('Ctrl Pts',(-0.474397600712889,2.65390294279477,
12.5540940315304));
#427158=CARTESIAN_POINT('Ctrl Pts',(-0.459096922082043,2.65984896909383,
12.5508374392248));
#427159=CARTESIAN_POINT('Ctrl Pts',(-0.493515622564045,2.68453323799796,
12.5434499600945));
#427160=CARTESIAN_POINT('Ctrl Pts',(-0.487487294375404,2.67487483958022,
12.5311293540532));
#427161=CARTESIAN_POINT('Ctrl Pts',(-0.472153863122835,2.6808612951745,
12.5278936106989));
#427162=CARTESIAN_POINT('Ctrl Pts',(-0.506612649674959,2.70551688420438,
12.5204817579905));
#427163=CARTESIAN_POINT('Ctrl Pts',(-0.500554485381652,2.69581068331508,
12.5081597038247));
#427164=CARTESIAN_POINT('Ctrl Pts',(-0.48519996421925,2.70185408672443,
12.5049254088044));
#427165=CARTESIAN_POINT('Ctrl Pts',(-0.497196489292348,2.69043060726394,
12.5369868989719));
#427166=CARTESIAN_POINT('Ctrl Pts',(-0.497689704890034,2.69122082213657,
12.5342545179733));
#427167=CARTESIAN_POINT('Ctrl Pts',(-0.498054582671471,2.69204101803876,
12.5314872231885));
#427168=CARTESIAN_POINT('Ctrl Pts',(-0.498219493613029,2.69286771356402,
12.5287124745063));
#427169=CARTESIAN_POINT('Ctrl Pts',(-0.498368218485575,2.6936132686222,
12.5262100684185));
#427170=CARTESIAN_POINT('Ctrl Pts',(-0.498353189084903,2.69436355020591,
12.5237004536639));
#427171=CARTESIAN_POINT('Ctrl Pts',(-0.49810787003645,2.6951301134035,12.5212220730815));
#427172=CARTESIAN_POINT('Ctrl Pts',(-0.497920057083069,2.69571698384426,
12.5193246583486));
#427173=CARTESIAN_POINT('Ctrl Pts',(-0.497594417118367,2.69632021782581,
12.517417831369));
#427174=CARTESIAN_POINT('Ctrl Pts',(-0.497037957625851,2.69691141790759,
12.5155812248347));
#427175=CARTESIAN_POINT('Ctrl Pts',(-0.496800902891061,2.69716327232013,
12.5147988205793));
#427176=CARTESIAN_POINT('Ctrl Pts',(-0.496521919973337,2.6974133883499,
12.5140295443047));
#427177=CARTESIAN_POINT('Ctrl Pts',(-0.496194277041749,2.6976616480168,
12.5132817086137));
#427178=CARTESIAN_POINT('Ctrl Pts',(-0.495698433787316,2.69803735543885,
12.5121499604604));
#427179=CARTESIAN_POINT('Ctrl Pts',(-0.495076119358838,2.69841122422461,
12.5110494206568));
#427180=CARTESIAN_POINT('Ctrl Pts',(-0.494298903258426,2.69875920015332,
12.5100666561695));
#427181=CARTESIAN_POINT('Ctrl Pts',(-0.49385262756334,2.69895900713027,
12.509502355064));
#427182=CARTESIAN_POINT('Ctrl Pts',(-0.493349857282979,2.69915198998088,
12.5089719619137));
#427183=CARTESIAN_POINT('Ctrl Pts',(-0.492797727532223,2.69932856864687,
12.5085043804652));
#427184=CARTESIAN_POINT('Ctrl Pts',(-0.49198975756195,2.69958696852355,
12.5078201359221));
#427185=CARTESIAN_POINT('Ctrl Pts',(-0.491052284959171,2.69981658370521,
12.5072563000949));
#427186=CARTESIAN_POINT('Ctrl Pts',(-0.490046842492173,2.69999362672806,
12.5068768744332));
#427187=CARTESIAN_POINT('Ctrl Pts',(-0.489321849258572,2.70012128693521,
12.5066032824114));
#427188=CARTESIAN_POINT('Ctrl Pts',(-0.488548789130486,2.70022391470455,
12.5064197834843));
#427189=CARTESIAN_POINT('Ctrl Pts',(-0.487771171960831,2.70029834141171,
12.5063282718343));
#427190=CARTESIAN_POINT('Ctrl Pts',(-0.486636091637325,2.70040698136224,
12.5061946931564));
#427191=CARTESIAN_POINT('Ctrl Pts',(-0.485467141851131,2.70045891282986,
12.5062515701262));
#427192=CARTESIAN_POINT('Ctrl Pts',(-0.484337556030415,2.70046636214881,
12.5064436508398));
#427193=CARTESIAN_POINT('',(-0.44602821481188,2.6388154701569,12.5737548217797));
#427194=CARTESIAN_POINT('Origin',(-0.448620866155238,2.65415424973716,12.5893111709658));
#427195=CARTESIAN_POINT('Ctrl Pts',(-0.484337556030415,2.70046636214881,
12.5064436508398));
#427196=CARTESIAN_POINT('Ctrl Pts',(-0.478666370156481,2.69134068198049,
12.5164271754438));
#427197=CARTESIAN_POINT('Ctrl Pts',(-0.472993113685128,2.6822112741119,
12.5264061185523));
#427198=CARTESIAN_POINT('Ctrl Pts',(-0.467317712887747,2.67307800775614,
12.536380305637));
#427199=CARTESIAN_POINT('Ctrl Pts',(-0.460224612986331,2.66166327723746,
12.5488460165097));
#427200=CARTESIAN_POINT('Ctrl Pts',(-0.45312816158799,2.65024251640408,
12.5613043021964));
#427201=CARTESIAN_POINT('Ctrl Pts',(-0.44602821481188,2.6388154701569,12.5737548217797));
#427202=CARTESIAN_POINT('Ctrl Pts',(-0.404665629804381,2.65281661438092,
12.5893111709658));
#427203=CARTESIAN_POINT('Ctrl Pts',(-0.407267077514747,2.64178524527415,
12.5770542771492));
#427204=CARTESIAN_POINT('Ctrl Pts',(-0.423615907027033,2.64250597298498,
12.5737548217797));
#427205=CARTESIAN_POINT('Ctrl Pts',(-0.407092757891956,2.64252444295008,
12.5928319619712));
#427206=CARTESIAN_POINT('Ctrl Pts',(-0.412011859954225,2.63585842080247,
12.5821634970842));
#427207=CARTESIAN_POINT('Ctrl Pts',(-0.424490864181512,2.63875461758363,
12.5773203894503));
#427208=CARTESIAN_POINT('Ctrl Pts',(-0.417387204414804,2.6293104931194,
12.5969440695591));
#427209=CARTESIAN_POINT('Ctrl Pts',(-0.42135055049259,2.62863935198698,
12.5878292599214));
#427210=CARTESIAN_POINT('Ctrl Pts',(-0.428161628981916,2.63404615362204,
12.5813877129824));
#427211=CARTESIAN_POINT('Ctrl Pts',(-0.44756881895074,2.62428601408715,
12.596957478804));
#427212=CARTESIAN_POINT('Ctrl Pts',(-0.443634776446592,2.62495227433994,
12.5878468778671));
#427213=CARTESIAN_POINT('Ctrl Pts',(-0.438965026764344,2.63225370706529,
12.5814011370086));
#427214=CARTESIAN_POINT('Ctrl Pts',(-0.461676783769701,2.63352204872367,
12.5928371701607));
#427215=CARTESIAN_POINT('Ctrl Pts',(-0.454881448360943,2.62879357302993,
12.5821692192952));
#427216=CARTESIAN_POINT('Ctrl Pts',(-0.443990357448371,2.63553211595122,
12.5773318885715));
#427217=CARTESIAN_POINT('Ctrl Pts',(-0.467283921385027,2.64250562881053,
12.5893111709658));
#427218=CARTESIAN_POINT('Ctrl Pts',(-0.461282785199942,2.63289079656822,
12.5770542771492));
#427219=CARTESIAN_POINT('Ctrl Pts',(-0.446028214811926,2.63881547015687,
12.5737548217797));
#427220=CARTESIAN_POINT('',(-0.423615907027033,2.64250597298498,12.5737548217797));
#427221=CARTESIAN_POINT('Origin',(-0.426078281186221,2.65786620454249,12.5893111709658));
#427222=CARTESIAN_POINT('Ctrl Pts',(-0.446028214811926,2.63881547015687,
12.5737548217797));
#427223=CARTESIAN_POINT('Ctrl Pts',(-0.445525600187509,2.63794846486834,
12.5746934679442));
#427224=CARTESIAN_POINT('Ctrl Pts',(-0.44481094380899,2.63708093867342,
12.5756680099006));
#427225=CARTESIAN_POINT('Ctrl Pts',(-0.443968123483801,2.63630947411337,
12.5765688348656));
#427226=CARTESIAN_POINT('Ctrl Pts',(-0.443744996133033,2.63610523741148,
12.5768073183026));
#427227=CARTESIAN_POINT('Ctrl Pts',(-0.443513100702999,2.63590759166848,
12.5770407398754));
#427228=CARTESIAN_POINT('Ctrl Pts',(-0.443274370359209,2.6357179104468,
12.5772674179684));
#427229=CARTESIAN_POINT('Ctrl Pts',(-0.442294685583711,2.63493951000499,
12.5781976435658));
#427230=CARTESIAN_POINT('Ctrl Pts',(-0.441137235981574,2.63425985722505,
12.5790594849312));
#427231=CARTESIAN_POINT('Ctrl Pts',(-0.439855722864257,2.63376648428921,
12.5797571720116));
#427232=CARTESIAN_POINT('Ctrl Pts',(-0.43902077098922,2.6334450340814,12.580211740231));
#427233=CARTESIAN_POINT('Ctrl Pts',(-0.438088465128481,2.63320557059283,
12.5806009430798));
#427234=CARTESIAN_POINT('Ctrl Pts',(-0.43712002807693,2.63308211071472,
12.5808812374708));
#427235=CARTESIAN_POINT('Ctrl Pts',(-0.436287819373999,2.63297601772203,
12.5811221033394));
#427236=CARTESIAN_POINT('Ctrl Pts',(-0.43541187759125,2.63295352892627,
12.581287365893));
#427237=CARTESIAN_POINT('Ctrl Pts',(-0.434541428297158,2.63302424886595,
12.581359338449));
#427238=CARTESIAN_POINT('Ctrl Pts',(-0.434420453819371,2.63303407747726,
12.5813693411482));
#427239=CARTESIAN_POINT('Ctrl Pts',(-0.434299560967986,2.63304565178682,
12.5813775999465));
#427240=CARTESIAN_POINT('Ctrl Pts',(-0.434178855836194,2.63305894204054,
12.5813841266931));
#427241=CARTESIAN_POINT('Ctrl Pts',(-0.433974064981122,2.6330814905634,
12.5813952001081));
#427242=CARTESIAN_POINT('Ctrl Pts',(-0.433768509527142,2.63310973470351,
12.5814007534795));
#427243=CARTESIAN_POINT('Ctrl Pts',(-0.433562305845541,2.63314385753371,
12.5814005856065));
#427244=CARTESIAN_POINT('Ctrl Pts',(-0.432618386011585,2.6333000585092,
12.5813998171494));
#427245=CARTESIAN_POINT('Ctrl Pts',(-0.431726045399303,2.63356831926361,
12.58127954464));
#427246=CARTESIAN_POINT('Ctrl Pts',(-0.430881831425681,2.63391878020847,
12.5810700125799));
#427247=CARTESIAN_POINT('Ctrl Pts',(-0.429862117067003,2.63434209712668,
12.5808169217085));
#427248=CARTESIAN_POINT('Ctrl Pts',(-0.428918943474546,2.63490083851046,
12.5804173076348));
#427249=CARTESIAN_POINT('Ctrl Pts',(-0.428121695428069,2.63552363134925,
12.5799304713245));
#427250=CARTESIAN_POINT('Ctrl Pts',(-0.427133653939449,2.63629546787648,
12.5793271277669));
#427251=CARTESIAN_POINT('Ctrl Pts',(-0.426288626927976,2.63718818404541,
12.5785808224116));
#427252=CARTESIAN_POINT('Ctrl Pts',(-0.425599199900031,2.63814234662912,
12.5777485681082));
#427253=CARTESIAN_POINT('Ctrl Pts',(-0.424571878096021,2.63956415341515,
12.576508418016));
#427254=CARTESIAN_POINT('Ctrl Pts',(-0.423893134534421,2.64110640070023,
12.5750928681475));
#427255=CARTESIAN_POINT('Ctrl Pts',(-0.423615907027033,2.64250597298498,
12.5737548217797));
#427256=CARTESIAN_POINT('Ctrl Pts',(-0.423615907027033,2.64250597298498,
12.5737548217797));
#427257=CARTESIAN_POINT('Ctrl Pts',(-0.407267077514747,2.64178524527415,
12.5770542771492));
#427258=CARTESIAN_POINT('Ctrl Pts',(-0.404665629804381,2.65281661438092,
12.5893111709658));
#427259=CARTESIAN_POINT('Ctrl Pts',(-0.417982099262763,2.66661562176396,
12.5508408821982));
#427260=CARTESIAN_POINT('Ctrl Pts',(-0.401582757830894,2.66588945013814,
12.55409748406));
#427261=CARTESIAN_POINT('Ctrl Pts',(-0.398977991339499,2.67693489244663,
12.5663972313419));
#427262=CARTESIAN_POINT('Ctrl Pts',(-0.412352646447294,2.69070145006173,
12.52790050457));
#427263=CARTESIAN_POINT('Ctrl Pts',(-0.395909324972191,2.6899474897126,
12.5311362602938));
#427264=CARTESIAN_POINT('Ctrl Pts',(-0.393296090767228,2.7010288391329,
12.5434568539655));
#427265=CARTESIAN_POINT('Ctrl Pts',(-0.406727196660406,2.71476530588435,
12.5049357605811));
#427266=CARTESIAN_POINT('Ctrl Pts',(-0.390245644042783,2.71396417649287,
12.5081700652078));
#427267=CARTESIAN_POINT('Ctrl Pts',(-0.38761947869465,2.72510036007836,
12.5204921097672));
#427268=CARTESIAN_POINT('Ctrl Pts',(-0.407096584199038,2.71318517842233,
12.5064436508395));
#427269=CARTESIAN_POINT('Ctrl Pts',(-0.405938267818595,2.71356878102058,
12.5062361689309));
#427270=CARTESIAN_POINT('Ctrl Pts',(-0.404717355904196,2.71391830314823,
12.5061871075061));
#427271=CARTESIAN_POINT('Ctrl Pts',(-0.403518447949327,2.71418966334587,
12.5063648335164));
#427272=CARTESIAN_POINT('Ctrl Pts',(-0.402973830004515,2.71431293188584,
12.5064455676329));
#427273=CARTESIAN_POINT('Ctrl Pts',(-0.402426107734433,2.71442157588489,
12.506574497099));
#427274=CARTESIAN_POINT('Ctrl Pts',(-0.401898561348905,2.71450990614909,
12.5067492519495));
#427275=CARTESIAN_POINT('Ctrl Pts',(-0.400838436409385,2.71468740924372,
12.5071004286051));
#427276=CARTESIAN_POINT('Ctrl Pts',(-0.399820676186354,2.71478860954198,
12.5076537929612));
#427277=CARTESIAN_POINT('Ctrl Pts',(-0.398922604801309,2.71481532346341,
12.5083435010503));
#427278=CARTESIAN_POINT('Ctrl Pts',(-0.39886606584061,2.71481700526441,
12.5083869222963));
#427279=CARTESIAN_POINT('Ctrl Pts',(-0.398809994740654,2.71481838009582,
12.5084308732336));
#427280=CARTESIAN_POINT('Ctrl Pts',(-0.398754407794718,2.71481944381979,
12.5084753333615));
#427281=CARTESIAN_POINT('Ctrl Pts',(-0.398308527120983,2.71482797629003,
12.508831962269));
#427282=CARTESIAN_POINT('Ctrl Pts',(-0.397884770249155,2.71481795468889,
12.509227847131));
#427283=CARTESIAN_POINT('Ctrl Pts',(-0.397495671478641,2.71479247628123,
12.5096423454524));
#427284=CARTESIAN_POINT('Ctrl Pts',(-0.396276408139752,2.71471263822789,
12.5109411997424));
#427285=CARTESIAN_POINT('Ctrl Pts',(-0.395321834754573,2.71448576438194,
12.5124831113042));
#427286=CARTESIAN_POINT('Ctrl Pts',(-0.394574919738505,2.71418737464644,
12.5140723025008));
#427287=CARTESIAN_POINT('Ctrl Pts',(-0.394504932983426,2.71415941520141,
12.5142212114565));
#427288=CARTESIAN_POINT('Ctrl Pts',(-0.394436744436691,2.71413084370056,
12.5143705582413));
#427289=CARTESIAN_POINT('Ctrl Pts',(-0.394370293720933,2.71410173263056,
12.5145201959299));
#427290=CARTESIAN_POINT('Ctrl Pts',(-0.393516635342246,2.71372775759454,
12.5164425148273));
#427291=CARTESIAN_POINT('Ctrl Pts',(-0.392916216798835,2.71326175828972,
12.5184635205941));
#427292=CARTESIAN_POINT('Ctrl Pts',(-0.392485164478752,2.71273694910712,
12.5205025929158));
#427293=CARTESIAN_POINT('Ctrl Pts',(-0.392235137047787,2.71243253897973,
12.5216853356836));
#427294=CARTESIAN_POINT('Ctrl Pts',(-0.392042170182552,2.71210919930776,
12.5228750347131));
#427295=CARTESIAN_POINT('Ctrl Pts',(-0.391892392212254,2.7117787837994,
12.5240609649613));
#427296=CARTESIAN_POINT('Ctrl Pts',(-0.391524770219468,2.71096779666032,
12.5269717671326));
#427297=CARTESIAN_POINT('Ctrl Pts',(-0.391416453375186,2.71008706602646,
12.5299036066169));
#427298=CARTESIAN_POINT('Ctrl Pts',(-0.391484251980021,2.70916086114884,
12.5328133004019));
#427299=CARTESIAN_POINT('Ctrl Pts',(-0.391516799258136,2.70871622887628,
12.5342101228451));
#427300=CARTESIAN_POINT('Ctrl Pts',(-0.391590415451197,2.70826170983071,
12.5356023438238));
#427301=CARTESIAN_POINT('Ctrl Pts',(-0.391698755050363,2.70780229831486,
12.5369868989719));
#427302=CARTESIAN_POINT('Origin',(2.53877470614877,15.1113213650641,-1.23968739425757));
#427303=CARTESIAN_POINT('Ctrl Pts',(-0.49717439363454,2.69039513131661,
12.5369868989719));
#427304=CARTESIAN_POINT('Ctrl Pts',(-0.50527136720736,2.70342288333476,
12.5369868989719));
#427305=CARTESIAN_POINT('Ctrl Pts',(-0.520295295224563,2.70033016759948,
12.5369868989719));
#427306=CARTESIAN_POINT('Ctrl Pts',(-0.499911543608354,2.6947989860598,
12.5218025310016));
#427307=CARTESIAN_POINT('Ctrl Pts',(-0.508715847286229,2.70268188530136,
12.5216901060418));
#427308=CARTESIAN_POINT('Ctrl Pts',(-0.520249500638078,2.70033961137504,
12.5161920673678));
#427309=CARTESIAN_POINT('Ctrl Pts',(-0.497609306258535,2.70036996213051,
12.5042015548894));
#427310=CARTESIAN_POINT('Ctrl Pts',(-0.503115446561909,2.70369558447474,
12.4980677368513));
#427311=CARTESIAN_POINT('Ctrl Pts',(-0.509796007626935,2.70244623120992,
12.4907278922777));
#427312=CARTESIAN_POINT('Ctrl Pts',(-0.48433402510107,2.70044667520282,
12.506463626192));
#427313=CARTESIAN_POINT('Ctrl Pts',(-0.485489056741789,2.7068866550355,
12.4999376786891));
#427314=CARTESIAN_POINT('Ctrl Pts',(-0.485474949709712,2.70680800004557,
12.4906970594712));
#427315=CARTESIAN_POINT('Origin',(-0.515859544522093,2.67878198633735,12.5369868989719));
#427316=CARTESIAN_POINT('Origin',(-0.515859544522093,2.67878198633735,14.));
#427317=CARTESIAN_POINT('Origin',(-0.515859544522093,2.67878198633735,13.7435492065112));
#427318=CARTESIAN_POINT('Ctrl Pts',(-0.484086463901995,2.66942608434243,
13.793642941384));
#427319=CARTESIAN_POINT('Ctrl Pts',(-0.489788288908134,2.67861278182332,
13.8071662555867));
#427320=CARTESIAN_POINT('Ctrl Pts',(-0.505420949465545,2.67185709477229,
13.8103758687955));
#427321=CARTESIAN_POINT('Ctrl Pts',(-0.492887059224724,2.68352612785969,
13.7804579775006));
#427322=CARTESIAN_POINT('Ctrl Pts',(-0.499931212062378,2.69485633450072,
13.7901904343351));
#427323=CARTESIAN_POINT('Ctrl Pts',(-0.515215284247408,2.69102840273443,
13.7927914348263));
#427324=CARTESIAN_POINT('Ctrl Pts',(-0.498068300927142,2.69182735410252,
13.7597120340895));
#427325=CARTESIAN_POINT('Ctrl Pts',(-0.506225236064354,2.70493656838637,
13.7635825532445));
#427326=CARTESIAN_POINT('Ctrl Pts',(-0.521013756001522,2.70232207145352,
13.7651073818884));
#427327=CARTESIAN_POINT('Ctrl Pts',(-0.497053695165545,2.69020178392726,
13.7381884353898));
#427328=CARTESIAN_POINT('Ctrl Pts',(-0.505018938881371,2.70300462748538,
13.7368803041982));
#427329=CARTESIAN_POINT('Ctrl Pts',(-0.519878682598321,2.70011020979169,
13.7363986145813));
#427330=CARTESIAN_POINT('Origin',(-0.504884945452719,2.66119882779466,13.7902182540695));
#427331=CARTESIAN_POINT('Ctrl Pts',(-0.467281837879557,2.64250228925016,
13.8235227101244));
#427332=CARTESIAN_POINT('Ctrl Pts',(-0.47336557853089,2.65225784090073,
13.8358800583119));
#427333=CARTESIAN_POINT('Ctrl Pts',(-0.488772600020449,2.64615458456686,
13.8390832900376));
#427334=CARTESIAN_POINT('Ctrl Pts',(-0.473597285630048,2.65262070162588,
13.8124254819053));
#427335=CARTESIAN_POINT('Ctrl Pts',(-0.479692841055534,2.66239519827228,
13.8247886449158));
#427336=CARTESIAN_POINT('Ctrl Pts',(-0.495113052711319,2.656268383962,13.8279860620657));
#427337=CARTESIAN_POINT('Ctrl Pts',(-0.479909903002316,2.66273457925838,
13.8013225099955));
#427338=CARTESIAN_POINT('Ctrl Pts',(-0.486014395377619,2.67252340996857,
13.8136962257787));
#427339=CARTESIAN_POINT('Ctrl Pts',(-0.501450340426691,2.66637764514034,
13.8168830918626));
#427340=CARTESIAN_POINT('Ctrl Pts',(-0.486219800122016,2.67284409858753,
13.7902140179785));
#427341=CARTESIAN_POINT('Ctrl Pts',(-0.492330539712305,2.68264295378619,
13.802602731458));
#427342=CARTESIAN_POINT('Ctrl Pts',(-0.507784585966958,2.67648254739697,
13.8057746032558));
#427343=CARTESIAN_POINT('Origin',(-0.485946976614727,2.63085700788397,13.8235269408515));
#427344=CARTESIAN_POINT('Ctrl Pts',(-0.404665629804381,2.65281661438092,
13.8235269408515));
#427345=CARTESIAN_POINT('Ctrl Pts',(-0.401955496063886,2.66430886367772,
13.8362179249168));
#427346=CARTESIAN_POINT('Ctrl Pts',(-0.384918149628171,2.66312910502163,
13.8391868794938));
#427347=CARTESIAN_POINT('Ctrl Pts',(-0.407145284211823,2.64230170650223,
13.8400110824519));
#427348=CARTESIAN_POINT('Ctrl Pts',(-0.401642753823838,2.65073046810706,
13.8494522556837));
#427349=CARTESIAN_POINT('Ctrl Pts',(-0.389108318008103,2.64585032402954,
13.85569149686));
#427350=CARTESIAN_POINT('Ctrl Pts',(-0.417047772027924,2.62936576969432,
13.8586819406588));
#427351=CARTESIAN_POINT('Ctrl Pts',(-0.412754051757822,2.6300868867979,
13.868010383617));
#427352=CARTESIAN_POINT('Ctrl Pts',(-0.40566257599941,2.62446515767242,
13.8744918421245));
#427353=CARTESIAN_POINT('Ctrl Pts',(-0.447913512718888,2.62422986183445,
13.8587686893867));
#427354=CARTESIAN_POINT('Ctrl Pts',(-0.4521690095924,2.62351510713571,13.8680909899357));
#427355=CARTESIAN_POINT('Ctrl Pts',(-0.457045392374262,2.61591791736115,
13.8745789365163));
#427356=CARTESIAN_POINT('Ctrl Pts',(-0.461554435365154,2.6333260259336,
13.8400379222776));
#427357=CARTESIAN_POINT('Ctrl Pts',(-0.469471404303291,2.63953825876411,
13.8494748685453));
#427358=CARTESIAN_POINT('Ctrl Pts',(-0.479775288452308,2.63090164619271,
13.8557104837033));
#427359=CARTESIAN_POINT('Ctrl Pts',(-0.467283921390512,2.64250562880694,
13.8235269408542));
#427360=CARTESIAN_POINT('Ctrl Pts',(-0.473535779381647,2.65252215966594,
13.8362179249195));
#427361=CARTESIAN_POINT('Ctrl Pts',(-0.489295333932619,2.64594192833176,
13.8391868794965));
#427362=CARTESIAN_POINT('Origin',(-0.383252978422541,2.64776702421936,13.8235269408515));
#427363=CARTESIAN_POINT('Ctrl Pts',(-0.39645706603083,2.68762480516188,
13.7902140241682));
#427364=CARTESIAN_POINT('Ctrl Pts',(-0.393810800458559,2.698865618029,13.8026027327198));
#427365=CARTESIAN_POINT('Ctrl Pts',(-0.377197449355658,2.69798556268688,
13.8057746032556));
#427366=CARTESIAN_POINT('Ctrl Pts',(-0.399192359301602,2.67602586755773,
13.8013225161808));
#427367=CARTESIAN_POINT('Ctrl Pts',(-0.396548796924342,2.68725518213354,
13.8136962270464));
#427368=CARTESIAN_POINT('Ctrl Pts',(-0.379957285915439,2.68638319144844,
13.8168830918628));
#427369=CARTESIAN_POINT('Ctrl Pts',(-0.401928831781928,2.66442192954721,
13.8124254880875));
#427370=CARTESIAN_POINT('Ctrl Pts',(-0.399289138525419,2.67563480137168,
13.8247886461867));
#427371=CARTESIAN_POINT('Ctrl Pts',(-0.382718606411943,2.67477571600085,
13.8279860620656));
#427372=CARTESIAN_POINT('Ctrl Pts',(-0.404666531210821,2.65281278869432,
13.8235227163065));
#427373=CARTESIAN_POINT('Ctrl Pts',(-0.402031954534204,2.66400392755378,
13.8358800595848));
#427374=CARTESIAN_POINT('Ctrl Pts',(-0.385481469674173,2.66316292713999,
13.8390832900376));
#427375=CARTESIAN_POINT('Origin',(-0.375043510389632,2.68257905279883,13.7902182540695));
#427376=CARTESIAN_POINT('Ctrl Pts',(-0.391760668288975,2.70753963671063,
13.7382347919292));
#427377=CARTESIAN_POINT('Ctrl Pts',(-0.388320398150704,2.72223257413337,
13.7369371795943));
#427378=CARTESIAN_POINT('Ctrl Pts',(-0.373304462126552,2.72424886834272,
13.7364597369711));
#427379=CARTESIAN_POINT('Ctrl Pts',(-0.391326505236804,2.70938069521824,
13.7595490285573));
#427380=CARTESIAN_POINT('Ctrl Pts',(-0.387803174254,2.72442396431789,13.7633824266925));
#427381=CARTESIAN_POINT('Ctrl Pts',(-0.372943370247577,2.72667782438402,
13.7648920890506));
#427382=CARTESIAN_POINT('Ctrl Pts',(-0.393540713025231,2.69999139769274,
13.7803806590111));
#427383=CARTESIAN_POINT('Ctrl Pts',(-0.390498414047488,2.71300451810768,
13.7901039518745));
#427384=CARTESIAN_POINT('Ctrl Pts',(-0.374787928484793,2.71429528718463,
13.7926933640892));
#427385=CARTESIAN_POINT('Ctrl Pts',(-0.39738950035983,2.68367070262093,
13.7936647693663));
#427386=CARTESIAN_POINT('Ctrl Pts',(-0.394936254100455,2.69420421650451,
13.8072068914932));
#427387=CARTESIAN_POINT('Ctrl Pts',(-0.377945431714628,2.69280556554734,
13.8104111085397));
#427388=CARTESIAN_POINT('Origin',(-0.370286103668523,2.7027527081533,13.7435492065112));
#427389=CARTESIAN_POINT('Origin',(-0.370286103668523,2.7027527081533,14.));
#427390=CARTESIAN_POINT('Origin',(-0.370286103668523,2.7027527081533,12.5369868989719));
#427391=CARTESIAN_POINT('Ctrl Pts',(-0.407093856453013,2.71316699868649,
12.506462012331));
#427392=CARTESIAN_POINT('Ctrl Pts',(-0.408064075637327,2.71963323891745,
12.4999388158272));
#427393=CARTESIAN_POINT('Ctrl Pts',(-0.408052596672013,2.71955673481557,
12.4907030323752));
#427394=CARTESIAN_POINT('Ctrl Pts',(-0.394494611539127,2.71734881775887,
12.5042014951931));
#427395=CARTESIAN_POINT('Ctrl Pts',(-0.390348035787285,2.72226277814235,
12.4980716682126));
#427396=CARTESIAN_POINT('Ctrl Pts',(-0.383624575490615,2.72322228158951,
12.4907355092743));
#427397=CARTESIAN_POINT('Ctrl Pts',(-0.390526476627142,2.71281234263312,
12.521804744651));
#427398=CARTESIAN_POINT('Ctrl Pts',(-0.38471641496952,2.72309641062548,
12.5216906929435));
#427399=CARTESIAN_POINT('Ctrl Pts',(-0.373047088808023,2.72457883474397,
12.5161988840776));
#427400=CARTESIAN_POINT('Ctrl Pts',(-0.391707539933291,2.70776490012432,
12.5369868989719));
#427401=CARTESIAN_POINT('Ctrl Pts',(-0.388214978467543,2.7226916394176,
12.5369868989719));
#427402=CARTESIAN_POINT('Ctrl Pts',(-0.373002382684925,2.72458437845827,
12.5369868989719));
#427403=CARTESIAN_POINT('Origin',(-8.37054729992257E-32,-6.84555113983452E-33,
12.5));
#427404=CARTESIAN_POINT('Origin',(-0.619548319923707,2.61100558037706,12.5));
#427405=CARTESIAN_POINT('',(-0.619548319923707,2.61100558037706,12.5893111709658));
#427406=CARTESIAN_POINT('',(-0.619548319923707,2.61100558037706,13.8235269408515));
#427407=CARTESIAN_POINT('',(-0.619548319923707,2.61100558037706,12.5));
#427408=CARTESIAN_POINT('',(-0.614203671726777,2.64637092266089,13.7902182540695));
#427409=CARTESIAN_POINT('',(-0.619548319923707,2.61100558037706,13.8235269408515));
#427410=CARTESIAN_POINT('',(-0.611106435078542,2.66686522465476,13.7435492065112));
#427411=CARTESIAN_POINT('Origin',(-0.621296624808806,2.59943929067106,13.7445212918714));
#427412=CARTESIAN_POINT('',(-0.611106435078542,2.66686522465476,12.5369868989719));
#427413=CARTESIAN_POINT('',(-0.611106435078542,2.66686522465476,12.5));
#427414=CARTESIAN_POINT('Ctrl Pts',(-0.611106435078542,2.66686522465476,
12.5369868989719));
#427415=CARTESIAN_POINT('Ctrl Pts',(-0.613918344361144,2.64825892343788,
12.5544431401645));
#427416=CARTESIAN_POINT('Ctrl Pts',(-0.616732264796001,2.62963931449985,
12.5718848856037));
#427417=CARTESIAN_POINT('Ctrl Pts',(-0.619548319923707,2.61100558037706,
12.5893111709658));
#427418=CARTESIAN_POINT('Origin',(-0.845256230282979,2.8162684905147,12.5));
#427419=CARTESIAN_POINT('',(-0.714837180221226,2.64095229173884,13.7435492065112));
#427420=CARTESIAN_POINT('',(-0.702465907569606,2.62432217141305,13.7902182540695));
#427421=CARTESIAN_POINT('Origin',(-0.669956341227117,2.58062108945978,13.7418732680448));
#427422=CARTESIAN_POINT('',(-0.681117813258215,2.59562493167691,13.8235269408515));
#427423=CARTESIAN_POINT('',(-0.702465907569606,2.62432217141305,13.7902182540695));
#427424=CARTESIAN_POINT('',(-0.681117813258215,2.59562493167691,12.5893111709658));
#427425=CARTESIAN_POINT('',(-0.681117813258215,2.59562493167691,12.5));
#427426=CARTESIAN_POINT('',(-0.714837180221226,2.64095229173884,12.5369868989719));
#427427=CARTESIAN_POINT('Ctrl Pts',(-0.681117813258215,2.59562493167691,
12.5893111709658));
#427428=CARTESIAN_POINT('Ctrl Pts',(-0.692365964350157,2.61074529248128,
12.5718848856037));
#427429=CARTESIAN_POINT('Ctrl Pts',(-0.703605588852024,2.62585419139138,
12.5544431401645));
#427430=CARTESIAN_POINT('Ctrl Pts',(-0.714837180221226,2.64095229173884,
12.5369868989719));
#427431=CARTESIAN_POINT('',(-0.714837180221226,2.64095229173884,12.5));
#427432=CARTESIAN_POINT('Origin',(-0.653537368403491,2.61614223380501,12.5));
#427433=CARTESIAN_POINT('',(-0.644124613647114,2.58308183120501,13.8587068136939));
#427434=CARTESIAN_POINT('Ctrl Pts',(-0.681117813263431,2.59562493167285,
13.8235269408542));
#427435=CARTESIAN_POINT('Ctrl Pts',(-0.680071924268647,2.59421899225819,
13.8262006681044));
#427436=CARTESIAN_POINT('Ctrl Pts',(-0.678862211642773,2.59288391795508,
13.8288634856214));
#427437=CARTESIAN_POINT('Ctrl Pts',(-0.677501420067256,2.59161578713848,
13.8314912288862));
#427438=CARTESIAN_POINT('Ctrl Pts',(-0.676098584312039,2.5903084750682,
13.8342001611531));
#427439=CARTESIAN_POINT('Ctrl Pts',(-0.674533970207235,2.58907049146711,
13.8368750301949));
#427440=CARTESIAN_POINT('Ctrl Pts',(-0.672779401734628,2.58791389361448,
13.8394886372968));
#427441=CARTESIAN_POINT('Ctrl Pts',(-0.672643892155498,2.58782456675681,
13.8396904925131));
#427442=CARTESIAN_POINT('Ctrl Pts',(-0.672507234333911,2.58773574146807,
13.8398919674349));
#427443=CARTESIAN_POINT('Ctrl Pts',(-0.672369408200813,2.58764743228681,
13.8400930404591));
#427444=CARTESIAN_POINT('Ctrl Pts',(-0.670221984322296,2.58627151583134,
13.8432258934518));
#427445=CARTESIAN_POINT('Ctrl Pts',(-0.667802508935009,2.5850269613997,
13.8462331177034));
#427446=CARTESIAN_POINT('Ctrl Pts',(-0.665145766550256,2.58404014231565,
13.8489036603661));
#427447=CARTESIAN_POINT('Ctrl Pts',(-0.664276449523898,2.58371724362716,
13.8497774930041));
#427448=CARTESIAN_POINT('Ctrl Pts',(-0.663381877274673,2.58342214115775,
13.85061494757));
#427449=CARTESIAN_POINT('Ctrl Pts',(-0.662463701712439,2.58315982958252,
13.8514076489583));
#427450=CARTESIAN_POINT('Ctrl Pts',(-0.660521627977569,2.5826050027699,
13.8530843267192));
#427451=CARTESIAN_POINT('Ctrl Pts',(-0.658282381615198,2.58214522256617,
13.8546805203176));
#427452=CARTESIAN_POINT('Ctrl Pts',(-0.655848484074212,2.58194083176989,
13.8559412814274));
#427453=CARTESIAN_POINT('Ctrl Pts',(-0.655522749650073,2.5819134776528,
13.8561100121513));
#427454=CARTESIAN_POINT('Ctrl Pts',(-0.655193583303564,2.58189064370139,
13.8562727473908));
#427455=CARTESIAN_POINT('Ctrl Pts',(-0.654861277483013,2.58187265450069,
13.8564289040185));
#427456=CARTESIAN_POINT('Ctrl Pts',(-0.65335427437784,2.58179107368073,
13.8571370725437));
#427457=CARTESIAN_POINT('Ctrl Pts',(-0.651756092511145,2.58180996973009,
13.8577210840554));
#427458=CARTESIAN_POINT('Ctrl Pts',(-0.650129200467877,2.58195795414735,
13.8581177131616));
#427459=CARTESIAN_POINT('Ctrl Pts',(-0.649671011672573,2.58199963165271,
13.8582294175695));
#427460=CARTESIAN_POINT('Ctrl Pts',(-0.649210564522325,2.58205137157636,
13.8583265086086));
#427461=CARTESIAN_POINT('Ctrl Pts',(-0.648749275031835,2.58211337395736,
13.8584082369006));
#427462=CARTESIAN_POINT('Ctrl Pts',(-0.648086525733664,2.58220245475225,
13.8585256585398));
#427463=CARTESIAN_POINT('Ctrl Pts',(-0.647413841217318,2.58231414724199,
13.8586122832068));
#427464=CARTESIAN_POINT('Ctrl Pts',(-0.646748825225599,2.58244632900087,
13.8586682984299));
#427465=CARTESIAN_POINT('Ctrl Pts',(-0.646216878353138,2.58255206130522,
13.8587131050557));
#427466=CARTESIAN_POINT('Ctrl Pts',(-0.645683917050552,2.58267184132321,
13.8587357943552));
#427467=CARTESIAN_POINT('Ctrl Pts',(-0.645149989038243,2.58280617740864,
13.8587355499465));
#427468=CARTESIAN_POINT('Ctrl Pts',(-0.644804898634477,2.58289300202337,
13.8587353919793));
#427469=CARTESIAN_POINT('Ctrl Pts',(-0.644463126728151,2.58298493079649,
13.8587257282814));
#427470=CARTESIAN_POINT('Ctrl Pts',(-0.644124613647114,2.58308183120501,
13.8587068136939));
#427471=CARTESIAN_POINT('Ctrl Pts',(-0.644124613647114,2.58308183120501,
13.8587068136939));
#427472=CARTESIAN_POINT('Ctrl Pts',(-0.643011262577741,2.58340053136607,
13.8586446046466));
#427473=CARTESIAN_POINT('Ctrl Pts',(-0.641933118551584,2.58377294442342,
13.858482427929));
#427474=CARTESIAN_POINT('Ctrl Pts',(-0.640888435961713,2.58419495469807,
13.8582284286032));
#427475=CARTESIAN_POINT('Ctrl Pts',(-0.639816713147,2.5846278881496,13.8579678548414));
#427476=CARTESIAN_POINT('Ctrl Pts',(-0.638778162154673,2.58511549725576,
13.857615680862));
#427477=CARTESIAN_POINT('Ctrl Pts',(-0.637809609004724,2.58562978735214,
13.8571944833187));
#427478=CARTESIAN_POINT('Ctrl Pts',(-0.63539248556353,2.58691325088495,
13.8561433417727));
#427479=CARTESIAN_POINT('Ctrl Pts',(-0.633295996435442,2.58841868548779,
13.8546163505474));
#427480=CARTESIAN_POINT('Ctrl Pts',(-0.631539601917027,2.58994022915956,
13.8528973491086));
#427481=CARTESIAN_POINT('Ctrl Pts',(-0.631218734551702,2.5902181927401,
13.8525833129072));
#427482=CARTESIAN_POINT('Ctrl Pts',(-0.630909086054786,2.59049664194987,
13.8522628768812));
#427483=CARTESIAN_POINT('Ctrl Pts',(-0.630610600565828,2.59077428266382,
13.851937733538));
#427484=CARTESIAN_POINT('Ctrl Pts',(-0.62878779109773,2.59246979598301,
13.8499521282529));
#427485=CARTESIAN_POINT('Ctrl Pts',(-0.627202916742444,2.5943066457283,
13.847639871647));
#427486=CARTESIAN_POINT('Ctrl Pts',(-0.625878444452019,2.59613580997153,
13.8452109780794));
#427487=CARTESIAN_POINT('Ctrl Pts',(-0.625282536953345,2.59695878882638,
13.8441181685877));
#427488=CARTESIAN_POINT('Ctrl Pts',(-0.624738651211423,2.59778001799223,
13.8430021611332));
#427489=CARTESIAN_POINT('Ctrl Pts',(-0.624245527489944,2.59858606088166,
13.8418824960098));
#427490=CARTESIAN_POINT('Ctrl Pts',(-0.623083468847915,2.60048552153364,
13.8392439765549));
#427491=CARTESIAN_POINT('Ctrl Pts',(-0.622144524779294,2.60238947799269,
13.8364981347964));
#427492=CARTESIAN_POINT('Ctrl Pts',(-0.621395520785306,2.60428782992262,
13.8336931113419));
#427493=CARTESIAN_POINT('Ctrl Pts',(-0.620666038461315,2.60613670414588,
13.8309611966328));
#427494=CARTESIAN_POINT('Ctrl Pts',(-0.620116518263491,2.60798232206115,
13.8281701127186));
#427495=CARTESIAN_POINT('Ctrl Pts',(-0.619755612381567,2.60981548820858,
13.8253580685121));
#427496=CARTESIAN_POINT('Ctrl Pts',(-0.619677367596864,2.61021292060776,
13.8247484142933));
#427497=CARTESIAN_POINT('Ctrl Pts',(-0.619608147908461,2.61060970078293,
13.8241378483365));
#427498=CARTESIAN_POINT('Ctrl Pts',(-0.619548319923707,2.61100558037706,
13.8235269408515));
#427499=CARTESIAN_POINT('',(-0.645325162980033,2.58276330623435,12.5969504640361));
#427500=CARTESIAN_POINT('Origin',(-0.653545197073089,2.61617438026271,12.584524458991));
#427501=CARTESIAN_POINT('Origin',(-0.653545197073089,2.61617438026271,12.584524458991));
#427502=CARTESIAN_POINT('Ctrl Pts',(-0.681117813258215,2.59562493167691,
12.5893111709658));
#427503=CARTESIAN_POINT('Ctrl Pts',(-0.67435294727123,2.58653124030664,
12.5770542771492));
#427504=CARTESIAN_POINT('Ctrl Pts',(-0.659632051107227,2.59367958913581,
12.5737548217797));
#427505=CARTESIAN_POINT('Ctrl Pts',(-0.695910304815245,2.61550978277018,
12.5663937883685));
#427506=CARTESIAN_POINT('Ctrl Pts',(-0.689136809302223,2.60640449113366,
12.5540940315304));
#427507=CARTESIAN_POINT('Ctrl Pts',(-0.674371698760894,2.61357787987369,
12.5508374392248));
#427508=CARTESIAN_POINT('Ctrl Pts',(-0.710687870929649,2.63537457029247,
12.5434499600945));
#427509=CARTESIAN_POINT('Ctrl Pts',(-0.703892352370572,2.62623967411034,
12.5311293540533));
#427510=CARTESIAN_POINT('Ctrl Pts',(-0.689097893551968,2.63345602726317,
12.5278936106989));
#427511=CARTESIAN_POINT('Ctrl Pts',(-0.725451680731751,2.65522086585074,
12.5204817579905));
#427512=CARTESIAN_POINT('Ctrl Pts',(-0.718622528999914,2.64604075817535,
12.5081597038247));
#427513=CARTESIAN_POINT('Ctrl Pts',(-0.703811692222104,2.65331558867755,
12.5049254088044));
#427514=CARTESIAN_POINT('Ctrl Pts',(-0.714837180221225,2.64095229173884,
12.5369868989719));
#427515=CARTESIAN_POINT('Ctrl Pts',(-0.715393164532816,2.64169967558667,
12.5342545179733));
#427516=CARTESIAN_POINT('Ctrl Pts',(-0.715823681793893,2.64248740142811,
12.5314872231885));
#427517=CARTESIAN_POINT('Ctrl Pts',(-0.716055427367871,2.64329790441951,
12.5287124745063));
#427518=CARTESIAN_POINT('Ctrl Pts',(-0.716264427029309,2.64402885624694,
12.5262100684184));
#427519=CARTESIAN_POINT('Ctrl Pts',(-0.716310602552072,2.64477786636624,
12.5237004536639));
#427520=CARTESIAN_POINT('Ctrl Pts',(-0.716128581799546,2.64556187466791,
12.5212220730815));
#427521=CARTESIAN_POINT('Ctrl Pts',(-0.715989229167435,2.64616210084496,
12.5193246583486));
#427522=CARTESIAN_POINT('Ctrl Pts',(-0.7157138419125,2.64678987029541,12.517417831369));
#427523=CARTESIAN_POINT('Ctrl Pts',(-0.715207422288142,2.64742445982225,
12.5155812248347));
#427524=CARTESIAN_POINT('Ctrl Pts',(-0.71499168480615,2.64769479837161,
12.5147988205793));
#427525=CARTESIAN_POINT('Ctrl Pts',(-0.714734016959458,2.64796682185866,
12.5140295443047));
#427526=CARTESIAN_POINT('Ctrl Pts',(-0.714427699700277,2.64824096140262,
12.5132817086137));
#427527=CARTESIAN_POINT('Ctrl Pts',(-0.713964129966165,2.64865583451764,
12.5121499604604));
#427528=CARTESIAN_POINT('Ctrl Pts',(-0.713374360014477,2.64907918368906,
12.5110494206568));
#427529=CARTESIAN_POINT('Ctrl Pts',(-0.712628093305165,2.64948935208408,
12.5100666561695));
#427530=CARTESIAN_POINT('Ctrl Pts',(-0.712199588679178,2.64972486983197,
12.5095023550641));
#427531=CARTESIAN_POINT('Ctrl Pts',(-0.711714221219373,2.6499581909934,
12.5089719619137));
#427532=CARTESIAN_POINT('Ctrl Pts',(-0.711178321435369,2.65017918580885,
12.5085043804652));
#427533=CARTESIAN_POINT('Ctrl Pts',(-0.710394101907337,2.65050258293467,
12.5078201359221));
#427534=CARTESIAN_POINT('Ctrl Pts',(-0.709478464436223,2.65080784681095,
12.5072563000949));
#427535=CARTESIAN_POINT('Ctrl Pts',(-0.70849079814604,2.65106625363288,
12.5068768744332));
#427536=CARTESIAN_POINT('Ctrl Pts',(-0.707778622759639,2.65125258274028,
12.5066032824114));
#427537=CARTESIAN_POINT('Ctrl Pts',(-0.707016500041307,2.65141788060135,
12.5064197834844));
#427538=CARTESIAN_POINT('Ctrl Pts',(-0.706247536796213,2.65155544267816,
12.5063282718343));
#427539=CARTESIAN_POINT('Ctrl Pts',(-0.705125088523378,2.65175624072215,
12.5061946931565));
#427540=CARTESIAN_POINT('Ctrl Pts',(-0.703964261217886,2.65190327965168,
12.5062515701262));
#427541=CARTESIAN_POINT('Ctrl Pts',(-0.702839041189455,2.65200277591458,
12.5064436508398));
#427542=CARTESIAN_POINT('',(-0.659632051107227,2.59367958913581,12.5737548217797));
#427543=CARTESIAN_POINT('Origin',(-0.663466328551192,2.6087560050389,12.5893111709658));
#427544=CARTESIAN_POINT('Ctrl Pts',(-0.702839041189455,2.65200277591458,
12.5064436508398));
#427545=CARTESIAN_POINT('Ctrl Pts',(-0.696442898066279,2.64336971499165,
12.5164271754438));
#427546=CARTESIAN_POINT('Ctrl Pts',(-0.690044387393246,2.63473310754498,
12.5264061185523));
#427547=CARTESIAN_POINT('Ctrl Pts',(-0.68364342502673,2.62609282923241,
12.536380305637));
#427548=CARTESIAN_POINT('Ctrl Pts',(-0.675643520323638,2.61529423377897,
12.5488460165097));
#427549=CARTESIAN_POINT('Ctrl Pts',(-0.66763978374881,2.60448990125433,
12.5613043021964));
#427550=CARTESIAN_POINT('Ctrl Pts',(-0.659632051107227,2.59367958913581,
12.5737548217797));
#427551=CARTESIAN_POINT('Ctrl Pts',(-0.619548319923707,2.61100558037706,
12.5893111709658));
#427552=CARTESIAN_POINT('Ctrl Pts',(-0.621241952538985,2.59979887510191,
12.5770542771492));
#427553=CARTESIAN_POINT('Ctrl Pts',(-0.637595128669095,2.59918462327036,
12.5737548217797));
#427554=CARTESIAN_POINT('Ctrl Pts',(-0.621128464423323,2.60054982182612,
12.5928319619712));
#427555=CARTESIAN_POINT('Ctrl Pts',(-0.625487855889913,2.59350502783251,
12.5821634970842));
#427556=CARTESIAN_POINT('Ctrl Pts',(-0.638161404184726,2.59537443306385,
12.5773203894503));
#427557=CARTESIAN_POINT('Ctrl Pts',(-0.630311597441073,2.58654074736283,
12.5969440695591));
#427558=CARTESIAN_POINT('Ctrl Pts',(-0.634207051578876,2.58554878989792,
12.5878292599214));
#427559=CARTESIAN_POINT('Ctrl Pts',(-0.641436171293958,2.59038243471871,
12.5813877129824));
#427560=CARTESIAN_POINT('Ctrl Pts',(-0.659983243458332,2.57907290509295,
12.596957478804));
#427561=CARTESIAN_POINT('Ctrl Pts',(-0.656116597551942,2.58005760940567,
12.5878468778671));
#427562=CARTESIAN_POINT('Ctrl Pts',(-0.652057520626844,2.58771537516689,
12.5814011370086));
#427563=CARTESIAN_POINT('Ctrl Pts',(-0.674797087754222,2.58712827748144,
12.5928371701607));
#427564=CARTESIAN_POINT('Ctrl Pts',(-0.667638948597393,2.58296941832113,
12.5821692192952));
#427565=CARTESIAN_POINT('Ctrl Pts',(-0.657333350697047,2.59057326431407,
12.5773318885715));
#427566=CARTESIAN_POINT('Ctrl Pts',(-0.681117813258257,2.59562493167688,
12.5893111709658));
#427567=CARTESIAN_POINT('Ctrl Pts',(-0.674352947271273,2.5865312403066,
12.5770542771492));
#427568=CARTESIAN_POINT('Ctrl Pts',(-0.659632051107271,2.59367958913578,
12.5737548217797));
#427569=CARTESIAN_POINT('',(-0.637595128669095,2.59918462327036,12.5737548217797));
#427570=CARTESIAN_POINT('Origin',(-0.641301310950769,2.61429303857095,12.5893111709658));
#427571=CARTESIAN_POINT('Ctrl Pts',(-0.659632051107271,2.59367958913578,
12.5737548217797));
#427572=CARTESIAN_POINT('Ctrl Pts',(-0.65906043991165,2.59285643649376,
12.5746934679442));
#427573=CARTESIAN_POINT('Ctrl Pts',(-0.658277450054665,2.59205004805008,
12.5756680099006));
#427574=CARTESIAN_POINT('Ctrl Pts',(-0.657374552621003,2.59134984815557,
12.5765688348656));
#427575=CARTESIAN_POINT('Ctrl Pts',(-0.657135520520848,2.59116447798497,
12.5768073183026));
#427576=CARTESIAN_POINT('Ctrl Pts',(-0.656888286740824,2.59098639152223,
12.5770407398754));
#427577=CARTESIAN_POINT('Ctrl Pts',(-0.656634889972081,2.59081680018845,
12.5772674179684));
#427578=CARTESIAN_POINT('Ctrl Pts',(-0.655595018154532,2.59012084321406,
12.5781976435658));
#427579=CARTESIAN_POINT('Ctrl Pts',(-0.654386021859309,2.58953779481049,
12.5790594849312));
#427580=CARTESIAN_POINT('Ctrl Pts',(-0.653068558396651,2.58915051874844,
12.5797571720116));
#427581=CARTESIAN_POINT('Ctrl Pts',(-0.652210183578965,2.58889819446881,
12.580211740231));
#427582=CARTESIAN_POINT('Ctrl Pts',(-0.651261461391678,2.58873551935799,
12.5806009430798));
#427583=CARTESIAN_POINT('Ctrl Pts',(-0.650286183608314,2.58869140689267,
12.5808812374708));
#427584=CARTESIAN_POINT('Ctrl Pts',(-0.649448096447365,2.58865349965081,
12.5811221033394));
#427585=CARTESIAN_POINT('Ctrl Pts',(-0.648573236243005,2.5887024830718,
12.581287365893));
#427586=CARTESIAN_POINT('Ctrl Pts',(-0.647711447628746,2.58884391739505,
12.581359338449));
#427587=CARTESIAN_POINT('Ctrl Pts',(-0.647591676806622,2.58886357384547,
12.5813693411482));
#427588=CARTESIAN_POINT('Ctrl Pts',(-0.647472129629909,2.58888496353217,
12.5813775999465));
#427589=CARTESIAN_POINT('Ctrl Pts',(-0.647352909413546,2.58890804815248,
12.5813841266931));
#427590=CARTESIAN_POINT('Ctrl Pts',(-0.647150637897095,2.58894721400287,
12.5813952001081));
#427591=CARTESIAN_POINT('Ctrl Pts',(-0.646948068571554,2.58899211884071,
12.5814007534795));
#427592=CARTESIAN_POINT('Ctrl Pts',(-0.646745332343135,2.58904293564436,
12.5814005856065));
#427593=CARTESIAN_POINT('Ctrl Pts',(-0.645817285154161,2.58927555510339,
12.5813998171494));
#427594=CARTESIAN_POINT('Ctrl Pts',(-0.64494977947355,2.58961565728625,
12.58127954464));
#427595=CARTESIAN_POINT('Ctrl Pts',(-0.644136940372809,2.59003376337738,
12.5810700125799));
#427596=CARTESIAN_POINT('Ctrl Pts',(-0.643155123288255,2.59053878793026,
12.5808169217085));
#427597=CARTESIAN_POINT('Ctrl Pts',(-0.642260630638001,2.59117254755197,
12.5804173076348));
#427598=CARTESIAN_POINT('Ctrl Pts',(-0.641516798766718,2.59185825121603,
12.5799304713245));
#427599=CARTESIAN_POINT('Ctrl Pts',(-0.640594956746993,2.59270805407474,
12.5793271277669));
#427600=CARTESIAN_POINT('Ctrl Pts',(-0.639825506148532,2.59366667735055,
12.5785808224116));
#427601=CARTESIAN_POINT('Ctrl Pts',(-0.639216146240733,2.59467385974008,
12.5777485681082));
#427602=CARTESIAN_POINT('Ctrl Pts',(-0.638308133217751,2.59617467184554,
12.576508418016));
#427603=CARTESIAN_POINT('Ctrl Pts',(-0.637757355590619,2.59776711133143,
12.5750928681475));
#427604=CARTESIAN_POINT('Ctrl Pts',(-0.637595128669095,2.59918462327036,
12.5737548217797));
#427605=CARTESIAN_POINT('Ctrl Pts',(-0.637595128669095,2.59918462327036,
12.5737548217797));
#427606=CARTESIAN_POINT('Ctrl Pts',(-0.621241952538985,2.59979887510191,
12.5770542771492));
#427607=CARTESIAN_POINT('Ctrl Pts',(-0.619548319923707,2.61100558037706,
12.5893111709658));
#427608=CARTESIAN_POINT('Ctrl Pts',(-0.633945227133948,2.62367325681644,
12.5508408821982));
#427609=CARTESIAN_POINT('Ctrl Pts',(-0.617541263428884,2.62428620003755,
12.55409748406));
#427610=CARTESIAN_POINT('Ctrl Pts',(-0.615845470172143,2.63550720219847,
12.5663972313419));
#427611=CARTESIAN_POINT('Ctrl Pts',(-0.630297724466514,2.64813779417324,
12.52790050457));
#427612=CARTESIAN_POINT('Ctrl Pts',(-0.613847662019243,2.64872662591756,
12.5311362602938));
#427613=CARTESIAN_POINT('Ctrl Pts',(-0.612146355987524,2.65998410590958,
12.5434568539655));
#427614=CARTESIAN_POINT('Ctrl Pts',(-0.626652420547208,2.6725801058825,
12.5049357605811));
#427615=CARTESIAN_POINT('Ctrl Pts',(-0.61016040945356,2.67312504172859,
12.5081700652078));
#427616=CARTESIAN_POINT('Ctrl Pts',(-0.608450684799481,2.68443822743786,
12.5204921097672));
#427617=CARTESIAN_POINT('Ctrl Pts',(-0.626891783921935,2.67097512765063,
12.5064436508395));
#427618=CARTESIAN_POINT('Ctrl Pts',(-0.625768588916643,2.67145186738117,
12.5062361689309));
#427619=CARTESIAN_POINT('Ctrl Pts',(-0.62458022878413,2.67189974215819,
12.5061871075061));
#427620=CARTESIAN_POINT('Ctrl Pts',(-0.623407428471871,2.67226792155561,
12.5063648335164));
#427621=CARTESIAN_POINT('Ctrl Pts',(-0.62287467022872,2.67243517134816,
12.5064455676329));
#427622=CARTESIAN_POINT('Ctrl Pts',(-0.622337625953831,2.67258809829308,
12.506574497099));
#427623=CARTESIAN_POINT('Ctrl Pts',(-0.621819034671932,2.67271913457354,
12.5067492519495));
#427624=CARTESIAN_POINT('Ctrl Pts',(-0.620776905360758,2.67298245706555,
12.5071004286051));
#427625=CARTESIAN_POINT('Ctrl Pts',(-0.619770780414712,2.67316627753478,
12.5076537929612));
#427626=CARTESIAN_POINT('Ctrl Pts',(-0.618877874720707,2.673266103723,12.5083435010503));
#427627=CARTESIAN_POINT('Ctrl Pts',(-0.618821660971136,2.67327238837813,
12.5083869222963));
#427628=CARTESIAN_POINT('Ctrl Pts',(-0.618765888504668,2.67327832895009,
12.5084308732336));
#427629=CARTESIAN_POINT('Ctrl Pts',(-0.618710573223093,2.67328391998674,
12.5084753333615));
#427630=CARTESIAN_POINT('Ctrl Pts',(-0.618266871656053,2.67332876748015,
12.508831962269));
#427631=CARTESIAN_POINT('Ctrl Pts',(-0.61784370794673,2.67335331934408,
12.509227847131));
#427632=CARTESIAN_POINT('Ctrl Pts',(-0.617453827143522,2.67335964087574,
12.5096423454524));
#427633=CARTESIAN_POINT('Ctrl Pts',(-0.616232113260281,2.67337944975814,
12.5109411997424));
#427634=CARTESIAN_POINT('Ctrl Pts',(-0.615262223814655,2.67323113740892,
12.5124831113042));
#427635=CARTESIAN_POINT('Ctrl Pts',(-0.614493472563127,2.67299462104848,
12.5140723025008));
#427636=CARTESIAN_POINT('Ctrl Pts',(-0.614421439728871,2.67297245920645,
12.5142212114565));
#427637=CARTESIAN_POINT('Ctrl Pts',(-0.614351149231337,2.67294954077451,
12.5143705582413));
#427638=CARTESIAN_POINT('Ctrl Pts',(-0.614282546802396,2.67292594291943,
12.5145201959299));
#427639=CARTESIAN_POINT('Ctrl Pts',(-0.613401246464292,2.67262279333733,
12.5164425148273));
#427640=CARTESIAN_POINT('Ctrl Pts',(-0.612764842494584,2.67220728429206,
12.5184635205941));
#427641=CARTESIAN_POINT('Ctrl Pts',(-0.612292447645065,2.6717193561345,
12.5205025929158));
#427642=CARTESIAN_POINT('Ctrl Pts',(-0.612018439908361,2.67143633846346,
12.5216853356836));
#427643=CARTESIAN_POINT('Ctrl Pts',(-0.611799759939447,2.67112980326851,
12.5228750347131));
#427644=CARTESIAN_POINT('Ctrl Pts',(-0.61162354841163,2.67081269548555,
12.5240609649613));
#427645=CARTESIAN_POINT('Ctrl Pts',(-0.611191046670025,2.67003437144451,
12.5269717671326));
#427646=CARTESIAN_POINT('Ctrl Pts',(-0.611011302518143,2.66916540019756,
12.5299036066169));
#427647=CARTESIAN_POINT('Ctrl Pts',(-0.611003381232721,2.66823675097456,
12.5328133004019));
#427648=CARTESIAN_POINT('Ctrl Pts',(-0.610999578554476,2.66779094527389,
12.5342101228451));
#427649=CARTESIAN_POINT('Ctrl Pts',(-0.611035902273964,2.66733193819979,
12.5356023438238));
#427650=CARTESIAN_POINT('Ctrl Pts',(-0.611106435078542,2.66686522465476,
12.5369868989719));
#427651=CARTESIAN_POINT('Origin',(1.29852573867523,15.2673948607278,-1.23905631314464));
#427652=CARTESIAN_POINT('Ctrl Pts',(-0.714812266465859,2.64091873483605,
12.5369868989719));
#427653=CARTESIAN_POINT('Ctrl Pts',(-0.723944180760299,2.65324315956923,
12.5369868989719));
#427654=CARTESIAN_POINT('Ctrl Pts',(-0.738666032852597,2.64893614498169,
12.5369868989719));
#427655=CARTESIAN_POINT('Ctrl Pts',(-0.717899263843912,2.64508483298256,
12.5218025310015));
#427656=CARTESIAN_POINT('Ctrl Pts',(-0.727316801397066,2.65222387004222,
12.5216901060417));
#427657=CARTESIAN_POINT('Ctrl Pts',(-0.738621160399221,2.6489492900178,
12.5161920673678));
#427658=CARTESIAN_POINT('Ctrl Pts',(-0.716058773267108,2.65082492580684,
12.5042015548895));
#427659=CARTESIAN_POINT('Ctrl Pts',(-0.721817661437463,2.65369068086588,
12.4980677368514));
#427660=CARTESIAN_POINT('Ctrl Pts',(-0.728374159597134,2.65190095697487,
12.4907278922777));
#427661=CARTESIAN_POINT('Ctrl Pts',(-0.702833917340125,2.65198344227881,
12.506463626192));
#427662=CARTESIAN_POINT('Ctrl Pts',(-0.704510023850558,2.65830784780834,
12.4999376786891));
#427663=CARTESIAN_POINT('Ctrl Pts',(-0.70448955264659,2.65823060439047,
12.4906970594712));
#427664=CARTESIAN_POINT('Origin',(-0.732488664928249,2.62782121837686,12.5369868989719));
#427665=CARTESIAN_POINT('Origin',(-0.732488664928249,2.62782121837686,14.));
#427666=CARTESIAN_POINT('Origin',(-0.732488664928249,2.62782121837686,13.7435492065112));
#427667=CARTESIAN_POINT('Ctrl Pts',(-0.700058713744277,2.62108624841145,
13.793642941384));
#427668=CARTESIAN_POINT('Ctrl Pts',(-0.706490367527905,2.62977762624316,
13.8071662555867));
#427669=CARTESIAN_POINT('Ctrl Pts',(-0.721520360485517,2.62177021122151,
13.8103758687955));
#427670=CARTESIAN_POINT('Ctrl Pts',(-0.709979310257147,2.63442204497754,
13.7804579775006));
#427671=CARTESIAN_POINT('Ctrl Pts',(-0.717923541283087,2.64514038743966,
13.7901904343351));
#427672=CARTESIAN_POINT('Ctrl Pts',(-0.732844745003035,2.64007939902705,
13.7927914348262));
#427673=CARTESIAN_POINT('Ctrl Pts',(-0.715819938808819,2.64227333027577,
13.7597120340895));
#427674=CARTESIAN_POINT('Ctrl Pts',(-0.725018255081397,2.65467405879156,
13.7635825532445));
#427675=CARTESIAN_POINT('Ctrl Pts',(-0.739544461666612,2.65086285971679,
13.7651073818885));
#427676=CARTESIAN_POINT('Ctrl Pts',(-0.714676210003871,2.64073586883991,
13.7381884353898));
#427677=CARTESIAN_POINT('Ctrl Pts',(-0.723658500634108,2.65284687068369,
13.7368803041982));
#427678=CARTESIAN_POINT('Ctrl Pts',(-0.738232877867184,2.64875087686204,
13.7363986145813));
#427679=CARTESIAN_POINT('Origin',(-0.720117392276629,2.61119109805107,13.7902182540695));
#427680=CARTESIAN_POINT('Ctrl Pts',(-0.681115464480307,2.59562177305366,
13.8235227101244));
#427681=CARTESIAN_POINT('Ctrl Pts',(-0.68797413001214,2.60484898256911,
13.8358800583119));
#427682=CARTESIAN_POINT('Ctrl Pts',(-0.702832413857604,2.597510219034,13.8390832900376));
#427683=CARTESIAN_POINT('Ctrl Pts',(-0.688234642642779,2.60519174962549,
13.8124254819053));
#427684=CARTESIAN_POINT('Ctrl Pts',(-0.69510662782911,2.61443687808509,
13.8247886449157));
#427685=CARTESIAN_POINT('Ctrl Pts',(-0.709976137757826,2.60707355983978,
13.8279860620657));
#427686=CARTESIAN_POINT('Ctrl Pts',(-0.695350630221196,2.61475743724518,
13.8013225099955));
#427687=CARTESIAN_POINT('Ctrl Pts',(-0.702232690979661,2.62401612362875,
13.8136962257787));
#427688=CARTESIAN_POINT('Ctrl Pts',(-0.717116337306965,2.6166326355042,
13.8168830918626));
#427689=CARTESIAN_POINT('Ctrl Pts',(-0.702463551356287,2.62431900278925,
13.7902140179785));
#427690=CARTESIAN_POINT('Ctrl Pts',(-0.709352655631513,2.63358717109964,
13.802602731458));
#427691=CARTESIAN_POINT('Ctrl Pts',(-0.724253149510978,2.62618761471636,
13.8057746032558));
#427692=CARTESIAN_POINT('Origin',(-0.698769297965238,2.58249385831493,13.8235269408515));
#427693=CARTESIAN_POINT('Ctrl Pts',(-0.619548319923707,2.61100558037706,
13.8235269408515));
#427694=CARTESIAN_POINT('Ctrl Pts',(-0.617783928936189,2.62268049122187,
13.8362179249168));
#427695=CARTESIAN_POINT('Ctrl Pts',(-0.600707111582438,2.6228933600169,
13.8391868794938));
#427696=CARTESIAN_POINT('Ctrl Pts',(-0.621162660877916,2.60032354513268,
13.8400110824519));
#427697=CARTESIAN_POINT('Ctrl Pts',(-0.616365462025495,2.6091727680382,
13.8494522556837));
#427698=CARTESIAN_POINT('Ctrl Pts',(-0.603474956463533,2.60533053512058,
13.85569149686));
#427699=CARTESIAN_POINT('Ctrl Pts',(-0.629977800041478,2.58662350690017,
13.8586819406588));
#427700=CARTESIAN_POINT('Ctrl Pts',(-0.625757144509834,2.58769220260906,
13.868010383617));
#427701=CARTESIAN_POINT('Ctrl Pts',(-0.618231041938688,2.58266720043183,
13.8744918421245));
#427702=CARTESIAN_POINT('Ctrl Pts',(-0.660322213356513,2.57898884394015,
13.8587686893867));
#427703=CARTESIAN_POINT('Ctrl Pts',(-0.664505291271827,2.57792960502741,
13.8680909899357));
#427704=CARTESIAN_POINT('Ctrl Pts',(-0.66874620679676,2.56996022380826,
13.8745789365163));
#427705=CARTESIAN_POINT('Ctrl Pts',(-0.674659168776717,2.58694287947182,
13.8400379222776));
#427706=CARTESIAN_POINT('Ctrl Pts',(-0.683056149301072,2.59248913514406,
13.8494748685453));
#427707=CARTESIAN_POINT('Ctrl Pts',(-0.692621784022613,2.58304139797377,
13.8557104837033));
#427708=CARTESIAN_POINT('Ctrl Pts',(-0.681117813263431,2.59562493167285,
13.8235269408542));
#427709=CARTESIAN_POINT('Ctrl Pts',(-0.688165308966787,2.60509854888603,
13.8362179249195));
#427710=CARTESIAN_POINT('Ctrl Pts',(-0.703336074958441,2.59725566272831,
13.8391868794965));
#427711=CARTESIAN_POINT('Origin',(-0.597795328896645,2.60771812218317,13.8235269408515));
#427712=CARTESIAN_POINT('Ctrl Pts',(-0.614204260161081,2.64636702392679,
13.7902140241682));
#427713=CARTESIAN_POINT('Ctrl Pts',(-0.612483030422494,2.65778612912728,
13.8026027327198));
#427714=CARTESIAN_POINT('Ctrl Pts',(-0.595853226194454,2.65826314444243,
13.8057746032556));
#427715=CARTESIAN_POINT('Ctrl Pts',(-0.615985030875118,2.63458372903589,
13.8013225161807));
#427716=CARTESIAN_POINT('Ctrl Pts',(-0.614265558119394,2.64599115386919,
13.8136962270464));
#427717=CARTESIAN_POINT('Ctrl Pts',(-0.597658178658661,2.64647442683644,
13.8168830918628));
#427718=CARTESIAN_POINT('Ctrl Pts',(-0.617766569295444,2.62279535426053,
13.8124254880876));
#427719=CARTESIAN_POINT('Ctrl Pts',(-0.616049612549406,2.63418607568515,
13.8247886461868));
#427720=CARTESIAN_POINT('Ctrl Pts',(-0.599464194081469,2.63468050105057,
13.8279860620656));
#427721=CARTESIAN_POINT('Ctrl Pts',(-0.619548906501818,2.61100169394711,
13.8235227163065));
#427722=CARTESIAN_POINT('Ctrl Pts',(-0.617835277872275,2.62237033767259,
13.8358800595847));
#427723=CARTESIAN_POINT('Ctrl Pts',(-0.601271314044096,2.62288115378159,
13.8390832900376));
#427724=CARTESIAN_POINT('Origin',(-0.592450680699715,2.643083464467,13.7902182540695));
#427725=CARTESIAN_POINT('Ctrl Pts',(-0.611146732946785,2.6665983905316,
13.7382347919292));
#427726=CARTESIAN_POINT('Ctrl Pts',(-0.608915520826138,2.68152285237136,
13.7369371795942));
#427727=CARTESIAN_POINT('Ctrl Pts',(-0.594113895786784,2.68475637571517,
13.7364597369711));
#427728=CARTESIAN_POINT('Ctrl Pts',(-0.61086407789628,2.66846871138821,
13.7595490285574));
#427729=CARTESIAN_POINT('Ctrl Pts',(-0.608578636593199,2.68374910943501,
13.7633824266926));
#427730=CARTESIAN_POINT('Ctrl Pts',(-0.593951987877943,2.68720668194595,
13.7648920890506));
#427731=CARTESIAN_POINT('Ctrl Pts',(-0.612305603176639,2.6589301774852,
13.780380659011));
#427732=CARTESIAN_POINT('Ctrl Pts',(-0.610334117319525,2.67214797342552,
13.7901039518743));
#427733=CARTESIAN_POINT('Ctrl Pts',(-0.594781116764188,2.67471499799725,
13.7926933640891));
#427734=CARTESIAN_POINT('Ctrl Pts',(-0.614811295826587,2.64235007628175,
13.7936647693663));
#427735=CARTESIAN_POINT('Ctrl Pts',(-0.613224791711657,2.65304850311181,
13.8072068914933));
#427736=CARTESIAN_POINT('Ctrl Pts',(-0.596176501848199,2.65303941580986,
13.8104111085397));
#427737=CARTESIAN_POINT('Origin',(-0.58935344405148,2.66357776646087,13.7435492065112));
#427738=CARTESIAN_POINT('Origin',(-0.58935344405148,2.66357776646087,14.));
#427739=CARTESIAN_POINT('Origin',(-0.58935344405148,2.66357776646087,12.5369868989719));
#427740=CARTESIAN_POINT('Ctrl Pts',(-0.626887583435017,2.67095723074299,
12.506462012331));
#427741=CARTESIAN_POINT('Ctrl Pts',(-0.628381632903502,2.67732287322241,
12.4999388158272));
#427742=CARTESIAN_POINT('Ctrl Pts',(-0.628363956338964,2.67724755932385,
12.4907030323752));
#427743=CARTESIAN_POINT('Ctrl Pts',(-0.614671118545729,2.67615209058353,
12.5042014951932));
#427744=CARTESIAN_POINT('Ctrl Pts',(-0.610938873572858,2.68138768458791,
12.4980716682126));
#427745=CARTESIAN_POINT('Ctrl Pts',(-0.604315993474235,2.68289201979826,
12.4907355092743));
#427746=CARTESIAN_POINT('Ctrl Pts',(-0.610346422437987,2.67195415003824,
12.521804744651));
#427747=CARTESIAN_POINT('Ctrl Pts',(-0.605393940295253,2.68267757260581,
12.5216906929435));
#427748=CARTESIAN_POINT('Ctrl Pts',(-0.593884274181701,2.68510622249523,
12.5161988840776));
#427749=CARTESIAN_POINT('Ctrl Pts',(-0.61111214243078,2.6668272348541,12.5369868989719));
#427750=CARTESIAN_POINT('Ctrl Pts',(-0.608847870000681,2.68198898283656,
12.5369868989719));
#427751=CARTESIAN_POINT('Ctrl Pts',(-0.593840168678727,2.68511539172735,
12.5369868989719));
#427752=CARTESIAN_POINT('Origin',(-1.24861436930108E-31,-1.53597860469562E-32,
12.5));
#427753=CARTESIAN_POINT('Origin',(-0.830308018192218,2.55181873502139,12.5));
#427754=CARTESIAN_POINT('',(-0.830308018192218,2.55181873502139,12.5893111709658));
#427755=CARTESIAN_POINT('',(-0.830308018192218,2.55181873502139,13.8235269408515));
#427756=CARTESIAN_POINT('',(-0.830308018192218,2.55181873502139,12.5));
#427757=CARTESIAN_POINT('',(-0.827863757583213,2.58750204049155,13.7902182540695));
#427758=CARTESIAN_POINT('',(-0.830308018192218,2.55181873502139,13.8235269408515));
#427759=CARTESIAN_POINT('',(-0.826447302606738,2.60818060292636,13.7435492065112));
#427760=CARTESIAN_POINT('Origin',(-0.831107745750198,2.54014842810589,13.7445212918695));
#427761=CARTESIAN_POINT('',(-0.826447302606738,2.60818060292636,12.5369868989719));
#427762=CARTESIAN_POINT('',(-0.826447302606738,2.60818060292636,12.5));
#427763=CARTESIAN_POINT('Ctrl Pts',(-0.826447302606738,2.60818060292636,
12.5369868989719));
#427764=CARTESIAN_POINT('Ctrl Pts',(-0.82773326921152,2.58940701593085,
12.5544431401645));
#427765=CARTESIAN_POINT('Ctrl Pts',(-0.829020155573796,2.57062000156695,
12.5718848856037));
#427766=CARTESIAN_POINT('Ctrl Pts',(-0.830308018192218,2.55181873502139,
12.5893111709658));
#427767=CARTESIAN_POINT('Origin',(-1.07199573684347,2.73800135969425,12.5));
#427768=CARTESIAN_POINT('',(-0.927720747655564,2.57389887443867,13.7435492065112));
#427769=CARTESIAN_POINT('',(-0.914035130200078,2.55833246303678,13.7902182540695));
#427770=CARTESIAN_POINT('Origin',(-0.878071692878184,2.5174266242904,13.7418732680452));
#427771=CARTESIAN_POINT('',(-0.890418978460743,2.53147077887092,13.8235269408515));
#427772=CARTESIAN_POINT('',(-0.914035130200078,2.55833246303678,13.7902182540695));
#427773=CARTESIAN_POINT('',(-0.890418978460743,2.53147077887092,12.5893111709658));
#427774=CARTESIAN_POINT('',(-0.890418978460743,2.53147077887092,12.5));
#427775=CARTESIAN_POINT('',(-0.927720747655564,2.57389887443867,12.5369868989719));
#427776=CARTESIAN_POINT('Ctrl Pts',(-0.890418978460743,2.53147077887092,
12.5893111709658));
#427777=CARTESIAN_POINT('Ctrl Pts',(-0.90286215203397,2.54562399918532,
12.5718848856037));
#427778=CARTESIAN_POINT('Ctrl Pts',(-0.915295893137859,2.55976649074021,
12.5544431401645));
#427779=CARTESIAN_POINT('Ctrl Pts',(-0.927720747655564,2.57389887443867,
12.5369868989719));
#427780=CARTESIAN_POINT('',(-0.927720747655564,2.57389887443867,12.5));
#427781=CARTESIAN_POINT('Origin',(-0.864602655857827,2.55416787366877,12.5));
#427782=CARTESIAN_POINT('',(-0.852526491536523,2.52198470372759,13.8587068136939));
#427783=CARTESIAN_POINT('Ctrl Pts',(-0.890418978465611,2.53147077886645,
13.8235269408542));
#427784=CARTESIAN_POINT('Ctrl Pts',(-0.889261972465776,2.53015476726184,
13.8262006681044));
#427785=CARTESIAN_POINT('Ctrl Pts',(-0.88794746410894,2.52892273811777,
13.8288634856214));
#427786=CARTESIAN_POINT('Ctrl Pts',(-0.886487836020826,2.52776974404823,
13.8314912288862));
#427787=CARTESIAN_POINT('Ctrl Pts',(-0.884983110015638,2.52658112608835,
13.8342001611531));
#427788=CARTESIAN_POINT('Ctrl Pts',(-0.883322794878828,2.52547479235028,
13.8368750301949));
#427789=CARTESIAN_POINT('Ctrl Pts',(-0.881479791125753,2.52446505660073,
13.8394886372969));
#427790=CARTESIAN_POINT('Ctrl Pts',(-0.881337451475401,2.52438707225952,
13.8396904925131));
#427791=CARTESIAN_POINT('Ctrl Pts',(-0.881194008285796,2.52430968141073,
13.8398919674349));
#427792=CARTESIAN_POINT('Ctrl Pts',(-0.881049442739693,2.52423290018035,
13.8400930404591));
#427793=CARTESIAN_POINT('Ctrl Pts',(-0.878797014272475,2.52303659695519,
13.8432258934518));
#427794=CARTESIAN_POINT('Ctrl Pts',(-0.876284146749888,2.52199339338113,
13.8462331177034));
#427795=CARTESIAN_POINT('Ctrl Pts',(-0.873555809539721,2.52122640702453,
13.8489036603661));
#427796=CARTESIAN_POINT('Ctrl Pts',(-0.872663065853298,2.52097544016277,
13.8497774930041));
#427797=CARTESIAN_POINT('Ctrl Pts',(-0.871747416628582,2.52075423556561,
13.85061494757));
#427798=CARTESIAN_POINT('Ctrl Pts',(-0.870810915391224,2.52056763664275,
13.8514076489583));
#427799=CARTESIAN_POINT('Ctrl Pts',(-0.868830080210522,2.52017295300931,
13.8530843267192));
#427800=CARTESIAN_POINT('Ctrl Pts',(-0.866560808400721,2.51989722205296,
13.8546805203176));
#427801=CARTESIAN_POINT('Ctrl Pts',(-0.864118349705672,2.51989189659498,
13.8559412814273));
#427802=CARTESIAN_POINT('Ctrl Pts',(-0.863791469521455,2.519891183876,13.8561100121513));
#427803=CARTESIAN_POINT('Ctrl Pts',(-0.863461537269772,2.51989525601575,
13.8562727473908));
#427804=CARTESIAN_POINT('Ctrl Pts',(-0.863128870882547,2.51990441268198,
13.8564289040185));
#427805=CARTESIAN_POINT('Ctrl Pts',(-0.861620232611703,2.51994593805888,
13.8571370725437));
#427806=CARTESIAN_POINT('Ctrl Pts',(-0.860028908766775,2.52009503789213,
13.8577210840553));
#427807=CARTESIAN_POINT('Ctrl Pts',(-0.8584194921764,2.5203751367083,13.8581177131616));
#427808=CARTESIAN_POINT('Ctrl Pts',(-0.857966225070116,2.52045402217564,
13.8582294175695));
#427809=CARTESIAN_POINT('Ctrl Pts',(-0.857511527303881,2.52054312065629,
13.8583265086086));
#427810=CARTESIAN_POINT('Ctrl Pts',(-0.857056826485769,2.52064251610535,
13.8584082369006));
#427811=CARTESIAN_POINT('Ctrl Pts',(-0.856403543342984,2.52078532071172,
13.8585256585398));
#427812=CARTESIAN_POINT('Ctrl Pts',(-0.85574220110369,2.52095147158689,
13.8586122832068));
#427813=CARTESIAN_POINT('Ctrl Pts',(-0.855090171938288,2.52113741849891,
13.8586682984299));
#427814=CARTESIAN_POINT('Ctrl Pts',(-0.854568613239538,2.52128615759619,
13.8587131050557));
#427815=CARTESIAN_POINT('Ctrl Pts',(-0.854047188505169,2.52144898034998,
13.8587357943552));
#427816=CARTESIAN_POINT('Ctrl Pts',(-0.853525986732354,2.52162638953292,
13.8587355499465));
#427817=CARTESIAN_POINT('Ctrl Pts',(-0.853189121600519,2.5217410533175,
13.8587353919793));
#427818=CARTESIAN_POINT('Ctrl Pts',(-0.852855979960392,2.52186053378845,
13.8587257282814));
#427819=CARTESIAN_POINT('Ctrl Pts',(-0.852526491536523,2.52198470372759,
13.8587068136939));
#427820=CARTESIAN_POINT('Ctrl Pts',(-0.852526491536523,2.52198470372759,
13.8587068136939));
#427821=CARTESIAN_POINT('Ctrl Pts',(-0.851442822072846,2.52239309188814,
13.8586446046466));
#427822=CARTESIAN_POINT('Ctrl Pts',(-0.850398620603542,2.52285214451888,
13.858482427929));
#427823=CARTESIAN_POINT('Ctrl Pts',(-0.849391811864,2.52335790191855,13.8582284286032));
#427824=CARTESIAN_POINT('Ctrl Pts',(-0.848358943213999,2.52387675017852,
13.8579678548414));
#427825=CARTESIAN_POINT('Ctrl Pts',(-0.847363592583318,2.52444738835292,
13.857615680862));
#427826=CARTESIAN_POINT('Ctrl Pts',(-0.846440181631368,2.52503891326476,
13.8571944833187));
#427827=CARTESIAN_POINT('Ctrl Pts',(-0.84413571516204,2.52651512417848,
13.8561433417727));
#427828=CARTESIAN_POINT('Ctrl Pts',(-0.842168908824479,2.52818643289867,
13.8546163505474));
#427829=CARTESIAN_POINT('Ctrl Pts',(-0.8405423784985,2.52984607621821,13.8528973491086));
#427830=CARTESIAN_POINT('Ctrl Pts',(-0.840245235405169,2.53014926856692,
13.8525833129072));
#427831=CARTESIAN_POINT('Ctrl Pts',(-0.839959313433678,2.53045203048706,
13.8522628768812));
#427832=CARTESIAN_POINT('Ctrl Pts',(-0.839684451426241,2.53075307671278,
13.851937733538));
#427833=CARTESIAN_POINT('Ctrl Pts',(-0.838005907282168,2.53259152424506,
13.8499521282529));
#427834=CARTESIAN_POINT('Ctrl Pts',(-0.836576026772279,2.53455144399757,
13.847639871647));
#427835=CARTESIAN_POINT('Ctrl Pts',(-0.835405055421095,2.53648247863514,
13.8452109780794));
#427836=CARTESIAN_POINT('Ctrl Pts',(-0.834878211172296,2.53735129108902,
13.8441181685877));
#427837=CARTESIAN_POINT('Ctrl Pts',(-0.83440307296625,2.53821411941972,
13.8430021611332));
#427838=CARTESIAN_POINT('Ctrl Pts',(-0.8339772900517,2.53905767442917,13.8418824960098));
#427839=CARTESIAN_POINT('Ctrl Pts',(-0.832973921740808,2.54104553334987,
13.8392439765549));
#427840=CARTESIAN_POINT('Ctrl Pts',(-0.832193292058001,2.54301968720919,
13.8364981347964));
#427841=CARTESIAN_POINT('Ctrl Pts',(-0.831601513618745,2.5449727733086,
13.8336931113419));
#427842=CARTESIAN_POINT('Ctrl Pts',(-0.831025159000315,2.54687495513699,
13.8309611966328));
#427843=CARTESIAN_POINT('Ctrl Pts',(-0.830627902279593,2.54875922290853,
13.8281701127186));
#427844=CARTESIAN_POINT('Ctrl Pts',(-0.830417617341518,2.55061570652669,
13.8253580685121));
#427845=CARTESIAN_POINT('Ctrl Pts',(-0.830372027339997,2.55101819417869,
13.8247484142933));
#427846=CARTESIAN_POINT('Ctrl Pts',(-0.8303353792422,2.55141929614777,13.8241378483365));
#427847=CARTESIAN_POINT('Ctrl Pts',(-0.830308018192218,2.55181873502139,
13.8235269408515));
#427848=CARTESIAN_POINT('',(-0.853697083398605,2.52156938270644,12.5969504640361));
#427849=CARTESIAN_POINT('Origin',(-0.864613078712907,2.55419927505252,12.584524458991));
#427850=CARTESIAN_POINT('Origin',(-0.864613078712907,2.55419927505252,12.584524458991));
#427851=CARTESIAN_POINT('Ctrl Pts',(-0.890418978460743,2.53147077887093,
12.5893111709658));
#427852=CARTESIAN_POINT('Ctrl Pts',(-0.882935401738879,2.5229587453884,
12.5770542771492));
#427853=CARTESIAN_POINT('Ctrl Pts',(-0.868846144934083,2.53128319837604,
12.5737548217797));
#427854=CARTESIAN_POINT('Ctrl Pts',(-0.906783049188463,2.55008373937387,
12.5663937883685));
#427855=CARTESIAN_POINT('Ctrl Pts',(-0.899289926125211,2.54156084761049,
12.5540940315304));
#427856=CARTESIAN_POINT('Ctrl Pts',(-0.885158643047976,2.54991386107299,
12.5508374392248));
#427857=CARTESIAN_POINT('Ctrl Pts',(-0.923130608769454,2.56867791962787,
12.5434499600945));
#427858=CARTESIAN_POINT('Ctrl Pts',(-0.915613122894688,2.56012731690829,
12.5311293540533));
#427859=CARTESIAN_POINT('Ctrl Pts',(-0.90145609119268,2.56852554398007,
12.5278936106989));
#427860=CARTESIAN_POINT('Ctrl Pts',(-0.939462950544374,2.58725479071547,
12.5204817579905));
#427861=CARTESIAN_POINT('Ctrl Pts',(-0.931908258252054,2.57866186835596,
12.5081597038247));
#427862=CARTESIAN_POINT('Ctrl Pts',(-0.917739669533975,2.58711971315429,
12.5049254088044));
#427863=CARTESIAN_POINT('Ctrl Pts',(-0.927720747655562,2.57389887443867,
12.5369868989719));
#427864=CARTESIAN_POINT('Ctrl Pts',(-0.928335800697191,2.5745984535455,
12.5342545179733));
#427865=CARTESIAN_POINT('Ctrl Pts',(-0.928829092416563,2.57534846714068,
12.5314872231885));
#427866=CARTESIAN_POINT('Ctrl Pts',(-0.929126130394403,2.57613738383454,
12.5287124745063));
#427867=CARTESIAN_POINT('Ctrl Pts',(-0.929394013986471,2.57684886806739,
12.5262100684184));
#427868=CARTESIAN_POINT('Ctrl Pts',(-0.929501087142187,2.57759162218354,
12.5237004536639));
#427869=CARTESIAN_POINT('Ctrl Pts',(-0.929383576003663,2.57838785814339,
12.5212220730815));
#427870=CARTESIAN_POINT('Ctrl Pts',(-0.929293611061598,2.57899744565056,
12.5193246583486));
#427871=CARTESIAN_POINT('Ctrl Pts',(-0.929070309173177,2.57964557286779,
12.517417831369));
#427872=CARTESIAN_POINT('Ctrl Pts',(-0.928617299556025,2.58031932875108,
12.5155812248347));
#427873=CARTESIAN_POINT('Ctrl Pts',(-0.928424315024181,2.58060635237881,
12.5147988205793));
#427874=CARTESIAN_POINT('Ctrl Pts',(-0.928189676985529,2.58089847305173,
12.5140295443047));
#427875=CARTESIAN_POINT('Ctrl Pts',(-0.927906723889576,2.58119666811931,
12.5132817086137));
#427876=CARTESIAN_POINT('Ctrl Pts',(-0.92747851265588,2.58164794601516,
12.5121499604604));
#427877=CARTESIAN_POINT('Ctrl Pts',(-0.926925212002706,2.58211795825336,
12.5110494206568));
#427878=CARTESIAN_POINT('Ctrl Pts',(-0.926214860966318,2.58258758951169,
12.5100666561695));
#427879=CARTESIAN_POINT('Ctrl Pts',(-0.925806979037018,2.58285725069876,
12.5095023550641));
#427880=CARTESIAN_POINT('Ctrl Pts',(-0.925342244438101,2.58312935745719,
12.5089719619137));
#427881=CARTESIAN_POINT('Ctrl Pts',(-0.924826140945495,2.58339329773807,
12.5085043804652));
#427882=CARTESIAN_POINT('Ctrl Pts',(-0.924070890711275,2.5837795399585,
12.5078201359221));
#427883=CARTESIAN_POINT('Ctrl Pts',(-0.923183181789113,2.58415842104837,
12.5072563000953));
#427884=CARTESIAN_POINT('Ctrl Pts',(-0.922219864431952,2.58449647201457,
12.5068768744336));
#427885=CARTESIAN_POINT('Ctrl Pts',(-0.921525246302446,2.58474023003271,
12.5066032824118));
#427886=CARTESIAN_POINT('Ctrl Pts',(-0.920779132793865,2.58496709795591,
12.5064197834844));
#427887=CARTESIAN_POINT('Ctrl Pts',(-0.920023940796857,2.58516687994944,
12.5063282718343));
#427888=CARTESIAN_POINT('Ctrl Pts',(-0.918921594282759,2.58545849980904,
12.5061946931565));
#427889=CARTESIAN_POINT('Ctrl Pts',(-0.917776614572163,2.58569966768065,
12.5062515701262));
#427890=CARTESIAN_POINT('Ctrl Pts',(-0.916663248489658,2.5858905487563,
12.5064436508398));
#427891=CARTESIAN_POINT('',(-0.868846144934083,2.53128319837604,12.5737548217797));
#427892=CARTESIAN_POINT('Origin',(-0.873896531994877,2.54599691954154,12.5893111709658));
#427893=CARTESIAN_POINT('Ctrl Pts',(-0.916663248489658,2.5858905487563,
12.5064436508398));
#427894=CARTESIAN_POINT('Ctrl Pts',(-0.909584713394436,2.57780755867484,
12.5164271754438));
#427895=CARTESIAN_POINT('Ctrl Pts',(-0.902503529552574,2.5697212268477,
12.5264061185523));
#427896=CARTESIAN_POINT('Ctrl Pts',(-0.895419602965386,2.56163143620496,
12.536380305637));
#427897=CARTESIAN_POINT('Ctrl Pts',(-0.886566131506523,2.55152083868786,
12.5488460165097));
#427898=CARTESIAN_POINT('Ctrl Pts',(-0.877708373301593,2.54140483552231,
12.5613043021964));
#427899=CARTESIAN_POINT('Ctrl Pts',(-0.868846144934083,2.53128319837604,
12.5737548217797));
#427900=CARTESIAN_POINT('Ctrl Pts',(-0.830308018192218,2.55181873502139,
12.5893111709658));
#427901=CARTESIAN_POINT('Ctrl Pts',(-0.831082564866783,2.54051127235248,
12.5770542771492));
#427902=CARTESIAN_POINT('Ctrl Pts',(-0.847331259925655,2.53856612872315,
12.5737548217797));
#427903=CARTESIAN_POINT('Ctrl Pts',(-0.831030663502936,2.54126897069842,
12.5928319619712));
#427904=CARTESIAN_POINT('Ctrl Pts',(-0.834801333342892,2.53389228680053,
12.5821634970842));
#427905=CARTESIAN_POINT('Ctrl Pts',(-0.847585085332313,2.53472245989866,
12.5773203894503));
#427906=CARTESIAN_POINT('Ctrl Pts',(-0.839041370780464,2.52655799968174,
12.5969440695591));
#427907=CARTESIAN_POINT('Ctrl Pts',(-0.842843009373702,2.5252518271976,
12.5878292599214));
#427908=CARTESIAN_POINT('Ctrl Pts',(-0.850442061715556,2.52948014809535,
12.5813877129824));
#427909=CARTESIAN_POINT('Ctrl Pts',(-0.868005588370279,2.51669649143244,
12.596957478804));
#427910=CARTESIAN_POINT('Ctrl Pts',(-0.864232070952202,2.51799308676035,
12.5878468778671));
#427911=CARTESIAN_POINT('Ctrl Pts',(-0.860810679271491,2.52595622438975,
12.5814011370086));
#427912=CARTESIAN_POINT('Ctrl Pts',(-0.883426728453422,2.52351759439869,
12.5928371701607));
#427913=CARTESIAN_POINT('Ctrl Pts',(-0.875953421783604,2.51995602829336,
12.5821692192952));
#427914=CARTESIAN_POINT('Ctrl Pts',(-0.866301898949204,2.52837457501741,
12.5773318885715));
#427915=CARTESIAN_POINT('Ctrl Pts',(-0.890418978460782,2.53147077887088,
12.5893111709658));
#427916=CARTESIAN_POINT('Ctrl Pts',(-0.882935401738917,2.52295874538836,
12.5770542771492));
#427917=CARTESIAN_POINT('Ctrl Pts',(-0.868846144934124,2.531283198376,12.5737548217797));
#427918=CARTESIAN_POINT('',(-0.847331259925655,2.53856612872315,12.5737548217797));
#427919=CARTESIAN_POINT('Origin',(-0.852256586298207,2.55332218375571,12.5893111709658));
#427920=CARTESIAN_POINT('Ctrl Pts',(-0.868846144934124,2.531283198376,12.5737548217797));
#427921=CARTESIAN_POINT('Ctrl Pts',(-0.868209341145503,2.53050937632552,
12.5746934679442));
#427922=CARTESIAN_POINT('Ctrl Pts',(-0.867363228478373,2.52976949201513,
12.5756680099006));
#427923=CARTESIAN_POINT('Ctrl Pts',(-0.866406262569698,2.52914521650094,
12.5765688348656));
#427924=CARTESIAN_POINT('Ctrl Pts',(-0.866152916439339,2.52897994646952,
12.5768073183026));
#427925=CARTESIAN_POINT('Ctrl Pts',(-0.865891989609333,2.52882260442307,
12.5770407398754));
#427926=CARTESIAN_POINT('Ctrl Pts',(-0.865625612729321,2.52867423157954,
12.5772674179684));
#427927=CARTESIAN_POINT('Ctrl Pts',(-0.864532474045098,2.5280653495514,
12.5781976435658));
#427928=CARTESIAN_POINT('Ctrl Pts',(-0.863279976727664,2.52758278561512,
12.5790594849312));
#427929=CARTESIAN_POINT('Ctrl Pts',(-0.861935330421642,2.52730418368516,
12.5797571720116));
#427930=CARTESIAN_POINT('Ctrl Pts',(-0.861059245004097,2.52712266451016,
12.580211740231));
#427931=CARTESIAN_POINT('Ctrl Pts',(-0.860100420079891,2.52703786035313,
12.5806009430798));
#427932=CARTESIAN_POINT('Ctrl Pts',(-0.859124791877453,2.52707338886178,
12.5808812374708));
#427933=CARTESIAN_POINT('Ctrl Pts',(-0.858286403590271,2.52710391963717,
12.5811221033394));
#427934=CARTESIAN_POINT('Ctrl Pts',(-0.857418447014624,2.52722404929833,
12.581287365893));
#427935=CARTESIAN_POINT('Ctrl Pts',(-0.856571054141246,2.52743525678305,
12.581359338449));
#427936=CARTESIAN_POINT('Ctrl Pts',(-0.85645328402984,2.52746461026216,
12.5813693411482));
#427937=CARTESIAN_POINT('Ctrl Pts',(-0.856335878094531,2.52749567298117,
12.5813775999465));
#427938=CARTESIAN_POINT('Ctrl Pts',(-0.856218936184463,2.52752839834373,
12.5813841266931));
#427939=CARTESIAN_POINT('Ctrl Pts',(-0.856020530090201,2.52758392087937,
12.5813952001081));
#427940=CARTESIAN_POINT('Ctrl Pts',(-0.855822294958541,2.52764518758066,
12.5814007534795));
#427941=CARTESIAN_POINT('Ctrl Pts',(-0.855624375359456,2.52771236018032,
12.5814005856065));
#427942=CARTESIAN_POINT('Ctrl Pts',(-0.854718376816389,2.52801985007875,
12.5813998171494));
#427943=CARTESIAN_POINT('Ctrl Pts',(-0.853881479174623,2.52842953036616,
12.58127954464));
#427944=CARTESIAN_POINT('Ctrl Pts',(-0.853105424256869,2.5289124991765,
12.5810700125799));
#427945=CARTESIAN_POINT('Ctrl Pts',(-0.85216803827715,2.52949587050898,
12.5808169217085));
#427946=CARTESIAN_POINT('Ctrl Pts',(-0.851328179270106,2.53020043080289,
12.5804173076348));
#427947=CARTESIAN_POINT('Ctrl Pts',(-0.850642713652396,2.53094448204749,
12.5799304713245));
#427948=CARTESIAN_POINT('Ctrl Pts',(-0.849793205808115,2.53186659593986,
12.5793271277669));
#427949=CARTESIAN_POINT('Ctrl Pts',(-0.849104452189448,2.53288474684281,
12.5785808224116));
#427950=CARTESIAN_POINT('Ctrl Pts',(-0.848579214591445,2.53393824640552,
12.5777485681082));
#427951=CARTESIAN_POINT('Ctrl Pts',(-0.847796553026346,2.53550807617347,
12.576508418016));
#427952=CARTESIAN_POINT('Ctrl Pts',(-0.847377406667919,2.53714011043811,
12.5750928681475));
#427953=CARTESIAN_POINT('Ctrl Pts',(-0.847331259925655,2.53856612872315,
12.5737548217797));
#427954=CARTESIAN_POINT('Ctrl Pts',(-0.847331259925655,2.53856612872315,
12.5737548217797));
#427955=CARTESIAN_POINT('Ctrl Pts',(-0.831082564866783,2.54051127235248,
12.5770542771492));
#427956=CARTESIAN_POINT('Ctrl Pts',(-0.830308018192218,2.55181873502139,
12.5893111709658));
#427957=CARTESIAN_POINT('Ctrl Pts',(-0.845689554112151,2.56327077922043,
12.5508408821982));
#427958=CARTESIAN_POINT('Ctrl Pts',(-0.829390133805893,2.56521875825246,
12.55409748406));
#427959=CARTESIAN_POINT('Ctrl Pts',(-0.828614599008143,2.57654064634775,
12.5663972313419));
#427960=CARTESIAN_POINT('Ctrl Pts',(-0.844048275121227,2.5879512181765,
12.52790050457));
#427961=CARTESIAN_POINT('Ctrl Pts',(-0.827700944153361,2.58987892343607,
12.5311362602937));
#427962=CARTESIAN_POINT('Ctrl Pts',(-0.826922888205761,2.60123761732792,
12.5434568539655));
#427963=CARTESIAN_POINT('Ctrl Pts',(-0.84240737596564,2.61260932622068,
12.5049357605811));
#427964=CARTESIAN_POINT('Ctrl Pts',(-0.826014658008805,2.61449670084619,
12.5081700652078));
#427965=CARTESIAN_POINT('Ctrl Pts',(-0.825232751984268,2.6259116012949,
12.5204921097672));
#427966=CARTESIAN_POINT('Ctrl Pts',(-0.842515122252696,2.61099017808429,
12.5064436508395));
#427967=CARTESIAN_POINT('Ctrl Pts',(-0.841434523300001,2.61155688232287,
12.5062361689309));
#427968=CARTESIAN_POINT('Ctrl Pts',(-0.84028662328999,2.61210012921652,
12.5061871075061));
#427969=CARTESIAN_POINT('Ctrl Pts',(-0.839147735412921,2.61256267764056,
12.5063648335164));
#427970=CARTESIAN_POINT('Ctrl Pts',(-0.838630382289638,2.61277279566592,
12.5064455676329));
#427971=CARTESIAN_POINT('Ctrl Pts',(-0.838107589950988,2.61296898785313,
12.506574497099));
#427972=CARTESIAN_POINT('Ctrl Pts',(-0.837601404912136,2.61314185812502,
12.5067492519495));
#427973=CARTESIAN_POINT('Ctrl Pts',(-0.836584206427947,2.61348924764668,
12.5071004286051));
#427974=CARTESIAN_POINT('Ctrl Pts',(-0.835596412354412,2.61375446499197,
12.5076537929612));
#427975=CARTESIAN_POINT('Ctrl Pts',(-0.834714614491528,2.61392673912018,
12.5083435010503));
#427976=CARTESIAN_POINT('Ctrl Pts',(-0.834659100046304,2.61393758480609,
12.5083869222963));
#427977=CARTESIAN_POINT('Ctrl Pts',(-0.834603997369877,2.61394805158507,
12.5084308732336));
#427978=CARTESIAN_POINT('Ctrl Pts',(-0.834549321866726,2.61395813272698,
12.5084753333615));
#427979=CARTESIAN_POINT('Ctrl Pts',(-0.834110752167104,2.61403899679089,
12.508831962269));
#427980=CARTESIAN_POINT('Ctrl Pts',(-0.833690997704952,2.61409795873129,
12.509227847131));
#427981=CARTESIAN_POINT('Ctrl Pts',(-0.83330292946147,2.61413603813351,
12.5096423454524));
#427982=CARTESIAN_POINT('Ctrl Pts',(-0.832086895338208,2.61425536212681,
12.5109411997424));
#427983=CARTESIAN_POINT('Ctrl Pts',(-0.831108144286379,2.61418659826853,
12.5124831113042));
#427984=CARTESIAN_POINT('Ctrl Pts',(-0.830322672712138,2.61401352926051,
12.5140723025007));
#427985=CARTESIAN_POINT('Ctrl Pts',(-0.830249073165328,2.6139973125049,
12.5142212114565));
#427986=CARTESIAN_POINT('Ctrl Pts',(-0.830177148488656,2.61398019966024,
12.5143705582413));
#427987=CARTESIAN_POINT('Ctrl Pts',(-0.830106850884374,2.6139622720599,
12.5145201959299));
#427988=CARTESIAN_POINT('Ctrl Pts',(-0.829203773495196,2.61373196534218,
12.5164425148273));
#427989=CARTESIAN_POINT('Ctrl Pts',(-0.82853561926261,2.6133697117006,12.5184635205941));
#427990=CARTESIAN_POINT('Ctrl Pts',(-0.828025025593438,2.61292191164947,
12.5205025929158));
#427991=CARTESIAN_POINT('Ctrl Pts',(-0.827728861027278,2.61266216987068,
12.5216853356836));
#427992=CARTESIAN_POINT('Ctrl Pts',(-0.827485923233799,2.6123744790939,
12.5228750347131));
#427993=CARTESIAN_POINT('Ctrl Pts',(-0.827284450807109,2.61207278933631,
12.5240609649613));
#427994=CARTESIAN_POINT('Ctrl Pts',(-0.826789947544418,2.61133230801141,
12.5269717671326));
#427995=CARTESIAN_POINT('Ctrl Pts',(-0.826539972252611,2.61048087901163,
12.5299036066169));
#427996=CARTESIAN_POINT('Ctrl Pts',(-0.82645638379178,2.60955596545061,
12.5328133004019));
#427997=CARTESIAN_POINT('Ctrl Pts',(-0.826416256463371,2.60911195308521,
12.5342101228451));
#427998=CARTESIAN_POINT('Ctrl Pts',(-0.826415045980927,2.60865151259894,
12.5356023438238));
#427999=CARTESIAN_POINT('Ctrl Pts',(-0.826447302606738,2.60818060292636,
12.5369868989719));
#428000=CARTESIAN_POINT('Origin',(0.0498110926827573,15.3230129328841,-1.23968016501985));
#428001=CARTESIAN_POINT('Ctrl Pts',(-0.927693181599444,2.57386745989593,
12.5369868989719));
#428002=CARTESIAN_POINT('Ctrl Pts',(-0.937799265232525,2.58540654033113,
12.5369868989719));
#428003=CARTESIAN_POINT('Ctrl Pts',(-0.952121069903317,2.57991388936274,
12.5369868989719));
#428004=CARTESIAN_POINT('Ctrl Pts',(-0.931109482923459,2.57776807674996,
12.5218025310015));
#428005=CARTESIAN_POINT('Ctrl Pts',(-0.941077582193263,2.58411574251414,
12.5216901060418));
#428006=CARTESIAN_POINT('Ctrl Pts',(-0.952077418201794,2.57993064818136,
12.5161920673677));
#428007=CARTESIAN_POINT('Ctrl Pts',(-0.929742987280898,2.58363908695726,
12.5042015548896));
#428008=CARTESIAN_POINT('Ctrl Pts',(-0.935716298867672,2.586025903604,12.4980677368514));
#428009=CARTESIAN_POINT('Ctrl Pts',(-0.942105101708514,2.58370771940401,
12.4907278922778));
#428010=CARTESIAN_POINT('Ctrl Pts',(-0.916656565818685,2.58587169709282,
12.5064636261921));
#428011=CARTESIAN_POINT('Ctrl Pts',(-0.918842592986576,2.59203844044394,
12.4999376786892));
#428012=CARTESIAN_POINT('Ctrl Pts',(-0.918815893843201,2.59196312264034,
12.4906970594712));
#428013=CARTESIAN_POINT('Origin',(-0.94424319412143,2.55937273376805,12.5369868989719));
#428014=CARTESIAN_POINT('Origin',(-0.944243194121431,2.55937273376806,14.));
#428015=CARTESIAN_POINT('Origin',(-0.944243194121431,2.55937273376806,13.7435492065112));
#428016=CARTESIAN_POINT('Ctrl Pts',(-0.911372188348151,2.55530351594609,
13.793642941384));
#428017=CARTESIAN_POINT('Ctrl Pts',(-0.918490869314486,2.56344173444312,
13.8071662555867));
#428018=CARTESIAN_POINT('Ctrl Pts',(-0.93281817254894,2.5542358794767,13.8103758687955));
#428019=CARTESIAN_POINT('Ctrl Pts',(-0.922346766118139,2.5677863180351,
13.7804579775006));
#428020=CARTESIAN_POINT('Ctrl Pts',(-0.931138207785595,2.5778214675176,
13.7901904343351));
#428021=CARTESIAN_POINT('Ctrl Pts',(-0.945597244891531,2.57156110250158,
13.7927914348262));
#428022=CARTESIAN_POINT('Ctrl Pts',(-0.92880791309972,2.57513541338049,
13.7597120340895));
#428023=CARTESIAN_POINT('Ctrl Pts',(-0.938986397230478,2.58674513132594,
13.7635825532445));
#428024=CARTESIAN_POINT('Ctrl Pts',(-0.953153620955572,2.58176259301024,
13.7651073818884));
#428025=CARTESIAN_POINT('Ctrl Pts',(-0.927542672577892,2.57369629223617,
13.7381884353898));
#428026=CARTESIAN_POINT('Ctrl Pts',(-0.937482234460371,2.58503485564652,
13.7368803041982));
#428027=CARTESIAN_POINT('Ctrl Pts',(-0.951674255133689,2.57976454386001,
13.7363986145813));
#428028=CARTESIAN_POINT('Origin',(-0.930557576665944,2.54380632236616,13.7902182540695));
#428029=CARTESIAN_POINT('Ctrl Pts',(-0.890416380041073,2.53146782220492,
13.8235227101244));
#428030=CARTESIAN_POINT('Ctrl Pts',(-0.898004327165888,2.54010528402833,
13.8358800583119));
#428031=CARTESIAN_POINT('Ctrl Pts',(-0.912214993939723,2.53157985155249,
13.8390832900376));
#428032=CARTESIAN_POINT('Ctrl Pts',(-0.898291911659455,2.54042567635774,
13.8124254819053));
#428033=CARTESIAN_POINT('Ctrl Pts',(-0.905894594678995,2.54907991182599,
13.8247886449158));
#428034=CARTESIAN_POINT('Ctrl Pts',(-0.920114448745398,2.5405290913137,
13.8279860620657));
#428035=CARTESIAN_POINT('Ctrl Pts',(-0.906163913720722,2.54937951589171,
13.8013225099954));
#428036=CARTESIAN_POINT('Ctrl Pts',(-0.913777743883447,2.55804644291841,
13.8136962257787));
#428037=CARTESIAN_POINT('Ctrl Pts',(-0.928010043278306,2.54947436739277,
13.8168830918626));
#428038=CARTESIAN_POINT('Ctrl Pts',(-0.9140325235546,2.55832949700957,13.7902140179785));
#428039=CARTESIAN_POINT('Ctrl Pts',(-0.921654146662431,2.56700530030073,
13.802602731458));
#428040=CARTESIAN_POINT('Ctrl Pts',(-0.935901927838362,2.55841583675028,
13.8057746032558));
#428041=CARTESIAN_POINT('Origin',(-0.906941424926609,2.51694463820031,13.8235269408515));
#428042=CARTESIAN_POINT('Ctrl Pts',(-0.830308018192218,2.55181873502139,
13.8235269408515));
#428043=CARTESIAN_POINT('Ctrl Pts',(-0.829501111688596,2.56359861280876,
13.8362179249168));
#428044=CARTESIAN_POINT('Ctrl Pts',(-0.812498466818824,2.56520269244821,
13.8391868794938));
#428045=CARTESIAN_POINT('Ctrl Pts',(-0.831046302520483,2.54104065959348,
13.8400110824519));
#428046=CARTESIAN_POINT('Ctrl Pts',(-0.826986359770495,2.55025145368134,
13.8494522556837));
#428047=CARTESIAN_POINT('Ctrl Pts',(-0.813825568650046,2.54747270134967,
13.85569149686));
#428048=CARTESIAN_POINT('Ctrl Pts',(-0.838715429734773,2.52666769143045,
13.8586819406588));
#428049=CARTESIAN_POINT('Ctrl Pts',(-0.834595926707794,2.528076853751,13.868010383617));
#428050=CARTESIAN_POINT('Ctrl Pts',(-0.826685282294806,2.52368201908246,
13.8744918421245));
#428051=CARTESIAN_POINT('Ctrl Pts',(-0.868336578609752,2.51658508079264,
13.8587686893867));
#428052=CARTESIAN_POINT('Ctrl Pts',(-0.872419399873498,2.51518840672611,
13.8680909899357));
#428053=CARTESIAN_POINT('Ctrl Pts',(-0.875996625548385,2.50689986897952,
13.8745789365163));
#428054=CARTESIAN_POINT('Ctrl Pts',(-0.883274156730999,2.52334405496269,
13.8400379222776));
#428055=CARTESIAN_POINT('Ctrl Pts',(-0.892095268321583,2.52818742406021,
13.8494748685453));
#428056=CARTESIAN_POINT('Ctrl Pts',(-0.900858995894796,2.51799143542316,
13.8557104837033));
#428057=CARTESIAN_POINT('Ctrl Pts',(-0.890418978465611,2.53147077886645,
13.8235269408542));
#428058=CARTESIAN_POINT('Ctrl Pts',(-0.898215211960036,2.54033843707429,
13.8362179249195));
#428059=CARTESIAN_POINT('Ctrl Pts',(-0.912696230447696,2.53128508920643,
13.8391868794965));
#428060=CARTESIAN_POINT('Origin',(-0.808359450086228,2.55031528628707,13.8235269408515));
#428061=CARTESIAN_POINT('Ctrl Pts',(-0.827864026276527,2.58749810676731,
13.7902140241682));
#428062=CARTESIAN_POINT('Ctrl Pts',(-0.827079286871544,2.59901951204006,
13.8026027327198));
#428063=CARTESIAN_POINT('Ctrl Pts',(-0.810543698121789,2.60085042355425,
13.8057746032556));
#428064=CARTESIAN_POINT('Ctrl Pts',(-0.828678423698535,2.57560887047302,
13.8013225161808));
#428065=CARTESIAN_POINT('Ctrl Pts',(-0.82789448337184,2.58711849103363,
13.8136962270464));
#428066=CARTESIAN_POINT('Ctrl Pts',(-0.811381754829571,2.58895381155141,
13.8168830918628));
#428067=CARTESIAN_POINT('Ctrl Pts',(-0.82949317221461,2.56371450862203,
13.8124254880875));
#428068=CARTESIAN_POINT('Ctrl Pts',(-0.82871037804292,2.57520727627501,
13.8247886461868));
#428069=CARTESIAN_POINT('Ctrl Pts',(-0.812220446444029,2.57705192205747,
13.8279860620656));
#428070=CARTESIAN_POINT('Ctrl Pts',(-0.830308286038418,2.55181481371165,
13.8235227163065));
#428071=CARTESIAN_POINT('Ctrl Pts',(-0.829527009371742,2.56328530585484,
13.8358800595847));
#428072=CARTESIAN_POINT('Ctrl Pts',(-0.813059797021839,2.56514453908972,
13.8390832900376));
#428073=CARTESIAN_POINT('Origin',(-0.805915189477223,2.58599859175722,13.7902182540695));
#428074=CARTESIAN_POINT('Ctrl Pts',(-0.826465716928943,2.60791137202139,
13.7382347919292));
#428075=CARTESIAN_POINT('Ctrl Pts',(-0.82545841117444,2.62296803844693,
13.7369371795943));
#428076=CARTESIAN_POINT('Ctrl Pts',(-0.810969599492456,2.62739727236085,
13.7364597369712));
#428077=CARTESIAN_POINT('Ctrl Pts',(-0.826336450902827,2.60979850855029,
13.7595490285573));
#428078=CARTESIAN_POINT('Ctrl Pts',(-0.825304108514234,2.62521434701637,
13.7633824266925));
#428079=CARTESIAN_POINT('Ctrl Pts',(-0.811007953024174,2.62985262239744,
13.7648920890506));
#428080=CARTESIAN_POINT('Ctrl Pts',(-0.826995700562206,2.6001742156392,
13.7803806590111));
#428081=CARTESIAN_POINT('Ctrl Pts',(-0.826108147738794,2.6135087248536,
13.7901039518745));
#428082=CARTESIAN_POINT('Ctrl Pts',(-0.81081613484347,2.61733492179509,
13.7926933640892));
#428083=CARTESIAN_POINT('Ctrl Pts',(-0.828141623556339,2.583445046142,13.7936647693663));
#428084=CARTESIAN_POINT('Ctrl Pts',(-0.827432419508959,2.59423718965308,
13.8072068914933));
#428085=CARTESIAN_POINT('Ctrl Pts',(-0.810440115724187,2.59561772648085,
13.8104111085397));
#428086=CARTESIAN_POINT('Origin',(-0.804498734500748,2.60667715419204,13.7435492065112));
#428087=CARTESIAN_POINT('Origin',(-0.804498734500748,2.60667715419204,14.));
#428088=CARTESIAN_POINT('Origin',(-0.804498734500748,2.60667715419204,12.5369868989719));
#428089=CARTESIAN_POINT('Ctrl Pts',(-0.842509476978436,2.61097268310583,
12.506462012331));
#428090=CARTESIAN_POINT('Ctrl Pts',(-0.844517414078375,2.61719536553326,
12.4999388158272));
#428091=CARTESIAN_POINT('Ctrl Pts',(-0.844493657549235,2.61712174303959,
12.4907030323752));
#428092=CARTESIAN_POINT('Ctrl Pts',(-0.830757090671982,2.61714601277937,
12.5042014951932));
#428093=CARTESIAN_POINT('Ctrl Pts',(-0.827464013952634,2.62266839839037,
12.4980716682127));
#428094=CARTESIAN_POINT('Ctrl Pts',(-0.820985788226397,2.62470755426128,
12.4907355092743));
#428095=CARTESIAN_POINT('Ctrl Pts',(-0.826104613507571,2.61331454341629,
12.5218047446509));
#428096=CARTESIAN_POINT('Ctrl Pts',(-0.822042668831244,2.6244059579511,
12.5216906929434));
#428097=CARTESIAN_POINT('Ctrl Pts',(-0.810769257694715,2.62776467134713,
12.5161988840776));
#428098=CARTESIAN_POINT('Ctrl Pts',(-0.826449894446796,2.60814227433147,
12.5369868989719));
#428099=CARTESIAN_POINT('Ctrl Pts',(-0.825428979411771,2.62343813207178,
12.5369868989719));
#428100=CARTESIAN_POINT('Ctrl Pts',(-0.810726046326702,2.62777740507733,
12.5369868989719));
#428101=CARTESIAN_POINT('Origin',(-1.65186468598908E-31,-2.72002836734944E-32,
12.5));
#428102=CARTESIAN_POINT('Origin',(-1.03554215359084,2.4756499570046,12.5));
#428103=CARTESIAN_POINT('',(-1.03554215359084,2.4756499570046,12.5893111709658));
#428104=CARTESIAN_POINT('',(-1.03554215359084,2.4756499570046,13.8235269408515));
#428105=CARTESIAN_POINT('',(-1.03554215359084,2.4756499570046,12.5));
#428106=CARTESIAN_POINT('',(-1.03601454672084,2.51141375915052,13.7902182540695));
#428107=CARTESIAN_POINT('',(-1.03554215359084,2.4756499570046,13.8235269408515));
#428108=CARTESIAN_POINT('',(-1.03628829969029,2.532138969605,13.7435492065112));
#428109=CARTESIAN_POINT('Origin',(-1.03538798176588,2.46395329685158,13.7445212918692));
#428110=CARTESIAN_POINT('',(-1.03628829969029,2.532138969605,12.5369868989719));
#428111=CARTESIAN_POINT('',(-1.03628829969029,2.532138969605,12.5));
#428112=CARTESIAN_POINT('Ctrl Pts',(-1.03628829969029,2.532138969605,12.5369868989719));
#428113=CARTESIAN_POINT('Ctrl Pts',(-1.03603976572167,2.51332303195488,
12.5544431401645));
#428114=CARTESIAN_POINT('Ctrl Pts',(-1.03579105399495,2.49449363664606,
12.5718848856037));
#428115=CARTESIAN_POINT('Ctrl Pts',(-1.03554215359084,2.4756499570046,12.5893111709658));
#428116=CARTESIAN_POINT('Origin',(-1.29160128864211,2.64151328156347,12.5));
#428117=CARTESIAN_POINT('',(-1.1344304865774,2.48971658479254,13.7435492065112));
#428118=CARTESIAN_POINT('',(-1.11952159984425,2.47531747421414,13.7902182540695));
#428119=CARTESIAN_POINT('Origin',(-1.08034362228217,2.43747910027977,13.7418732680441));
#428120=CARTESIAN_POINT('',(-1.09379455227041,2.45047010569483,13.8235269408515));
#428121=CARTESIAN_POINT('',(-1.11952159984425,2.47531747421414,13.7902182540695));
#428122=CARTESIAN_POINT('',(-1.09379455227041,2.45047010569483,12.5893111709658));
#428123=CARTESIAN_POINT('',(-1.09379455227041,2.45047010569483,12.5));
#428124=CARTESIAN_POINT('',(-1.1344304865774,2.48971658479254,12.5369868989719));
#428125=CARTESIAN_POINT('Ctrl Pts',(-1.09379455227041,2.45047010569483,
12.5893111709658));
#428126=CARTESIAN_POINT('Ctrl Pts',(-1.10734994105777,2.46356199817318,
12.5718848856037));
#428127=CARTESIAN_POINT('Ctrl Pts',(-1.12089505426805,2.47664396642491,
12.5544431401645));
#428128=CARTESIAN_POINT('Ctrl Pts',(-1.1344304865774,2.48971658479254,12.5369868989719));
#428129=CARTESIAN_POINT('',(-1.1344304865774,2.48971658479254,12.5));
#428130=CARTESIAN_POINT('Origin',(-1.06991415528683,2.47519594774129,12.5));
#428131=CARTESIAN_POINT('',(-1.05525494628247,2.44410418414473,13.8587068136939));
#428132=CARTESIAN_POINT('Ctrl Pts',(-1.09379455227489,2.45047010568997,
13.8235269408542));
#428133=CARTESIAN_POINT('Ctrl Pts',(-1.09253412895405,2.44925277973552,
13.8262006681044));
#428134=CARTESIAN_POINT('Ctrl Pts',(-1.09112357270249,2.44813199470117,
13.8288634856214));
#428135=CARTESIAN_POINT('Ctrl Pts',(-1.08957482168588,2.44710181036399,
13.8314912288862));
#428136=CARTESIAN_POINT('Ctrl Pts',(-1.08797821913402,2.44603979657094,
13.8342001611531));
#428137=CARTESIAN_POINT('Ctrl Pts',(-1.08623325208851,2.44507247516437,
13.8368750301949));
#428138=CARTESIAN_POINT('Ctrl Pts',(-1.08431407794086,2.44421632114273,
13.8394886372969));
#428139=CARTESIAN_POINT('Ctrl Pts',(-1.08416585546618,2.4441501982909,13.8396904925131));
#428140=CARTESIAN_POINT('Ctrl Pts',(-1.08401658149932,2.44408475690539,
13.8398919674349));
#428141=CARTESIAN_POINT('Ctrl Pts',(-1.08386623860007,2.44402001459231,
13.8400930404591));
#428142=CARTESIAN_POINT('Ctrl Pts',(-1.08152379508397,2.44301128579805,
13.8432258934518));
#428143=CARTESIAN_POINT('Ctrl Pts',(-1.07893425814486,2.44217637542924,
13.8462331177034));
#428144=CARTESIAN_POINT('Ctrl Pts',(-1.07615248274327,2.44163432596774,
13.8489036603661));
#428145=CARTESIAN_POINT('Ctrl Pts',(-1.07524225345872,2.44145696107579,
13.849777493004));
#428146=CARTESIAN_POINT('Ctrl Pts',(-1.07431162075303,2.44131112643096,
13.85061494757));
#428147=CARTESIAN_POINT('Ctrl Pts',(-1.07336302610177,2.44120148194552,
13.8514076489583));
#428148=CARTESIAN_POINT('Ctrl Pts',(-1.07135661160652,2.44096956804571,
13.8530843267192));
#428149=CARTESIAN_POINT('Ctrl Pts',(-1.06907241597874,2.44087972128076,
13.8546805203176));
#428150=CARTESIAN_POINT('Ctrl Pts',(-1.06663765028923,2.44107349660114,
13.8559412814274));
#428151=CARTESIAN_POINT('Ctrl Pts',(-1.06631179967866,2.44109943002329,
13.8561100121513));
#428152=CARTESIAN_POINT('Ctrl Pts',(-1.06598329716654,2.44113038115478,
13.8562727473908));
#428153=CARTESIAN_POINT('Ctrl Pts',(-1.0656524840526,2.44116662275184,13.8564289040185));
#428154=CARTESIAN_POINT('Ctrl Pts',(-1.06415225035486,2.44133097798106,
13.8571370725437));
#428155=CARTESIAN_POINT('Ctrl Pts',(-1.06257837452934,2.44160928936341,
13.8577210840553));
#428156=CARTESIAN_POINT('Ctrl Pts',(-1.06099714379373,2.44201963856708,
13.8581177131616));
#428157=CARTESIAN_POINT('Ctrl Pts',(-1.06055181479428,2.44213520702663,
13.8582294175695));
#428158=CARTESIAN_POINT('Ctrl Pts',(-1.06010589235067,2.44226107112859,
13.8583265086086));
#428159=CARTESIAN_POINT('Ctrl Pts',(-1.05966080616386,2.44239719818541,
13.8584082369006));
#428160=CARTESIAN_POINT('Ctrl Pts',(-1.059021336668,2.44259277626215,13.8585256585398));
#428161=CARTESIAN_POINT('Ctrl Pts',(-1.05837573782924,2.44281227981609,
13.8586122832068));
#428162=CARTESIAN_POINT('Ctrl Pts',(-1.05774103463668,2.44305075443522,
13.8586682984299));
#428163=CARTESIAN_POINT('Ctrl Pts',(-1.05723333499873,2.4432415104913,13.8587131050557));
#428164=CARTESIAN_POINT('Ctrl Pts',(-1.05672691682815,2.44344629242233,
13.8587357943552));
#428165=CARTESIAN_POINT('Ctrl Pts',(-1.05622190980664,2.44366559407393,
13.8587355499465));
#428166=CARTESIAN_POINT('Ctrl Pts',(-1.05589551172886,2.44380733395969,
13.8587353919793));
#428167=CARTESIAN_POINT('Ctrl Pts',(-1.05557321735783,2.44395357100555,
13.8587257282814));
#428168=CARTESIAN_POINT('Ctrl Pts',(-1.05525494628247,2.44410418414473,
13.8587068136939));
#428169=CARTESIAN_POINT('Ctrl Pts',(-1.05525494628247,2.44410418414473,
13.8587068136939));
#428170=CARTESIAN_POINT('Ctrl Pts',(-1.05420817006571,2.44459954254902,
13.8586446046467));
#428171=CARTESIAN_POINT('Ctrl Pts',(-1.05320486014151,2.44514217983373,
13.858482427929));
#428172=CARTESIAN_POINT('Ctrl Pts',(-1.05224262539812,2.44572831862652,
13.8582284286032));
#428173=CARTESIAN_POINT('Ctrl Pts',(-1.05125548448328,2.44632962884536,
13.8579678548414));
#428174=CARTESIAN_POINT('Ctrl Pts',(-1.05030995810848,2.44697949858509,
13.857615680862));
#428175=CARTESIAN_POINT('Ctrl Pts',(-1.04943783450206,2.4476443218117,13.8571944833187));
#428176=CARTESIAN_POINT('Ctrl Pts',(-1.04726136084877,2.44930345616624,
13.8561433417727));
#428177=CARTESIAN_POINT('Ctrl Pts',(-1.04543732607343,2.45112951671997,
13.8546163505475));
#428178=CARTESIAN_POINT('Ctrl Pts',(-1.04395148423086,2.45291621503479,
13.8528973491086));
#428179=CARTESIAN_POINT('Ctrl Pts',(-1.04368004284776,2.45324261845664,
13.8525833129073));
#428180=CARTESIAN_POINT('Ctrl Pts',(-1.04341975016522,2.45356767825653,
13.8522628768812));
#428181=CARTESIAN_POINT('Ctrl Pts',(-1.0431703408006,2.45389012658109,13.851937733538));
#428182=CARTESIAN_POINT('Ctrl Pts',(-1.04164723241489,2.45585927376145,
13.8499521282529));
#428183=CARTESIAN_POINT('Ctrl Pts',(-1.04038186136928,2.45792922057858,
13.847639871647));
#428184=CARTESIAN_POINT('Ctrl Pts',(-1.03937218357848,2.45994927489359,
13.8452109780794));
#428185=CARTESIAN_POINT('Ctrl Pts',(-1.03891790864111,2.46085813914296,
13.8441181685877));
#428186=CARTESIAN_POINT('Ctrl Pts',(-1.03851467993731,2.46175682465833,
13.8430021611332));
#428187=CARTESIAN_POINT('Ctrl Pts',(-1.03815907134473,2.46263227806838,
13.8418824960098));
#428188=CARTESIAN_POINT('Ctrl Pts',(-1.03732107061554,2.46469530638467,
13.8392439765549));
#428189=CARTESIAN_POINT('Ctrl Pts',(-1.03670395028029,2.46672651997604,
13.8364981347964));
#428190=CARTESIAN_POINT('Ctrl Pts',(-1.03627333558364,2.46872134277917,
13.833693111342));
#428191=CARTESIAN_POINT('Ctrl Pts',(-1.03585394421567,2.47066417350646,
13.8309611966328));
#428192=CARTESIAN_POINT('Ctrl Pts',(-1.03561159464998,2.47257455164312,
13.8281701127186));
#428193=CARTESIAN_POINT('Ctrl Pts',(-1.03555333006732,2.47444199813983,
13.8253580685121));
#428194=CARTESIAN_POINT('Ctrl Pts',(-1.03554069824292,2.47484686255574,
13.8247484142933));
#428195=CARTESIAN_POINT('Ctrl Pts',(-1.03553686562278,2.4752496170513,13.8241378483365));
#428196=CARTESIAN_POINT('Ctrl Pts',(-1.03554215359084,2.4756499570046,13.8235269408515));
#428197=CARTESIAN_POINT('',(-1.05638779057725,2.44359483096628,12.5969504640361));
#428198=CARTESIAN_POINT('Origin',(-1.06992710296501,2.47522639508009,12.584524458991));
#428199=CARTESIAN_POINT('Origin',(-1.06992710296501,2.47522639508009,12.584524458991));
#428200=CARTESIAN_POINT('Ctrl Pts',(-1.09379455227041,2.45047010569483,
12.5893111709658));
#428201=CARTESIAN_POINT('Ctrl Pts',(-1.08564206678204,2.44259637627849,
12.5770542771492));
#428202=CARTESIAN_POINT('Ctrl Pts',(-1.07227821101593,2.4520415355634,12.5737548217797));
#428203=CARTESIAN_POINT('Ctrl Pts',(-1.11162130197801,2.46768730942624,
12.5663937883685));
#428204=CARTESIAN_POINT('Ctrl Pts',(-1.10345841686222,2.45980353597454,
12.5540940315304));
#428205=CARTESIAN_POINT('Ctrl Pts',(-1.09005500260645,2.46928058623304,
12.5508374392248));
#428206=CARTESIAN_POINT('Ctrl Pts',(-1.1294300647137,2.48488714121014,12.5434499600945));
#428207=CARTESIAN_POINT('Ctrl Pts',(-1.12124063915155,2.47697773480345,
12.5311293540533));
#428208=CARTESIAN_POINT('Ctrl Pts',(-1.10781524727627,2.48650194697867,
12.5278936106989));
#428209=CARTESIAN_POINT('Ctrl Pts',(-1.1472222494216,2.50207096181498,12.5204817579905));
#428210=CARTESIAN_POINT('Ctrl Pts',(-1.13899229179957,2.49412240925192,
12.5081597038247));
#428211=CARTESIAN_POINT('Ctrl Pts',(-1.12556024076148,2.50370698278469,
12.5049254088044));
#428212=CARTESIAN_POINT('Ctrl Pts',(-1.1344304865774,2.48971658479254,12.5369868989719));
#428213=CARTESIAN_POINT('Ctrl Pts',(-1.13510051527256,2.49036370357483,
12.5342545179733));
#428214=CARTESIAN_POINT('Ctrl Pts',(-1.13565329867523,2.49107101370702,
12.5314872231885));
#428215=CARTESIAN_POINT('Ctrl Pts',(-1.1360136523182,2.49183309399291,12.5287124745063));
#428216=CARTESIAN_POINT('Ctrl Pts',(-1.13633863711978,2.492520375821,12.5262100684184));
#428217=CARTESIAN_POINT('Ctrl Pts',(-1.13650589535426,2.49325193102789,
12.5237004536639));
#428218=CARTESIAN_POINT('Ctrl Pts',(-1.13645367584698,2.49405509582697,
12.5212220730815));
#428219=CARTESIAN_POINT('Ctrl Pts',(-1.1364136972968,2.49466998795997,12.5193246583486));
#428220=CARTESIAN_POINT('Ctrl Pts',(-1.13624396681212,2.4953341597643,12.517417831369));
#428221=CARTESIAN_POINT('Ctrl Pts',(-1.13584738190643,2.4960425982698,12.5155812248347));
#428222=CARTESIAN_POINT('Ctrl Pts',(-1.13567843460495,2.49634439688102,
12.5147988205793));
#428223=CARTESIAN_POINT('Ctrl Pts',(-1.13546838785177,2.49665467072492,
12.5140295443047));
#428224=CARTESIAN_POINT('Ctrl Pts',(-1.13521068192522,2.49697493687713,
12.5132817086137));
#428225=CARTESIAN_POINT('Ctrl Pts',(-1.13482067886705,2.49745961637389,
12.5121499604604));
#428226=CARTESIAN_POINT('Ctrl Pts',(-1.13430752963695,2.49797316382496,
12.5110494206568));
#428227=CARTESIAN_POINT('Ctrl Pts',(-1.13363782154244,2.49849913262807,
12.5100666561695));
#428228=CARTESIAN_POINT('Ctrl Pts',(-1.13325327669677,2.49880114270361,
12.5095023550641));
#428229=CARTESIAN_POINT('Ctrl Pts',(-1.13281226769082,2.49911022423344,
12.5089719619137));
#428230=CARTESIAN_POINT('Ctrl Pts',(-1.1323193950732,2.49941535350073,12.5085043804652));
#428231=CARTESIAN_POINT('Ctrl Pts',(-1.13159814019849,2.49986187043752,
12.5078201359222));
#428232=CARTESIAN_POINT('Ctrl Pts',(-1.1307442673798,2.50031184735045,12.5072563000949));
#428233=CARTESIAN_POINT('Ctrl Pts',(-1.12981170967374,2.5007272927876,12.5068768744332));
#428234=CARTESIAN_POINT('Ctrl Pts',(-1.12913927137018,2.50102685754714,
12.5066032824114));
#428235=CARTESIAN_POINT('Ctrl Pts',(-1.12841413233554,2.50131378576313,
12.5064197834844));
#428236=CARTESIAN_POINT('Ctrl Pts',(-1.12767773726476,2.50157445815717,
12.5063282718343));
#428237=CARTESIAN_POINT('Ctrl Pts',(-1.12660282844358,2.50195495915033,
12.5061946931565));
#428238=CARTESIAN_POINT('Ctrl Pts',(-1.12548131597894,2.50228865103162,
12.5062515701262));
#428239=CARTESIAN_POINT('Ctrl Pts',(-1.12438721310995,2.50256964663795,
12.5064436508398));
#428240=CARTESIAN_POINT('',(-1.07227821101593,2.4520415355634,12.5737548217797));
#428241=CARTESIAN_POINT('Origin',(-1.07851109820091,2.46629464460456,12.5893111709658));
#428242=CARTESIAN_POINT('Ctrl Pts',(-1.12438721310995,2.50256964663795,
12.5064436508398));
#428243=CARTESIAN_POINT('Ctrl Pts',(-1.11667339252586,2.49509051836337,
12.5164271754438));
#428244=CARTESIAN_POINT('Ctrl Pts',(-1.10895665962532,2.48760827535993,
12.5264061185523));
#428245=CARTESIAN_POINT('Ctrl Pts',(-1.10123691118013,2.48012280860901,
12.536380305637));
#428246=CARTESIAN_POINT('Ctrl Pts',(-1.09158879135733,2.4707674933866,12.5488460165097));
#428247=CARTESIAN_POINT('Ctrl Pts',(-1.08193595844174,2.46140713991218,
12.5613043021964));
#428248=CARTESIAN_POINT('Ctrl Pts',(-1.07227821101593,2.4520415355634,12.5737548217797));
#428249=CARTESIAN_POINT('Ctrl Pts',(-1.03554215359084,2.4756499570046,12.5893111709658));
#428250=CARTESIAN_POINT('Ctrl Pts',(-1.03539245984436,2.46431698624041,
12.5770542771492));
#428251=CARTESIAN_POINT('Ctrl Pts',(-1.05142854144723,2.46105389542322,
12.5737548217797));
#428252=CARTESIAN_POINT('Ctrl Pts',(-1.03540249062735,2.46507639385059,
12.5928319619712));
#428253=CARTESIAN_POINT('Ctrl Pts',(-1.038559345655,2.45741691066269,12.5821634970843));
#428254=CARTESIAN_POINT('Ctrl Pts',(-1.0513682275787,2.45720232696262,12.5773203894503));
#428255=CARTESIAN_POINT('Ctrl Pts',(-1.04218746222939,2.44976142536551,
12.5969440695591));
#428256=CARTESIAN_POINT('Ctrl Pts',(-1.04586998600045,2.44814973022451,
12.5878292599214));
#428257=CARTESIAN_POINT('Ctrl Pts',(-1.0537884005295,2.45174458842127,12.5813877129824));
#428258=CARTESIAN_POINT('Ctrl Pts',(-1.07025149930247,2.43757187784713,
12.596957478804));
#428259=CARTESIAN_POINT('Ctrl Pts',(-1.06659622250853,2.43917173556225,
12.5878468778671));
#428260=CARTESIAN_POINT('Ctrl Pts',(-1.06383528486935,2.44738725169273,
12.5814011370086));
#428261=CARTESIAN_POINT('Ctrl Pts',(-1.08617731002991,2.4431133180763,12.5928371701607));
#428262=CARTESIAN_POINT('Ctrl Pts',(-1.07843856946996,2.44017274666077,
12.5821692192951));
#428263=CARTESIAN_POINT('Ctrl Pts',(-1.0695053509936,2.44934997007645,12.5773318885715));
#428264=CARTESIAN_POINT('Ctrl Pts',(-1.09379455227044,2.45047010569479,
12.5893111709658));
#428265=CARTESIAN_POINT('Ctrl Pts',(-1.08564206678208,2.44259637627845,
12.5770542771492));
#428266=CARTESIAN_POINT('Ctrl Pts',(-1.07227821101596,2.45204153556336,
12.5737548217797));
#428267=CARTESIAN_POINT('',(-1.05142854144723,2.46105389542322,12.5737548217797));
#428268=CARTESIAN_POINT('Origin',(-1.05754023467627,2.47535939107608,12.5893111709658));
#428269=CARTESIAN_POINT('Ctrl Pts',(-1.07227821101596,2.45204153556336,
12.5737548217797));
#428270=CARTESIAN_POINT('Ctrl Pts',(-1.07158045245849,2.45132219376248,
12.5746934679442));
#428271=CARTESIAN_POINT('Ctrl Pts',(-1.07067684772141,2.4506537373934,12.5756680099006));
#428272=CARTESIAN_POINT('Ctrl Pts',(-1.06967218178794,2.45010954071008,
12.5765688348656));
#428273=CARTESIAN_POINT('Ctrl Pts',(-1.06940620760409,2.44996547066263,
12.5768073183026));
#428274=CARTESIAN_POINT('Ctrl Pts',(-1.06913332414911,2.44982992011784,
12.5770407398754));
#428275=CARTESIAN_POINT('Ctrl Pts',(-1.06885573985202,2.44970375316135,
12.5772674179684));
#428276=CARTESIAN_POINT('Ctrl Pts',(-1.06771660895871,2.44918599808889,
12.5781976435658));
#428277=CARTESIAN_POINT('Ctrl Pts',(-1.06642894578207,2.44880713000329,
12.5790594849312));
#428278=CARTESIAN_POINT('Ctrl Pts',(-1.065066065032,2.4486390562553,12.5797571720116));
#428279=CARTESIAN_POINT('Ctrl Pts',(-1.0641780992185,2.44852955016509,12.580211740231));
#428280=CARTESIAN_POINT('Ctrl Pts',(-1.06321555237905,2.44852318131952,
12.5806009430798));
#428281=CARTESIAN_POINT('Ctrl Pts',(-1.06224606640226,2.44863811436578,
12.5808812374708));
#428282=CARTESIAN_POINT('Ctrl Pts',(-1.06141295632457,2.44873687998115,
12.5811221033394));
#428283=CARTESIAN_POINT('Ctrl Pts',(-1.06055767948544,2.44892735643941,
12.581287365893));
#428284=CARTESIAN_POINT('Ctrl Pts',(-1.0597303216127,2.44920693153464,12.581359338449));
#428285=CARTESIAN_POINT('Ctrl Pts',(-1.05961533595268,2.44924578669987,
12.5813693411482));
#428286=CARTESIAN_POINT('Ctrl Pts',(-1.05950085257591,2.44928631573391,
12.5813775999465));
#428287=CARTESIAN_POINT('Ctrl Pts',(-1.05938696720125,2.44932846405683,
12.5813841266931));
#428288=CARTESIAN_POINT('Ctrl Pts',(-1.059193746889,2.44939997378441,12.5813952001081));
#428289=CARTESIAN_POINT('Ctrl Pts',(-1.05900116517332,2.44947719462936,
12.5814007534795));
#428290=CARTESIAN_POINT('Ctrl Pts',(-1.05880937932584,2.44956027600246,
12.5814005856065));
#428291=CARTESIAN_POINT('Ctrl Pts',(-1.05793145869951,2.44994059004576,
12.5813998171494));
#428292=CARTESIAN_POINT('Ctrl Pts',(-1.05713073851232,2.45041712208299,
12.58127954464));
#428293=CARTESIAN_POINT('Ctrl Pts',(-1.05639663229499,2.4509617395348,12.5810700125799));
#428294=CARTESIAN_POINT('Ctrl Pts',(-1.05550991556914,2.45161957540691,
12.5808169217085));
#428295=CARTESIAN_POINT('Ctrl Pts',(-1.05473027932843,2.4523902476405,12.5804173076348));
#428296=CARTESIAN_POINT('Ctrl Pts',(-1.05410774162489,2.45318769492736,
12.5799304713245));
#428297=CARTESIAN_POINT('Ctrl Pts',(-1.05333622129059,2.45417598333758,
12.5793271277669));
#428298=CARTESIAN_POINT('Ctrl Pts',(-1.05273274819342,2.45524688624139,
12.5785808224116));
#428299=CARTESIAN_POINT('Ctrl Pts',(-1.05229512827477,2.45633969211152,
12.5777485681082));
#428300=CARTESIAN_POINT('Ctrl Pts',(-1.05164302665113,2.45796809258384,
12.576508418016));
#428301=CARTESIAN_POINT('Ctrl Pts',(-1.05135830091127,2.45962886070849,
12.5750928681475));
#428302=CARTESIAN_POINT('Ctrl Pts',(-1.05142854144723,2.46105389542322,
12.5737548217797));
#428303=CARTESIAN_POINT('Ctrl Pts',(-1.05142854144723,2.46105389542322,
12.5737548217797));
#428304=CARTESIAN_POINT('Ctrl Pts',(-1.03539245984436,2.46431698624041,
12.5770542771492));
#428305=CARTESIAN_POINT('Ctrl Pts',(-1.03554215359084,2.4756499570046,12.5893111709658));
#428306=CARTESIAN_POINT('Ctrl Pts',(-1.0518059566367,2.48581015749861,12.5508408821982));
#428307=CARTESIAN_POINT('Ctrl Pts',(-1.03571954968216,2.4890802088625,12.55409748406));
#428308=CARTESIAN_POINT('Ctrl Pts',(-1.03586943439953,2.50042763759486,
12.5663972313419));
#428309=CARTESIAN_POINT('Ctrl Pts',(-1.05218182376314,2.51054225380471,
12.52790050457));
#428310=CARTESIAN_POINT('Ctrl Pts',(-1.03604601306511,2.51379600401922,
12.5311362602938));
#428311=CARTESIAN_POINT('Ctrl Pts',(-1.03619638503566,2.52518032157695,
12.5434568539655));
#428312=CARTESIAN_POINT('Ctrl Pts',(-1.05255624928446,2.53525206254306,
12.5049357605811));
#428313=CARTESIAN_POINT('Ctrl Pts',(-1.03637191529783,2.53846931578125,
12.5081700652078));
#428314=CARTESIAN_POINT('Ctrl Pts',(-1.03652303135842,2.54990996669025,
12.5204921097672));
#428315=CARTESIAN_POINT('Ctrl Pts',(-1.05253166145008,2.53362951966586,
12.5064436508395));
#428316=CARTESIAN_POINT('Ctrl Pts',(-1.05150084975772,2.53428241708927,
12.5062361689309));
#428317=CARTESIAN_POINT('Ctrl Pts',(-1.05040104895539,2.53491742088109,
12.5061871075061));
#428318=CARTESIAN_POINT('Ctrl Pts',(-1.04930365262443,2.53547126014831,
12.5063648335164));
#428319=CARTESIAN_POINT('Ctrl Pts',(-1.04880514752069,2.5357228481057,12.5064455676329));
#428320=CARTESIAN_POINT('Ctrl Pts',(-1.04830008621504,2.53596099990856,
12.506574497099));
#428321=CARTESIAN_POINT('Ctrl Pts',(-1.04780967599716,2.53617455374873,
12.5067492519495));
#428322=CARTESIAN_POINT('Ctrl Pts',(-1.04682417762803,2.53660369848009,
12.5071004286051));
#428323=CARTESIAN_POINT('Ctrl Pts',(-1.04586128803358,2.53694854772377,
12.5076537929612));
#428324=CARTESIAN_POINT('Ctrl Pts',(-1.04499646622111,2.53719212333607,
12.5083435010503));
#428325=CARTESIAN_POINT('Ctrl Pts',(-1.04494202051971,2.53720745787651,
12.5083869222963));
#428326=CARTESIAN_POINT('Ctrl Pts',(-1.04488795433255,2.53722238120782,
12.5084308732336));
#428327=CARTESIAN_POINT('Ctrl Pts',(-1.04483428246428,2.53723688536665,
12.5084753333615));
#428328=CARTESIAN_POINT('Ctrl Pts',(-1.04440376324107,2.53735322786407,
12.508831962269));
#428329=CARTESIAN_POINT('Ctrl Pts',(-1.04399021142279,2.53744620749895,
12.509227847131));
#428330=CARTESIAN_POINT('Ctrl Pts',(-1.04360653826916,2.53751579135959,
12.5096423454524));
#428331=CARTESIAN_POINT('Ctrl Pts',(-1.04240427641233,2.5377338363823,12.5109411997424));
#428332=CARTESIAN_POINT('Ctrl Pts',(-1.04142317718106,2.5377450786271,12.5124831113042));
#428333=CARTESIAN_POINT('Ctrl Pts',(-1.04062621246784,2.53763660871718,
12.5140723025008));
#428334=CARTESIAN_POINT('Ctrl Pts',(-1.04055153600132,2.53762644496782,
12.5142212114565));
#428335=CARTESIAN_POINT('Ctrl Pts',(-1.04047845579237,2.5376152515936,12.5143705582413));
#428336=CARTESIAN_POINT('Ctrl Pts',(-1.04040693083171,2.53760311355324,
12.5145201959299));
#428337=CARTESIAN_POINT('Ctrl Pts',(-1.03948808622249,2.5374471823531,12.5164425148273));
#428338=CARTESIAN_POINT('Ctrl Pts',(-1.03879262818321,2.53714059485342,
12.5184635205941));
#428339=CARTESIAN_POINT('Ctrl Pts',(-1.03824723361101,2.53673590294418,
12.5205025929158));
#428340=CARTESIAN_POINT('Ctrl Pts',(-1.03793088314171,2.53650116559633,
12.5216853356836));
#428341=CARTESIAN_POINT('Ctrl Pts',(-1.0376653042346,2.53623423377237,12.5228750347131));
#428342=CARTESIAN_POINT('Ctrl Pts',(-1.03743991167479,2.53594996973572,
12.5240609649613));
#428343=CARTESIAN_POINT('Ctrl Pts',(-1.03688669772864,2.53525225890799,
12.5269717671327));
#428344=CARTESIAN_POINT('Ctrl Pts',(-1.03656815484123,2.53442403827491,
12.5299036066169));
#428345=CARTESIAN_POINT('Ctrl Pts',(-1.03640945547241,2.53350901552302,
12.5328133004019));
#428346=CARTESIAN_POINT('Ctrl Pts',(-1.03633327053459,2.53306975132193,
12.5342101228451));
#428347=CARTESIAN_POINT('Ctrl Pts',(-1.03629453390577,2.53261094157895,
12.5356023438238));
#428348=CARTESIAN_POINT('Ctrl Pts',(-1.03628829969029,2.532138969605,12.5369868989719));
#428349=CARTESIAN_POINT('Origin',(-1.19934860600709,15.2783548945013,-1.24212577218808));
#428350=CARTESIAN_POINT('Ctrl Pts',(-1.13440045166831,2.4896875216687,12.5369868989719));
#428351=CARTESIAN_POINT('Ctrl Pts',(-1.14541345032086,2.50036446712909,
12.5369868989719));
#428352=CARTESIAN_POINT('Ctrl Pts',(-1.15923989832276,2.49372273246592,
12.5369868989719));
#428353=CARTESIAN_POINT('Ctrl Pts',(-1.13812332201667,2.49329669926858,
12.5218025310015));
#428354=CARTESIAN_POINT('Ctrl Pts',(-1.14857564694703,2.49881075106864,
12.5216901060418));
#428355=CARTESIAN_POINT('Ctrl Pts',(-1.15919775786794,2.49374299353988,
12.5161920673677));
#428356=CARTESIAN_POINT('Ctrl Pts',(-1.13723991511127,2.49925955625448,
12.5042015548895));
#428357=CARTESIAN_POINT('Ctrl Pts',(-1.14338789871131,2.50115155061784,
12.4980677368513));
#428358=CARTESIAN_POINT('Ctrl Pts',(-1.14956648980444,2.49832033324227,
12.4907278922778));
#428359=CARTESIAN_POINT('Ctrl Pts',(-1.12437901608947,2.50255140240162,
12.506463626192));
#428360=CARTESIAN_POINT('Ctrl Pts',(-1.12706041626462,2.50851944491462,
12.4999376786891));
#428361=CARTESIAN_POINT('Ctrl Pts',(-1.12702766686024,2.50844655395285,
12.4906970594712));
#428362=CARTESIAN_POINT('Origin',(-1.1497139406469,2.4738920458828,12.5369868989719));
#428363=CARTESIAN_POINT('Origin',(-1.1497139406469,2.4738920458828,14.));
#428364=CARTESIAN_POINT('Origin',(-1.1497139406469,2.4738920458828,13.7435492065112));
#428365=CARTESIAN_POINT('Ctrl Pts',(-1.11662063140439,2.4725156601775,13.793642941384));
#428366=CARTESIAN_POINT('Ctrl Pts',(-1.12437896590609,2.48004656083848,
13.8071662555867));
#428367=CARTESIAN_POINT('Ctrl Pts',(-1.13790823357821,2.46970352937323,
13.8103758687955));
#428368=CARTESIAN_POINT('Ctrl Pts',(-1.12857615642712,2.48406239680105,
13.7804579775006));
#428369=CARTESIAN_POINT('Ctrl Pts',(-1.13815630314232,2.49334757103985,
13.7901904343351));
#428370=CARTESIAN_POINT('Ctrl Pts',(-1.15205695112785,2.48592949111667,
13.7927914348263));
#428371=CARTESIAN_POINT('Ctrl Pts',(-1.13561482397145,2.49086039517658,
13.7597120340895));
#428372=CARTESIAN_POINT('Ctrl Pts',(-1.14670573982784,2.50160184179418,
13.7635825532445));
#428373=CARTESIAN_POINT('Ctrl Pts',(-1.16041970015636,2.49548112220804,
13.7651073818884));
#428374=CARTESIAN_POINT('Ctrl Pts',(-1.13423649169967,2.4895291914376,13.7381884353898));
#428375=CARTESIAN_POINT('Ctrl Pts',(-1.14506717868998,2.50001986014577,
13.7368803041982));
#428376=CARTESIAN_POINT('Ctrl Pts',(-1.15878239724748,2.49361030344978,
13.7363986145813));
#428377=CARTESIAN_POINT('Origin',(-1.13480505391374,2.45949293530441,13.7902182540695));
#428378=CARTESIAN_POINT('Ctrl Pts',(-1.09379172150105,2.45046737066223,
13.8235227101244));
#428379=CARTESIAN_POINT('Ctrl Pts',(-1.10205845368266,2.45845760391019,
13.8358800583119));
#428380=CARTESIAN_POINT('Ctrl Pts',(-1.11552693374205,2.44880223784017,
13.8390832900376));
#428381=CARTESIAN_POINT('Ctrl Pts',(-1.10237119621174,2.45875348935453,
13.8124254819053));
#428382=CARTESIAN_POINT('Ctrl Pts',(-1.11065398246338,2.4667592393222,13.8247886449157));
#428383=CARTESIAN_POINT('Ctrl Pts',(-1.12412954988472,2.4570778208427,13.8279860620657));
#428384=CARTESIAN_POINT('Ctrl Pts',(-1.11094682588098,2.46703589447802,
13.8013225099955));
#428385=CARTESIAN_POINT('Ctrl Pts',(-1.11924175666444,2.47505338517836,
13.8136962257787));
#428386=CARTESIAN_POINT('Ctrl Pts',(-1.13272799552254,2.46534976800002,
13.8168830918626));
#428387=CARTESIAN_POINT('Ctrl Pts',(-1.11951876011343,2.47531473052196,
13.7902140179785));
#428388=CARTESIAN_POINT('Ctrl Pts',(-1.12782218140957,2.48334043275437,
13.802602731458));
#428389=CARTESIAN_POINT('Ctrl Pts',(-1.14132243324893,2.47361822349952,
13.8057746032558));
#428390=CARTESIAN_POINT('Origin',(-1.1090780063399,2.43464556678509,13.8235269408515));
#428391=CARTESIAN_POINT('Ctrl Pts',(-1.03554215359084,2.4756499570046,13.8235269408515));
#428392=CARTESIAN_POINT('Ctrl Pts',(-1.03569810140076,2.48745640859141,
13.8362179249168));
#428393=CARTESIAN_POINT('Ctrl Pts',(-1.01888277881134,2.49044102418992,
13.8391868794938));
#428394=CARTESIAN_POINT('Ctrl Pts',(-1.03539946813276,2.4648475677069,13.8400110824519));
#428395=CARTESIAN_POINT('Ctrl Pts',(-1.03210379973435,2.47435863666198,
13.8494522556836));
#428396=CARTESIAN_POINT('Ctrl Pts',(-1.01876030594897,2.47266185705468,
13.85569149686));
#428397=CARTESIAN_POINT('Ctrl Pts',(-1.0418715466215,2.44989731934508,13.8586819406588));
#428398=CARTESIAN_POINT('Ctrl Pts',(-1.03788061071216,2.45163757053456,
13.868010383617));
#428399=CARTESIAN_POINT('Ctrl Pts',(-1.02963806849073,2.44790215027432,
13.8744918421245));
#428400=CARTESIAN_POINT('Ctrl Pts',(-1.07057230719779,2.43743385913977,
13.8587686893867));
#428401=CARTESIAN_POINT('Ctrl Pts',(-1.07452770130807,2.43570904455491,
13.8680909899357));
#428402=CARTESIAN_POINT('Ctrl Pts',(-1.07741743128625,2.42715650913208,
13.8745789365162));
#428403=CARTESIAN_POINT('Ctrl Pts',(-1.08601110090223,2.44295279209027,
13.8400379222776));
#428404=CARTESIAN_POINT('Ctrl Pts',(-1.09519764051676,2.4470610427908,13.8494748685452));
#428405=CARTESIAN_POINT('Ctrl Pts',(-1.10310113978058,2.43618465530915,
13.8557104837033));
#428406=CARTESIAN_POINT('Ctrl Pts',(-1.09379455227489,2.45047010568997,
13.8235269408542));
#428407=CARTESIAN_POINT('Ctrl Pts',(-1.10228764091277,2.45867279209016,
13.8362179249195));
#428408=CARTESIAN_POINT('Ctrl Pts',(-1.1159825431076,2.44846923104852,13.8391868794965));
#428409=CARTESIAN_POINT('Origin',(-1.01354407250541,2.47594052293312,13.8235269408515));
#428410=CARTESIAN_POINT('Ctrl Pts',(-1.03601449388505,2.51140981661443,
13.7902140241683));
#428411=CARTESIAN_POINT('Ctrl Pts',(-1.03617146712492,2.52295684890825,
13.8026027327198));
#428412=CARTESIAN_POINT('Ctrl Pts',(-1.01984013546842,2.52612947220744,
13.8057746032556));
#428413=CARTESIAN_POINT('Ctrl Pts',(-1.03585709833455,2.49949375982273,
13.8013225161808));
#428414=CARTESIAN_POINT('Ctrl Pts',(-1.0360139074304,2.51102898148478,13.8136962270464));
#428415=CARTESIAN_POINT('Ctrl Pts',(-1.01970571929065,2.51420413579781,
13.8168830918628));
#428416=CARTESIAN_POINT('Ctrl Pts',(-1.03569963492943,2.48757256591174,
13.8124254880875));
#428417=CARTESIAN_POINT('Ctrl Pts',(-1.03585621269812,2.49909089732053,
13.8247886461867));
#428418=CARTESIAN_POINT('Ctrl Pts',(-1.01957150574246,2.5022734877067,13.8279860620656));
#428419=CARTESIAN_POINT('Ctrl Pts',(-1.03554210092266,2.47564602691076,
13.8235227163066));
#428420=CARTESIAN_POINT('Ctrl Pts',(-1.03569837548615,2.48714203323894,
13.8358800595848));
#428421=CARTESIAN_POINT('Ctrl Pts',(-1.01943750119583,2.49033731070925,
13.8390832900376));
#428422=CARTESIAN_POINT('Origin',(-1.01401646563541,2.51170432507903,13.7902182540695));
#428423=CARTESIAN_POINT('Ctrl Pts',(-1.03628470792219,2.53186913360543,
13.7382347919292));
#428424=CARTESIAN_POINT('Ctrl Pts',(-1.03650801198745,2.54695780498591,
13.7369371795942));
#428425=CARTESIAN_POINT('Ctrl Pts',(-1.02242843431407,2.55255327364901,
13.7364597369711));
#428426=CARTESIAN_POINT('Ctrl Pts',(-1.03630969116454,2.53376052722437,
13.7595490285574));
#428427=CARTESIAN_POINT('Ctrl Pts',(-1.03653731775874,2.54920921624813,
13.7633824266926));
#428428=CARTESIAN_POINT('Ctrl Pts',(-1.0226667940499,2.55499732754202,13.7648920890506));
#428429=CARTESIAN_POINT('Ctrl Pts',(-1.03618227800523,2.52411452338656,
13.780380659011));
#428430=CARTESIAN_POINT('Ctrl Pts',(-1.03638456473314,2.53747700691635,
13.7901039518744));
#428431=CARTESIAN_POINT('Ctrl Pts',(-1.02145530532064,2.54253691351826,
13.7926933640892));
#428432=CARTESIAN_POINT('Ctrl Pts',(-1.03596080541507,2.50734761545859,
13.7936647693663));
#428433=CARTESIAN_POINT('Ctrl Pts',(-1.0361336210712,2.51816165571623,13.8072068914933));
#428434=CARTESIAN_POINT('Ctrl Pts',(-1.01931038434322,2.52092262942891,
13.8104111085397));
#428435=CARTESIAN_POINT('Origin',(-1.01429021860486,2.53242953553352,13.7435492065112));
#428436=CARTESIAN_POINT('Origin',(-1.01429021860486,2.53242953553352,14.));
#428437=CARTESIAN_POINT('Origin',(-1.01429021860486,2.53242953553352,12.5369868989719));
#428438=CARTESIAN_POINT('Ctrl Pts',(-1.05252460895684,2.53361254304276,
12.506462012331));
#428439=CARTESIAN_POINT('Ctrl Pts',(-1.05503307119812,2.53965085449332,
12.4999388158272));
#428440=CARTESIAN_POINT('Ctrl Pts',(-1.05500339280016,2.5395794133501,12.4907030323752));
#428441=CARTESIAN_POINT('Ctrl Pts',(-1.04131451142509,2.54072326005886,
12.5042014951932));
#428442=CARTESIAN_POINT('Ctrl Pts',(-1.03848251784149,2.54649568671134,
12.4980716682128));
#428443=CARTESIAN_POINT('Ctrl Pts',(-1.03219205801105,2.54905609299695,
12.4907355092743));
#428444=CARTESIAN_POINT('Ctrl Pts',(-1.03636521467194,2.53728375967444,
12.5218047446509));
#428445=CARTESIAN_POINT('Ctrl Pts',(-1.03322083903367,2.54866935464272,
12.5216906929433));
#428446=CARTESIAN_POINT('Ctrl Pts',(-1.02225870556527,2.55293577986187,
12.5161988840776));
#428447=CARTESIAN_POINT('Ctrl Pts',(-1.03628775876991,2.53210055728633,
12.5369868989719));
#428448=CARTESIAN_POINT('Ctrl Pts',(-1.03651699515108,2.54742873337489,
12.5369868989719));
#428449=CARTESIAN_POINT('Ctrl Pts',(-1.02221667589676,2.55295199334928,
12.5369868989719));
#428450=CARTESIAN_POINT('Origin',(-2.0441221157303E-31,-4.22882474612891E-32,
12.5));
#428451=CARTESIAN_POINT('Origin',(-1.23388492680974,2.38300613697744,12.5));
#428452=CARTESIAN_POINT('',(-1.23388492680974,2.38300613697744,12.5893111709658));
#428453=CARTESIAN_POINT('',(-1.23388492680974,2.38300613697744,13.8235269408515));
#428454=CARTESIAN_POINT('',(-1.23388492680974,2.38300613697744,12.5));
#428455=CARTESIAN_POINT('',(-1.2372708299804,2.41861243359644,13.7902182540695));
#428456=CARTESIAN_POINT('',(-1.23388492680974,2.38300613697744,13.8235269408515));
#428457=CARTESIAN_POINT('',(-1.23923296911494,2.43924636921444,13.7435492065112));
#428458=CARTESIAN_POINT('Origin',(-1.23277788158981,2.37136096293081,13.7445212918691));
#428459=CARTESIAN_POINT('',(-1.23923296911494,2.43924636921444,12.5369868989719));
#428460=CARTESIAN_POINT('',(-1.23923296911494,2.43924636921444,12.5));
#428461=CARTESIAN_POINT('Ctrl Pts',(-1.23923296911494,2.43924636921444,
12.5369868989719));
#428462=CARTESIAN_POINT('Ctrl Pts',(-1.23745158852547,2.42051329787037,
12.5544431401645));
#428463=CARTESIAN_POINT('Ctrl Pts',(-1.23566893384525,2.40176682813578,
12.5718848856037));
#428464=CARTESIAN_POINT('Ctrl Pts',(-1.23388492680974,2.38300613697744,
12.5893111709658));
#428465=CARTESIAN_POINT('Origin',(-1.50261144696405,2.52744636836289,12.5));
#428466=CARTESIAN_POINT('',(-1.33359077777893,2.38896564204893,13.7435492065112));
#428467=CARTESIAN_POINT('',(-1.31755783794952,2.37582965599925,13.7902182540695));
#428468=CARTESIAN_POINT('Origin',(-1.27542604312872,2.34131055501697,13.7418732680455));
#428469=CARTESIAN_POINT('',(-1.28989110379811,2.35316195826444,13.8235269408515));
#428470=CARTESIAN_POINT('',(-1.31755783794952,2.37582965599925,13.7902182540695));
#428471=CARTESIAN_POINT('',(-1.28989110379811,2.35316195826444,12.5893111709658));
#428472=CARTESIAN_POINT('',(-1.28989110379811,2.35316195826444,12.5));
#428473=CARTESIAN_POINT('',(-1.33359077777893,2.38896564204893,12.5369868989719));
#428474=CARTESIAN_POINT('Ctrl Pts',(-1.28989110379811,2.35316195826444,
12.5893111709658));
#428475=CARTESIAN_POINT('Ctrl Pts',(-1.30446849892371,2.36510539852232,
12.5718848856037));
#428476=CARTESIAN_POINT('Ctrl Pts',(-1.31903484374676,2.37703978513054,
12.5544431401645));
#428477=CARTESIAN_POINT('Ctrl Pts',(-1.33359077777893,2.38896564204893,
12.5369868989719));
#428478=CARTESIAN_POINT('',(-1.33359077777893,2.38896564204893,12.5));
#428479=CARTESIAN_POINT('Origin',(-1.2681055525358,2.37975200116018,12.5));
#428480=CARTESIAN_POINT('',(-1.25096085346492,2.34995855446554,13.8587068136939));
#428481=CARTESIAN_POINT('Ctrl Pts',(-1.28989110380218,2.35316195825924,
13.8235269408542));
#428482=CARTESIAN_POINT('Ctrl Pts',(-1.28853565106957,2.35205141905832,
13.8262006681044));
#428483=CARTESIAN_POINT('Ctrl Pts',(-1.28703843394242,2.35104933677319,
13.8288634856214));
#428484=CARTESIAN_POINT('Ctrl Pts',(-1.28541086667981,2.35014881787516,
13.8314912288862));
#428485=CARTESIAN_POINT('Ctrl Pts',(-1.28373301270785,2.34922047577551,
13.834200161153));
#428486=CARTESIAN_POINT('Ctrl Pts',(-1.28191500622142,2.34839860406482,
13.8368750301949));
#428487=CARTESIAN_POINT('Ctrl Pts',(-1.27993243346653,2.34770172933483,
13.8394886372968));
#428488=CARTESIAN_POINT('Ctrl Pts',(-1.27977931456361,2.34764790800905,
13.8396904925131));
#428489=CARTESIAN_POINT('Ctrl Pts',(-1.27962520321311,2.34759485158844,
13.8398919674349));
#428490=CARTESIAN_POINT('Ctrl Pts',(-1.2794700834679,2.34754257904207,13.8400930404591));
#428491=CARTESIAN_POINT('Ctrl Pts',(-1.27705321347805,2.3467281376024,13.8432258934518));
#428492=CARTESIAN_POINT('Ctrl Pts',(-1.27440424006349,2.3461070766296,13.8462331177034));
#428493=CARTESIAN_POINT('Ctrl Pts',(-1.27158753872682,2.34579357131293,
13.8489036603661));
#428494=CARTESIAN_POINT('Ctrl Pts',(-1.27066588126985,2.34569098872488,
13.8497774930041));
#428495=CARTESIAN_POINT('Ctrl Pts',(-1.2697264582903,2.34562149453788,13.85061494757));
#428496=CARTESIAN_POINT('Ctrl Pts',(-1.26877208296604,2.34558953415582,
13.8514076489583));
#428497=CARTESIAN_POINT('Ctrl Pts',(-1.26675344151369,2.34552193333839,
13.8530843267192));
#428498=CARTESIAN_POINT('Ctrl Pts',(-1.26446952301299,2.34561856868024,
13.8546805203176));
#428499=CARTESIAN_POINT('Ctrl Pts',(-1.26205865329298,2.34601015523619,
13.8559412814274));
#428500=CARTESIAN_POINT('Ctrl Pts',(-1.2617360007381,2.34606256221682,13.8561100121513));
#428501=CARTESIAN_POINT('Ctrl Pts',(-1.26141111409554,2.34612018636539,
13.8562727473908));
#428502=CARTESIAN_POINT('Ctrl Pts',(-1.26108435576156,2.34618327171143,
13.8564289040185));
#428503=CARTESIAN_POINT('Ctrl Pts',(-1.25960251044468,2.34646936303604,
13.8571370725437));
#428504=CARTESIAN_POINT('Ctrl Pts',(-1.25805655652251,2.34687503385115,
13.8577210840553));
#428505=CARTESIAN_POINT('Ctrl Pts',(-1.25651403447133,2.34741290263608,
13.8581177131616));
#428506=CARTESIAN_POINT('Ctrl Pts',(-1.25607960716972,2.3475643849988,13.8582294175695));
#428507=CARTESIAN_POINT('Ctrl Pts',(-1.25564542758903,2.34772617711724,
13.8583265086086));
#428508=CARTESIAN_POINT('Ctrl Pts',(-1.25521291800866,2.34789812987871,
13.8584082369006));
#428509=CARTESIAN_POINT('Ctrl Pts',(-1.2545915177237,2.34814517988599,13.8585256585398));
#428510=CARTESIAN_POINT('Ctrl Pts',(-1.25396595863925,2.34841657535878,
13.8586122832068));
#428511=CARTESIAN_POINT('Ctrl Pts',(-1.25335280526454,2.34870599067578,
13.8586682984299));
#428512=CARTESIAN_POINT('Ctrl Pts',(-1.25286234334472,2.34893749424056,
13.8587131050557));
#428513=CARTESIAN_POINT('Ctrl Pts',(-1.25237430186731,2.34918287255886,
13.8587357943552));
#428514=CARTESIAN_POINT('Ctrl Pts',(-1.2518888503355,2.34944260726282,13.8587355499465));
#428515=CARTESIAN_POINT('Ctrl Pts',(-1.25157509143687,2.34961047999432,
13.8587353919793));
#428516=CARTESIAN_POINT('Ctrl Pts',(-1.25126578915053,2.34978250043178,
13.8587257282814));
#428517=CARTESIAN_POINT('Ctrl Pts',(-1.25096085346492,2.34995855446554,
13.8587068136939));
#428518=CARTESIAN_POINT('Ctrl Pts',(-1.25096085346492,2.34995855446554,
13.8587068136939));
#428519=CARTESIAN_POINT('Ctrl Pts',(-1.24995793661838,2.35053758658503,
13.8586446046466));
#428520=CARTESIAN_POINT('Ctrl Pts',(-1.24900219510156,2.35116019736199,
13.858482427929));
#428521=CARTESIAN_POINT('Ctrl Pts',(-1.24809093786802,2.35182281689079,
13.8582284286032));
#428522=CARTESIAN_POINT('Ctrl Pts',(-1.24715609394828,2.35250258744822,
13.8579678548414));
#428523=CARTESIAN_POINT('Ctrl Pts',(-1.24626668415136,2.35322736397738,
13.857615680862));
#428524=CARTESIAN_POINT('Ctrl Pts',(-1.24545165172919,2.35396106122987,
13.8571944833187));
#428525=CARTESIAN_POINT('Ctrl Pts',(-1.24341765496499,2.35579207775985,
13.8561433417727));
#428526=CARTESIAN_POINT('Ctrl Pts',(-1.24174853040234,2.35776073801542,
13.8546163505475));
#428527=CARTESIAN_POINT('Ctrl Pts',(-1.24041326507549,2.35966260114303,
13.8528973491087));
#428528=CARTESIAN_POINT('Ctrl Pts',(-1.24016933180026,2.3600100434771,13.8525833129073));
#428529=CARTESIAN_POINT('Ctrl Pts',(-1.23993640061154,2.36035523793739,
13.8522628768812));
#428530=CARTESIAN_POINT('Ctrl Pts',(-1.23971410366792,2.36069694252038,
13.851937733538));
#428531=CARTESIAN_POINT('Ctrl Pts',(-1.23835656707558,2.36278368499922,
13.8499521282529));
#428532=CARTESIAN_POINT('Ctrl Pts',(-1.23726412632978,2.36494988372643,
13.847639871647));
#428533=CARTESIAN_POINT('Ctrl Pts',(-1.23642246133848,2.36704551459069,
13.8452109780794));
#428534=CARTESIAN_POINT('Ctrl Pts',(-1.2360437788373,2.36798838229392,13.8441181685877));
#428535=CARTESIAN_POINT('Ctrl Pts',(-1.23571514305624,2.36891694439013,
13.8430021611332));
#428536=CARTESIAN_POINT('Ctrl Pts',(-1.23543207530215,2.36981847020278,
13.8418824960098));
#428537=CARTESIAN_POINT('Ctrl Pts',(-1.23476501891126,2.37194293880158,
13.8392439765549));
#428538=CARTESIAN_POINT('Ctrl Pts',(-1.23431551475758,2.37401769473368,
13.8364981347964));
#428539=CARTESIAN_POINT('Ctrl Pts',(-1.23404892947329,2.37604097902391,
13.8336931113419));
#428540=CARTESIAN_POINT('Ctrl Pts',(-1.23378929233613,2.37801152943216,
13.8309611966328));
#428541=CARTESIAN_POINT('Ctrl Pts',(-1.23370346272186,2.37993530468263,
13.8281701127186));
#428542=CARTESIAN_POINT('Ctrl Pts',(-1.2337976062358,2.38180128650958,13.8253580685121));
#428543=CARTESIAN_POINT('Ctrl Pts',(-1.23381801665123,2.38220583338349,
13.8247484142933));
#428544=CARTESIAN_POINT('Ctrl Pts',(-1.23384702501419,2.3826075601408,13.8241378483365));
#428545=CARTESIAN_POINT('Ctrl Pts',(-1.23388492680974,2.38300613697744,
13.8235269408515));
#428546=CARTESIAN_POINT('',(-1.25204841130135,2.3493585587908,12.5969504640361));
#428547=CARTESIAN_POINT('Origin',(-1.26812093887242,2.379781291832,12.584524458991));
#428548=CARTESIAN_POINT('Origin',(-1.26812093887242,2.379781291832,12.584524458991));
#428549=CARTESIAN_POINT('Ctrl Pts',(-1.28989110379811,2.35316195826444,
12.5893111709658));
#428550=CARTESIAN_POINT('Ctrl Pts',(-1.2811239629891,2.34597893128448,12.5770542771492));
#428551=CARTESIAN_POINT('Ctrl Pts',(-1.26857444251691,2.35648194088997,
12.5737548217797));
#428552=CARTESIAN_POINT('Ctrl Pts',(-1.3090618984075,2.36886882757411,12.5663937883685));
#428553=CARTESIAN_POINT('Ctrl Pts',(-1.30028357389284,2.36167663764567,
12.5540940315304));
#428554=CARTESIAN_POINT('Ctrl Pts',(-1.28769722596902,2.37221465649431,
12.5508374392248));
#428555=CARTESIAN_POINT('Ctrl Pts',(-1.32821334992012,2.38455984884519,
12.5434499600945));
#428556=CARTESIAN_POINT('Ctrl Pts',(-1.31940648394648,2.37734427454605,
12.5311293540533));
#428557=CARTESIAN_POINT('Ctrl Pts',(-1.30680207566588,2.38793108976406,
12.5278936106989));
#428558=CARTESIAN_POINT('Ctrl Pts',(-1.34734697350727,2.40023626347626,
12.5204817579905));
#428559=CARTESIAN_POINT('Ctrl Pts',(-1.33849651956565,2.39298497701554,
12.5081597038247));
#428560=CARTESIAN_POINT('Ctrl Pts',(-1.32589039429109,2.40363249552723,
12.5049254088044));
#428561=CARTESIAN_POINT('Ctrl Pts',(-1.33359077777893,2.38896564204893,
12.5369868989719));
#428562=CARTESIAN_POINT('Ctrl Pts',(-1.33431132319719,2.38955599403796,
12.5342545179733));
#428563=CARTESIAN_POINT('Ctrl Pts',(-1.33491991960081,2.39021589367493,
12.5314872231885));
#428564=CARTESIAN_POINT('Ctrl Pts',(-1.33534119081486,2.39094606603426,
12.5287124745063));
#428565=CARTESIAN_POINT('Ctrl Pts',(-1.33572111410573,2.39160457171043,
12.5262100684184));
#428566=CARTESIAN_POINT('Ctrl Pts',(-1.33594744434302,2.39232005962886,
12.5237004536639));
#428567=CARTESIAN_POINT('Ctrl Pts',(-1.33596086397918,2.39312480833795,
12.5212220730815));
#428568=CARTESIAN_POINT('Ctrl Pts',(-1.33597113787156,2.39374091309109,
12.5193246583486));
#428569=CARTESIAN_POINT('Ctrl Pts',(-1.33585610831898,2.39441670952873,
12.517417831369));
#428570=CARTESIAN_POINT('Ctrl Pts',(-1.33551858733187,2.39515511611507,
12.5155812248348));
#428571=CARTESIAN_POINT('Ctrl Pts',(-1.33537480157718,2.39546968128981,
12.5147988205793));
#428572=CARTESIAN_POINT('Ctrl Pts',(-1.33519074393596,2.39579604348345,
12.5140295443047));
#428573=CARTESIAN_POINT('Ctrl Pts',(-1.33496000016923,2.39613624940191,
12.5132817086137));
#428574=CARTESIAN_POINT('Ctrl Pts',(-1.3346108006926,2.39665110503747,12.5121499604604));
#428575=CARTESIAN_POINT('Ctrl Pts',(-1.33414121780903,2.39720477012786,
12.5110494206568));
#428576=CARTESIAN_POINT('Ctrl Pts',(-1.33351660945326,2.39778357624014,
12.5100666561695));
#428577=CARTESIAN_POINT('Ctrl Pts',(-1.33315796077373,2.39811592537693,
12.5095023550641));
#428578=CARTESIAN_POINT('Ctrl Pts',(-1.33274361220289,2.39845992479159,
12.5089719619137));
#428579=CARTESIAN_POINT('Ctrl Pts',(-1.33227725044621,2.39880421246036,
12.5085043804652));
#428580=CARTESIAN_POINT('Ctrl Pts',(-1.33159479076321,2.39930803261697,
12.5078201359221));
#428581=CARTESIAN_POINT('Ctrl Pts',(-1.3307804364317,2.39982611083052,12.5072563000949));
#428582=CARTESIAN_POINT('Ctrl Pts',(-1.32988484439441,2.40031618601774,
12.5068768744332));
#428583=CARTESIAN_POINT('Ctrl Pts',(-1.32923906088276,2.40066956396461,
12.5066032824114));
#428584=CARTESIAN_POINT('Ctrl Pts',(-1.32853972200176,2.40101464301381,
12.5064197834844));
#428585=CARTESIAN_POINT('Ctrl Pts',(-1.3278270244449,2.40133447107659,12.5063282718343));
#428586=CARTESIAN_POINT('Ctrl Pts',(-1.32678670665749,2.40180132103198,
12.5061946931565));
#428587=CARTESIAN_POINT('Ctrl Pts',(-1.32569612491923,2.40222531625855,
12.5062515701262));
#428588=CARTESIAN_POINT('Ctrl Pts',(-1.32462856633783,2.40259455641616,
12.5064436508398));
#428589=CARTESIAN_POINT('',(-1.26857444251691,2.35648194088997,12.5737548217797));
#428590=CARTESIAN_POINT('Origin',(-1.27594835099023,2.37017958571772,12.5893111709658));
#428591=CARTESIAN_POINT('Ctrl Pts',(-1.32462856633783,2.40259455641616,
12.5064436508398));
#428592=CARTESIAN_POINT('Ctrl Pts',(-1.31633079446817,2.39576906231314,
12.5164271754438));
#428593=CARTESIAN_POINT('Ctrl Pts',(-1.30802986609324,2.3889407012261,12.5264061185523));
#428594=CARTESIAN_POINT('Ctrl Pts',(-1.29972566944228,2.38210937291322,
12.536380305637));
#428595=CARTESIAN_POINT('Ctrl Pts',(-1.28934710790115,2.37357159806479,
12.5488460165097));
#428596=CARTESIAN_POINT('Ctrl Pts',(-1.27896343828533,2.36502918588953,
12.5613043021964));
#428597=CARTESIAN_POINT('Ctrl Pts',(-1.26857444251691,2.35648194088997,
12.5737548217797));
#428598=CARTESIAN_POINT('Ctrl Pts',(-1.23388492680974,2.38300613697744,
12.5893111709658));
#428599=CARTESIAN_POINT('Ctrl Pts',(-1.23281198882941,2.37172307716859,
12.5770542771492));
#428600=CARTESIAN_POINT('Ctrl Pts',(-1.24852873949897,2.36716375449456,
12.5737548217797));
#428601=CARTESIAN_POINT('Ctrl Pts',(-1.23288388500602,2.37247914031066,
12.5928319619712));
#428602=CARTESIAN_POINT('Ctrl Pts',(-1.235405916872,2.36458783042964,12.5821634970842));
#428603=CARTESIAN_POINT('Ctrl Pts',(-1.24815468773411,2.3633299179505,12.5773203894503));
#428604=CARTESIAN_POINT('Ctrl Pts',(-1.23839796806602,2.35666209294564,
12.5969440695591));
#428605=CARTESIAN_POINT('Ctrl Pts',(-1.24193687042678,2.35475560071305,
12.5878292599214));
#428606=CARTESIAN_POINT('Ctrl Pts',(-1.25012195140077,2.35769307302062,
12.5813877129824));
#428607=CARTESIAN_POINT('Ctrl Pts',(-1.26537506308586,2.34222562558581,
12.596957478804));
#428608=CARTESIAN_POINT('Ctrl Pts',(-1.26186235218005,2.344118098899,12.5878468778671));
#428609=CARTESIAN_POINT('Ctrl Pts',(-1.25978024216687,2.35253132062618,
12.5814011370086));
#428610=CARTESIAN_POINT('Ctrl Pts',(-1.2816995608148,2.34645052570746,12.5928371701607));
#428611=CARTESIAN_POINT('Ctrl Pts',(-1.27374688640638,2.34415051799933,
12.5821692192952));
#428612=CARTESIAN_POINT('Ctrl Pts',(-1.26559142138311,2.35402534519893,
12.5773318885715));
#428613=CARTESIAN_POINT('Ctrl Pts',(-1.28989110379814,2.3531619582644,12.5893111709658));
#428614=CARTESIAN_POINT('Ctrl Pts',(-1.28112396298914,2.34597893128444,
12.5770542771492));
#428615=CARTESIAN_POINT('Ctrl Pts',(-1.26857444251695,2.35648194088993,
12.5737548217797));
#428616=CARTESIAN_POINT('',(-1.24852873949897,2.36716375449456,12.5737548217797));
#428617=CARTESIAN_POINT('Origin',(-1.25578612727442,2.3809234900544,12.5893111709658));
#428618=CARTESIAN_POINT('Ctrl Pts',(-1.26857444251695,2.35648194088993,
12.5737548217797));
#428619=CARTESIAN_POINT('Ctrl Pts',(-1.26782037265869,2.35582186643966,
12.5746934679442));
#428620=CARTESIAN_POINT('Ctrl Pts',(-1.26686528919211,2.35522928647873,
12.5756680099006));
#428621=CARTESIAN_POINT('Ctrl Pts',(-1.2658196091199,2.35476879016542,12.5765688348656));
#428622=CARTESIAN_POINT('Ctrl Pts',(-1.26554277689685,2.35464687886433,
12.5768073183026));
#428623=CARTESIAN_POINT('Ctrl Pts',(-1.26525975281126,2.3545340218877,12.5770407398754));
#428624=CARTESIAN_POINT('Ctrl Pts',(-1.26497280837479,2.35443090043853,
12.5772674179684));
#428625=CARTESIAN_POINT('Ctrl Pts',(-1.26379526600055,2.35400771789635,
12.5781976435658));
#428626=CARTESIAN_POINT('Ctrl Pts',(-1.26248100615068,2.35373506696603,
12.5790594849312));
#428627=CARTESIAN_POINT('Ctrl Pts',(-1.2611089607031,2.35367863990307,12.5797571720116));
#428628=CARTESIAN_POINT('Ctrl Pts',(-1.26021502375964,2.35364187564261,
12.580211740231));
#428629=CARTESIAN_POINT('Ctrl Pts',(-1.25925516059535,2.35371398449211,
12.5806009430798));
#428630=CARTESIAN_POINT('Ctrl Pts',(-1.25829826861342,2.35390755721551,
12.5808812374708));
#428631=CARTESIAN_POINT('Ctrl Pts',(-1.25747598095534,2.354073900402,12.5811221033394));
#428632=CARTESIAN_POINT('Ctrl Pts',(-1.25663907557899,2.35433345606794,
12.581287365893));
#428633=CARTESIAN_POINT('Ctrl Pts',(-1.25583725863703,2.35467953824755,
12.581359338449));
#428634=CARTESIAN_POINT('Ctrl Pts',(-1.25572582263898,2.35472763652419,
12.5813693411482));
#428635=CARTESIAN_POINT('Ctrl Pts',(-1.25561502368873,2.35477736215924,
12.5813775999465));
#428636=CARTESIAN_POINT('Ctrl Pts',(-1.25550495273787,2.35482865295239,
12.5813841266931));
#428637=CARTESIAN_POINT('Ctrl Pts',(-1.25531820405693,2.35491567398647,
12.5813952001081));
#428638=CARTESIAN_POINT('Ctrl Pts',(-1.25513255735676,2.3550083350831,12.5814007534795));
#428639=CARTESIAN_POINT('Ctrl Pts',(-1.25494818156407,2.3551067723368,12.5814005856065));
#428640=CARTESIAN_POINT('Ctrl Pts',(-1.25410418127139,2.35555737959776,
12.5813998171494));
#428641=CARTESIAN_POINT('Ctrl Pts',(-1.25334496719951,2.35609759214273,
12.58127954464));
#428642=CARTESIAN_POINT('Ctrl Pts',(-1.25265769503836,2.35670023389671,
12.5810700125799));
#428643=CARTESIAN_POINT('Ctrl Pts',(-1.2518275485199,2.35742815651926,12.5808169217085));
#428644=CARTESIAN_POINT('Ctrl Pts',(-1.25111332339607,2.35825981199598,
12.5804173076348));
#428645=CARTESIAN_POINT('Ctrl Pts',(-1.2505578564924,2.35910534844497,12.5799304713245));
#428646=CARTESIAN_POINT('Ctrl Pts',(-1.24986945800863,2.36015323447673,
12.5793271277669));
#428647=CARTESIAN_POINT('Ctrl Pts',(-1.24935528144683,2.36126976269925,
12.5785808224116));
#428648=CARTESIAN_POINT('Ctrl Pts',(-1.24900819149589,2.36239460243404,
12.5777485681082));
#428649=CARTESIAN_POINT('Ctrl Pts',(-1.24849098944245,2.36407073687427,
12.576508418016));
#428650=CARTESIAN_POINT('Ctrl Pts',(-1.24834257912397,2.36574918672104,
12.5750928681475));
#428651=CARTESIAN_POINT('Ctrl Pts',(-1.24852873949897,2.36716375449456,
12.5737548217797));
#428652=CARTESIAN_POINT('Ctrl Pts',(-1.24852873949897,2.36716375449456,
12.5737548217797));
#428653=CARTESIAN_POINT('Ctrl Pts',(-1.23281198882941,2.37172307716859,
12.5770542771492));
#428654=CARTESIAN_POINT('Ctrl Pts',(-1.23388492680974,2.38300613697744,
12.5893111709658));
#428655=CARTESIAN_POINT('Ctrl Pts',(-1.25092276405561,2.39180687930844,
12.5508408821982));
#428656=CARTESIAN_POINT('Ctrl Pts',(-1.23515642283701,2.39637724135191,
12.55409748406));
#428657=CARTESIAN_POINT('Ctrl Pts',(-1.23623072961141,2.40767469545534,
12.5663972313419));
#428658=CARTESIAN_POINT('Ctrl Pts',(-1.25331327596572,2.41642604494416,
12.52790050457));
#428659=CARTESIAN_POINT('Ctrl Pts',(-1.23749636669548,2.42098418694264,
12.5311362602938));
#428660=CARTESIAN_POINT('Ctrl Pts',(-1.23857416588352,2.4323183674113,12.5434568539655));
#428661=CARTESIAN_POINT('Ctrl Pts',(-1.25570053442384,2.44102311467636,
12.5049357605811));
#428662=CARTESIAN_POINT('Ctrl Pts',(-1.23983228847987,2.44554883623774,
12.5081700652078));
#428663=CARTESIAN_POINT('Ctrl Pts',(-1.24091542097314,2.45693910196279,
12.5204921097672));
#428664=CARTESIAN_POINT('Ctrl Pts',(-1.25554377609601,2.4394079748135,12.5064436508395));
#428665=CARTESIAN_POINT('Ctrl Pts',(-1.25456961154573,2.44014272049711,
12.5062361689309));
#428666=CARTESIAN_POINT('Ctrl Pts',(-1.25352522894396,2.44086525534164,
12.5061871075061));
#428667=CARTESIAN_POINT('Ctrl Pts',(-1.25247662715064,2.44150669974309,
12.5063648335164));
#428668=CARTESIAN_POINT('Ctrl Pts',(-1.25200028753567,2.44179808335616,
12.5064455676329));
#428669=CARTESIAN_POINT('Ctrl Pts',(-1.25151631836267,2.44207660991371,
12.506574497099));
#428670=CARTESIAN_POINT('Ctrl Pts',(-1.25104494656484,2.4423294261566,12.5067492519495));
#428671=CARTESIAN_POINT('Ctrl Pts',(-1.25009770663982,2.44283747021027,
12.5071004286051));
#428672=CARTESIAN_POINT('Ctrl Pts',(-1.24916612939584,2.44325965643752,
12.5076537929612));
#428673=CARTESIAN_POINT('Ctrl Pts',(-1.24832403888024,2.4435729125784,12.5083435010503));
#428674=CARTESIAN_POINT('Ctrl Pts',(-1.24827102424984,2.44359263392453,
12.5083869222963));
#428675=CARTESIAN_POINT('Ctrl Pts',(-1.24821835435351,2.44361191449586,
12.5084308732336));
#428676=CARTESIAN_POINT('Ctrl Pts',(-1.24816604329756,2.44363074514883,
12.5084753333615));
#428677=CARTESIAN_POINT('Ctrl Pts',(-1.24774643958516,2.44378179183962,
12.508831962269));
#428678=CARTESIAN_POINT('Ctrl Pts',(-1.24734184252986,2.44390817040486,
12.509227847131));
#428679=CARTESIAN_POINT('Ctrl Pts',(-1.24696511774763,2.44400879565481,
12.5096423454524));
#428680=CARTESIAN_POINT('Ctrl Pts',(-1.24578462901153,2.44432411065328,
12.5109411997424));
#428681=CARTESIAN_POINT('Ctrl Pts',(-1.24480771065434,2.44441528418586,
12.5124831113042));
#428682=CARTESIAN_POINT('Ctrl Pts',(-1.24400455647081,2.44437213522341,
12.5140723025008));
#428683=CARTESIAN_POINT('Ctrl Pts',(-1.24392930004414,2.44436809211837,
12.5142212114565));
#428684=CARTESIAN_POINT('Ctrl Pts',(-1.24385555063965,2.44436289270466,
12.5143705582413));
#428685=CARTESIAN_POINT('Ctrl Pts',(-1.24378327430942,2.44435662500092,
12.5145201959299));
#428686=CARTESIAN_POINT('Ctrl Pts',(-1.24285477723943,2.44427610701477,
12.5164425148273));
#428687=CARTESIAN_POINT('Ctrl Pts',(-1.24213664355196,2.44402722594623,
12.5184635205941));
#428688=CARTESIAN_POINT('Ctrl Pts',(-1.24156007758763,2.44366833533676,
12.5205025929157));
#428689=CARTESIAN_POINT('Ctrl Pts',(-1.24122564647538,2.44346016455818,
12.5216853356836));
#428690=CARTESIAN_POINT('Ctrl Pts',(-1.24093919383844,2.44321576807429,
12.5228750347131));
#428691=CARTESIAN_POINT('Ctrl Pts',(-1.24069138109582,2.44295082148883,
12.5240609649613));
#428692=CARTESIAN_POINT('Ctrl Pts',(-1.24008313801374,2.44230052430872,
12.5269717671327));
#428693=CARTESIAN_POINT('Ctrl Pts',(-1.2396981473811,2.44150102371401,12.5299036066169));
#428694=CARTESIAN_POINT('Ctrl Pts',(-1.23946539322239,2.44060198109668,
12.5328133004019));
#428695=CARTESIAN_POINT('Ctrl Pts',(-1.23935365767335,2.44017038829069,
12.5342101228451));
#428696=CARTESIAN_POINT('Ctrl Pts',(-1.23927765268403,2.43971626259414,
12.5356023438238));
#428697=CARTESIAN_POINT('Ctrl Pts',(-1.23923296911494,2.43924636921444,
12.5369868989719));
#428698=CARTESIAN_POINT('Origin',(-2.44055823560797,15.1283953684929,-1.24064857945397));
#428699=CARTESIAN_POINT('Ctrl Pts',(-1.33355847389414,2.38893912375418,
12.5369868989719));
#428700=CARTESIAN_POINT('Ctrl Pts',(-1.34540509787711,2.39868288092943,
12.5369868989719));
#428701=CARTESIAN_POINT('Ctrl Pts',(-1.35864417647996,2.39093626221983,
12.5369868989719));
#428702=CARTESIAN_POINT('Ctrl Pts',(-1.33756313817891,2.39223284361851,
12.5218025310015));
#428703=CARTESIAN_POINT('Ctrl Pts',(-1.34843013027199,2.39687658634958,
12.5216901060417));
#428704=CARTESIAN_POINT('Ctrl Pts',(-1.35860382770967,2.390959890715,12.5161920673677));
#428705=CARTESIAN_POINT('Ctrl Pts',(-1.33716869893787,2.39824786555357,
12.5042015548895));
#428706=CARTESIAN_POINT('Ctrl Pts',(-1.34345044073467,2.39963244672326,
12.4980677368515));
#428707=CARTESIAN_POINT('Ctrl Pts',(-1.3493777025758,2.39630703745667,12.4907278922778));
#428708=CARTESIAN_POINT('Ctrl Pts',(-1.32461890951763,2.40257704101929,
12.506463626192));
#428709=CARTESIAN_POINT('Ctrl Pts',(-1.32777783842431,2.40830666635597,
12.4999376786891));
#428710=CARTESIAN_POINT('Ctrl Pts',(-1.32773925670079,2.40823668731335,
12.4906970594712));
#428711=CARTESIAN_POINT('Origin',(-1.3475335305868,2.37194801459566,12.5369868989719));
#428712=CARTESIAN_POINT('Origin',(-1.3475335305868,2.37194801459566,14.));
#428713=CARTESIAN_POINT('Origin',(-1.3475335305868,2.37194801459566,13.7435492065112));
#428714=CARTESIAN_POINT('Ctrl Pts',(-1.31443814838807,2.3732736206268,13.793642941384));
#428715=CARTESIAN_POINT('Ctrl Pts',(-1.32278450598908,2.38014708655031,
13.8071662555867));
#428716=CARTESIAN_POINT('Ctrl Pts',(-1.33542570305467,2.36873570975417,
13.8103758687955));
#428717=CARTESIAN_POINT('Ctrl Pts',(-1.32729505861706,2.38380745015776,
13.7804579775006));
#428718=CARTESIAN_POINT('Ctrl Pts',(-1.33760015608416,2.39228085785026,
13.7901904343351));
#428719=CARTESIAN_POINT('Ctrl Pts',(-1.3508499084304,2.38375442911789,13.7927914348262));
#428720=CARTESIAN_POINT('Ctrl Pts',(-1.3348644055529,2.3900091120058,13.7597120340895));
#428721=CARTESIAN_POINT('Ctrl Pts',(-1.34679394491978,2.39981080474053,
13.7635825532445));
#428722=CARTESIAN_POINT('Ctrl Pts',(-1.35996337770837,2.39259263626295,
13.7651073818885));
#428723=CARTESIAN_POINT('Ctrl Pts',(-1.33338215410505,2.38879468461343,
13.7381884353898));
#428724=CARTESIAN_POINT('Ctrl Pts',(-1.3450318897682,2.39836764494998,13.7368803041982));
#428725=CARTESIAN_POINT('Ctrl Pts',(-1.35817903369322,2.39086149788683,
13.7363986145813));
#428726=CARTESIAN_POINT('Origin',(-1.3315005907574,2.35881202854597,13.7902182540695));
#428727=CARTESIAN_POINT('Ctrl Pts',(-1.28988805951734,2.35315946306641,
13.8235227101244));
#428728=CARTESIAN_POINT('Ctrl Pts',(-1.29877856301699,2.36044929405501,
13.8358800583119));
#428729=CARTESIAN_POINT('Ctrl Pts',(-1.31141522584932,2.34972824925896,
13.8390832900376));
#428730=CARTESIAN_POINT('Ctrl Pts',(-1.2991143823317,2.36071870354545,13.8124254819053));
#428731=CARTESIAN_POINT('Ctrl Pts',(-1.30802215123948,2.36802269106741,
13.8247886449158));
#428732=CARTESIAN_POINT('Ctrl Pts',(-1.32066375433791,2.35727510286332,
13.8279860620657));
#428733=CARTESIAN_POINT('Ctrl Pts',(-1.30833657020832,2.36827455621884,
13.8013225099955));
#428734=CARTESIAN_POINT('Ctrl Pts',(-1.31725740021674,2.37558925551505,
13.8136962257787));
#428735=CARTESIAN_POINT('Ctrl Pts',(-1.32990782984351,2.3648186726553,13.8168830918626));
#428736=CARTESIAN_POINT('Ctrl Pts',(-1.31755478403128,2.37582715290089,
13.7902140179785));
#428737=CARTESIAN_POINT('Ctrl Pts',(-1.32648474561696,2.38314934435037,
13.802602731458));
#428738=CARTESIAN_POINT('Ctrl Pts',(-1.33914762617117,2.37235908908966,
13.8057746032558));
#428739=CARTESIAN_POINT('Origin',(-1.30383385660598,2.33614433081117,13.8235269408515));
#428740=CARTESIAN_POINT('Ctrl Pts',(-1.23388492680974,2.38300613697744,
13.8235269408515));
#428741=CARTESIAN_POINT('Ctrl Pts',(-1.23500269112627,2.3947605923763,13.8362179249168));
#428742=CARTESIAN_POINT('Ctrl Pts',(-1.2184865940147,2.3991058818095,13.8391868794938));
#428743=CARTESIAN_POINT('Ctrl Pts',(-1.23286222111351,2.37225132192846,
13.8400110824519));
#428744=CARTESIAN_POINT('Ctrl Pts',(-1.2303527591961,2.38199937115624,13.8494522556837));
#428745=CARTESIAN_POINT('Ctrl Pts',(-1.21691536149542,2.38139585606149,
13.85569149686));
#428746=CARTESIAN_POINT('Ctrl Pts',(-1.23809418026215,2.35682328480407,
13.8586819406588));
#428747=CARTESIAN_POINT('Ctrl Pts',(-1.23425837049046,2.35888304377793,
13.868010383617));
#428748=CARTESIAN_POINT('Ctrl Pts',(-1.22573878321916,2.35583189653154,
13.8744918421245));
#428749=CARTESIAN_POINT('Ctrl Pts',(-1.26568355371342,2.34206191730261,
13.8587686893867));
#428750=CARTESIAN_POINT('Ctrl Pts',(-1.26948519817504,2.34002044055592,
13.8680909899357));
#428751=CARTESIAN_POINT('Ctrl Pts',(-1.27166820178028,2.33126082316899,
13.8745789365163));
#428752=CARTESIAN_POINT('Ctrl Pts',(-1.28152082037615,2.3463040814453,13.8400379222776));
#428753=CARTESIAN_POINT('Ctrl Pts',(-1.29101165310921,2.34964987401829,
13.8494748685453));
#428754=CARTESIAN_POINT('Ctrl Pts',(-1.29800232757999,2.33816546825623,
13.8557104837033));
#428755=CARTESIAN_POINT('Ctrl Pts',(-1.28989110380218,2.35316195825924,
13.8235269408542));
#428756=CARTESIAN_POINT('Ctrl Pts',(-1.29902452747989,2.36064508532712,
13.8362179249195));
#428757=CARTESIAN_POINT('Ctrl Pts',(-1.31184217606728,2.34935921412697,
13.8391868794965));
#428758=CARTESIAN_POINT('Origin',(-1.21198372634507,2.38508878390049,13.8235269408515));
#428759=CARTESIAN_POINT('Ctrl Pts',(-1.23727045596713,2.41860850848543,
13.7902140241683));
#428760=CARTESIAN_POINT('Ctrl Pts',(-1.23836809722087,2.43010432420553,
13.8026027327198));
#428761=CARTESIAN_POINT('Ctrl Pts',(-1.22234970497529,2.43459754600511,
13.8057746032556));
#428762=CARTESIAN_POINT('Ctrl Pts',(-1.23614231488555,2.40674493058826,
13.8013225161808));
#428763=CARTESIAN_POINT('Ctrl Pts',(-1.2372388298653,2.41822898835476,13.8136962270464));
#428764=CARTESIAN_POINT('Ctrl Pts',(-1.22124371042945,2.42272284633497,
13.8168830918628));
#428765=CARTESIAN_POINT('Ctrl Pts',(-1.2350136874522,2.3948762381959,13.8124254880875));
#428766=CARTESIAN_POINT('Ctrl Pts',(-1.23610859516207,2.40634348076539,
13.8247886461867));
#428767=CARTESIAN_POINT('Ctrl Pts',(-1.22013748488761,2.41084283614132,
13.8279860620656));
#428768=CARTESIAN_POINT('Ctrl Pts',(-1.23388455397768,2.38300222425361,
13.8235227163065));
#428769=CARTESIAN_POINT('Ctrl Pts',(-1.23497733978991,2.39444724074138,
13.8358800595847));
#428770=CARTESIAN_POINT('Ctrl Pts',(-1.2190310169947,2.39895729840275,13.8390832900376));
#428771=CARTESIAN_POINT('Origin',(-1.21536962951573,2.42069508051949,13.7902182540695));
#428772=CARTESIAN_POINT('Ctrl Pts',(-1.23920739515915,2.43897772383434,
13.7382347919292));
#428773=CARTESIAN_POINT('Ctrl Pts',(-1.24065982299245,2.45399798755115,
13.7369371795942));
#428774=CARTESIAN_POINT('Ctrl Pts',(-1.22708317659414,2.46072245404268,
13.7364597369712));
#428775=CARTESIAN_POINT('Ctrl Pts',(-1.23938646141061,2.44086078763087,
13.7595490285574));
#428776=CARTESIAN_POINT('Ctrl Pts',(-1.24087254217017,2.45623951873574,
13.7633824266926));
#428777=CARTESIAN_POINT('Ctrl Pts',(-1.22751995628939,2.46313894701669,
13.7648920890506));
#428778=CARTESIAN_POINT('Ctrl Pts',(-1.23847323334616,2.43125726543041,
13.7803806590111));
#428779=CARTESIAN_POINT('Ctrl Pts',(-1.2397640134406,2.44455879815232,13.7901039518744));
#428780=CARTESIAN_POINT('Ctrl Pts',(-1.22529685926915,2.45081874157102,
13.7926933640892));
#428781=CARTESIAN_POINT('Ctrl Pts',(-1.23688583903527,2.41456420007755,
13.7936647693663));
#428782=CARTESIAN_POINT('Ctrl Pts',(-1.23793952433521,2.42532817142801,
13.8072068914933));
#428783=CARTESIAN_POINT('Ctrl Pts',(-1.22139731052884,2.42945120820106,
13.8104111085397));
#428784=CARTESIAN_POINT('Origin',(-1.21733176865027,2.44132901613749,13.7435492065112));
#428785=CARTESIAN_POINT('Origin',(-1.21733176865027,2.44132901613749,14.));
#428786=CARTESIAN_POINT('Origin',(-1.21733176865027,2.44132901613749,12.5369868989719));
#428787=CARTESIAN_POINT('Ctrl Pts',(-1.25553536331697,2.43939162952238,
12.506462012331));
#428788=CARTESIAN_POINT('Ctrl Pts',(-1.25852765729725,2.44520538602962,
12.4999388158272));
#428789=CARTESIAN_POINT('Ctrl Pts',(-1.25849225453531,2.44513660166587,
12.4907030323752));
#428790=CARTESIAN_POINT('Ctrl Pts',(-1.2449421559095,2.44739241323252,12.5042014951932));
#428791=CARTESIAN_POINT('Ctrl Pts',(-1.24259009191169,2.45337646637956,
12.4980716682127));
#428792=CARTESIAN_POINT('Ctrl Pts',(-1.23652925994931,2.45644108399838,
12.4907355092744));
#428793=CARTESIAN_POINT('Ctrl Pts',(-1.2397289763209,2.44436777113429,12.5218047446509));
#428794=CARTESIAN_POINT('Ctrl Pts',(-1.23752309502183,2.45597177728004,
12.5216906929434));
#428795=CARTESIAN_POINT('Ctrl Pts',(-1.22694519041112,2.46111752196638,
12.5161988840775));
#428796=CARTESIAN_POINT('Ctrl Pts',(-1.23922929903385,2.43920812879961,
12.5369868989719));
#428797=CARTESIAN_POINT('Ctrl Pts',(-1.24070716130095,2.45446661675355,
12.5369868989719));
#428798=CARTESIAN_POINT('Ctrl Pts',(-1.22690462214259,2.46113710731293,
12.5369868989719));
#428799=CARTESIAN_POINT('Origin',(-2.42277625004775E-31,-6.05232695006712E-32,
12.5));
#428800=CARTESIAN_POINT('Origin',(-1.42401639941741,2.27450380427704,12.5));
#428801=CARTESIAN_POINT('',(-1.42401639941741,2.27450380427704,12.5893111709658));
#428802=CARTESIAN_POINT('',(-1.42401639941741,2.27450380427704,13.8235269408515));
#428803=CARTESIAN_POINT('',(-1.42401639941741,2.27450380427704,12.5));
#428804=CARTESIAN_POINT('',(-1.43029328000177,2.30971564133975,13.7902182540695));
#428805=CARTESIAN_POINT('',(-1.42401639941741,2.27450380427704,13.8235269408515));
#428806=CARTESIAN_POINT('',(-1.43393074758918,2.33012098668408,13.7435492065112));
#428807=CARTESIAN_POINT('Origin',(-1.42196384800666,2.26298761305396,13.7445212918707));
#428808=CARTESIAN_POINT('',(-1.43393074758918,2.33012098668408,12.5369868989719));
#428809=CARTESIAN_POINT('',(-1.43393074758918,2.33012098668408,12.5));
#428810=CARTESIAN_POINT('Ctrl Pts',(-1.43393074758918,2.33012098668408,
12.5369868989719));
#428811=CARTESIAN_POINT('Ctrl Pts',(-1.43062837517278,2.31159544714511,
12.5544431401645));
#428812=CARTESIAN_POINT('Ctrl Pts',(-1.42732364081185,2.29305665764788,
12.5718848856037));
#428813=CARTESIAN_POINT('Ctrl Pts',(-1.42401639941741,2.27450380427704,
12.5893111709658));
#428814=CARTESIAN_POINT('Origin',(-1.70362197401988,2.39655971658016,12.5));
#428815=CARTESIAN_POINT('',(-1.52387624238132,2.27231652710908,13.7435492065112));
#428816=CARTESIAN_POINT('',(-1.50682594602498,2.26053108340798,13.7902182540695));
#428817=CARTESIAN_POINT('Origin',(-1.46202071408172,2.22956097429398,13.7418732680435));
#428818=CARTESIAN_POINT('',(-1.47740364284708,2.2401939062462,13.8235269408515));
#428819=CARTESIAN_POINT('',(-1.50682594602498,2.26053108340798,13.7902182540695));
#428820=CARTESIAN_POINT('',(-1.47740364284708,2.2401939062462,12.5893111709658));
#428821=CARTESIAN_POINT('',(-1.47740364284708,2.2401939062462,12.5));
#428822=CARTESIAN_POINT('',(-1.52387624238132,2.27231652710908,12.5369868989719));
#428823=CARTESIAN_POINT('Ctrl Pts',(-1.47740364284708,2.2401939062462,12.5893111709658));
#428824=CARTESIAN_POINT('Ctrl Pts',(-1.49290603415146,2.25090941265921,
12.5718848856037));
#428825=CARTESIAN_POINT('Ctrl Pts',(-1.50839667396577,2.26161679625009,
12.5544431401645));
#428826=CARTESIAN_POINT('Ctrl Pts',(-1.52387624238132,2.27231652710908,
12.5369868989719));
#428827=CARTESIAN_POINT('',(-1.52387624238132,2.27231652710908,12.5));
#428828=CARTESIAN_POINT('Origin',(-1.45785791655534,2.2684711976428,12.5));
#428829=CARTESIAN_POINT('',(-1.43834182256171,2.2401743383222,13.8587068136939));
#428830=CARTESIAN_POINT('Ctrl Pts',(-1.47740364285072,2.24019390624068,
13.8235269408542));
#428831=CARTESIAN_POINT('Ctrl Pts',(-1.47596218102064,2.23919754424846,
13.8262006681044));
#428832=CARTESIAN_POINT('Ctrl Pts',(-1.47438826675084,2.23832083340481,
13.8288634856214));
#428833=CARTESIAN_POINT('Ctrl Pts',(-1.47269271443384,2.23755597275063,
13.8314912288862));
#428834=CARTESIAN_POINT('Ctrl Pts',(-1.47094477488312,2.23676748030788,
13.8342001611531));
#428835=CARTESIAN_POINT('Ctrl Pts',(-1.46906582748899,2.2360965277137,13.8368750301949));
#428836=CARTESIAN_POINT('Ctrl Pts',(-1.46703304982142,2.23556356986172,
13.8394886372969));
#428837=CARTESIAN_POINT('Ctrl Pts',(-1.46687605347133,2.23552240823403,
13.8396904925131));
#428838=CARTESIAN_POINT('Ctrl Pts',(-1.46671813032281,2.23548208986005,
13.8398919674349));
#428839=CARTESIAN_POINT('Ctrl Pts',(-1.46655926602795,2.23544263494557,
13.8400930404591));
#428840=CARTESIAN_POINT('Ctrl Pts',(-1.46408405343539,2.23482790083391,
13.8432258934518));
#428841=CARTESIAN_POINT('Ctrl Pts',(-1.4613932720264,2.23442482231541,13.8462331177034));
#428842=CARTESIAN_POINT('Ctrl Pts',(-1.45856038943732,2.23434194746974,
13.8489036603661));
#428843=CARTESIAN_POINT('Ctrl Pts',(-1.45763343728625,2.23431482985578,
13.849777493004));
#428844=CARTESIAN_POINT('Ctrl Pts',(-1.45669147573778,2.23432213859897,
13.85061494757));
#428845=CARTESIAN_POINT('Ctrl Pts',(-1.45573767095083,2.23436807501136,
13.8514076489583));
#428846=CARTESIAN_POINT('Ctrl Pts',(-1.45372023626719,2.23446523714859,
13.8530843267192));
#428847=CARTESIAN_POINT('Ctrl Pts',(-1.45145179399437,2.23474771150499,
13.8546805203176));
#428848=CARTESIAN_POINT('Ctrl Pts',(-1.44908086418411,2.23533450335257,
13.8559412814274));
#428849=CARTESIAN_POINT('Ctrl Pts',(-1.44876355688443,2.23541303513189,
13.8561100121513));
#428850=CARTESIAN_POINT('Ctrl Pts',(-1.44844444817843,2.23549694881832,
13.8562727473908));
#428851=CARTESIAN_POINT('Ctrl Pts',(-1.4481239191472,2.23558645809077,13.8564289040185));
#428852=CARTESIAN_POINT('Ctrl Pts',(-1.44667032364727,2.2359923816202,13.8571370725437));
#428853=CARTESIAN_POINT('Ctrl Pts',(-1.44516257969674,2.23652271219574,
13.8577210840554));
#428854=CARTESIAN_POINT('Ctrl Pts',(-1.44366903155974,2.2371845211339,13.8581177131616));
#428855=CARTESIAN_POINT('Ctrl Pts',(-1.44324839699799,2.23737090930966,
13.8582294175695));
#428856=CARTESIAN_POINT('Ctrl Pts',(-1.4428288496737,2.23756755274473,13.8583265086086));
#428857=CARTESIAN_POINT('Ctrl Pts',(-1.44241179497967,2.2377741868936,13.8584082369006));
#428858=CARTESIAN_POINT('Ctrl Pts',(-1.44181259922199,2.23807106475438,
13.8585256585398));
#428859=CARTESIAN_POINT('Ctrl Pts',(-1.44121124288433,2.23839254605391,
13.8586122832068));
#428860=CARTESIAN_POINT('Ctrl Pts',(-1.44062371976203,2.23873097605759,
13.8586682984299));
#428861=CARTESIAN_POINT('Ctrl Pts',(-1.44015375950349,2.23900168651305,
13.8587131050557));
#428862=CARTESIAN_POINT('Ctrl Pts',(-1.43968734255476,2.23928602826641,
13.8587357943552));
#428863=CARTESIAN_POINT('Ctrl Pts',(-1.43922467711251,2.23958446753113,
13.8587355499465));
#428864=CARTESIAN_POINT('Ctrl Pts',(-1.43892564540677,2.23977735594301,
13.8587353919793));
#428865=CARTESIAN_POINT('Ctrl Pts',(-1.43863139356086,2.23997401500444,
13.8587257282814));
#428866=CARTESIAN_POINT('Ctrl Pts',(-1.43834182256171,2.2401743383222,13.8587068136939));
#428867=CARTESIAN_POINT('Ctrl Pts',(-1.43834182256171,2.2401743383222,13.8587068136939));
#428868=CARTESIAN_POINT('Ctrl Pts',(-1.43738943933149,2.24083319079368,
13.8586446046466));
#428869=CARTESIAN_POINT('Ctrl Pts',(-1.43648762652411,2.24153163169092,
13.858482427929));
#428870=CARTESIAN_POINT('Ctrl Pts',(-1.43563341106693,2.24226632233211,
13.8582284286032));
#428871=CARTESIAN_POINT('Ctrl Pts',(-1.43475708537432,2.24302002946721,
13.8579678548414));
#428872=CARTESIAN_POINT('Ctrl Pts',(-1.43392971103076,2.24381488951759,
13.857615680862));
#428873=CARTESIAN_POINT('Ctrl Pts',(-1.43317719369912,2.2446125781618,13.8571944833187));
#428874=CARTESIAN_POINT('Ctrl Pts',(-1.43129920973686,2.24660329175433,
13.8561433417727));
#428875=CARTESIAN_POINT('Ctrl Pts',(-1.42979610313547,2.24870145060258,
13.8546163505474));
#428876=CARTESIAN_POINT('Ctrl Pts',(-1.42862030029477,2.25070582195769,
13.8528973491086));
#428877=CARTESIAN_POINT('Ctrl Pts',(-1.42840549846313,2.25107199103252,
13.8525833129072));
#428878=CARTESIAN_POINT('Ctrl Pts',(-1.42820147888688,2.25143502294101,
13.8522628768812));
#428879=CARTESIAN_POINT('Ctrl Pts',(-1.42800777371376,2.25179370979477,
13.851937733538));
#428880=CARTESIAN_POINT('Ctrl Pts',(-1.42682484309684,2.25398416064518,
13.8499521282529));
#428881=CARTESIAN_POINT('Ctrl Pts',(-1.42591260266378,2.25623219558733,
13.847639871647));
#428882=CARTESIAN_POINT('Ctrl Pts',(-1.42524455161363,2.25838945692319,
13.8452109780794));
#428883=CARTESIAN_POINT('Ctrl Pts',(-1.4249439816182,2.25936005345129,13.8441181685877));
#428884=CARTESIAN_POINT('Ctrl Pts',(-1.42469212577678,2.26031231270079,
13.8430021611332));
#428885=CARTESIAN_POINT('Ctrl Pts',(-1.42448348263038,2.26123391141051,
13.8418824960098));
#428886=CARTESIAN_POINT('Ctrl Pts',(-1.42399180972801,2.26340568230381,
13.8392439765549));
#428887=CARTESIAN_POINT('Ctrl Pts',(-1.42371291313188,2.26551017341821,
13.8364981347964));
#428888=CARTESIAN_POINT('Ctrl Pts',(-1.42361213134105,2.2675484545724,13.8336931113419));
#428889=CARTESIAN_POINT('Ctrl Pts',(-1.42351397627701,2.26953361097376,
13.8309611966328));
#428890=CARTESIAN_POINT('Ctrl Pts',(-1.42358523779606,2.27145798093114,
13.8281701127186));
#428891=CARTESIAN_POINT('Ctrl Pts',(-1.42383116289706,2.27331008028712,
13.8253580685121));
#428892=CARTESIAN_POINT('Ctrl Pts',(-1.42388447972437,2.27371161742634,
13.8247484142933));
#428893=CARTESIAN_POINT('Ctrl Pts',(-1.42394613602456,2.27410964302014,
13.8241378483365));
#428894=CARTESIAN_POINT('Ctrl Pts',(-1.42401639941741,2.27450380427704,
13.8235269408515));
#428895=CARTESIAN_POINT('',(-1.43937685642172,2.23948769302342,12.5969504640361));
#428896=CARTESIAN_POINT('Origin',(-1.45787563915687,2.26849913672305,12.584524458991));
#428897=CARTESIAN_POINT('Origin',(-1.45787563915687,2.26849913672305,12.584524458991));
#428898=CARTESIAN_POINT('Ctrl Pts',(-1.47740364284708,2.2401939062462,12.5893111709658));
#428899=CARTESIAN_POINT('Ctrl Pts',(-1.46808019059305,2.23374938356206,
12.5770542771492));
#428900=CARTESIAN_POINT('Ctrl Pts',(-1.456428520403,2.24524034769207,12.5737548217797));
#428901=CARTESIAN_POINT('Ctrl Pts',(-1.49779090388309,2.25428591451033,
12.5663937883685));
#428902=CARTESIAN_POINT('Ctrl Pts',(-1.4884555582709,2.2478331709425,12.5540940315304));
#428903=CARTESIAN_POINT('Ctrl Pts',(-1.47677003674784,2.25936202960448,
12.5508374392248));
#428904=CARTESIAN_POINT('Ctrl Pts',(-1.51815759442263,2.26836370411087,
12.5434499600945));
#428905=CARTESIAN_POINT('Ctrl Pts',(-1.50879189627741,2.26188998037585,
12.5311293540533));
#428906=CARTESIAN_POINT('Ctrl Pts',(-1.49709235184912,2.273468945128,12.5278936106989));
#428907=CARTESIAN_POINT('Ctrl Pts',(-1.53850532578086,2.28242838881521,
12.5204817579905));
#428908=CARTESIAN_POINT('Ctrl Pts',(-1.52909327383041,2.27592262457185,
12.5081597038247));
#428909=CARTESIAN_POINT('Ctrl Pts',(-1.51739696600321,2.28756223058349,
12.5049254088044));
#428910=CARTESIAN_POINT('Ctrl Pts',(-1.52387624238132,2.27231652710908,
12.5369868989719));
#428911=CARTESIAN_POINT('Ctrl Pts',(-1.52464250941181,2.27284618360976,
12.5342545179733));
#428912=CARTESIAN_POINT('Ctrl Pts',(-1.52530286870771,2.27345428122829,
12.5314872231885));
#428913=CARTESIAN_POINT('Ctrl Pts',(-1.52578225400243,2.2741476864845,12.5287124745063));
#428914=CARTESIAN_POINT('Ctrl Pts',(-1.52621458745577,2.27477303376212,
12.5262100684184));
#428915=CARTESIAN_POINT('Ctrl Pts',(-1.52649848350549,2.27546769293803,
12.5237004536639));
#428916=CARTESIAN_POINT('Ctrl Pts',(-1.52657745297963,2.27626867008726,
12.5212220730815));
#428917=CARTESIAN_POINT('Ctrl Pts',(-1.5266379109435,2.27688188738504,12.5193246583486));
#428918=CARTESIAN_POINT('Ctrl Pts',(-1.52657834782572,2.27756481114221,
12.517417831369));
#428919=CARTESIAN_POINT('Ctrl Pts',(-1.52630213690367,2.27832827183539,
12.5155812248347));
#428920=CARTESIAN_POINT('Ctrl Pts',(-1.52618446956624,2.27865351019431,
12.5147988205793));
#428921=CARTESIAN_POINT('Ctrl Pts',(-1.52602762591022,2.27899378885114,
12.5140295443047));
#428922=CARTESIAN_POINT('Ctrl Pts',(-1.52582537986502,2.27935167052157,
12.5132817086137));
#428923=CARTESIAN_POINT('Ctrl Pts',(-1.52551930783482,2.27989327601663,
12.5121499604604));
#428924=CARTESIAN_POINT('Ctrl Pts',(-1.5250964162944,2.28048337419652,12.5110494206568));
#428925=CARTESIAN_POINT('Ctrl Pts',(-1.52452106434293,2.28111116575878,
12.5100666561695));
#428926=CARTESIAN_POINT('Ctrl Pts',(-1.52419069857732,2.28147164222815,
12.5095023550641));
#428927=CARTESIAN_POINT('Ctrl Pts',(-1.523805767863,2.28184827026828,12.5089719619137));
#428928=CARTESIAN_POINT('Ctrl Pts',(-1.52336902052781,2.28222942516089,
12.5085043804652));
#428929=CARTESIAN_POINT('Ctrl Pts',(-1.52272989769311,2.28278719569731,
12.5078201359221));
#428930=CARTESIAN_POINT('Ctrl Pts',(-1.52196048124246,2.28336992748646,
12.5072563000949));
#428931=CARTESIAN_POINT('Ctrl Pts',(-1.52110781489119,2.28393137105423,
12.5068768744332));
#428932=CARTESIAN_POINT('Ctrl Pts',(-1.52049298375417,2.2843362105165,12.5066032824114));
#428933=CARTESIAN_POINT('Ctrl Pts',(-1.51982409901167,2.28473714395477,
12.5064197834844));
#428934=CARTESIAN_POINT('Ctrl Pts',(-1.5191398418534,2.2851139992833,12.5063282718343));
#428935=CARTESIAN_POINT('Ctrl Pts',(-1.51814103824299,2.28566409139149,
12.5061946931565));
#428936=CARTESIAN_POINT('Ctrl Pts',(-1.51708864487265,2.28617556834506,
12.5062515701262));
#428937=CARTESIAN_POINT('Ctrl Pts',(-1.51605473500506,2.28663059582161,
12.5064436508398));
#428938=CARTESIAN_POINT('',(-1.456428520403,2.24524034769207,12.5737548217797));
#428939=CARTESIAN_POINT('Origin',(-1.46489437802037,2.25829137274002,12.5893111709658));
#428940=CARTESIAN_POINT('Ctrl Pts',(-1.51605473500506,2.28663059582161,
12.5064436508398));
#428941=CARTESIAN_POINT('Ctrl Pts',(-1.50722823215259,2.2805041584273,12.5164271754438));
#428942=CARTESIAN_POINT('Ctrl Pts',(-1.49839834961203,2.27437512087309,
12.5264061185523));
#428943=CARTESIAN_POINT('Ctrl Pts',(-1.48956496781393,2.26824339236108,
12.536380305637));
#428944=CARTESIAN_POINT('Ctrl Pts',(-1.47852503216917,2.2605799753696,12.5488460165097));
#428945=CARTESIAN_POINT('Ctrl Pts',(-1.46747962746124,2.25291235283713,
12.5613043021964));
#428946=CARTESIAN_POINT('Ctrl Pts',(-1.456428520403,2.24524034769207,12.5737548217797));
#428947=CARTESIAN_POINT('Ctrl Pts',(-1.42401639941741,2.27450380427703,
12.5893111709658));
#428948=CARTESIAN_POINT('Ctrl Pts',(-1.42202735742846,2.26334574232498,
12.5770542771492));
#428949=CARTESIAN_POINT('Ctrl Pts',(-1.43732018478208,2.25752052933426,
12.5737548217797));
#428950=CARTESIAN_POINT('Ctrl Pts',(-1.42216064054149,2.26409342952347,
12.5928319619712));
#428951=CARTESIAN_POINT('Ctrl Pts',(-1.42403106553985,2.25602280831461,
12.5821634970843));
#428952=CARTESIAN_POINT('Ctrl Pts',(-1.43663488437367,2.25372993825639,
12.5773203894503));
#428953=CARTESIAN_POINT('Ctrl Pts',(-1.42636713974644,2.24787956311911,
12.5969440695591));
#428954=CARTESIAN_POINT('Ctrl Pts',(-1.42973886988556,2.24569096118618,
12.5878292599214));
#428955=CARTESIAN_POINT('Ctrl Pts',(-1.43813614694107,2.247951499211,12.5813877129824));
#428956=CARTESIAN_POINT('Ctrl Pts',(-1.45207776459661,2.23129224822624,
12.596957478804));
#428957=CARTESIAN_POINT('Ctrl Pts',(-1.44873099609045,2.23346474303984,
12.5878468778671));
#428958=CARTESIAN_POINT('Ctrl Pts',(-1.44734156980188,2.2420196817612,12.5814011370086));
#428959=CARTESIAN_POINT('Ctrl Pts',(-1.468692312488,2.23417249222711,12.5928371701607));
#428960=CARTESIAN_POINT('Ctrl Pts',(-1.46057862796719,2.2325283543982,12.5821692192952));
#428961=CARTESIAN_POINT('Ctrl Pts',(-1.45325518967119,2.24303507003596,
12.5773318885715));
#428962=CARTESIAN_POINT('Ctrl Pts',(-1.47740364284711,2.24019390624615,
12.5893111709658));
#428963=CARTESIAN_POINT('Ctrl Pts',(-1.46808019059308,2.23374938356201,
12.5770542771492));
#428964=CARTESIAN_POINT('Ctrl Pts',(-1.45642852040303,2.24524034769202,
12.5737548217797));
#428965=CARTESIAN_POINT('',(-1.43732018478208,2.25752052933426,12.5737548217797));
#428966=CARTESIAN_POINT('Origin',(-1.44567497038569,2.27064293603112,12.5893111709658));
#428967=CARTESIAN_POINT('Ctrl Pts',(-1.45642852040303,2.24524034769202,
12.5737548217797));
#428968=CARTESIAN_POINT('Ctrl Pts',(-1.45562315745449,2.24464393327892,
12.5746934679442));
#428969=CARTESIAN_POINT('Ctrl Pts',(-1.45462295118129,2.24413117324802,
12.5756680099006));
#428970=CARTESIAN_POINT('Ctrl Pts',(-1.45354321579869,2.24375744183171,
12.5765688348656));
#428971=CARTESIAN_POINT('Ctrl Pts',(-1.45325736780921,2.24365850057658,
12.5768073183026));
#428972=CARTESIAN_POINT('Ctrl Pts',(-1.45296608657162,2.24356908821268,
12.5770407398754));
#428973=CARTESIAN_POINT('Ctrl Pts',(-1.45267169156365,2.24348969852705,
12.5772674179684));
#428974=CARTESIAN_POINT('Ctrl Pts',(-1.45146357405869,2.24316390472514,
12.5781976435658));
#428975=CARTESIAN_POINT('Ctrl Pts',(-1.45013146371807,2.24299928539706,
12.5790594849312));
#428976=CARTESIAN_POINT('Ctrl Pts',(-1.44875938430905,2.24305488053192,
12.5797571720116));
#428977=CARTESIAN_POINT('Ctrl Pts',(-1.44786542523849,2.2430911027613,12.580211740231));
#428978=CARTESIAN_POINT('Ctrl Pts',(-1.44691463348036,2.24324120943337,
12.5806009430798));
#428979=CARTESIAN_POINT('Ctrl Pts',(-1.44597670345157,2.24351213363939,
12.5808812374708));
#428980=CARTESIAN_POINT('Ctrl Pts',(-1.44517071040179,2.24374494741053,
12.5811221033394));
#428981=CARTESIAN_POINT('Ctrl Pts',(-1.4443577459554,2.24407185498403,12.581287365893));
#428982=CARTESIAN_POINT('Ctrl Pts',(-1.44358680590368,2.24448214112821,
12.581359338449));
#428983=CARTESIAN_POINT('Ctrl Pts',(-1.44347966115579,2.24453916243017,
12.5813693411482));
#428984=CARTESIAN_POINT('Ctrl Pts',(-1.44337328398079,2.24459775375031,
12.5813775999465));
#428985=CARTESIAN_POINT('Ctrl Pts',(-1.44326775995774,2.24465784568193,
12.5813841266931));
#428986=CARTESIAN_POINT('Ctrl Pts',(-1.44308872568978,2.24475979891188,
12.5813952001081));
#428987=CARTESIAN_POINT('Ctrl Pts',(-1.44291124945329,2.24486728361588,
12.5814007534795));
#428988=CARTESIAN_POINT('Ctrl Pts',(-1.44273551070586,2.2449804216665,12.5814005856065));
#428989=CARTESIAN_POINT('Ctrl Pts',(-1.44193104742953,2.24549832342815,
12.5813998171494));
#428990=CARTESIAN_POINT('Ctrl Pts',(-1.44121839191735,2.24609862145549,
12.58127954464));
#428991=CARTESIAN_POINT('Ctrl Pts',(-1.44058252749522,2.24675527703021,
12.5810700125799));
#428992=CARTESIAN_POINT('Ctrl Pts',(-1.43981447567226,2.24754844219824,
12.5808169217085));
#428993=CARTESIAN_POINT('Ctrl Pts',(-1.43917041471568,2.2484355463881,12.5804173076348));
#428994=CARTESIAN_POINT('Ctrl Pts',(-1.43868571515248,2.24932354509367,
12.5799304713245));
#428995=CARTESIAN_POINT('Ctrl Pts',(-1.43808501969756,2.2504240552383,12.5793271277669));
#428996=CARTESIAN_POINT('Ctrl Pts',(-1.43766356143134,2.25157877846844,
12.5785808224116));
#428997=CARTESIAN_POINT('Ctrl Pts',(-1.43740931127446,2.25272816644503,
12.5777485681082));
#428998=CARTESIAN_POINT('Ctrl Pts',(-1.43703045068553,2.25444088045501,
12.576508418016));
#428999=CARTESIAN_POINT('Ctrl Pts',(-1.43701934343463,2.25612584221711,
12.5750928681475));
#429000=CARTESIAN_POINT('Ctrl Pts',(-1.43732018478208,2.25752052933426,
12.5737548217797));
#429001=CARTESIAN_POINT('Ctrl Pts',(-1.43732018478208,2.25752052933426,
12.5737548217797));
#429002=CARTESIAN_POINT('Ctrl Pts',(-1.42202735742846,2.26334574232498,
12.5770542771492));
#429003=CARTESIAN_POINT('Ctrl Pts',(-1.42401639941741,2.27450380427704,
12.5893111709658));
#429004=CARTESIAN_POINT('Ctrl Pts',(-1.44171488686745,2.28188652095685,
12.5508408821982));
#429005=CARTESIAN_POINT('Ctrl Pts',(-1.42637353378435,2.2877267786745,12.55409748406));
#429006=CARTESIAN_POINT('Ctrl Pts',(-1.42836511328145,2.2988990754559,12.5663972313419));
#429007=CARTESIAN_POINT('Ctrl Pts',(-1.44610413509887,2.30622891943672,
12.52790050457));
#429008=CARTESIAN_POINT('Ctrl Pts',(-1.43071138617805,2.31206111953635,
12.5311362602938));
#429009=CARTESIAN_POINT('Ctrl Pts',(-1.43270944000778,2.32326973581482,
12.5434568539655));
#429010=CARTESIAN_POINT('Ctrl Pts',(-1.45048833968264,2.33054956072195,
12.5049357605811));
#429011=CARTESIAN_POINT('Ctrl Pts',(-1.43504178234001,2.33635363267623,
12.5081700652078));
#429012=CARTESIAN_POINT('Ctrl Pts',(-1.43704972319792,2.3476177128782,12.5204921097672));
#429013=CARTESIAN_POINT('Ctrl Pts',(-1.45020045406216,2.32895257236274,
12.5064436508395));
#429014=CARTESIAN_POINT('Ctrl Pts',(-1.44928941955832,2.32976427669525,
12.5062361689309));
#429015=CARTESIAN_POINT('Ctrl Pts',(-1.44830740535102,2.33056953424231,
12.5061871075062));
#429016=CARTESIAN_POINT('Ctrl Pts',(-1.44731457636726,2.33129431507133,
12.5063648335164));
#429017=CARTESIAN_POINT('Ctrl Pts',(-1.4468635722026,2.3316235552302,12.5064455676329));
#429018=CARTESIAN_POINT('Ctrl Pts',(-1.44640391589726,2.33194060299416,
12.506574497099));
#429019=CARTESIAN_POINT('Ctrl Pts',(-1.44595471942102,2.33223099918938,
12.5067492519495));
#429020=CARTESIAN_POINT('Ctrl Pts',(-1.44505204166545,2.33281456161607,
12.5071004286051));
#429021=CARTESIAN_POINT('Ctrl Pts',(-1.44415797626474,2.33331127524723,
12.5076537929613));
#429022=CARTESIAN_POINT('Ctrl Pts',(-1.44334422101941,2.33369212724876,
12.5083435010505));
#429023=CARTESIAN_POINT('Ctrl Pts',(-1.44329299026369,2.33371610415824,
12.5083869222964));
#429024=CARTESIAN_POINT('Ctrl Pts',(-1.44324206716773,2.33373961366055,
12.5084308732337));
#429025=CARTESIAN_POINT('Ctrl Pts',(-1.44319146504562,2.33376264549273,
12.5084753333615));
#429026=CARTESIAN_POINT('Ctrl Pts',(-1.4427855692375,2.33394739118608,12.5088319622689));
#429027=CARTESIAN_POINT('Ctrl Pts',(-1.44239261947182,2.33410632765318,
12.509227847131));
#429028=CARTESIAN_POINT('Ctrl Pts',(-1.44202535010225,2.33423732464801,
12.5096423454524));
#429029=CARTESIAN_POINT('Ctrl Pts',(-1.44087449044466,2.33464781125296,
12.5109411997424));
#429030=CARTESIAN_POINT('Ctrl Pts',(-1.43990825419202,2.3348183093285,12.5124831113042));
#429031=CARTESIAN_POINT('Ctrl Pts',(-1.43910425539677,2.33484076846274,
12.5140723025008));
#429032=CARTESIAN_POINT('Ctrl Pts',(-1.43902891982906,2.33484287290822,
12.5142212114565));
#429033=CARTESIAN_POINT('Ctrl Pts',(-1.43895499201914,2.33484370205625,
12.5143705582413));
#429034=CARTESIAN_POINT('Ctrl Pts',(-1.4388824453064,2.33484334639968,12.5145201959299));
#429035=CARTESIAN_POINT('Ctrl Pts',(-1.43795047477045,2.33483877746143,
12.5164425148273));
#429036=CARTESIAN_POINT('Ctrl Pts',(-1.437214444496,2.33464925908648,12.518463520594));
#429037=CARTESIAN_POINT('Ctrl Pts',(-1.4366105440909,2.33433855813458,12.5205025929157));
#429038=CARTESIAN_POINT('Ctrl Pts',(-1.43626025791957,2.33415833926744,
12.5216853356836));
#429039=CARTESIAN_POINT('Ctrl Pts',(-1.43595483784785,2.33393810454189,
12.5228750347131));
#429040=CARTESIAN_POINT('Ctrl Pts',(-1.43568625407533,2.33369423858345,
12.5240609649613));
#429041=CARTESIAN_POINT('Ctrl Pts',(-1.43502702961469,2.3330956826714,12.5269717671326));
#429042=CARTESIAN_POINT('Ctrl Pts',(-1.43457815328594,2.33233022265961,
12.5299036066169));
#429043=CARTESIAN_POINT('Ctrl Pts',(-1.43427289327788,2.33145314315715,
12.5328133004019));
#429044=CARTESIAN_POINT('Ctrl Pts',(-1.43412635069925,2.33103209392516,
12.5342101228451));
#429045=CARTESIAN_POINT('Ctrl Pts',(-1.43401358315011,2.33058567440663,
12.5356023438238));
#429046=CARTESIAN_POINT('Ctrl Pts',(-1.43393074758918,2.33012098668408,
12.5369868989719));
#429047=CARTESIAN_POINT('Origin',(-3.66550788035654,14.8789346212549,-1.24043609528171));
#429048=CARTESIAN_POINT('Ctrl Pts',(-1.52384188449782,2.27229273011825,
12.5369868989719));
#429049=CARTESIAN_POINT('Ctrl Pts',(-1.53644329648318,2.28103845591202,
12.5369868989719));
#429050=CARTESIAN_POINT('Ctrl Pts',(-1.54900690180321,2.27223850562538,
12.5369868989719));
#429051=CARTESIAN_POINT('Ctrl Pts',(-1.52810169233888,2.27524907308474,
12.5218025310015));
#429052=CARTESIAN_POINT('Ctrl Pts',(-1.53931103355524,2.27899160340515,
12.5216901060417));
#429053=CARTESIAN_POINT('Ctrl Pts',(-1.54896861323185,2.27226534429804,
12.5161920673678));
#429054=CARTESIAN_POINT('Ctrl Pts',(-1.52819884569036,2.28127623099051,
12.5042015548895));
#429055=CARTESIAN_POINT('Ctrl Pts',(-1.53457254172868,2.28214418480728,
12.4980677368514));
#429056=CARTESIAN_POINT('Ctrl Pts',(-1.54020902936817,2.27834671369962,
12.4907278922777));
#429057=CARTESIAN_POINT('Ctrl Pts',(-1.51604368264968,2.28661392582627,
12.506463626192));
#429058=CARTESIAN_POINT('Ctrl Pts',(-1.51965911813721,2.29206700427535,
12.4999376786891));
#429059=CARTESIAN_POINT('Ctrl Pts',(-1.51961496084956,2.29200040285086,
12.4906970594712));
#429060=CARTESIAN_POINT('Origin',(-1.53638550720804,2.25421906061525,12.5369868989719));
#429061=CARTESIAN_POINT('Origin',(-1.53638550720804,2.25421906061525,14.));
#429062=CARTESIAN_POINT('Origin',(-1.53638550720804,2.25421906061525,13.7435492065112));
#429063=CARTESIAN_POINT('Ctrl Pts',(-1.50350829636126,2.25823783669342,
13.793642941384));
#429064=CARTESIAN_POINT('Ctrl Pts',(-1.51238713342879,2.26440812609782,
13.8071662555867));
#429065=CARTESIAN_POINT('Ctrl Pts',(-1.52405613480702,2.25200434480059,
13.8103758687955));
#429066=CARTESIAN_POINT('Ctrl Pts',(-1.51718103118014,2.26768865823418,
13.7804579775006));
#429067=CARTESIAN_POINT('Ctrl Pts',(-1.52814250067577,2.27529391025014,
13.7901904343351));
#429068=CARTESIAN_POINT('Ctrl Pts',(-1.54065318246692,2.26571587468511,
13.7927914348262));
#429069=CARTESIAN_POINT('Ctrl Pts',(-1.52523068475255,2.27325271251839,
13.7597120340895));
#429070=CARTESIAN_POINT('Ctrl Pts',(-1.53791945851365,2.28204942272231,
13.7635825532445));
#429071=CARTESIAN_POINT('Ctrl Pts',(-1.5504567233599,2.27378184107353,13.7651073818884));
#429072=CARTESIAN_POINT('Ctrl Pts',(-1.52365437826742,2.27216314328652,
13.7381884353898));
#429073=CARTESIAN_POINT('Ctrl Pts',(-1.53604563553464,2.28075468877985,
13.7368803041982));
#429074=CARTESIAN_POINT('Ctrl Pts',(-1.54853721275351,2.27220190351982,
13.7363986145813));
#429075=CARTESIAN_POINT('Origin',(-1.5193352108517,2.24243361691415,13.7902182540695));
#429076=CARTESIAN_POINT('Ctrl Pts',(-1.47740040531412,2.24019166748788,
13.8235227101244));
#429077=CARTESIAN_POINT('Ctrl Pts',(-1.48685551529785,2.24673258359459,
13.8358800583119));
#429078=CARTESIAN_POINT('Ctrl Pts',(-1.49857626599684,2.2350172068568,13.8390832900376));
#429079=CARTESIAN_POINT('Ctrl Pts',(-1.48721217657602,2.24697372425544,
13.8124254819053));
#429080=CARTESIAN_POINT('Ctrl Pts',(-1.49668564840759,2.25352734249975,
13.8247886449157));
#429081=CARTESIAN_POINT('Ctrl Pts',(-1.50840915940017,2.24178510799739,
13.8279860620657));
#429082=CARTESIAN_POINT('Ctrl Pts',(-1.49701955052126,2.25375274152581,
13.8013225099955));
#429083=CARTESIAN_POINT('Ctrl Pts',(-1.50650691310271,2.26031597130091,
13.8136962257787));
#429084=CARTESIAN_POINT('Ctrl Pts',(-1.51823734697624,2.24855009921166,
13.8168830918626));
#429085=CARTESIAN_POINT('Ctrl Pts',(-1.50682269824265,2.26052883756116,
13.7902140179785));
#429086=CARTESIAN_POINT('Ctrl Pts',(-1.51631977269687,2.26709879025167,
13.802602731458));
#429087=CARTESIAN_POINT('Ctrl Pts',(-1.52806101258505,2.2553122963536,13.8057746032558));
#429088=CARTESIAN_POINT('Origin',(-1.4899129076738,2.22209643975238,13.8235269408515));
#429089=CARTESIAN_POINT('Ctrl Pts',(-1.42401639941741,2.27450380427704,
13.8235269408515));
#429090=CARTESIAN_POINT('Ctrl Pts',(-1.42608854170343,2.28612803952662,
13.8362179249168));
#429091=CARTESIAN_POINT('Ctrl Pts',(-1.40998158197101,2.29180508561024,
13.8391868794938));
#429092=CARTESIAN_POINT('Ctrl Pts',(-1.42212047942069,2.2638681349965,13.8400110824519));
#429093=CARTESIAN_POINT('Ctrl Pts',(-1.42041392403934,2.27378829283754,
13.8494522556836));
#429094=CARTESIAN_POINT('Ctrl Pts',(-1.406972046088,2.27428205854887,13.85569149686));
#429095=CARTESIAN_POINT('Ctrl Pts',(-1.42607750140433,2.24806498015116,
13.8586819406588));
#429096=CARTESIAN_POINT('Ctrl Pts',(-1.42242234445147,2.25043053955327,
13.868010383617));
#429097=CARTESIAN_POINT('Ctrl Pts',(-1.41368240857793,2.24808397020224,
13.8744918421245));
#429098=CARTESIAN_POINT('Ctrl Pts',(-1.45237188500218,2.23110393981881,
13.8587686893867));
#429099=CARTESIAN_POINT('Ctrl Pts',(-1.45599448049846,2.22875938660122,
13.8680909899357));
#429100=CARTESIAN_POINT('Ctrl Pts',(-1.45745623020193,2.21985098105868,
13.8745789365163));
#429101=CARTESIAN_POINT('Ctrl Pts',(-1.46850223022654,2.23404110425126,
13.8400379222776));
#429102=CARTESIAN_POINT('Ctrl Pts',(-1.47823419615212,2.23660217299914,
13.8494748685453));
#429103=CARTESIAN_POINT('Ctrl Pts',(-1.48426552404467,2.22458617578222,
13.8557104837033));
#429104=CARTESIAN_POINT('Ctrl Pts',(-1.47740364285072,2.24019390624068,
13.8235269408542));
#429105=CARTESIAN_POINT('Ctrl Pts',(-1.48711662014059,2.24690767500026,
13.8362179249195));
#429106=CARTESIAN_POINT('Ctrl Pts',(-1.49897171578396,2.23461459925239,
13.8391868794965));
#429107=CARTESIAN_POINT('Origin',(-1.40235782844914,2.27836467252295,13.8235269408515));
#429108=CARTESIAN_POINT('Ctrl Pts',(-1.43029258730001,2.30971175977477,
13.7902140241683));
#429109=CARTESIAN_POINT('Ctrl Pts',(-1.43232359194615,2.32107985616422,
13.8026027327198));
#429110=CARTESIAN_POINT('Ctrl Pts',(-1.41672473886905,2.32686377481444,
13.8057746032556));
#429111=CARTESIAN_POINT('Ctrl Pts',(-1.4282012082801,2.29797961092568,13.8013225161808));
#429112=CARTESIAN_POINT('Ctrl Pts',(-1.43023013201747,2.30933608028693,
13.8136962270464));
#429113=CARTESIAN_POINT('Ctrl Pts',(-1.41465452616637,2.3151187360509,13.8168830918628));
#429114=CARTESIAN_POINT('Ctrl Pts',(-1.4261089276479,2.28624240424164,13.8124254880875));
#429115=CARTESIAN_POINT('Ctrl Pts',(-1.42813487886878,2.29758224536448,
13.8247886461867));
#429116=CARTESIAN_POINT('Ctrl Pts',(-1.41258365037936,2.30336842326249,
13.8279860620656));
#429117=CARTESIAN_POINT('Ctrl Pts',(-1.4240157089026,2.27449993496174,13.8235227163066));
#429118=CARTESIAN_POINT('Ctrl Pts',(-1.42603773365429,2.28581779691267,
13.8358800595848));
#429119=CARTESIAN_POINT('Ctrl Pts',(-1.41051208250144,2.29161262107548,
13.8390832900376));
#429120=CARTESIAN_POINT('Origin',(-1.4086347090335,2.31357650958566,13.7902182540695));
#429121=CARTESIAN_POINT('Ctrl Pts',(-1.43388336163615,2.32985531971413,
13.7382347919292));
#429122=CARTESIAN_POINT('Ctrl Pts',(-1.43655524756991,2.34470721839042,
13.7369371795942));
#429123=CARTESIAN_POINT('Ctrl Pts',(-1.42357188278845,2.35251593249532,
13.7364597369711));
#429124=CARTESIAN_POINT('Ctrl Pts',(-1.43421531924036,2.33171752220937,
13.7595490285574));
#429125=CARTESIAN_POINT('Ctrl Pts',(-1.43694996454301,2.34692395247711,
13.7633824266926));
#429126=CARTESIAN_POINT('Ctrl Pts',(-1.42420417574629,2.35488878318828,
13.7648920890506));
#429127=CARTESIAN_POINT('Ctrl Pts',(-1.43252235365287,2.32222039150202,
13.780380659011));
#429128=CARTESIAN_POINT('Ctrl Pts',(-1.43489303718528,2.3353724539104,13.7901039518744));
#429129=CARTESIAN_POINT('Ctrl Pts',(-1.42098426477899,2.34279077525527,
13.7926933640891));
#429130=CARTESIAN_POINT('Ctrl Pts',(-1.42957960146849,2.30571225832004,
13.7936647693663));
#429131=CARTESIAN_POINT('Ctrl Pts',(-1.43150714431042,2.31635452830992,
13.8072068914933));
#429132=CARTESIAN_POINT('Ctrl Pts',(-1.41535603912925,2.32181219001387,
13.8104111085397));
#429133=CARTESIAN_POINT('Origin',(-1.41227217662091,2.33398185492999,13.7435492065112));
#429134=CARTESIAN_POINT('Origin',(-1.41227217662091,2.33398185492999,14.));
#429135=CARTESIAN_POINT('Origin',(-1.41227217662091,2.33398185492999,12.5369868989719));
#429136=CARTESIAN_POINT('Ctrl Pts',(-1.45019073698299,2.32893696717882,
12.506462012331));
#429137=CARTESIAN_POINT('Ctrl Pts',(-1.45364694947951,2.33448747915239,
12.4999388158272));
#429138=CARTESIAN_POINT('Ctrl Pts',(-1.45360605795313,2.33442180931669,
12.4907030323752));
#429139=CARTESIAN_POINT('Ctrl Pts',(-1.44028491574729,2.33777457368743,
12.5042014951932));
#429140=CARTESIAN_POINT('Ctrl Pts',(-1.43842843393313,2.34393043044257,
12.4980716682127));
#429141=CARTESIAN_POINT('Ctrl Pts',(-1.4326375636756,2.34747886487005,12.4907355092743));
#429142=CARTESIAN_POINT('Ctrl Pts',(-1.43484254617332,2.33518491836954,
12.5218047446509));
#429143=CARTESIAN_POINT('Ctrl Pts',(-1.43358983898951,2.34693011294637,
12.5216906929434));
#429144=CARTESIAN_POINT('Ctrl Pts',(-1.42346655744649,2.35292093301802,
12.5161988840776));
#429145=CARTESIAN_POINT('Ctrl Pts',(-1.43392397277117,2.33008317265677,
12.5369868989719));
#429146=CARTESIAN_POINT('Ctrl Pts',(-1.43664062599462,2.34517042975619,
12.5369868989719));
#429147=CARTESIAN_POINT('Ctrl Pts',(-1.42342772055309,2.35294375988644,
12.5369868989719));
#429148=CARTESIAN_POINT('Origin',(-2.78530720815108E-31,-8.17839987285357E-32,
12.5));
#429149=CARTESIAN_POINT('Origin',(-1.60467127783313,2.15086502402588,12.5));
#429150=CARTESIAN_POINT('',(-1.60467127783313,2.15086502402588,12.5893111709658));
#429151=CARTESIAN_POINT('',(-1.60467127783313,2.15086502402588,13.8235269408515));
#429152=CARTESIAN_POINT('',(-1.60467127783313,2.15086502402588,12.5));
#429153=CARTESIAN_POINT('',(-1.6137973642265,2.1854480725662,13.7902182540695));
#429154=CARTESIAN_POINT('',(-1.60467127783313,2.15086502402588,13.8235269408515));
#429155=CARTESIAN_POINT('',(-1.61908595352014,2.20548903343024,13.7435492065112));
#429156=CARTESIAN_POINT('Origin',(-1.60168687962198,2.13955445397357,13.7445212918705));
#429157=CARTESIAN_POINT('',(-1.61908595352014,2.20548903343024,12.5369868989719));
#429158=CARTESIAN_POINT('',(-1.61908595352014,2.20548903343024,12.5));
#429159=CARTESIAN_POINT('Ctrl Pts',(-1.61908595352014,2.20548903343024,
12.5369868989719));
#429160=CARTESIAN_POINT('Ctrl Pts',(-1.61428456602037,2.1872943101055,12.5544431401645));
#429161=CARTESIAN_POINT('Ctrl Pts',(-1.60947974444066,2.16908657343106,
12.5718848856037));
#429162=CARTESIAN_POINT('Ctrl Pts',(-1.60467127783313,2.15086502402588,
12.5893111709658));
#429163=CARTESIAN_POINT('Origin',(-1.89329517791645,2.2497243552881,12.5));
#429164=CARTESIAN_POINT('',(-1.70402056201255,2.14054552058715,13.7435492065112));
#429165=CARTESIAN_POINT('',(-1.68606637603842,2.130189049418,13.7902182540695));
#429166=CARTESIAN_POINT('Origin',(-1.63888587840916,2.10297403314562,13.7418732680461));
#429167=CARTESIAN_POINT('',(-1.65508430440736,2.11231773338787,13.8235269408515));
#429168=CARTESIAN_POINT('',(-1.68606637603842,2.130189049418,13.7902182540695));
#429169=CARTESIAN_POINT('',(-1.65508430440736,2.11231773338787,12.5893111709658));
#429170=CARTESIAN_POINT('',(-1.65508430440736,2.11231773338787,12.5));
#429171=CARTESIAN_POINT('',(-1.70402056201255,2.14054552058715,12.5369868989719));
#429172=CARTESIAN_POINT('Ctrl Pts',(-1.65508430440736,2.11231773338787,
12.5893111709658));
#429173=CARTESIAN_POINT('Ctrl Pts',(-1.67140852603409,2.12173399602877,
12.5718848856037));
#429174=CARTESIAN_POINT('Ctrl Pts',(-1.68772037318746,2.1311431207311,12.5544431401645));
#429175=CARTESIAN_POINT('Ctrl Pts',(-1.70402056201255,2.14054552058715,
12.5369868989719));
#429176=CARTESIAN_POINT('',(-1.70402056201255,2.14054552058715,12.5));
#429177=CARTESIAN_POINT('Origin',(-1.63790847666983,2.1420940925765,12.5));
#429178=CARTESIAN_POINT('',(-1.61615086413916,2.11548213156001,13.8587068136939));
#429179=CARTESIAN_POINT('Ctrl Pts',(-1.65508430441053,2.11231773338207,
13.8235269408542));
#429180=CARTESIAN_POINT('Ctrl Pts',(-1.65356642617364,2.11144217922321,
13.8262006681044));
#429181=CARTESIAN_POINT('Ctrl Pts',(-1.65192628890099,2.11069667418707,
13.8288634856214));
#429182=CARTESIAN_POINT('Ctrl Pts',(-1.65017403515052,2.11007256179819,
13.8314912288862));
#429183=CARTESIAN_POINT('Ctrl Pts',(-1.64836764227037,2.10942916629946,
13.8342001611531));
#429184=CARTESIAN_POINT('Ctrl Pts',(-1.64644025805345,2.10891359790061,
13.8368750301949));
#429185=CARTESIAN_POINT('Ctrl Pts',(-1.6443708032732,2.10854810367321,13.8394886372969));
#429186=CARTESIAN_POINT('Ctrl Pts',(-1.64421097426073,2.10851987566746,
13.8396904925131));
#429187=CARTESIAN_POINT('Ctrl Pts',(-1.64405029026668,2.10849256365223,
13.8398919674349));
#429188=CARTESIAN_POINT('Ctrl Pts',(-1.64388873863784,2.10846618893557,
13.8400930404591));
#429189=CARTESIAN_POINT('Ctrl Pts',(-1.64137165557397,2.108055253106,13.8432258934518));
#429190=CARTESIAN_POINT('Ctrl Pts',(-1.6386569728769,2.10787283946285,13.8462331177034));
#429191=CARTESIAN_POINT('Ctrl Pts',(-1.63582676140163,2.10802114660661,
13.8489036603661));
#429192=CARTESIAN_POINT('Ctrl Pts',(-1.6349006832701,2.10806967442998,13.8497774930041));
#429193=CARTESIAN_POINT('Ctrl Pts',(-1.63396245175139,2.10815373746488,
13.85061494757));
#429194=CARTESIAN_POINT('Ctrl Pts',(-1.63301556491525,2.10827726497248,
13.8514076489583));
#429195=CARTESIAN_POINT('Ctrl Pts',(-1.63101276269529,2.10853854346638,
13.8530843267192));
#429196=CARTESIAN_POINT('Ctrl Pts',(-1.62877489275942,2.10900497701708,
13.8546805203176));
#429197=CARTESIAN_POINT('Ctrl Pts',(-1.6264596810056,2.10978306915337,13.8559412814273));
#429198=CARTESIAN_POINT('Ctrl Pts',(-1.62614983058885,2.10988720311533,
13.8561100121513));
#429199=CARTESIAN_POINT('Ctrl Pts',(-1.6258386234352,2.1099968479079,13.8562727473908));
#429200=CARTESIAN_POINT('Ctrl Pts',(-1.62552645677455,2.11011218543732,
13.8564289040185));
#429201=CARTESIAN_POINT('Ctrl Pts',(-1.6241107845298,2.11063523981746,13.8571370725437));
#429202=CARTESIAN_POINT('Ctrl Pts',(-1.62265128433814,2.11128670089093,
13.8577210840553));
#429203=CARTESIAN_POINT('Ctrl Pts',(-1.62121664943176,2.11206804575303,
13.8581177131616));
#429204=CARTESIAN_POINT('Ctrl Pts',(-1.62081260686348,2.11228809935928,
13.8582294175695));
#429205=CARTESIAN_POINT('Ctrl Pts',(-1.6204104838138,2.11251828548136,13.8583265086086));
#429206=CARTESIAN_POINT('Ctrl Pts',(-1.62001165943628,2.11275822590146,
13.8584082369006));
#429207=CARTESIAN_POINT('Ctrl Pts',(-1.61943865575479,2.11310295594257,
13.8585256585398));
#429208=CARTESIAN_POINT('Ctrl Pts',(-1.61886550409113,2.11347238366383,
13.8586122832068));
#429209=CARTESIAN_POINT('Ctrl Pts',(-1.61830752109069,2.11385757615836,
13.8586682984299));
#429210=CARTESIAN_POINT('Ctrl Pts',(-1.61786119000141,2.11416569197108,
13.8587131050557));
#429211=CARTESIAN_POINT('Ctrl Pts',(-1.6174195015092,2.11448710491203,13.8587357943552));
#429212=CARTESIAN_POINT('Ctrl Pts',(-1.61698270111869,2.11482226267343,
13.8587355499465));
#429213=CARTESIAN_POINT('Ctrl Pts',(-1.61670038661254,2.11503888312512,
13.8587353919793));
#429214=CARTESIAN_POINT('Ctrl Pts',(-1.61642314340459,2.11525887207689,
13.8587257282814));
#429215=CARTESIAN_POINT('Ctrl Pts',(-1.61615086413916,2.11548213156001,
13.8587068136939));
#429216=CARTESIAN_POINT('Ctrl Pts',(-1.61615086413916,2.11548213156001,
13.8587068136939));
#429217=CARTESIAN_POINT('Ctrl Pts',(-1.61525535247848,2.11621641982901,
13.8586446046466));
#429218=CARTESIAN_POINT('Ctrl Pts',(-1.61441346979595,2.11698604283761,
13.858482427929));
#429219=CARTESIAN_POINT('Ctrl Pts',(-1.61362198077802,2.11778791534621,
13.8582284286032));
#429220=CARTESIAN_POINT('Ctrl Pts',(-1.61281000511545,2.11861054326235,
13.8579678548414));
#429221=CARTESIAN_POINT('Ctrl Pts',(-1.61205017226499,2.11947019717145,
13.857615680862));
#429222=CARTESIAN_POINT('Ctrl Pts',(-1.61136517790258,2.12032656872106,
13.8571944833187));
#429223=CARTESIAN_POINT('Ctrl Pts',(-1.6096557044157,2.12246373150562,13.8561433417727));
#429224=CARTESIAN_POINT('Ctrl Pts',(-1.60832861870202,2.12467742604556,
13.8546163505474));
#429225=CARTESIAN_POINT('Ctrl Pts',(-1.60732010312139,2.12677096686748,
13.8528973491086));
#429226=CARTESIAN_POINT('Ctrl Pts',(-1.60713586220407,2.12715342588832,
13.8525833129072));
#429227=CARTESIAN_POINT('Ctrl Pts',(-1.6069621119569,2.12753187932757,13.8522628768811));
#429228=CARTESIAN_POINT('Ctrl Pts',(-1.60679828763023,2.12790516145029,
13.851937733538));
#429229=CARTESIAN_POINT('Ctrl Pts',(-1.60579783519682,2.13018474358327,
13.8499521282529));
#429230=CARTESIAN_POINT('Ctrl Pts',(-1.60507186588607,2.13249965443872,
13.847639871647));
#429231=CARTESIAN_POINT('Ctrl Pts',(-1.60458187454659,2.13470419002792,
13.8452109780794));
#429232=CARTESIAN_POINT('Ctrl Pts',(-1.60436141730064,2.13569605622112,
13.8441181685877));
#429233=CARTESIAN_POINT('Ctrl Pts',(-1.60418801745794,2.13666567549571,
13.8430021611332));
#429234=CARTESIAN_POINT('Ctrl Pts',(-1.60405518740495,2.13760121401513,
13.8418824960098));
#429235=CARTESIAN_POINT('Ctrl Pts',(-1.60374216999313,2.13980583442596,
13.8392439765549));
#429236=CARTESIAN_POINT('Ctrl Pts',(-1.60363573696538,2.14192605568153,
13.8364981347964));
#429237=CARTESIAN_POINT('Ctrl Pts',(-1.60370142935419,2.1439657692749,13.8336931113419));
#429238=CARTESIAN_POINT('Ctrl Pts',(-1.60376540956904,2.14595232078104,
13.8309611966328));
#429239=CARTESIAN_POINT('Ctrl Pts',(-1.60399328798778,2.14786447908079,
13.8281701127185));
#429240=CARTESIAN_POINT('Ctrl Pts',(-1.60438935808485,2.14969037055016,
13.825358068512));
#429241=CARTESIAN_POINT('Ctrl Pts',(-1.60447522650935,2.15008622579127,
13.8247484142932));
#429242=CARTESIAN_POINT('Ctrl Pts',(-1.60456912043427,2.15047790142687,
13.8241378483365));
#429243=CARTESIAN_POINT('Ctrl Pts',(-1.60467127783313,2.15086502402588,
13.8235269408515));
#429244=CARTESIAN_POINT('',(-1.61712648604294,2.11471340614851,12.5969504640361));
#429245=CARTESIAN_POINT('Origin',(-1.63792841759527,2.14212049413521,12.584524458991));
#429246=CARTESIAN_POINT('Origin',(-1.63792841759527,2.14212049413521,12.584524458991));
#429247=CARTESIAN_POINT('Ctrl Pts',(-1.65508430440736,2.11231773338787,
12.5893111709658));
#429248=CARTESIAN_POINT('Ctrl Pts',(-1.64526658674478,2.10665460223473,
12.5770542771492));
#429249=CARTESIAN_POINT('Ctrl Pts',(-1.63459030677959,2.11905705041885,
12.5737548217797));
#429250=CARTESIAN_POINT('Ctrl Pts',(-1.67655235801145,2.12470110061648,
12.5663937883685));
#429251=CARTESIAN_POINT('Ctrl Pts',(-1.66672211648652,2.11903074535306,
12.5540940315304));
#429252=CARTESIAN_POINT('Ctrl Pts',(-1.65601518658201,2.13147372117614,
12.5508374392248));
#429253=CARTESIAN_POINT('Ctrl Pts',(-1.69799875061259,2.13707197317934,
12.5434499600945));
#429254=CARTESIAN_POINT('Ctrl Pts',(-1.68813654747176,2.13138318157174,
12.5311293540532));
#429255=CARTESIAN_POINT('Ctrl Pts',(-1.67741972543363,2.14387723975807,
12.5278936106989));
#429256=CARTESIAN_POINT('Ctrl Pts',(-1.71942517894689,2.14943132980078,
12.5204817579905));
#429257=CARTESIAN_POINT('Ctrl Pts',(-1.70951416464046,2.14371438256243,
12.5081597038247));
#429258=CARTESIAN_POINT('Ctrl Pts',(-1.69880551125946,2.15626861641641,
12.5049254088044));
#429259=CARTESIAN_POINT('Ctrl Pts',(-1.70402056201255,2.14054552058714,
12.5369868989719));
#429260=CARTESIAN_POINT('Ctrl Pts',(-1.7048274512746,2.14101095682285,12.5342545179733));
#429261=CARTESIAN_POINT('Ctrl Pts',(-1.70553517888064,2.14156320563363,
12.5314872231885));
#429262=CARTESIAN_POINT('Ctrl Pts',(-1.70606948802598,2.14221522928913,
12.5287124745063));
#429263=CARTESIAN_POINT('Ctrl Pts',(-1.70655135453398,2.14280325658524,
12.5262100684185));
#429264=CARTESIAN_POINT('Ctrl Pts',(-1.70689092711476,2.14347246417644,
12.5237004536639));
#429265=CARTESIAN_POINT('Ctrl Pts',(-1.70703492089806,2.14426433939502,
12.5212220730815));
#429266=CARTESIAN_POINT('Ctrl Pts',(-1.70714516059564,2.14487058837751,
12.5193246583486));
#429267=CARTESIAN_POINT('Ctrl Pts',(-1.70714146029539,2.14555609470927,
12.517417831369));
#429268=CARTESIAN_POINT('Ctrl Pts',(-1.70692839757651,2.14633952880434,
12.5155812248347));
#429269=CARTESIAN_POINT('Ctrl Pts',(-1.70683763171305,2.14667327593982,
12.5147988205793));
#429270=CARTESIAN_POINT('Ctrl Pts',(-1.70670904581089,2.14702520656152,
12.5140295443047));
#429271=CARTESIAN_POINT('Ctrl Pts',(-1.70653664340126,2.14739838234046,
12.5132817086137));
#429272=CARTESIAN_POINT('Ctrl Pts',(-1.70627573567636,2.14796313339982,
12.5121499604604));
#429273=CARTESIAN_POINT('Ctrl Pts',(-1.70590234975253,2.14858573766316,
12.5110494206568));
#429274=CARTESIAN_POINT('Ctrl Pts',(-1.70538008307767,2.14925833682614,
12.5100666561695));
#429275=CARTESIAN_POINT('Ctrl Pts',(-1.70508019875564,2.14964454171666,
12.5095023550641));
#429276=CARTESIAN_POINT('Ctrl Pts',(-1.70472724754823,2.1500512919848,12.5089719619137));
#429277=CARTESIAN_POINT('Ctrl Pts',(-1.70432302111599,2.15046677757833,
12.5085043804652));
#429278=CARTESIAN_POINT('Ctrl Pts',(-1.70373148838661,2.15107478662366,
12.5078201359221));
#429279=CARTESIAN_POINT('Ctrl Pts',(-1.70301213015636,2.15171829400449,
12.5072563000949));
#429280=CARTESIAN_POINT('Ctrl Pts',(-1.70220806384499,2.1523473696385,12.5068768744332));
#429281=CARTESIAN_POINT('Ctrl Pts',(-1.70162827668238,2.15280097647633,
12.5066032824114));
#429282=CARTESIAN_POINT('Ctrl Pts',(-1.70099429739599,2.15325509615781,
12.5064197834844));
#429283=CARTESIAN_POINT('Ctrl Pts',(-1.7003430342548,2.15368647084205,12.5063282718343));
#429284=CARTESIAN_POINT('Ctrl Pts',(-1.69939239169463,2.15431614433082,
12.5061946931565));
#429285=CARTESIAN_POINT('Ctrl Pts',(-1.69838519019644,2.15491169921664,
12.5062515701262));
#429286=CARTESIAN_POINT('Ctrl Pts',(-1.69739180954226,2.15544948587937,
12.5064436508398));
#429287=CARTESIAN_POINT('',(-1.63459030677959,2.11905705041885,12.5737548217797));
#429288=CARTESIAN_POINT('Origin',(-1.64409177465534,2.13137460326859,12.5893111709658));
#429289=CARTESIAN_POINT('Ctrl Pts',(-1.69739180954226,2.15544948587937,
12.5064436508398));
#429290=CARTESIAN_POINT('Ctrl Pts',(-1.68809531462718,2.15006287562382,
12.5164271754438));
#429291=CARTESIAN_POINT('Ctrl Pts',(-1.67879523933249,2.14467394933615,
12.5264061185523));
#429292=CARTESIAN_POINT('Ctrl Pts',(-1.66949145708569,2.13928262626659,
12.536380305637));
#429293=CARTESIAN_POINT('Ctrl Pts',(-1.65786361628756,2.13254456590778,
12.5488460165097));
#429294=CARTESIAN_POINT('Ctrl Pts',(-1.6462299818335,2.12580275978098,12.5613043021964));
#429295=CARTESIAN_POINT('Ctrl Pts',(-1.63459030677959,2.11905705041885,
12.5737548217797));
#429296=CARTESIAN_POINT('Ctrl Pts',(-1.60467127783313,2.15086502402588,
12.5893111709658));
#429297=CARTESIAN_POINT('Ctrl Pts',(-1.60177936858182,2.13990621499196,
12.5770542771492));
#429298=CARTESIAN_POINT('Ctrl Pts',(-1.61654650137661,2.13285387751592,
12.5737548217797));
#429299=CARTESIAN_POINT('Ctrl Pts',(-1.60197315165416,2.14064055051192,
12.5928319619712));
#429300=CARTESIAN_POINT('Ctrl Pts',(-1.60317952241511,2.1324443266278,12.5821634970842));
#429301=CARTESIAN_POINT('Ctrl Pts',(-1.6155545128858,2.12913175766246,12.5773203894503));
#429302=CARTESIAN_POINT('Ctrl Pts',(-1.60484407344586,2.12413776567403,
12.5969440695591));
#429303=CARTESIAN_POINT('Ctrl Pts',(-1.60802619305558,2.12168161882553,
12.5878292599214));
#429304=CARTESIAN_POINT('Ctrl Pts',(-1.61657978369924,2.12325017906002,
12.5813877129824));
#429305=CARTESIAN_POINT('Ctrl Pts',(-1.62911712815993,2.10550998909203,
12.596957478804));
#429306=CARTESIAN_POINT('Ctrl Pts',(-1.62595857424566,2.10794804781149,
12.5878468778671));
#429307=CARTESIAN_POINT('Ctrl Pts',(-1.62527107808441,2.11658777182131,
12.5814011370086));
#429308=CARTESIAN_POINT('Ctrl Pts',(-1.64591115913877,2.1070264094235,12.5928371701607));
#429309=CARTESIAN_POINT('Ctrl Pts',(-1.63769045973738,2.1060490829398,12.5821692192952));
#429310=CARTESIAN_POINT('Ctrl Pts',(-1.63124778444224,2.11711776655663,
12.5773318885715));
#429311=CARTESIAN_POINT('Ctrl Pts',(-1.65508430440738,2.11231773338782,
12.5893111709658));
#429312=CARTESIAN_POINT('Ctrl Pts',(-1.6452665867448,2.10665460223468,12.5770542771492));
#429313=CARTESIAN_POINT('Ctrl Pts',(-1.63459030677962,2.11905705041881,
12.5737548217797));
#429314=CARTESIAN_POINT('',(-1.61654650137661,2.13285387751592,12.5737548217797));
#429315=CARTESIAN_POINT('Origin',(-1.62594308508861,2.14525162789828,12.5893111709658));
#429316=CARTESIAN_POINT('Ctrl Pts',(-1.63459030677962,2.11905705041881,
12.5737548217797));
#429317=CARTESIAN_POINT('Ctrl Pts',(-1.63373901029835,2.1185282650824,12.5746934679442));
#429318=CARTESIAN_POINT('Ctrl Pts',(-1.63270033742626,2.11809873731492,
12.5756680099006));
#429319=CARTESIAN_POINT('Ctrl Pts',(-1.63159373219408,2.11781425791652,
12.5765688348656));
#429320=CARTESIAN_POINT('Ctrl Pts',(-1.63130077070939,2.11773894514509,
12.5768073183026));
#429321=CARTESIAN_POINT('Ctrl Pts',(-1.63100317074836,2.11767357241844,
12.5770407398754));
#429322=CARTESIAN_POINT('Ctrl Pts',(-1.6307032843191,2.11761844282163,12.5772674179684));
#429323=CARTESIAN_POINT('Ctrl Pts',(-1.62947263150611,2.11739220586398,
12.5781976435658));
#429324=CARTESIAN_POINT('Ctrl Pts',(-1.62813153564926,2.1173367136526,12.5790594849312));
#429325=CARTESIAN_POINT('Ctrl Pts',(-1.6267685532409,2.11750396100884,12.5797571720116));
#429326=CARTESIAN_POINT('Ctrl Pts',(-1.62588052119337,2.1176129286751,12.580211740231));
#429327=CARTESIAN_POINT('Ctrl Pts',(-1.62494512820368,2.11784003423461,
12.5806009430798));
#429328=CARTESIAN_POINT('Ctrl Pts',(-1.62403240189761,2.11818650696735,
12.5808812374708));
#429329=CARTESIAN_POINT('Ctrl Pts',(-1.62324806720689,2.1184842419859,12.5811221033394));
#429330=CARTESIAN_POINT('Ctrl Pts',(-1.62246445383474,2.118876325951,12.581287365893));
#429331=CARTESIAN_POINT('Ctrl Pts',(-1.6217295211521,2.11934808567315,12.581359338449));
#429332=CARTESIAN_POINT('Ctrl Pts',(-1.62162738068499,2.11941365053306,
12.5813693411482));
#429333=CARTESIAN_POINT('Ctrl Pts',(-1.6215261332078,2.11948071762274,12.5813775999465));
#429334=CARTESIAN_POINT('Ctrl Pts',(-1.62142585835752,2.11954921079093,
12.5813841266931));
#429335=CARTESIAN_POINT('Ctrl Pts',(-1.62125572994604,2.11966541773483,
12.5813952001081));
#429336=CARTESIAN_POINT('Ctrl Pts',(-1.62108760524831,2.11978701075322,
12.5814007534795));
#429337=CARTESIAN_POINT('Ctrl Pts',(-1.62092167305851,2.11991409668571,
12.5814005856065));
#429338=CARTESIAN_POINT('Ctrl Pts',(-1.62016210036891,2.12049584639726,
12.5813998171494));
#429339=CARTESIAN_POINT('Ctrl Pts',(-1.61950074602127,2.12115223502266,
12.58127954464));
#429340=CARTESIAN_POINT('Ctrl Pts',(-1.61892052091099,2.1218585344836,12.5810700125799));
#429341=CARTESIAN_POINT('Ctrl Pts',(-1.61821967504169,2.12271166381379,
12.5808169217085));
#429342=CARTESIAN_POINT('Ctrl Pts',(-1.61765006437176,2.12364831318477,
12.5804173076348));
#429343=CARTESIAN_POINT('Ctrl Pts',(-1.61723935774465,2.12457286466203,
12.5799304713245));
#429344=CARTESIAN_POINT('Ctrl Pts',(-1.61673036284773,2.1257186752061,12.5793271277669));
#429345=CARTESIAN_POINT('Ctrl Pts',(-1.61640442761231,2.12690390895128,
12.5785808224116));
#429346=CARTESIAN_POINT('Ctrl Pts',(-1.61624470924234,2.12807019618232,
12.5777485681082));
#429347=CARTESIAN_POINT('Ctrl Pts',(-1.61600671137264,2.12980809193288,
12.576508418016));
#429348=CARTESIAN_POINT('Ctrl Pts',(-1.61613298110624,2.13148835246778,
12.5750928681475));
#429349=CARTESIAN_POINT('Ctrl Pts',(-1.61654650137661,2.13285387751592,
12.5737548217797));
#429350=CARTESIAN_POINT('Ctrl Pts',(-1.61654650137661,2.13285387751592,
12.5737548217797));
#429351=CARTESIAN_POINT('Ctrl Pts',(-1.60177936858182,2.13990621499196,
12.5770542771492));
#429352=CARTESIAN_POINT('Ctrl Pts',(-1.60467127783313,2.15086502402588,
12.5893111709658));
#429353=CARTESIAN_POINT('Ctrl Pts',(-1.62291263497338,2.15678058429305,
12.5508408821982));
#429354=CARTESIAN_POINT('Ctrl Pts',(-1.60809836419938,2.16385187173341,
12.55409748406));
#429355=CARTESIAN_POINT('Ctrl Pts',(-1.61099396278624,2.17482466140095,
12.5663972313419));
#429356=CARTESIAN_POINT('Ctrl Pts',(-1.62927140980334,2.18068422097144,
12.52790050457));
#429357=CARTESIAN_POINT('Ctrl Pts',(-1.61440525743634,2.18775166684268,
12.5311362602938));
#429358=CARTESIAN_POINT('Ctrl Pts',(-1.6173102691892,2.198760127439,12.5434568539654));
#429359=CARTESIAN_POINT('Ctrl Pts',(-1.63562338435458,2.20456658395455,
12.5049357605811));
#429360=CARTESIAN_POINT('Ctrl Pts',(-1.62070130990391,2.21161038116047,
12.5081700652078));
#429361=CARTESIAN_POINT('Ctrl Pts',(-1.62362069661134,2.22267331524406,
12.5204921097672));
#429362=CARTESIAN_POINT('Ctrl Pts',(-1.63520628727276,2.20299837479304,
12.5064436508395));
#429363=CARTESIAN_POINT('Ctrl Pts',(-1.63436444559968,2.20388163601603,
12.5062361689309));
#429364=CARTESIAN_POINT('Ctrl Pts',(-1.63345133492937,2.2047642574095,12.5061871075061));
#429365=CARTESIAN_POINT('Ctrl Pts',(-1.63252088586825,2.20556755136925,
12.5063648335164));
#429366=CARTESIAN_POINT('Ctrl Pts',(-1.63209821851221,2.205932457035,12.5064455676329));
#429367=CARTESIAN_POINT('Ctrl Pts',(-1.63166593401139,2.20628591610481,
12.506574497099));
#429368=CARTESIAN_POINT('Ctrl Pts',(-1.6312419021852,2.20661195971359,12.5067492519495));
#429369=CARTESIAN_POINT('Ctrl Pts',(-1.63038979377069,2.20726715700158,
12.5071004286051));
#429370=CARTESIAN_POINT('Ctrl Pts',(-1.62953919007105,2.20783509248937,
12.5076537929613));
#429371=CARTESIAN_POINT('Ctrl Pts',(-1.62875918550295,2.20828100584431,
12.5083435010505));
#429372=CARTESIAN_POINT('Ctrl Pts',(-1.62871007955406,2.20830907875479,
12.5083869222964));
#429373=CARTESIAN_POINT('Ctrl Pts',(-1.62866124214319,2.20833666073623,
12.5084308732337));
#429374=CARTESIAN_POINT('Ctrl Pts',(-1.6286126857036,2.20836374047461,12.5084753333615));
#429375=CARTESIAN_POINT('Ctrl Pts',(-1.62822319896941,2.20858095571843,
12.5088319622689));
#429376=CARTESIAN_POINT('Ctrl Pts',(-1.62784451150921,2.20877139239141,
12.509227847131));
#429377=CARTESIAN_POINT('Ctrl Pts',(-1.62748914166938,2.20893188936773,
12.5096423454524));
#429378=CARTESIAN_POINT('Ctrl Pts',(-1.62637556987143,2.20943481585851,
12.5109411997424));
#429379=CARTESIAN_POINT('Ctrl Pts',(-1.6254264458662,2.20968350384047,12.5124831113042));
#429380=CARTESIAN_POINT('Ctrl Pts',(-1.62462695293855,2.20977142160957,
12.5140723025008));
#429381=CARTESIAN_POINT('Ctrl Pts',(-1.62455203957557,2.20977965960083,
12.5142212114565));
#429382=CARTESIAN_POINT('Ctrl Pts',(-1.6244784253376,2.20978651179276,12.5143705582413));
#429383=CARTESIAN_POINT('Ctrl Pts',(-1.62440609102875,2.20979207055018,
12.5145201959299));
#429384=CARTESIAN_POINT('Ctrl Pts',(-1.623476849137,2.20986348106537,12.5164425148273));
#429385=CARTESIAN_POINT('Ctrl Pts',(-1.62272782043561,2.20973458659751,
12.518463520594));
#429386=CARTESIAN_POINT('Ctrl Pts',(-1.6221006044473,2.20947414296675,12.5205025929157));
#429387=CARTESIAN_POINT('Ctrl Pts',(-1.62173679431356,2.20932307533789,
12.5216853356836));
#429388=CARTESIAN_POINT('Ctrl Pts',(-1.62141443932725,2.20912846799645,
12.5228750347131));
#429389=CARTESIAN_POINT('Ctrl Pts',(-1.62112687190551,2.20890730555274,
12.5240609649613));
#429390=CARTESIAN_POINT('Ctrl Pts',(-1.62042105309633,2.2083644741996,12.5269717671327));
#429391=CARTESIAN_POINT('Ctrl Pts',(-1.61991127826939,2.2076381487808,12.5299036066169));
#429392=CARTESIAN_POINT('Ctrl Pts',(-1.61953554386697,2.20678886921258,
12.532813300402));
#429393=CARTESIAN_POINT('Ctrl Pts',(-1.61935516947545,2.20638116556777,
12.5342101228452));
#429394=CARTESIAN_POINT('Ctrl Pts',(-1.6192063898159,2.2059454230755,12.5356023438238));
#429395=CARTESIAN_POINT('Ctrl Pts',(-1.61908595352013,2.20548903343024,
12.5369868989719));
#429396=CARTESIAN_POINT('Origin',(-4.86600595941219,14.5303612090825,-1.24011047643264));
#429397=CARTESIAN_POINT('Ctrl Pts',(-1.70398437877637,2.1405246032653,12.5369868989719));
#429398=CARTESIAN_POINT('Ctrl Pts',(-1.71725671844646,2.14821409631539,
12.5369868989719));
#429399=CARTESIAN_POINT('Ctrl Pts',(-1.72906124176311,2.13841937666895,
12.5369868989719));
#429400=CARTESIAN_POINT('Ctrl Pts',(-1.70847098185535,2.14312389535928,
12.5218025310016));
#429401=CARTESIAN_POINT('Ctrl Pts',(-1.7199480758786,2.14594030734725,12.5216901060418));
#429402=CARTESIAN_POINT('Ctrl Pts',(-1.72902526819479,2.13844924691217,
12.5161920673678));
#429403=CARTESIAN_POINT('Ctrl Pts',(-1.70905908125986,2.14912307949432,
12.5042015548894));
#429404=CARTESIAN_POINT('Ctrl Pts',(-1.71548231564416,2.14946862986869,
12.4980677368513));
#429405=CARTESIAN_POINT('Ctrl Pts',(-1.72079051918672,2.14522436846363,
12.4907278922777));
#429406=CARTESIAN_POINT('Ctrl Pts',(-1.69737943520329,2.15543377222162,
12.506463626192));
#429407=CARTESIAN_POINT('Ctrl Pts',(-1.70142731714501,2.16057401444572,
12.4999376786891));
#429408=CARTESIAN_POINT('Ctrl Pts',(-1.7013778781527,2.16051123386085,12.4906970594712));
#429409=CARTESIAN_POINT('Origin',(-1.71501309176457,2.12148865070642,12.5369868989719));
#429410=CARTESIAN_POINT('Origin',(-1.71501309176457,2.12148865070642,14.));
#429411=CARTESIAN_POINT('Origin',(-1.71501309176457,2.12148865070642,13.7435492065112));
#429412=CARTESIAN_POINT('Ctrl Pts',(-1.68257284468358,2.12817385253986,
13.793642941384));
#429413=CARTESIAN_POINT('Ctrl Pts',(-1.69192507402185,2.13359990316717,
13.8071662555867));
#429414=CARTESIAN_POINT('Ctrl Pts',(-1.70254422443381,2.12028626248691,
13.8103758687955));
#429415=CARTESIAN_POINT('Ctrl Pts',(-1.69697041429798,2.13647877243237,
13.7804579775006));
#429416=CARTESIAN_POINT('Ctrl Pts',(-1.7085153090511,2.14316525707442,13.7901904343351));
#429417=CARTESIAN_POINT('Ctrl Pts',(-1.72020366376397,2.13259935492315,
13.7927914348262));
#429418=CARTESIAN_POINT('Ctrl Pts',(-1.70544680539051,2.14136819128946,
13.7597120340895));
#429419=CARTESIAN_POINT('Ctrl Pts',(-1.71881037184997,2.14910137830751,
13.7635825532445));
#429420=CARTESIAN_POINT('Ctrl Pts',(-1.73063203532483,2.13983940287936,
13.7651073818885));
#429421=CARTESIAN_POINT('Ctrl Pts',(-1.7037869339277,2.14041073112157,13.7381884353898));
#429422=CARTESIAN_POINT('Ctrl Pts',(-1.71683725102629,2.14796368645392,
13.7368803041982));
#429423=CARTESIAN_POINT('Ctrl Pts',(-1.72859013215357,2.13842118037182,
13.7363986145813));
#429424=CARTESIAN_POINT('Origin',(-1.69705890579044,2.11113217953728,13.7902182540695));
#429425=CARTESIAN_POINT('Ctrl Pts',(-1.65508089516743,2.11231576596783,
13.8235227101244));
#429426=CARTESIAN_POINT('Ctrl Pts',(-1.66503768943828,2.11806423847515,
13.8358800583119));
#429427=CARTESIAN_POINT('Ctrl Pts',(-1.67576452834183,2.10543249369488,
13.8390832900376));
#429428=CARTESIAN_POINT('Ctrl Pts',(-1.66541281915797,2.11827550555509,
13.8124254819052));
#429429=CARTESIAN_POINT('Ctrl Pts',(-1.67538894952124,2.12403514127364,
13.8247886449157));
#429430=CARTESIAN_POINT('Ctrl Pts',(-1.68611635037659,2.11137640310625,
13.8279860620657));
#429431=CARTESIAN_POINT('Ctrl Pts',(-1.67574011271632,2.12423257418097,
13.8013225099955));
#429432=CARTESIAN_POINT('Ctrl Pts',(-1.68573087103815,2.13000065722366,
13.8136962257787));
#429433=CARTESIAN_POINT('Ctrl Pts',(-1.69646324505636,2.11731779584243,
13.8168830918626));
#429434=CARTESIAN_POINT('Ctrl Pts',(-1.68606295600545,2.13018707576847,
13.7902140179785));
#429435=CARTESIAN_POINT('Ctrl Pts',(-1.69606394186462,2.13596106774883,
13.802602731458));
#429436=CARTESIAN_POINT('Ctrl Pts',(-1.7068054050725,2.12325677238564,13.8057746032558));
#429437=CARTESIAN_POINT('Origin',(-1.66607683415938,2.09326086350714,13.8235269408515));
#429438=CARTESIAN_POINT('Ctrl Pts',(-1.60467127783313,2.15086502402588,
13.8235269408515));
#429439=CARTESIAN_POINT('Ctrl Pts',(-1.6076840083236,2.16228168175845,13.8362179249168));
#429440=CARTESIAN_POINT('Ctrl Pts',(-1.59209337512992,2.16925270468747,
13.8391868794938));
#429441=CARTESIAN_POINT('Ctrl Pts',(-1.6019147605707,2.14041927913812,13.8400110824519));
#429442=CARTESIAN_POINT('Ctrl Pts',(-1.60102246856986,2.15044552857883,
13.8494522556837));
#429443=CARTESIAN_POINT('Ctrl Pts',(-1.58766556384792,2.15203328916674,
13.85569149686));
#429444=CARTESIAN_POINT('Ctrl Pts',(-1.60457051206087,2.12434617395997,
13.8586819406588));
#429445=CARTESIAN_POINT('Ctrl Pts',(-1.6011203323933,2.12700179138279,13.868010383617));
#429446=CARTESIAN_POINT('Ctrl Pts',(-1.5922182107488,2.125375415959,13.8744918421245));
#429447=CARTESIAN_POINT('Ctrl Pts',(-1.62939492102075,2.10529833372175,
13.8587686893867));
#429448=CARTESIAN_POINT('Ctrl Pts',(-1.63281435977636,2.1026663066481,13.8680909899357));
#429449=CARTESIAN_POINT('Ctrl Pts',(-1.63354512787496,2.09366839691907,
13.8745789365162));
#429450=CARTESIAN_POINT('Ctrl Pts',(-1.64571100002057,2.10691095209924,
13.8400379222776));
#429451=CARTESIAN_POINT('Ctrl Pts',(-1.65561933451111,2.10867025353205,
13.8494748685452));
#429452=CARTESIAN_POINT('Ctrl Pts',(-1.66065117833342,2.09620262933925,
13.8557104837033));
#429453=CARTESIAN_POINT('Ctrl Pts',(-1.65508430441053,2.11231773338207,
13.8235269408542));
#429454=CARTESIAN_POINT('Ctrl Pts',(-1.66531219705122,2.11821746480994,
13.8362179249195));
#429455=CARTESIAN_POINT('Ctrl Pts',(-1.67612584604502,2.10499899290525,
13.8391868794965));
#429456=CARTESIAN_POINT('Origin',(-1.58339947057764,2.15647842015348,13.8235269408515));
#429457=CARTESIAN_POINT('Ctrl Pts',(-1.61379635744607,2.18544426037843,
13.7902140241682));
#429458=CARTESIAN_POINT('Ctrl Pts',(-1.6167472094838,2.19660898463136,13.8026027327198));
#429459=CARTESIAN_POINT('Ctrl Pts',(-1.60167170336877,2.20364510910788,
13.8057746032556));
#429460=CARTESIAN_POINT('Ctrl Pts',(-1.61075565827017,2.17392161609233,
13.8013225161808));
#429461=CARTESIAN_POINT('Ctrl Pts',(-1.61370348861245,2.18507492161842,
13.8136962270464));
#429462=CARTESIAN_POINT('Ctrl Pts',(-1.59865104943324,2.1921078925461,13.8168830918628));
#429463=CARTESIAN_POINT('Ctrl Pts',(-1.60771364822151,2.1623940042906,13.8124254880875));
#429464=CARTESIAN_POINT('Ctrl Pts',(-1.61065716058229,2.17353097919505,
13.8247886461867));
#429465=CARTESIAN_POINT('Ctrl Pts',(-1.59562930473771,2.18056547355589,
13.8279860620656));
#429466=CARTESIAN_POINT('Ctrl Pts',(-1.60467027423082,2.15086122386878,
13.8235227163065));
#429467=CARTESIAN_POINT('Ctrl Pts',(-1.60760808168087,2.1619766127789,13.8358800595847));
#429468=CARTESIAN_POINT('Ctrl Pts',(-1.59260642281724,2.16901763984442,
13.8390832900376));
#429469=CARTESIAN_POINT('Origin',(-1.59252555697101,2.1910614686938,13.7902182540695));
#429470=CARTESIAN_POINT('Ctrl Pts',(-1.61901707091557,2.2052281128403,13.7382347919292));
#429471=CARTESIAN_POINT('Ctrl Pts',(-1.62289063398972,2.21981280954076,
13.7369371795943));
#429472=CARTESIAN_POINT('Ctrl Pts',(-1.61058695297563,2.22865380555502,
13.7364597369711));
#429473=CARTESIAN_POINT('Ctrl Pts',(-1.61949971074945,2.20705706138388,
13.7595490285574));
#429474=CARTESIAN_POINT('Ctrl Pts',(-1.62346472198187,2.22198999452996,
13.7633824266926));
#429475=CARTESIAN_POINT('Ctrl Pts',(-1.61141055139078,2.23096722303704,
13.7648920890506));
#429476=CARTESIAN_POINT('Ctrl Pts',(-1.61703827404558,2.1977295240076,13.7803806590111));
#429477=CARTESIAN_POINT('Ctrl Pts',(-1.62047308450817,2.21064459129706,
13.7901039518744));
#429478=CARTESIAN_POINT('Ctrl Pts',(-1.60721525445259,2.21917192286346,
13.7926933640892));
#429479=CARTESIAN_POINT('Ctrl Pts',(-1.61275974751797,2.18151618189917,
13.7936647693663));
#429480=CARTESIAN_POINT('Ctrl Pts',(-1.61554832042228,2.19196592797752,
13.8072068914933));
#429481=CARTESIAN_POINT('Ctrl Pts',(-1.59989580680658,2.19872189477419,
13.8104111085397));
#429482=CARTESIAN_POINT('Origin',(-1.59781414626465,2.21110242955784,13.7435492065112));
#429483=CARTESIAN_POINT('Origin',(-1.59781414626465,2.21110242955784,14.));
#429484=CARTESIAN_POINT('Origin',(-1.59781414626465,2.21110242955784,12.5369868989719));
#429485=CARTESIAN_POINT('Ctrl Pts',(-1.63519533055901,2.20298361356624,
12.506462012331));
#429486=CARTESIAN_POINT('Ctrl Pts',(-1.63909246104785,2.20823394326472,
12.4999388158272));
#429487=CARTESIAN_POINT('Ctrl Pts',(-1.6390463528834,2.20817182497901,12.4907030323752));
#429488=CARTESIAN_POINT('Ctrl Pts',(-1.6260428171011,2.21259923006011,12.5042014951932));
#429489=CARTESIAN_POINT('Ctrl Pts',(-1.62469427205075,2.21888592421232,
12.4980716682127));
#429490=CARTESIAN_POINT('Ctrl Pts',(-1.61921190078417,2.22289456120277,
12.4907355092744));
#429491=CARTESIAN_POINT('Ctrl Pts',(-1.62040747561331,2.21046179525144,
12.5218047446509));
#429492=CARTESIAN_POINT('Ctrl Pts',(-1.6201162791044,2.22227001592727,12.5216906929434));
#429493=CARTESIAN_POINT('Ctrl Pts',(-1.6105149893975,2.22906604346504,12.5161988840775));
#429494=CARTESIAN_POINT('Ctrl Pts',(-1.61907611905049,2.20545189743654,
12.5369868989719));
#429495=CARTESIAN_POINT('Ctrl Pts',(-1.62301348435132,2.2202675204747,12.5369868989719));
#429496=CARTESIAN_POINT('Ctrl Pts',(-1.61047814233234,2.2290919599463,12.5369868989719));
#429497=CARTESIAN_POINT('Origin',(-3.12930240632751E-31,-1.05928948499644E-31,
12.5));
#429498=CARTESIAN_POINT('Origin',(-1.77464733364699,2.01291259190758,12.5));
#429499=CARTESIAN_POINT('',(-1.77464733364699,2.01291259190758,12.5893111709658));
#429500=CARTESIAN_POINT('',(-1.77464733364699,2.01291259190758,13.8235269408515));
#429501=CARTESIAN_POINT('',(-1.77464733364699,2.01291259190758,12.5));
#429502=CARTESIAN_POINT('',(-1.78656189325013,2.04663670744327,13.7902182540695));
#429503=CARTESIAN_POINT('',(-1.77464733364699,2.01291259190758,13.8235269408515));
#429504=CARTESIAN_POINT('',(-1.79346640956079,2.066179914539,13.7435492065112));
#429505=CARTESIAN_POINT('Origin',(-1.77075094931264,2.00188291300246,13.7445212918702));
#429506=CARTESIAN_POINT('',(-1.79346640956079,2.066179914539,12.5369868989719));
#429507=CARTESIAN_POINT('',(-1.79346640956079,2.066179914539,12.5));
#429508=CARTESIAN_POINT('Ctrl Pts',(-1.79346640956079,2.066179914539,12.5369868989719));
#429509=CARTESIAN_POINT('Ctrl Pts',(-1.78719795941931,2.04843709031031,
12.5544431401645));
#429510=CARTESIAN_POINT('Ctrl Pts',(-1.78092502591569,2.03068157594215,
12.5718848856037));
#429511=CARTESIAN_POINT('Ctrl Pts',(-1.77464733364699,2.01291259190758,
12.5893111709658));
#429512=CARTESIAN_POINT('Origin',(-2.0703688147757,2.08791744959,12.5));
#429513=CARTESIAN_POINT('',(-1.87282490594719,1.99452953679086,13.7435492065112));
#429514=CARTESIAN_POINT('',(-1.8540863125007,1.98567095876061,13.7902182540695));
#429515=CARTESIAN_POINT('Origin',(-1.80484452760419,1.96239214676757,13.7418732680449));
#429516=CARTESIAN_POINT('',(-1.82175065299149,1.97038443452173,13.8235269408515));
#429517=CARTESIAN_POINT('',(-1.8540863125007,1.98567095876061,13.7902182540695));
#429518=CARTESIAN_POINT('',(-1.82175065299149,1.97038443452173,12.5893111709658));
#429519=CARTESIAN_POINT('',(-1.82175065299149,1.97038443452173,12.5));
#429520=CARTESIAN_POINT('',(-1.87282490594719,1.99452953679086,12.5369868989719));
#429521=CARTESIAN_POINT('Ctrl Pts',(-1.82175065299149,1.97038443452173,
12.5893111709658));
#429522=CARTESIAN_POINT('Ctrl Pts',(-1.83878806993896,1.97843878971623,
12.5718848856037));
#429523=CARTESIAN_POINT('Ctrl Pts',(-1.85581257177986,1.9864870393575,12.5544431401645));
#429524=CARTESIAN_POINT('Ctrl Pts',(-1.87282490594719,1.99452953679086,
12.5369868989719));
#429525=CARTESIAN_POINT('',(-1.87282490594719,1.99452953679086,12.5));
#429526=CARTESIAN_POINT('Origin',(-1.80705902610795,2.00146170474476,12.5));
#429527=CARTESIAN_POINT('',(-1.78320468836154,1.97671174024261,13.8587068136939));
#429528=CARTESIAN_POINT('Ctrl Pts',(-1.82175065299418,1.9703844345157,13.8235269408542));
#429529=CARTESIAN_POINT('Ctrl Pts',(-1.82016645957971,1.96963551485868,
13.8262006681044));
#429530=CARTESIAN_POINT('Ctrl Pts',(-1.81847101414716,1.96902617684305,
13.8288634856214));
#429531=CARTESIAN_POINT('Ctrl Pts',(-1.81667371992282,1.96854696608446,
13.8314912288862));
#429532=CARTESIAN_POINT('Ctrl Pts',(-1.81482089495982,1.96805294922064,
13.8342001611531));
#429533=CARTESIAN_POINT('Ctrl Pts',(-1.81285790034408,1.96769619603974,
13.8368750301949));
#429534=CARTESIAN_POINT('Ctrl Pts',(-1.81076554033127,1.9675005977407,13.8394886372969));
#429535=CARTESIAN_POINT('Ctrl Pts',(-1.81060394229213,1.96748549120961,
13.8396904925131));
#429536=CARTESIAN_POINT('Ctrl Pts',(-1.81044156677802,1.9674713673101,13.8398919674349));
#429537=CARTESIAN_POINT('Ctrl Pts',(-1.81027840291465,1.96745824831066,
13.8400930404591));
#429538=CARTESIAN_POINT('Ctrl Pts',(-1.80773620015197,1.96725384547332,
13.8432258934518));
#429539=CARTESIAN_POINT('Ctrl Pts',(-1.80501568193227,1.96729331063822,
13.8462331177034));
#429540=CARTESIAN_POINT('Ctrl Pts',(-1.80220697616124,1.96767181281182,
13.8489036603661));
#429541=CARTESIAN_POINT('Ctrl Pts',(-1.80128793494641,1.96779566312788,
13.8497774930041));
#429542=CARTESIAN_POINT('Ctrl Pts',(-1.80035967723343,1.96795592102885,
13.85061494757));
#429543=CARTESIAN_POINT('Ctrl Pts',(-1.79942600972377,1.96815621757647,
13.8514076489583));
#429544=CARTESIAN_POINT('Ctrl Pts',(-1.79745116828584,1.96857987366177,
13.8530843267192));
#429545=CARTESIAN_POINT('Ctrl Pts',(-1.79525876334212,1.96922716236845,
13.8546805203176));
#429546=CARTESIAN_POINT('Ctrl Pts',(-1.793014676997,1.97019137671864,13.8559412814273));
#429547=CARTESIAN_POINT('Ctrl Pts',(-1.79271434546656,1.97032041986892,
13.8561100121513));
#429548=CARTESIAN_POINT('Ctrl Pts',(-1.79241311089752,1.97045506609962,
13.8562727473908));
#429549=CARTESIAN_POINT('Ctrl Pts',(-1.79211138402505,1.97059546433379,
13.8564289040185));
#429550=CARTESIAN_POINT('Ctrl Pts',(-1.79074305610068,1.97123216872404,
13.8571370725437));
#429551=CARTESIAN_POINT('Ctrl Pts',(-1.78934151240086,1.9720004249295,13.8577210840554));
#429552=CARTESIAN_POINT('Ctrl Pts',(-1.78797533798368,1.97289610599441,
13.8581177131616));
#429553=CARTESIAN_POINT('Ctrl Pts',(-1.78759057624551,1.97314836061069,
13.8582294175695));
#429554=CARTESIAN_POINT('Ctrl Pts',(-1.78720855353301,1.97341055756911,
13.8583265086086));
#429555=CARTESIAN_POINT('Ctrl Pts',(-1.78683061358246,1.97368220749652,
13.8584082369006));
#429556=CARTESIAN_POINT('Ctrl Pts',(-1.78628761522211,1.9740724955964,13.8585256585398));
#429557=CARTESIAN_POINT('Ctrl Pts',(-1.78574648246221,1.97448741125886,
13.8586122832068));
#429558=CARTESIAN_POINT('Ctrl Pts',(-1.78522175286843,1.97491680285174,
13.8586682984299));
#429559=CARTESIAN_POINT('Ctrl Pts',(-1.78480202120818,1.97526027356182,
13.8587131050557));
#429560=CARTESIAN_POINT('Ctrl Pts',(-1.78438800053653,1.97561661874028,
13.8587357943552));
#429561=CARTESIAN_POINT('Ctrl Pts',(-1.78397997203229,1.97598626457877,
13.8587355499465));
#429562=CARTESIAN_POINT('Ctrl Pts',(-1.78371625348208,1.97622517549701,
13.8587353919793));
#429563=CARTESIAN_POINT('Ctrl Pts',(-1.78345786391976,1.97646703034904,
13.8587257282814));
#429564=CARTESIAN_POINT('Ctrl Pts',(-1.78320468836154,1.97671174024261,
13.8587068136939));
#429565=CARTESIAN_POINT('Ctrl Pts',(-1.78320468836154,1.97671174024261,
13.8587068136939));
#429566=CARTESIAN_POINT('Ctrl Pts',(-1.78237200775288,1.97751657774173,
13.8586446046466));
#429567=CARTESIAN_POINT('Ctrl Pts',(-1.78159565778567,1.97835226114744,
13.858482427929));
#429568=CARTESIAN_POINT('Ctrl Pts',(-1.78087216243592,1.97921597919409,
13.8582284286032));
#429569=CARTESIAN_POINT('Ctrl Pts',(-1.78012994036745,1.98010205343822,
13.8579678548414));
#429570=CARTESIAN_POINT('Ctrl Pts',(-1.77944270557235,1.98102078035111,
13.857615680862));
#429571=CARTESIAN_POINT('Ctrl Pts',(-1.77882979270363,1.98193013579475,
13.8571944833187));
#429572=CARTESIAN_POINT('Ctrl Pts',(-1.77730020595615,1.98419952530559,
13.8561433417727));
#429573=CARTESIAN_POINT('Ctrl Pts',(-1.77615797266665,1.9865140237653,13.8546163505474));
#429574=CARTESIAN_POINT('Ctrl Pts',(-1.77532345585089,1.98868280188526,
13.8528973491086));
#429575=CARTESIAN_POINT('Ctrl Pts',(-1.7751710019408,1.98907900565043,13.8525833129072));
#429576=CARTESIAN_POINT('Ctrl Pts',(-1.77502867730194,1.98947036207524,
13.8522628768812));
#429577=CARTESIAN_POINT('Ctrl Pts',(-1.77489582404558,1.989855755336,13.851937733538));
#429578=CARTESIAN_POINT('Ctrl Pts',(-1.77408450764156,1.99220929850855,
13.8499521282529));
#429579=CARTESIAN_POINT('Ctrl Pts',(-1.7735496406591,1.99457567992749,13.847639871647));
#429580=CARTESIAN_POINT('Ctrl Pts',(-1.77324096984181,1.9968128189494,13.8452109780794));
#429581=CARTESIAN_POINT('Ctrl Pts',(-1.77310209245195,1.99781935410184,
13.8441181685877));
#429582=CARTESIAN_POINT('Ctrl Pts',(-1.7730083025553,1.99879988074523,13.8430021611332));
#429583=CARTESIAN_POINT('Ctrl Pts',(-1.7729521695578,1.99974313321985,13.8418824960098));
#429584=CARTESIAN_POINT('Ctrl Pts',(-1.77281989071578,2.0019659317631,13.8392439765549));
#429585=CARTESIAN_POINT('Ctrl Pts',(-1.77288662955065,2.00408777343718,
13.8364981347964));
#429586=CARTESIAN_POINT('Ctrl Pts',(-1.77311835894709,2.00611534551228,
13.8336931113419));
#429587=CARTESIAN_POINT('Ctrl Pts',(-1.77334404866305,2.00809007195069,
13.8309611966328));
#429588=CARTESIAN_POINT('Ctrl Pts',(-1.77372702748818,2.00997729349478,
13.8281701127186));
#429589=CARTESIAN_POINT('Ctrl Pts',(-1.77427060680018,2.01176482607106,
13.8253580685121));
#429590=CARTESIAN_POINT('Ctrl Pts',(-1.77438845538168,2.01215236506277,
13.8247484142933));
#429591=CARTESIAN_POINT('Ctrl Pts',(-1.77451396208275,2.01253508420346,
13.8241378483365));
#429592=CARTESIAN_POINT('Ctrl Pts',(-1.77464733364699,2.01291259190758,
13.8235269408515));
#429593=CARTESIAN_POINT('',(-1.78411440570672,1.97586605045878,12.5969504640361));
#429594=CARTESIAN_POINT('Origin',(-1.80708105265376,2.00148639308392,12.584524458991));
#429595=CARTESIAN_POINT('Origin',(-1.80708105265376,2.00148639308392,12.584524458991));
#429596=CARTESIAN_POINT('Ctrl Pts',(-1.82175065299149,1.97038443452173,
12.5893111709658));
#429597=CARTESIAN_POINT('Ctrl Pts',(-1.8115040052116,1.96554038210308,12.5770542771492));
#429598=CARTESIAN_POINT('Ctrl Pts',(-1.80187416435298,1.97877177809491,
12.5737548217797));
#429599=CARTESIAN_POINT('Ctrl Pts',(-1.8441566328089,1.98097675144902,12.5663937883685));
#429600=CARTESIAN_POINT('Ctrl Pts',(-1.83389691400673,1.97612651976878,
12.5540940315304));
#429601=CARTESIAN_POINT('Ctrl Pts',(-1.82423982857276,1.98940080680176,
12.5508374392248));
#429602=CARTESIAN_POINT('Ctrl Pts',(-1.86654000526735,1.99155838085839,
12.5434499600945));
#429603=CARTESIAN_POINT('Ctrl Pts',(-1.85624692846577,1.98669237934775,
12.5311293540533));
#429604=CARTESIAN_POINT('Ctrl Pts',(-1.84658414750019,2.00001838507236,
12.5278936106989));
#429605=CARTESIAN_POINT('Ctrl Pts',(-1.88890254123221,2.00213015991773,
12.5204817579905));
#429606=CARTESIAN_POINT('Ctrl Pts',(-1.87855852073481,1.99724007502505,
12.5081597038247));
#429607=CARTESIAN_POINT('Ctrl Pts',(-1.86890878612145,2.01062539036636,
12.5049254088044));
#429608=CARTESIAN_POINT('Ctrl Pts',(-1.87282490594719,1.99452953679086,
12.5369868989719));
#429609=CARTESIAN_POINT('Ctrl Pts',(-1.8736670477259,1.99492765536024,12.5342545179733));
#429610=CARTESIAN_POINT('Ctrl Pts',(-1.87441743383162,1.99542038023855,
12.5314872231885));
#429611=CARTESIAN_POINT('Ctrl Pts',(-1.87500311108837,1.9960266831835,12.5287124745063));
#429612=CARTESIAN_POINT('Ctrl Pts',(-1.87553130390893,1.99657347727345,
12.5262100684184));
#429613=CARTESIAN_POINT('Ctrl Pts',(-1.87592429322125,1.99721277981382,
12.5237004536639));
#429614=CARTESIAN_POINT('Ctrl Pts',(-1.87613235305885,1.99799028330282,
12.5212220730815));
#429615=CARTESIAN_POINT('Ctrl Pts',(-1.87629164086314,1.99858552948307,
12.5193246583486));
#429616=CARTESIAN_POINT('Ctrl Pts',(-1.8763438280053,1.99926905645787,12.517417831369));
#429617=CARTESIAN_POINT('Ctrl Pts',(-1.87619533138684,2.00006725033019,
12.5155812248348));
#429618=CARTESIAN_POINT('Ctrl Pts',(-1.8761320710292,2.00040728521011,12.5147988205793));
#429619=CARTESIAN_POINT('Ctrl Pts',(-1.87603259859886,2.00076852575646,
12.5140295443047));
#429620=CARTESIAN_POINT('Ctrl Pts',(-1.8758911871344,2.00115451222068,12.5132817086137));
#429621=CARTESIAN_POINT('Ctrl Pts',(-1.87567718001267,2.0017386505192,12.5121499604604));
#429622=CARTESIAN_POINT('Ctrl Pts',(-1.87535578452713,2.00238961753736,
12.5110494206568));
#429623=CARTESIAN_POINT('Ctrl Pts',(-1.87489007872744,2.00310254826459,
12.5100666561695));
#429624=CARTESIAN_POINT('Ctrl Pts',(-1.87462267152968,2.00351191144643,
12.5095023550641));
#429625=CARTESIAN_POINT('Ctrl Pts',(-1.87430404866123,2.00394607708666,
12.5089719619137));
#429626=CARTESIAN_POINT('Ctrl Pts',(-1.87393503319215,2.00439312839303,
12.5085043804652));
#429627=CARTESIAN_POINT('Ctrl Pts',(-1.8733950271208,2.00504732974738,12.5078201359221));
#429628=CARTESIAN_POINT('Ctrl Pts',(-1.87273051432205,2.00574733028379,
12.5072563000953));
#429629=CARTESIAN_POINT('Ctrl Pts',(-1.87198039897921,2.00643985158945,
12.5068768744336));
#429630=CARTESIAN_POINT('Ctrl Pts',(-1.8714395141789,2.00693920712416,12.5066032824118));
#429631=CARTESIAN_POINT('Ctrl Pts',(-1.87084465937544,2.007443490958,12.5064197834844));
#429632=CARTESIAN_POINT('Ctrl Pts',(-1.87023072430008,2.0079265142706,12.5063282718343));
#429633=CARTESIAN_POINT('Ctrl Pts',(-1.86933456915955,2.00863157876677,
12.5061946931565));
#429634=CARTESIAN_POINT('Ctrl Pts',(-1.86837926229331,2.00930724826534,
12.5062515701262));
#429635=CARTESIAN_POINT('Ctrl Pts',(-1.86743302163689,2.00992421523273,
12.5064436508398));
#429636=CARTESIAN_POINT('',(-1.80187416435298,1.97877177809491,12.5737548217797));
#429637=CARTESIAN_POINT('Origin',(-1.81234801178603,1.99027388746447,12.5893111709658));
#429638=CARTESIAN_POINT('Ctrl Pts',(-1.86743302163689,2.00992421523273,
12.5064436508398));
#429639=CARTESIAN_POINT('Ctrl Pts',(-1.85772840129906,2.00531327911846,
12.5164271754438));
#429640=CARTESIAN_POINT('Ctrl Pts',(-1.84802002371692,2.00070032651266,
12.5264061185523));
#429641=CARTESIAN_POINT('Ctrl Pts',(-1.83830775615727,1.99608528725107,
12.536380305637));
#429642=CARTESIAN_POINT('Ctrl Pts',(-1.82616939156783,1.99031742420491,
12.5488460165097));
#429643=CARTESIAN_POINT('Ctrl Pts',(-1.81402494728548,1.98454630009124,
12.5613043021964));
#429644=CARTESIAN_POINT('Ctrl Pts',(-1.80187416435298,1.97877177809491,
12.5737548217797));
#429645=CARTESIAN_POINT('Ctrl Pts',(-1.77464733364699,2.01291259190758,
12.5893111709658));
#429646=CARTESIAN_POINT('Ctrl Pts',(-1.77087180231227,2.00222596485784,
12.5770542771492));
#429647=CARTESIAN_POINT('Ctrl Pts',(-1.78501496771588,1.99399343503882,
12.5737548217797));
#429648=CARTESIAN_POINT('Ctrl Pts',(-1.77112479574953,2.00294206181754,
12.5928319619712));
#429649=CARTESIAN_POINT('Ctrl Pts',(-1.77165908407471,1.99467477977585,
12.5821634970842));
#429650=CARTESIAN_POINT('Ctrl Pts',(-1.78372289266241,1.9903645565033,12.5773203894503));
#429651=CARTESIAN_POINT('Ctrl Pts',(-1.77264103461714,1.98626018185646,
12.5969440695591));
#429652=CARTESIAN_POINT('Ctrl Pts',(-1.77561236721645,1.98355283534443,
12.5878292599214));
#429653=CARTESIAN_POINT('Ctrl Pts',(-1.78426534871378,1.98441897927902,
12.5813877129824));
#429654=CARTESIAN_POINT('Ctrl Pts',(-1.79531498602076,1.9657159083651,12.596957478804));
#429655=CARTESIAN_POINT('Ctrl Pts',(-1.79236566635355,1.9684033061119,12.5878468778671));
#429656=CARTESIAN_POINT('Ctrl Pts',(-1.79238467549314,1.97707031947235,
12.5814011370086));
#429657=CARTESIAN_POINT('Ctrl Pts',(-1.81217673858171,1.96585841350007,
12.5928371701607));
#429658=CARTESIAN_POINT('Ctrl Pts',(-1.80390373169794,1.96555440230808,
12.5821692192952));
#429659=CARTESIAN_POINT('Ctrl Pts',(-1.79838469434477,1.97711139364071,
12.5773318885715));
#429660=CARTESIAN_POINT('Ctrl Pts',(-1.82175065299151,1.97038443452168,
12.5893111709658));
#429661=CARTESIAN_POINT('Ctrl Pts',(-1.81150400521162,1.96554038210303,
12.5770542771492));
#429662=CARTESIAN_POINT('Ctrl Pts',(-1.80187416435301,1.97877177809486,
12.5737548217797));
#429663=CARTESIAN_POINT('',(-1.78501496771588,1.99399343503882,12.5737548217797));
#429664=CARTESIAN_POINT('Origin',(-1.79539081682201,2.00558402412337,12.5893111709658));
#429665=CARTESIAN_POINT('Ctrl Pts',(-1.80187416435301,1.97877177809486,
12.5737548217797));
#429666=CARTESIAN_POINT('Ctrl Pts',(-1.80098259957663,1.97831414081431,
12.5746934679442));
#429667=CARTESIAN_POINT('Ctrl Pts',(-1.79991237230225,1.97797070374669,
12.5756680099006));
#429668=CARTESIAN_POINT('Ctrl Pts',(-1.79878626149575,1.97777736952967,
12.5765688348656));
#429669=CARTESIAN_POINT('Ctrl Pts',(-1.79848813612619,1.97772618643599,
12.5768073183026));
#429670=CARTESIAN_POINT('Ctrl Pts',(-1.79818619792037,1.9776852883913,12.5770407398754));
#429671=CARTESIAN_POINT('Ctrl Pts',(-1.79788281576452,1.97765478576167,
12.5772674179684));
#429672=CARTESIAN_POINT('Ctrl Pts',(-1.79663781743491,1.97752961121792,
12.5781976435658));
#429673=CARTESIAN_POINT('Ctrl Pts',(-1.7952966608335,1.97758361541476,12.5790594849312));
#429674=CARTESIAN_POINT('Ctrl Pts',(-1.79395184584885,1.9778614019888,12.5797571720116));
#429675=CARTESIAN_POINT('Ctrl Pts',(-1.79307565053111,1.97804238993011,
12.580211740231));
#429676=CARTESIAN_POINT('Ctrl Pts',(-1.79216188119587,1.97834498302703,
12.5806009430798));
#429677=CARTESIAN_POINT('Ctrl Pts',(-1.7912804326555,1.97876469856761,12.5808812374708));
#429678=CARTESIAN_POINT('Ctrl Pts',(-1.79052297594182,1.97912537345615,
12.5811221033394));
#429679=CARTESIAN_POINT('Ctrl Pts',(-1.7897739284616,1.97958002455874,12.581287365893));
#429680=CARTESIAN_POINT('Ctrl Pts',(-1.7890798940038,1.98011011837575,12.581359338449));
#429681=CARTESIAN_POINT('Ctrl Pts',(-1.78898343754543,1.98018379047029,
12.5813693411482));
#429682=CARTESIAN_POINT('Ctrl Pts',(-1.78888799355128,1.9802588870091,12.5813775999465));
#429683=CARTESIAN_POINT('Ctrl Pts',(-1.78879363518637,1.98033532560312,
12.5813841266931));
#429684=CARTESIAN_POINT('Ctrl Pts',(-1.78863354480788,1.98046501292293,
12.5813952001081));
#429685=CARTESIAN_POINT('Ctrl Pts',(-1.78847589049102,1.98059990507425,
12.5814007534795));
#429686=CARTESIAN_POINT('Ctrl Pts',(-1.78832086911021,1.98074009315269,
12.5814005856065));
#429687=CARTESIAN_POINT('Ctrl Pts',(-1.78761124183826,1.9813818193658,12.5813998171494));
#429688=CARTESIAN_POINT('Ctrl Pts',(-1.78700558985925,1.98208993043124,
12.58127954464));
#429689=CARTESIAN_POINT('Ctrl Pts',(-1.78648486536318,1.98284117347202,
12.5810700125799));
#429690=CARTESIAN_POINT('Ctrl Pts',(-1.78585588946117,1.98374858952942,
12.5808169217085));
#429691=CARTESIAN_POINT('Ctrl Pts',(-1.78536451974292,1.9847285508345,12.5804173076348));
#429692=CARTESIAN_POINT('Ctrl Pts',(-1.78503053923674,1.98568350234591,
12.5799304713245));
#429693=CARTESIAN_POINT('Ctrl Pts',(-1.78461663217488,1.9868669881093,12.5793271277669));
#429694=CARTESIAN_POINT('Ctrl Pts',(-1.78438838901547,1.98807484483448,
12.5785808224116));
#429695=CARTESIAN_POINT('Ctrl Pts',(-1.78432426533182,1.98925026987088,
12.5777485681082));
#429696=CARTESIAN_POINT('Ctrl Pts',(-1.78422871401791,1.99100178195255,
12.576508418016));
#429697=CARTESIAN_POINT('Ctrl Pts',(-1.78449152043175,1.99266615940361,
12.5750928681475));
#429698=CARTESIAN_POINT('Ctrl Pts',(-1.78501496771588,1.99399343503882,
12.5737548217797));
#429699=CARTESIAN_POINT('Ctrl Pts',(-1.78501496771588,1.99399343503882,
12.5737548217797));
#429700=CARTESIAN_POINT('Ctrl Pts',(-1.77087180231227,2.00222596485784,
12.5770542771492));
#429701=CARTESIAN_POINT('Ctrl Pts',(-1.77464733364699,2.01291259190758,
12.5893111709658));
#429702=CARTESIAN_POINT('Ctrl Pts',(-1.79331016725534,2.01732162868452,
12.5508408821982));
#429703=CARTESIAN_POINT('Ctrl Pts',(-1.77912156531826,2.02557688759631,
12.55409748406));
#429704=CARTESIAN_POINT('Ctrl Pts',(-1.78290191326399,2.03627714804518,
12.5663972313419));
#429705=CARTESIAN_POINT('Ctrl Pts',(-1.80159615208642,2.04062742880315,
12.52790050457));
#429706=CARTESIAN_POINT('Ctrl Pts',(-1.78735552806453,2.04888308775984,
12.5311362602938));
#429707=CARTESIAN_POINT('Ctrl Pts',(-1.79114816536659,2.05961813318499,
12.5434568539655));
#429708=CARTESIAN_POINT('Ctrl Pts',(-1.8098736252625,2.06391258029882,12.5049357605811));
#429709=CARTESIAN_POINT('Ctrl Pts',(-1.79557533764729,2.07214922744812,
12.5081700652078));
#429710=CARTESIAN_POINT('Ctrl Pts',(-1.79938674216736,2.08293739341225,
12.5204921097672));
#429711=CARTESIAN_POINT('Ctrl Pts',(-1.80933009243161,2.06238358650823,
12.5064436508395));
#429712=CARTESIAN_POINT('Ctrl Pts',(-1.80856304590672,2.063332526664,12.5062361689309));
#429713=CARTESIAN_POINT('Ctrl Pts',(-1.80772491537427,2.06428663820413,
12.5061871075061));
#429714=CARTESIAN_POINT('Ctrl Pts',(-1.80686303822078,2.06516309950585,
12.5063648335164));
#429715=CARTESIAN_POINT('Ctrl Pts',(-1.80647152045487,2.06556124229146,
12.5064455676329));
#429716=CARTESIAN_POINT('Ctrl Pts',(-1.80606948454061,2.06594876045532,
12.506574497099));
#429717=CARTESIAN_POINT('Ctrl Pts',(-1.8056734392263,2.06630828171125,12.5067492519495));
#429718=CARTESIAN_POINT('Ctrl Pts',(-1.80487757079387,2.0670307536306,12.5071004286051));
#429719=CARTESIAN_POINT('Ctrl Pts',(-1.80407608942265,2.06766613145799,
12.5076537929612));
#429720=CARTESIAN_POINT('Ctrl Pts',(-1.80333502633357,2.06817413868651,
12.5083435010503));
#429721=CARTESIAN_POINT('Ctrl Pts',(-1.8032883719834,2.06820612077748,12.5083869222963));
#429722=CARTESIAN_POINT('Ctrl Pts',(-1.80324194526245,2.06823759168458,
12.5084308732336));
#429723=CARTESIAN_POINT('Ctrl Pts',(-1.8031957576404,2.06826853911802,12.5084753333615));
#429724=CARTESIAN_POINT('Ctrl Pts',(-1.80282527195008,2.06851677838069,
12.508831962269));
#429725=CARTESIAN_POINT('Ctrl Pts',(-1.80246336689796,2.06873744793491,
12.509227847131));
#429726=CARTESIAN_POINT('Ctrl Pts',(-1.8021222615155,2.06892637681182,12.5096423454524));
#429727=CARTESIAN_POINT('Ctrl Pts',(-1.80105338821379,2.06951839629562,
12.5109411997424));
#429728=CARTESIAN_POINT('Ctrl Pts',(-1.80012769271963,2.0698436192065,12.5124831113042));
#429729=CARTESIAN_POINT('Ctrl Pts',(-1.79933802615312,2.0699964105322,12.5140723025008));
#429730=CARTESIAN_POINT('Ctrl Pts',(-1.79926403353094,2.07001072724677,
12.5142212114565));
#429731=CARTESIAN_POINT('Ctrl Pts',(-1.79919122275552,2.07002355688239,
12.5143705582413));
#429732=CARTESIAN_POINT('Ctrl Pts',(-1.79911958222345,2.0700349930612,12.5145201959299));
#429733=CARTESIAN_POINT('Ctrl Pts',(-1.79819925292737,2.07018190780463,
12.5164425148273));
#429734=CARTESIAN_POINT('Ctrl Pts',(-1.79744221046146,2.07011449501529,
12.518463520594));
#429735=CARTESIAN_POINT('Ctrl Pts',(-1.79679585290887,2.06990604191506,
12.5205025929157));
#429736=CARTESIAN_POINT('Ctrl Pts',(-1.79642093990914,2.06978513085462,
12.5216853356836));
#429737=CARTESIAN_POINT('Ctrl Pts',(-1.79608379522748,2.06961744597704,
12.5228750347131));
#429738=CARTESIAN_POINT('Ctrl Pts',(-1.79577915787028,2.06942045884763,
12.5240609649613));
#429739=CARTESIAN_POINT('Ctrl Pts',(-1.79503144182028,2.06893696450648,
12.5269717671327));
#429740=CARTESIAN_POINT('Ctrl Pts',(-1.79446416096251,2.06825460725651,
12.5299036066169));
#429741=CARTESIAN_POINT('Ctrl Pts',(-1.79402045261618,2.06743877943794,
12.532813300402));
#429742=CARTESIAN_POINT('Ctrl Pts',(-1.79380744677358,2.0670471345808,12.5342101228452));
#429743=CARTESIAN_POINT('Ctrl Pts',(-1.79362364510772,2.06662496890918,
12.5356023438238));
#429744=CARTESIAN_POINT('Ctrl Pts',(-1.79346640956079,2.066179914539,12.5369868989719));
#429745=CARTESIAN_POINT('Origin',(-6.03418914296824,14.0854309020258,-1.24015958218552));
#429746=CARTESIAN_POINT('Ctrl Pts',(-1.8727871381517,1.99451163833927,12.5369868989719));
#429747=CARTESIAN_POINT('Ctrl Pts',(-1.88664208027583,2.00109372633821,
12.5369868989719));
#429748=CARTESIAN_POINT('Ctrl Pts',(-1.8976089644341,1.99036941957516,12.5369868989719));
#429749=CARTESIAN_POINT('Ctrl Pts',(-1.87747067886539,1.99673658170076,
12.5218025310016));
#429750=CARTESIAN_POINT('Ctrl Pts',(-1.88913914752845,1.9986081325992,12.5216901060418));
#429751=CARTESIAN_POINT('Ctrl Pts',(-1.89757554526698,1.99040212260739,
12.5161920673678));
#429752=CARTESIAN_POINT('Ctrl Pts',(-1.87854581061836,2.00266786848435,
12.5042015548895));
#429753=CARTESIAN_POINT('Ctrl Pts',(-1.88497583778361,2.00248871583569,
12.4980677368514));
#429754=CARTESIAN_POINT('Ctrl Pts',(-1.88992043201053,1.99782590899263,
12.4907278922777));
#429755=CARTESIAN_POINT('Ctrl Pts',(-1.86741940766348,2.00990956248433,
12.5064636261921));
#429756=CARTESIAN_POINT('Ctrl Pts',(-1.87187279807295,2.01470276101957,
12.4999376786892));
#429757=CARTESIAN_POINT('Ctrl Pts',(-1.87181840638433,2.01464421906876,
12.4906970594712));
#429758=CARTESIAN_POINT('Origin',(-1.88222754715265,1.97464008384812,12.5369868989719));
#429759=CARTESIAN_POINT('Origin',(-1.88222754715265,1.97464008384812,14.));
#429760=CARTESIAN_POINT('Origin',(-1.88222754715265,1.97464008384812,13.7435492065112));
#429761=CARTESIAN_POINT('Ctrl Pts',(-1.8504401483295,1.98394722252162,13.793642941384));
#429762=CARTESIAN_POINT('Ctrl Pts',(-1.86020353239528,1.98859292490015,
13.8071662555867));
#429763=CARTESIAN_POINT('Ctrl Pts',(-1.86970216314701,1.97445802491901,
13.8103758687955));
#429764=CARTESIAN_POINT('Ctrl Pts',(-1.86546673928909,1.9910509728942,13.7804579775006));
#429765=CARTESIAN_POINT('Ctrl Pts',(-1.87751822992994,1.99677419271026,
13.7901904343352));
#429766=CARTESIAN_POINT('Ctrl Pts',(-1.88830647349234,1.98529073830824,
13.7927914348262));
#429767=CARTESIAN_POINT('Ctrl Pts',(-1.87431345891751,1.99523321804838,
13.7597120340895));
#429768=CARTESIAN_POINT('Ctrl Pts',(-1.88826288574537,2.00185141879679,
13.7635825532445));
#429769=CARTESIAN_POINT('Ctrl Pts',(-1.89929027662885,1.99165668650768,
13.7651073818884));
#429770=CARTESIAN_POINT('Ctrl Pts',(-1.87258106864775,1.99441423868393,
13.7381884353898));
#429771=CARTESIAN_POINT('Ctrl Pts',(-1.88620359787057,2.00087834018372,
13.7368803041982));
#429772=CARTESIAN_POINT('Ctrl Pts',(-1.89713956942145,1.9904096170831,13.7363986145813));
#429773=CARTESIAN_POINT('Origin',(-1.86348895370616,1.96578150581787,13.7902182540695));
#429774=CARTESIAN_POINT('Ctrl Pts',(-1.82174709473251,1.97038275153282,
13.8235227101244));
#429775=CARTESIAN_POINT('Ctrl Pts',(-1.83213931246737,1.97530052530466,
13.8358800583119));
#429776=CARTESIAN_POINT('Ctrl Pts',(-1.84180085423239,1.96183647465935,
13.8390832900376));
#429777=CARTESIAN_POINT('Ctrl Pts',(-1.83253041420221,1.97548051285612,
13.8124254819053));
#429778=CARTESIAN_POINT('Ctrl Pts',(-1.84294281359559,1.9804078366235,13.8247886449158));
#429779=CARTESIAN_POINT('Ctrl Pts',(-1.85260271523091,1.966916836605,13.8279860620657));
#429780=CARTESIAN_POINT('Ctrl Pts',(-1.8433089009389,1.98057598952865,13.8013225099954));
#429781=CARTESIAN_POINT('Ctrl Pts',(-1.85373656815285,1.98551054019794,
13.8136962257787));
#429782=CARTESIAN_POINT('Ctrl Pts',(-1.86339946013736,1.97199509187472,
13.8168830918626));
#429783=CARTESIAN_POINT('Ctrl Pts',(-1.85408274297684,1.98566927044266,
13.7902140179785));
#429784=CARTESIAN_POINT('Ctrl Pts',(-1.86452108533012,1.99060887674889,
13.802602731458));
#429785=CARTESIAN_POINT('Ctrl Pts',(-1.87419128919226,1.97707132491017,
13.8057746032558));
#429786=CARTESIAN_POINT('Origin',(-1.83115329419695,1.950494981579,13.8235269408515));
#429787=CARTESIAN_POINT('Ctrl Pts',(-1.77464733364699,2.01291259190758,
13.8235269408515));
#429788=CARTESIAN_POINT('Ctrl Pts',(-1.77858060311757,2.02404569614956,
13.8362179249168));
#429789=CARTESIAN_POINT('Ctrl Pts',(-1.76361004955423,2.03226430491651,
13.8391868794938));
#429790=CARTESIAN_POINT('Ctrl Pts',(-1.77104856328642,2.00272628612134,
13.8400110824519));
#429791=CARTESIAN_POINT('Ctrl Pts',(-1.77097647272219,2.0127919041258,13.8494522556836));
#429792=CARTESIAN_POINT('Ctrl Pts',(-1.75779342922683,2.0154630933057,13.85569149686));
#429793=CARTESIAN_POINT('Ctrl Pts',(-1.77238537069517,1.9864901944735,13.8586819406588));
#429794=CARTESIAN_POINT('Ctrl Pts',(-1.76916312868933,1.98941819722124,
13.868010383617));
#429795=CARTESIAN_POINT('Ctrl Pts',(-1.76015806342466,1.98852283898479,
13.8744918421245));
#429796=CARTESIAN_POINT('Ctrl Pts',(-1.79557460267115,1.96548231456356,
13.8587686893867));
#429797=CARTESIAN_POINT('Ctrl Pts',(-1.79876812888534,1.96258032933977,
13.8680909899357));
#429798=CARTESIAN_POINT('Ctrl Pts',(-1.79876305223794,1.95355279502892,
13.8745789365163));
#429799=CARTESIAN_POINT('Ctrl Pts',(-1.81196783463268,1.96575965517686,
13.8400379222776));
#429800=CARTESIAN_POINT('Ctrl Pts',(-1.82198659935692,1.9667054814338,13.8494748685453));
#429801=CARTESIAN_POINT('Ctrl Pts',(-1.82598547301851,1.95386920024712,
13.8557104837033));
#429802=CARTESIAN_POINT('Ctrl Pts',(-1.82175065299418,1.9703844345157,13.8235269408542));
#429803=CARTESIAN_POINT('Ctrl Pts',(-1.83242539604766,1.9754308668726,13.8362179249195));
#429804=CARTESIAN_POINT('Ctrl Pts',(-1.84212563534195,1.9613749655607,13.8391868794965));
#429805=CARTESIAN_POINT('Origin',(-1.75390385047197,2.02024115969178,13.8235269408515));
#429806=CARTESIAN_POINT('Ctrl Pts',(-1.78656057909098,2.04663299000219,
13.7902140241682));
#429807=CARTESIAN_POINT('Ctrl Pts',(-1.79041164108685,2.05752004272074,
13.8026027327198));
#429808=CARTESIAN_POINT('Ctrl Pts',(-1.7759598069398,2.06576154877605,13.8057746032556));
#429809=CARTESIAN_POINT('Ctrl Pts',(-1.78259079511043,2.03539653157572,
13.8013225161808));
#429810=CARTESIAN_POINT('Ctrl Pts',(-1.78643791473303,2.04627244985853,
13.8136962270464));
#429811=CARTESIAN_POINT('Ctrl Pts',(-1.77200881372497,2.05450893268876,
13.8168830918628));
#429812=CARTESIAN_POINT('Ctrl Pts',(-1.77861929972028,2.0241552290109,13.8124254880875));
#429813=CARTESIAN_POINT('Ctrl Pts',(-1.78246078463185,2.03501522296646,
13.8247886461867));
#429814=CARTESIAN_POINT('Ctrl Pts',(-1.76805630933336,2.04325122039075,
13.8279860620656));
#429815=CARTESIAN_POINT('Ctrl Pts',(-1.774646023636,2.01290888619809,13.8235227163065));
#429816=CARTESIAN_POINT('Ctrl Pts',(-1.77848006316053,2.02374783098812,
13.8358800595847));
#429817=CARTESIAN_POINT('Ctrl Pts',(-1.76410223015076,2.03198820408291,
13.8390832900376));
#429818=CARTESIAN_POINT('Origin',(-1.76581841007511,2.05396527522747,13.7902182540695));
#429819=CARTESIAN_POINT('Ctrl Pts',(-1.79337648870707,2.06592547671255,
13.7382347919292));
#429820=CARTESIAN_POINT('Ctrl Pts',(-1.79842595099843,2.08014591268695,
13.7369371795942));
#429821=CARTESIAN_POINT('Ctrl Pts',(-1.7868838327189,2.08996035524074,13.7364597369711));
#429822=CARTESIAN_POINT('Ctrl Pts',(-1.79400659888214,2.06770899995365,
13.7595490285574));
#429823=CARTESIAN_POINT('Ctrl Pts',(-1.79917558954875,2.08226905977173,
13.7633824266926));
#429824=CARTESIAN_POINT('Ctrl Pts',(-1.78789325567977,2.09219894410019,
13.7648920890506));
#429825=CARTESIAN_POINT('Ctrl Pts',(-1.79079307151705,2.05861312913077,
13.7803806590111));
#429826=CARTESIAN_POINT('Ctrl Pts',(-1.79526915081292,2.07120525365933,
13.7901039518744));
#429827=CARTESIAN_POINT('Ctrl Pts',(-1.78275049177969,2.08078484746259,
13.7926933640892));
#429828=CARTESIAN_POINT('Ctrl Pts',(-1.78520724353435,2.04280247521258,
13.7936647693663));
#429829=CARTESIAN_POINT('Ctrl Pts',(-1.78883828900845,2.05299015604334,
13.8072068914933));
#429830=CARTESIAN_POINT('Ctrl Pts',(-1.77378853185383,2.06099946808836,
13.8104111085397));
#429831=CARTESIAN_POINT('Origin',(-1.77272292638577,2.0735084823232,13.7435492065112));
#429832=CARTESIAN_POINT('Origin',(-1.77272292638577,2.0735084823232,14.));
#429833=CARTESIAN_POINT('Origin',(-1.77272292638577,2.0735084823232,12.5369868989719));
#429834=CARTESIAN_POINT('Ctrl Pts',(-1.8093179689984,2.06236976747208,12.506462012331));
#429835=CARTESIAN_POINT('Ctrl Pts',(-1.81363008271914,2.06728497481759,
12.4999388158272));
#429836=CARTESIAN_POINT('Ctrl Pts',(-1.81357906475883,2.06722682146879,
12.4907030323752));
#429837=CARTESIAN_POINT('Ctrl Pts',(-1.80097967178528,2.07269940360991,
12.5042014951932));
#429838=CARTESIAN_POINT('Ctrl Pts',(-1.80014803784357,2.07907509824681,
12.4980716682127));
#429839=CARTESIAN_POINT('Ctrl Pts',(-1.79501064984419,2.08351726098247,
12.4907355092744));
#429840=CARTESIAN_POINT('Ctrl Pts',(-1.79518886065152,2.07102841358646,
12.5218047446509));
#429841=CARTESIAN_POINT('Ctrl Pts',(-1.7958611126822,2.08282107860093,12.5216906929434));
#429842=CARTESIAN_POINT('Ctrl Pts',(-1.78684570981034,2.09037708716282,
12.5161988840775));
#429843=CARTESIAN_POINT('Ctrl Pts',(-1.7934535808863,2.06614370371284,12.5369868989719));
#429844=CARTESIAN_POINT('Ctrl Pts',(-1.79858545574804,2.0805890971628,12.5369868989719));
#429845=CARTESIAN_POINT('Ctrl Pts',(-1.78681109778457,2.09040592078701,
12.5369868989719));
#429846=CARTESIAN_POINT('Origin',(-3.45247261328837E-31,-1.32797438156907E-31,
12.5));
#429847=CARTESIAN_POINT('Origin',(-1.93281340425162,1.86156455859733,12.5));
#429848=CARTESIAN_POINT('',(-1.93281340425162,1.86156455859733,12.5893111709658));
#429849=CARTESIAN_POINT('',(-1.93281340425162,1.86156455859733,13.8235269408515));
#429850=CARTESIAN_POINT('',(-1.93281340425162,1.86156455859733,12.5));
#429851=CARTESIAN_POINT('',(-1.94743714763615,1.89420531270359,13.7902182540695));
#429852=CARTESIAN_POINT('',(-1.93281340425162,1.86156455859733,13.8235269408515));
#429853=CARTESIAN_POINT('',(-1.95591164254695,1.91312070921219,13.7435492065112));
#429854=CARTESIAN_POINT('Origin',(-1.92803096359008,1.85088917153589,13.7445212918708));
#429855=CARTESIAN_POINT('',(-1.95591164254695,1.91312070921219,12.5369868989719));
#429856=CARTESIAN_POINT('',(-1.95591164254695,1.91312070921219,12.5));
#429857=CARTESIAN_POINT('Ctrl Pts',(-1.95591164254695,1.91312070921219,
12.5369868989719));
#429858=CARTESIAN_POINT('Ctrl Pts',(-1.94821784526522,1.89594785964742,
12.5544431401645));
#429859=CARTESIAN_POINT('Ctrl Pts',(-1.94051854517519,1.87876272760421,
12.5718848856037));
#429860=CARTESIAN_POINT('Ctrl Pts',(-1.93281340425162,1.86156455859733,
12.5893111709658));
#429861=CARTESIAN_POINT('Origin',(-2.23366448875944,1.912215797747,12.5));
#429862=CARTESIAN_POINT('',(-2.02916590912711,1.83524028800144,13.7435492065112));
#429863=CARTESIAN_POINT('',(-2.009767610456,1.82793855548531,13.7902182540695));
#429864=CARTESIAN_POINT('Origin',(-1.9587922342461,1.80875086442513,13.7418732680437));
#429865=CARTESIAN_POINT('',(-1.97629355154766,1.8153385523344,13.8235269408515));
#429866=CARTESIAN_POINT('',(-2.009767610456,1.82793855548531,13.7902182540695));
#429867=CARTESIAN_POINT('',(-1.97629355154766,1.8153385523344,12.5893111709658));
#429868=CARTESIAN_POINT('',(-1.97629355154766,1.8153385523344,12.5));
#429869=CARTESIAN_POINT('',(-2.02916590912711,1.83524028800144,12.5369868989719));
#429870=CARTESIAN_POINT('Ctrl Pts',(-1.97629355154766,1.8153385523344,12.5893111709658));
#429871=CARTESIAN_POINT('Ctrl Pts',(-1.99393078261707,1.82197739967754,
12.5718848856037));
#429872=CARTESIAN_POINT('Ctrl Pts',(-2.01155464389458,1.82861121448428,
12.5544431401645));
#429873=CARTESIAN_POINT('Ctrl Pts',(-2.02916590912711,1.83524028800144,
12.5369868989719));
#429874=CARTESIAN_POINT('',(-2.02916590912711,1.83524028800144,12.5));
#429875=CARTESIAN_POINT('Origin',(-1.96418389587109,1.84750991948588,12.5));
#429876=CARTESIAN_POINT('',(-1.93839157959151,1.82478665842783,13.8587068136939));
#429877=CARTESIAN_POINT('Ctrl Pts',(-1.97629355154985,1.81533855232817,
13.8235269408542));
#429878=CARTESIAN_POINT('Ctrl Pts',(-1.9746535855036,1.81472125110974,13.8262006681044));
#429879=CARTESIAN_POINT('Ctrl Pts',(-1.97291411482078,1.8142521351586,13.8288634856214));
#429880=CARTESIAN_POINT('Ctrl Pts',(-1.9710837408191,1.81392101509882,13.8314912288862));
#429881=CARTESIAN_POINT('Ctrl Pts',(-1.96919681401769,1.81357966447064,
13.8342001611531));
#429882=CARTESIAN_POINT('Ctrl Pts',(-1.96721127240841,1.81338410064125,
13.8368750301949));
#429883=CARTESIAN_POINT('Ctrl Pts',(-1.96510993147372,1.81335969994498,
13.8394886372969));
#429884=CARTESIAN_POINT('Ctrl Pts',(-1.9649476398162,1.81335781542002,13.8396904925131));
#429885=CARTESIAN_POINT('Ctrl Pts',(-1.96478465336429,1.81335697362844,
13.8398919674349));
#429886=CARTESIAN_POINT('Ctrl Pts',(-1.96462096309497,1.81335719765099,
13.8400930404591));
#429887=CARTESIAN_POINT('Ctrl Pts',(-1.96207055857344,1.81336068807305,
13.8432258934518));
#429888=CARTESIAN_POINT('Ctrl Pts',(-1.959362309431,1.81362176941183,13.8462331177034));
#429889=CARTESIAN_POINT('Ctrl Pts',(-1.95659380083772,1.81422794774577,
13.8489036603661));
#429890=CARTESIAN_POINT('Ctrl Pts',(-1.95568791260724,1.81442629635108,
13.849777493004));
#429891=CARTESIAN_POINT('Ctrl Pts',(-1.95477580610192,1.81466168262824,
13.85061494757));
#429892=CARTESIAN_POINT('Ctrl Pts',(-1.95386157132197,1.81493741527541,
13.8514076489583));
#429893=CARTESIAN_POINT('Ctrl Pts',(-1.95192783290997,1.81552062959076,
13.8530843267192));
#429894=CARTESIAN_POINT('Ctrl Pts',(-1.94979548305156,1.81634446585388,
13.8546805203176));
#429895=CARTESIAN_POINT('Ctrl Pts',(-1.94763745613948,1.81748838573059,
13.8559412814273));
#429896=CARTESIAN_POINT('Ctrl Pts',(-1.94734864215218,1.81764147930829,
13.8561100121513));
#429897=CARTESIAN_POINT('Ctrl Pts',(-1.94705938483413,1.81780023092866,
13.8562727473908));
#429898=CARTESIAN_POINT('Ctrl Pts',(-1.94677010569243,1.81796475554049,
13.8564289040185));
#429899=CARTESIAN_POINT('Ctrl Pts',(-1.94545822808503,1.81871087277817,
13.8571370725437));
#429900=CARTESIAN_POINT('Ctrl Pts',(-1.94412396791914,1.81959081149731,
13.8577210840554));
#429901=CARTESIAN_POINT('Ctrl Pts',(-1.94283534565652,1.82059486815531,
13.8581177131616));
#429902=CARTESIAN_POINT('Ctrl Pts',(-1.94247242527434,1.82087764506878,
13.8582294175695));
#429903=CARTESIAN_POINT('Ctrl Pts',(-1.94211304519712,1.82117010798605,
13.8583265086086));
#429904=CARTESIAN_POINT('Ctrl Pts',(-1.94175850480154,1.82147165963533,
13.8584082369006));
#429905=CARTESIAN_POINT('Ctrl Pts',(-1.94124912532684,1.82190490849107,
13.8585256585398));
#429906=CARTESIAN_POINT('Ctrl Pts',(-1.94074361261994,1.82236255089946,
13.8586122832068));
#429907=CARTESIAN_POINT('Ctrl Pts',(-1.94025562842169,1.82283328406048,
13.8586682984299));
#429908=CARTESIAN_POINT('Ctrl Pts',(-1.93986528943541,1.82320982392702,
13.8587131050557));
#429909=CARTESIAN_POINT('Ctrl Pts',(-1.93948169182359,1.82359872992462,
13.8587357943552));
#429910=CARTESIAN_POINT('Ctrl Pts',(-1.939105150568,1.82400040390811,13.8587355499465));
#429911=CARTESIAN_POINT('Ctrl Pts',(-1.93886178297736,1.82426001537999,
13.8587353919793));
#429912=CARTESIAN_POINT('Ctrl Pts',(-1.93862396660077,1.82452212662797,
13.8587257282814));
#429913=CARTESIAN_POINT('Ctrl Pts',(-1.93839157959151,1.82478665842783,
13.8587068136939));
#429914=CARTESIAN_POINT('Ctrl Pts',(-1.93839157959151,1.82478665842783,
13.8587068136939));
#429915=CARTESIAN_POINT('Ctrl Pts',(-1.93762727138672,1.82565668909649,
13.8586446046466));
#429916=CARTESIAN_POINT('Ctrl Pts',(-1.93692162061559,1.82655287156429,
13.858482427929));
#429917=CARTESIAN_POINT('Ctrl Pts',(-1.93627093367604,1.82747268724808,
13.8582284286032));
#429918=CARTESIAN_POINT('Ctrl Pts',(-1.93560340456708,1.82841631114229,
13.8579678548414));
#429919=CARTESIAN_POINT('Ctrl Pts',(-1.93499334126151,1.82938799708295,
13.857615680862));
#429920=CARTESIAN_POINT('Ctrl Pts',(-1.9344565887205,1.83034428481017,13.8571944833187));
#429921=CARTESIAN_POINT('Ctrl Pts',(-1.93311706785987,1.83273079863454,
13.8561433417727));
#429922=CARTESIAN_POINT('Ctrl Pts',(-1.93216728836863,1.83513069840862,
13.8546163505474));
#429923=CARTESIAN_POINT('Ctrl Pts',(-1.93151232388946,1.83736028096605,
13.8528973491086));
#429924=CARTESIAN_POINT('Ctrl Pts',(-1.93139267154222,1.83776759280487,
13.8525833129072));
#429925=CARTESIAN_POINT('Ctrl Pts',(-1.93128271965864,1.83816924780281,
13.8522628768812));
#429926=CARTESIAN_POINT('Ctrl Pts',(-1.9311817215891,1.83856418747303,13.851937733538));
#429927=CARTESIAN_POINT('Ctrl Pts',(-1.93056494039128,1.84097602924366,
13.8499521282529));
#429928=CARTESIAN_POINT('Ctrl Pts',(-1.93022473518864,1.84337813334817,
13.847639871647));
#429929=CARTESIAN_POINT('Ctrl Pts',(-1.9300994390469,1.84563298801171,13.8452109780794));
#429930=CARTESIAN_POINT('Ctrl Pts',(-1.93004306571924,1.846647493798,13.8441181685877));
#429931=CARTESIAN_POINT('Ctrl Pts',(-1.93002950992493,1.84763240256716,
13.8430021611332));
#429932=CARTESIAN_POINT('Ctrl Pts',(-1.93005044753876,1.84857709180739,
13.8418824960098));
#429933=CARTESIAN_POINT('Ctrl Pts',(-1.93009978756041,1.8508032761255,13.8392439765549));
#429934=CARTESIAN_POINT('Ctrl Pts',(-1.93033925412197,1.85291261771184,
13.8364981347964));
#429935=CARTESIAN_POINT('Ctrl Pts',(-1.93073547840514,1.85491455511104,
13.8336931113419));
#429936=CARTESIAN_POINT('Ctrl Pts',(-1.93112137569438,1.85686431500308,
13.8309611966328));
#429937=CARTESIAN_POINT('Ctrl Pts',(-1.93165690626502,1.85871404064352,
13.8281701127186));
#429938=CARTESIAN_POINT('Ctrl Pts',(-1.93234437736132,1.86045131859234,
13.8253580685121));
#429939=CARTESIAN_POINT('Ctrl Pts',(-1.93249342183694,1.86082796232657,
13.8247484142933));
#429940=CARTESIAN_POINT('Ctrl Pts',(-1.93264970608777,1.86119917803961,
13.8241378483365));
#429941=CARTESIAN_POINT('Ctrl Pts',(-1.93281340425162,1.86156455859733,
13.8235269408515));
#429942=CARTESIAN_POINT('',(-1.93922933835866,1.82386963219822,12.5969504640361));
#429943=CARTESIAN_POINT('Origin',(-1.96420786145421,1.84753273030865,12.584524458991));
#429944=CARTESIAN_POINT('Origin',(-1.96420786145421,1.84753273030865,12.584524458991));
#429945=CARTESIAN_POINT('Ctrl Pts',(-1.97629355154766,1.8153385523344,12.5893111709658));
#429946=CARTESIAN_POINT('Ctrl Pts',(-1.96568616340087,1.81134581501986,
12.5770542771492));
#429947=CARTESIAN_POINT('Ctrl Pts',(-1.95716684665092,1.8253181060621,12.5737548217797));
#429948=CARTESIAN_POINT('Ctrl Pts',(-1.99948834947938,1.82406932883881,
12.5663937883685));
#429949=CARTESIAN_POINT('Ctrl Pts',(-1.98886743013587,1.82007149823336,
12.5540940315303));
#429950=CARTESIAN_POINT('Ctrl Pts',(-1.98032445548272,1.8340887582862,12.5508374392248));
#429951=CARTESIAN_POINT('Ctrl Pts',(-2.02265974414446,1.83279129609681,
12.5434499600945));
#429952=CARTESIAN_POINT('Ctrl Pts',(-2.01200429240993,1.82878046712038,
12.5311293540533));
#429953=CARTESIAN_POINT('Ctrl Pts',(-2.00345985673006,1.84284973801384,
12.5278936106989));
#429954=CARTESIAN_POINT('Ctrl Pts',(-2.04580956875261,1.84150514414865,
12.5204817579905));
#429955=CARTESIAN_POINT('Ctrl Pts',(-2.03510137981401,1.83747446430979,
12.5081597038247));
#429956=CARTESIAN_POINT('Ctrl Pts',(-2.02657478136005,1.85160178407327,
12.5049254088044));
#429957=CARTESIAN_POINT('Ctrl Pts',(-2.02916590912711,1.83524028800144,
12.5369868989719));
#429958=CARTESIAN_POINT('Ctrl Pts',(-2.03003769910788,1.8355684394911,12.5342545179733));
#429959=CARTESIAN_POINT('Ctrl Pts',(-2.03082575001755,1.83599836143416,
12.5314872231885));
#429960=CARTESIAN_POINT('Ctrl Pts',(-2.0314588978002,1.83655490882249,12.5287124745063));
#429961=CARTESIAN_POINT('Ctrl Pts',(-2.03202990189724,1.83705683088183,
12.5262100684184));
#429962=CARTESIAN_POINT('Ctrl Pts',(-2.03247369266208,1.83766197391845,
12.5237004536639));
#429963=CARTESIAN_POINT('Ctrl Pts',(-2.03274443395007,1.83841993152044,
12.5212220730815));
#429964=CARTESIAN_POINT('Ctrl Pts',(-2.03295170982702,1.83900021363332,
12.5193246583486));
#429965=CARTESIAN_POINT('Ctrl Pts',(-2.03305943711478,1.83967721249193,
12.5174178313691));
#429966=CARTESIAN_POINT('Ctrl Pts',(-2.03297649481723,1.84048485429296,
12.5155812248348));
#429967=CARTESIAN_POINT('Ctrl Pts',(-2.03294116095266,1.84082891404129,
12.5147988205794));
#429968=CARTESIAN_POINT('Ctrl Pts',(-2.03287146396674,1.84119706051606,
12.5140295443047));
#429969=CARTESIAN_POINT('Ctrl Pts',(-2.03276198451743,1.84159328898931,
12.5132817086137));
#429970=CARTESIAN_POINT('Ctrl Pts',(-2.03259630218093,1.842192927183,12.5121499604604));
#429971=CARTESIAN_POINT('Ctrl Pts',(-2.03232903596763,1.84286792487787,
12.5110494206568));
#429972=CARTESIAN_POINT('Ctrl Pts',(-2.03192299023836,1.843616442733,12.5100666561695));
#429973=CARTESIAN_POINT('Ctrl Pts',(-2.03168983971566,1.84404623996173,
12.5095023550641));
#429974=CARTESIAN_POINT('Ctrl Pts',(-2.03140766556882,1.84450493167331,
12.5089719619137));
#429975=CARTESIAN_POINT('Ctrl Pts',(-2.03107631679997,1.84498057363984,
12.5085043804652));
#429976=CARTESIAN_POINT('Ctrl Pts',(-2.03059143103796,1.84567661370114,
12.5078201359221));
#429977=CARTESIAN_POINT('Ctrl Pts',(-2.0299861858922,1.84642844900638,12.5072563000949));
#429978=CARTESIAN_POINT('Ctrl Pts',(-2.02929501341177,1.84717980736874,
12.5068768744332));
#429979=CARTESIAN_POINT('Ctrl Pts',(-2.0287966304729,1.84772158847168,12.5066032824114));
#429980=CARTESIAN_POINT('Ctrl Pts',(-2.02824485881439,1.84827268053072,
12.5064197834844));
#429981=CARTESIAN_POINT('Ctrl Pts',(-2.0276723374415,1.84880413803124,12.5063282718343));
#429982=CARTESIAN_POINT('Ctrl Pts',(-2.0268366334852,1.84957990144691,12.5061946931565));
#429983=CARTESIAN_POINT('Ctrl Pts',(-2.0259395786605,1.8503311890892,12.5062515701262));
#429984=CARTESIAN_POINT('Ctrl Pts',(-2.02504677507729,1.85102323054787,
12.5064436508398));
#429985=CARTESIAN_POINT('',(-1.95716684665092,1.8253181060621,12.5737548217797));
#429986=CARTESIAN_POINT('Origin',(-1.96854337191465,1.83592822731135,12.5893111709658));
#429987=CARTESIAN_POINT('Ctrl Pts',(-2.02504677507729,1.85102323054787,
12.5064436508398));
#429988=CARTESIAN_POINT('Ctrl Pts',(-2.0149986119639,1.84721865359398,12.5164271754438));
#429989=CARTESIAN_POINT('Ctrl Pts',(-2.00494653974534,1.84341237310856,
12.5264061185523));
#429990=CARTESIAN_POINT('Ctrl Pts',(-1.99489042041103,1.83960432997982,
12.536380305637));
#429991=CARTESIAN_POINT('Ctrl Pts',(-1.98232231084392,1.83484504842325,
12.5488460165097));
#429992=CARTESIAN_POINT('Ctrl Pts',(-1.96974787600632,1.8300830122015,12.5613043021964));
#429993=CARTESIAN_POINT('Ctrl Pts',(-1.95716684665092,1.8253181060621,12.5737548217797));
#429994=CARTESIAN_POINT('Ctrl Pts',(-1.93281340425162,1.86156455859733,
12.5893111709658));
#429995=CARTESIAN_POINT('Ctrl Pts',(-1.9281793763716,1.85122123127162,12.5770542771492));
#429996=CARTESIAN_POINT('Ctrl Pts',(-1.94160445395174,1.84186329523731,
12.5737548217797));
#429997=CARTESIAN_POINT('Ctrl Pts',(-1.92848989654421,1.85191432416395,
12.5928319619712));
#429998=CARTESIAN_POINT('Ctrl Pts',(-1.92834854683296,1.84363100136265,
12.5821634970843));
#429999=CARTESIAN_POINT('Ctrl Pts',(-1.94002089088191,1.83835180760764,
12.5773203894503));
#430000=CARTESIAN_POINT('Ctrl Pts',(-1.92864136216822,1.8351643642385,12.5969440695591));
#430001=CARTESIAN_POINT('Ctrl Pts',(-1.93138213402892,1.8322238350073,12.5878292599214));
#430002=CARTESIAN_POINT('Ctrl Pts',(-1.9400769222157,1.832381798597,12.5813877129824));
#430003=CARTESIAN_POINT('Ctrl Pts',(-1.94956531885574,1.81284031258831,
12.596957478804));
#430004=CARTESIAN_POINT('Ctrl Pts',(-1.94684486067137,1.81575916517382,
12.5878468778671));
#430005=CARTESIAN_POINT('Ctrl Pts',(-1.94757024860912,1.82439579034094,
12.5814011370086));
#430006=CARTESIAN_POINT('Ctrl Pts',(-1.96638258081749,1.8116079541786,12.5928371701607));
#430007=CARTESIAN_POINT('Ctrl Pts',(-1.9581123219472,1.81197928142266,12.5821692192952));
#430008=CARTESIAN_POINT('Ctrl Pts',(-1.95355365081902,1.82394767060053,
12.5773318885715));
#430009=CARTESIAN_POINT('Ctrl Pts',(-1.97629355154768,1.81533855233435,
12.5893111709658));
#430010=CARTESIAN_POINT('Ctrl Pts',(-1.96568616340088,1.81134581501981,
12.5770542771492));
#430011=CARTESIAN_POINT('Ctrl Pts',(-1.95716684665094,1.82531810606205,
12.5737548217797));
#430012=CARTESIAN_POINT('',(-1.94160445395174,1.84186329523731,12.5737548217797));
#430013=CARTESIAN_POINT('Origin',(-1.95289051888808,1.852569589566,12.5893111709658));
#430014=CARTESIAN_POINT('Ctrl Pts',(-1.95716684665094,1.82531810606205,
12.5737548217797));
#430015=CARTESIAN_POINT('Ctrl Pts',(-1.95624094679594,1.82493466233796,
12.5746934679442));
#430016=CARTESIAN_POINT('Ctrl Pts',(-1.95514628730521,1.82467960148722,
12.5756680099006));
#430017=CARTESIAN_POINT('Ctrl Pts',(-1.954008165006,1.82457869905889,12.5765688348656));
#430018=CARTESIAN_POINT('Ctrl Pts',(-1.95370685972672,1.82455198625801,
12.5768073183026));
#430019=CARTESIAN_POINT('Ctrl Pts',(-1.95340259262505,1.82453583506502,
12.5770407398754));
#430020=CARTESIAN_POINT('Ctrl Pts',(-1.95309773370081,1.82453016239254,
12.5772674179684));
#430021=CARTESIAN_POINT('Ctrl Pts',(-1.95184667511306,1.82450688327862,
12.5781976435658));
#430022=CARTESIAN_POINT('Ctrl Pts',(-1.950514382943,1.82467002449465,12.5790594849312));
#430023=CARTESIAN_POINT('Ctrl Pts',(-1.94919668490389,1.82505650166269,
12.5797571720116));
#430024=CARTESIAN_POINT('Ctrl Pts',(-1.94833815725122,1.82530830543415,
12.580211740231));
#430025=CARTESIAN_POINT('Ctrl Pts',(-1.9474520925546,1.82568437236135,12.5806009430798));
#430026=CARTESIAN_POINT('Ctrl Pts',(-1.94660778767454,1.8261745375721,12.5808812374708));
#430027=CARTESIAN_POINT('Ctrl Pts',(-1.94588224968734,1.82659575209876,
12.5811221033394));
#430028=CARTESIAN_POINT('Ctrl Pts',(-1.94517275288646,1.82710994471076,
12.581287365893));
#430029=CARTESIAN_POINT('Ctrl Pts',(-1.9445242353383,1.82769484493574,12.581359338449));
#430030=CARTESIAN_POINT('Ctrl Pts',(-1.94443410479048,1.82777613398928,
12.5813693411482));
#430031=CARTESIAN_POINT('Ctrl Pts',(-1.94434509944343,1.82785876022213,
12.5813775999465));
#430032=CARTESIAN_POINT('Ctrl Pts',(-1.94425728550322,1.82794263555575,
12.5813841266931));
#430033=CARTESIAN_POINT('Ctrl Pts',(-1.94410829853279,1.82808494020376,
12.5813952001081));
#430034=CARTESIAN_POINT('Ctrl Pts',(-1.94396216376027,1.82823223380299,
12.5814007534795));
#430035=CARTESIAN_POINT('Ctrl Pts',(-1.94381908483015,1.82838459109884,
12.5814005856065));
#430036=CARTESIAN_POINT('Ctrl Pts',(-1.94316412542827,1.82908202323144,
12.5813998171494));
#430037=CARTESIAN_POINT('Ctrl Pts',(-1.94261820633187,1.82983714437461,
12.58127954464));
#430038=CARTESIAN_POINT('Ctrl Pts',(-1.94216044778564,1.83062833159675,
12.5810700125799));
#430039=CARTESIAN_POINT('Ctrl Pts',(-1.94160752758177,1.83158399567722,
12.5808169217085));
#430040=CARTESIAN_POINT('Ctrl Pts',(-1.9411976687996,1.83260074743558,12.5804173076348));
#430041=CARTESIAN_POINT('Ctrl Pts',(-1.94094263699953,1.8335797439364,12.5799304713245));
#430042=CARTESIAN_POINT('Ctrl Pts',(-1.94062657225593,1.83479302901661,
12.5793271277669));
#430043=CARTESIAN_POINT('Ctrl Pts',(-1.9404975400931,1.83601547063458,12.5785808224116));
#430044=CARTESIAN_POINT('Ctrl Pts',(-1.9405294378283,1.83719221121665,12.5777485681082));
#430045=CARTESIAN_POINT('Ctrl Pts',(-1.9405769689484,1.83894568360549,12.576508418016));
#430046=CARTESIAN_POINT('Ctrl Pts',(-1.94097456310917,1.84058310181538,
12.5750928681475));
#430047=CARTESIAN_POINT('Ctrl Pts',(-1.94160445395174,1.84186329523731,
12.5737548217797));
#430048=CARTESIAN_POINT('Ctrl Pts',(-1.94160445395174,1.84186329523731,
12.5737548217797));
#430049=CARTESIAN_POINT('Ctrl Pts',(-1.9281793763716,1.85122123127162,12.5770542771492));
#430050=CARTESIAN_POINT('Ctrl Pts',(-1.93281340425162,1.86156455859733,
12.5893111709658));
#430051=CARTESIAN_POINT('Ctrl Pts',(-1.95177351624953,1.86443773047174,
12.5508408821982));
#430052=CARTESIAN_POINT('Ctrl Pts',(-1.9383050059543,1.87382202346895,12.55409748406));
#430053=CARTESIAN_POINT('Ctrl Pts',(-1.94294494566708,1.88417854623126,
12.5663972313419));
#430054=CARTESIAN_POINT('Ctrl Pts',(-1.96193156921978,1.88699059777604,
12.52790050457));
#430055=CARTESIAN_POINT('Ctrl Pts',(-1.94841124254629,1.89637952976981,
12.5311362602938));
#430056=CARTESIAN_POINT('Ctrl Pts',(-1.9530662660221,1.90676972006767,12.5434568539655));
#430057=CARTESIAN_POINT('Ctrl Pts',(-1.97207945580243,1.90952357894281,
12.5049357605811));
#430058=CARTESIAN_POINT('Ctrl Pts',(-1.9585001077677,1.91889826250765,12.5081700652078));
#430059=CARTESIAN_POINT('Ctrl Pts',(-1.96317816583218,1.92933986688776,
12.5204921097672));
#430060=CARTESIAN_POINT('Ctrl Pts',(-1.97141310434378,1.90804397572455,
12.5064436508395));
#430061=CARTESIAN_POINT('Ctrl Pts',(-1.97072595753515,1.90905227977293,
12.5062361689309));
#430062=CARTESIAN_POINT('Ctrl Pts',(-1.96996838476096,1.91007153200484,
12.5061871075061));
#430063=CARTESIAN_POINT('Ctrl Pts',(-1.96918081516536,1.91101532794316,
12.5063648335164));
#430064=CARTESIAN_POINT('Ctrl Pts',(-1.96882305247573,1.9114440582741,12.5064455676329));
#430065=CARTESIAN_POINT('Ctrl Pts',(-1.96845394063071,1.91186305666257,
12.506574497099));
#430066=CARTESIAN_POINT('Ctrl Pts',(-1.96808851744449,1.912253663011,12.5067492519495));
#430067=CARTESIAN_POINT('Ctrl Pts',(-1.96735418536714,1.91303860163037,
12.5071004286051));
#430068=CARTESIAN_POINT('Ctrl Pts',(-1.96660716005056,1.9137371934628,12.5076537929612));
#430069=CARTESIAN_POINT('Ctrl Pts',(-1.965909970093,1.91430391386063,12.5083435010503));
#430070=CARTESIAN_POINT('Ctrl Pts',(-1.96586607781866,1.91433959229648,
12.5083869222963));
#430071=CARTESIAN_POINT('Ctrl Pts',(-1.96582237074989,1.91437474269549,
12.5084308732336));
#430072=CARTESIAN_POINT('Ctrl Pts',(-1.96577885931647,1.91440935187388,
12.5084753333615));
#430073=CARTESIAN_POINT('Ctrl Pts',(-1.96542984019117,1.91468696316406,
12.508831962269));
#430074=CARTESIAN_POINT('Ctrl Pts',(-1.96508712596552,1.91493639708005,
12.509227847131));
#430075=CARTESIAN_POINT('Ctrl Pts',(-1.96476255504048,1.91515250056705,
12.5096423454524));
#430076=CARTESIAN_POINT('Ctrl Pts',(-1.96374549341047,1.91582967325188,
12.5109411997424));
#430077=CARTESIAN_POINT('Ctrl Pts',(-1.96284938677816,1.91622926678686,
12.5124831113042));
#430078=CARTESIAN_POINT('Ctrl Pts',(-1.9620748016735,1.91644591486811,12.5140723025008));
#430079=CARTESIAN_POINT('Ctrl Pts',(-1.96200222220081,1.91646621503062,
12.5142212114565));
#430080=CARTESIAN_POINT('Ctrl Pts',(-1.96193069943166,1.91648493673082,
12.5143705582413));
#430081=CARTESIAN_POINT('Ctrl Pts',(-1.96186022943228,1.91650217422513,
12.5145201959299));
#430082=CARTESIAN_POINT('Ctrl Pts',(-1.96095493737149,1.91672361550343,
12.5164425148273));
#430083=CARTESIAN_POINT('Ctrl Pts',(-1.96019491913377,1.91671813301359,
12.5184635205941));
#430084=CARTESIAN_POINT('Ctrl Pts',(-1.95953372141976,1.91656305766488,
12.5205025929157));
#430085=CARTESIAN_POINT('Ctrl Pts',(-1.95915020053821,1.91647310781602,
12.5216853356836));
#430086=CARTESIAN_POINT('Ctrl Pts',(-1.95880050980342,1.91633346131749,
12.5228750347131));
#430087=CARTESIAN_POINT('Ctrl Pts',(-1.95848082982212,1.91616196041923,
12.5240609649613));
#430088=CARTESIAN_POINT('Ctrl Pts',(-1.95769619245825,1.91574102066515,
12.5269717671326));
#430089=CARTESIAN_POINT('Ctrl Pts',(-1.95707518073017,1.91510717255893,
12.5299036066169));
#430090=CARTESIAN_POINT('Ctrl Pts',(-1.95656645124578,1.91433022568954,
12.5328133004019));
#430091=CARTESIAN_POINT('Ctrl Pts',(-1.95632223147083,1.91395724595197,
12.5342101228451));
#430092=CARTESIAN_POINT('Ctrl Pts',(-1.95610463096842,1.9135514665439,12.5356023438238));
#430093=CARTESIAN_POINT('Ctrl Pts',(-1.95591164254695,1.91312070921219,
12.5369868989719));
#430094=CARTESIAN_POINT('Origin',(-7.16189571922773,13.5460285809191,-1.23934284754315));
#430095=CARTESIAN_POINT('Ctrl Pts',(-2.02912680811102,1.83522552753148,
12.5369868989719));
#430096=CARTESIAN_POINT('Ctrl Pts',(-2.04347215033515,1.84065640776932,
12.5369868989719));
#430097=CARTESIAN_POINT('Ctrl Pts',(-2.05352841253022,1.82907388238194,
12.5369868989719));
#430098=CARTESIAN_POINT('Ctrl Pts',(-2.03397611826865,1.83706131552939,
12.5218025310016));
#430099=CARTESIAN_POINT('Ctrl Pts',(-2.04575830983759,1.83797555047574,
12.5216901060418));
#430100=CARTESIAN_POINT('Ctrl Pts',(-2.05349777016335,1.82910920056989,
12.5161920673678));
#430101=CARTESIAN_POINT('Ctrl Pts',(-2.03553112754562,1.8428852332266,12.5042015548895));
#430102=CARTESIAN_POINT('Ctrl Pts',(-2.04192515672187,1.84218256978616,
12.4980677368513));
#430103=CARTESIAN_POINT('Ctrl Pts',(-2.04647323617422,1.83713224771536,
12.4907278922777));
#430104=CARTESIAN_POINT('Ctrl Pts',(-2.02503201206828,1.85100973622055,
12.506463626192));
#430105=CARTESIAN_POINT('Ctrl Pts',(-2.029861274367,1.85542399312139,12.4999376786891));
#430106=CARTESIAN_POINT('Ctrl Pts',(-2.02980229194976,1.85537007939167,
12.4906970594712));
#430107=CARTESIAN_POINT('Origin',(-2.03691608876012,1.8146506130245,12.5369868989719));
#430108=CARTESIAN_POINT('Origin',(-2.03691608876012,1.8146506130245,14.));
#430109=CARTESIAN_POINT('Origin',(-2.03691608876012,1.8146506130245,13.7435492065112));
#430110=CARTESIAN_POINT('Ctrl Pts',(-2.00599307808942,1.82651775106574,
13.793642941384));
#430111=CARTESIAN_POINT('Ctrl Pts',(-2.01610264317258,1.83035218881266,
13.8071662555867));
#430112=CARTESIAN_POINT('Ctrl Pts',(-2.0244175424436,1.8154900949579,13.8103758687955));
#430113=CARTESIAN_POINT('Ctrl Pts',(-2.02154869091056,1.83237305763171,
13.7804579775006));
#430114=CARTESIAN_POINT('Ctrl Pts',(-2.03402657675728,1.83709492553815,
13.7901904343351));
#430115=CARTESIAN_POINT('Ctrl Pts',(-2.04384291518824,1.82477033937984,
13.7927914348262));
#430116=CARTESIAN_POINT('Ctrl Pts',(-2.03070686561534,1.83582029693149,
13.7597120340895));
#430117=CARTESIAN_POINT('Ctrl Pts',(-2.04514932167757,1.84127946837625,
13.7635825532445));
#430118=CARTESIAN_POINT('Ctrl Pts',(-2.05530905450276,1.83021982348751,
13.7651073818884));
#430119=CARTESIAN_POINT('Ctrl Pts',(-2.02891348531008,1.83514524854303,
13.7381884353898));
#430120=CARTESIAN_POINT('Ctrl Pts',(-2.04301757097271,1.84047747868129,
13.7368803041982));
#430121=CARTESIAN_POINT('Ctrl Pts',(-2.05306385586082,1.82915220618717,
13.7363986145813));
#430122=CARTESIAN_POINT('Origin',(-2.01751779008901,1.80734888050836,13.7902182540695));
#430123=CARTESIAN_POINT('Ctrl Pts',(-1.97628986794929,1.81533716497664,
13.8235227101244));
#430124=CARTESIAN_POINT('Ctrl Pts',(-1.98704835065372,1.8193915130399,13.8358800583119));
#430125=CARTESIAN_POINT('Ctrl Pts',(-1.99558029931379,1.80518475756518,
13.8390832900376));
#430126=CARTESIAN_POINT('Ctrl Pts',(-1.98745282168616,1.81953902327544,
13.8124254819052));
#430127=CARTESIAN_POINT('Ctrl Pts',(-1.99823219730958,1.82360124456487,
13.8247886449157));
#430128=CARTESIAN_POINT('Ctrl Pts',(-2.00676031467326,1.80936776307462,
13.8279860620657));
#430129=CARTESIAN_POINT('Ctrl Pts',(-1.9986107725503,1.82373899843805,13.8013225099955));
#430130=CARTESIAN_POINT('Ctrl Pts',(-2.00940595425151,1.8278071781134,13.8136962257787));
#430131=CARTESIAN_POINT('Ctrl Pts',(-2.01793505925043,1.81354908592687,
13.8168830918626));
#430132=CARTESIAN_POINT('Ctrl Pts',(-2.00976391519586,1.82793716373444,
13.7902140179785));
#430133=CARTESIAN_POINT('Ctrl Pts',(-2.02057014859708,1.83200951210152,
13.802602731458));
#430134=CARTESIAN_POINT('Ctrl Pts',(-2.02910473950224,1.81772879396123,
13.8057746032558));
#430135=CARTESIAN_POINT('Origin',(-1.98404373118067,1.79474887735746,13.8235269408515));
#430136=CARTESIAN_POINT('Ctrl Pts',(-1.93281340425162,1.86156455859733,
13.8235269408515));
#430137=CARTESIAN_POINT('Ctrl Pts',(-1.93764103744294,1.87234002037682,
13.8362179249168));
#430138=CARTESIAN_POINT('Ctrl Pts',(-1.92339019007394,1.88175152149634,
13.8391868794938));
#430139=CARTESIAN_POINT('Ctrl Pts',(-1.92839633001593,1.85170548009703,
13.8400110824519));
#430140=CARTESIAN_POINT('Ctrl Pts',(-1.92914492063915,1.8617434816382,13.8494522556837));
#430141=CARTESIAN_POINT('Ctrl Pts',(-1.91622346934972,1.8654803230867,13.85569149686));
#430142=CARTESIAN_POINT('Ctrl Pts',(-1.92840529711048,1.83541445049064,
13.8586819406588));
#430143=CARTESIAN_POINT('Ctrl Pts',(-1.92543243625529,1.83859535318809,
13.868010383617));
#430144=CARTESIAN_POINT('Ctrl Pts',(-1.91638435459405,1.83843697060033,
13.8744918421245));
#430145=CARTESIAN_POINT('Ctrl Pts',(-1.94980503158974,1.8125863348837,13.8587686893867));
#430146=CARTESIAN_POINT('Ctrl Pts',(-1.95275139287244,1.80943370374263,
13.8680909899357));
#430147=CARTESIAN_POINT('Ctrl Pts',(-1.95201050526329,1.80043662160138,
13.8745789365163));
#430148=CARTESIAN_POINT('Ctrl Pts',(-1.96616632225896,1.81152655207678,
13.8400379222776));
#430149=CARTESIAN_POINT('Ctrl Pts',(-1.97622884399063,1.81165260884018,
13.8494748685453));
#430150=CARTESIAN_POINT('Ctrl Pts',(-1.97916813564705,1.79853309399309,
13.8557104837033));
#430151=CARTESIAN_POINT('Ctrl Pts',(-1.97629355154985,1.81533855232817,
13.8235269408542));
#430152=CARTESIAN_POINT('Ctrl Pts',(-1.98734410636231,1.81949810243936,
13.8362179249195));
#430153=CARTESIAN_POINT('Ctrl Pts',(-1.99586638246502,1.80469831142444,
13.8391868794965));
#430154=CARTESIAN_POINT('Origin',(-1.91273628961517,1.87055952762867,13.8235269408515));
#430155=CARTESIAN_POINT('Ctrl Pts',(-1.9474355348438,1.89420171474816,13.7902140241683));
#430156=CARTESIAN_POINT('Ctrl Pts',(-1.95216117861558,1.90473864439274,
13.8026027327198));
#430157=CARTESIAN_POINT('Ctrl Pts',(-1.93842919100838,1.91413068616379,
13.8057746032556));
#430158=CARTESIAN_POINT('Ctrl Pts',(-1.942563084316,1.88332621895825,13.8013225161808));
#430159=CARTESIAN_POINT('Ctrl Pts',(-1.94728389127257,1.89385237255602,
13.8136962270464));
#430160=CARTESIAN_POINT('Ctrl Pts',(-1.93357415172225,1.90323755485449,
13.8168830918628));
#430161=CARTESIAN_POINT('Ctrl Pts',(-1.93768853323095,1.87244603464424,
13.8124254880875));
#430162=CARTESIAN_POINT('Ctrl Pts',(-1.94240242624502,1.88295677618289,
13.8247886461867));
#430163=CARTESIAN_POINT('Ctrl Pts',(-1.92871719089915,1.89233946746664,
13.8279860620656));
#430164=CARTESIAN_POINT('Ctrl Pts',(-1.93281179654987,1.86156097199635,
13.8235227163065));
#430165=CARTESIAN_POINT('Ctrl Pts',(-1.9375165532484,1.872051341277,13.8358800595847));
#430166=CARTESIAN_POINT('Ctrl Pts',(-1.92385822819901,1.88143622207769,
13.8390832900376));
#430167=CARTESIAN_POINT('Origin',(-1.92736003299969,1.90320028173492,13.7902182540695));
#430168=CARTESIAN_POINT('Ctrl Pts',(-1.95580128185251,1.91287444739099,
13.7382347919292));
#430169=CARTESIAN_POINT('Ctrl Pts',(-1.96199304002264,1.92663598798411,
13.7369371795942));
#430170=CARTESIAN_POINT('Ctrl Pts',(-1.9512892953705,1.93735856358153,13.7364597369711));
#430171=CARTESIAN_POINT('Ctrl Pts',(-1.95657466908952,1.9146006762767,13.7595490285574));
#430172=CARTESIAN_POINT('Ctrl Pts',(-1.9629132404103,1.92869096797099,13.7633824266926));
#430173=CARTESIAN_POINT('Ctrl Pts',(-1.95247782533384,1.93950742637888,
13.7648920890506));
#430174=CARTESIAN_POINT('Ctrl Pts',(-1.95263043655764,1.90579700352681,
13.780380659011));
#430175=CARTESIAN_POINT('Ctrl Pts',(-1.95811799711753,1.91798238678324,
13.7901039518744));
#430176=CARTESIAN_POINT('Ctrl Pts',(-1.94642181871712,1.92855049220719,
13.7926933640892));
#430177=CARTESIAN_POINT('Ctrl Pts',(-1.94577447988346,1.89049425509214,
13.7936647693663));
#430178=CARTESIAN_POINT('Ctrl Pts',(-1.95022383391882,1.90035207334026,
13.8072068914933));
#430179=CARTESIAN_POINT('Ctrl Pts',(-1.93587698687609,1.90956142998339,
13.8104111085397));
#430180=CARTESIAN_POINT('Origin',(-1.93583452791049,1.92211567824353,13.7435492065112));
#430181=CARTESIAN_POINT('Origin',(-1.93583452791049,1.92211567824353,14.));
#430182=CARTESIAN_POINT('Origin',(-1.93583452791049,1.92211567824353,12.5369868989719));
#430183=CARTESIAN_POINT('Ctrl Pts',(-1.97139989487055,1.90803119084247,
12.506462012331));
#430184=CARTESIAN_POINT('Ctrl Pts',(-1.97609829541783,1.91257856594105,
12.4999388158272));
#430185=CARTESIAN_POINT('Ctrl Pts',(-1.97604270717779,1.91252476453011,
12.4907030323752));
#430186=CARTESIAN_POINT('Ctrl Pts',(-1.96393130389444,1.91900610460002,
12.5042014951932));
#430187=CARTESIAN_POINT('Ctrl Pts',(-1.96362211544802,1.92542837052573,
12.4980716682127));
#430188=CARTESIAN_POINT('Ctrl Pts',(-1.95886389918542,1.93027449714647,
12.4907355092744));
#430189=CARTESIAN_POINT('Ctrl Pts',(-1.9580235600074,1.91781267952468,12.5218047446509));
#430190=CARTESIAN_POINT('Ctrl Pts',(-1.95965478685134,1.92951131063775,
12.5216906929434));
#430191=CARTESIAN_POINT('Ctrl Pts',(-1.95128526683317,1.93777701623348,
12.5161988840775));
#430192=CARTESIAN_POINT('Ctrl Pts',(-1.95589590504031,1.91308566453063,
12.5369868989719));
#430193=CARTESIAN_POINT('Ctrl Pts',(-1.96218813768246,1.92706469668231,
12.5369868989719));
#430194=CARTESIAN_POINT('Ctrl Pts',(-1.95125312018413,1.93780857511758,
12.5369868989719));
#430195=CARTESIAN_POINT('Origin',(-3.7526671846257E-31,-1.62210662334643E-31,
12.5));
#430196=CARTESIAN_POINT('Origin',(-2.07811692054273,1.69782812028616,12.5));
#430197=CARTESIAN_POINT('',(-2.07811692054273,1.69782812028616,12.5893111709658));
#430198=CARTESIAN_POINT('',(-2.07811692054273,1.69782812028616,13.8235269408515));
#430199=CARTESIAN_POINT('',(-2.07811692054273,1.69782812028616,12.5));
#430200=CARTESIAN_POINT('',(-2.09535252910915,1.72916829412975,13.7902182540695));
#430201=CARTESIAN_POINT('',(-2.07811692054273,1.69782812028616,13.8235269408515));
#430202=CARTESIAN_POINT('',(-2.10534060625466,1.74733000120828,13.7435492065112));
#430203=CARTESIAN_POINT('Origin',(-2.07248024990848,1.68757806800912,13.7445212918717));
#430204=CARTESIAN_POINT('',(-2.10534060625466,1.74733000120828,12.5369868989719));
#430205=CARTESIAN_POINT('',(-2.10534060625466,1.74733000120828,12.5));
#430206=CARTESIAN_POINT('Ctrl Pts',(-2.10534060625466,1.74733000120828,
12.5369868989719));
#430207=CARTESIAN_POINT('Ctrl Pts',(-2.09627266278421,1.73084140878796,
12.5544431401645));
#430208=CARTESIAN_POINT('Ctrl Pts',(-2.08719823367958,1.71434102328811,
12.5718848856037));
#430209=CARTESIAN_POINT('Ctrl Pts',(-2.07811692054273,1.69782812028616,
12.5893111709658));
#430210=CARTESIAN_POINT('Origin',(-2.38209549409917,1.7237886652634,12.5));
#430211=CARTESIAN_POINT('',(-2.1720031479706,1.66373781788871,13.7435492065112));
#430212=CARTESIAN_POINT('',(-2.15207423655202,1.65804152271188,13.7902182540695));
#430213=CARTESIAN_POINT('Origin',(-2.09970450175266,1.643072643505,13.7418732680448));
#430214=CARTESIAN_POINT('',(-2.11768454258377,1.64821189159107,13.8235269408515));
#430215=CARTESIAN_POINT('',(-2.15207423655202,1.65804152271188,13.7902182540695));
#430216=CARTESIAN_POINT('',(-2.11768454258377,1.64821189159107,12.5893111709658));
#430217=CARTESIAN_POINT('',(-2.11768454258377,1.64821189159107,12.5));
#430218=CARTESIAN_POINT('',(-2.1720031479706,1.66373781788871,12.5369868989719));
#430219=CARTESIAN_POINT('Ctrl Pts',(-2.11768454258377,1.64821189159107,
12.5893111709658));
#430220=CARTESIAN_POINT('Ctrl Pts',(-2.13580421491228,1.65339105064912,
12.5718848856037));
#430221=CARTESIAN_POINT('Ctrl Pts',(-2.15391015173733,1.65856628367827,
12.5544431401645));
#430222=CARTESIAN_POINT('Ctrl Pts',(-2.1720031479706,1.66373781788871,12.5369868989719));
#430223=CARTESIAN_POINT('',(-2.1720031479706,1.66373781788871,12.5));
#430224=CARTESIAN_POINT('Origin',(-2.10823744587473,1.6812632605305,12.5));
#430225=CARTESIAN_POINT('',(-2.08067879467115,1.66071792247006,13.8587068136939));
#430226=CARTESIAN_POINT('Ctrl Pts',(-2.11768454258545,1.64821189158468,
13.8235269408542));
#430227=CARTESIAN_POINT('Ctrl Pts',(-2.11599971761088,1.6477303168426,13.8262006681044));
#430228=CARTESIAN_POINT('Ctrl Pts',(-2.11422779756818,1.64740454484519,
13.8288634856214));
#430229=CARTESIAN_POINT('Ctrl Pts',(-2.11237652462616,1.6472237190336,13.8314912288862));
#430230=CARTESIAN_POINT('Ctrl Pts',(-2.11046805317288,1.64703730627316,
13.8342001611531));
#430231=CARTESIAN_POINT('Ctrl Pts',(-2.1084731780219,1.64700423324031,13.8368750301949));
#430232=CARTESIAN_POINT('Ctrl Pts',(-2.10637684024255,1.64715119252942,
13.8394886372968));
#430233=CARTESIAN_POINT('Ctrl Pts',(-2.10621493499085,1.64716254255179,
13.8396904925131));
#430234=CARTESIAN_POINT('Ctrl Pts',(-2.10605242224907,1.64717498847012,
13.8398919674349));
#430235=CARTESIAN_POINT('Ctrl Pts',(-2.10588929490553,1.64718855402383,
13.8400930404591));
#430236=CARTESIAN_POINT('Ctrl Pts',(-2.10334766114646,1.64739991447711,
13.8432258934518));
#430237=CARTESIAN_POINT('Ctrl Pts',(-2.1006697040325,1.64788087453654,13.8462331177034));
#430238=CARTESIAN_POINT('Ctrl Pts',(-2.09795981658488,1.648710695014,13.8489036603661));
#430239=CARTESIAN_POINT('Ctrl Pts',(-2.09707310987547,1.64898222193134,
13.8497774930041));
#430240=CARTESIAN_POINT('Ctrl Pts',(-2.09618322449611,1.64929117012785,
13.85061494757));
#430241=CARTESIAN_POINT('Ctrl Pts',(-2.09529450652748,1.64964050391928,
13.8514076489583));
#430242=CARTESIAN_POINT('Ctrl Pts',(-2.09341473985153,1.65037939526964,
13.8530843267192));
#430243=CARTESIAN_POINT('Ctrl Pts',(-2.09135663551493,1.65137429659479,
13.8546805203176));
#430244=CARTESIAN_POINT('Ctrl Pts',(-2.08929902934897,1.65269030939996,
13.8559412814274));
#430245=CARTESIAN_POINT('Ctrl Pts',(-2.08902365491422,1.65286643459259,
13.8561100121513));
#430246=CARTESIAN_POINT('Ctrl Pts',(-2.08874829980687,1.65304823513679,
13.8562727473908));
#430247=CARTESIAN_POINT('Ctrl Pts',(-2.08847339350089,1.65323579124213,
13.8564289040185));
#430248=CARTESIAN_POINT('Ctrl Pts',(-2.08722669653949,1.65408635604014,
13.8571370725437));
#430249=CARTESIAN_POINT('Ctrl Pts',(-2.0859685991888,1.65507212142597,13.8577210840553));
#430250=CARTESIAN_POINT('Ctrl Pts',(-2.08476610464929,1.65617787184565,
13.8581177131616));
#430251=CARTESIAN_POINT('Ctrl Pts',(-2.08442744079835,1.65648928922261,
13.8582294175695));
#430252=CARTESIAN_POINT('Ctrl Pts',(-2.08409309497155,1.65681007180626,
13.8583265086086));
#430253=CARTESIAN_POINT('Ctrl Pts',(-2.08376431353877,1.65713951840094,
13.8584082369006));
#430254=CARTESIAN_POINT('Ctrl Pts',(-2.08329194278608,1.65761284481289,
13.8585256585398));
#430255=CARTESIAN_POINT('Ctrl Pts',(-2.08282541423584,1.65811016843248,
13.8586122832068));
#430256=CARTESIAN_POINT('Ctrl Pts',(-2.08237742288745,1.65861911051012,
13.8586682984299));
#430257=CARTESIAN_POINT('Ctrl Pts',(-2.08201907421669,1.65902621372243,
13.8587131050557));
#430258=CARTESIAN_POINT('Ctrl Pts',(-2.08166845244351,1.65944509243391,
13.8587357943552));
#430259=CARTESIAN_POINT('Ctrl Pts',(-2.0813259042565,1.65987612148833,13.8587355499465));
#430260=CARTESIAN_POINT('Ctrl Pts',(-2.08110450719651,1.6601547058424,13.8587353919793));
#430261=CARTESIAN_POINT('Ctrl Pts',(-2.08088884663434,1.66043532917931,
13.8587257282814));
#430262=CARTESIAN_POINT('Ctrl Pts',(-2.08067879467115,1.66071792247006,
13.8587068136939));
#430263=CARTESIAN_POINT('Ctrl Pts',(-2.08067879467115,1.66071792247006,
13.8587068136939));
#430264=CARTESIAN_POINT('Ctrl Pts',(-2.07998794521534,1.66164735639762,
13.8586446046466));
#430265=CARTESIAN_POINT('Ctrl Pts',(-2.07935768962981,1.66259807398097,
13.858482427929));
#430266=CARTESIAN_POINT('Ctrl Pts',(-2.07878414131476,1.66356786608021,
13.8582284286032));
#430267=CARTESIAN_POINT('Ctrl Pts',(-2.0781957474614,1.66456275996318,13.8579678548414));
#430268=CARTESIAN_POINT('Ctrl Pts',(-2.07766691551601,1.66558093852198,
13.857615680862));
#430269=CARTESIAN_POINT('Ctrl Pts',(-2.07720989530231,1.66657779459574,
13.8571944833187));
#430270=CARTESIAN_POINT('Ctrl Pts',(-2.07606935461884,1.66906555087786,
13.8561433417727));
#430271=CARTESIAN_POINT('Ctrl Pts',(-2.07531834955168,1.67153488102927,
13.8546163505475));
#430272=CARTESIAN_POINT('Ctrl Pts',(-2.07484729608965,1.6738104305201,13.8528973491086));
#430273=CARTESIAN_POINT('Ctrl Pts',(-2.07476124157188,1.67422613983949,
13.8525833129073));
#430274=CARTESIAN_POINT('Ctrl Pts',(-2.07468439415524,1.67463542046283,
13.8522628768812));
#430275=CARTESIAN_POINT('Ctrl Pts',(-2.07461592339801,1.67503727828417,
13.851937733538));
#430276=CARTESIAN_POINT('Ctrl Pts',(-2.07419778198349,1.67749136824381,
13.8499521282529));
#430277=CARTESIAN_POINT('Ctrl Pts',(-2.07405450257017,1.6799132094274,13.847639871647));
#430278=CARTESIAN_POINT('Ctrl Pts',(-2.07411341492913,1.6821707740468,13.8452109780794));
#430279=CARTESIAN_POINT('Ctrl Pts',(-2.07413992081886,1.68318649909833,
13.8441181685877));
#430280=CARTESIAN_POINT('Ctrl Pts',(-2.07420668933847,1.68416923558789,
13.8430021611332));
#430281=CARTESIAN_POINT('Ctrl Pts',(-2.07430455822727,1.6851090748427,13.8418824960098));
#430282=CARTESIAN_POINT('Ctrl Pts',(-2.07453518876287,1.68732383004633,
13.8392439765549));
#430283=CARTESIAN_POINT('Ctrl Pts',(-2.07494578944066,1.68940663422467,
13.8364981347964));
#430284=CARTESIAN_POINT('Ctrl Pts',(-2.07550387180333,1.69136961438488,
13.8336931113419));
#430285=CARTESIAN_POINT('Ctrl Pts',(-2.07604740858306,1.69328143240015,
13.8309611966328));
#430286=CARTESIAN_POINT('Ctrl Pts',(-2.07673192703162,1.69508135251798,
13.8281701127186));
#430287=CARTESIAN_POINT('Ctrl Pts',(-2.07755871490548,1.69675681454122,
13.8253580685121));
#430288=CARTESIAN_POINT('Ctrl Pts',(-2.07773796340883,1.69712005651608,
13.8247484142933));
#430289=CARTESIAN_POINT('Ctrl Pts',(-2.07792398516354,1.69747729842215,
13.8241378483365));
#430290=CARTESIAN_POINT('Ctrl Pts',(-2.07811692054273,1.69782812028616,
13.8235269408515));
#430291=CARTESIAN_POINT('',(-2.08143901971418,1.65973566245264,12.5969504640361));
#430292=CARTESIAN_POINT('Origin',(-2.10826319100818,1.68128404203464,12.584524458991));
#430293=CARTESIAN_POINT('Origin',(-2.10826319100818,1.68128404203464,12.584524458991));
#430294=CARTESIAN_POINT('Ctrl Pts',(-2.11768454258377,1.64821189159107,
12.5893111709658));
#430295=CARTESIAN_POINT('Ctrl Pts',(-2.10678700448808,1.64509704038872,
12.5770542771492));
#430296=CARTESIAN_POINT('Ctrl Pts',(-2.09943490649419,1.65971724318974,
12.5737548217797));
#430297=CARTESIAN_POINT('Ctrl Pts',(-2.14151380107655,1.65502302579549,
12.5663937883685));
#430298=CARTESIAN_POINT('Ctrl Pts',(-2.13060236165761,1.65190420116785,
12.5540940315304));
#430299=CARTESIAN_POINT('Ctrl Pts',(-2.12323034987202,1.66657115168753,
12.5508374392248));
#430300=CARTESIAN_POINT('Ctrl Pts',(-2.16531901613962,1.66182728764898,
12.5434499600944));
#430301=CARTESIAN_POINT('Ctrl Pts',(-2.15437209974549,1.65869832261179,
12.5311293540533));
#430302=CARTESIAN_POINT('Ctrl Pts',(-2.14700287116098,1.67341722999765,
12.5278936106989));
#430303=CARTESIAN_POINT('Ctrl Pts',(-2.18910207112778,1.66862521547222,
12.5204817579905));
#430304=CARTESIAN_POINT('Ctrl Pts',(-2.17810097497864,1.66548076419649,
12.5081597038247));
#430305=CARTESIAN_POINT('Ctrl Pts',(-2.17075425579,1.68025607339996,12.5049254088044));
#430306=CARTESIAN_POINT('Ctrl Pts',(-2.1720031479706,1.66373781788871,12.5369868989719));
#430307=CARTESIAN_POINT('Ctrl Pts',(-2.17289878453494,1.66399381850462,
12.5342545179733));
#430308=CARTESIAN_POINT('Ctrl Pts',(-2.17371925589978,1.66435807645283,
12.5314872231885));
#430309=CARTESIAN_POINT('Ctrl Pts',(-2.1743956607143,1.66486116455349,12.5287124745063));
#430310=CARTESIAN_POINT('Ctrl Pts',(-2.17500567614977,1.66531487437373,
12.5262100684184));
#430311=CARTESIAN_POINT('Ctrl Pts',(-2.1754973150128,1.66588183077953,12.5237004536639));
#430312=CARTESIAN_POINT('Ctrl Pts',(-2.17582893601259,1.66661519841171,
12.5212220730815));
#430313=CARTESIAN_POINT('Ctrl Pts',(-2.17608282057543,1.66717665477551,
12.5193246583486));
#430314=CARTESIAN_POINT('Ctrl Pts',(-2.17624537110145,1.66784262020223,
12.517417831369));
#430315=CARTESIAN_POINT('Ctrl Pts',(-2.17622853509212,1.66865433520904,
12.5155812248347));
#430316=CARTESIAN_POINT('Ctrl Pts',(-2.17622136286165,1.66900013016493,
12.5147988205793));
#430317=CARTESIAN_POINT('Ctrl Pts',(-2.1761819051421,1.66937273261406,12.5140295443047));
#430318=CARTESIAN_POINT('Ctrl Pts',(-2.1761050862756,1.66977656626123,12.5132817086137));
#430319=CARTESIAN_POINT('Ctrl Pts',(-2.17598883131297,1.67038771385684,
12.5121499604604));
#430320=CARTESIAN_POINT('Ctrl Pts',(-2.17577747298445,1.67108225023013,
12.5110494206568));
#430321=CARTESIAN_POINT('Ctrl Pts',(-2.17543378949294,1.67186137395032,
12.5100666561695));
#430322=CARTESIAN_POINT('Ctrl Pts',(-2.17523644722355,1.67230874499629,
12.5095023550641));
#430323=CARTESIAN_POINT('Ctrl Pts',(-2.17499259962067,1.67278891026161,
12.5089719619137));
#430324=CARTESIAN_POINT('Ctrl Pts',(-2.17470112262343,1.67328997756949,
12.5085043804652));
#430325=CARTESIAN_POINT('Ctrl Pts',(-2.17427458400551,1.67402322430597,
12.5078201359221));
#430326=CARTESIAN_POINT('Ctrl Pts',(-2.17373263432014,1.67482189103943,
12.5072563000949));
#430327=CARTESIAN_POINT('Ctrl Pts',(-2.17310500434093,1.6756270862925,12.5068768744332));
#430328=CARTESIAN_POINT('Ctrl Pts',(-2.17265243991971,1.6762076874998,12.5066032824114));
#430329=CARTESIAN_POINT('Ctrl Pts',(-2.17214742335478,1.67680192035804,
12.5064197834844));
#430330=CARTESIAN_POINT('Ctrl Pts',(-2.17162012571962,1.67737827528449,
12.5063282718343));
#430331=CARTESIAN_POINT('Ctrl Pts',(-2.17085043441952,1.67821957504213,
12.5061946931565));
#430332=CARTESIAN_POINT('Ctrl Pts',(-2.17001760138821,1.67904148113283,
12.5062515701262));
#430333=CARTESIAN_POINT('Ctrl Pts',(-2.16918417633874,1.67980399166105,
12.5064436508398));
#430334=CARTESIAN_POINT('',(-2.09943490649419,1.65971724318974,12.5737548217797));
#430335=CARTESIAN_POINT('Origin',(-2.11163840068998,1.6693647677123,12.5893111709658));
#430336=CARTESIAN_POINT('Ctrl Pts',(-2.16918417633874,1.67980399166105,
12.5064436508398));
#430337=CARTESIAN_POINT('Ctrl Pts',(-2.15885933931749,1.67683109269946,
12.5164271754438));
#430338=CARTESIAN_POINT('Ctrl Pts',(-2.14853046734465,1.67385681450306,
12.5264061185523));
#430339=CARTESIAN_POINT('Ctrl Pts',(-2.13819741805072,1.67088110940588,
12.536380305637));
#430340=CARTESIAN_POINT('Ctrl Pts',(-2.12528320220153,1.66716208157243,
12.5488460165097));
#430341=CARTESIAN_POINT('Ctrl Pts',(-2.11236245759787,1.66344082380799,
12.5613043021964));
#430342=CARTESIAN_POINT('Ctrl Pts',(-2.09943490649419,1.65971724318974,
12.5737548217797));
#430343=CARTESIAN_POINT('Ctrl Pts',(-2.07811692054273,1.69782812028616,
12.5893111709658));
#430344=CARTESIAN_POINT('Ctrl Pts',(-2.07265523480839,1.68789692582129,
12.5770542771492));
#430345=CARTESIAN_POINT('Ctrl Pts',(-2.08527288288873,1.67747585909204,
12.5737548217797));
#430346=CARTESIAN_POINT('Ctrl Pts',(-2.07302121525583,1.68856240222741,
12.5928319619712));
#430347=CARTESIAN_POINT('Ctrl Pts',(-2.07220516816716,1.6803181628131,12.5821634970842));
#430348=CARTESIAN_POINT('Ctrl Pts',(-2.08340837015351,1.67410513073906,
12.5773203894503));
#430349=CARTESIAN_POINT('Ctrl Pts',(-2.0718068996575,1.67185583055733,12.5969440695591));
#430350=CARTESIAN_POINT('Ctrl Pts',(-2.07429887139505,1.66870168734384,
12.5878292599214));
#430351=CARTESIAN_POINT('Ctrl Pts',(-2.08297760389043,1.66815041936703,
12.5813877129824));
#430352=CARTESIAN_POINT('Ctrl Pts',(-2.09084161614938,1.64790056362884,
12.596957478804));
#430353=CARTESIAN_POINT('Ctrl Pts',(-2.08836812364821,1.65103144657069,
12.5878468778671));
#430354=CARTESIAN_POINT('Ctrl Pts',(-2.08979506304708,1.65958020822894,
12.5814011370086));
#430355=CARTESIAN_POINT('Ctrl Pts',(-2.10750247140822,1.64530154281635,
12.5928371701607));
#430356=CARTESIAN_POINT('Ctrl Pts',(-2.0992899977597,1.6463457373749,12.5821692192952));
#430357=CARTESIAN_POINT('Ctrl Pts',(-2.09572203006074,1.65864587674269,
12.5773318885715));
#430358=CARTESIAN_POINT('Ctrl Pts',(-2.11768454258378,1.64821189159102,
12.5893111709658));
#430359=CARTESIAN_POINT('Ctrl Pts',(-2.10678700448809,1.64509704038866,
12.5770542771492));
#430360=CARTESIAN_POINT('Ctrl Pts',(-2.09943490649421,1.65971724318969,
12.5737548217797));
#430361=CARTESIAN_POINT('',(-2.08527288288873,1.67747585909204,12.5737548217797));
#430362=CARTESIAN_POINT('Origin',(-2.09739405675521,1.68722661004253,12.5893111709658));
#430363=CARTESIAN_POINT('Ctrl Pts',(-2.09943490649421,1.65971724318969,
12.5737548217797));
#430364=CARTESIAN_POINT('Ctrl Pts',(-2.09848083327137,1.65941054477678,
12.5746934679442));
#430365=CARTESIAN_POINT('Ctrl Pts',(-2.09736902634259,1.6592455575308,12.5756680099006));
#430366=CARTESIAN_POINT('Ctrl Pts',(-2.09622646656681,1.65923775838016,
12.5765688348656));
#430367=CARTESIAN_POINT('Ctrl Pts',(-2.09592398651472,1.65923569364137,
12.5768073183026));
#430368=CARTESIAN_POINT('Ctrl Pts',(-2.09561941536456,1.65924439678361,
12.5770407398754));
#430369=CARTESIAN_POINT('Ctrl Pts',(-2.09531510845777,1.65926359181898,
12.5772674179684));
#430370=CARTESIAN_POINT('Ctrl Pts',(-2.09406631520036,1.65934236305355,
12.5781976435658));
#430371=CARTESIAN_POINT('Ctrl Pts',(-2.09275175364623,1.6596135556109,12.5790594849312));
#430372=CARTESIAN_POINT('Ctrl Pts',(-2.09146994161572,1.66010615143115,
12.5797571720116));
#430373=CARTESIAN_POINT('Ctrl Pts',(-2.09063479498799,1.6604270953202,12.580211740231));
#430374=CARTESIAN_POINT('Ctrl Pts',(-2.08978233154435,1.66087413341432,
12.5806009430798));
#430375=CARTESIAN_POINT('Ctrl Pts',(-2.08898078903428,1.66143148632664,
12.5808812374708));
#430376=CARTESIAN_POINT('Ctrl Pts',(-2.08829199810917,1.66191043737823,
12.5811221033394));
#430377=CARTESIAN_POINT('Ctrl Pts',(-2.08762677357178,1.66248074963265,
12.581287365893));
#430378=CARTESIAN_POINT('Ctrl Pts',(-2.08702808871054,1.6631165638511,12.581359338449));
#430379=CARTESIAN_POINT('Ctrl Pts',(-2.0869448838772,1.6632049288984,12.5813693411482));
#430380=CARTESIAN_POINT('Ctrl Pts',(-2.08686290949314,1.66329453496134,
12.5813775999465));
#430381=CARTESIAN_POINT('Ctrl Pts',(-2.08678222436493,1.66338528885807,
12.5813841266931));
#430382=CARTESIAN_POINT('Ctrl Pts',(-2.08664533228625,1.66353926382032,
12.5813952001081));
#430383=CARTESIAN_POINT('Ctrl Pts',(-2.08651168956088,1.66369797865285,
12.5814007534795));
#430384=CARTESIAN_POINT('Ctrl Pts',(-2.08638150524812,1.66386149125346,
12.5814005856065));
#430385=CARTESIAN_POINT('Ctrl Pts',(-2.08578557236308,1.66460998800977,
12.5813998171494));
#430386=CARTESIAN_POINT('Ctrl Pts',(-2.0853030191508,1.66540709402405,12.58127954464));
#430387=CARTESIAN_POINT('Ctrl Pts',(-2.084911272862,1.66623296020712,12.5810700125799));
#430388=CARTESIAN_POINT('Ctrl Pts',(-2.08443808794901,1.66723051252387,
12.5808169217085));
#430389=CARTESIAN_POINT('Ctrl Pts',(-2.08411246764549,1.66827728842033,
12.5804173076348));
#430390=CARTESIAN_POINT('Ctrl Pts',(-2.08393808174607,1.66927381485035,
12.5799304713245));
#430391=CARTESIAN_POINT('Ctrl Pts',(-2.08372196267946,1.67050882503535,
12.5793271277669));
#430392=CARTESIAN_POINT('Ctrl Pts',(-2.08369300020097,1.67173771639883,
12.5785808224116));
#430393=CARTESIAN_POINT('Ctrl Pts',(-2.08382070708085,1.67290794151214,
12.5777485681082));
#430394=CARTESIAN_POINT('Ctrl Pts',(-2.0840110043232,1.67465170513872,12.576508418016));
#430395=CARTESIAN_POINT('Ctrl Pts',(-2.08454074030736,1.67625126735941,
12.5750928681475));
#430396=CARTESIAN_POINT('Ctrl Pts',(-2.08527288288873,1.67747585909204,
12.5737548217797));
#430397=CARTESIAN_POINT('Ctrl Pts',(-2.08527288288873,1.67747585909204,
12.5737548217797));
#430398=CARTESIAN_POINT('Ctrl Pts',(-2.07265523480839,1.68789692582129,
12.5770542771492));
#430399=CARTESIAN_POINT('Ctrl Pts',(-2.07811692054273,1.69782812028616,
12.5893111709658));
#430400=CARTESIAN_POINT('Ctrl Pts',(-2.09724813451306,1.69914630677325,
12.5508408821982));
#430401=CARTESIAN_POINT('Ctrl Pts',(-2.08458934657359,1.70959718293428,
12.55409748406));
#430402=CARTESIAN_POINT('Ctrl Pts',(-2.09005800002012,1.71954104705978,
12.5663972313419));
#430403=CARTESIAN_POINT('Ctrl Pts',(-2.10921065545595,1.72079615565222,
12.52790050457));
#430404=CARTESIAN_POINT('Ctrl Pts',(-2.09650060167422,1.73125587888978,
12.5311362602938));
#430405=CARTESIAN_POINT('Ctrl Pts',(-2.10198703291048,1.74123206905817,
12.5434568539655));
#430406=CARTESIAN_POINT('Ctrl Pts',(-2.12116142293421,1.74242701321815,
12.5049357605811));
#430407=CARTESIAN_POINT('Ctrl Pts',(-2.10839138280069,1.75287734622613,
12.5081700652078));
#430408=CARTESIAN_POINT('Ctrl Pts',(-2.11390496270498,1.76290290186781,
12.5204921097672));
#430409=CARTESIAN_POINT('Ctrl Pts',(-2.12037668730681,1.74100664708752,
12.5064436508395));
#430410=CARTESIAN_POINT('Ctrl Pts',(-2.11977401306308,1.74206760493142,
12.5062361689309));
#430411=CARTESIAN_POINT('Ctrl Pts',(-2.11910203956898,1.74314521489967,
12.5061871075061));
#430412=CARTESIAN_POINT('Ctrl Pts',(-2.11839401867698,1.74415006466835,
12.5063648335164));
#430413=CARTESIAN_POINT('Ctrl Pts',(-2.1180723919153,1.74460652941499,12.5064455676329));
#430414=CARTESIAN_POINT('Ctrl Pts',(-2.11773866051794,1.74505421966292,
12.506574497099));
#430415=CARTESIAN_POINT('Ctrl Pts',(-2.11740629129084,1.74547331168305,
12.5067492519495));
#430416=CARTESIAN_POINT('Ctrl Pts',(-2.11673838242732,1.74631549336552,
12.5071004286051));
#430417=CARTESIAN_POINT('Ctrl Pts',(-2.11605078449554,1.74707265018967,
12.5076537929613));
#430418=CARTESIAN_POINT('Ctrl Pts',(-2.11540210735358,1.7476943123261,12.5083435010505));
#430419=CARTESIAN_POINT('Ctrl Pts',(-2.11536126925098,1.74773344967266,
12.5083869222964));
#430420=CARTESIAN_POINT('Ctrl Pts',(-2.11532057269779,1.74777204564341,
12.5084308732337));
#430421=CARTESIAN_POINT('Ctrl Pts',(-2.11528002701449,1.74781008624831,
12.5084753333615));
#430422=CARTESIAN_POINT('Ctrl Pts',(-2.1149547971189,1.74811522210867,12.5088319622689));
#430423=CARTESIAN_POINT('Ctrl Pts',(-2.11463355442634,1.7483917604449,12.509227847131));
#430424=CARTESIAN_POINT('Ctrl Pts',(-2.11432767792467,1.74863360040892,
12.5096423454524));
#430425=CARTESIAN_POINT('Ctrl Pts',(-2.11336919634372,1.7493914198223,12.5109411997424));
#430426=CARTESIAN_POINT('Ctrl Pts',(-2.11250864201505,1.74986272475234,
12.5124831113042));
#430427=CARTESIAN_POINT('Ctrl Pts',(-2.11175429310831,1.7501417878319,12.5140723025008));
#430428=CARTESIAN_POINT('Ctrl Pts',(-2.11168360978953,1.7501679363481,12.5142212114565));
#430429=CARTESIAN_POINT('Ctrl Pts',(-2.11161385099886,1.75019242552307,
12.5143705582413));
#430430=CARTESIAN_POINT('Ctrl Pts',(-2.11154502049841,1.75021534962019,
12.5145201959299));
#430431=CARTESIAN_POINT('Ctrl Pts',(-2.11066079024221,1.75050984377818,
12.5164425148273));
#430432=CARTESIAN_POINT('Ctrl Pts',(-2.10990285402866,1.75056632807291,
12.518463520594));
#430433=CARTESIAN_POINT('Ctrl Pts',(-2.10923121631493,1.75046566247659,
12.5205025929157));
#430434=CARTESIAN_POINT('Ctrl Pts',(-2.10884163981974,1.75040727244071,
12.5216853356836));
#430435=CARTESIAN_POINT('Ctrl Pts',(-2.10848173016598,1.75029659364564,
12.5228750347131));
#430436=CARTESIAN_POINT('Ctrl Pts',(-2.10814913497809,1.75015172028871,
12.5240609649613));
#430437=CARTESIAN_POINT('Ctrl Pts',(-2.10733279793255,1.74979613640631,
12.5269717671327));
#430438=CARTESIAN_POINT('Ctrl Pts',(-2.10666218806475,1.7492150155984,12.5299036066169));
#430439=CARTESIAN_POINT('Ctrl Pts',(-2.10609182295306,1.74848212013141,
12.5328133004019));
#430440=CARTESIAN_POINT('Ctrl Pts',(-2.10581801448809,1.74813028763204,
12.5342101228451));
#430441=CARTESIAN_POINT('Ctrl Pts',(-2.10556806324457,1.74774359488252,
12.5356023438238));
#430442=CARTESIAN_POINT('Ctrl Pts',(-2.10534060625466,1.74733000120828,
12.5369868989719));
#430443=CARTESIAN_POINT('Origin',(-8.24240891046344,12.9175899459587,-1.23982923200078));
#430444=CARTESIAN_POINT('Ctrl Pts',(-2.17196297394457,1.6637262936288,12.5369868989719));
#430445=CARTESIAN_POINT('Ctrl Pts',(-2.18670325038309,1.66796982449374,
12.5369868989719));
#430446=CARTESIAN_POINT('Ctrl Pts',(-2.1957819678493,1.65560616027741,12.5369868989719));
#430447=CARTESIAN_POINT('Ctrl Pts',(-2.17694578218716,1.66516070939695,
12.5218025310016));
#430448=CARTESIAN_POINT('Ctrl Pts',(-2.1887632881211,1.66511154430852,12.5216901060418));
#430449=CARTESIAN_POINT('Ctrl Pts',(-2.19575430620257,1.65564385858438,
12.5161920673678));
#430450=CARTESIAN_POINT('Ctrl Pts',(-2.17897032065797,1.67083850079639,
12.5042015548895));
#430451=CARTESIAN_POINT('Ctrl Pts',(-2.18528580063597,1.66961700267343,
12.4980677368513));
#430452=CARTESIAN_POINT('Ctrl Pts',(-2.1894070985955,1.66421277443503,12.4907278922777));
#430453=CARTESIAN_POINT('Ctrl Pts',(-2.16916836253948,1.67979174555728,
12.506463626192));
#430454=CARTESIAN_POINT('Ctrl Pts',(-2.17434135878366,1.6837976846724,12.4999376786891));
#430455=CARTESIAN_POINT('Ctrl Pts',(-2.17427817815607,1.68374875795074,
12.4906970594712));
#430456=CARTESIAN_POINT('Origin',(-2.17804928986438,1.64258494176748,12.5369868989719));
#430457=CARTESIAN_POINT('Origin',(-2.17804928986438,1.64258494176748,14.));
#430458=CARTESIAN_POINT('Origin',(-2.17804928986438,1.64258494176748,13.7435492065112));
#430459=CARTESIAN_POINT('Ctrl Pts',(-2.14819645488023,1.65693310533074,
13.793642941384));
#430460=CARTESIAN_POINT('Ctrl Pts',(-2.15858492349311,1.65993076089547,
13.8071662555867));
#430461=CARTESIAN_POINT('Ctrl Pts',(-2.16566075700062,1.64444037794964,
13.8103758687955));
#430462=CARTESIAN_POINT('Ctrl Pts',(-2.1641775695261,1.66150100199096,13.7804579775006));
#430463=CARTESIAN_POINT('Ctrl Pts',(-2.17699881230708,1.66519009473591,
13.7901904343353));
#430464=CARTESIAN_POINT('Ctrl Pts',(-2.1857779194939,1.65210639490877,13.7927914348263));
#430465=CARTESIAN_POINT('Ctrl Pts',(-2.1735862531656,1.66419029462756,13.7597120340895));
#430466=CARTESIAN_POINT('Ctrl Pts',(-2.18842562629994,1.66845410688339,
13.7635825532444));
#430467=CARTESIAN_POINT('Ctrl Pts',(-2.19765008972107,1.65660314950704,
13.7651073818884));
#430468=CARTESIAN_POINT('Ctrl Pts',(-2.17174381747484,1.66366366955073,
13.7381884353898));
#430469=CARTESIAN_POINT('Ctrl Pts',(-2.1862355992142,1.66782854321562,13.7368803041982));
#430470=CARTESIAN_POINT('Ctrl Pts',(-2.19532534107114,1.65572208914794,
13.7363986145813));
#430471=CARTESIAN_POINT('Origin',(-2.15812037844581,1.63688864659065,13.7902182540695));
#430472=CARTESIAN_POINT('Ctrl Pts',(-2.11768075815972,1.64821080909709,
13.8235227101244));
#430473=CARTESIAN_POINT('Ctrl Pts',(-2.12873390990635,1.65137475043435,
13.8358800583119));
#430474=CARTESIAN_POINT('Ctrl Pts',(-2.13607948675083,1.63651983374394,
13.8390832900376));
#430475=CARTESIAN_POINT('Ctrl Pts',(-2.12914905854842,1.65148880169767,
13.8124254819053));
#430476=CARTESIAN_POINT('Ctrl Pts',(-2.14022367543563,1.65465888709674,
13.8247886449158));
#430477=CARTESIAN_POINT('Ctrl Pts',(-2.14756325531363,1.63977764560561,
13.8279860620657));
#430478=CARTESIAN_POINT('Ctrl Pts',(-2.14061221921795,1.65476532520861,
13.8013225099954));
#430479=CARTESIAN_POINT('Ctrl Pts',(-2.15170307525326,1.65794006082546,
13.8136962257787));
#430480=CARTESIAN_POINT('Ctrl Pts',(-2.15904163348003,1.64303421002671,
13.8168830918626));
#430481=CARTESIAN_POINT('Ctrl Pts',(-2.15207044014693,1.65804043678995,
13.7902140179785));
#430482=CARTESIAN_POINT('Ctrl Pts',(-2.16317265089572,1.66121842641144,
13.802602731458));
#430483=CARTESIAN_POINT('Ctrl Pts',(-2.17051483254955,1.64628957779261,
13.8057746032558));
#430484=CARTESIAN_POINT('Origin',(-2.12373068447755,1.62705901546984,13.8235269408515));
#430485=CARTESIAN_POINT('Ctrl Pts',(-2.07811692054273,1.69782812028616,
13.8235269408515));
#430486=CARTESIAN_POINT('Ctrl Pts',(-2.08380679035239,1.70817423068283,
13.8362179249168));
#430487=CARTESIAN_POINT('Ctrl Pts',(-2.07037048621576,1.71871599216776,
13.8391868794938));
#430488=CARTESIAN_POINT('Ctrl Pts',(-2.07291093733218,1.68836187961257,
13.8400110824519));
#430489=CARTESIAN_POINT('Ctrl Pts',(-2.07447522739571,1.69830546344632,
13.8494522556837));
#430490=CARTESIAN_POINT('Ctrl Pts',(-2.06190135843871,1.70308308910016,
13.85569149686));
#430491=CARTESIAN_POINT('Ctrl Pts',(-2.07159200443801,1.67212432616183,
13.8586819406588));
#430492=CARTESIAN_POINT('Ctrl Pts',(-2.06888830863196,1.67553696042635,
13.868010383617));
#430493=CARTESIAN_POINT('Ctrl Pts',(-2.05985742406479,1.67611660749727,
13.8744918421245));
#430494=CARTESIAN_POINT('Ctrl Pts',(-2.09105982971829,1.64762789220088,
13.8587686893867));
#430495=CARTESIAN_POINT('Ctrl Pts',(-2.09373941852129,1.64424559538263,
13.8680909899357));
#430496=CARTESIAN_POINT('Ctrl Pts',(-2.09226765043519,1.63533883950822,
13.8745789365163));
#430497=CARTESIAN_POINT('Ctrl Pts',(-2.1072802974052,1.64523803865347,13.8400379222776));
#430498=CARTESIAN_POINT('Ctrl Pts',(-2.11731961172237,1.64454348703638,
13.8494748685453));
#430499=CARTESIAN_POINT('Ctrl Pts',(-2.11917976087262,1.6312280467356,13.8557104837033));
#430500=CARTESIAN_POINT('Ctrl Pts',(-2.11768454258545,1.64821189158468,
13.8235269408542));
#430501=CARTESIAN_POINT('Ctrl Pts',(-2.12903736953781,1.65145687833045,
13.8362179249195));
#430502=CARTESIAN_POINT('Ctrl Pts',(-2.13632496810756,1.63601168777992,
13.8391868794965));
#430503=CARTESIAN_POINT('Origin',(-2.05883978433026,1.70842963052978,13.8235269408515));
#430504=CARTESIAN_POINT('Ctrl Pts',(-2.09535062841647,1.72916483960377,
13.7902140241683));
#430505=CARTESIAN_POINT('Ctrl Pts',(-2.10091940558456,1.73928152464605,
13.8026027327198));
#430506=CARTESIAN_POINT('Ctrl Pts',(-2.08799864862912,1.74976159964444,
13.8057746032556));
#430507=CARTESIAN_POINT('Ctrl Pts',(-2.0896079366958,1.71872268108058,13.8013225161808));
#430508=CARTESIAN_POINT('Ctrl Pts',(-2.09517101479492,1.7288290201778,13.8136962270464));
#430509=CARTESIAN_POINT('Ctrl Pts',(-2.08227187275708,1.73930044510477,
13.8168830918628));
#430510=CARTESIAN_POINT('Ctrl Pts',(-2.08386276924907,1.70827602084888,
13.8124254880875));
#430511=CARTESIAN_POINT('Ctrl Pts',(-2.08941770018537,1.71836756271985,
13.8247886461867));
#430512=CARTESIAN_POINT('Ctrl Pts',(-2.07654277777542,1.72883450760057,
13.8279860620656));
#430513=CARTESIAN_POINT('Ctrl Pts',(-2.0781150258492,1.69782467666191,13.8235227163065));
#430514=CARTESIAN_POINT('Ctrl Pts',(-2.08365919034214,1.70789665875641,
13.8358800595848));
#430515=CARTESIAN_POINT('Ctrl Pts',(-2.07081126715285,1.71836359242966,
13.8390832900376));
#430516=CARTESIAN_POINT('Origin',(-2.07607539289668,1.73976980437337,13.7902182540695));
#430517=CARTESIAN_POINT('Ctrl Pts',(-2.10521054015172,1.7470935542241,13.7382347919292));
#430518=CARTESIAN_POINT('Ctrl Pts',(-2.11250338907157,1.76030461865379,
13.7369371795942));
#430519=CARTESIAN_POINT('Ctrl Pts',(-2.10270924970151,1.77186397032332,
13.7364597369711));
#430520=CARTESIAN_POINT('Ctrl Pts',(-2.10612205768621,1.74875100098601,
13.7595490285574));
#430521=CARTESIAN_POINT('Ctrl Pts',(-2.1135880275148,1.76227775599,13.7633824266926));
#430522=CARTESIAN_POINT('Ctrl Pts',(-2.10406897719646,1.77390880673123,
13.7648920890506));
#430523=CARTESIAN_POINT('Ctrl Pts',(-2.10147336820428,1.74029811329877,
13.780380659011));
#430524=CARTESIAN_POINT('Ctrl Pts',(-2.10793589121805,1.75199566356795,
13.7901039518744));
#430525=CARTESIAN_POINT('Ctrl Pts',(-2.09714002958799,1.76348195161457,
13.7926933640892));
#430526=CARTESIAN_POINT('Ctrl Pts',(-2.09339290809914,1.72560510761366,
13.7936647693663));
#430527=CARTESIAN_POINT('Ctrl Pts',(-2.09863096097873,1.73506746112509,
13.8072068914933));
#430528=CARTESIAN_POINT('Ctrl Pts',(-2.08508249994794,1.74541557561732,
13.8104111085397));
#430529=CARTESIAN_POINT('Origin',(-2.08606347004218,1.7579315114519,13.7435492065112));
#430530=CARTESIAN_POINT('Origin',(-2.08606347004219,1.7579315114519,14.));
#430531=CARTESIAN_POINT('Origin',(-2.08606347004219,1.7579315114519,12.5369868989719));
#430532=CARTESIAN_POINT('Ctrl Pts',(-2.12036247970043,1.74099498144077,
12.506462012331));
#430533=CARTESIAN_POINT('Ctrl Pts',(-2.12541589999379,1.74514426226142,
12.4999388158272));
#430534=CARTESIAN_POINT('Ctrl Pts',(-2.12535611140457,1.74509517082787,
12.4907030323752));
#430535=CARTESIAN_POINT('Ctrl Pts',(-2.11381329720205,1.75254213657774,
12.5042014951932));
#430536=CARTESIAN_POINT('Ctrl Pts',(-2.11402861184905,1.75896823467215,
12.4980716682127));
#430537=CARTESIAN_POINT('Ctrl Pts',(-2.10968123246735,1.76418607500484,
12.4907355092743));
#430538=CARTESIAN_POINT('Ctrl Pts',(-2.10782793562257,1.75183421849748,
12.5218047446509));
#430539=CARTESIAN_POINT('Ctrl Pts',(-2.11040728173428,1.76336096324925,
12.5216906929434));
#430540=CARTESIAN_POINT('Ctrl Pts',(-2.10273934234465,1.7722813589718,12.5161988840776));
#430541=CARTESIAN_POINT('Ctrl Pts',(-2.10532206464639,1.74729635588789,
12.5369868989719));
#430542=CARTESIAN_POINT('Ctrl Pts',(-2.11273278129887,1.7607159985887,12.5369868989719));
#430543=CARTESIAN_POINT('Ctrl Pts',(-2.10270987500295,1.77231543309665,
12.5369868989719));
#430544=CARTESIAN_POINT('Origin',(-4.02788837499584E-31,-1.9397288087879E-31,
12.5));
#430545=CARTESIAN_POINT('Origin',(-2.20959091159279,1.5227929159564,12.5));
#430546=CARTESIAN_POINT('',(-2.20959091159279,1.5227929159564,12.5893111709658));
#430547=CARTESIAN_POINT('',(-2.20959091159279,1.5227929159564,13.8235269408515));
#430548=CARTESIAN_POINT('',(-2.20959091159279,1.5227929159564,12.5));
#430549=CARTESIAN_POINT('',(-2.22932368520977,1.55262394585116,13.7902182540695));
#430550=CARTESIAN_POINT('',(-2.20959091159279,1.5227929159564,13.8235269408515));
#430551=CARTESIAN_POINT('',(-2.2407588755845,1.56991110033548,13.7435492065112));
#430552=CARTESIAN_POINT('Origin',(-2.20313752209684,1.51303641086648,13.7445212918712));
#430553=CARTESIAN_POINT('',(-2.2407588755845,1.56991110033548,12.5369868989719));
#430554=CARTESIAN_POINT('',(-2.2407588755845,1.56991110033548,12.5));
#430555=CARTESIAN_POINT('Ctrl Pts',(-2.2407588755845,1.56991110033548,12.5369868989719));
#430556=CARTESIAN_POINT('Ctrl Pts',(-2.23037713159302,1.55421649392175,
12.5544431401645));
#430557=CARTESIAN_POINT('Ctrl Pts',(-2.2199879623023,1.53851066230838,12.5718848856037));
#430558=CARTESIAN_POINT('Ctrl Pts',(-2.20959091159279,1.5227929159564,12.5893111709658));
#430559=CARTESIAN_POINT('Origin',(-2.51467404694377,1.52389000361758,12.5));
#430560=CARTESIAN_POINT('',(-2.30038606421963,1.48116344709534,13.7435492065112));
#430561=CARTESIAN_POINT('',(-2.28005916367105,1.47711049716241,13.7902182540695));
#430562=CARTESIAN_POINT('Origin',(-2.22664358222596,1.46646004522961,13.7418732680453));
#430563=CARTESIAN_POINT('',(-2.24498269238234,1.47011665264502,13.8235269408515));
#430564=CARTESIAN_POINT('',(-2.28005916367105,1.47711049716241,13.7902182540695));
#430565=CARTESIAN_POINT('',(-2.24498269238234,1.47011665264502,12.5893111709658));
#430566=CARTESIAN_POINT('',(-2.24498269238234,1.47011665264502,12.5));
#430567=CARTESIAN_POINT('',(-2.30038606421963,1.48116344709534,12.5369868989719));
#430568=CARTESIAN_POINT('Ctrl Pts',(-2.24498269238234,1.47011665264502,
12.5893111709658));
#430569=CARTESIAN_POINT('Ctrl Pts',(-2.26346422254014,1.47380165696895,
12.5718848856037));
#430570=CARTESIAN_POINT('Ctrl Pts',(-2.28193174289044,1.47748386789857,
12.5544431401645));
#430571=CARTESIAN_POINT('Ctrl Pts',(-2.30038606421963,1.48116344709534,
12.5369868989719));
#430572=CARTESIAN_POINT('',(-2.30038606421963,1.48116344709534,12.5));
#430573=CARTESIAN_POINT('Origin',(-2.23826102351077,1.5038280719652,12.5));
#430574=CARTESIAN_POINT('',(-2.20911943565999,1.48559738273759,13.8587068136939));
#430575=CARTESIAN_POINT('Ctrl Pts',(-2.24498269238349,1.47011665263851,
13.8235269408542));
#430576=CARTESIAN_POINT('Ctrl Pts',(-2.24326422071284,1.46977400917324,
13.8262006681044));
#430577=CARTESIAN_POINT('Ctrl Pts',(-2.2414716431458,1.46959374908846,13.8288634856214));
#430578=CARTESIAN_POINT('Ctrl Pts',(-2.23961179117942,1.46956442089099,
13.8314912288862));
#430579=CARTESIAN_POINT('Ctrl Pts',(-2.23769447563692,1.46953418654446,
13.834200161153));
#430580=CARTESIAN_POINT('Ctrl Pts',(-2.23570354250922,1.46966382440372,
13.8368750301949));
#430581=CARTESIAN_POINT('Ctrl Pts',(-2.23362615866727,1.46998116568839,
13.8394886372968));
#430582=CARTESIAN_POINT('Ctrl Pts',(-2.23346571727412,1.47000567472556,
13.8396904925131));
#430583=CARTESIAN_POINT('Ctrl Pts',(-2.23330475973798,1.47003132552828,
13.8398919674349));
#430584=CARTESIAN_POINT('Ctrl Pts',(-2.23314328090578,1.47005814233663,
13.8400930404591));
#430585=CARTESIAN_POINT('Ctrl Pts',(-2.23062733206249,1.47047596625217,
13.8432258934518));
#430586=CARTESIAN_POINT('Ctrl Pts',(-2.22799748833976,1.47117360432241,
13.8462331177034));
#430587=CARTESIAN_POINT('Ctrl Pts',(-2.22536425589166,1.47222154462504,
13.8489036603661));
#430588=CARTESIAN_POINT('Ctrl Pts',(-2.22450263159018,1.47256444288756,
13.8497774930041));
#430589=CARTESIAN_POINT('Ctrl Pts',(-2.22364088937716,1.47294489700414,
13.85061494757));
#430590=CARTESIAN_POINT('Ctrl Pts',(-2.22278360249132,1.4733655071811,13.8514076489583));
#430591=CARTESIAN_POINT('Ctrl Pts',(-2.2209703170885,1.47425515836644,13.8530843267192));
#430592=CARTESIAN_POINT('Ctrl Pts',(-2.21900015461852,1.47541450384944,
13.8546805203176));
#430593=CARTESIAN_POINT('Ctrl Pts',(-2.21705666222821,1.47689385173497,
13.8559412814273));
#430594=CARTESIAN_POINT('Ctrl Pts',(-2.21679655991744,1.47709183645844,
13.8561100121513));
#430595=CARTESIAN_POINT('Ctrl Pts',(-2.2165369394636,1.47729547607385,13.8562727473908));
#430596=CARTESIAN_POINT('Ctrl Pts',(-2.21627823544945,1.47750481551776,
13.8564289040185));
#430597=CARTESIAN_POINT('Ctrl Pts',(-2.21510501569664,1.4784541675077,13.8571370725437));
#430598=CARTESIAN_POINT('Ctrl Pts',(-2.21393145359144,1.47953919945421,
13.8577210840553));
#430599=CARTESIAN_POINT('Ctrl Pts',(-2.2128230891778,1.48073928504898,13.8581177131616));
#430600=CARTESIAN_POINT('Ctrl Pts',(-2.21251093561018,1.48107727045816,
13.8582294175695));
#430601=CARTESIAN_POINT('Ctrl Pts',(-2.2122038490501,1.48142423795302,13.8583265086086));
#430602=CARTESIAN_POINT('Ctrl Pts',(-2.21190301456631,1.48177938708036,
13.8584082369006));
#430603=CARTESIAN_POINT('Ctrl Pts',(-2.21147079608506,1.48228964113935,
13.8585256585398));
#430604=CARTESIAN_POINT('Ctrl Pts',(-2.211046356362,1.4828233363635,13.8586122832068));
#430605=CARTESIAN_POINT('Ctrl Pts',(-2.21064133917199,1.48336710043221,
13.8586682984299));
#430606=CARTESIAN_POINT('Ctrl Pts',(-2.21031736556804,1.48380205778557,
13.8587131050557));
#430607=CARTESIAN_POINT('Ctrl Pts',(-2.21000205296354,1.48424812164223,
13.8587357943552));
#430608=CARTESIAN_POINT('Ctrl Pts',(-2.20969577744678,1.48470563734033,
13.8587355499465));
#430609=CARTESIAN_POINT('Ctrl Pts',(-2.20949782427831,1.48500134064375,
13.8587353919793));
#430610=CARTESIAN_POINT('Ctrl Pts',(-2.20930575471597,1.48529860856762,
13.8587257282814));
#430611=CARTESIAN_POINT('Ctrl Pts',(-2.20911943565999,1.48559738273759,
13.8587068136939));
#430612=CARTESIAN_POINT('Ctrl Pts',(-2.20911943565999,1.48559738273759,
13.8587068136939));
#430613=CARTESIAN_POINT('Ctrl Pts',(-2.20850664244234,1.48658003469455,
13.8586446046466));
#430614=CARTESIAN_POINT('Ctrl Pts',(-2.20795597628939,1.48757896052475,
13.858482427929));
#430615=CARTESIAN_POINT('Ctrl Pts',(-2.20746338346827,1.48859227523296,
13.8582284286032));
#430616=CARTESIAN_POINT('Ctrl Pts',(-2.20695804053452,1.48963181825003,
13.8579678548414));
#430617=CARTESIAN_POINT('Ctrl Pts',(-2.20651395923866,1.49068971361666,
13.857615680862));
#430618=CARTESIAN_POINT('Ctrl Pts',(-2.20613971274639,1.49172050412425,
13.8571944833187));
#430619=CARTESIAN_POINT('Ctrl Pts',(-2.20520574235014,1.49429294725656,
13.8561433417727));
#430620=CARTESIAN_POINT('Ctrl Pts',(-2.20465850952187,1.49681527480058,
13.8546163505474));
#430621=CARTESIAN_POINT('Ctrl Pts',(-2.20437450186005,1.49912164781843,
13.8528973491086));
#430622=CARTESIAN_POINT('Ctrl Pts',(-2.20432261785038,1.49954298814142,
13.8525833129072));
#430623=CARTESIAN_POINT('Ctrl Pts',(-2.20427938630757,1.49995717069509,
13.8522628768812));
#430624=CARTESIAN_POINT('Ctrl Pts',(-2.20424389852424,1.50036327237003,
13.851937733538));
#430625=CARTESIAN_POINT('Ctrl Pts',(-2.20402717955515,1.50284327895489,
13.8499521282529));
#430626=CARTESIAN_POINT('Ctrl Pts',(-2.20408177943199,1.50526874026406,
13.847639871647));
#430627=CARTESIAN_POINT('Ctrl Pts',(-2.20432450823963,1.50751399111926,
13.8452109780794));
#430628=CARTESIAN_POINT('Ctrl Pts',(-2.20443371695443,1.50852417595339,
13.8441181685877));
#430629=CARTESIAN_POINT('Ctrl Pts',(-2.20458036545448,1.50949820021415,
13.8430021611332));
#430630=CARTESIAN_POINT('Ctrl Pts',(-2.20475451431693,1.51042693500837,
13.8418824960098));
#430631=CARTESIAN_POINT('Ctrl Pts',(-2.20516490055834,1.51261552226703,
13.8392439765549));
#430632=CARTESIAN_POINT('Ctrl Pts',(-2.20574390287259,1.51465792831923,
13.8364981347964));
#430633=CARTESIAN_POINT('Ctrl Pts',(-2.20646012936871,1.51656888793135,
13.8336931113419));
#430634=CARTESIAN_POINT('Ctrl Pts',(-2.20715768849135,1.5184300412364,13.8309611966328));
#430635=CARTESIAN_POINT('Ctrl Pts',(-2.20798663946049,1.52016817766021,
13.8281701127186));
#430636=CARTESIAN_POINT('Ctrl Pts',(-2.20894724197503,1.52177067383454,
13.8253580685121));
#430637=CARTESIAN_POINT('Ctrl Pts',(-2.20915550163689,1.5221180967346,13.8247484142932));
#430638=CARTESIAN_POINT('Ctrl Pts',(-2.20937002295136,1.52245898744773,
13.8241378483365));
#430639=CARTESIAN_POINT('Ctrl Pts',(-2.20959091159279,1.5227929159564,13.8235269408515));
#430640=CARTESIAN_POINT('',(-2.20979706780673,1.48455642571058,12.5969504640361));
#430641=CARTESIAN_POINT('Origin',(-2.23828837686492,1.50384668585321,12.584524458991));
#430642=CARTESIAN_POINT('Origin',(-2.23828837686492,1.50384668585321,12.584524458991));
#430643=CARTESIAN_POINT('Ctrl Pts',(-2.24498269238234,1.47011665264502,
12.5893111709658));
#430644=CARTESIAN_POINT('Ctrl Pts',(-2.23386752565582,1.46790041637569,
12.5770542771492));
#430645=CARTESIAN_POINT('Ctrl Pts',(-2.22773157341713,1.48307123589803,
12.5737548217797));
#430646=CARTESIAN_POINT('Ctrl Pts',(-2.26928783165239,1.47496281757504,
12.5663937883685));
#430647=CARTESIAN_POINT('Ctrl Pts',(-2.25815848598708,1.47274375418857,
12.5540940315304));
#430648=CARTESIAN_POINT('Ctrl Pts',(-2.25200649659126,1.48796278903927,
12.5508374392248));
#430649=CARTESIAN_POINT('Ctrl Pts',(-2.2935684473349,1.47980409278406,12.5434499600944));
#430650=CARTESIAN_POINT('Ctrl Pts',(-2.28240291620359,1.47757781443226,
12.5311293540533));
#430651=CARTESIAN_POINT('Ctrl Pts',(-2.27625793571488,1.4928484064102,12.5278936106989));
#430652=CARTESIAN_POINT('Ctrl Pts',(-2.31782646039602,1.48464086129061,
12.5204817579905));
#430653=CARTESIAN_POINT('Ctrl Pts',(-2.30660566751615,1.48240356438245,
12.5081597038247));
#430654=CARTESIAN_POINT('Ctrl Pts',(-2.30048771879692,1.4977285357809,12.5049254088044));
#430655=CARTESIAN_POINT('Ctrl Pts',(-2.30038606421963,1.48116344709534,
12.5369868989719));
#430656=CARTESIAN_POINT('Ctrl Pts',(-2.30129958705399,1.48134559319564,
12.5342545179733));
#430657=CARTESIAN_POINT('Ctrl Pts',(-2.30214701877243,1.48164176307246,
12.5314872231885));
#430658=CARTESIAN_POINT('Ctrl Pts',(-2.30286217925637,1.48208804391716,
12.5287124745063));
#430659=CARTESIAN_POINT('Ctrl Pts',(-2.30350714647819,1.4824905221343,12.5262100684184));
#430660=CARTESIAN_POINT('Ctrl Pts',(-2.3040433616639,1.48301551890794,12.5237004536639));
#430661=CARTESIAN_POINT('Ctrl Pts',(-2.30443365549245,1.48371941612972,
12.5212220730815));
#430662=CARTESIAN_POINT('Ctrl Pts',(-2.3047324591813,1.48425831034496,12.5193246583486));
#430663=CARTESIAN_POINT('Ctrl Pts',(-2.30494875119866,1.48490881044974,
12.517417831369));
#430664=CARTESIAN_POINT('Ctrl Pts',(-2.30499813351841,1.48571919683289,
12.5155812248348));
#430665=CARTESIAN_POINT('Ctrl Pts',(-2.30501917065206,1.48606442578796,
12.5147988205793));
#430666=CARTESIAN_POINT('Ctrl Pts',(-2.30501021478349,1.48643900460363,
12.5140295443047));
#430667=CARTESIAN_POINT('Ctrl Pts',(-2.30496656771668,1.48684775597842,
12.5132817086137));
#430668=CARTESIAN_POINT('Ctrl Pts',(-2.30490051378551,1.48746634588954,
12.5121499604604));
#430669=CARTESIAN_POINT('Ctrl Pts',(-2.30474646989657,1.48817579891627,
12.5110494206568));
#430670=CARTESIAN_POINT('Ctrl Pts',(-2.30446743579976,1.48898034356171,
12.5100666561695));
#430671=CARTESIAN_POINT('Ctrl Pts',(-2.30430721506393,1.48944231124443,
12.5095023550641));
#430672=CARTESIAN_POINT('Ctrl Pts',(-2.30410331677059,1.48994075464284,
12.5089719619137));
#430673=CARTESIAN_POINT('Ctrl Pts',(-2.30385365127628,1.4904639127718,12.5085043804652));
#430674=CARTESIAN_POINT('Ctrl Pts',(-2.30348829834658,1.49122948654741,
12.5078201359221));
#430675=CARTESIAN_POINT('Ctrl Pts',(-2.30301325070733,1.49206966971377,
12.5072563000949));
#430676=CARTESIAN_POINT('Ctrl Pts',(-2.30245334000328,1.492923343416,12.5068768744332));
#430677=CARTESIAN_POINT('Ctrl Pts',(-2.30204960584128,1.49353890092241,
12.5066032824114));
#430678=CARTESIAN_POINT('Ctrl Pts',(-2.30159470517184,1.49417232005823,
12.5064197834844));
#430679=CARTESIAN_POINT('Ctrl Pts',(-2.30111614035319,1.49478973686366,
12.5063282718343));
#430680=CARTESIAN_POINT('Ctrl Pts',(-2.30041758387788,1.49569097425218,
12.5061946931565));
#430681=CARTESIAN_POINT('Ctrl Pts',(-2.29965451500638,1.49657802914186,
12.5062515701262));
#430682=CARTESIAN_POINT('Ctrl Pts',(-2.29888601479686,1.49740593435787,
12.5064436508398));
#430683=CARTESIAN_POINT('',(-2.22773157341713,1.48307123589803,12.5737548217797));
#430684=CARTESIAN_POINT('Origin',(-2.24068082430453,1.49169196100993,12.5893111709658));
#430685=CARTESIAN_POINT('Ctrl Pts',(-2.29888601479686,1.49740593435787,
12.5064436508398));
#430686=CARTESIAN_POINT('Ctrl Pts',(-2.28835321395465,1.49528449754067,
12.5164271754438));
#430687=CARTESIAN_POINT('Ctrl Pts',(-2.27781627916637,1.49316201496396,
12.5264061185523));
#430688=CARTESIAN_POINT('Ctrl Pts',(-2.26727506465103,1.49103845072481,
12.536380305637));
#430689=CARTESIAN_POINT('Ctrl Pts',(-2.25410068449553,1.48838442613112,
12.5488460165097));
#430690=CARTESIAN_POINT('Ctrl Pts',(-2.24091961554937,1.48572871118047,
12.5613043021964));
#430691=CARTESIAN_POINT('Ctrl Pts',(-2.22773157341713,1.48307123589803,
12.5737548217797));
#430692=CARTESIAN_POINT('Ctrl Pts',(-2.20959091159279,1.5227929159564,12.5893111709658));
#430693=CARTESIAN_POINT('Ctrl Pts',(-2.20333791462157,1.51333994481301,
12.5770542771492));
#430694=CARTESIAN_POINT('Ctrl Pts',(-2.21506416483591,1.50192509786855,
12.5737548217797));
#430695=CARTESIAN_POINT('Ctrl Pts',(-2.20375691980434,1.51397337609722,
12.5928319619712));
#430696=CARTESIAN_POINT('Ctrl Pts',(-2.20227160599699,1.505823084123,12.5821634970843));
#430697=CARTESIAN_POINT('Ctrl Pts',(-2.21293111045991,1.49871756043331,
12.5773203894503));
#430698=CARTESIAN_POINT('Ctrl Pts',(-2.20118490405364,1.49742137216061,
12.5969440695591));
#430699=CARTESIAN_POINT('Ctrl Pts',(-2.20341149200726,1.49407460526751,
12.5878292599214));
#430700=CARTESIAN_POINT('Ctrl Pts',(-2.21201641327838,1.49281777432162,
12.5813877129824));
#430701=CARTESIAN_POINT('Ctrl Pts',(-2.21820370745212,1.47199430830287,
12.596957478804));
#430702=CARTESIAN_POINT('Ctrl Pts',(-2.21599364131866,1.47531638609164,
12.5878468778671));
#430703=CARTESIAN_POINT('Ctrl Pts',(-2.21811263613238,1.48372039364263,
12.5814011370086));
#430704=CARTESIAN_POINT('Ctrl Pts',(-2.23459728076517,1.46804592114231,
12.5928371701607));
#430705=CARTESIAN_POINT('Ctrl Pts',(-2.22649724499558,1.46975603407284,
12.5821692192952));
#430706=CARTESIAN_POINT('Ctrl Pts',(-2.2239437249622,1.48230606823244,12.5773318885715));
#430707=CARTESIAN_POINT('Ctrl Pts',(-2.24498269238234,1.47011665264496,
12.5893111709658));
#430708=CARTESIAN_POINT('Ctrl Pts',(-2.23386752565583,1.46790041637563,
12.5770542771492));
#430709=CARTESIAN_POINT('Ctrl Pts',(-2.22773157341714,1.48307123589797,
12.5737548217797));
#430710=CARTESIAN_POINT('',(-2.21506416483591,1.50192509786855,12.5737548217797));
#430711=CARTESIAN_POINT('Origin',(-2.22793978322029,1.51065541580203,12.5893111709658));
#430712=CARTESIAN_POINT('Ctrl Pts',(-2.22773157341714,1.48307123589797,
12.5737548217797));
#430713=CARTESIAN_POINT('Ctrl Pts',(-2.22675567602634,1.48284332382357,
12.5746934679442));
#430714=CARTESIAN_POINT('Ctrl Pts',(-2.22563412055118,1.48276950814525,
12.5756680099006));
#430715=CARTESIAN_POINT('Ctrl Pts',(-2.22449472684561,1.48285486417438,
12.5765688348656));
#430716=CARTESIAN_POINT('Ctrl Pts',(-2.22419308497557,1.48287746123817,
12.5768073183026));
#430717=CARTESIAN_POINT('Ctrl Pts',(-2.22389023664768,1.48291096079766,
12.5770407398754));
#430718=CARTESIAN_POINT('Ctrl Pts',(-2.22358850687059,1.48295489580108,
12.5772674179684));
#430719=CARTESIAN_POINT('Ctrl Pts',(-2.22235028945663,1.48313519317458,
12.5781976435658));
#430720=CARTESIAN_POINT('Ctrl Pts',(-2.22106220670867,1.48351263233153,
12.5790594849312));
#430721=CARTESIAN_POINT('Ctrl Pts',(-2.21982481093434,1.48410806866006,
12.5797571720116));
#430722=CARTESIAN_POINT('Ctrl Pts',(-2.21901860309458,1.48449601683809,
12.580211740231));
#430723=CARTESIAN_POINT('Ctrl Pts',(-2.2182054139075,1.48501105113437,12.5806009430798));
#430724=CARTESIAN_POINT('Ctrl Pts',(-2.21745196790057,1.48563188265658,
12.5808812374708));
#430725=CARTESIAN_POINT('Ctrl Pts',(-2.21680450782752,1.48616538289287,
12.5811221033394));
#430726=CARTESIAN_POINT('Ctrl Pts',(-2.21618798251315,1.48678801945575,
12.581287365893));
#430727=CARTESIAN_POINT('Ctrl Pts',(-2.21564311448782,1.48747051642895,
12.581359338449));
#430728=CARTESIAN_POINT('Ctrl Pts',(-2.21556738908339,1.4875653694152,12.5813693411482));
#430729=CARTESIAN_POINT('Ctrl Pts',(-2.21549299118832,1.48766135899467,
12.5813775999465));
#430730=CARTESIAN_POINT('Ctrl Pts',(-2.21541997181832,1.48775838750229,
12.5813841266931));
#430731=CARTESIAN_POINT('Ctrl Pts',(-2.2152960856256,1.48792300810081,12.5813952001081));
#430732=CARTESIAN_POINT('Ctrl Pts',(-2.21517582431766,1.48809208794563,
12.5814007534795));
#430733=CARTESIAN_POINT('Ctrl Pts',(-2.21505940097739,1.48826566770161,
12.5814005856065));
#430734=CARTESIAN_POINT('Ctrl Pts',(-2.2145264604442,1.48906024795921,12.5813998171494));
#430735=CARTESIAN_POINT('Ctrl Pts',(-2.21411048442807,1.48989403423559,
12.58127954464));
#430736=CARTESIAN_POINT('Ctrl Pts',(-2.21378735740361,1.4907490833764,12.5810700125799));
#430737=CARTESIAN_POINT('Ctrl Pts',(-2.21339705674902,1.49178188538335,
12.5808169217085));
#430738=CARTESIAN_POINT('Ctrl Pts',(-2.21315784187356,1.49285171929701,
12.5804173076348));
#430739=CARTESIAN_POINT('Ctrl Pts',(-2.21306526238418,1.49385914393727,
12.5799304713245));
#430740=CARTESIAN_POINT('Ctrl Pts',(-2.21295052723128,1.49510766043804,
12.5793271277669));
#430741=CARTESIAN_POINT('Ctrl Pts',(-2.21302182717764,1.49633482347775,
12.5785808224116));
#430742=CARTESIAN_POINT('Ctrl Pts',(-2.21324449333399,1.49749074546726,
12.5777485681082));
#430743=CARTESIAN_POINT('Ctrl Pts',(-2.21357629030185,1.49921319587233,
12.576508418016));
#430744=CARTESIAN_POINT('Ctrl Pts',(-2.21423464280381,1.50076425728114,
12.5750928681475));
#430745=CARTESIAN_POINT('Ctrl Pts',(-2.21506416483591,1.50192509786855,
12.5737548217797));
#430746=CARTESIAN_POINT('Ctrl Pts',(-2.21506416483591,1.50192509786855,
12.5737548217797));
#430747=CARTESIAN_POINT('Ctrl Pts',(-2.20333791462157,1.51333994481301,
12.5770542771492));
#430748=CARTESIAN_POINT('Ctrl Pts',(-2.20959091159279,1.5227929159564,12.5893111709658));
#430749=CARTESIAN_POINT('Ctrl Pts',(-2.22876591246297,1.5225473447426,12.5508408821982));
#430750=CARTESIAN_POINT('Ctrl Pts',(-2.21700108902443,1.53399525521084,
12.55409748406));
#430751=CARTESIAN_POINT('Ctrl Pts',(-2.22326206321831,1.54346028592439,
12.5663972313419));
#430752=CARTESIAN_POINT('Ctrl Pts',(-2.2424532927753,1.54315009902394,12.52790050457));
#430753=CARTESIAN_POINT('Ctrl Pts',(-2.23063809519623,1.55461100577294,
12.5311362602938));
#430754=CARTESIAN_POINT('Ctrl Pts',(-2.2369194228983,1.56410680591216,12.5434568539655));
#430755=CARTESIAN_POINT('Ctrl Pts',(-2.25612741076335,1.56373488320074,
12.5049357605811));
#430756=CARTESIAN_POINT('Ctrl Pts',(-2.24425166104124,1.57519132040988,
12.5081700652078));
#430757=CARTESIAN_POINT('Ctrl Pts',(-2.25056407082075,1.58473410889444,
12.5204921097672));
#430758=CARTESIAN_POINT('Ctrl Pts',(-2.25522951325334,1.56238320646001,
12.5064436508395));
#430759=CARTESIAN_POINT('Ctrl Pts',(-2.25471532227217,1.56348975760002,
12.5062361689309));
#430760=CARTESIAN_POINT('Ctrl Pts',(-2.25413341993089,1.56461855398806,
12.5061871075061));
#430761=CARTESIAN_POINT('Ctrl Pts',(-2.25350965950472,1.56567777047767,
12.5063648335164));
#430762=CARTESIAN_POINT('Ctrl Pts',(-2.25322630904402,1.56615893194244,
12.5064455676329));
#430763=CARTESIAN_POINT('Ctrl Pts',(-2.25293017902171,1.5666323347451,12.506574497099));
#430764=CARTESIAN_POINT('Ctrl Pts',(-2.2526330756161,1.56707712344868,12.5067492519495));
#430765=CARTESIAN_POINT('Ctrl Pts',(-2.25203603478978,1.56797094361401,
12.5071004286051));
#430766=CARTESIAN_POINT('Ctrl Pts',(-2.25141244009367,1.56878162667607,
12.5076537929613));
#430767=CARTESIAN_POINT('Ctrl Pts',(-2.25081659260674,1.56945409349212,
12.5083435010505));
#430768=CARTESIAN_POINT('Ctrl Pts',(-2.25077908044664,1.56949642929687,
12.5083869222964));
#430769=CARTESIAN_POINT('Ctrl Pts',(-2.25074166523779,1.56953821398961,
12.5084308732337));
#430770=CARTESIAN_POINT('Ctrl Pts',(-2.25070435512934,1.56957943286714,
12.5084753333615));
#430771=CARTESIAN_POINT('Ctrl Pts',(-2.25040507881477,1.56991006266887,
12.5088319622689));
#430772=CARTESIAN_POINT('Ctrl Pts',(-2.25010744547243,1.57021186510831,
12.509227847131));
#430773=CARTESIAN_POINT('Ctrl Pts',(-2.24982229895179,1.57047783214431,
12.5096423454524));
#430774=CARTESIAN_POINT('Ctrl Pts',(-2.24892877595666,1.57131125512306,
12.5109411997424));
#430775=CARTESIAN_POINT('Ctrl Pts',(-2.24810950077872,1.57185113499161,
12.5124831113042));
#430776=CARTESIAN_POINT('Ctrl Pts',(-2.24738040813741,1.57219075595073,
12.5140723025008));
#430777=CARTESIAN_POINT('Ctrl Pts',(-2.24731209135837,1.57222257880657,
12.5142212114565));
#430778=CARTESIAN_POINT('Ctrl Pts',(-2.24724456077942,1.57225267248488,
12.5143705582413));
#430779=CARTESIAN_POINT('Ctrl Pts',(-2.24717782783351,1.57228113062874,
12.5145201959299));
#430780=CARTESIAN_POINT('Ctrl Pts',(-2.24632054378837,1.57264671785638,
12.5164425148273));
#430781=CARTESIAN_POINT('Ctrl Pts',(-2.24556973353945,1.57276479304203,
12.518463520594));
#430782=CARTESIAN_POINT('Ctrl Pts',(-2.24489212546417,1.57271920711102,
12.5205025929157));
#430783=CARTESIAN_POINT('Ctrl Pts',(-2.24449908592263,1.57269276546418,
12.5216853356836));
#430784=CARTESIAN_POINT('Ctrl Pts',(-2.24413135248927,1.57261179092169,
12.5228750347131));
#430785=CARTESIAN_POINT('Ctrl Pts',(-2.24378805546091,1.57249450921438,
12.5240609649613));
#430786=CARTESIAN_POINT('Ctrl Pts',(-2.24294545132205,1.57220664755573,
12.5269717671326));
#430787=CARTESIAN_POINT('Ctrl Pts',(-2.24222970611256,1.57168212130923,
12.5299036066169));
#430788=CARTESIAN_POINT('Ctrl Pts',(-2.2416015010593,1.57099815454307,12.5328133004019));
#430789=CARTESIAN_POINT('Ctrl Pts',(-2.24129992605445,1.57066981066912,
12.5342101228451));
#430790=CARTESIAN_POINT('Ctrl Pts',(-2.24101928745411,1.57030477795461,
12.5356023438238));
#430791=CARTESIAN_POINT('Ctrl Pts',(-2.2407588755845,1.56991110033548,12.5369868989719));
#430792=CARTESIAN_POINT('Origin',(-9.26738283409461,12.2020107234904,-1.2388424640659));
#430793=CARTESIAN_POINT('Ctrl Pts',(-2.30034508453518,1.48115523573753,
12.5369868989719));
#430794=CARTESIAN_POINT('Ctrl Pts',(-2.31538220108036,1.48418317723182,
12.5369868989719));
#430795=CARTESIAN_POINT('Ctrl Pts',(-2.32342295645086,1.47112065233202,
12.5369868989719));
#430796=CARTESIAN_POINT('Ctrl Pts',(-2.30542823109593,1.48217873347564,
12.5218025310016));
#430797=CARTESIAN_POINT('Ctrl Pts',(-2.31720240784264,1.48116649553802,
12.5216901060418));
#430798=CARTESIAN_POINT('Ctrl Pts',(-2.32339845960796,1.471160479882,12.5161920673678));
#430799=CARTESIAN_POINT('Ctrl Pts',(-2.30790882579116,1.48767261381232,
12.5042015548894));
#430800=CARTESIAN_POINT('Ctrl Pts',(-2.31410372809367,1.48594040987532,
12.4980677368513));
#430801=CARTESIAN_POINT('Ctrl Pts',(-2.31777081800236,1.48021823971661,
12.4907278922777));
#430802=CARTESIAN_POINT('Ctrl Pts',(-2.29886925544556,1.49739501797345,
12.506463626192));
#430803=CARTESIAN_POINT('Ctrl Pts',(-2.3043515601987,1.50096598043898,12.4999376786891));
#430804=CARTESIAN_POINT('Ctrl Pts',(-2.3042846018174,1.50092236632464,12.4906970594712));
#430805=CARTESIAN_POINT('Origin',(-2.30468793229744,1.45958813873043,12.5369868989719));
#430806=CARTESIAN_POINT('Origin',(-2.30468793229744,1.45958813873043,14.));
#430807=CARTESIAN_POINT('Origin',(-2.30468793229744,1.45958813873043,13.7435492065112));
#430808=CARTESIAN_POINT('Ctrl Pts',(-2.27610393869126,1.47632184315448,
13.793642941384));
#430809=CARTESIAN_POINT('Ctrl Pts',(-2.28670217728922,1.47846276763383,
13.8071662555867));
#430810=CARTESIAN_POINT('Ctrl Pts',(-2.29249185652868,1.46244718153968,
13.8103758687955));
#430811=CARTESIAN_POINT('Ctrl Pts',(-2.29240420348061,1.47957193131032,
13.7804579775005));
#430812=CARTESIAN_POINT('Ctrl Pts',(-2.30548347994049,1.48220369859024,
13.7901904343351));
#430813=CARTESIAN_POINT('Ctrl Pts',(-2.31316693237331,1.46844795495796,
13.7927914348262));
#430814=CARTESIAN_POINT('Ctrl Pts',(-2.30200078281746,1.48148538048494,
13.7597120340895));
#430815=CARTESIAN_POINT('Ctrl Pts',(-2.31713831944396,1.48452545858477,
13.7635825532445));
#430816=CARTESIAN_POINT('Ctrl Pts',(-2.325366126179,1.47196205488693,13.7651073818884));
#430817=CARTESIAN_POINT('Ctrl Pts',(-2.3001215528468,1.48111068332275,13.7381884353898));
#430818=CARTESIAN_POINT('Ctrl Pts',(-2.31490459024643,1.48408048396722,
13.7368803041982));
#430819=CARTESIAN_POINT('Ctrl Pts',(-2.32297729833982,1.47127341478032,
13.7363986145813));
#430820=CARTESIAN_POINT('Origin',(-2.28436103174886,1.45553518879749,13.7902182540695));
#430821=CARTESIAN_POINT('Ctrl Pts',(-2.24497883231734,1.47011588221864,
13.8235227101244));
#430822=CARTESIAN_POINT('Ctrl Pts',(-2.25625309620494,1.4723683613223,13.8358800583119));
#430823=CARTESIAN_POINT('Ctrl Pts',(-2.26236341763185,1.4569641404359,13.8390832900376));
#430824=CARTESIAN_POINT('Ctrl Pts',(-2.25667615971092,1.47244819462107,
13.8124254819053));
#430825=CARTESIAN_POINT('Ctrl Pts',(-2.26797231811368,1.47470504773445,
13.8247886449158));
#430826=CARTESIAN_POINT('Ctrl Pts',(-2.27407451681287,1.45927507844938,
13.8279860620657));
#430827=CARTESIAN_POINT('Ctrl Pts',(-2.26836824474284,1.47477946175696,
13.8013225099954));
#430828=CARTESIAN_POINT('Ctrl Pts',(-2.2796809672952,1.47703962597359,13.8136962257787));
#430829=CARTESIAN_POINT('Ctrl Pts',(-2.28578014185561,1.4615852125404,13.8168830918626));
#430830=CARTESIAN_POINT('Ctrl Pts',(-2.28005529138546,1.47710972429605,
13.7902140179785));
#430831=CARTESIAN_POINT('Ctrl Pts',(-2.29137959610102,1.47937220617531,
13.802602731458));
#430832=CARTESIAN_POINT('Ctrl Pts',(-2.29748050749599,1.46389457610245,
13.8057746032558));
#430833=CARTESIAN_POINT('Origin',(-2.24928456046014,1.4485413442801,13.8235269408515));
#430834=CARTESIAN_POINT('Ctrl Pts',(-2.20959091159279,1.5227929159564,13.8235269408515));
#430835=CARTESIAN_POINT('Ctrl Pts',(-2.21610515287597,1.53264082331256,
13.8362179249168));
#430836=CARTESIAN_POINT('Ctrl Pts',(-2.20357280835889,1.54424269147948,
13.8391868794938));
#430837=CARTESIAN_POINT('Ctrl Pts',(-2.20363066436673,1.5137825093794,13.8400110824519));
#430838=CARTESIAN_POINT('Ctrl Pts',(-2.20600024377829,1.52356550259586,
13.8494522556837));
#430839=CARTESIAN_POINT('Ctrl Pts',(-2.19385763417706,1.5293521181446,13.85569149686));
#430840=CARTESIAN_POINT('Ctrl Pts',(-2.20099260876462,1.49770649032351,
13.8586819406588));
#430841=CARTESIAN_POINT('Ctrl Pts',(-2.19857607065724,1.50132814563712,
13.868010383617));
#430842=CARTESIAN_POINT('Ctrl Pts',(-2.18962248223092,1.50264196491109,
13.8744918421245));
#430843=CARTESIAN_POINT('Ctrl Pts',(-2.21839896968065,1.47170475773493,
13.8587686893867));
#430844=CARTESIAN_POINT('Ctrl Pts',(-2.22079395378256,1.4681153038668,13.8680909899357));
#430845=CARTESIAN_POINT('Ctrl Pts',(-2.2186010995933,1.45935814725004,13.8745789365163));
#430846=CARTESIAN_POINT('Ctrl Pts',(-2.23437066984899,1.4680007375281,13.8400379222776));
#430847=CARTESIAN_POINT('Ctrl Pts',(-2.24431996677128,1.46649019965689,
13.8494748685453));
#430848=CARTESIAN_POINT('Ctrl Pts',(-2.24508859442963,1.45306744596076,
13.8557104837033));
#430849=CARTESIAN_POINT('Ctrl Pts',(-2.24498269238349,1.47011665263851,
13.8235269408542));
#430850=CARTESIAN_POINT('Ctrl Pts',(-2.25656224028548,1.47242548116746,
13.8362179249195));
#430851=CARTESIAN_POINT('Ctrl Pts',(-2.26256666355615,1.45643767627614,
13.8391868794965));
#430852=CARTESIAN_POINT('Origin',(-2.19124203996528,1.53493041611077,13.8235269408515));
#430853=CARTESIAN_POINT('Ctrl Pts',(-2.22932150926554,1.55262065774392,
13.7902140241682));
#430854=CARTESIAN_POINT('Ctrl Pts',(-2.23569636053668,1.56224977331409,
13.8026027327198));
#430855=CARTESIAN_POINT('Ctrl Pts',(-2.22367281973875,1.5737481383698,13.8057746032556));
#430856=CARTESIAN_POINT('Ctrl Pts',(-2.22274679301792,1.54268132732958,
13.8013225161807));
#430857=CARTESIAN_POINT('Ctrl Pts',(-2.22911512089271,1.552300595907,13.8136962270464));
#430858=CARTESIAN_POINT('Ctrl Pts',(-2.21711241802939,1.56378857785723,
13.8168830918628));
#430859=CARTESIAN_POINT('Ctrl Pts',(-2.216169242351,1.53273771198048,13.8124254880875));
#430860=CARTESIAN_POINT('Ctrl Pts',(-2.22252824406069,1.54234289663759,
13.8247886461868));
#430861=CARTESIAN_POINT('Ctrl Pts',(-2.21054931507107,1.55382443932404,
13.8279860620656));
#430862=CARTESIAN_POINT('Ctrl Pts',(-2.20958874251634,1.52278963822562,
13.8235227163065));
#430863=CARTESIAN_POINT('Ctrl Pts',(-2.21593541930373,1.5323762057549,13.8358800595847));
#430864=CARTESIAN_POINT('Ctrl Pts',(-2.20398339878361,1.54385553658406,
13.8390832900376));
#430865=CARTESIAN_POINT('Origin',(-2.21097481358226,1.56476144600553,13.7902182540695));
#430866=CARTESIAN_POINT('Ctrl Pts',(-2.24060996964151,1.56968604170401,
13.7382347919292));
#430867=CARTESIAN_POINT('Ctrl Pts',(-2.24895537660476,1.58225871251618,
13.7369371795943));
#430868=CARTESIAN_POINT('Ctrl Pts',(-2.24013602089833,1.59457791467962,
13.7364597369711));
#430869=CARTESIAN_POINT('Ctrl Pts',(-2.24165355147467,1.57126367630735,
13.7595490285574));
#430870=CARTESIAN_POINT('Ctrl Pts',(-2.25019723501361,1.58413687629824,
13.7633824266925));
#430871=CARTESIAN_POINT('Ctrl Pts',(-2.24165789716282,1.59650511664909,
13.7648920890506));
#430872=CARTESIAN_POINT('Ctrl Pts',(-2.23633134130424,1.56321782625572,
13.7803806590111));
#430873=CARTESIAN_POINT('Ctrl Pts',(-2.24372581974754,1.57434969827063,
13.7901039518745));
#430874=CARTESIAN_POINT('Ctrl Pts',(-2.23390211956567,1.58667772958803,
13.7926933640892));
#430875=CARTESIAN_POINT('Ctrl Pts',(-2.22708015189695,1.54923234284881,
13.7936647693663));
#430876=CARTESIAN_POINT('Ctrl Pts',(-2.23307204524306,1.55823626122213,
13.8072068914933));
#430877=CARTESIAN_POINT('Ctrl Pts',(-2.22041213299701,1.56965426856883,
13.8104111085397));
#430878=CARTESIAN_POINT('Origin',(-2.22241000395699,1.58204860048985,13.7435492065112));
#430879=CARTESIAN_POINT('Origin',(-2.22241000395699,1.58204860048985,14.));
#430880=CARTESIAN_POINT('Origin',(-2.22241000395699,1.58204860048985,12.5369868989719));
#430881=CARTESIAN_POINT('Ctrl Pts',(-2.2552144020631,1.56237273768155,12.506462012331));
#430882=CARTESIAN_POINT('Ctrl Pts',(-2.26058921242423,1.56609631144499,
12.4999388158272));
#430883=CARTESIAN_POINT('Ctrl Pts',(-2.26052562136902,1.5660522566842,12.4907030323752));
#430884=CARTESIAN_POINT('Ctrl Pts',(-2.24962821177142,1.57441528978563,
12.5042014951932));
#430885=CARTESIAN_POINT('Ctrl Pts',(-2.25036659662837,1.58080245542613,
12.4980716682127));
#430886=CARTESIAN_POINT('Ctrl Pts',(-2.24645898522011,1.58635728560428,
12.4907355092743));
#430887=CARTESIAN_POINT('Ctrl Pts',(-2.24360506409332,1.57419758977853,
12.5218047446509));
#430888=CARTESIAN_POINT('Ctrl Pts',(-2.24711536434996,1.58547573958442,
12.5216906929434));
#430889=CARTESIAN_POINT('Ctrl Pts',(-2.2402000344604,1.59499146167199,12.5161988840776));
#430890=CARTESIAN_POINT('Ctrl Pts',(-2.24073765326595,1.56987907828033,
12.5369868989719));
#430891=CARTESIAN_POINT('Ctrl Pts',(-2.24921753683209,1.58265002602219,
12.5369868989719));
#430892=CARTESIAN_POINT('Ctrl Pts',(-2.24017344252634,1.59502782427993,
12.5369868989719));
#430893=CARTESIAN_POINT('Origin',(-4.27630463278518E-31,-2.27872721465334E-31,
12.5));
#430894=CARTESIAN_POINT('Origin',(-2.32636043968303,1.3376237760141,12.5));
#430895=CARTESIAN_POINT('',(-2.32636043968303,1.3376237760141,12.5893111709658));
#430896=CARTESIAN_POINT('',(-2.32636043968303,1.3376237760141,13.8235269408515));
#430897=CARTESIAN_POINT('',(-2.32636043968303,1.3376237760141,12.5));
#430898=CARTESIAN_POINT('',(-2.34845905999784,1.36574714137786,13.7902182540695));
#430899=CARTESIAN_POINT('',(-2.32636043968303,1.3376237760141,13.8235269408515));
#430900=CARTESIAN_POINT('',(-2.36126526429652,1.38204470010705,13.7435492065112));
#430901=CARTESIAN_POINT('Origin',(-2.31913327757043,1.3284257460468,13.7445212918724));
#430902=CARTESIAN_POINT('',(-2.36126526429652,1.38204470010705,12.5369868989719));
#430903=CARTESIAN_POINT('',(-2.36126526429652,1.38204470010705,12.5));
#430904=CARTESIAN_POINT('Ctrl Pts',(-2.36126526429652,1.38204470010705,
12.5369868989719));
#430905=CARTESIAN_POINT('Ctrl Pts',(-2.34963880857739,1.36724852471616,
12.5544431401645));
#430906=CARTESIAN_POINT('Ctrl Pts',(-2.33800403730813,1.35244176670738,
12.5718848856037));
#430907=CARTESIAN_POINT('Ctrl Pts',(-2.32636043968303,1.3376237760141,12.5893111709658));
#430908=CARTESIAN_POINT('Origin',(-2.63051785889797,1.31385010542184,12.5));
#430909=CARTESIAN_POINT('',(-2.41346029074828,1.28873217793633,13.7435492065112));
#430910=CARTESIAN_POINT('',(-2.39287067323913,1.28634954496039,13.7902182540695));
#430911=CARTESIAN_POINT('Origin',(-2.3387647170221,1.28008839730092,13.741873268043));
#430912=CARTESIAN_POINT('',(-2.35734085275917,1.28223802992779,13.8235269408515));
#430913=CARTESIAN_POINT('',(-2.39287067323913,1.28634954496039,13.7902182540695));
#430914=CARTESIAN_POINT('',(-2.35734085275917,1.28223802992779,12.5893111709658));
#430915=CARTESIAN_POINT('',(-2.35734085275917,1.28223802992779,12.5));
#430916=CARTESIAN_POINT('',(-2.41346029074828,1.28873217793633,12.5369868989719));
#430917=CARTESIAN_POINT('Ctrl Pts',(-2.35734085275917,1.28223802992779,
12.5893111709658));
#430918=CARTESIAN_POINT('Ctrl Pts',(-2.37606124921231,1.28440435642181,
12.5718848856037));
#430919=CARTESIAN_POINT('Ctrl Pts',(-2.39476745478685,1.28656904074567,
12.5544431401645));
#430920=CARTESIAN_POINT('Ctrl Pts',(-2.41346029074828,1.28873217793633,
12.5369868989719));
#430921=CARTESIAN_POINT('',(-2.41346029074828,1.28873217793633,12.5));
#430922=CARTESIAN_POINT('Origin',(-2.35338934332242,1.31638515569514,12.5));
#430923=CARTESIAN_POINT('',(-2.32285875128382,1.30059043752891,13.8587068136939));
#430924=CARTESIAN_POINT('Ctrl Pts',(-2.35734085275979,1.28223802992121,
13.8235269408542));
#430925=CARTESIAN_POINT('Ctrl Pts',(-2.35560017053849,1.28203659796847,
13.8262006681044));
#430926=CARTESIAN_POINT('Ctrl Pts',(-2.35379886475506,1.28200304939745,
13.8288634856214));
#430927=CARTESIAN_POINT('Ctrl Pts',(-2.35194281077231,1.28212541398842,
13.8314912288862));
#430928=CARTESIAN_POINT('Ctrl Pts',(-2.35002941055919,1.28225155926039,
13.8342001611531));
#430929=CARTESIAN_POINT('Ctrl Pts',(-2.34805566878626,1.28254304529319,
13.8368750301949));
#430930=CARTESIAN_POINT('Ctrl Pts',(-2.34601106352842,1.28302865671952,
13.8394886372969));
#430931=CARTESIAN_POINT('Ctrl Pts',(-2.34585315370484,1.2830661616679,13.8396904925131));
#430932=CARTESIAN_POINT('Ctrl Pts',(-2.34569482252017,1.28310484665314,
13.8398919674349));
#430933=CARTESIAN_POINT('Ctrl Pts',(-2.3455360668143,1.28314473625469,13.8400930404591));
#430934=CARTESIAN_POINT('Ctrl Pts',(-2.34306254611124,1.28376624308328,
13.8432258934518));
#430935=CARTESIAN_POINT('Ctrl Pts',(-2.34049831695584,1.28467591649807,
13.8462331177034));
#430936=CARTESIAN_POINT('Ctrl Pts',(-2.33795926323475,1.28593500275606,
13.8489036603661));
#430937=CARTESIAN_POINT('Ctrl Pts',(-2.33712845530876,1.28634699043239,
13.8497774930041));
#430938=CARTESIAN_POINT('Ctrl Pts',(-2.33630059101433,1.28679641860967,
13.85061494757));
#430939=CARTESIAN_POINT('Ctrl Pts',(-2.33548044031406,1.28728550608083,
13.8514076489583));
#430940=CARTESIAN_POINT('Ctrl Pts',(-2.33374570329957,1.28831999661928,
13.8530843267192));
#430941=CARTESIAN_POINT('Ctrl Pts',(-2.3318765938024,1.2896360710072,13.8546805203176));
#430942=CARTESIAN_POINT('Ctrl Pts',(-2.33006014880899,1.29126890915697,
13.8559412814273));
#430943=CARTESIAN_POINT('Ctrl Pts',(-2.32981704956014,1.29148743585562,
13.8561100121513));
#430944=CARTESIAN_POINT('Ctrl Pts',(-2.32957489149108,1.29171155935421,
13.8562727473908));
#430945=CARTESIAN_POINT('Ctrl Pts',(-2.32933411140126,1.29194128901726,
13.8564289040185));
#430946=CARTESIAN_POINT('Ctrl Pts',(-2.32824217644093,1.29298311041826,
13.8571370725437));
#430947=CARTESIAN_POINT('Ctrl Pts',(-2.32716095944341,1.29416018821688,
13.8577210840554));
#430948=CARTESIAN_POINT('Ctrl Pts',(-2.32615410113795,1.2954466226151,13.8581177131616));
#430949=CARTESIAN_POINT('Ctrl Pts',(-2.32587053518412,1.29580892681936,
13.8582294175695));
#430950=CARTESIAN_POINT('Ctrl Pts',(-2.32559275150116,1.296179770214,13.8583265086086));
#430951=CARTESIAN_POINT('Ctrl Pts',(-2.32532186597022,1.29655825841516,
13.8584082369006));
#430952=CARTESIAN_POINT('Ctrl Pts',(-2.32493267610309,1.2971020444646,13.8585256585398));
#430953=CARTESIAN_POINT('Ctrl Pts',(-2.32455314978355,1.29766855963966,
13.8586122832068));
#430954=CARTESIAN_POINT('Ctrl Pts',(-2.32419380207448,1.29824352703926,
13.8586682984299));
#430955=CARTESIAN_POINT('Ctrl Pts',(-2.32390635952822,1.29870344396426,
13.8587131050557));
#430956=CARTESIAN_POINT('Ctrl Pts',(-2.32362845444578,1.29917372448472,
13.8587357943552));
#430957=CARTESIAN_POINT('Ctrl Pts',(-2.32336048981229,1.29965468213501,
13.8587355499465));
#430958=CARTESIAN_POINT('Ctrl Pts',(-2.32318729788112,1.29996553653094,
13.8587353919793));
#430959=CARTESIAN_POINT('Ctrl Pts',(-2.32302009750993,1.30027747077265,
13.8587257282814));
#430960=CARTESIAN_POINT('Ctrl Pts',(-2.32285875128382,1.30059043752891,
13.8587068136939));
#430961=CARTESIAN_POINT('Ctrl Pts',(-2.32285875128382,1.30059043752891,
13.8587068136939));
#430962=CARTESIAN_POINT('Ctrl Pts',(-2.32232809234198,1.30161976812876,
13.8586446046466));
#430963=CARTESIAN_POINT('Ctrl Pts',(-2.32186068021392,1.30266025451934,
13.858482427929));
#430964=CARTESIAN_POINT('Ctrl Pts',(-2.32145232101062,1.30371034839446,
13.8582284286032));
#430965=CARTESIAN_POINT('Ctrl Pts',(-2.32103339197034,1.30478762255838,
13.8579678548414));
#430966=CARTESIAN_POINT('Ctrl Pts',(-2.32067701661175,1.30587819461371,
13.857615680862));
#430967=CARTESIAN_POINT('Ctrl Pts',(-2.32038803438958,1.30693605981437,
13.8571944833187));
#430968=CARTESIAN_POINT('Ctrl Pts',(-2.31966684969946,1.30957607061221,
13.8561433417727));
#430969=CARTESIAN_POINT('Ctrl Pts',(-2.31932703085426,1.31213460987516,
13.8546163505474));
#430970=CARTESIAN_POINT('Ctrl Pts',(-2.31923195901678,1.31445645788808,
13.8528973491086));
#430971=CARTESIAN_POINT('Ctrl Pts',(-2.31921459079473,1.31488062526437,
13.8525833129072));
#430972=CARTESIAN_POINT('Ctrl Pts',(-2.31920526282451,1.31529695343186,
13.8522628768812));
#430973=CARTESIAN_POINT('Ctrl Pts',(-2.31920299418043,1.31570459642078,
13.851937733538));
#430974=CARTESIAN_POINT('Ctrl Pts',(-2.31918913988576,1.31819401559622,
13.8499521282529));
#430975=CARTESIAN_POINT('Ctrl Pts',(-2.31944125569959,1.32060695598612,
13.847639871647));
#430976=CARTESIAN_POINT('Ctrl Pts',(-2.31986618563574,1.32282495130311,
13.8452109780794));
#430977=CARTESIAN_POINT('Ctrl Pts',(-2.32005737040963,1.32382287330644,
13.8441181685877));
#430978=CARTESIAN_POINT('Ctrl Pts',(-2.32028292296854,1.32478170336765,
13.8430021611332));
#430979=CARTESIAN_POINT('Ctrl Pts',(-2.3205321928727,1.32569315312445,13.8418824960098));
#430980=CARTESIAN_POINT('Ctrl Pts',(-2.32111960376718,1.32784100775104,
13.8392439765549));
#430981=CARTESIAN_POINT('Ctrl Pts',(-2.32186315455302,1.32982942380178,
13.8364981347964));
#430982=CARTESIAN_POINT('Ctrl Pts',(-2.32273275881343,1.33167564574487,
13.8336931113419));
#430983=CARTESIAN_POINT('Ctrl Pts',(-2.32357969813809,1.3334737486715,13.8309611966328));
#430984=CARTESIAN_POINT('Ctrl Pts',(-2.32454756509587,1.33513853439016,
13.8281701127186));
#430985=CARTESIAN_POINT('Ctrl Pts',(-2.32563558959985,1.33665740036793,
13.8253580685121));
#430986=CARTESIAN_POINT('Ctrl Pts',(-2.32587147448655,1.33698669215113,
13.8247484142933));
#430987=CARTESIAN_POINT('Ctrl Pts',(-2.32611306775684,1.3373089630999,13.8241378483365));
#430988=CARTESIAN_POINT('Ctrl Pts',(-2.32636043968303,1.3376237760141,13.8235269408515));
#430989=CARTESIAN_POINT('',(-2.3234492810039,1.29949771088997,12.5969504640361));
#430990=CARTESIAN_POINT('Origin',(-2.35341812286521,1.31640147809467,12.584524458991));
#430991=CARTESIAN_POINT('Origin',(-2.35341812286521,1.31640147809467,12.584524458991));
#430992=CARTESIAN_POINT('Ctrl Pts',(-2.35734085275917,1.28223802992779,
12.5893111709658));
#430993=CARTESIAN_POINT('Ctrl Pts',(-2.34608202700252,1.2809351572782,12.5770542771492));
#430994=CARTESIAN_POINT('Ctrl Pts',(-2.34120305426881,1.29655563422094,
12.5737548217797));
#430995=CARTESIAN_POINT('Ctrl Pts',(-2.38196012611476,1.28508697515537,
12.5663937883685));
#430996=CARTESIAN_POINT('Ctrl Pts',(-2.37068693816224,1.28378244051078,
12.5540940315304));
#430997=CARTESIAN_POINT('Ctrl Pts',(-2.36579591163059,1.29945227952655,
12.5508374392248));
#430998=CARTESIAN_POINT('Ctrl Pts',(-2.40655455892536,1.28793304583215,
12.5434499600945));
#430999=CARTESIAN_POINT('Ctrl Pts',(-2.3952447178243,1.28662426968091,12.5311293540533));
#431000=CARTESIAN_POINT('Ctrl Pts',(-2.39036487926272,1.30234492298075,
12.5278936106989));
#431001=CARTESIAN_POINT('Ctrl Pts',(-2.43112609698477,1.29077646712561,
12.5204817579905));
#431002=CARTESIAN_POINT('Ctrl Pts',(-2.41976027989949,1.28946121342681,
12.5081597038247));
#431003=CARTESIAN_POINT('Ctrl Pts',(-2.41491181558899,1.30523386186405,
12.5049254088044));
#431004=CARTESIAN_POINT('Ctrl Pts',(-2.41346029074828,1.28873217793633,
12.5369868989719));
#431005=CARTESIAN_POINT('Ctrl Pts',(-2.41438562050889,1.28883925736877,
12.5342545179733));
#431006=CARTESIAN_POINT('Ctrl Pts',(-2.41525437306266,1.28906536821254,
12.5314872231885));
#431007=CARTESIAN_POINT('Ctrl Pts',(-2.416003529941,1.28945187187587,12.5287124745063));
#431008=CARTESIAN_POINT('Ctrl Pts',(-2.41667915679872,1.28980044006379,
12.5262100684184));
#431009=CARTESIAN_POINT('Ctrl Pts',(-2.41725637988353,1.29027998343836,
12.5237004536639));
#431010=CARTESIAN_POINT('Ctrl Pts',(-2.41770274919979,1.29094972592987,
12.5212220730815));
#431011=CARTESIAN_POINT('Ctrl Pts',(-2.41804448352542,1.29146247174446,
12.5193246583486));
#431012=CARTESIAN_POINT('Ctrl Pts',(-2.41831307764641,1.29209317755643,
12.517417831369));
#431013=CARTESIAN_POINT('Ctrl Pts',(-2.41842834966406,1.29289684232824,
12.5155812248348));
#431014=CARTESIAN_POINT('Ctrl Pts',(-2.41847745616316,1.29323920784074,
12.5147988205794));
#431015=CARTESIAN_POINT('Ctrl Pts',(-2.41849906174541,1.29361327026274,
12.5140295443047));
#431016=CARTESIAN_POINT('Ctrl Pts',(-2.41848887694232,1.29402421919219,
12.5132817086137));
#431017=CARTESIAN_POINT('Ctrl Pts',(-2.41847346362062,1.29464613480501,
12.5121499604604));
#431018=CARTESIAN_POINT('Ctrl Pts',(-2.41837775930793,1.29536578319234,
12.5110494206568));
#431019=CARTESIAN_POINT('Ctrl Pts',(-2.41816523153169,1.29619039465117,
12.5100666561695));
#431020=CARTESIAN_POINT('Ctrl Pts',(-2.41804319857198,1.29666388465191,
12.5095023550641));
#431021=CARTESIAN_POINT('Ctrl Pts',(-2.41788060649771,1.29717728912481,
12.5089719619137));
#431022=CARTESIAN_POINT('Ctrl Pts',(-2.41767441398901,1.29771905654383,
12.5085043804652));
#431023=CARTESIAN_POINT('Ctrl Pts',(-2.41737267811099,1.29851186259139,
12.5078201359221));
#431024=CARTESIAN_POINT('Ctrl Pts',(-2.41696769388149,1.29938797091034,
12.5072563000949));
#431025=CARTESIAN_POINT('Ctrl Pts',(-2.41647922856598,1.30028444200408,
12.5068768744332));
#431026=CARTESIAN_POINT('Ctrl Pts',(-2.41612701144742,1.30093085937595,
12.5066032824114));
#431027=CARTESIAN_POINT('Ctrl Pts',(-2.41572525396238,1.3015992494895,12.5064197834844));
#431028=CARTESIAN_POINT('Ctrl Pts',(-2.41529860673015,1.30225361936695,
12.5063282718343));
#431029=CARTESIAN_POINT('Ctrl Pts',(-2.41467583385773,1.30320879680022,
12.5061946931565));
#431030=CARTESIAN_POINT('Ctrl Pts',(-2.41398760724347,1.30415509728495,
12.5062515701262));
#431031=CARTESIAN_POINT('Ctrl Pts',(-2.41328914611601,1.30504288761613,
12.5064436508398));
#431032=CARTESIAN_POINT('',(-2.34120305426881,1.29655563422094,12.5737548217797));
#431033=CARTESIAN_POINT('Origin',(-2.35481188671965,1.30409219041889,12.5893111709658));
#431034=CARTESIAN_POINT('Ctrl Pts',(-2.41328914611601,1.30504288761613,
12.5064436508398));
#431035=CARTESIAN_POINT('Ctrl Pts',(-2.40261847550464,1.30378703075533,
12.5164271754438));
#431036=CARTESIAN_POINT('Ctrl Pts',(-2.39194359946346,1.30253046856967,
12.5264061185523));
#431037=CARTESIAN_POINT('Ctrl Pts',(-2.38126436977013,1.30127317715821,
12.536380305637));
#431038=CARTESIAN_POINT('Ctrl Pts',(-2.36791749863464,1.29970181790006,
12.5488460165097));
#431039=CARTESIAN_POINT('Ctrl Pts',(-2.35456382318511,1.29812931910801,
12.5613043021964));
#431040=CARTESIAN_POINT('Ctrl Pts',(-2.34120305426881,1.29655563422094,
12.5737548217797));
#431041=CARTESIAN_POINT('Ctrl Pts',(-2.32636043968303,1.33762377601409,
12.5893111709658));
#431042=CARTESIAN_POINT('Ctrl Pts',(-2.31935774413811,1.32871193615552,
12.5770542771492));
#431043=CARTESIAN_POINT('Ctrl Pts',(-2.33011456022597,1.31637927291894,
12.5737548217797));
#431044=CARTESIAN_POINT('Ctrl Pts',(-2.31982698564585,1.32930910693714,
12.5928319619712));
#431045=CARTESIAN_POINT('Ctrl Pts',(-2.31768228963815,1.32130700125139,
12.5821634970842));
#431046=CARTESIAN_POINT('Ctrl Pts',(-2.32772715933415,1.31335627203387,
12.5773203894503));
#431047=CARTESIAN_POINT('Ctrl Pts',(-2.31591438608324,1.31302182158929,
12.5969440695591));
#431048=CARTESIAN_POINT('Ctrl Pts',(-2.31786077267748,1.30950470319809,
12.5878292599214));
#431049=CARTESIAN_POINT('Ctrl Pts',(-2.32633461839298,1.3075506732857,12.5813877129824));
#431050=CARTESIAN_POINT('Ctrl Pts',(-2.33080401905962,1.28629217371711,
12.596957478804));
#431051=CARTESIAN_POINT('Ctrl Pts',(-2.32887208691935,1.28978333847323,
12.5878468778671));
#431052=CARTESIAN_POINT('Ctrl Pts',(-2.33166903558704,1.29798666463326,
12.5814011370086));
#431053=CARTESIAN_POINT('Ctrl Pts',(-2.34682121390122,1.28102069607358,
12.5928371701607));
#431054=CARTESIAN_POINT('Ctrl Pts',(-2.3388875204122,1.2833853468567,12.5821692192952));
#431055=CARTESIAN_POINT('Ctrl Pts',(-2.33736544129892,1.29610175740138,
12.5773318885715));
#431056=CARTESIAN_POINT('Ctrl Pts',(-2.35734085275918,1.28223802992773,
12.5893111709658));
#431057=CARTESIAN_POINT('Ctrl Pts',(-2.34608202700252,1.28093515727815,
12.5770542771492));
#431058=CARTESIAN_POINT('Ctrl Pts',(-2.34120305426881,1.29655563422088,
12.5737548217797));
#431059=CARTESIAN_POINT('',(-2.33011456022597,1.31637927291894,12.5737548217797));
#431060=CARTESIAN_POINT('Origin',(-2.34365893801224,1.32403105900996,12.5893111709658));
#431061=CARTESIAN_POINT('Ctrl Pts',(-2.34120305426881,1.29655563422088,
12.5737548217797));
#431062=CARTESIAN_POINT('Ctrl Pts',(-2.34021182714618,1.29640802520225,
12.5746934679442));
#431063=CARTESIAN_POINT('Ctrl Pts',(-2.33908798689128,1.29642587232275,
12.5756680099006));
#431064=CARTESIAN_POINT('Ctrl Pts',(-2.33795934173306,1.29660381550135,
12.5765688348656));
#431065=CARTESIAN_POINT('Ctrl Pts',(-2.33766054542194,1.29665092398799,
12.5768073183026));
#431066=CARTESIAN_POINT('Ctrl Pts',(-2.33736143532197,1.29670899703069,
12.5770407398754));
#431067=CARTESIAN_POINT('Ctrl Pts',(-2.33706429063648,1.29677737962196,
12.5772674179684));
#431068=CARTESIAN_POINT('Ctrl Pts',(-2.33584488919855,1.29705800328511,
12.5781976435658));
#431069=CARTESIAN_POINT('Ctrl Pts',(-2.33459185723495,1.29753917724634,
12.5790594849312));
#431070=CARTESIAN_POINT('Ctrl Pts',(-2.33340711238151,1.29823349155264,
12.5797571720116));
#431071=CARTESIAN_POINT('Ctrl Pts',(-2.33263520850987,1.29868586228851,
12.580211740231));
#431072=CARTESIAN_POINT('Ctrl Pts',(-2.33186670521922,1.29926546531869,
12.5806009430798));
#431073=CARTESIAN_POINT('Ctrl Pts',(-2.33116636977431,1.29994564391944,
12.5808812374708));
#431074=CARTESIAN_POINT('Ctrl Pts',(-2.33056454929326,1.30053014298438,
12.5811221033394));
#431075=CARTESIAN_POINT('Ctrl Pts',(-2.33000082607617,1.30120096031213,
12.581287365893));
#431076=CARTESIAN_POINT('Ctrl Pts',(-2.32951340089355,1.30192559813532,
12.581359338449));
#431077=CARTESIAN_POINT('Ctrl Pts',(-2.32944565885811,1.30202630782955,
12.5813693411482));
#431078=CARTESIAN_POINT('Ctrl Pts',(-2.32937933255776,1.30212804213074,
12.5813775999465));
#431079=CARTESIAN_POINT('Ctrl Pts',(-2.32931446487782,1.30223069954053,
12.5813841266931));
#431080=CARTESIAN_POINT('Ctrl Pts',(-2.32920440901323,1.3024048702524,12.5813952001081));
#431081=CARTESIAN_POINT('Ctrl Pts',(-2.32909832944188,1.30258318991104,
12.5814007534795));
#431082=CARTESIAN_POINT('Ctrl Pts',(-2.32899644185222,1.30276568167775,
12.5814005856065));
#431083=CARTESIAN_POINT('Ctrl Pts',(-2.32853004030221,1.30360105763613,
12.5813998171494));
#431084=CARTESIAN_POINT('Ctrl Pts',(-2.32818340973398,1.30446597546451,
12.58127954464));
#431085=CARTESIAN_POINT('Ctrl Pts',(-2.3279310523309,1.30534451735209,12.5810700125799));
#431086=CARTESIAN_POINT('Ctrl Pts',(-2.32762623332117,1.30640569592229,
12.5808169217085));
#431087=CARTESIAN_POINT('Ctrl Pts',(-2.32747501580929,1.30749146828497,
12.5804173076348));
#431088=CARTESIAN_POINT('Ctrl Pts',(-2.32746485883118,1.30850308689069,
12.5799304713245));
#431089=CARTESIAN_POINT('Ctrl Pts',(-2.32745227113552,1.30975680103591,
12.5793271277669));
#431090=CARTESIAN_POINT('Ctrl Pts',(-2.32762335901736,1.3109740691843,12.5785808224116));
#431091=CARTESIAN_POINT('Ctrl Pts',(-2.32793950264364,1.31210799557987,
12.5777485681082));
#431092=CARTESIAN_POINT('Ctrl Pts',(-2.32841059128292,1.31379767014018,
12.576508418016));
#431093=CARTESIAN_POINT('Ctrl Pts',(-2.32919317907541,1.31528990867935,
12.5750928681475));
#431094=CARTESIAN_POINT('Ctrl Pts',(-2.33011456022597,1.31637927291894,
12.5737548217797));
#431095=CARTESIAN_POINT('Ctrl Pts',(-2.33011456022597,1.31637927291894,
12.5737548217797));
#431096=CARTESIAN_POINT('Ctrl Pts',(-2.31935774413811,1.32871193615552,
12.5770542771492));
#431097=CARTESIAN_POINT('Ctrl Pts',(-2.32636043968303,1.3376237760141,12.5893111709658));
#431098=CARTESIAN_POINT('Ctrl Pts',(-2.34545162098595,1.33581608133531,
12.5508408821982));
#431099=CARTESIAN_POINT('Ctrl Pts',(-2.33465905500726,1.3481848421554,12.55409748406));
#431100=CARTESIAN_POINT('Ctrl Pts',(-2.3416706841982,1.35710805123919,12.5663972313419));
#431101=CARTESIAN_POINT('Ctrl Pts',(-2.36077277340999,1.35523463308848,
12.52790050457));
#431102=CARTESIAN_POINT('Ctrl Pts',(-2.34993106022407,1.36762045290534,
12.5311362602938));
#431103=CARTESIAN_POINT('Ctrl Pts',(-2.35696548319246,1.37657267003228,
12.5434568539655));
#431104=CARTESIAN_POINT('Ctrl Pts',(-2.37607924290869,1.37463635553372,
12.5049357605811));
#431105=CARTESIAN_POINT('Ctrl Pts',(-2.36517681475302,1.38702265624458,
12.5081700652078));
#431106=CARTESIAN_POINT('Ctrl Pts',(-2.37224604636214,1.39601917188909,
12.5204921097672));
#431107=CARTESIAN_POINT('Ctrl Pts',(-2.37507415887584,1.37336236336858,
12.5064436508395));
#431108=CARTESIAN_POINT('Ctrl Pts',(-2.37465187301338,1.37450714388944,
12.5062361689309));
#431109=CARTESIAN_POINT('Ctrl Pts',(-2.374163914289,1.37567961474355,12.5061871075061));
#431110=CARTESIAN_POINT('Ctrl Pts',(-2.37362856535138,1.37678614904312,
12.5063648335164));
#431111=CARTESIAN_POINT('Ctrl Pts',(-2.37338537684222,1.37728880517584,
12.5064455676329));
#431112=CARTESIAN_POINT('Ctrl Pts',(-2.37312881889141,1.37778477011569,
12.506574497099));
#431113=CARTESIAN_POINT('Ctrl Pts',(-2.37286895848143,1.37825229550728,
12.5067492519495));
#431114=CARTESIAN_POINT('Ctrl Pts',(-2.37234675890051,1.37919180592974,
12.5071004286051));
#431115=CARTESIAN_POINT('Ctrl Pts',(-2.37179131735987,1.3800506202677,12.5076537929613));
#431116=CARTESIAN_POINT('Ctrl Pts',(-2.37125226479469,1.38076941660765,
12.5083435010505));
#431117=CARTESIAN_POINT('Ctrl Pts',(-2.37121832821432,1.3808146691328,12.5083869222964));
#431118=CARTESIAN_POINT('Ctrl Pts',(-2.37118444334185,1.38085936447729,
12.5084308732337));
#431119=CARTESIAN_POINT('Ctrl Pts',(-2.3711506171009,1.38090348732261,12.5084753333615));
#431120=CARTESIAN_POINT('Ctrl Pts',(-2.37087928600183,1.38125741077894,
12.5088319622689));
#431121=CARTESIAN_POINT('Ctrl Pts',(-2.3706072427105,1.38158246887616,12.509227847131));
#431122=CARTESIAN_POINT('Ctrl Pts',(-2.37034472377393,1.38187079301739,
12.5096423454524));
#431123=CARTESIAN_POINT('Ctrl Pts',(-2.36952210561275,1.38277427326909,
12.5109411997424));
#431124=CARTESIAN_POINT('Ctrl Pts',(-2.36874956172666,1.3833791352647,12.5124831113042));
#431125=CARTESIAN_POINT('Ctrl Pts',(-2.36805057734202,1.38377705398192,
12.5140723025008));
#431126=CARTESIAN_POINT('Ctrl Pts',(-2.36798508173961,1.38381433940156,
12.5142212114565));
#431127=CARTESIAN_POINT('Ctrl Pts',(-2.36792022877725,1.38384983731474,
12.5143705582413));
#431128=CARTESIAN_POINT('Ctrl Pts',(-2.36785603748264,1.38388364012108,
12.5145201959299));
#431129=CARTESIAN_POINT('Ctrl Pts',(-2.36703140473243,1.3843178874957,12.5164425148273));
#431130=CARTESIAN_POINT('Ctrl Pts',(-2.36629271696646,1.38449676780137,
12.5184635205941));
#431131=CARTESIAN_POINT('Ctrl Pts',(-2.36561364789958,1.38450656490253,
12.5205025929158));
#431132=CARTESIAN_POINT('Ctrl Pts',(-2.365219760925,1.38451224760952,12.5216853356836));
#431133=CARTESIAN_POINT('Ctrl Pts',(-2.36484665091736,1.38446151619183,
12.5228750347131));
#431134=CARTESIAN_POINT('Ctrl Pts',(-2.3644949366336,1.38437260662455,12.5240609649613));
#431135=CARTESIAN_POINT('Ctrl Pts',(-2.36363167279295,1.3841543828615,12.5269717671326));
#431136=CARTESIAN_POINT('Ctrl Pts',(-2.36287555540805,1.38368994181205,
12.5299036066169));
#431137=CARTESIAN_POINT('Ctrl Pts',(-2.36219369101421,1.3830594554327,12.5328133004019));
#431138=CARTESIAN_POINT('Ctrl Pts',(-2.36186635640138,1.38275678525848,
12.5342101228451));
#431139=CARTESIAN_POINT('Ctrl Pts',(-2.3615568980478,1.38241584181146,12.5356023438238));
#431140=CARTESIAN_POINT('Ctrl Pts',(-2.36126526429652,1.38204470010705,
12.5369868989719));
#431141=CARTESIAN_POINT('Origin',(-10.2316378295468,11.4066885757328,-1.23974187479773));
#431142=CARTESIAN_POINT('Ctrl Pts',(-2.41341877811849,1.28872733412586,
12.5369868989719));
#431143=CARTESIAN_POINT('Ctrl Pts',(-2.42865266524063,1.29051953579836,
12.5369868989719));
#431144=CARTESIAN_POINT('Ctrl Pts',(-2.43560194861504,1.27684507916319,
12.5369868989719));
#431145=CARTESIAN_POINT('Ctrl Pts',(-2.41856843549576,1.28933310262533,
12.5218025310015));
#431146=CARTESIAN_POINT('Ctrl Pts',(-2.43022092785154,1.28736452811494,
12.5216901060417));
#431147=CARTESIAN_POINT('Ctrl Pts',(-2.43558077959844,1.27688677091039,
12.5161920673678));
#431148=CARTESIAN_POINT('Ctrl Pts',(-2.42148857846681,1.29460651103199,
12.5042015548895));
#431149=CARTESIAN_POINT('Ctrl Pts',(-2.42752167704109,1.2923751288124,12.4980677368514));
#431150=CARTESIAN_POINT('Ctrl Pts',(-2.43071015502069,1.2863730968317,12.4907278922777));
#431151=CARTESIAN_POINT('Ctrl Pts',(-2.4132715527434,1.3050333735978,12.506463626192));
#431152=CARTESIAN_POINT('Ctrl Pts',(-2.41902668217186,1.30814559524769,
12.4999376786891));
#431153=CARTESIAN_POINT('Ctrl Pts',(-2.41895639163384,1.30810758398541,
12.4906970594712));
#431154=CARTESIAN_POINT('Origin',(-2.4159892567878,1.26687801744522,12.5369868989719));
#431155=CARTESIAN_POINT('Origin',(-2.4159892567878,1.26687801744522,14.));
#431156=CARTESIAN_POINT('Origin',(-2.4159892567878,1.26687801744522,13.7435492065112));
#431157=CARTESIAN_POINT('Ctrl Pts',(-2.38886432632103,1.28588590268799,
13.793642941384));
#431158=CARTESIAN_POINT('Ctrl Pts',(-2.3996018053748,1.28715584858276,13.8071662555867));
#431159=CARTESIAN_POINT('Ctrl Pts',(-2.40406680098607,1.27072164042337,
13.8103758687955));
#431160=CARTESIAN_POINT('Ctrl Pts',(-2.40537526568099,1.287796553539,13.7804579775006));
#431161=CARTESIAN_POINT('Ctrl Pts',(-2.41862553539282,1.28935348137683,
13.7901904343351));
#431162=CARTESIAN_POINT('Ctrl Pts',(-2.42516220096345,1.27501723614377,
13.7927914348262));
#431163=CARTESIAN_POINT('Ctrl Pts',(-2.41509587706315,1.28892142556309,
13.7597120340895));
#431164=CARTESIAN_POINT('Ctrl Pts',(-2.43043083937317,1.29071753828875,
13.7635825532445));
#431165=CARTESIAN_POINT('Ctrl Pts',(-2.43760723472565,1.27752529564813,
13.7651073818884));
#431166=CARTESIAN_POINT('Ctrl Pts',(-2.41319235877791,1.28870114986332,
13.7381884353898));
#431167=CARTESIAN_POINT('Ctrl Pts',(-2.42816827316289,1.29045611395404,
13.7368803041982));
#431168=CARTESIAN_POINT('Ctrl Pts',(-2.43517022495231,1.27703365858039,
13.7363986145813));
#431169=CARTESIAN_POINT('Origin',(-2.39539963927866,1.26449538446929,13.7902182540695));
#431170=CARTESIAN_POINT('Ctrl Pts',(-2.35733694274133,1.28223757669607,
13.8235227101244));
#431171=CARTESIAN_POINT('Ctrl Pts',(-2.36875729040384,1.28356360368931,
13.8358800583119));
#431172=CARTESIAN_POINT('Ctrl Pts',(-2.37359169323221,1.26771259115543,
13.8390832900376));
#431173=CARTESIAN_POINT('Ctrl Pts',(-2.36918545335587,1.28360868774612,
13.8124254819053));
#431174=CARTESIAN_POINT('Ctrl Pts',(-2.38062797920374,1.28493728958868,
13.8247886449157));
#431175=CARTESIAN_POINT('Ctrl Pts',(-2.38545218759861,1.26906127640952,
13.8279860620657));
#431176=CARTESIAN_POINT('Ctrl Pts',(-2.38102865385343,1.28497918430881,
13.8013225099955));
#431177=CARTESIAN_POINT('Ctrl Pts',(-2.39248795862072,1.28630973610524,
13.8136962257787));
#431178=CARTESIAN_POINT('Ctrl Pts',(-2.39730716051433,1.27040960660921,
13.8168830918626));
#431179=CARTESIAN_POINT('Ctrl Pts',(-2.39286675084249,1.28634909029291,
13.7902140179785));
#431180=CARTESIAN_POINT('Ctrl Pts',(-2.4043377881453,1.28768100798631,13.802602731458));
#431181=CARTESIAN_POINT('Ctrl Pts',(-2.40915682872264,1.27175759753393,
13.8057746032558));
#431182=CARTESIAN_POINT('Origin',(-2.3598698187987,1.26038386943668,13.8235269408515));
#431183=CARTESIAN_POINT('Ctrl Pts',(-2.32636043968303,1.3376237760141,13.8235269408515));
#431184=CARTESIAN_POINT('Ctrl Pts',(-2.33365570123877,1.34690794413108,
13.8362179249168));
#431185=CARTESIAN_POINT('Ctrl Pts',(-2.32211071702631,1.35949271046151,
13.8391868794938));
#431186=CARTESIAN_POINT('Ctrl Pts',(-2.31968559290336,1.32912916630282,
13.8400110824519));
#431187=CARTESIAN_POINT('Ctrl Pts',(-2.32284469250289,1.33868646469628,
13.8494522556836));
#431188=CARTESIAN_POINT('Ctrl Pts',(-2.31121414932101,1.34544356116811,
13.85569149686));
#431189=CARTESIAN_POINT('Ctrl Pts',(-2.31574597041812,1.31332166489626,
13.8586819406588));
#431190=CARTESIAN_POINT('Ctrl Pts',(-2.31363267167181,1.31712823974037,
13.868010383617));
#431191=CARTESIAN_POINT('Ctrl Pts',(-2.30481596404009,1.3191674879669,13.8744918421245));
#431192=CARTESIAN_POINT('Ctrl Pts',(-2.33097503050985,1.28598767092046,
13.8587686893867));
#431193=CARTESIAN_POINT('Ctrl Pts',(-2.33306947168661,1.2822149472257,13.8680909899357));
#431194=CARTESIAN_POINT('Ctrl Pts',(-2.33017012447703,1.27366566729906,
13.8745789365163));
#431195=CARTESIAN_POINT('Ctrl Pts',(-2.34659167413014,1.28099413369755,
13.8400379222776));
#431196=CARTESIAN_POINT('Ctrl Pts',(-2.35638474272802,1.2786776619526,13.8494748685453));
#431197=CARTESIAN_POINT('Ctrl Pts',(-2.35605673380427,1.26523692107231,
13.8557104837033));
#431198=CARTESIAN_POINT('Ctrl Pts',(-2.35734085275979,1.28223802992121,
13.8235269408542));
#431199=CARTESIAN_POINT('Ctrl Pts',(-2.36907006163061,1.2835953353604,13.8362179249195));
#431200=CARTESIAN_POINT('Ctrl Pts',(-2.37375135115599,1.26717131233205,
13.8391868794965));
#431201=CARTESIAN_POINT('Origin',(-2.30906194135383,1.35121649301823,13.8235269408515));
#431202=CARTESIAN_POINT('Ctrl Pts',(-2.34845662328262,1.36574404157119,
13.7902140241682));
#431203=CARTESIAN_POINT('Ctrl Pts',(-2.35559512507335,1.37482150749381,
13.8026027327198));
#431204=CARTESIAN_POINT('Ctrl Pts',(-2.34454881511321,1.38726164288447,
13.8057746032556));
#431205=CARTESIAN_POINT('Ctrl Pts',(-2.34109363615993,1.35637368386972,
13.8013225161808));
#431206=CARTESIAN_POINT('Ctrl Pts',(-2.34822483363906,1.36544186728202,
13.8136962270464));
#431207=CARTESIAN_POINT('Ctrl Pts',(-2.33719844595753,1.37786995563101,
13.8168830918628));
#431208=CARTESIAN_POINT('Ctrl Pts',(-2.33372747478725,1.34699928652274,
13.8124254880875));
#431209=CARTESIAN_POINT('Ctrl Pts',(-2.34084822916302,1.35605419304686,
13.8247886461867));
#431210=CARTESIAN_POINT('Ctrl Pts',(-2.32984501138987,1.36847392576679,
13.8279860620656));
#431211=CARTESIAN_POINT('Ctrl Pts',(-2.32635801065852,1.33762068598958,
13.8235227163065));
#431212=CARTESIAN_POINT('Ctrl Pts',(-2.33346496365344,1.3466580419284,13.8358800595848));
#431213=CARTESIAN_POINT('Ctrl Pts',(-2.32248838452712,1.35907337686072,
13.8390832900376));
#431214=CARTESIAN_POINT('Origin',(-2.33116056166863,1.37933985838199,13.7902182540695));
#431215=CARTESIAN_POINT('Ctrl Pts',(-2.36109850945796,1.38183252755633,
13.7382347919292));
#431216=CARTESIAN_POINT('Ctrl Pts',(-2.37044093715816,1.39368313570106,
13.7369371795942));
#431217=CARTESIAN_POINT('Ctrl Pts',(-2.36265505647251,1.40668020610054,
13.7364597369711));
#431218=CARTESIAN_POINT('Ctrl Pts',(-2.36226721072488,1.38331985110314,
13.7595490285574));
#431219=CARTESIAN_POINT('Ctrl Pts',(-2.37183175116987,1.39545382705888,
13.7633824266926));
#431220=CARTESIAN_POINT('Ctrl Pts',(-2.36432895367105,1.4084769484205,13.7648920890506));
#431221=CARTESIAN_POINT('Ctrl Pts',(-2.35630689829647,1.37573458249166,
13.780380659011));
#431222=CARTESIAN_POINT('Ctrl Pts',(-2.36458412313523,1.38622669548064,
13.7901039518744));
#431223=CARTESIAN_POINT('Ctrl Pts',(-2.35579795950558,1.39931442905445,
13.7926933640892));
#431224=CARTESIAN_POINT('Ctrl Pts',(-2.34594654472624,1.36254969244765,
13.7936647693663));
#431225=CARTESIAN_POINT('Ctrl Pts',(-2.35265240347727,1.37103525609161,
13.8072068914933));
#431226=CARTESIAN_POINT('Ctrl Pts',(-2.34096528964321,1.38344717133773,
13.8104111085397));
#431227=CARTESIAN_POINT('Origin',(-2.34396676596731,1.39563741711118,13.7435492065112));
#431228=CARTESIAN_POINT('Origin',(-2.34396676596731,1.39563741711118,14.));
#431229=CARTESIAN_POINT('Origin',(-2.34396676596731,1.39563741711118,12.5369868989719));
#431230=CARTESIAN_POINT('Ctrl Pts',(-2.37505824466421,1.37335316112641,
12.506462012331));
#431231=CARTESIAN_POINT('Ctrl Pts',(-2.38071867661695,1.37662624806359,
12.4999388158272));
#431232=CARTESIAN_POINT('Ctrl Pts',(-2.38065170628375,1.37658752315273,
12.4907030323752));
#431233=CARTESIAN_POINT('Ctrl Pts',(-2.37047222175398,1.38581096900024,
12.5042014951932));
#431234=CARTESIAN_POINT('Ctrl Pts',(-2.37172876299148,1.39211669665329,
12.4980716682127));
#431235=CARTESIAN_POINT('Ctrl Pts',(-2.36828692406589,1.39797155019853,
12.4907355092744));
#431236=CARTESIAN_POINT('Ctrl Pts',(-2.3644513710313,1.38608493582388,12.5218047446509));
#431237=CARTESIAN_POINT('Ctrl Pts',(-2.36886926496384,1.39703943645774,
12.5216906929434));
#431238=CARTESIAN_POINT('Ctrl Pts',(-2.36275256495378,1.40708715934986,
12.5161988840775));
#431239=CARTESIAN_POINT('Ctrl Pts',(-2.36124150249871,1.38201451441863,
12.5369868989719));
#431240=CARTESIAN_POINT('Ctrl Pts',(-2.37073412075248,1.39405177865136,
12.5369868989719));
#431241=CARTESIAN_POINT('Ctrl Pts',(-2.36272902539233,1.40712556845369,
12.5369868989719));
#431242=CARTESIAN_POINT('Origin',(-4.49626278878395E-31,-2.63684586248252E-31,
12.5));
#431243=CARTESIAN_POINT('Origin',(-2.42764842286964,1.14355297053481,12.5));
#431244=CARTESIAN_POINT('',(-2.42764842286964,1.14355297053481,12.5893111709658));
#431245=CARTESIAN_POINT('',(-2.42764842286964,1.14355297053481,13.8235269408515));
#431246=CARTESIAN_POINT('',(-2.42764842286964,1.14355297053481,12.5));
#431247=CARTESIAN_POINT('',(-2.45196582721009,1.1697815150111,13.7902182540695));
#431248=CARTESIAN_POINT('',(-2.42764842286964,1.14355297053481,13.8235269408515));
#431249=CARTESIAN_POINT('',(-2.46605782225598,1.18498102042073,13.7435492065112));
#431250=CARTESIAN_POINT('Origin',(-2.41969558370818,1.13497462705725,13.7445212918713));
#431251=CARTESIAN_POINT('',(-2.46605782225598,1.18498102042073,12.5369868989719));
#431252=CARTESIAN_POINT('',(-2.46605782225598,1.18498102042073,12.5));
#431253=CARTESIAN_POINT('Ctrl Pts',(-2.46605782225598,1.18498102042073,
12.5369868989719));
#431254=CARTESIAN_POINT('Ctrl Pts',(-2.4532640269538,1.17118174215871,12.5544431401645));
#431255=CARTESIAN_POINT('Ctrl Pts',(-2.44046108118918,1.15737259428612,
12.5718848856037));
#431256=CARTESIAN_POINT('Ctrl Pts',(-2.42764842286964,1.14355297053481,
12.5893111709658));
#431257=CARTESIAN_POINT('Origin',(-2.72885600850611,1.09506675154452,12.5));
#431258=CARTESIAN_POINT('',(-2.51047333723491,1.08772460875899,13.7435492065112));
#431259=CARTESIAN_POINT('',(-2.48975802327268,1.08702814876941,13.7902182540695));
#431260=CARTESIAN_POINT('Origin',(-2.4353217585087,1.08519797228937,13.7418732680457));
#431261=CARTESIAN_POINT('',(-2.45401129869476,1.08582632467577,13.8235269408515));
#431262=CARTESIAN_POINT('',(-2.48975802327268,1.08702814876941,13.7902182540695));
#431263=CARTESIAN_POINT('',(-2.45401129869476,1.08582632467577,12.5893111709658));
#431264=CARTESIAN_POINT('',(-2.45401129869476,1.08582632467577,12.5));
#431265=CARTESIAN_POINT('',(-2.51047333723491,1.08772460875899,12.5369868989719));
#431266=CARTESIAN_POINT('Ctrl Pts',(-2.45401129869476,1.08582632467577,
12.5893111709658));
#431267=CARTESIAN_POINT('Ctrl Pts',(-2.47284598029348,1.08645955679448,
12.5718848856037));
#431268=CARTESIAN_POINT('Ctrl Pts',(-2.49166638438046,1.08709230889557,
12.5544431401645));
#431269=CARTESIAN_POINT('Ctrl Pts',(-2.51047333723491,1.08772460875899,
12.5369868989719));
#431270=CARTESIAN_POINT('',(-2.51047333723491,1.08772460875899,12.5));
#431271=CARTESIAN_POINT('Origin',(-2.45285624533617,1.12018191340219,12.5));
#431272=CARTESIAN_POINT('',(-2.42113982516251,1.10692827754081,13.8587068136939));
#431273=CARTESIAN_POINT('Ctrl Pts',(-2.45401129869484,1.08582632466916,
13.8235269408542));
#431274=CARTESIAN_POINT('Ctrl Pts',(-2.45225998987588,1.08576744472537,
13.8262006681044));
#431275=CARTESIAN_POINT('Ctrl Pts',(-2.45046194326886,1.08588083092831,
13.8288634856214));
#431276=CARTESIAN_POINT('Ctrl Pts',(-2.44862203900277,1.08615407399156,
13.8314912288862));
#431277=CARTESIAN_POINT('Ctrl Pts',(-2.44672528748175,1.08643575940605,
13.8342001611531));
#431278=CARTESIAN_POINT('Ctrl Pts',(-2.44478187198945,1.08688715382095,
13.8368750301949));
#431279=CARTESIAN_POINT('Ctrl Pts',(-2.44278365182638,1.08753780372501,
13.8394886372968));
#431280=CARTESIAN_POINT('Ctrl Pts',(-2.44262932443618,1.08758805499536,
13.8396904925131));
#431281=CARTESIAN_POINT('Ctrl Pts',(-2.4424746732709,1.08763951672092,13.8398919674349));
#431282=CARTESIAN_POINT('Ctrl Pts',(-2.44231969718439,1.08769221365696,
13.8400930404591));
#431283=CARTESIAN_POINT('Ctrl Pts',(-2.43990506549373,1.0885132673732,13.8432258934518));
#431284=CARTESIAN_POINT('Ctrl Pts',(-2.43742351542761,1.08962892240605,
13.8462331177034));
#431285=CARTESIAN_POINT('Ctrl Pts',(-2.43499553741713,1.09109077560807,
13.8489036603661));
#431286=CARTESIAN_POINT('Ctrl Pts',(-2.43420107475631,1.09156911098822,
13.8497774930041));
#431287=CARTESIAN_POINT('Ctrl Pts',(-2.43341259768076,1.09208452235582,
13.85061494757));
#431288=CARTESIAN_POINT('Ctrl Pts',(-2.43263504113365,1.09263883232474,
13.8514076489583));
#431289=CARTESIAN_POINT('Ctrl Pts',(-2.4309903968961,1.09381127785246,13.8530843267192));
#431290=CARTESIAN_POINT('Ctrl Pts',(-2.42923477898703,1.09527532288743,
13.8546805203176));
#431291=CARTESIAN_POINT('Ctrl Pts',(-2.42755746953222,1.09705078503298,
13.8559412814273));
#431292=CARTESIAN_POINT('Ctrl Pts',(-2.42733299113072,1.09728839944766,
13.8561100121513));
#431293=CARTESIAN_POINT('Ctrl Pts',(-2.42710990696846,1.09753151532451,
13.8562727473908));
#431294=CARTESIAN_POINT('Ctrl Pts',(-2.42688865315478,1.09778010639366,
13.8564289040185));
#431295=CARTESIAN_POINT('Ctrl Pts',(-2.42588526963393,1.09890746405619,
13.8571370725437));
#431296=CARTESIAN_POINT('Ctrl Pts',(-2.42490359306482,1.10016875444836,
13.8577210840554));
#431297=CARTESIAN_POINT('Ctrl Pts',(-2.42400494134343,1.10153297664135,
13.8581177131616));
#431298=CARTESIAN_POINT('Ctrl Pts',(-2.42375185008804,1.101917188566,13.8582294175695));
#431299=CARTESIAN_POINT('Ctrl Pts',(-2.42350521788678,1.10230943995882,
13.8583265086086));
#431300=CARTESIAN_POINT('Ctrl Pts',(-2.42326608400721,1.10270874845725,
13.8584082369006));
#431301=CARTESIAN_POINT('Ctrl Pts',(-2.42292251274854,1.10328244769071,
13.8585256585398));
#431302=CARTESIAN_POINT('Ctrl Pts',(-2.42259042551756,1.10387801275165,
13.8586122832068));
#431303=CARTESIAN_POINT('Ctrl Pts',(-2.42227913868915,1.10448035716898,
13.8586682984299));
#431304=CARTESIAN_POINT('Ctrl Pts',(-2.4220301400833,1.10496217299436,13.8587131050557));
#431305=CARTESIAN_POINT('Ctrl Pts',(-2.42179149193538,1.10545354053934,
13.8587357943552));
#431306=CARTESIAN_POINT('Ctrl Pts',(-2.4215636214456,1.10595473944802,13.8587355499465));
#431307=CARTESIAN_POINT('Ctrl Pts',(-2.42141634331542,1.10627867625174,
13.8587353919793));
#431308=CARTESIAN_POINT('Ctrl Pts',(-2.42127512482626,1.10660320094039,
13.8587257282814));
#431309=CARTESIAN_POINT('Ctrl Pts',(-2.42113982516251,1.10692827754081,
13.8587068136939));
#431310=CARTESIAN_POINT('Ctrl Pts',(-2.42113982516251,1.10692827754081,
13.8587068136939));
#431311=CARTESIAN_POINT('Ctrl Pts',(-2.42069483194421,1.10799743675823,
13.8586446046466));
#431312=CARTESIAN_POINT('Ctrl Pts',(-2.42031378439166,1.10907255944393,
13.858482427929));
#431313=CARTESIAN_POINT('Ctrl Pts',(-2.41999237636932,1.11015244428447,
13.8582284286032));
#431314=CARTESIAN_POINT('Ctrl Pts',(-2.41966264912614,1.1112602805134,13.8579678548414));
#431315=CARTESIAN_POINT('Ctrl Pts',(-2.41939635132405,1.11237627168034,
13.857615680862));
#431316=CARTESIAN_POINT('Ctrl Pts',(-2.41919455650097,1.1134541716557,13.8571944833187));
#431317=CARTESIAN_POINT('Ctrl Pts',(-2.41869095688211,1.1161441812828,13.8561433417727));
#431318=CARTESIAN_POINT('Ctrl Pts',(-2.41856081345834,1.11872190560802,
13.8546163505474));
#431319=CARTESIAN_POINT('Ctrl Pts',(-2.41865531013259,1.12104377710058,
13.8528973491086));
#431320=CARTESIAN_POINT('Ctrl Pts',(-2.41867257328081,1.12146794876624,
13.8525833129072));
#431321=CARTESIAN_POINT('Ctrl Pts',(-2.4186972109593,1.12188365195227,13.8522628768812));
#431322=CARTESIAN_POINT('Ctrl Pts',(-2.41872817655191,1.12229012345833,
13.851937733538));
#431323=CARTESIAN_POINT('Ctrl Pts',(-2.4189172791297,1.12477238855045,13.8499521282529));
#431324=CARTESIAN_POINT('Ctrl Pts',(-2.41936523309139,1.12715675030091,
13.847639871647));
#431325=CARTESIAN_POINT('Ctrl Pts',(-2.41996953631742,1.1293327296868,13.8452109780794));
#431326=CARTESIAN_POINT('Ctrl Pts',(-2.42024142484727,1.13031174785304,
13.8441181685877));
#431327=CARTESIAN_POINT('Ctrl Pts',(-2.42054438044999,1.13124900285884,
13.8430021611332));
#431328=CARTESIAN_POINT('Ctrl Pts',(-2.42086711254577,1.13213710203047,
13.8418824960098));
#431329=CARTESIAN_POINT('Ctrl Pts',(-2.42162763897073,1.13422993040682,
13.8392439765549));
#431330=CARTESIAN_POINT('Ctrl Pts',(-2.42253079002036,1.13615112387534,
13.8364981347964));
#431331=CARTESIAN_POINT('Ctrl Pts',(-2.42354798497218,1.13792032184698,
13.8336931113419));
#431332=CARTESIAN_POINT('Ctrl Pts',(-2.4245386682574,1.1396434083169,13.8309611966328));
#431333=CARTESIAN_POINT('Ctrl Pts',(-2.4256390102089,1.1412237644561,13.8281701127186));
#431334=CARTESIAN_POINT('Ctrl Pts',(-2.42684721607875,1.14264889243483,
13.8253580685121));
#431335=CARTESIAN_POINT('Ctrl Pts',(-2.42710915641527,1.14295786171868,
13.8247484142933));
#431336=CARTESIAN_POINT('Ctrl Pts',(-2.42737621387803,1.14325936824308,
13.8241378483365));
#431337=CARTESIAN_POINT('Ctrl Pts',(-2.42764842286964,1.14355297053481,
13.8235269408515));
#431338=CARTESIAN_POINT('',(-2.4216393225781,1.10579105320548,12.5969504640361));
#431339=CARTESIAN_POINT('Origin',(-2.45288625954449,1.12019583569037,12.584524458991));
#431340=CARTESIAN_POINT('Origin',(-2.45288625954449,1.12019583569037,12.584524458991));
#431341=CARTESIAN_POINT('Ctrl Pts',(-2.45401129869476,1.08582632467577,
12.5893111709658));
#431342=CARTESIAN_POINT('Ctrl Pts',(-2.44268373953581,1.08544548604845,
12.5770542771492));
#431343=CARTESIAN_POINT('Ctrl Pts',(-2.43909421506564,1.10141166871473,
12.5737548217797));
#431344=CARTESIAN_POINT('Ctrl Pts',(-2.47878086893348,1.08665909094047,
12.5663937883685));
#431345=CARTESIAN_POINT('Ctrl Pts',(-2.46743885989968,1.08627776650061,
12.5540940315303));
#431346=CARTESIAN_POINT('Ctrl Pts',(-2.46384134520686,1.10229412948815,
12.5508374392248));
#431347=CARTESIAN_POINT('Ctrl Pts',(-2.50352544697966,1.08749101695422,
12.5434499600945));
#431348=CARTESIAN_POINT('Ctrl Pts',(-2.49214656103544,1.0871084526928,12.5311293540533));
#431349=CARTESIAN_POINT('Ctrl Pts',(-2.48856433892152,1.10317454896066,
12.5278936106989));
#431350=CARTESIAN_POINT('Ctrl Pts',(-2.52824699050566,1.08832216853502,
12.5204817579905));
#431351=CARTESIAN_POINT('Ctrl Pts',(-2.51681178685245,1.08793771084195,
12.5081597038247));
#431352=CARTESIAN_POINT('Ctrl Pts',(-2.51326507268073,1.10405307194491,
12.5049254088044));
#431353=CARTESIAN_POINT('Ctrl Pts',(-2.51047333723491,1.08772460875899,
12.5369868989719));
#431354=CARTESIAN_POINT('Ctrl Pts',(-2.5114043160049,1.08775590892762,12.5342545179733));
#431355=CARTESIAN_POINT('Ctrl Pts',(-2.5122886079891,1.08791045600796,12.5314872231885));
#431356=CARTESIAN_POINT('Ctrl Pts',(-2.51306677574641,1.08823461037182,
12.5287124745063));
#431357=CARTESIAN_POINT('Ctrl Pts',(-2.51376856605476,1.08852694886673,
12.5262100684184));
#431358=CARTESIAN_POINT('Ctrl Pts',(-2.51438295571426,1.0889578475602,12.5237004536639));
#431359=CARTESIAN_POINT('Ctrl Pts',(-2.51488243000409,1.08958897829564,
12.5212220730815));
#431360=CARTESIAN_POINT('Ctrl Pts',(-2.51526482078093,1.09007216347079,
12.5193246583486));
#431361=CARTESIAN_POINT('Ctrl Pts',(-2.51558392955601,1.09067887774684,
12.517417831369));
#431362=CARTESIAN_POINT('Ctrl Pts',(-2.51576432415528,1.09147047265085,
12.5155812248347));
#431363=CARTESIAN_POINT('Ctrl Pts',(-2.5158411732242,1.0918076963348,12.5147988205793));
#431364=CARTESIAN_POINT('Ctrl Pts',(-2.51589319647567,1.09217875303941,
12.5140295443047));
#431365=CARTESIAN_POINT('Ctrl Pts',(-2.51591654171449,1.0925891647262,12.5132817086137));
#431366=CARTESIAN_POINT('Ctrl Pts',(-2.51595187157537,1.09321026729493,
12.5121499604604));
#431367=CARTESIAN_POINT('Ctrl Pts',(-2.51591514373557,1.0939353219013,12.511049420657));
#431368=CARTESIAN_POINT('Ctrl Pts',(-2.51577053661718,1.09477451252028,
12.5100666561697));
#431369=CARTESIAN_POINT('Ctrl Pts',(-2.5156875035428,1.09525637384121,12.5095023550643));
#431370=CARTESIAN_POINT('Ctrl Pts',(-2.51556729971076,1.09578132276691,
12.5089719619137));
#431371=CARTESIAN_POINT('Ctrl Pts',(-2.5154059523648,1.09633809410319,12.5085043804652));
#431372=CARTESIAN_POINT('Ctrl Pts',(-2.51516984154096,1.09715285642926,
12.5078201359221));
#431373=CARTESIAN_POINT('Ctrl Pts',(-2.51483761582447,1.09805905954442,
12.5072563000949));
#431374=CARTESIAN_POINT('Ctrl Pts',(-2.51442384655357,1.09899236216246,
12.5068768744332));
#431375=CARTESIAN_POINT('Ctrl Pts',(-2.51412549042528,1.09966533759884,
12.5066032824114));
#431376=CARTESIAN_POINT('Ctrl Pts',(-2.51377954975441,1.10036425066418,
12.5064197834844));
#431377=CARTESIAN_POINT('Ctrl Pts',(-2.51340765937553,1.10105121889007,
12.5063282718343));
#431378=CARTESIAN_POINT('Ctrl Pts',(-2.51286481455672,1.10205397981988,
12.5061946931565));
#431379=CARTESIAN_POINT('Ctrl Pts',(-2.51225601023427,1.10305322842605,
12.5062515701262));
#431380=CARTESIAN_POINT('Ctrl Pts',(-2.51163223633243,1.10399499577423,
12.5064436508398));
#431381=CARTESIAN_POINT('',(-2.43909421506564,1.10141166871474,12.5737548217797));
#431382=CARTESIAN_POINT('Origin',(-2.45327206454526,1.10781390146068,12.5893111709658));
#431383=CARTESIAN_POINT('Ctrl Pts',(-2.51163223633243,1.10399499577423,
12.5064436508398));
#431384=CARTESIAN_POINT('Ctrl Pts',(-2.50089470750429,1.10361307639003,
12.5164271754438));
#431385=CARTESIAN_POINT('Ctrl Pts',(-2.49015292974903,1.10323079680946,
12.5264061185523));
#431386=CARTESIAN_POINT('Ctrl Pts',(-2.47940675338938,1.1028481452926,12.536380305637));
#431387=CARTESIAN_POINT('Ctrl Pts',(-2.46597621249922,1.10236990850661,
12.5488460165097));
#431388=CARTESIAN_POINT('Ctrl Pts',(-2.45253879705324,1.10189109059316,
12.5613043021964));
#431389=CARTESIAN_POINT('Ctrl Pts',(-2.43909421506564,1.10141166871473,
12.5737548217797));
#431390=CARTESIAN_POINT('Ctrl Pts',(-2.42764842286964,1.14355297053481,
12.5893111709658));
#431391=CARTESIAN_POINT('Ctrl Pts',(-2.41994263053451,1.13524156878495,
12.5770542771492));
#431392=CARTESIAN_POINT('Ctrl Pts',(-2.42965842765956,1.12207316109535,
12.5737548217797));
#431393=CARTESIAN_POINT('Ctrl Pts',(-2.4204589856424,1.13579850499095,12.5928319619712));
#431394=CARTESIAN_POINT('Ctrl Pts',(-2.41766918003243,1.12799783828675,
12.5821634970842));
#431395=CARTESIAN_POINT('Ctrl Pts',(-2.42703256801096,1.11925481433258,
12.5773203894503));
#431396=CARTESIAN_POINT('Ctrl Pts',(-2.41523183997244,1.11988432742864,
12.5969440695591));
#431397=CARTESIAN_POINT('Ctrl Pts',(-2.41688507232563,1.11622026338195,
12.5878292599214));
#431398=CARTESIAN_POINT('Ctrl Pts',(-2.42517145044037,1.11358203824974,
12.5813877129824));
#431399=CARTESIAN_POINT('Ctrl Pts',(-2.42789321447587,1.09202997693854,
12.596957478804));
#431400=CARTESIAN_POINT('Ctrl Pts',(-2.42625227301845,1.09566699553654,
12.5878468778671));
#431401=CARTESIAN_POINT('Ctrl Pts',(-2.42970856230818,1.10361504852349,
12.5814011370086));
#431402=CARTESIAN_POINT('Ctrl Pts',(-2.443427439057,1.08547048962603,12.5928371701607));
#431403=CARTESIAN_POINT('Ctrl Pts',(-2.43571288526976,1.08847394190091,
12.5821692192952));
#431404=CARTESIAN_POINT('Ctrl Pts',(-2.43523237626195,1.10127210321656,
12.5773318885715));
#431405=CARTESIAN_POINT('Ctrl Pts',(-2.45401129869476,1.08582632467571,
12.5893111709658));
#431406=CARTESIAN_POINT('Ctrl Pts',(-2.4426837395358,1.0854454860484,12.5770542771492));
#431407=CARTESIAN_POINT('Ctrl Pts',(-2.43909421506564,1.10141166871468,
12.5737548217797));
#431408=CARTESIAN_POINT('',(-2.42965842765956,1.12207316109535,12.5737548217797));
#431409=CARTESIAN_POINT('Origin',(-2.44378142924822,1.12859549396993,12.5893111709658));
#431410=CARTESIAN_POINT('Ctrl Pts',(-2.43909421506564,1.10141166871468,
12.5737548217797));
#431411=CARTESIAN_POINT('Ctrl Pts',(-2.43809425466414,1.10134534506547,
12.5746934679442));
#431412=CARTESIAN_POINT('Ctrl Pts',(-2.43697560860098,1.10145473621515,
12.5756680099006));
#431413=CARTESIAN_POINT('Ctrl Pts',(-2.43586522293742,1.10172408236073,
12.5765688348656));
#431414=CARTESIAN_POINT('Ctrl Pts',(-2.43557126062537,1.10179538877101,
12.5768073183026));
#431415=CARTESIAN_POINT('Ctrl Pts',(-2.43527787928168,1.1018776488304,12.5770407398754));
#431416=CARTESIAN_POINT('Ctrl Pts',(-2.43498729713664,1.10197002393467,
12.5772674179684));
#431417=CARTESIAN_POINT('Ctrl Pts',(-2.43379482659014,1.10234910638329,
12.5781976435658));
#431418=CARTESIAN_POINT('Ctrl Pts',(-2.43258518413186,1.10293081301547,
12.5790594849312));
#431419=CARTESIAN_POINT('Ctrl Pts',(-2.43146097448086,1.10371938475238,
12.5797571720116));
#431420=CARTESIAN_POINT('Ctrl Pts',(-2.43072851147025,1.1042331675935,12.580211740231));
#431421=CARTESIAN_POINT('Ctrl Pts',(-2.43000980833863,1.10487348219503,
12.5806009430798));
#431422=CARTESIAN_POINT('Ctrl Pts',(-2.42936724407257,1.10560848139795,
12.5808812374708));
#431423=CARTESIAN_POINT('Ctrl Pts',(-2.42881506819955,1.10624008954671,
12.5811221033394));
#431424=CARTESIAN_POINT('Ctrl Pts',(-2.42830789856473,1.10695462346068,
12.581287365893));
#431425=CARTESIAN_POINT('Ctrl Pts',(-2.427881159959,1.10771657978872,12.581359338449));
#431426=CARTESIAN_POINT('Ctrl Pts',(-2.42782185210462,1.10782247598452,
12.5813693411482));
#431427=CARTESIAN_POINT('Ctrl Pts',(-2.42776403878955,1.10792927798243,
12.5813775999465));
#431428=CARTESIAN_POINT('Ctrl Pts',(-2.4277077544834,1.10803688112628,12.5813841266931));
#431429=CARTESIAN_POINT('Ctrl Pts',(-2.42761226135055,1.10821944287415,
12.5813952001081));
#431430=CARTESIAN_POINT('Ctrl Pts',(-2.42752106945785,1.10840581565869,
12.5814007534795));
#431431=CARTESIAN_POINT('Ctrl Pts',(-2.42743439566389,1.10859600498354,
12.5814005856065));
#431432=CARTESIAN_POINT('Ctrl Pts',(-2.42703763692243,1.10946661735351,
12.5813998171494));
#431433=CARTESIAN_POINT('Ctrl Pts',(-2.42676265857133,1.11035691084844,
12.58127954464));
#431434=CARTESIAN_POINT('Ctrl Pts',(-2.42658275018652,1.11125309893149,
12.5810700125799));
#431435=CARTESIAN_POINT('Ctrl Pts',(-2.42636544134188,1.11233559209663,
12.5808169217085));
#431436=CARTESIAN_POINT('Ctrl Pts',(-2.42630322752117,1.1134300772724,12.5804173076348));
#431437=CARTESIAN_POINT('Ctrl Pts',(-2.42637556064734,1.11443915768868,
12.5799304713245));
#431438=CARTESIAN_POINT('Ctrl Pts',(-2.42646520417795,1.11568972621756,
12.5793271277669));
#431439=CARTESIAN_POINT('Ctrl Pts',(-2.42673494143363,1.11688899875593,
12.5785808224116));
#431440=CARTESIAN_POINT('Ctrl Pts',(-2.42714245864617,1.11799338346448,
12.5777485681082));
#431441=CARTESIAN_POINT('Ctrl Pts',(-2.4277497039397,1.1196390376746,12.576508418016));
#431442=CARTESIAN_POINT('Ctrl Pts',(-2.42865131903009,1.12106252274286,
12.5750928681475));
#431443=CARTESIAN_POINT('Ctrl Pts',(-2.42965842765956,1.12207316109535,
12.5737548217797));
#431444=CARTESIAN_POINT('Ctrl Pts',(-2.42965842765956,1.12207316109535,
12.5737548217797));
#431445=CARTESIAN_POINT('Ctrl Pts',(-2.41994263053451,1.13524156878495,
12.5770542771492));
#431446=CARTESIAN_POINT('Ctrl Pts',(-2.42764842286964,1.14355297053481,
12.5893111709658));
#431447=CARTESIAN_POINT('Ctrl Pts',(-2.44652873594355,1.14019518230089,
12.5508408821982));
#431448=CARTESIAN_POINT('Ctrl Pts',(-2.43678025017059,1.15340248141025,
12.55409748406));
#431449=CARTESIAN_POINT('Ctrl Pts',(-2.44449587312322,1.16172448638006,
12.5663972313419));
#431450=CARTESIAN_POINT('Ctrl Pts',(-2.46338170073771,1.15830030426781,
12.52790050457));
#431451=CARTESIAN_POINT('Ctrl Pts',(-2.45358562175745,1.1715286115652,12.5311362602938));
#431452=CARTESIAN_POINT('Ctrl Pts',(-2.4613263270679,1.17987767015181,12.5434568539655));
#431453=CARTESIAN_POINT('Ctrl Pts',(-2.48021865971795,1.17638984971966,
12.5049357605811));
#431454=CARTESIAN_POINT('Ctrl Pts',(-2.47036210698932,1.18962358514459,
12.5081700652078));
#431455=CARTESIAN_POINT('Ctrl Pts',(-2.47814111585804,1.19801395762177,
12.5204921097672));
#431456=CARTESIAN_POINT('Ctrl Pts',(-2.47911307783068,1.17520202033778,
12.5064436508395));
#431457=CARTESIAN_POINT('Ctrl Pts',(-2.47878550732966,1.176377411914,12.5062361689309));
#431458=CARTESIAN_POINT('Ctrl Pts',(-2.47839473950699,1.17758575463409,
12.5061871075061));
#431459=CARTESIAN_POINT('Ctrl Pts',(-2.47795136471677,1.1787322429404,12.5063648335164));
#431460=CARTESIAN_POINT('Ctrl Pts',(-2.47774995653857,1.17925304864746,
12.5064455676329));
#431461=CARTESIAN_POINT('Ctrl Pts',(-2.47753467801008,1.17976827515964,
12.506574497099));
#431462=CARTESIAN_POINT('Ctrl Pts',(-2.47731378992389,1.1802554259349,12.5067492519495));
#431463=CARTESIAN_POINT('Ctrl Pts',(-2.47686990674041,1.18123437432765,
12.5071004286051));
#431464=CARTESIAN_POINT('Ctrl Pts',(-2.47638631472707,1.18213560467378,
12.5076537929613));
#431465=CARTESIAN_POINT('Ctrl Pts',(-2.47590764438951,1.18289594706659,
12.5083435010505));
#431466=CARTESIAN_POINT('Ctrl Pts',(-2.47587750923121,1.18294381516405,
12.5083869222964));
#431467=CARTESIAN_POINT('Ctrl Pts',(-2.47584738019338,1.18299112372014,
12.5084308732337));
#431468=CARTESIAN_POINT('Ctrl Pts',(-2.47581726292796,1.18303785690299,
12.5084753333615));
#431469=CARTESIAN_POINT('Ctrl Pts',(-2.4755756827081,1.18341271871171,12.5088319622689));
#431470=CARTESIAN_POINT('Ctrl Pts',(-2.47533103987099,1.18375886925869,
12.509227847131));
#431471=CARTESIAN_POINT('Ctrl Pts',(-2.47509289553871,1.18406763175556,
12.5096423454524));
#431472=CARTESIAN_POINT('Ctrl Pts',(-2.47434665659961,1.18503515676821,
12.5109411997424));
#431473=CARTESIAN_POINT('Ctrl Pts',(-2.47362598515748,1.18570097563409,
12.5124831113042));
#431474=CARTESIAN_POINT('Ctrl Pts',(-2.47296176065527,1.18615454402601,
12.5140723025008));
#431475=CARTESIAN_POINT('Ctrl Pts',(-2.47289952209191,1.18619704388111,
12.5142212114565));
#431476=CARTESIAN_POINT('Ctrl Pts',(-2.47283777833191,1.18623770979641,
12.5143705582413));
#431477=CARTESIAN_POINT('Ctrl Pts',(-2.47277655587106,1.18627663231314,
12.5145201959299));
#431478=CARTESIAN_POINT('Ctrl Pts',(-2.47199006221069,1.18677664999011,
12.5164425148273));
#431479=CARTESIAN_POINT('Ctrl Pts',(-2.47126841277287,1.18701514499689,
12.5184635205941));
#431480=CARTESIAN_POINT('Ctrl Pts',(-2.47059240180699,1.18708025993212,
12.5205025929158));
#431481=CARTESIAN_POINT('Ctrl Pts',(-2.4702002886522,1.18711802917547,12.5216853356836));
#431482=CARTESIAN_POINT('Ctrl Pts',(-2.46982428505582,1.18709787849179,
12.5228750347131));
#431483=CARTESIAN_POINT('Ctrl Pts',(-2.4694664941172,1.18703793274305,12.5240609649613));
#431484=CARTESIAN_POINT('Ctrl Pts',(-2.46858831545318,1.18689079911873,
12.5269717671326));
#431485=CARTESIAN_POINT('Ctrl Pts',(-2.46779685772931,1.18648953404488,
12.5299036066169));
#431486=CARTESIAN_POINT('Ctrl Pts',(-2.46706587168992,1.18591672383515,
12.5328133004019));
#431487=CARTESIAN_POINT('Ctrl Pts',(-2.46671495582697,1.18564174158075,
12.5342101228451));
#431488=CARTESIAN_POINT('Ctrl Pts',(-2.46637873711443,1.18532715632361,
12.5356023438238));
#431489=CARTESIAN_POINT('Ctrl Pts',(-2.46605782225598,1.18498102042073,
12.5369868989719));
#431490=CARTESIAN_POINT('Origin',(-11.1269742283812,10.5343602107449,-1.23915455685045));
#431491=CARTESIAN_POINT('Ctrl Pts',(-2.51043156791945,1.08772316473061,
12.5369868989719));
#431492=CARTESIAN_POINT('Ctrl Pts',(-2.5257608466132,1.08826769977493,12.5369868989719));
#431493=CARTESIAN_POINT('Ctrl Pts',(-2.53157241165723,1.07407231265713,
12.5369868989719));
#431494=CARTESIAN_POINT('Ctrl Pts',(-2.51561346599296,1.08790717270204,
12.5218025310015));
#431495=CARTESIAN_POINT('Ctrl Pts',(-2.52706672854372,1.08499536215749,
12.5216901060418));
#431496=CARTESIAN_POINT('Ctrl Pts',(-2.53155471134322,1.07411559114987,
12.5161920673677));
#431497=CARTESIAN_POINT('Ctrl Pts',(-2.5189537241703,1.09292501551582,12.5042015548895));
#431498=CARTESIAN_POINT('Ctrl Pts',(-2.52478486974079,1.09020930449414,
12.4980677368513));
#431499=CARTESIAN_POINT('Ctrl Pts',(-2.5274735169963,1.08396735322399,12.4907278922778));
#431500=CARTESIAN_POINT('Ctrl Pts',(-2.5116139260195,1.10398694743621,12.506463626192));
#431501=CARTESIAN_POINT('Ctrl Pts',(-2.51760358068647,1.10661971694886,
12.4999376786891));
#431502=CARTESIAN_POINT('Ctrl Pts',(-2.51753042576366,1.10658756149731,
12.4906970594712));
#431503=CARTESIAN_POINT('Origin',(-2.51121257138441,1.06573703197408,12.5369868989719));
#431504=CARTESIAN_POINT('Origin',(-2.51121257138441,1.06573703197408,14.));
#431505=CARTESIAN_POINT('Origin',(-2.51121257138441,1.06573703197408,13.7435492065112));
#431506=CARTESIAN_POINT('Ctrl Pts',(-2.48572721599399,1.08689260369535,
13.793642941384));
#431507=CARTESIAN_POINT('Ctrl Pts',(-2.49653247935202,1.08728311972515,
13.8071662555867));
#431508=CARTESIAN_POINT('Ctrl Pts',(-2.499643077526,1.07053965644437,13.8103758687955));
#431509=CARTESIAN_POINT('Ctrl Pts',(-2.50233895234728,1.08745110217535,
13.7804579775006));
#431510=CARTESIAN_POINT('Ctrl Pts',(-2.51567203695235,1.08792282947323,
13.7901904343351));
#431511=CARTESIAN_POINT('Ctrl Pts',(-2.52101841522977,1.07310148798607,
13.7927914348263));
#431512=CARTESIAN_POINT('Ctrl Pts',(-2.51211890670968,1.08777991121118,
13.7597120340895));
#431513=CARTESIAN_POINT('Ctrl Pts',(-2.52754924305908,1.08832010572878,
13.7635825532445));
#431514=CARTESIAN_POINT('Ctrl Pts',(-2.53362646930207,1.07458681634366,
13.7651073818884));
#431515=CARTESIAN_POINT('Ctrl Pts',(-2.51020376771007,1.08771552287228,
13.7381884353898));
#431516=CARTESIAN_POINT('Ctrl Pts',(-2.52527289684106,1.08824397141278,
13.7368803041982));
#431517=CARTESIAN_POINT('Ctrl Pts',(-2.53115749549256,1.07429545407832,
13.7363986145813));
#431518=CARTESIAN_POINT('Origin',(-2.49049725742218,1.0650405719845,13.7902182540695));
#431519=CARTESIAN_POINT('Ctrl Pts',(-2.45400736474459,1.0858261916549,13.8235227101244));
#431520=CARTESIAN_POINT('Ctrl Pts',(-2.46549779565255,1.08621694204688,
13.8358800583119));
#431521=CARTESIAN_POINT('Ctrl Pts',(-2.46902410772919,1.07002462373867,
13.8390832900376));
#431522=CARTESIAN_POINT('Ctrl Pts',(-2.46592820869684,1.08622697683474,
13.8124254819052));
#431523=CARTESIAN_POINT('Ctrl Pts',(-2.47744095386821,1.08661848578045,
13.8247886449157));
#431524=CARTESIAN_POINT('Ctrl Pts',(-2.48095506764779,1.07040208095551,
13.8279860620657));
#431525=CARTESIAN_POINT('Ctrl Pts',(-2.47784371011467,1.08662758239573,
13.8013225099955));
#431526=CARTESIAN_POINT('Ctrl Pts',(-2.48937333731432,1.08701966716926,
13.8136962257787));
#431527=CARTESIAN_POINT('Ctrl Pts',(-2.49288049554766,1.07077963434886,
13.8168830918626));
#431528=CARTESIAN_POINT('Ctrl Pts',(-2.48975407686786,1.08702801532653,
13.7902140179785));
#431529=CARTESIAN_POINT('Ctrl Pts',(-2.50129550889728,1.08742050514159,
13.802602731458));
#431530=CARTESIAN_POINT('Ctrl Pts',(-2.50480060873704,1.07115728197905,
13.8057746032558));
#431531=CARTESIAN_POINT('Origin',(-2.45475053284426,1.06383874789086,13.8235269408515));
#431532=CARTESIAN_POINT('Ctrl Pts',(-2.42764842286964,1.14355297053481,
13.8235269408515));
#431533=CARTESIAN_POINT('Ctrl Pts',(-2.43567615593591,1.15221161480558,
13.8362179249168));
#431534=CARTESIAN_POINT('Ctrl Pts',(-2.42519536199323,1.16569552975593,
13.8391868794938));
#431535=CARTESIAN_POINT('Ctrl Pts',(-2.42030339654042,1.13563068791539,
13.8400110824519));
#431536=CARTESIAN_POINT('Ctrl Pts',(-2.42423099304139,1.14489868924187,
13.8494522556837));
#431537=CARTESIAN_POINT('Ctrl Pts',(-2.41318991562471,1.15258129927463,
13.85569149686));
#431538=CARTESIAN_POINT('Ctrl Pts',(-2.41508842470968,1.12019690047195,
13.8586819406589));
#431539=CARTESIAN_POINT('Ctrl Pts',(-2.41329242897892,1.12416306271903,
13.868010383617));
#431540=CARTESIAN_POINT('Ctrl Pts',(-2.40467127587644,1.1269141690376,13.8744918421245));
#431541=CARTESIAN_POINT('Ctrl Pts',(-2.42803883709481,1.09171254832903,
13.8587686893867));
#431542=CARTESIAN_POINT('Ctrl Pts',(-2.42981879718596,1.08778166166139,
13.8680909899357));
#431543=CARTESIAN_POINT('Ctrl Pts',(-2.42623225163339,1.07949715247226,
13.8745789365162));
#431544=CARTESIAN_POINT('Ctrl Pts',(-2.44319649798033,1.08546272525639,
13.8400379222776));
#431545=CARTESIAN_POINT('Ctrl Pts',(-2.45276816699803,1.08235573537491,
13.8494748685453));
#431546=CARTESIAN_POINT('Ctrl Pts',(-2.45134570433742,1.06898645322352,
13.8557104837033));
#431547=CARTESIAN_POINT('Ctrl Pts',(-2.45401129869484,1.08582632466916,
13.8235269408542));
#431548=CARTESIAN_POINT('Ctrl Pts',(-2.46581211258463,1.08622307437485,
13.8362179249195));
#431549=CARTESIAN_POINT('Ctrl Pts',(-2.4691391151553,1.06947213237294,13.8391868794965));
#431550=CARTESIAN_POINT('Origin',(-2.41151541649107,1.15851044709968,13.8235269408515));
#431551=CARTESIAN_POINT('Ctrl Pts',(-2.45196314593983,1.16977862413369,
13.7902140241683));
#431552=CARTESIAN_POINT('Ctrl Pts',(-2.4598177926985,1.17824403137073,13.8026027327198));
#431553=CARTESIAN_POINT('Ctrl Pts',(-2.44982222494642,1.19154315004781,
13.8057746032556));
#431554=CARTESIAN_POINT('Ctrl Pts',(-2.44386088740655,1.16103959732961,
13.8013225161808));
#431555=CARTESIAN_POINT('Ctrl Pts',(-2.45170749754734,1.16949634831233,
13.8136962270464));
#431556=CARTESIAN_POINT('Ctrl Pts',(-2.44173080383841,1.18278183618263,
13.8168830918628));
#431557=CARTESIAN_POINT('Ctrl Pts',(-2.43575513591674,1.15229680305245,
13.8124254880875));
#431558=CARTESIAN_POINT('Ctrl Pts',(-2.44359025551311,1.1607411725346,13.8247886461867));
#431559=CARTESIAN_POINT('Ctrl Pts',(-2.43363597355523,1.17401644401586,
13.8279860620656));
#431560=CARTESIAN_POINT('Ctrl Pts',(-2.42764575006183,1.14355008878014,
13.8235227163065));
#431561=CARTESIAN_POINT('Ctrl Pts',(-2.43546568366467,1.15197809101578,
13.8358800595848));
#431562=CARTESIAN_POINT('Ctrl Pts',(-2.42553759325522,1.16524680804569,
13.8390832900376));
#431563=CARTESIAN_POINT('Origin',(-2.43583282083151,1.18473899157597,13.7902182540695));
#431564=CARTESIAN_POINT('Ctrl Pts',(-2.46587432824779,1.18478314592408,
13.7382347919292));
#431565=CARTESIAN_POINT('Ctrl Pts',(-2.47615160437,1.19583282755939,13.7369371795942));
#431566=CARTESIAN_POINT('Ctrl Pts',(-2.46945101245651,1.20942127283577,
13.7364597369711));
#431567=CARTESIAN_POINT('Ctrl Pts',(-2.46716037143437,1.18617026052154,
13.7595490285574));
#431568=CARTESIAN_POINT('Ctrl Pts',(-2.47768211834678,1.19748426283415,
13.7633824266927));
#431569=CARTESIAN_POINT('Ctrl Pts',(-2.47126579107942,1.2110755984825,13.7648920890506));
#431570=CARTESIAN_POINT('Ctrl Pts',(-2.46060162164384,1.17909605206138,
13.780380659011));
#431571=CARTESIAN_POINT('Ctrl Pts',(-2.46970650931237,1.18887858274357,
13.7901039518743));
#431572=CARTESIAN_POINT('Ctrl Pts',(-2.46201635270427,1.20263892186614,
13.7926933640892));
#431573=CARTESIAN_POINT('Ctrl Pts',(-2.44920105035431,1.16679949864812,
13.7936647693663));
#431574=CARTESIAN_POINT('Ctrl Pts',(-2.45657624812666,1.17471023753671,
13.8072068914933));
#431575=CARTESIAN_POINT('Ctrl Pts',(-2.44593970851891,1.18803346143411,
13.8104111085397));
#431576=CARTESIAN_POINT('Origin',(-2.44992481587741,1.1999384969856,13.7435492065112));
#431577=CARTESIAN_POINT('Origin',(-2.44992481587741,1.1999384969856,14.));
#431578=CARTESIAN_POINT('Origin',(-2.44992481587741,1.1999384969856,12.5369868989719));
#431579=CARTESIAN_POINT('Ctrl Pts',(-2.47909646650412,1.1751941458713,12.506462012331));
#431580=CARTESIAN_POINT('Ctrl Pts',(-2.48500485080772,1.17799496412867,
12.4999388158272));
#431581=CARTESIAN_POINT('Ctrl Pts',(-2.48493494687304,1.17796182677563,
12.4907030323752));
#431582=CARTESIAN_POINT('Ctrl Pts',(-2.47554113020114,1.18798430485887,
12.5042014951932));
#431583=CARTESIAN_POINT('Ctrl Pts',(-2.47730746574457,1.19416663094731,
12.4980716682127));
#431584=CARTESIAN_POINT('Ctrl Pts',(-2.47435430417184,1.20028254477528,
12.4907355092743));
#431585=CARTESIAN_POINT('Ctrl Pts',(-2.46956264420209,1.18874811530927,
12.5218047446509));
#431586=CARTESIAN_POINT('Ctrl Pts',(-2.47485873145528,1.19930606637672,
12.5216906929434));
#431587=CARTESIAN_POINT('Ctrl Pts',(-2.46958136695414,1.20981892413528,
12.5161988840776));
#431588=CARTESIAN_POINT('Ctrl Pts',(-2.46603167910977,1.18495287197982,
12.5369868989719));
#431589=CARTESIAN_POINT('Ctrl Pts',(-2.47647386024285,1.19617634669597,
12.5369868989719));
#431590=CARTESIAN_POINT('Ctrl Pts',(-2.46956103641718,1.20985912412876,
12.5369868989719));
#431591=CARTESIAN_POINT('Origin',(-4.6862990577545E-31,-3.01170153175954E-31,
12.5));
#431592=CARTESIAN_POINT('Origin',(-2.51278080633585,0.94187200870957,12.5));
#431593=CARTESIAN_POINT('',(-2.51278080633585,0.94187200870957,12.5893111709658));
#431594=CARTESIAN_POINT('',(-2.51278080633585,0.94187200870957,13.8235269408515));
#431595=CARTESIAN_POINT('',(-2.51278080633585,0.94187200870957,12.5));
#431596=CARTESIAN_POINT('',(-2.53915516638814,0.966031185662302,13.7902182540695));
#431597=CARTESIAN_POINT('',(-2.51278080633585,0.94187200870957,13.8235269408515));
#431598=CARTESIAN_POINT('',(-2.55443917227924,0.980031487551614,13.7435492065112));
#431599=CARTESIAN_POINT('Origin',(-2.50415521495494,0.933970439180074,13.7445212918689));
#431600=CARTESIAN_POINT('',(-2.55443917227924,0.980031487551614,12.5369868989719));
#431601=CARTESIAN_POINT('',(-2.55443917227924,0.980031487551614,12.5));
#431602=CARTESIAN_POINT('Ctrl Pts',(-2.55443917227924,0.980031487551614,
12.5369868989719));
#431603=CARTESIAN_POINT('Ctrl Pts',(-2.54056317799091,0.967320938338584,
12.5544431401645));
#431604=CARTESIAN_POINT('Ctrl Pts',(-2.52667725922266,0.954601298202932,
12.5718848856037));
#431605=CARTESIAN_POINT('Ctrl Pts',(-2.51278080633585,0.94187200870957,
12.5893111709658));
#431606=CARTESIAN_POINT('Origin',(-2.80903407160718,0.868995909108973,12.5));
#431607=CARTESIAN_POINT('',(-2.59077959786119,0.879478411772282,13.7435492065112));
#431608=CARTESIAN_POINT('',(-2.5700764444425,0.880472759595378,13.7902182540695));
#431609=CARTESIAN_POINT('Origin',(-2.51567213548189,0.883085733816646,13.7418732680441));
#431610=CARTESIAN_POINT('',(-2.5343507043209,0.88218862438177,13.8235269408515));
#431611=CARTESIAN_POINT('',(-2.5700764444425,0.880472759595378,13.7902182540695));
#431612=CARTESIAN_POINT('',(-2.5343507043209,0.88218862438177,12.5893111709658));
#431613=CARTESIAN_POINT('',(-2.5343507043209,0.88218862438177,12.5));
#431614=CARTESIAN_POINT('',(-2.59077959786119,0.879478411772282,12.5369868989719));
#431615=CARTESIAN_POINT('Ctrl Pts',(-2.5343507043209,0.88218862438177,12.5893111709658));
#431616=CARTESIAN_POINT('Ctrl Pts',(-2.55317432936666,0.881284548069891,
12.5718848856037));
#431617=CARTESIAN_POINT('Ctrl Pts',(-2.57198368528205,0.880381157087365,
12.5544431401645));
#431618=CARTESIAN_POINT('Ctrl Pts',(-2.59077959786119,0.879478411772282,
12.5369868989719));
#431619=CARTESIAN_POINT('',(-2.59077959786119,0.879478411772282,12.5));
#431620=CARTESIAN_POINT('Origin',(-2.53599979373,0.916524045292556,12.5));
#431621=CARTESIAN_POINT('',(-2.50330861296455,0.90589969249633,13.8587068136939));
#431622=CARTESIAN_POINT('Ctrl Pts',(-2.53435070432044,0.882188624375176,
13.8235269408542));
#431623=CARTESIAN_POINT('Ctrl Pts',(-2.53260042357507,0.882272688276647,
13.8262006681044));
#431624=CARTESIAN_POINT('Ctrl Pts',(-2.53081760184798,0.882532254687068,
13.8288634856214));
#431625=CARTESIAN_POINT('Ctrl Pts',(-2.52900609155787,0.882954557835087,
13.8314912288862));
#431626=CARTESIAN_POINT('Ctrl Pts',(-2.52713861129738,0.883389908822146,
13.8342001611531));
#431627=CARTESIAN_POINT('Ctrl Pts',(-2.52523845519516,0.88399820766378,
13.8368750301949));
#431628=CARTESIAN_POINT('Ctrl Pts',(-2.52329991795237,0.884809566077829,
13.8394886372969));
#431629=CARTESIAN_POINT('Ctrl Pts',(-2.52315020001887,0.884872229256226,
13.8396904925131));
#431630=CARTESIAN_POINT('Ctrl Pts',(-2.52300025805097,0.884936125252825,
13.8398919674349));
#431631=CARTESIAN_POINT('Ctrl Pts',(-2.5228500929241,0.885001278833934,
13.8400930404591));
#431632=CARTESIAN_POINT('Ctrl Pts',(-2.52051041922137,0.886016415460797,
13.8432258934518));
#431633=CARTESIAN_POINT('Ctrl Pts',(-2.51812806255079,0.887330627611538,
13.8462331177034));
#431634=CARTESIAN_POINT('Ctrl Pts',(-2.515827318044,0.888985519365726,13.8489036603661));
#431635=CARTESIAN_POINT('Ctrl Pts',(-2.51507448766627,0.889527019206639,
13.8497774930041));
#431636=CARTESIAN_POINT('Ctrl Pts',(-2.51433064499445,0.890104983786962,
13.85061494757));
#431637=CARTESIAN_POINT('Ctrl Pts',(-2.51360085711104,0.890720827412258,
13.8514076489583));
#431638=CARTESIAN_POINT('Ctrl Pts',(-2.51205725048647,0.892023425497699,
13.8530843267192));
#431639=CARTESIAN_POINT('Ctrl Pts',(-2.51042680751305,0.893625698201537,
13.8546805203176));
#431640=CARTESIAN_POINT('Ctrl Pts',(-2.50889979581452,0.895531968935214,
13.8559412814273));
#431641=CARTESIAN_POINT('Ctrl Pts',(-2.50869543212709,0.895787089781212,
13.8561100121513));
#431642=CARTESIAN_POINT('Ctrl Pts',(-2.50849290645992,0.896047580140268,
13.8562727473908));
#431643=CARTESIAN_POINT('Ctrl Pts',(-2.50829265133,0.896313378282975,13.8564289040185));
#431644=CARTESIAN_POINT('Ctrl Pts',(-2.50738449660041,0.89751876982779,
13.8571370725437));
#431645=CARTESIAN_POINT('Ctrl Pts',(-2.50650889335531,0.898855879134049,
13.8577210840554));
#431646=CARTESIAN_POINT('Ctrl Pts',(-2.50572442859695,0.900288810448204,
13.8581177131616));
#431647=CARTESIAN_POINT('Ctrl Pts',(-2.50550349632054,0.900692373226265,
13.8582294175695));
#431648=CARTESIAN_POINT('Ctrl Pts',(-2.50528965689758,0.90110342224896,
13.8583265086086));
#431649=CARTESIAN_POINT('Ctrl Pts',(-2.50508386606588,0.901520893712507,
13.8584082369006));
#431650=CARTESIAN_POINT('Ctrl Pts',(-2.50478819982573,0.902120688256229,
13.8585256585398));
#431651=CARTESIAN_POINT('Ctrl Pts',(-2.50450576166904,0.902741339815834,
13.8586122832068));
#431652=CARTESIAN_POINT('Ctrl Pts',(-2.50424460728378,0.903367052748162,
13.8586682984299));
#431653=CARTESIAN_POINT('Ctrl Pts',(-2.50403570966297,0.903867561069096,
13.8587131050557));
#431654=CARTESIAN_POINT('Ctrl Pts',(-2.50383790661363,0.904376745668662,
13.8587357943552));
#431655=CARTESIAN_POINT('Ctrl Pts',(-2.50365164670807,0.904894850439687,
13.8587355499465));
#431656=CARTESIAN_POINT('Ctrl Pts',(-2.50353126249048,0.905229713905339,
13.8587353919793));
#431657=CARTESIAN_POINT('Ctrl Pts',(-2.50341696566905,0.905564669382782,
13.8587257282814));
#431658=CARTESIAN_POINT('Ctrl Pts',(-2.50330861296455,0.90589969249633,
13.8587068136939));
#431659=CARTESIAN_POINT('Ctrl Pts',(-2.50330861296455,0.90589969249633,
13.8587068136939));
#431660=CARTESIAN_POINT('Ctrl Pts',(-2.50295224682631,0.907001565253013,
13.8586446046466));
#431661=CARTESIAN_POINT('Ctrl Pts',(-2.50266009965791,0.908104169469626,
13.858482427929));
#431662=CARTESIAN_POINT('Ctrl Pts',(-2.50242778173392,0.909206658820027,
13.8582284286032));
#431663=CARTESIAN_POINT('Ctrl Pts',(-2.50218945056825,0.910337684646655,
13.8579678548414));
#431664=CARTESIAN_POINT('Ctrl Pts',(-2.50201500249059,0.911471668188101,
13.857615680862));
#431665=CARTESIAN_POINT('Ctrl Pts',(-2.50190173797787,0.912562429691672,
13.8571944833187));
#431666=CARTESIAN_POINT('Ctrl Pts',(-2.50161907480263,0.915284536577744,
13.8561433417727));
#431667=CARTESIAN_POINT('Ctrl Pts',(-2.50169947288329,0.91786429163513,
13.8546163505475));
#431668=CARTESIAN_POINT('Ctrl Pts',(-2.5019829092095,0.920170734935598,
13.8528973491087));
#431669=CARTESIAN_POINT('Ctrl Pts',(-2.50203468884459,0.920592088098222,
13.8525833129073));
#431670=CARTESIAN_POINT('Ctrl Pts',(-2.50209312821209,0.921004399866691,
13.8522628768812));
#431671=CARTESIAN_POINT('Ctrl Pts',(-2.50215712197049,0.921406994889097,
13.851937733538));
#431672=CARTESIAN_POINT('Ctrl Pts',(-2.50254792297429,0.923865586833268,
13.8499521282529));
#431673=CARTESIAN_POINT('Ctrl Pts',(-2.50318873402412,0.926205502410216,
13.847639871647));
#431674=CARTESIAN_POINT('Ctrl Pts',(-2.50396838900178,0.928324985081203,
13.8452109780794));
#431675=CARTESIAN_POINT('Ctrl Pts',(-2.50431917191428,0.929278584205991,
13.8441181685877));
#431676=CARTESIAN_POINT('Ctrl Pts',(-2.50469751444125,0.930188026878953,
13.8430021611332));
#431677=CARTESIAN_POINT('Ctrl Pts',(-2.5050915609998,0.931046865311944,
13.8418824960098));
#431678=CARTESIAN_POINT('Ctrl Pts',(-2.50602014177737,0.933070740010502,
13.8392439765549));
#431679=CARTESIAN_POINT('Ctrl Pts',(-2.50707688276956,0.934911925671254,
13.8364981347964));
#431680=CARTESIAN_POINT('Ctrl Pts',(-2.50823489914821,0.936592325950845,
13.8336931113419));
#431681=CARTESIAN_POINT('Ctrl Pts',(-2.50936273356018,0.938228929107881,
13.8309611966328));
#431682=CARTESIAN_POINT('Ctrl Pts',(-2.51058822791128,0.939714338658285,
13.8281701127186));
#431683=CARTESIAN_POINT('Ctrl Pts',(-2.51190857473627,0.941036244646406,
13.8253580685121));
#431684=CARTESIAN_POINT('Ctrl Pts',(-2.5121948273529,0.941322835291278,
13.8247484142933));
#431685=CARTESIAN_POINT('Ctrl Pts',(-2.51248557178476,0.941601570915133,
13.8241378483365));
#431686=CARTESIAN_POINT('Ctrl Pts',(-2.51278080633585,0.94187200870957,
13.8235269408515));
#431687=CARTESIAN_POINT('',(-2.50371375400294,0.904725538504549,12.5969504640361));
#431688=CARTESIAN_POINT('Origin',(-2.53603084286427,0.916535474818858,12.584524458991));
#431689=CARTESIAN_POINT('Origin',(-2.53603084286427,0.916535474818858,12.584524458991));
#431690=CARTESIAN_POINT('Ctrl Pts',(-2.5343507043209,0.88218862438177,12.5893111709658));
#431691=CARTESIAN_POINT('Ctrl Pts',(-2.52302979479693,0.882732354194952,
12.5770542771492));
#431692=CARTESIAN_POINT('Ctrl Pts',(-2.52075360628343,0.898937990273366,
12.5737548217797));
#431693=CARTESIAN_POINT('Ctrl Pts',(-2.5591057340396,0.880999669761492,
12.5663937883685));
#431694=CARTESIAN_POINT('Ctrl Pts',(-2.54777038312331,0.881544093177552,
12.5540940315303));
#431695=CARTESIAN_POINT('Ctrl Pts',(-2.545490321136,0.897800393883671,12.5508374392248));
#431696=CARTESIAN_POINT('Ctrl Pts',(-2.58383578623695,0.879811914781843,
12.5434499600945));
#431697=CARTESIAN_POINT('Ctrl Pts',(-2.57246358005819,0.88035810831233,
12.5311293540533));
#431698=CARTESIAN_POINT('Ctrl Pts',(-2.57020281348901,0.896662730328217,
12.5278936106989));
#431699=CARTESIAN_POINT('Ctrl Pts',(-2.60854281743612,0.878625265473343,
12.5204817579905));
#431700=CARTESIAN_POINT('Ctrl Pts',(-2.59711432660861,0.87917416228852,
12.5081597038247));
#431701=CARTESIAN_POINT('Ctrl Pts',(-2.59489296537332,0.895524990987918,
12.5049254088044));
#431702=CARTESIAN_POINT('Ctrl Pts',(-2.59077959786119,0.879478411772282,
12.5369868989719));
#431703=CARTESIAN_POINT('Ctrl Pts',(-2.59171003013044,0.879433724379648,
12.5342545179733));
#431704=CARTESIAN_POINT('Ctrl Pts',(-2.5926039767278,0.879515679211253,
12.5314872231885));
#431705=CARTESIAN_POINT('Ctrl Pts',(-2.59340597678606,0.879775327081827,
12.5287124745063));
#431706=CARTESIAN_POINT('Ctrl Pts',(-2.59412926024632,0.880009490419281,
12.5262100684184));
#431707=CARTESIAN_POINT('Ctrl Pts',(-2.5947767278187,0.880388876871923,
12.5237004536639));
#431708=CARTESIAN_POINT('Ctrl Pts',(-2.5953259831631,0.880977195780399,
12.5212220730815));
#431709=CARTESIAN_POINT('Ctrl Pts',(-2.59574648564362,0.881427604798481,
12.5193246583486));
#431710=CARTESIAN_POINT('Ctrl Pts',(-2.59611398545653,0.882006289955195,
12.5174178313691));
#431711=CARTESIAN_POINT('Ctrl Pts',(-2.59635830214115,0.882780547057912,
12.5155812248348));
#431712=CARTESIAN_POINT('Ctrl Pts',(-2.596462382362,0.883110384745324,12.5147988205794));
#431713=CARTESIAN_POINT('Ctrl Pts',(-2.59654447707654,0.883475966411407,
12.5140295443047));
#431714=CARTESIAN_POINT('Ctrl Pts',(-2.59660119699856,0.883883109633485,
12.5132817086137));
#431715=CARTESIAN_POINT('Ctrl Pts',(-2.59668703492763,0.884499265823006,
12.5121499604604));
#431716=CARTESIAN_POINT('Ctrl Pts',(-2.59670952797798,0.885224901530192,
12.5110494206568));
#431717=CARTESIAN_POINT('Ctrl Pts',(-2.59663380385397,0.886073086634248,
12.5100666561695));
#431718=CARTESIAN_POINT('Ctrl Pts',(-2.59659032323634,0.8865601125678,12.5095023550641));
#431719=CARTESIAN_POINT('Ctrl Pts',(-2.59651330758367,0.88709311249712,
12.5089719619137));
#431720=CARTESIAN_POINT('Ctrl Pts',(-2.59639787914041,0.88766118252928,
12.5085043804652));
#431721=CARTESIAN_POINT('Ctrl Pts',(-2.59622896464932,0.88849247902502,
12.5078201359221));
#431722=CARTESIAN_POINT('Ctrl Pts',(-2.59597170835315,0.88942274630422,
12.5072563000949));
#431723=CARTESIAN_POINT('Ctrl Pts',(-2.59563538869309,0.890386669471616,
12.5068768744332));
#431724=CARTESIAN_POINT('Ctrl Pts',(-2.59539287906586,0.891081724432006,
12.5066032824114));
#431725=CARTESIAN_POINT('Ctrl Pts',(-2.59510505738726,0.891806509298019,
12.5064197834844));
#431726=CARTESIAN_POINT('Ctrl Pts',(-2.59479039873085,0.892521504212145,
12.5063282718343));
#431727=CARTESIAN_POINT('Ctrl Pts',(-2.59433109450834,0.893565175429939,
12.5061946931565));
#431728=CARTESIAN_POINT('Ctrl Pts',(-2.59380576397003,0.894610722322953,
12.5062515701262));
#431729=CARTESIAN_POINT('Ctrl Pts',(-2.59326082840621,0.895600199381803,
12.5064436508398));
#431730=CARTESIAN_POINT('',(-2.52075360628343,0.898937990273366,12.5737548217797));
#431731=CARTESIAN_POINT('Origin',(-2.53540612154272,0.904163293764673,12.5893111709658));
#431732=CARTESIAN_POINT('Ctrl Pts',(-2.59326082840621,0.895600199381803,
12.5064436508398));
#431733=CARTESIAN_POINT('Ctrl Pts',(-2.58252789784408,0.896094759084691,
12.5164271754438));
#431734=CARTESIAN_POINT('Ctrl Pts',(-2.57179070313345,0.89658930611674,
12.5264061185523));
#431735=CARTESIAN_POINT('Ctrl Pts',(-2.56104909413815,0.897083840977176,
12.536380305637));
#431736=CARTESIAN_POINT('Ctrl Pts',(-2.54762426152707,0.897701909250244,
12.5488460165097));
#431737=CARTESIAN_POINT('Ctrl Pts',(-2.53419252986739,0.898319958669642,
12.5613043021964));
#431738=CARTESIAN_POINT('Ctrl Pts',(-2.52075360628343,0.898937990273366,
12.5737548217797));
#431739=CARTESIAN_POINT('Ctrl Pts',(-2.51278080633585,0.941872008709569,
12.5893111709658));
#431740=CARTESIAN_POINT('Ctrl Pts',(-2.50442319798712,0.934216356075794,
12.5770542771492));
#431741=CARTESIAN_POINT('Ctrl Pts',(-2.51303331912251,0.920299837513707,
12.5737548217797));
#431742=CARTESIAN_POINT('Ctrl Pts',(-2.50498323043713,0.934729351387608,
12.5928319619712));
#431743=CARTESIAN_POINT('Ctrl Pts',(-2.50156688092093,0.927182035814867,
12.5821634970842));
#431744=CARTESIAN_POINT('Ctrl Pts',(-2.51018647537985,0.91770490050594,
12.5773203894503));
#431745=CARTESIAN_POINT('Ctrl Pts',(-2.49847632445183,0.919294187836864,
12.5969440695591));
#431746=CARTESIAN_POINT('Ctrl Pts',(-2.49982540057543,0.915507561876375,
12.5878292599214));
#431747=CARTESIAN_POINT('Ctrl Pts',(-2.50786916661021,0.912202698477325,
12.5813877129824));
#431748=CARTESIAN_POINT('Ctrl Pts',(-2.50882518112397,0.890500500835704,
12.596957478804));
#431749=CARTESIAN_POINT('Ctrl Pts',(-2.50748615054405,0.89425916951689,
12.5878468778671));
#431750=CARTESIAN_POINT('Ctrl Pts',(-2.51157877942085,0.901899056349452,
12.5814011370086));
#431751=CARTESIAN_POINT('Ctrl Pts',(-2.52377305774301,0.882696656160039,
12.5928371701607));
#431752=CARTESIAN_POINT('Ctrl Pts',(-2.51632898274018,0.886318922447337,
12.5821692192951));
#431753=CARTESIAN_POINT('Ctrl Pts',(-2.51689324154602,0.899113664881937,
12.5773318885715));
#431754=CARTESIAN_POINT('Ctrl Pts',(-2.53435070432089,0.882188624381715,
12.5893111709658));
#431755=CARTESIAN_POINT('Ctrl Pts',(-2.52302979479692,0.882732354194897,
12.5770542771492));
#431756=CARTESIAN_POINT('Ctrl Pts',(-2.52075360628343,0.898937990273311,
12.5737548217797));
#431757=CARTESIAN_POINT('',(-2.51303331912251,0.920299837513707,12.5737548217797));
#431758=CARTESIAN_POINT('Origin',(-2.52764095826811,0.925649312122681,12.5893111709658));
#431759=CARTESIAN_POINT('Ctrl Pts',(-2.52075360628343,0.898937990273311,
12.5737548217797));
#431760=CARTESIAN_POINT('Ctrl Pts',(-2.51975156717454,0.898953393366479,
12.5746934679442));
#431761=CARTESIAN_POINT('Ctrl Pts',(-2.51864555970812,0.899153600565276,
12.5756680099006));
#431762=CARTESIAN_POINT('Ctrl Pts',(-2.5175608229726,0.899512557223679,
12.5765688348656));
#431763=CARTESIAN_POINT('Ctrl Pts',(-2.51727365093031,0.899607587025209,
12.5768073183026));
#431764=CARTESIAN_POINT('Ctrl Pts',(-2.51698795074734,0.899713486674167,
12.5770407398754));
#431765=CARTESIAN_POINT('Ctrl Pts',(-2.51670586491899,0.899829239550346,
12.5772674179684));
#431766=CARTESIAN_POINT('Ctrl Pts',(-2.51554826095865,0.900304258053291,
12.5781976435658));
#431767=CARTESIAN_POINT('Ctrl Pts',(-2.51439005797669,0.900982626194758,
12.5790594849312));
#431768=CARTESIAN_POINT('Ctrl Pts',(-2.51333386495786,0.901860207547482,
12.5797571720116));
#431769=CARTESIAN_POINT('Ctrl Pts',(-2.51264571722877,0.902431983353795,
12.580211740231));
#431770=CARTESIAN_POINT('Ctrl Pts',(-2.51198159710695,0.903128748338649,
12.5806009430798));
#431771=CARTESIAN_POINT('Ctrl Pts',(-2.51140108017891,0.903913676845319,
12.5808812374708));
#431772=CARTESIAN_POINT('Ctrl Pts',(-2.51090222355325,0.904588190829869,
12.5811221033394));
#431773=CARTESIAN_POINT('Ctrl Pts',(-2.51045498263095,0.905341686224759,
12.581287365893));
#431774=CARTESIAN_POINT('Ctrl Pts',(-2.51009177047712,0.906135890363982,
12.581359338449));
#431775=CARTESIAN_POINT('Ctrl Pts',(-2.51004129148778,0.906246268339646,
12.5813693411482));
#431776=CARTESIAN_POINT('Ctrl Pts',(-2.50999237589608,0.906357427284618,
12.5813775999465));
#431777=CARTESIAN_POINT('Ctrl Pts',(-2.50994504952647,0.906469260081351,
12.5813841266931));
#431778=CARTESIAN_POINT('Ctrl Pts',(-2.50986475461642,0.906658997946903,
12.5813952001081));
#431779=CARTESIAN_POINT('Ctrl Pts',(-2.50978905726936,0.906852183577215,
12.5814007534795));
#431780=CARTESIAN_POINT('Ctrl Pts',(-2.50971817407091,0.907048804781627,
12.5814005856065));
#431781=CARTESIAN_POINT('Ctrl Pts',(-2.50939369850195,0.907948859781517,
12.5813998171494));
#431782=CARTESIAN_POINT('Ctrl Pts',(-2.50919220230355,0.908858604186674,
12.58127954464));
#431783=CARTESIAN_POINT('Ctrl Pts',(-2.50908594019762,0.909766474481359,
12.5810700125799));
#431784=CARTESIAN_POINT('Ctrl Pts',(-2.50895758767257,0.910863078428028,
12.5808169217085));
#431785=CARTESIAN_POINT('Ctrl Pts',(-2.50898479156574,0.911958992798614,
12.5804173076348));
#431786=CARTESIAN_POINT('Ctrl Pts',(-2.50913913343118,0.912958819761757,
12.5799304713245));
#431787=CARTESIAN_POINT('Ctrl Pts',(-2.50933041162515,0.914197920347066,
12.5793271277669));
#431788=CARTESIAN_POINT('Ctrl Pts',(-2.50969700319774,0.915371216314544,
12.5785808224116));
#431789=CARTESIAN_POINT('Ctrl Pts',(-2.51019318203673,0.916438709838056,
12.5777485681082));
#431790=CARTESIAN_POINT('Ctrl Pts',(-2.51093254286728,0.918029392140734,
12.576508418016));
#431791=CARTESIAN_POINT('Ctrl Pts',(-2.51194718515588,0.919374650679806,
12.5750928681475));
#431792=CARTESIAN_POINT('Ctrl Pts',(-2.51303331912251,0.920299837513707,
12.5737548217797));
#431793=CARTESIAN_POINT('Ctrl Pts',(-2.51303331912251,0.920299837513707,
12.5737548217797));
#431794=CARTESIAN_POINT('Ctrl Pts',(-2.50442319798712,0.934216356075795,
12.5770542771492));
#431795=CARTESIAN_POINT('Ctrl Pts',(-2.51278080633585,0.94187200870957,
12.5893111709658));
#431796=CARTESIAN_POINT('Ctrl Pts',(-2.53132460581228,0.936986472447185,
12.5508408821982));
#431797=CARTESIAN_POINT('Ctrl Pts',(-2.52268507480955,0.950944417449307,
12.55409748406));
#431798=CARTESIAN_POINT('Ctrl Pts',(-2.53105334532603,0.958609836735127,
12.5663972313419));
#431799=CARTESIAN_POINT('Ctrl Pts',(-2.54959722927643,0.953657678028315,
12.52790050457));
#431800=CARTESIAN_POINT('Ctrl Pts',(-2.54091197579121,0.967640440603685,
12.5311362602938));
#431801=CARTESIAN_POINT('Ctrl Pts',(-2.54930745032697,0.97533077904262,
12.5434568539655));
#431802=CARTESIAN_POINT('Ctrl Pts',(-2.56785263055407,0.970314663546385,
12.5049357605811));
#431803=CARTESIAN_POINT('Ctrl Pts',(-2.55910754698467,0.984307765359549,
12.5081700652078));
#431804=CARTESIAN_POINT('Ctrl Pts',(-2.5675445650924,0.992036158124872,
12.5204921097672));
#431805=CARTESIAN_POINT('Ctrl Pts',(-2.56665390827743,0.969220901756311,
12.5064436508395));
#431806=CARTESIAN_POINT('Ctrl Pts',(-2.56642323306549,0.970419082350872,
12.5062361689309));
#431807=CARTESIAN_POINT('Ctrl Pts',(-2.5661322566399,0.971655255615505,
12.5061871075061));
#431808=CARTESIAN_POINT('Ctrl Pts',(-2.56578380658317,0.972834068238053,
12.5063648335164));
#431809=CARTESIAN_POINT('Ctrl Pts',(-2.56562551907411,0.973369557643392,
12.5064455676329));
#431810=CARTESIAN_POINT('Ctrl Pts',(-2.56545295261105,0.973900616980473,
12.506574497099));
#431811=CARTESIAN_POINT('Ctrl Pts',(-2.56527250682241,0.974404151231364,
12.5067492519495));
#431812=CARTESIAN_POINT('Ctrl Pts',(-2.56490989400573,0.975416022854365,
12.5071004286051));
#431813=CARTESIAN_POINT('Ctrl Pts',(-2.56450136974474,0.976353671669394,
12.5076537929613));
#431814=CARTESIAN_POINT('Ctrl Pts',(-2.56408626710693,0.977150500161891,
12.5083435010505));
#431815=CARTESIAN_POINT('Ctrl Pts',(-2.56406013391521,0.977200665277364,
12.5083869222964));
#431816=CARTESIAN_POINT('Ctrl Pts',(-2.56403396121578,0.977250272214424,
12.5084308732337));
#431817=CARTESIAN_POINT('Ctrl Pts',(-2.56400775335133,0.977299304733193,
12.5084753333615));
#431818=CARTESIAN_POINT('Ctrl Pts',(-2.56379753168718,0.977692610250802,
12.5088319622689));
#431819=CARTESIAN_POINT('Ctrl Pts',(-2.56358191736201,0.978057549672773,
12.509227847131));
#431820=CARTESIAN_POINT('Ctrl Pts',(-2.56336973244526,0.978384695761815,
12.5096423454524));
#431821=CARTESIAN_POINT('Ctrl Pts',(-2.56270483882527,0.979409826816081,
12.5109411997424));
#431822=CARTESIAN_POINT('Ctrl Pts',(-2.56204083577664,0.980132171637527,
12.5124831113042));
#431823=CARTESIAN_POINT('Ctrl Pts',(-2.56141579146133,0.980638371281332,
12.5140723025008));
#431824=CARTESIAN_POINT('Ctrl Pts',(-2.5613572241244,0.980685802742381,
12.5142212114565));
#431825=CARTESIAN_POINT('Ctrl Pts',(-2.56129900046128,0.980731366034844,
12.5143705582413));
#431826=CARTESIAN_POINT('Ctrl Pts',(-2.56124115425957,0.980775149239031,
12.5145201959299));
#431827=CARTESIAN_POINT('Ctrl Pts',(-2.56049803367459,0.981337609683192,
12.5164425148273));
#431828=CARTESIAN_POINT('Ctrl Pts',(-2.55979822502288,0.981634132246162,
12.5184635205941));
#431829=CARTESIAN_POINT('Ctrl Pts',(-2.55912977089943,0.981754131686319,
12.5205025929158));
#431830=CARTESIAN_POINT('Ctrl Pts',(-2.55874204101279,0.981823736117943,
12.5216853356836));
#431831=CARTESIAN_POINT('Ctrl Pts',(-2.55836564606957,0.981834300267755,
12.5228750347131));
#431832=CARTESIAN_POINT('Ctrl Pts',(-2.55800415951575,0.98180371726661,
12.5240609649613));
#431833=CARTESIAN_POINT('Ctrl Pts',(-2.55711691016249,0.981728652931021,
12.5269717671326));
#431834=CARTESIAN_POINT('Ctrl Pts',(-2.55629537912022,0.98139323418563,
12.5299036066169));
#431835=CARTESIAN_POINT('Ctrl Pts',(-2.55552013602678,0.980881912102984,
12.5328133004019));
#431836=CARTESIAN_POINT('Ctrl Pts',(-2.55514797420086,0.980636447729916,
12.5342101228451));
#431837=CARTESIAN_POINT('Ctrl Pts',(-2.55478723260943,0.980350314175644,
12.5356023438238));
#431838=CARTESIAN_POINT('Ctrl Pts',(-2.55443917227924,0.980031487551613,
12.5369868989719));
#431839=CARTESIAN_POINT('Origin',(-11.9498738845008,9.59352869647897,-1.24102268496923));
#431840=CARTESIAN_POINT('Ctrl Pts',(-2.59073784982797,0.879480377135765,
12.5369868989719));
#431841=CARTESIAN_POINT('Ctrl Pts',(-2.60606050627276,0.878773621761026,
12.5369868989719));
#431842=CARTESIAN_POINT('Ctrl Pts',(-2.61069567797988,0.864151772119807,
12.5369868989719));
#431843=CARTESIAN_POINT('Ctrl Pts',(-2.59591750392105,0.879241400036461,
12.5218025310015));
#431844=CARTESIAN_POINT('Ctrl Pts',(-2.6070953170942,0.875405731076495,
12.5216901060418));
#431845=CARTESIAN_POINT('Ctrl Pts',(-2.61068156416115,0.864196349346829,
12.5161920673677));
#431846=CARTESIAN_POINT('Ctrl Pts',(-2.59965564843752,0.88397028434133,
12.5042015548895));
#431847=CARTESIAN_POINT('Ctrl Pts',(-2.60524603569246,0.880788317126344,
12.4980677368513));
#431848=CARTESIAN_POINT('Ctrl Pts',(-2.60741695972008,0.874347985722612,
12.4907278922778));
#431849=CARTESIAN_POINT('Ctrl Pts',(-2.59324192300507,0.895593670284452,
12.506463626192));
#431850=CARTESIAN_POINT('Ctrl Pts',(-2.59942624274697,0.897729467013142,
12.4999376786891));
#431851=CARTESIAN_POINT('Ctrl Pts',(-2.59935071027332,0.897703381361547,
12.4906970594712));
#431852=CARTESIAN_POINT('Origin',(-2.58972418063936,0.857503742389379,12.5369868989719));
#431853=CARTESIAN_POINT('Origin',(-2.58972418063936,0.857503742389379,14.));
#431854=CARTESIAN_POINT('Origin',(-2.58972418063936,0.857503742389379,13.7435492065112));
#431855=CARTESIAN_POINT('Ctrl Pts',(-2.56604800116064,0.880666213749779,
13.793642941384));
#431856=CARTESIAN_POINT('Ctrl Pts',(-2.576849141578,0.880174701094858,13.8071662555867));
#431857=CARTESIAN_POINT('Ctrl Pts',(-2.57858464179707,0.863233407678336,
13.8103758687955));
#431858=CARTESIAN_POINT('Ctrl Pts',(-2.58264998614256,0.879868843143524,
13.7804579775005));
#431859=CARTESIAN_POINT('Ctrl Pts',(-2.59597715616263,0.879252230634105,
13.7901904343351));
#431860=CARTESIAN_POINT('Ctrl Pts',(-2.60009766788152,0.864044426475094,
13.7927914348262));
#431861=CARTESIAN_POINT('Ctrl Pts',(-2.59242419950251,0.879399401021213,
13.7597120340895));
#431862=CARTESIAN_POINT('Ctrl Pts',(-2.60784722354869,0.878680082425412,
13.7635825532445));
#431863=CARTESIAN_POINT('Ctrl Pts',(-2.61278483774422,0.864497139070781,
13.7651073818884));
#431864=CARTESIAN_POINT('Ctrl Pts',(-2.59051018472259,0.879491328536952,
13.7381884353898));
#431865=CARTESIAN_POINT('Ctrl Pts',(-2.60557224603145,0.878789744789382,
13.7368803041982));
#431866=CARTESIAN_POINT('Ctrl Pts',(-2.6103003305119,0.864407990575627,
13.7363986145813));
#431867=CARTESIAN_POINT('Origin',(-2.56902102722068,0.858498090212475,13.7902182540695));
#431868=CARTESIAN_POINT('Ctrl Pts',(-2.53434677261819,0.882188812456973,
13.8235227101244));
#431869=CARTESIAN_POINT('Ctrl Pts',(-2.54583081984969,0.881641685868309,
13.8358800583119));
#431870=CARTESIAN_POINT('Ctrl Pts',(-2.54802557414952,0.865215818992561,
13.8390832900376));
#431871=CARTESIAN_POINT('Ctrl Pts',(-2.54626061865845,0.881616604607372,
13.8124254819053));
#431872=CARTESIAN_POINT('Ctrl Pts',(-2.55776696773367,0.881068415228781,
13.8247886449158));
#431873=CARTESIAN_POINT('Ctrl Pts',(-2.55994760105056,0.864619536256662,
13.8279860620657));
#431874=CARTESIAN_POINT('Ctrl Pts',(-2.55816912530053,0.881044653202725,
13.8013225099955));
#431875=CARTESIAN_POINT('Ctrl Pts',(-2.56969234716577,0.880495661693927,
13.8136962257787));
#431876=CARTESIAN_POINT('Ctrl Pts',(-2.57186412217945,0.864023800288131,
13.8168830918626));
#431877=CARTESIAN_POINT('Ctrl Pts',(-2.57007250029219,0.880472948265155,
13.7902140179785));
#431878=CARTESIAN_POINT('Ctrl Pts',(-2.58160752072225,0.879923398246903,
13.802602731458));
#431879=CARTESIAN_POINT('Ctrl Pts',(-2.58377535396331,0.863428591441119,
13.8057746032558));
#431880=CARTESIAN_POINT('Origin',(-2.53329528709908,0.860213954998868,13.8235269408515));
#431881=CARTESIAN_POINT('Ctrl Pts',(-2.51278080633585,0.94187200870957,
13.8235269408515));
#431882=CARTESIAN_POINT('Ctrl Pts',(-2.52148758767358,0.94984750728508,
13.8362179249168));
#431883=CARTESIAN_POINT('Ctrl Pts',(-2.51214073195516,0.964140837626054,
13.8391868794938));
#431884=CARTESIAN_POINT('Ctrl Pts',(-2.50481448039544,0.934574774665753,
13.8400110824519));
#431885=CARTESIAN_POINT('Ctrl Pts',(-2.50948443629105,0.943491801905506,
13.8494522556836));
#431886=CARTESIAN_POINT('Ctrl Pts',(-2.49910630118824,0.952048798996971,
13.85569149686));
#431887=CARTESIAN_POINT('Ctrl Pts',(-2.49835886399634,0.919617410494477,
13.8586819406588));
#431888=CARTESIAN_POINT('Ctrl Pts',(-2.49689212333642,0.923716765989122,
13.868010383617));
#431889=CARTESIAN_POINT('Ctrl Pts',(-2.48852389711468,0.927161422241115,
13.8744918421245));
#431890=CARTESIAN_POINT('Ctrl Pts',(-2.50894444581712,0.890172258848369,
13.8587686893867));
#431891=CARTESIAN_POINT('Ctrl Pts',(-2.51039807948191,0.886109368610075,
13.8680909899357));
#431892=CARTESIAN_POINT('Ctrl Pts',(-2.50614820345524,0.878144762200234,
13.8745789365163));
#431893=CARTESIAN_POINT('Ctrl Pts',(-2.52354225223554,0.882707741467401,
13.8400379222776));
#431894=CARTESIAN_POINT('Ctrl Pts',(-2.53282882379497,0.878830909954466,
13.8494748685453));
#431895=CARTESIAN_POINT('Ctrl Pts',(-2.5303213736518,0.865622056898879,
13.8557104837033));
#431896=CARTESIAN_POINT('Ctrl Pts',(-2.53435070432044,0.882188624375176,
13.8235269408542));
#431897=CARTESIAN_POINT('Ctrl Pts',(-2.54614459075977,0.881622178043516,
13.8362179249195));
#431898=CARTESIAN_POINT('Ctrl Pts',(-2.54809516572253,0.864655791823373,
13.8391868794965));
#431899=CARTESIAN_POINT('Origin',(-2.49792065440359,0.958094705296459,13.8235269408515));
#431900=CARTESIAN_POINT('Ctrl Pts',(-2.53915225840624,0.966028522952471,
13.7902140241683));
#431901=CARTESIAN_POINT('Ctrl Pts',(-2.54767077875461,0.973825535615466,
13.8026027327198));
#431902=CARTESIAN_POINT('Ctrl Pts',(-2.53879247206483,0.98789513413836,
13.8057746032556));
#431903=CARTESIAN_POINT('Ctrl Pts',(-2.53036464765615,0.957978983827332,
13.8013225161808));
#431904=CARTESIAN_POINT('Ctrl Pts',(-2.53887445256273,0.965768024097925,
13.8136962270464));
#431905=CARTESIAN_POINT('Ctrl Pts',(-2.53001384607697,0.97982249875968,
13.8168830918628));
#431906=CARTESIAN_POINT('Ctrl Pts',(-2.521573248488,0.949925974473432,13.8124254880875));
#431907=CARTESIAN_POINT('Ctrl Pts',(-2.53007059187678,0.957703611027938,
13.8247886461867));
#431908=CARTESIAN_POINT('Ctrl Pts',(-2.52123148983828,0.971746076529088,
13.8279860620656));
#431909=CARTESIAN_POINT('Ctrl Pts',(-2.51277790753183,0.941869354402355,
13.8235227163066));
#431910=CARTESIAN_POINT('Ctrl Pts',(-2.52125878137466,0.949631915970467,
13.8358800595848));
#431911=CARTESIAN_POINT('Ctrl Pts',(-2.51244524948573,0.963665713975314,
13.8390832900376));
#431912=CARTESIAN_POINT('Origin',(-2.52429501445589,0.98225388224919,13.7902182540695));
#431913=CARTESIAN_POINT('Ctrl Pts',(-2.55424016022377,0.97984922793118,
13.7382347919292));
#431914=CARTESIAN_POINT('Ctrl Pts',(-2.56538389119101,0.990024449248841,
13.7369371795942));
#431915=CARTESIAN_POINT('Ctrl Pts',(-2.55981317938335,1.00411384054075,
13.7364597369711));
#431916=CARTESIAN_POINT('Ctrl Pts',(-2.55563498692476,0.981126902560485,
13.7595490285574));
#431917=CARTESIAN_POINT('Ctrl Pts',(-2.56704391981487,0.991545638411246,
13.7633824266926));
#431918=CARTESIAN_POINT('Ctrl Pts',(-2.56175676237833,1.00561474025,13.7648920890506));
#431919=CARTESIAN_POINT('Ctrl Pts',(-2.54852144716987,0.974610831941804,
13.780380659011));
#431920=CARTESIAN_POINT('Ctrl Pts',(-2.55839340614298,0.983618679189502,
13.7901039518744));
#431921=CARTESIAN_POINT('Ctrl Pts',(-2.55185043327982,0.997960051074283,
13.7926933640892));
#431922=CARTESIAN_POINT('Ctrl Pts',(-2.53615652708199,0.963284446693457,
13.7936647693663));
#431923=CARTESIAN_POINT('Ctrl Pts',(-2.54415198315131,0.970567716164538,
13.8072068914933));
#431924=CARTESIAN_POINT('Ctrl Pts',(-2.53463680218607,0.984713584856361,
13.8104111085397));
#431925=CARTESIAN_POINT('Origin',(-2.53957902034698,0.996254184138503,13.7435492065112));
#431926=CARTESIAN_POINT('Origin',(-2.53957902034698,0.996254184138503,14.));
#431927=CARTESIAN_POINT('Origin',(-2.53957902034698,0.996254184138503,12.5369868989719));
#431928=CARTESIAN_POINT('Ctrl Pts',(-2.56663671038155,0.969214407468799,
12.506462012331));
#431929=CARTESIAN_POINT('Ctrl Pts',(-2.5727537277133,0.971524318062958,
12.4999388158272));
#431930=CARTESIAN_POINT('Ctrl Pts',(-2.57268135537629,0.971496988791367,
12.4907030323752));
#431931=CARTESIAN_POINT('Ctrl Pts',(-2.56413572086239,0.982251801172283,
12.5042014951932));
#431932=CARTESIAN_POINT('Ctrl Pts',(-2.56640009604014,0.988269583336049,
12.4980716682127));
#431933=CARTESIAN_POINT('Ctrl Pts',(-2.56395526462324,0.994605857049262,
12.4907355092743));
#431934=CARTESIAN_POINT('Ctrl Pts',(-2.55823938542484,0.983500372216855,
12.5218047446509));
#431935=CARTESIAN_POINT('Ctrl Pts',(-2.56437842141187,0.993591512295486,
12.5216906929434));
#431936=CARTESIAN_POINT('Ctrl Pts',(-2.55997551240968,1.00449954358663,
12.5161988840776));
#431937=CARTESIAN_POINT('Ctrl Pts',(-2.55441082176292,0.980005563681427,
12.5369868989719));
#431938=CARTESIAN_POINT('Ctrl Pts',(-2.56573307478275,0.990340558508506,
12.5369868989719));
#431939=CARTESIAN_POINT('Ctrl Pts',(-2.55995852619355,1.00454126694547,
12.5369868989719));
#431940=CARTESIAN_POINT('Origin',(-4.84514877968061E-31,-3.40079961985221E-31,
12.5));
#431941=CARTESIAN_POINT('Origin',(-2.58119104811554,0.733923044064313,12.5));
#431942=CARTESIAN_POINT('',(-2.58119104811554,0.733923044064313,12.5893111709658));
#431943=CARTESIAN_POINT('',(-2.58119104811554,0.733923044064313,13.8235269408515));
#431944=CARTESIAN_POINT('',(-2.58119104811554,0.733923044064313,12.5));
#431945=CARTESIAN_POINT('',(-2.609446846865,0.755852078156851,13.7902182540695));
#431946=CARTESIAN_POINT('',(-2.58119104811554,0.733923044064313,13.8235269408515));
#431947=CARTESIAN_POINT('',(-2.62582115106377,0.768560006826658,13.7435492065112));
#431948=CARTESIAN_POINT('Origin',(-2.57195010640843,0.726750832130225,13.7445212918697));
#431949=CARTESIAN_POINT('',(-2.62582115106377,0.768560006826658,12.5369868989719));
#431950=CARTESIAN_POINT('',(-2.62582115106377,0.768560006826658,12.5));
#431951=CARTESIAN_POINT('Ctrl Pts',(-2.62582115106377,0.768560006826658,
12.5369868989719));
#431952=CARTESIAN_POINT('Ctrl Pts',(-2.6109553002419,0.757022773270534,
12.5544431401645));
#431953=CARTESIAN_POINT('Ctrl Pts',(-2.59607881696842,0.745477287978329,
12.5718848856037));
#431954=CARTESIAN_POINT('Ctrl Pts',(-2.58119104811554,0.733923044064313,
12.5893111709658));
#431955=CARTESIAN_POINT('Origin',(-2.87051847641971,0.637142042272538,12.5));
#431956=CARTESIAN_POINT('',(-2.65384464771224,0.665379431058958,13.7435492065112));
#431957=CARTESIAN_POINT('',(-2.63329143090733,0.668057969474022,13.7902182540695));
#431958=CARTESIAN_POINT('Origin',(-2.57928112945653,0.675096705483978,13.7418732680456));
#431959=CARTESIAN_POINT('',(-2.59782442414822,0.672680104343387,13.8235269408515));
#431960=CARTESIAN_POINT('',(-2.63329143090733,0.668057969474022,13.7902182540695));
#431961=CARTESIAN_POINT('',(-2.59782442414822,0.672680104343387,12.5893111709658));
#431962=CARTESIAN_POINT('',(-2.59782442414822,0.672680104343387,12.5));
#431963=CARTESIAN_POINT('',(-2.65384464771224,0.665379431058958,12.5369868989719));
#431964=CARTESIAN_POINT('Ctrl Pts',(-2.59782442414822,0.672680104343387,
12.5893111709658));
#431965=CARTESIAN_POINT('Ctrl Pts',(-2.61651172452203,0.670244736079616,
12.5718848856037));
#431966=CARTESIAN_POINT('Ctrl Pts',(-2.63518485910551,0.667811213931415,
12.5544431401645));
#431967=CARTESIAN_POINT('Ctrl Pts',(-2.65384464771224,0.665379431058958,
12.5369868989719));
#431968=CARTESIAN_POINT('',(-2.65384464771224,0.665379431058958,12.5));
#431969=CARTESIAN_POINT('Origin',(-2.60226668190707,0.706766860877324,12.5));
#431970=CARTESIAN_POINT('',(-2.56881829496413,0.698842494461434,13.8587068136939));
#431971=CARTESIAN_POINT('Ctrl Pts',(-2.59782442414722,0.672680104336852,
13.8235269408542));
#431972=CARTESIAN_POINT('Ctrl Pts',(-2.59608681930503,0.672906552652186,
13.8262006681044));
#431973=CARTESIAN_POINT('Ctrl Pts',(-2.5943310868423,0.673310571898458,
13.8288634856214));
#431974=CARTESIAN_POINT('Ctrl Pts',(-2.59256002583027,0.673879124773476,
13.8314912288862));
#431975=CARTESIAN_POINT('Ctrl Pts',(-2.59073424460335,0.67446524414411,
13.8342001611531));
#431976=CARTESIAN_POINT('Ctrl Pts',(-2.58888999311657,0.67522639928405,
13.8368750301949));
#431977=CARTESIAN_POINT('Ctrl Pts',(-2.58702403943955,0.6761930667517,13.8394886372969));
#431978=CARTESIAN_POINT('Ctrl Pts',(-2.58687992731091,0.676267724825033,
13.8396904925131));
#431979=CARTESIAN_POINT('Ctrl Pts',(-2.58673569237944,0.67634362987535,
13.8398919674349));
#431980=CARTESIAN_POINT('Ctrl Pts',(-2.58659133753637,0.676420806515196,
13.8400930404591));
#431981=CARTESIAN_POINT('Ctrl Pts',(-2.58434219196403,0.677623270485919,
13.8432258934518));
#431982=CARTESIAN_POINT('Ctrl Pts',(-2.58207488287958,0.679127293889516,
13.8462331177034));
#431983=CARTESIAN_POINT('Ctrl Pts',(-2.57991668295157,0.680964211164284,
13.8489036603661));
#431984=CARTESIAN_POINT('Ctrl Pts',(-2.57921049481889,0.681565271873869,
13.8497774930041));
#431985=CARTESIAN_POINT('Ctrl Pts',(-2.57851623670105,0.682201943407981,
13.85061494757));
#431986=CARTESIAN_POINT('Ctrl Pts',(-2.5778390740993,0.682875222351935,
13.8514076489583));
#431987=CARTESIAN_POINT('Ctrl Pts',(-2.57640677753513,0.684299304419751,
13.8530843267192));
#431988=CARTESIAN_POINT('Ctrl Pts',(-2.57491235982633,0.686029141931973,
13.8546805203176));
#431989=CARTESIAN_POINT('Ctrl Pts',(-2.57354580789501,0.688053535336556,
13.8559412814273));
#431990=CARTESIAN_POINT('Ctrl Pts',(-2.57336291892827,0.68832446482673,
13.8561100121513));
#431991=CARTESIAN_POINT('Ctrl Pts',(-2.57318229953109,0.688600596147636,
13.8562727473908));
#431992=CARTESIAN_POINT('Ctrl Pts',(-2.57300437574977,0.688881832521115,
13.8564289040185));
#431993=CARTESIAN_POINT('Ctrl Pts',(-2.57219749343134,0.690157236266359,
13.8571370725437));
#431994=CARTESIAN_POINT('Ctrl Pts',(-2.57143379050539,0.691561266244882,
13.8577210840554));
#431995=CARTESIAN_POINT('Ctrl Pts',(-2.57076873319358,0.693053370758716,
13.8581177131616));
#431996=CARTESIAN_POINT('Ctrl Pts',(-2.570581430164,0.69347359874649,13.8582294175695));
#431997=CARTESIAN_POINT('Ctrl Pts',(-2.57040180658542,0.693900709935634,
13.8583265086086));
#431998=CARTESIAN_POINT('Ctrl Pts',(-2.57023072830563,0.69433356616058,
13.8584082369006));
#431999=CARTESIAN_POINT('Ctrl Pts',(-2.56998493469404,0.694955464480841,
13.8585256585398));
#432000=CARTESIAN_POINT('Ctrl Pts',(-2.56975402519097,0.69559707220538,
13.8586122832068));
#432001=CARTESIAN_POINT('Ctrl Pts',(-2.5695447411882,0.696241989636382,
13.8586682984299));
#432002=CARTESIAN_POINT('Ctrl Pts',(-2.56937733473164,0.696757859652574,
13.8587131050557));
#432003=CARTESIAN_POINT('Ctrl Pts',(-2.56922169312754,0.697281472767224,
13.8587357943552));
#432004=CARTESIAN_POINT('Ctrl Pts',(-2.56907828333514,0.697813035498819,
13.8587355499465));
#432005=CARTESIAN_POINT('Ctrl Pts',(-2.56898559416724,0.698156597165358,
13.8587353919793));
#432006=CARTESIAN_POINT('Ctrl Pts',(-2.56889897964001,0.698499754358227,
13.8587257282814));
#432007=CARTESIAN_POINT('Ctrl Pts',(-2.56881829496413,0.698842494461434,
13.8587068136939));
#432008=CARTESIAN_POINT('Ctrl Pts',(-2.56881829496413,0.698842494461434,
13.8587068136939));
#432009=CARTESIAN_POINT('Ctrl Pts',(-2.56855292746382,0.699969747975907,
13.8586446046466));
#432010=CARTESIAN_POINT('Ctrl Pts',(-2.56835162487077,0.701092496074216,
13.858482427929));
#432011=CARTESIAN_POINT('Ctrl Pts',(-2.5682099430826,0.702210253049674,
13.8582284286032));
#432012=CARTESIAN_POINT('Ctrl Pts',(-2.56806459404903,0.703356941683728,
13.8579678548414));
#432013=CARTESIAN_POINT('Ctrl Pts',(-2.56798315661897,0.704501371126314,
13.857615680862));
#432014=CARTESIAN_POINT('Ctrl Pts',(-2.56795917617325,0.705597735320246,
13.8571944833187));
#432015=CARTESIAN_POINT('Ctrl Pts',(-2.56789933051843,0.708333824293116,
13.8561433417727));
#432016=CARTESIAN_POINT('Ctrl Pts',(-2.56818973506757,0.710898442238415,
13.8546163505475));
#432017=CARTESIAN_POINT('Ctrl Pts',(-2.56866022482375,0.713174108347192,
13.8528973491087));
#432018=CARTESIAN_POINT('Ctrl Pts',(-2.56874617636078,0.713589838970963,
13.8525833129073));
#432019=CARTESIAN_POINT('Ctrl Pts',(-2.56883802851296,0.713996015455054,
13.8522628768812));
#432020=CARTESIAN_POINT('Ctrl Pts',(-2.56893462456924,0.714392054790332,
13.851937733538));
#432021=CARTESIAN_POINT('Ctrl Pts',(-2.56952452328284,0.716810612062803,
13.8499521282529));
#432022=CARTESIAN_POINT('Ctrl Pts',(-2.570353926929,0.719090509714142,13.847639871647));
#432023=CARTESIAN_POINT('Ctrl Pts',(-2.57130374518305,0.721139390862746,
13.8452109780794));
#432024=CARTESIAN_POINT('Ctrl Pts',(-2.5717310880758,0.722061224901229,
13.8441181685877));
#432025=CARTESIAN_POINT('Ctrl Pts',(-2.57218229971992,0.722936803050407,
13.8430021611332));
#432026=CARTESIAN_POINT('Ctrl Pts',(-2.57264503842641,0.723760665316686,
13.8418824960098));
#432027=CARTESIAN_POINT('Ctrl Pts',(-2.57373549400471,0.725702117785256,
13.8392439765549));
#432028=CARTESIAN_POINT('Ctrl Pts',(-2.57493879250251,0.727451042851449,
13.8364981347964));
#432029=CARTESIAN_POINT('Ctrl Pts',(-2.57622992390006,0.72903146265238,
13.8336931113419));
#432030=CARTESIAN_POINT('Ctrl Pts',(-2.57748740388685,0.730570691172548,
13.8309611966328));
#432031=CARTESIAN_POINT('Ctrl Pts',(-2.57882989517482,0.731951268978667,
13.8281701127185));
#432032=CARTESIAN_POINT('Ctrl Pts',(-2.58025359626469,0.733161155909921,
13.825358068512));
#432033=CARTESIAN_POINT('Ctrl Pts',(-2.58056225619747,0.733423460702361,
13.8247484142932));
#432034=CARTESIAN_POINT('Ctrl Pts',(-2.58087475274221,0.733677570486074,
13.8241378483365));
#432035=CARTESIAN_POINT('Ctrl Pts',(-2.58119104811554,0.733923044064313,
13.8235269408515));
#432036=CARTESIAN_POINT('',(-2.56912638347858,0.697639224614051,12.5969504640361));
#432037=CARTESIAN_POINT('Origin',(-2.60229855934039,0.706775721580128,12.584524458991));
#432038=CARTESIAN_POINT('Origin',(-2.60229855934039,0.706775721580128,12.584524458991));
#432039=CARTESIAN_POINT('Ctrl Pts',(-2.59782442414822,0.672680104343387,
12.5893111709658));
#432040=CARTESIAN_POINT('Ctrl Pts',(-2.58658550304429,0.674144784164871,
12.5770542771492));
#432041=CARTESIAN_POINT('Ctrl Pts',(-2.58563779814648,0.690482027821057,
12.5737548217797));
#432042=CARTESIAN_POINT('Ctrl Pts',(-2.62240017270848,0.669477341134959,
12.5663937883685));
#432043=CARTESIAN_POINT('Ctrl Pts',(-2.61114691479985,0.67094388935897,
12.5540940315304));
#432044=CARTESIAN_POINT('Ctrl Pts',(-2.61019947895433,0.687331944784543,
12.5508374392248));
#432045=CARTESIAN_POINT('Ctrl Pts',(-2.6469511246397,0.666277809475349,
12.5434499600945));
#432046=CARTESIAN_POINT('Ctrl Pts',(-2.63566127838219,0.667749125969949,
12.5311293540532));
#432047=CARTESIAN_POINT('Ctrl Pts',(-2.63473701238633,0.6841837691644,12.5278936106989));
#432048=CARTESIAN_POINT('Ctrl Pts',(-2.67147922229582,0.663081256232907,
12.5204817579905));
#432049=CARTESIAN_POINT('Ctrl Pts',(-2.6601334990149,0.664559854738586,
12.5081597038247));
#432050=CARTESIAN_POINT('Ctrl Pts',(-2.65925227350856,0.681037338967124,
12.5049254088044));
#432051=CARTESIAN_POINT('Ctrl Pts',(-2.65384464771224,0.665379431058958,
12.5369868989719));
#432052=CARTESIAN_POINT('Ctrl Pts',(-2.65476834160751,0.665259053492282,
12.5342545179733));
#432053=CARTESIAN_POINT('Ctrl Pts',(-2.65566599375092,0.665267870679265,
12.5314872231885));
#432054=CARTESIAN_POINT('Ctrl Pts',(-2.65648648893205,0.665461284142814,
12.5287124745063));
#432055=CARTESIAN_POINT('Ctrl Pts',(-2.65722645221213,0.665635714004431,
12.5262100684184));
#432056=CARTESIAN_POINT('Ctrl Pts',(-2.65790268890752,0.665961063462004,
12.5237004536639));
#432057=CARTESIAN_POINT('Ctrl Pts',(-2.65849807010281,0.66650265537824,
12.5212220730815));
#432058=CARTESIAN_POINT('Ctrl Pts',(-2.65895388591238,0.666917290841554,
12.5193246583486));
#432059=CARTESIAN_POINT('Ctrl Pts',(-2.6593673311125,0.667464095824692,
12.5174178313691));
#432060=CARTESIAN_POINT('Ctrl Pts',(-2.65967394399523,0.66821586257285,
12.5155812248348));
#432061=CARTESIAN_POINT('Ctrl Pts',(-2.65980456273132,0.668536119248333,
12.5147988205794));
#432062=CARTESIAN_POINT('Ctrl Pts',(-2.65991618258215,0.668893792990215,
12.5140295443047));
#432063=CARTESIAN_POINT('Ctrl Pts',(-2.66000589972564,0.669294958276603,
12.5132817086137));
#432064=CARTESIAN_POINT('Ctrl Pts',(-2.66014167448565,0.669902067669133,
12.5121499604604));
#432065=CARTESIAN_POINT('Ctrl Pts',(-2.66022323873884,0.670623455490945,
12.5110494206568));
#432066=CARTESIAN_POINT('Ctrl Pts',(-2.66021690154075,0.671474990548134,
12.5100666561695));
#432067=CARTESIAN_POINT('Ctrl Pts',(-2.6602132627362,0.67196394001706,12.5095023550641));
#432068=CARTESIAN_POINT('Ctrl Pts',(-2.66017994778913,0.672501443923755,
12.5089719619137));
#432069=CARTESIAN_POINT('Ctrl Pts',(-2.66011120640582,0.673077032239456,
12.5085043804652));
#432070=CARTESIAN_POINT('Ctrl Pts',(-2.66001061234554,0.673919330763834,
12.5078201359221));
#432071=CARTESIAN_POINT('Ctrl Pts',(-2.65983003746791,0.674867471431794,
12.5072563000949));
#432072=CARTESIAN_POINT('Ctrl Pts',(-2.65957340557055,0.675855600398903,
12.5068768744332));
#432073=CARTESIAN_POINT('Ctrl Pts',(-2.65938835630595,0.676568109407218,
12.5066032824114));
#432074=CARTESIAN_POINT('Ctrl Pts',(-2.65916056902539,0.677313942750192,
12.5064197834844));
#432075=CARTESIAN_POINT('Ctrl Pts',(-2.65890523609289,0.67805220617937,
12.5063282718343));
#432076=CARTESIAN_POINT('Ctrl Pts',(-2.65853252906052,0.67912984222539,
12.5061946931565));
#432077=CARTESIAN_POINT('Ctrl Pts',(-2.6580941682944,0.680214729463172,
12.5062515701262));
#432078=CARTESIAN_POINT('Ctrl Pts',(-2.65763169752486,0.681245331426123,
12.5064436508398));
#432079=CARTESIAN_POINT('',(-2.58563779814648,0.690482027821057,12.5737548217797));
#432080=CARTESIAN_POINT('Origin',(-2.60066746911388,0.694495628525106,12.5893111709658));
#432081=CARTESIAN_POINT('Ctrl Pts',(-2.65763169752486,0.681245331426123,
12.5064436508398));
#432082=CARTESIAN_POINT('Ctrl Pts',(-2.64697479111083,0.682613079002884,
12.5164271754438));
#432083=CARTESIAN_POINT('Ctrl Pts',(-2.6363136337041,0.683981161518646,
12.5264061185523));
#432084=CARTESIAN_POINT('Ctrl Pts',(-2.62564807570878,0.685349591708476,
12.536380305637));
#432085=CARTESIAN_POINT('Ctrl Pts',(-2.61231829142286,0.687059851898216,
12.5488460165097));
#432086=CARTESIAN_POINT('Ctrl Pts',(-2.59898162950762,0.688770655633538,
12.5613043021964));
#432087=CARTESIAN_POINT('Ctrl Pts',(-2.58563779814648,0.690482027821057,
12.5737548217797));
#432088=CARTESIAN_POINT('Ctrl Pts',(-2.58119104811554,0.733923044064313,
12.5893111709658));
#432089=CARTESIAN_POINT('Ctrl Pts',(-2.57223724225788,0.726974087651802,
12.5770542771492));
#432090=CARTESIAN_POINT('Ctrl Pts',(-2.57968438846801,0.712402070352199,
12.5737548217797));
#432091=CARTESIAN_POINT('Ctrl Pts',(-2.57283722512644,0.727439728170275,
12.5928319619712));
#432092=CARTESIAN_POINT('Ctrl Pts',(-2.56881706694639,0.720195989868897,
12.5821634970842));
#432093=CARTESIAN_POINT('Ctrl Pts',(-2.57663550590669,0.710047811977098,
12.5773203894503));
#432094=CARTESIAN_POINT('Ctrl Pts',(-2.56509386121157,0.712586297097903,
12.5969440695591));
#432095=CARTESIAN_POINT('Ctrl Pts',(-2.56612980322656,0.708702308594637,
12.5878292599214));
#432096=CARTESIAN_POINT('Ctrl Pts',(-2.57387742724554,0.7047528002494,12.5813877129824));
#432097=CARTESIAN_POINT('Ctrl Pts',(-2.57306133011871,0.683044890822048,
12.596957478804));
#432098=CARTESIAN_POINT('Ctrl Pts',(-2.57203312144387,0.686900196266482,
12.5878468778671));
#432099=CARTESIAN_POINT('Ctrl Pts',(-2.57673485413781,0.694181074758283,
12.5814011370086));
#432100=CARTESIAN_POINT('Ctrl Pts',(-2.58732338312299,0.674048622082001,
12.5928371701607));
#432101=CARTESIAN_POINT('Ctrl Pts',(-2.58019932599553,0.678265596797179,
12.5821692192952));
#432102=CARTESIAN_POINT('Ctrl Pts',(-2.58180459756576,0.690971773450833,
12.5773318885715));
#432103=CARTESIAN_POINT('Ctrl Pts',(-2.5978244241482,0.672680104343332,
12.5893111709658));
#432104=CARTESIAN_POINT('Ctrl Pts',(-2.58658550304428,0.674144784164816,
12.5770542771492));
#432105=CARTESIAN_POINT('Ctrl Pts',(-2.58563779814647,0.690482027821002,
12.5737548217797));
#432106=CARTESIAN_POINT('',(-2.57968438846801,0.712402070352199,12.5737548217797));
#432107=CARTESIAN_POINT('Origin',(-2.59467945374212,0.71654308682464,12.5893111709658));
#432108=CARTESIAN_POINT('Ctrl Pts',(-2.58563779814647,0.690482027821002,
12.5737548217797));
#432109=CARTESIAN_POINT('Ctrl Pts',(-2.58464034873514,0.6905790551515,12.5746934679442));
#432110=CARTESIAN_POINT('Ctrl Pts',(-2.58355434016266,0.690868746053545,
12.5756680099006));
#432111=CARTESIAN_POINT('Ctrl Pts',(-2.5825024710992,0.691314924427426,
12.5765688348656));
#432112=CARTESIAN_POINT('Ctrl Pts',(-2.58222400040923,0.691433045212554,
12.5768073183026));
#432113=CARTESIAN_POINT('Ctrl Pts',(-2.58194788267456,0.691561879706389,
12.5770407398754));
#432114=CARTESIAN_POINT('Ctrl Pts',(-2.58167617039754,0.691700240038191,
12.5772674179684));
#432115=CARTESIAN_POINT('Ctrl Pts',(-2.58056113668672,0.692268033425692,
12.5781976435658));
#432116=CARTESIAN_POINT('Ctrl Pts',(-2.57946208083084,0.69303854864839,
12.5790594849312));
#432117=CARTESIAN_POINT('Ctrl Pts',(-2.57848093323446,0.693999299457811,
12.5797571720116));
#432118=CARTESIAN_POINT('Ctrl Pts',(-2.5778416802965,0.694625263155669,
12.580211740231));
#432119=CARTESIAN_POINT('Ctrl Pts',(-2.57723656279431,0.695373841667835,
12.5806009430798));
#432120=CARTESIAN_POINT('Ctrl Pts',(-2.57672195644868,0.696203475908542,
12.5808812374708));
#432121=CARTESIAN_POINT('Ctrl Pts',(-2.5762797388789,0.696916406949604,
12.5811221033394));
#432122=CARTESIAN_POINT('Ctrl Pts',(-2.57589540298367,0.697703849437877,
12.581287365893));
#432123=CARTESIAN_POINT('Ctrl Pts',(-2.5755981343987,0.698525016090779,
12.581359338449));
#432124=CARTESIAN_POINT('Ctrl Pts',(-2.57555682020375,0.698639141299089,
12.5813693411482));
#432125=CARTESIAN_POINT('Ctrl Pts',(-2.57551712786061,0.698753917446674,
12.5813775999465));
#432126=CARTESIAN_POINT('Ctrl Pts',(-2.57547907437673,0.698869235667479,
12.5813841266931));
#432127=CARTESIAN_POINT('Ctrl Pts',(-2.57541451203886,0.699064886976527,
12.5813952001081));
#432128=CARTESIAN_POINT('Ctrl Pts',(-2.57535481299079,0.699263599834116,
12.5814007534795));
#432129=CARTESIAN_POINT('Ctrl Pts',(-2.57530019210384,0.699465344436412,
12.5814005856065));
#432130=CARTESIAN_POINT('Ctrl Pts',(-2.57505015903876,0.700388852348694,
12.5813998171494));
#432131=CARTESIAN_POINT('Ctrl Pts',(-2.57492348591701,0.70131199346516,
12.58127954464));
#432132=CARTESIAN_POINT('Ctrl Pts',(-2.57489157724675,0.702225504244456,
12.5810700125799));
#432133=CARTESIAN_POINT('Ctrl Pts',(-2.57485303520616,0.703328921254315,
12.5808169217085));
#432134=CARTESIAN_POINT('Ctrl Pts',(-2.5749694757758,0.704418971690396,
12.5804173076348));
#432135=CARTESIAN_POINT('Ctrl Pts',(-2.57520479926084,0.705402891516927,
12.5799304713245));
#432136=CARTESIAN_POINT('Ctrl Pts',(-2.57549643919336,0.706622278148708,
12.5793271277669));
#432137=CARTESIAN_POINT('Ctrl Pts',(-2.57595744547643,0.707761789454208,
12.5785808224116));
#432138=CARTESIAN_POINT('Ctrl Pts',(-2.57653898395356,0.708785287799404,
12.5777485681082));
#432139=CARTESIAN_POINT('Ctrl Pts',(-2.57740553999678,0.710310412466362,
12.576508418016));
#432140=CARTESIAN_POINT('Ctrl Pts',(-2.57852645720657,0.711568492002621,
12.5750928681475));
#432141=CARTESIAN_POINT('Ctrl Pts',(-2.57968438846801,0.712402070352199,
12.5737548217797));
#432142=CARTESIAN_POINT('Ctrl Pts',(-2.57968438846801,0.712402070352199,
12.5737548217797));
#432143=CARTESIAN_POINT('Ctrl Pts',(-2.57223724225788,0.726974087651802,
12.5770542771492));
#432144=CARTESIAN_POINT('Ctrl Pts',(-2.58119104811554,0.733923044064313,
12.5893111709658));
#432145=CARTESIAN_POINT('Ctrl Pts',(-2.59927492806847,0.727542272211241,
12.5508408821982));
#432146=CARTESIAN_POINT('Ctrl Pts',(-2.59180184648936,0.74215797528504,
12.55409748406));
#432147=CARTESIAN_POINT('Ctrl Pts',(-2.60076707511013,0.749115796786229,
12.5663972313419));
#432148=CARTESIAN_POINT('Ctrl Pts',(-2.61884560890822,0.742668617284018,
12.52790050457));
#432149=CARTESIAN_POINT('Ctrl Pts',(-2.611328979847,0.757312782159411,12.5311362602938));
#432150=CARTESIAN_POINT('Ctrl Pts',(-2.62032335311021,0.764293222517126,
12.5434568539655));
#432151=CARTESIAN_POINT('Ctrl Pts',(-2.63839796579971,0.757782193377856,
12.5049357605811));
#432152=CARTESIAN_POINT('Ctrl Pts',(-2.63082254847786,0.772441539795387,
12.5081700652078));
#432153=CARTESIAN_POINT('Ctrl Pts',(-2.63986142886112,0.779456521670096,
12.5204921097672));
#432154=CARTESIAN_POINT('Ctrl Pts',(-2.63711408043268,0.756789777983852,
12.5064436508395));
#432155=CARTESIAN_POINT('Ctrl Pts',(-2.6369818356153,0.758002773902584,
12.5062361689309));
#432156=CARTESIAN_POINT('Ctrl Pts',(-2.6367925869869,0.759258551182633,
12.5061871075061));
#432157=CARTESIAN_POINT('Ctrl Pts',(-2.63654138054129,0.760461843317901,
12.5063648335164));
#432158=CARTESIAN_POINT('Ctrl Pts',(-2.63642726707863,0.761008452827877,
12.5064455676329));
#432159=CARTESIAN_POINT('Ctrl Pts',(-2.63629856108233,0.761551810877591,
12.506574497099));
#432160=CARTESIAN_POINT('Ctrl Pts',(-2.6361597584282,0.762068377666752,
12.5067492519495));
#432161=CARTESIAN_POINT('Ctrl Pts',(-2.63588082910678,0.763106438681291,
12.5071004286051));
#432162=CARTESIAN_POINT('Ctrl Pts',(-2.6355500912597,0.764074266067061,
12.5076537929613));
#432163=CARTESIAN_POINT('Ctrl Pts',(-2.63520131876121,0.764902277897087,
12.5083435010505));
#432164=CARTESIAN_POINT('Ctrl Pts',(-2.63517936144816,0.764954406190012,
12.5083869222964));
#432165=CARTESIAN_POINT('Ctrl Pts',(-2.63515731926212,0.765005981382064,
12.5084308732337));
#432166=CARTESIAN_POINT('Ctrl Pts',(-2.63513519520765,0.765056986933429,
12.5084753333615));
#432167=CARTESIAN_POINT('Ctrl Pts',(-2.6349577310897,0.765466118776604,
12.5088319622689));
#432168=CARTESIAN_POINT('Ctrl Pts',(-2.63477258015423,0.765847418461921,
12.509227847131));
#432169=CARTESIAN_POINT('Ctrl Pts',(-2.63458776670862,0.766190771039883,
12.5096423454524));
#432170=CARTESIAN_POINT('Ctrl Pts',(-2.63400864316508,0.767266686057732,
12.5109411997424));
#432171=CARTESIAN_POINT('Ctrl Pts',(-2.63340572734068,0.768040749749141,
12.5124831113042));
#432172=CARTESIAN_POINT('Ctrl Pts',(-2.63282402277907,0.768596211969716,
12.5140723025008));
#432173=CARTESIAN_POINT('Ctrl Pts',(-2.63276951642453,0.768648259388164,
12.5142212114565));
#432174=CARTESIAN_POINT('Ctrl Pts',(-2.63271520032718,0.768698416841596,
12.5143705582413));
#432175=CARTESIAN_POINT('Ctrl Pts',(-2.63266111534153,0.768746769363242,
12.5145201959299));
#432176=CARTESIAN_POINT('Ctrl Pts',(-2.63196631317682,0.769367929493147,
12.5164425148273));
#432177=CARTESIAN_POINT('Ctrl Pts',(-2.63129300242233,0.769720506303571,
12.5184635205941));
#432178=CARTESIAN_POINT('Ctrl Pts',(-2.63063655359323,0.769894591672177,
12.5205025929158));
#432179=CARTESIAN_POINT('Ctrl Pts',(-2.63025578725315,0.769995568086067,
12.5216853356836));
#432180=CARTESIAN_POINT('Ctrl Pts',(-2.62988150580933,0.770036776766694,
12.5228750347131));
#432181=CARTESIAN_POINT('Ctrl Pts',(-2.62951872927369,0.770035760037976,
12.5240609649613));
#432182=CARTESIAN_POINT('Ctrl Pts',(-2.62862831372925,0.770033264531883,
12.5269717671326));
#432183=CARTESIAN_POINT('Ctrl Pts',(-2.62778217652212,0.769765924271362,
12.5299036066169));
#432184=CARTESIAN_POINT('Ctrl Pts',(-2.6269678354895,0.769319493079882,
12.5328133004019));
#432185=CARTESIAN_POINT('Ctrl Pts',(-2.62657690437617,0.769105180113062,
12.5342101228451));
#432186=CARTESIAN_POINT('Ctrl Pts',(-2.62619404058162,0.768849402433252,
12.5356023438238));
#432187=CARTESIAN_POINT('Ctrl Pts',(-2.62582115106377,0.768560006826658,
12.5369868989719));
#432188=CARTESIAN_POINT('Origin',(-12.6912014024061,8.58690233099497,-1.23983103325459));
#432189=CARTESIAN_POINT('Ctrl Pts',(-2.65380319878753,0.665384792735134,
12.5369868989719));
#432190=CARTESIAN_POINT('Ctrl Pts',(-2.6690172632328,0.66343145028175,12.5369868989719));
#432191=CARTESIAN_POINT('Ctrl Pts',(-2.67244519530005,0.648480444114029,
12.5369868989719));
#432192=CARTESIAN_POINT('Ctrl Pts',(-2.65894613915679,0.664724420918261,
12.5218025310015));
#432193=CARTESIAN_POINT('Ctrl Pts',(-2.66977411644987,0.659990419286952,
12.5216901060417));
#432194=CARTESIAN_POINT('Ctrl Pts',(-2.67243476190172,0.64852602342125,
12.5161920673678));
#432195=CARTESIAN_POINT('Ctrl Pts',(-2.66305729327739,0.669132876769389,
12.5042015548895));
#432196=CARTESIAN_POINT('Ctrl Pts',(-2.66836971911194,0.665505828827929,
12.4980677368514));
#432197=CARTESIAN_POINT('Ctrl Pts',(-2.67000847277043,0.658909976633512,
12.4907278922777));
#432198=CARTESIAN_POINT('Ctrl Pts',(-2.65761232284785,0.681240365019505,
12.506463626192));
#432199=CARTESIAN_POINT('Ctrl Pts',(-2.66395015203713,0.682864975589384,
12.4999376786891));
#432200=CARTESIAN_POINT('Ctrl Pts',(-2.66387274466878,0.682845133333455,
12.4906970594712));
#432201=CARTESIAN_POINT('Origin',(-2.65100160274658,0.643563906877238,12.5369868989719));
#432202=CARTESIAN_POINT('Origin',(-2.65100160274658,0.643563906877238,14.));
#432203=CARTESIAN_POINT('Origin',(-2.65100160274658,0.643563906877238,13.7435492065112));
#432204=CARTESIAN_POINT('Ctrl Pts',(-2.6292921602477,0.668579135451396,
13.793642941384));
#432205=CARTESIAN_POINT('Ctrl Pts',(-2.640017297917,0.667208865047367,13.8071662555867));
#432206=CARTESIAN_POINT('Ctrl Pts',(-2.6403661507135,0.650182483007689,
13.8103758687955));
#432207=CARTESIAN_POINT('Ctrl Pts',(-2.64577391038728,0.666431202128725,
13.7804579775006));
#432208=CARTESIAN_POINT('Ctrl Pts',(-2.65900647570461,0.664730353266513,
13.7901904343351));
#432209=CARTESIAN_POINT('Ctrl Pts',(-2.66187369953941,0.649237291863243,
13.7927914348263));
#432210=CARTESIAN_POINT('Ctrl Pts',(-2.65547733696763,0.665166632908131,
13.7597120340895));
#432211=CARTESIAN_POINT('Ctrl Pts',(-2.67079041103023,0.663192588145461,
13.7635825532445));
#432212=CARTESIAN_POINT('Ctrl Pts',(-2.67455555417036,0.648654375969331,
13.7651073818884));
#432213=CARTESIAN_POINT('Ctrl Pts',(-2.65357718385987,0.665414264516065,
13.7381884353898));
#432214=CARTESIAN_POINT('Ctrl Pts',(-2.66853194181363,0.663487317404509,
13.7368803041982));
#432215=CARTESIAN_POINT('Ctrl Pts',(-2.67207204750091,0.648768034512946,
13.7363986145813));
#432216=CARTESIAN_POINT('Origin',(-2.63044838594166,0.646242445292302,13.7902182540695));
#432217=CARTESIAN_POINT('Ctrl Pts',(-2.59782052085778,0.672680612263058,
13.8235227101244));
#432218=CARTESIAN_POINT('Ctrl Pts',(-2.60922175997325,0.671199249730936,
13.8358800583119));
#432219=CARTESIAN_POINT('Ctrl Pts',(-2.61007035076852,0.654649145721622,
13.8390832900376));
#432220=CARTESIAN_POINT('Ctrl Pts',(-2.60964808430635,0.671139219332836,
13.8124254819053));
#432221=CARTESIAN_POINT('Ctrl Pts',(-2.62107146443071,0.669654979739829,
13.8247886449158));
#432222=CARTESIAN_POINT('Ctrl Pts',(-2.62190410552995,0.653083091196193,
13.8279860620657));
#432223=CARTESIAN_POINT('Ctrl Pts',(-2.6214703470257,0.669598517204799,
13.8013225099955));
#432224=CARTESIAN_POINT('Ctrl Pts',(-2.63291047841627,0.668112102861582,
13.8136962257787));
#432225=CARTESIAN_POINT('Ctrl Pts',(-2.63373241740585,0.651518030390368,
13.8168830918626));
#432226=CARTESIAN_POINT('Ctrl Pts',(-2.63328751525918,0.668058479000884,
13.7902140179785));
#432227=CARTESIAN_POINT('Ctrl Pts',(-2.64473936043208,0.666570546314042,
13.802602731458));
#432228=CARTESIAN_POINT('Ctrl Pts',(-2.64555550050187,0.649953926082836,
13.8057746032558));
#432229=CARTESIAN_POINT('Origin',(-2.59498137918255,0.650864580161667,13.8235269408515));
#432230=CARTESIAN_POINT('Ctrl Pts',(-2.58119104811554,0.733923044064314,
13.8235269408515));
#432231=CARTESIAN_POINT('Ctrl Pts',(-2.59051893553145,0.741162321317405,
13.8362179249168));
#432232=CARTESIAN_POINT('Ctrl Pts',(-2.58236821981996,0.756169947293812,
13.8391868794938));
#432233=CARTESIAN_POINT('Ctrl Pts',(-2.57265643714878,0.727299420484737,
13.8400110824519));
#432234=CARTESIAN_POINT('Ctrl Pts',(-2.57803767465309,0.735806132292735,
13.8494522556837));
#432235=CARTESIAN_POINT('Ctrl Pts',(-2.56839154664088,0.745180571039019,
13.85569149686));
#432236=CARTESIAN_POINT('Ctrl Pts',(-2.5650031372433,0.71291801837636,13.8586819406588));
#432237=CARTESIAN_POINT('Ctrl Pts',(-2.56387541257129,0.71712328658411,
13.868010383617));
#432238=CARTESIAN_POINT('Ctrl Pts',(-2.55581580239515,0.721238569150482,
13.8744918421245));
#432239=CARTESIAN_POINT('Ctrl Pts',(-2.57315344319922,0.682708019853152,
13.8587686893867));
#432240=CARTESIAN_POINT('Ctrl Pts',(-2.57427107674546,0.678540163908405,
13.8680909899357));
#432241=CARTESIAN_POINT('Ctrl Pts',(-2.56938615246847,0.670948463419457,
13.8745789365163));
#432242=CARTESIAN_POINT('Ctrl Pts',(-2.58709424915727,0.674078483295469,
13.8400379222776));
#432243=CARTESIAN_POINT('Ctrl Pts',(-2.59603392265685,0.669457609825165,
13.8494748685453));
#432244=CARTESIAN_POINT('Ctrl Pts',(-2.59245817169815,0.656497088603161,
13.8557104837033));
#432245=CARTESIAN_POINT('Ctrl Pts',(-2.59782442414722,0.672680104336852,
13.8235269408542));
#432246=CARTESIAN_POINT('Ctrl Pts',(-2.60953289676769,0.671154231574727,
13.8362179249195));
#432247=CARTESIAN_POINT('Ctrl Pts',(-2.61009406336799,0.654085309637386,
13.8391868794965));
#432248=CARTESIAN_POINT('Origin',(-2.56770264248896,0.751303001303987,13.8235269408515));
#432249=CARTESIAN_POINT('Ctrl Pts',(-2.60944373152358,0.755849661334478,
13.7902140241682));
#432250=CARTESIAN_POINT('Ctrl Pts',(-2.61856943611421,0.762926391590561,
13.8026027327198));
#432251=CARTESIAN_POINT('Ctrl Pts',(-2.61086747415291,0.777672839102445,
13.8057746032556));
#432252=CARTESIAN_POINT('Ctrl Pts',(-2.60002924865636,0.748543178243071,
13.8013225161807));
#432253=CARTESIAN_POINT('Ctrl Pts',(-2.60914561698112,0.755612673023652,
13.8136962270464));
#432254=CARTESIAN_POINT('Ctrl Pts',(-2.6014600635928,0.770342604266843,
13.8168830918628));
#432255=CARTESIAN_POINT('Ctrl Pts',(-2.5906107071209,0.741233545261063,
13.8124254880875));
#432256=CARTESIAN_POINT('Ctrl Pts',(-2.5997137258838,0.748292689999847,
13.8247886461868));
#432257=CARTESIAN_POINT('Ctrl Pts',(-2.59204862653035,0.763008899229835,
13.8279860620656));
#432258=CARTESIAN_POINT('Ctrl Pts',(-2.58118794260636,0.733920634868514,
13.8235227163065));
#432259=CARTESIAN_POINT('Ctrl Pts',(-2.59027331787303,0.740966097202585,
13.8358800595847));
#432260=CARTESIAN_POINT('Ctrl Pts',(-2.58263299710521,0.755671583572082,
13.8390832900376));
#432261=CARTESIAN_POINT('Origin',(-2.59595844123842,0.773232035396524,13.7902182540695));
#432262=CARTESIAN_POINT('Ctrl Pts',(-2.62560794535342,0.768394574990138,
13.7382347919292));
#432263=CARTESIAN_POINT('Ctrl Pts',(-2.63754397147469,0.777627621571077,
13.7369371795943));
#432264=CARTESIAN_POINT('Ctrl Pts',(-2.63314021194084,0.792124196304043,
13.7364597369711));
#432265=CARTESIAN_POINT('Ctrl Pts',(-2.62710227322728,0.769554306937452,
13.7595490285574));
#432266=CARTESIAN_POINT('Ctrl Pts',(-2.63932246752902,0.779008441358257,
13.7633824266926));
#432267=CARTESIAN_POINT('Ctrl Pts',(-2.63519966508372,0.793461681835887,
13.7648920890506));
#432268=CARTESIAN_POINT('Ctrl Pts',(-2.61948128294142,0.763639737535113,
13.780380659011));
#432269=CARTESIAN_POINT('Ctrl Pts',(-2.63005461696086,0.771812955611082,
13.7901039518744));
#432270=CARTESIAN_POINT('Ctrl Pts',(-2.62470237024758,0.78663992079435,
13.7926933640892));
#432271=CARTESIAN_POINT('Ctrl Pts',(-2.60623430055833,0.7533588956768,13.7936647693663));
#432272=CARTESIAN_POINT('Ctrl Pts',(-2.61479680648362,0.759966226773704,
13.8072068914933));
#432273=CARTESIAN_POINT('Ctrl Pts',(-2.60646630612032,0.774840601837694,
13.8104111085397));
#432274=CARTESIAN_POINT('Origin',(-2.61233274543719,0.785939964066332,13.7435492065112));
#432275=CARTESIAN_POINT('Origin',(-2.61233274543719,0.785939964066332,14.));
#432276=CARTESIAN_POINT('Origin',(-2.61233274543719,0.785939964066332,12.5369868989719));
#432277=CARTESIAN_POINT('Ctrl Pts',(-2.63709641041666,0.756784707093716,
12.506462012331));
#432278=CARTESIAN_POINT('Ctrl Pts',(-2.64338135303544,0.75858833795077,
12.4999388158272));
#432279=CARTESIAN_POINT('Ctrl Pts',(-2.64330699392206,0.758566998632415,
12.4907030323752));
#432280=CARTESIAN_POINT('Ctrl Pts',(-2.63566641135388,0.769982573809021,
12.5042014951932));
#432281=CARTESIAN_POINT('Ctrl Pts',(-2.63841375712275,0.775795764700635,
12.4980716682127));
#432282=CARTESIAN_POINT('Ctrl Pts',(-2.63649352581143,0.78231023144297,
12.4907355092743));
#432283=CARTESIAN_POINT('Ctrl Pts',(-2.62989146561741,0.771707596413527,
12.5218047446509));
#432284=CARTESIAN_POINT('Ctrl Pts',(-2.63683259606657,0.78126477063104,
12.5216906929434));
#432285=CARTESIAN_POINT('Ctrl Pts',(-2.63333344319635,0.792495384306188,
12.5161988840776));
#432286=CARTESIAN_POINT('Ctrl Pts',(-2.62579078184538,0.768536480046287,
12.5369868989719));
#432287=CARTESIAN_POINT('Ctrl Pts',(-2.63791775902611,0.77791421729887,
12.5369868989719));
#432288=CARTESIAN_POINT('Ctrl Pts',(-2.63331991434154,0.792538353368299,
12.5369868989719));
#432289=CARTESIAN_POINT('Origin',(-4.97175483587123E-31,-3.80155074318093E-31,
12.5));
#432290=CARTESIAN_POINT('Origin',(-2.63242388933657,0.521089942649588,12.5));
#432291=CARTESIAN_POINT('',(-2.63242388933657,0.521089942649588,12.5893111709658));
#432292=CARTESIAN_POINT('',(-2.63242388933657,0.521089942649588,13.8235269408515));
#432293=CARTESIAN_POINT('',(-2.63242388933657,0.521089942649588,12.5));
#432294=CARTESIAN_POINT('',(-2.66237308910439,0.540642899778083,13.7902182540695));
#432295=CARTESIAN_POINT('',(-2.63242388933657,0.521089942649588,13.8235269408515));
#432296=CARTESIAN_POINT('',(-2.67972872331797,0.551973886059748,13.7435492065112));
#432297=CARTESIAN_POINT('Origin',(-2.62262909424378,0.514694818196436,13.7445212918693));
#432298=CARTESIAN_POINT('',(-2.67972872331797,0.551973886059748,12.5369868989719));
#432299=CARTESIAN_POINT('',(-2.67972872331797,0.551973886059748,12.5));
#432300=CARTESIAN_POINT('Ctrl Pts',(-2.67972872331797,0.551973886059748,
12.5369868989719));
#432301=CARTESIAN_POINT('Ctrl Pts',(-2.66397194574709,0.541686746546334,
12.5544431401645));
#432302=CARTESIAN_POINT('Ctrl Pts',(-2.64820389851011,0.531392249397325,
12.5718848856037));
#432303=CARTESIAN_POINT('Ctrl Pts',(-2.63242388933657,0.521089942649588,
12.5893111709658));
#432304=CARTESIAN_POINT('Origin',(-2.91290005437388,0.401048100265817,12.5));
#432305=CARTESIAN_POINT('',(-2.69924879928632,0.446852460011815,13.7435492065112));
#432306=CARTESIAN_POINT('',(-2.67898229736197,0.451197363787623,13.7902182540695));
#432307=CARTESIAN_POINT('Origin',(-2.62572543305949,0.462615019960319,13.7418732680442));
#432308=CARTESIAN_POINT('',(-2.64401005104369,0.458695009195004,13.8235269408515));
#432309=CARTESIAN_POINT('',(-2.67898229736197,0.451197363787623,13.7902182540695));
#432310=CARTESIAN_POINT('',(-2.64401005104369,0.458695009195004,12.5893111709658));
#432311=CARTESIAN_POINT('',(-2.64401005104369,0.458695009195004,12.5));
#432312=CARTESIAN_POINT('',(-2.69924879928632,0.446852460011815,12.5369868989719));
#432313=CARTESIAN_POINT('Ctrl Pts',(-2.64401005104369,0.458695009195004,
12.5893111709658));
#432314=CARTESIAN_POINT('Ctrl Pts',(-2.66243666584474,0.454744555953329,
12.5718848856037));
#432315=CARTESIAN_POINT('Ctrl Pts',(-2.68084931246654,0.450797097327846,
12.5544431401645));
#432316=CARTESIAN_POINT('Ctrl Pts',(-2.69924879928632,0.446852460011815,
12.5369868989719));
#432317=CARTESIAN_POINT('',(-2.69924879928632,0.446852460011815,12.5));
#432318=CARTESIAN_POINT('Origin',(-2.65121591465983,0.492306259611278,12.5));
#432319=CARTESIAN_POINT('',(-2.61723291503602,0.487134614926502,13.8587068136939));
#432320=CARTESIAN_POINT('Ctrl Pts',(-2.64401005104216,0.458695009188572,
13.8235269408542));
#432321=CARTESIAN_POINT('Ctrl Pts',(-2.64229668557668,0.459062334941593,
13.8262006681044));
#432322=CARTESIAN_POINT('Ctrl Pts',(-2.64057972648819,0.459608118342289,
13.8288634856214));
#432323=CARTESIAN_POINT('Ctrl Pts',(-2.63886090087308,0.460319137318725,
13.8314912288862));
#432324=CARTESIAN_POINT('Ctrl Pts',(-2.63708896895254,0.461052124545224,
13.8342001611531));
#432325=CARTESIAN_POINT('Ctrl Pts',(-2.63531289527057,0.461961070621593,
13.8368750301949));
#432326=CARTESIAN_POINT('Ctrl Pts',(-2.63353194277321,0.463076614130332,
13.8394886372969));
#432327=CARTESIAN_POINT('Ctrl Pts',(-2.63339439549185,0.463162770261442,
13.8396904925131));
#432328=CARTESIAN_POINT('Ctrl Pts',(-2.63325682745648,0.463250179229894,
13.8398919674349));
#432329=CARTESIAN_POINT('Ctrl Pts',(-2.63311924355486,0.463338865330674,
13.8400930404591));
#432330=CARTESIAN_POINT('Ctrl Pts',(-2.63097559380562,0.464720654445926,
13.8432258934518));
#432331=CARTESIAN_POINT('Ctrl Pts',(-2.62883842087517,0.466404480074774,
13.8462331177034));
#432332=CARTESIAN_POINT('Ctrl Pts',(-2.62683712799038,0.468411198488729,
13.8489036603661));
#432333=CARTESIAN_POINT('Ctrl Pts',(-2.62618228166826,0.469067820107131,
13.8497774930041));
#432334=CARTESIAN_POINT('Ctrl Pts',(-2.62554222827764,0.469758961651016,
13.85061494757));
#432335=CARTESIAN_POINT('Ctrl Pts',(-2.62492219736293,0.470485195353339,
13.8514076489583));
#432336=CARTESIAN_POINT('Ctrl Pts',(-2.62361074255648,0.472021284372325,
13.8530843267192));
#432337=CARTESIAN_POINT('Ctrl Pts',(-2.62226229521561,0.473867174909691,
13.8546805203176));
#432338=CARTESIAN_POINT('Ctrl Pts',(-2.62106529722913,0.475996218981072,
13.8559412814273));
#432339=CARTESIAN_POINT('Ctrl Pts',(-2.62090510007897,0.476281154124366,
13.8561100121513));
#432340=CARTESIAN_POINT('Ctrl Pts',(-2.62074758894407,0.476571088798741,
13.8562727473908));
#432341=CARTESIAN_POINT('Ctrl Pts',(-2.62059318056477,0.47686589182133,
13.8564289040185));
#432342=CARTESIAN_POINT('Ctrl Pts',(-2.61989294032619,0.478202820165509,
13.8571370725437));
#432343=CARTESIAN_POINT('Ctrl Pts',(-2.61924622003635,0.479664427228443,
13.8577210840553));
#432344=CARTESIAN_POINT('Ctrl Pts',(-2.61870499601779,0.481205775232603,
13.8581177131616));
#432345=CARTESIAN_POINT('Ctrl Pts',(-2.6185525687058,0.481639871882158,
13.8582294175695));
#432346=CARTESIAN_POINT('Ctrl Pts',(-2.61840835633688,0.48208020288325,
13.8583265086086));
#432347=CARTESIAN_POINT('Ctrl Pts',(-2.61827312910673,0.482525563282829,
13.8584082369006));
#432348=CARTESIAN_POINT('Ctrl Pts',(-2.61807884383963,0.483165426748914,
13.8585256585398));
#432349=CARTESIAN_POINT('Ctrl Pts',(-2.61790099965483,0.483823720844838,
13.8586122832068));
#432350=CARTESIAN_POINT('Ctrl Pts',(-2.61774497878506,0.484483550955413,
13.8586682984299));
#432351=CARTESIAN_POINT('Ctrl Pts',(-2.6176201775551,0.485011349637018,
13.8587131050557));
#432352=CARTESIAN_POINT('Ctrl Pts',(-2.61750773316542,0.485545906707866,
13.8587357943552));
#432353=CARTESIAN_POINT('Ctrl Pts',(-2.61740812785469,0.486087389937754,
13.8587355499465));
#432354=CARTESIAN_POINT('Ctrl Pts',(-2.61734375056764,0.486437363458876,
13.8587353919793));
#432355=CARTESIAN_POINT('Ctrl Pts',(-2.61728539474004,0.486786438712572,
13.8587257282814));
#432356=CARTESIAN_POINT('Ctrl Pts',(-2.61723291503602,0.487134614926502,
13.8587068136939));
#432357=CARTESIAN_POINT('Ctrl Pts',(-2.61723291503602,0.487134614926502,
13.8587068136939));
#432358=CARTESIAN_POINT('Ctrl Pts',(-2.61706031215051,0.488279747512706,
13.8586446046466));
#432359=CARTESIAN_POINT('Ctrl Pts',(-2.61695119376834,0.489415167789454,
13.858482427929));
#432360=CARTESIAN_POINT('Ctrl Pts',(-2.61690109098488,0.490540753901813,
13.8582284286032));
#432361=CARTESIAN_POINT('Ctrl Pts',(-2.61684969135724,0.491695474319623,
13.8579678548414));
#432362=CARTESIAN_POINT('Ctrl Pts',(-2.61686180652745,0.492842733674225,
13.857615680862));
#432363=CARTESIAN_POINT('Ctrl Pts',(-2.61692726973463,0.493937404435696,
13.8571944833187));
#432364=CARTESIAN_POINT('Ctrl Pts',(-2.6170906398632,0.496669267274696,
13.8561433417727));
#432365=CARTESIAN_POINT('Ctrl Pts',(-2.61758911828645,0.499201680998632,
13.8546163505474));
#432366=CARTESIAN_POINT('Ctrl Pts',(-2.61824353044091,0.501431425733235,
13.8528973491086));
#432367=CARTESIAN_POINT('Ctrl Pts',(-2.61836308188658,0.501838767199425,
13.8525833129072));
#432368=CARTESIAN_POINT('Ctrl Pts',(-2.6184877355625,0.502236105361634,
13.8522628768812));
#432369=CARTESIAN_POINT('Ctrl Pts',(-2.61861629108584,0.502622953433333,
13.851937733538));
#432370=CARTESIAN_POINT('Ctrl Pts',(-2.61940136183063,0.504985380934481,
13.8499521282529));
#432371=CARTESIAN_POINT('Ctrl Pts',(-2.6204138385287,0.507190088317489,
13.847639871647));
#432372=CARTESIAN_POINT('Ctrl Pts',(-2.62152749917535,0.509154732977702,
13.8452109780794));
#432373=CARTESIAN_POINT('Ctrl Pts',(-2.62202855815191,0.510038667276455,
13.8441181685877));
#432374=CARTESIAN_POINT('Ctrl Pts',(-2.62254963617414,0.510874554073736,
13.8430021611332));
#432375=CARTESIAN_POINT('Ctrl Pts',(-2.62307798757882,0.511657957505856,
13.8418824960098));
#432376=CARTESIAN_POINT('Ctrl Pts',(-2.62432306115589,0.513504067698561,
13.8392439765549));
#432377=CARTESIAN_POINT('Ctrl Pts',(-2.62566490940633,0.515149093362416,
13.8364981347964));
#432378=CARTESIAN_POINT('Ctrl Pts',(-2.62708056355634,0.516619015251649,
13.8336931113419));
#432379=CARTESIAN_POINT('Ctrl Pts',(-2.62845932079609,0.518050625823091,
13.8309611966328));
#432380=CARTESIAN_POINT('Ctrl Pts',(-2.6299098749629,0.519317184367395,
13.8281701127186));
#432381=CARTESIAN_POINT('Ctrl Pts',(-2.63142745582177,0.520407000643875,
13.8253580685121));
#432382=CARTESIAN_POINT('Ctrl Pts',(-2.63175646898981,0.520643273988785,
13.8247484142933));
#432383=CARTESIAN_POINT('Ctrl Pts',(-2.6320886380345,0.520871066873691,
13.8241378483365));
#432384=CARTESIAN_POINT('Ctrl Pts',(-2.63242388933657,0.521089942649588,
13.8235269408515));
#432385=CARTESIAN_POINT('',(-2.61744190074819,0.485910236786106,12.5969504640361));
#432386=CARTESIAN_POINT('Origin',(-2.65124840825318,0.492312492524074,12.584524458991));
#432387=CARTESIAN_POINT('Origin',(-2.65124840825318,0.492312492524074,12.584524458991));
#432388=CARTESIAN_POINT('Ctrl Pts',(-2.64401005104369,0.458695009195004,
12.5893111709658));
#432389=CARTESIAN_POINT('Ctrl Pts',(-2.63292791152546,0.461070891822232,
12.5770542771492));
#432390=CARTESIAN_POINT('Ctrl Pts',(-2.63331499706307,0.477431021395115,
12.5737548217797));
#432391=CARTESIAN_POINT('Ctrl Pts',(-2.66824297089342,0.453499751259175,
12.5663937883685));
#432392=CARTESIAN_POINT('Ctrl Pts',(-2.6571466945672,0.455878664654639,
12.5540940315303));
#432393=CARTESIAN_POINT('Ctrl Pts',(-2.65753818989281,0.472289414994709,
12.5508374392248));
#432394=CARTESIAN_POINT('Ctrl Pts',(-2.69245144002421,0.448309735274893,
12.5434499600945));
#432395=CARTESIAN_POINT('Ctrl Pts',(-2.68131908575214,0.450696383364917,
12.5311293540533));
#432396=CARTESIAN_POINT('Ctrl Pts',(-2.68173747116724,0.467151677899152,
12.5278936106989));
#432397=CARTESIAN_POINT('Ctrl Pts',(-2.71663737369418,0.443124550632948,
12.5204817579905));
#432398=CARTESIAN_POINT('Ctrl Pts',(-2.70544992187638,0.445523011000026,
12.5081597038247));
#432399=CARTESIAN_POINT('Ctrl Pts',(-2.70591469650934,0.462017495818755,
12.5049254088044));
#432400=CARTESIAN_POINT('Ctrl Pts',(-2.69924879928632,0.446852460011815,
12.5369868989719));
#432401=CARTESIAN_POINT('Ctrl Pts',(-2.70015960777715,0.446657193363936,
12.5342545179733));
#432402=CARTESIAN_POINT('Ctrl Pts',(-2.7010549917397,0.446592814229371,
12.5314872231885));
#432403=CARTESIAN_POINT('Ctrl Pts',(-2.70188852178364,0.446718706151211,
12.5287124745063));
#432404=CARTESIAN_POINT('Ctrl Pts',(-2.70264024055,0.446832241735042,12.5262100684184));
#432405=CARTESIAN_POINT('Ctrl Pts',(-2.70334074612475,0.447101389050586,
12.5237004536639));
#432406=CARTESIAN_POINT('Ctrl Pts',(-2.70397829100729,0.447592649769733,
12.5212220730815));
#432407=CARTESIAN_POINT('Ctrl Pts',(-2.7044663867669,0.447968752347681,
12.5193246583486));
#432408=CARTESIAN_POINT('Ctrl Pts',(-2.70492302594465,0.448480038260301,
12.517417831369));
#432409=CARTESIAN_POINT('Ctrl Pts',(-2.70528989456734,0.449204311770227,
12.5155812248348));
#432410=CARTESIAN_POINT('Ctrl Pts',(-2.70544618257253,0.449512856178445,
12.5147988205793));
#432411=CARTESIAN_POINT('Ctrl Pts',(-2.70558658474796,0.449860241736385,
12.5140295443047));
#432412=CARTESIAN_POINT('Ctrl Pts',(-2.70570870206013,0.450252759398287,
12.5132817086137));
#432413=CARTESIAN_POINT('Ctrl Pts',(-2.70589351009244,0.450846781780985,
12.5121499604604));
#432414=CARTESIAN_POINT('Ctrl Pts',(-2.70603360275183,0.451559121000489,
12.5110494206568));
#432415=CARTESIAN_POINT('Ctrl Pts',(-2.70609669465267,0.452408339185497,
12.5100666561695));
#432416=CARTESIAN_POINT('Ctrl Pts',(-2.70613292187684,0.452895958311753,
12.5095023550641));
#432417=CARTESIAN_POINT('Ctrl Pts',(-2.70614352934085,0.453434389196007,
12.5089719619137));
#432418=CARTESIAN_POINT('Ctrl Pts',(-2.70612193248006,0.454013665349975,
12.5085043804652));
#432419=CARTESIAN_POINT('Ctrl Pts',(-2.70609032828747,0.45486136054528,
12.5078201359221));
#432420=CARTESIAN_POINT('Ctrl Pts',(-2.70598763652439,0.455821064882285,
12.5072563000949));
#432421=CARTESIAN_POINT('Ctrl Pts',(-2.70581240023266,0.45682682381386,
12.5068768744332));
#432422=CARTESIAN_POINT('Ctrl Pts',(-2.70568604280301,0.457552045240207,
12.5066032824114));
#432423=CARTESIAN_POINT('Ctrl Pts',(-2.70551980580727,0.458313963662298,
12.5064197834844));
#432424=CARTESIAN_POINT('Ctrl Pts',(-2.70532549779722,0.459070582585212,
12.5063282718343));
#432425=CARTESIAN_POINT('Ctrl Pts',(-2.70504186825879,0.460175011969369,
12.5061946931565));
#432426=CARTESIAN_POINT('Ctrl Pts',(-2.70469339448344,0.461292019806346,
12.5062515701262));
#432427=CARTESIAN_POINT('Ctrl Pts',(-2.70431646617486,0.46235688818737,
12.5064436508398));
#432428=CARTESIAN_POINT('',(-2.63331499706307,0.477431021395115,12.5737548217797));
#432429=CARTESIAN_POINT('Origin',(-2.64862180375802,0.480206209461419,12.5893111709658));
#432430=CARTESIAN_POINT('Ctrl Pts',(-2.70431646617486,0.46235688818737,
12.5064436508398));
#432431=CARTESIAN_POINT('Ctrl Pts',(-2.69380650386284,0.464588721503536,
12.5164271754438));
#432432=CARTESIAN_POINT('Ctrl Pts',(-2.68329233200359,0.466821235139596,
12.5264061185523));
#432433=CARTESIAN_POINT('Ctrl Pts',(-2.67277380253701,0.469054453981689,
12.536380305637));
#432434=CARTESIAN_POINT('Ctrl Pts',(-2.65962777409142,0.471845524588721,
12.5488460165097));
#432435=CARTESIAN_POINT('Ctrl Pts',(-2.64647493520526,0.474637697523352,
12.5613043021964));
#432436=CARTESIAN_POINT('Ctrl Pts',(-2.63331499706307,0.477431021395115,
12.5737548217797));
#432437=CARTESIAN_POINT('Ctrl Pts',(-2.63242388933657,0.521089942649588,
12.5893111709658));
#432438=CARTESIAN_POINT('Ctrl Pts',(-2.62293347207068,0.514893926616768,
12.5770542771492));
#432439=CARTESIAN_POINT('Ctrl Pts',(-2.62916808382621,0.499763384950565,
12.5737548217797));
#432440=CARTESIAN_POINT('Ctrl Pts',(-2.62356941257079,0.515309113581068,
12.5928319619712));
#432441=CARTESIAN_POINT('Ctrl Pts',(-2.61897219921629,0.508417158434331,
12.5821634970842));
#432442=CARTESIAN_POINT('Ctrl Pts',(-2.62593745225667,0.497665472409182,
12.5773203894503));
#432443=CARTESIAN_POINT('Ctrl Pts',(-2.61464112153564,0.501136262120216,
12.5969440695591));
#432444=CARTESIAN_POINT('Ctrl Pts',(-2.61535703541883,0.497180758376851,
12.5878292599214));
#432445=CARTESIAN_POINT('Ctrl Pts',(-2.62275695826244,0.492612888411841,
12.5813877129824));
#432446=CARTESIAN_POINT('Ctrl Pts',(-2.62017418048675,0.471043729754444,
12.596957478804));
#432447=CARTESIAN_POINT('Ctrl Pts',(-2.61946363627608,0.474970015540476,
12.5878468778671));
#432448=CARTESIAN_POINT('Ctrl Pts',(-2.62474318353181,0.481843432646413,
12.5814011370086));
#432449=CARTESIAN_POINT('Ctrl Pts',(-2.63365549826659,0.460914905634202,
12.5928371701607));
#432450=CARTESIAN_POINT('Ctrl Pts',(-2.6268988684393,0.465698525506302,
12.5821692192952));
#432451=CARTESIAN_POINT('Ctrl Pts',(-2.62953446995646,0.478231578869737,
12.5773318885715));
#432452=CARTESIAN_POINT('Ctrl Pts',(-2.64401005104367,0.45869500919495,
12.5893111709658));
#432453=CARTESIAN_POINT('Ctrl Pts',(-2.63292791152545,0.461070891822178,
12.5770542771492));
#432454=CARTESIAN_POINT('Ctrl Pts',(-2.63331499706305,0.477431021395061,
12.5737548217797));
#432455=CARTESIAN_POINT('',(-2.62916808382621,0.499763384950565,12.5737548217797));
#432456=CARTESIAN_POINT('Origin',(-2.64445078554346,0.502668385505069,12.5893111709658));
#432457=CARTESIAN_POINT('Ctrl Pts',(-2.63331499706305,0.477431021395061,
12.5737548217797));
#432458=CARTESIAN_POINT('Ctrl Pts',(-2.63232877521056,0.477609027262011,
12.5746934679442));
#432459=CARTESIAN_POINT('Ctrl Pts',(-2.63126999273989,0.477986274022145,
12.5756680099006));
#432460=CARTESIAN_POINT('Ctrl Pts',(-2.63025799136356,0.478516704868041,
12.5765688348656));
#432461=CARTESIAN_POINT('Ctrl Pts',(-2.62999007520239,0.47865713056243,
12.5768073183026));
#432462=CARTESIAN_POINT('Ctrl Pts',(-2.629725377434,0.478808042528843,12.5770407398754));
#432463=CARTESIAN_POINT('Ctrl Pts',(-2.62946584690868,0.478968089551087,
12.5772674179684));
#432464=CARTESIAN_POINT('Ctrl Pts',(-2.62840080381277,0.47962487925183,
12.5781976435658));
#432465=CARTESIAN_POINT('Ctrl Pts',(-2.62736820911834,0.48048241390408,
12.5790594849312));
#432466=CARTESIAN_POINT('Ctrl Pts',(-2.6264686363198,0.481519940532074,
12.5797571720116));
#432467=CARTESIAN_POINT('Ctrl Pts',(-2.62588253229579,0.482195926436344,
12.580211740231));
#432468=CARTESIAN_POINT('Ctrl Pts',(-2.62534044437038,0.482991336809329,
12.5806009430798));
#432469=CARTESIAN_POINT('Ctrl Pts',(-2.62489517322748,0.483860155705081,
12.5808812374708));
#432470=CARTESIAN_POINT('Ctrl Pts',(-2.62451253759856,0.484606759364201,
12.5811221033394));
#432471=CARTESIAN_POINT('Ctrl Pts',(-2.62419366442237,0.485422908646014,
12.581287365893));
#432472=CARTESIAN_POINT('Ctrl Pts',(-2.62396431767964,0.486265573084002,
12.581359338449));
#432473=CARTESIAN_POINT('Ctrl Pts',(-2.62393244321822,0.486382686040527,
12.5813693411482));
#432474=CARTESIAN_POINT('Ctrl Pts',(-2.62390223826965,0.486500315574401,
12.5813775999465));
#432475=CARTESIAN_POINT('Ctrl Pts',(-2.62387371091115,0.486618351795548,
12.5813841266931));
#432476=CARTESIAN_POINT('Ctrl Pts',(-2.62382531079715,0.48681861452091,
12.5813952001081));
#432477=CARTESIAN_POINT('Ctrl Pts',(-2.6237820073354,0.487021532204495,
12.5814007534795));
#432478=CARTESIAN_POINT('Ctrl Pts',(-2.62374401225294,0.487227057627631,
12.5814005856065));
#432479=CARTESIAN_POINT('Ctrl Pts',(-2.62357008562053,0.488167872659516,
12.5813998171494));
#432480=CARTESIAN_POINT('Ctrl Pts',(-2.62351907856417,0.48909826713547,
12.58127954464));
#432481=CARTESIAN_POINT('Ctrl Pts',(-2.6235617356765,0.490011339135859,
12.5810700125799));
#432482=CARTESIAN_POINT('Ctrl Pts',(-2.6236132606113,0.491114226150758,
12.5808169217085));
#432483=CARTESIAN_POINT('Ctrl Pts',(-2.62381816296463,0.492191158546528,
12.5804173076348));
#432484=CARTESIAN_POINT('Ctrl Pts',(-2.62413290203032,0.493152623412337,
12.5799304713245));
#432485=CARTESIAN_POINT('Ctrl Pts',(-2.62452296288574,0.49434418127374,
12.5793271277669));
#432486=CARTESIAN_POINT('Ctrl Pts',(-2.62507531595854,0.495442324657529,
12.5785808224116));
#432487=CARTESIAN_POINT('Ctrl Pts',(-2.62573834403119,0.496415016611789,
12.5777485681082));
#432488=CARTESIAN_POINT('Ctrl Pts',(-2.62672632849958,0.497864434189996,
12.576508418016));
#432489=CARTESIAN_POINT('Ctrl Pts',(-2.62794606111148,0.499026962411696,
12.5750928681475));
#432490=CARTESIAN_POINT('Ctrl Pts',(-2.62916808382621,0.499763384950565,
12.5737548217797));
#432491=CARTESIAN_POINT('Ctrl Pts',(-2.62916808382621,0.499763384950565,
12.5737548217797));
#432492=CARTESIAN_POINT('Ctrl Pts',(-2.62293347207068,0.514893926616768,
12.5770542771492));
#432493=CARTESIAN_POINT('Ctrl Pts',(-2.63242388933657,0.521089942649588,
12.5893111709658));
#432494=CARTESIAN_POINT('Ctrl Pts',(-2.64992750452856,0.513256398189767,
12.5508408821982));
#432495=CARTESIAN_POINT('Ctrl Pts',(-2.64367060449799,0.5284325942427,12.55409748406));
#432496=CARTESIAN_POINT('Ctrl Pts',(-2.65317312910571,0.534636514805103,
12.5663972313419));
#432497=CARTESIAN_POINT('Ctrl Pts',(-2.67066600309183,0.526737219423367,
12.52790050457));
#432498=CARTESIAN_POINT('Ctrl Pts',(-2.6643680203809,0.54194533209766,12.5311362602938));
#432499=CARTESIAN_POINT('Ctrl Pts',(-2.67390143630145,0.548169420695304,
12.5434568539655));
#432500=CARTESIAN_POINT('Ctrl Pts',(-2.69138519788797,0.540206807737659,
12.5049357605811));
#432501=CARTESIAN_POINT('Ctrl Pts',(-2.68502985996609,0.555434843227771,
12.5081700652078));
#432502=CARTESIAN_POINT('Ctrl Pts',(-2.69461045036723,0.56168973066488,
12.5204921097672));
#432503=CARTESIAN_POINT('Ctrl Pts',(-2.69002469347584,0.539322343100433,
12.5064436508395));
#432504=CARTESIAN_POINT('Ctrl Pts',(-2.68999175912047,0.540542082055627,
12.5062361689309));
#432505=CARTESIAN_POINT('Ctrl Pts',(-2.68990549770766,0.541809106360485,
12.5061871075061));
#432506=CARTESIAN_POINT('Ctrl Pts',(-2.68975320661061,0.543028870297842,
12.5063648335164));
#432507=CARTESIAN_POINT('Ctrl Pts',(-2.68968402660063,0.54358296231635,
12.5064455676329));
#432508=CARTESIAN_POINT('Ctrl Pts',(-2.68960003758825,0.544135003120524,
12.506574497099));
#432509=CARTESIAN_POINT('Ctrl Pts',(-2.68950380177739,0.5446611647812,12.5067492519495));
#432510=CARTESIAN_POINT('Ctrl Pts',(-2.68931041217985,0.545718507062495,
12.5071004286051));
#432511=CARTESIAN_POINT('Ctrl Pts',(-2.68905966175249,0.546710072287434,
12.5076537929613));
#432512=CARTESIAN_POINT('Ctrl Pts',(-2.68877954041675,0.547563757172874,
12.5083435010505));
#432513=CARTESIAN_POINT('Ctrl Pts',(-2.68876190510465,0.547617501738062,
12.5083869222964));
#432514=CARTESIAN_POINT('Ctrl Pts',(-2.68874414011912,0.54767070196071,
12.5084308732337));
#432515=CARTESIAN_POINT('Ctrl Pts',(-2.68872624710657,0.547723341111141,
12.5084753333615));
#432516=CARTESIAN_POINT('Ctrl Pts',(-2.68858272152925,0.548145576574968,
12.5088319622689));
#432517=CARTESIAN_POINT('Ctrl Pts',(-2.68842926613241,0.548540699037134,
12.509227847131));
#432518=CARTESIAN_POINT('Ctrl Pts',(-2.68827305406093,0.54889797314926,
12.5096423454524));
#432519=CARTESIAN_POINT('Ctrl Pts',(-2.68778355456546,0.550017512093765,
12.5109411997424));
#432520=CARTESIAN_POINT('Ctrl Pts',(-2.68724573827064,0.550838143388983,
12.5124831113042));
#432521=CARTESIAN_POINT('Ctrl Pts',(-2.68671124461061,0.551439171676893,
12.5140723025008));
#432522=CARTESIAN_POINT('Ctrl Pts',(-2.68666116196925,0.551495488685758,
12.5142212114565));
#432523=CARTESIAN_POINT('Ctrl Pts',(-2.68661111490232,0.551549906510581,
12.5143705582413));
#432524=CARTESIAN_POINT('Ctrl Pts',(-2.68656115105941,0.551602506571629,
12.5145201959299));
#432525=CARTESIAN_POINT('Ctrl Pts',(-2.68591929110873,0.552278232669096,
12.5164425148273));
#432526=CARTESIAN_POINT('Ctrl Pts',(-2.68527695902345,0.552684517386472,
12.5184635205941));
#432527=CARTESIAN_POINT('Ctrl Pts',(-2.68463688404735,0.55291153017412,
12.5205025929158));
#432528=CARTESIAN_POINT('Ctrl Pts',(-2.68426561519101,0.553043206588901,
12.5216853356836));
#432529=CARTESIAN_POINT('Ctrl Pts',(-2.68389593802785,0.553114785563373,
12.5228750347131));
#432530=CARTESIAN_POINT('Ctrl Pts',(-2.68353428572838,0.553143341873244,
12.5240609649613));
#432531=CARTESIAN_POINT('Ctrl Pts',(-2.68264662956129,0.553213431803828,
12.5269717671326));
#432532=CARTESIAN_POINT('Ctrl Pts',(-2.68178151709282,0.553015949133506,
12.5299036066169));
#432533=CARTESIAN_POINT('Ctrl Pts',(-2.68093349742623,0.552637379759122,
12.5328133004019));
#432534=CARTESIAN_POINT('Ctrl Pts',(-2.68052639860756,0.552455644415982,
12.5342101228451));
#432535=CARTESIAN_POINT('Ctrl Pts',(-2.68012396050527,0.552231924768891,
12.5356023438238));
#432536=CARTESIAN_POINT('Ctrl Pts',(-2.67972872331797,0.551973886059748,
12.5369868989719));
#432537=CARTESIAN_POINT('Origin',(-13.3497998213102,7.52447901476919,-1.24101070188029));
#432538=CARTESIAN_POINT('Ctrl Pts',(-2.69920792530587,0.446861182319613,
12.5369868989719));
#432539=CARTESIAN_POINT('Ctrl Pts',(-2.71421215066287,0.443674251959329,
12.5369868989719));
#432540=CARTESIAN_POINT('Ctrl Pts',(-2.71641003076791,0.428493585744408,
12.5369868989719));
#432541=CARTESIAN_POINT('Ctrl Pts',(-2.70427992653162,0.445783810450665,
12.5218025310015));
#432542=CARTESIAN_POINT('Ctrl Pts',(-2.71468600954219,0.440182980147849,
12.5216901060417));
#432543=CARTESIAN_POINT('Ctrl Pts',(-2.71640334722253,0.428539863809084,
12.5161920673678));
#432544=CARTESIAN_POINT('Ctrl Pts',(-2.70873673120405,0.449842500301691,
12.5042015548895));
#432545=CARTESIAN_POINT('Ctrl Pts',(-2.71373584230073,0.44579450903935,
12.4980677368514));
#432546=CARTESIAN_POINT('Ctrl Pts',(-2.7148315199549,0.439087030362391,
12.4907278922777));
#432547=CARTESIAN_POINT('Ctrl Pts',(-2.70429675115723,0.462353517522103,
12.506463626192));
#432548=CARTESIAN_POINT('Ctrl Pts',(-2.71074591258632,0.463456130417869,
12.4999376786891));
#432549=CARTESIAN_POINT('Ctrl Pts',(-2.71066714545653,0.463442663604545,
12.4906970594712));
#432550=CARTESIAN_POINT('Origin',(-2.69463704657199,0.425341259745399,12.5369868989719));
#432551=CARTESIAN_POINT('Origin',(-2.69463704657199,0.425341259745399,14.));
#432552=CARTESIAN_POINT('Origin',(-2.69463704657199,0.4253412597454,13.7435492065112));
#432553=CARTESIAN_POINT('Ctrl Pts',(-2.67503881381097,0.452042773314378,
13.793642941384));
#432554=CARTESIAN_POINT('Ctrl Pts',(-2.68561657471053,0.449802864084712,
13.8071662555867));
#432555=CARTESIAN_POINT('Ctrl Pts',(-2.68457645852668,0.432804701185187,
13.8103758687955));
#432556=CARTESIAN_POINT('Ctrl Pts',(-2.69129064578038,0.448558571417166,
13.7804579775006));
#432557=CARTESIAN_POINT('Ctrl Pts',(-2.70434054585607,0.44578480507073,
13.7901904343351));
#432558=CARTESIAN_POINT('Ctrl Pts',(-2.70593540090513,0.43010959019064,
13.7927914348262));
#432559=CARTESIAN_POINT('Ctrl Pts',(-2.70085871087808,0.446507290597821,
13.7597120340895));
#432560=CARTESIAN_POINT('Ctrl Pts',(-2.71595992897568,0.443291656610529,
13.7635825532445));
#432561=CARTESIAN_POINT('Ctrl Pts',(-2.71852754465409,0.428494925016269,
13.7651073818884));
#432562=CARTESIAN_POINT('Ctrl Pts',(-2.69898506464799,0.446908978350449,
13.7381884353898));
#432563=CARTESIAN_POINT('Ctrl Pts',(-2.71373299779985,0.44376949139001,
13.7368803041982));
#432564=CARTESIAN_POINT('Ctrl Pts',(-2.71606156587467,0.428810634219766,
13.7363986145813));
#432565=CARTESIAN_POINT('Origin',(-2.67437054464763,0.429686163521208,13.7902182540695));
#432566=CARTESIAN_POINT('Ctrl Pts',(-2.64400620214131,0.458695833579019,
13.8235227101244));
#432567=CARTESIAN_POINT('Ctrl Pts',(-2.65524875977548,0.456290093326659,
13.8358800583119));
#432568=CARTESIAN_POINT('Ctrl Pts',(-2.65474553983446,0.439725890395412,
13.8390832900376));
#432569=CARTESIAN_POINT('Ctrl Pts',(-2.6556687725148,0.456195513283816,
13.8124254819053));
#432570=CARTESIAN_POINT('Ctrl Pts',(-2.66693316297831,0.453785100845986,
13.8247886449158));
#432571=CARTESIAN_POINT('Ctrl Pts',(-2.66641227077076,0.437200485914952,
13.8279860620657));
#432572=CARTESIAN_POINT('Ctrl Pts',(-2.66732611610358,0.453696313550856,
13.8013225099954));
#432573=CARTESIAN_POINT('Ctrl Pts',(-2.67860702483252,0.451282368215402,
13.8136962257787));
#432574=CARTESIAN_POINT('Ctrl Pts',(-2.67807365792967,0.434676515493284,
13.8168830918626));
#432575=CARTESIAN_POINT('Ctrl Pts',(-2.67897843627399,0.45119819078075,
13.7902140179785));
#432576=CARTESIAN_POINT('Ctrl Pts',(-2.69027089604951,0.448781777371834,
13.802602731458));
#432577=CARTESIAN_POINT('Ctrl Pts',(-2.68972991167053,0.43215392458132,
13.8057746032558));
#432578=CARTESIAN_POINT('Origin',(-2.63939829832935,0.437183808928588,13.8235269408515));
#432579=CARTESIAN_POINT('Ctrl Pts',(-2.63242388933657,0.521089942649588,
13.8235269408515));
#432580=CARTESIAN_POINT('Ctrl Pts',(-2.6423108072789,0.52754482238454,13.8362179249168));
#432581=CARTESIAN_POINT('Ctrl Pts',(-2.63541047324264,0.54316687072159,
13.8391868794938));
#432582=CARTESIAN_POINT('Ctrl Pts',(-2.62337778977126,0.515184008656295,
13.8400110824519));
#432583=CARTESIAN_POINT('Ctrl Pts',(-2.62943449763647,0.523223794268897,
13.8494522556836));
#432584=CARTESIAN_POINT('Ctrl Pts',(-2.62058457010541,0.533353289326912,
13.85569149686));
#432585=CARTESIAN_POINT('Ctrl Pts',(-2.61457773780764,0.501474274469136,
13.8586819406588));
#432586=CARTESIAN_POINT('Ctrl Pts',(-2.61379653394518,0.505757470023888,
13.868010383617));
#432587=CARTESIAN_POINT('Ctrl Pts',(-2.6060991751906,0.510515992378134,
13.8744918421245));
#432588=CARTESIAN_POINT('Ctrl Pts',(-2.62023852895725,0.470700471624714,
13.8587686893867));
#432589=CARTESIAN_POINT('Ctrl Pts',(-2.62101272471808,0.466455386367178,
13.8680909899357));
#432590=CARTESIAN_POINT('Ctrl Pts',(-2.6155252605559,0.459287113313332,
13.8745789365162));
#432591=CARTESIAN_POINT('Ctrl Pts',(-2.63342956069134,0.460963344032332,
13.8400379222776));
#432592=CARTESIAN_POINT('Ctrl Pts',(-2.64196284407893,0.455629179755203,
13.8494748685453));
#432593=CARTESIAN_POINT('Ctrl Pts',(-2.63734258833735,0.443003240497187,
13.8557104837033));
#432594=CARTESIAN_POINT('Ctrl Pts',(-2.64401005104216,0.458695009188572,
13.8235269408542));
#432595=CARTESIAN_POINT('Ctrl Pts',(-2.65555519189024,0.456219864427462,
13.8362179249195));
#432596=CARTESIAN_POINT('Ctrl Pts',(-2.65472321565694,0.439161997632241,
13.8391868794965));
#432597=CARTESIAN_POINT('Origin',(-2.62039699312969,0.539511499794106,13.8235269408515));
#432598=CARTESIAN_POINT('Ctrl Pts',(-2.66236978713557,0.540640744926744,
13.7902140241683));
#432599=CARTESIAN_POINT('Ctrl Pts',(-2.67204194591,0.546950098303653,13.8026027327198));
#432600=CARTESIAN_POINT('Ctrl Pts',(-2.66556758396333,0.562275259629291,
13.8057746032556));
#432601=CARTESIAN_POINT('Ctrl Pts',(-2.65239108398142,0.53412594130855,
13.8013225161808));
#432602=CARTESIAN_POINT('Ctrl Pts',(-2.66205334779722,0.540428844277751,
13.8136962270464));
#432603=CARTESIAN_POINT('Ctrl Pts',(-2.65559399359612,0.555736206840193,
13.8168830918628));
#432604=CARTESIAN_POINT('Ctrl Pts',(-2.64240807891856,0.527608329099887,
13.8124254880875));
#432605=CARTESIAN_POINT('Ctrl Pts',(-2.65205619396754,0.533902004579433,
13.8247886461867));
#432606=CARTESIAN_POINT('Ctrl Pts',(-2.64561610727078,0.549194023593803,
13.8279860620656));
#432607=CARTESIAN_POINT('Ctrl Pts',(-2.63242059778891,0.521087794598028,
13.8235227163066));
#432608=CARTESIAN_POINT('Ctrl Pts',(-2.64205001280595,0.527369271308659,
13.8358800595848));
#432609=CARTESIAN_POINT('Ctrl Pts',(-2.6356337482334,0.542648583457214,
13.8390832900376));
#432610=CARTESIAN_POINT('Origin',(-2.6503461928975,0.559064456922601,13.7902182540695));
#432611=CARTESIAN_POINT('Ctrl Pts',(-2.67950274280156,0.551826382928712,
13.7382347919292));
#432612=CARTESIAN_POINT('Ctrl Pts',(-2.69215163179234,0.560055810371279,
13.7369371795942));
#432613=CARTESIAN_POINT('Ctrl Pts',(-2.68894413082543,0.574863096232227,
13.7364597369711));
#432614=CARTESIAN_POINT('Ctrl Pts',(-2.68108662734283,0.552860454369261,
13.7595490285574));
#432615=CARTESIAN_POINT('Ctrl Pts',(-2.69403675967933,0.561287071655363,
13.7633824266926));
#432616=CARTESIAN_POINT('Ctrl Pts',(-2.69110574879531,0.576028266841136,
13.7648920890506));
#432617=CARTESIAN_POINT('Ctrl Pts',(-2.67300890295897,0.547586746666806,
13.780380659011));
#432618=CARTESIAN_POINT('Ctrl Pts',(-2.68421324823137,0.554870944153222,
13.7901039518744));
#432619=CARTESIAN_POINT('Ctrl Pts',(-2.68008734598676,0.570084831627961,
13.7926933640891));
#432620=CARTESIAN_POINT('Ctrl Pts',(-2.65896801476284,0.538419865504878,
13.7936647693663));
#432621=CARTESIAN_POINT('Ctrl Pts',(-2.66804058847989,0.54430728752929,
13.8072068914933));
#432622=CARTESIAN_POINT('Ctrl Pts',(-2.660950206824,0.559811182453508,13.8104111085397));
#432623=CARTESIAN_POINT('Origin',(-2.66770182711108,0.570395443204266,13.7435492065112));
#432624=CARTESIAN_POINT('Origin',(-2.66770182711109,0.570395443204266,14.));
#432625=CARTESIAN_POINT('Origin',(-2.66770182711109,0.570395443204266,12.5369868989719));
#432626=CARTESIAN_POINT('Ctrl Pts',(-2.69000666893073,0.539318729353612,
12.506462012331));
#432627=CARTESIAN_POINT('Ctrl Pts',(-2.69641771158035,0.540604077607787,
12.4999388158272));
#432628=CARTESIAN_POINT('Ctrl Pts',(-2.69634186053824,0.540588870252309,
12.4907030323752));
#432629=CARTESIAN_POINT('Ctrl Pts',(-2.68965717673216,0.552589239455252,
12.5042014951932));
#432630=CARTESIAN_POINT('Ctrl Pts',(-2.69286920995931,0.558159153248441,
12.4980716682128));
#432631=CARTESIAN_POINT('Ctrl Pts',(-2.69148635757615,0.564808460318541,
12.4907355092743));
#432632=CARTESIAN_POINT('Ctrl Pts',(-2.68404205200784,0.554779233878853,
12.5218047446509));
#432633=CARTESIAN_POINT('Ctrl Pts',(-2.69173908484124,0.563738840817663,
12.5216906929433));
#432634=CARTESIAN_POINT('Ctrl Pts',(-2.68916697438798,0.575217298995718,
12.5161988840776));
#432635=CARTESIAN_POINT('Ctrl Pts',(-2.67969653749964,0.551952912936035,
12.5369868989719));
#432636=CARTESIAN_POINT('Ctrl Pts',(-2.69254753580896,0.560310985319929,
12.5369868989719));
#432637=CARTESIAN_POINT('Ctrl Pts',(-2.68915699292679,0.575261227809088,
12.5369868989719));
#432638=CARTESIAN_POINT('Origin',(-5.06527468391093E-31,-4.21128796913923E-31,
12.5));
#432639=CARTESIAN_POINT('Origin',(-2.66613838389344,0.304789073640317,12.5));
#432640=CARTESIAN_POINT('',(-2.66613838389344,0.304789073640317,12.5893111709658));
#432641=CARTESIAN_POINT('',(-2.66613838389344,0.304789073640317,13.8235269408515));
#432642=CARTESIAN_POINT('',(-2.66613838389344,0.304789073640317,12.5));
#432643=CARTESIAN_POINT('',(-2.69758167769643,0.32183583210109,13.7902182540695));
#432644=CARTESIAN_POINT('',(-2.66613838389344,0.304789073640317,13.8235269408515));
#432645=CARTESIAN_POINT('',(-2.71580314304261,0.331714470150389,13.7435492065112));
#432646=CARTESIAN_POINT('Origin',(-2.65585491815991,0.299213595166166,13.7445212918688));
#432647=CARTESIAN_POINT('',(-2.71580314304261,0.331714470150389,12.5369868989719));
#432648=CARTESIAN_POINT('',(-2.71580314304261,0.331714470150389,12.5));
#432649=CARTESIAN_POINT('Ctrl Pts',(-2.71580314304261,0.331714470150389,
12.5369868989719));
#432650=CARTESIAN_POINT('Ctrl Pts',(-2.69926029747777,0.32274588389589,
12.5544431401645));
#432651=CARTESIAN_POINT('Ctrl Pts',(-2.6827056200301,0.313770883070132,
12.5718848856037));
#432652=CARTESIAN_POINT('Ctrl Pts',(-2.66613838389344,0.304789073640317,
12.5893111709658));
#432653=CARTESIAN_POINT('Origin',(-2.93589676306087,0.162285249320105,12.5));
#432654=CARTESIAN_POINT('',(-2.72668989544586,0.225351759568759,13.7435492065112));
#432655=CARTESIAN_POINT('',(-2.70684497862863,0.231334114087542,13.7902182540695));
#432656=CARTESIAN_POINT('Origin',(-2.65469596712568,0.247054707803714,13.7418732680452));
#432657=CARTESIAN_POINT('',(-2.67260022728041,0.241657374439776,13.8235269408515));
#432658=CARTESIAN_POINT('',(-2.70684497862863,0.231334114087542,13.7902182540695));
#432659=CARTESIAN_POINT('',(-2.67260022728041,0.241657374439776,12.5893111709658));
#432660=CARTESIAN_POINT('',(-2.67260022728041,0.241657374439776,12.5));
#432661=CARTESIAN_POINT('',(-2.72668989544586,0.225351759568759,12.5369868989719));
#432662=CARTESIAN_POINT('Ctrl Pts',(-2.67260022728041,0.241657374439776,
12.5893111709658));
#432663=CARTESIAN_POINT('Ctrl Pts',(-2.69064353042739,0.236218125834742,
12.5718848856037));
#432664=CARTESIAN_POINT('Ctrl Pts',(-2.70867315596209,0.230783000417846,
12.5544431401645));
#432665=CARTESIAN_POINT('Ctrl Pts',(-2.72668989544586,0.225351759568759,
12.5369868989719));
#432666=CARTESIAN_POINT('',(-2.72668989544586,0.225351759568759,12.5));
#432667=CARTESIAN_POINT('Origin',(-2.68252174292037,0.274569441412333,12.5));
#432668=CARTESIAN_POINT('',(-2.64823028187141,0.272184934900437,13.8587068136939));
#432669=CARTESIAN_POINT('Ctrl Pts',(-2.67260022727837,0.241657374433491,
13.8235269408542));
#432670=CARTESIAN_POINT('Ctrl Pts',(-2.67092250335409,0.242163133131915,
13.8262006681044));
#432671=CARTESIAN_POINT('Ctrl Pts',(-2.6692557437193,0.242847048588549,
13.8288634856214));
#432672=CARTESIAN_POINT('Ctrl Pts',(-2.66760059200199,0.243695801952421,
13.8314912288862));
#432673=CARTESIAN_POINT('Ctrl Pts',(-2.66589430130243,0.244570779125726,
13.834200161153));
#432674=CARTESIAN_POINT('Ctrl Pts',(-2.66419822490259,0.245621467252351,
13.8368750301949));
#432675=CARTESIAN_POINT('Ctrl Pts',(-2.66251412552991,0.246878463044179,
13.8394886372968));
#432676=CARTESIAN_POINT('Ctrl Pts',(-2.66238405845029,0.246975543878232,
13.839690492513));
#432677=CARTESIAN_POINT('Ctrl Pts',(-2.6622540728036,0.24707387507256,13.8398919674349));
#432678=CARTESIAN_POINT('Ctrl Pts',(-2.66212417544159,0.24717348044291,
13.8400930404591));
#432679=CARTESIAN_POINT('Ctrl Pts',(-2.66010028715085,0.248725399124106,
13.8432258934518));
#432680=CARTESIAN_POINT('Ctrl Pts',(-2.65810747290765,0.250577821396457,
13.8462331177034));
#432681=CARTESIAN_POINT('Ctrl Pts',(-2.65627640534004,0.252740986569638,
13.8489036603661));
#432682=CARTESIAN_POINT('Ctrl Pts',(-2.65567725872272,0.253448799388322,
13.8497774930041));
#432683=CARTESIAN_POINT('Ctrl Pts',(-2.65509566950902,0.254189811509037,
13.85061494757));
#432684=CARTESIAN_POINT('Ctrl Pts',(-2.6545368964848,0.254964167004262,
13.8514076489583));
#432685=CARTESIAN_POINT('Ctrl Pts',(-2.65335501095143,0.256602040555441,
13.8530843267192));
#432686=CARTESIAN_POINT('Ctrl Pts',(-2.65216150767304,0.258551700020984,
13.8546805203176));
#432687=CARTESIAN_POINT('Ctrl Pts',(-2.65114202945552,0.260771226322149,
13.8559412814273));
#432688=CARTESIAN_POINT('Ctrl Pts',(-2.65100559020755,0.261068270922185,
13.8561100121513));
#432689=CARTESIAN_POINT('Ctrl Pts',(-2.65087223554554,0.261370079482595,
13.8562727473908));
#432690=CARTESIAN_POINT('Ctrl Pts',(-2.65074237013054,0.261676487288807,
13.8564289040185));
#432691=CARTESIAN_POINT('Ctrl Pts',(-2.65015343195509,0.263066043194364,
13.8571370725437));
#432692=CARTESIAN_POINT('Ctrl Pts',(-2.64962799811819,0.264575500587848,
13.8577210840553));
#432693=CARTESIAN_POINT('Ctrl Pts',(-2.64921420914942,0.266155834665666,
13.8581177131616));
#432694=CARTESIAN_POINT('Ctrl Pts',(-2.64909767193363,0.266600911135426,
13.8582294175695));
#432695=CARTESIAN_POINT('Ctrl Pts',(-2.64898983048389,0.267051531618308,
13.8583265086086));
#432696=CARTESIAN_POINT('Ctrl Pts',(-2.64889135421829,0.267506432392544,
13.8584082369006));
#432697=CARTESIAN_POINT('Ctrl Pts',(-2.64874987023207,0.268160002818657,
13.8585256585398));
#432698=CARTESIAN_POINT('Ctrl Pts',(-2.64862627488924,0.268830602447368,
13.8586122832068));
#432699=CARTESIAN_POINT('Ctrl Pts',(-2.64852455544563,0.269500954176995,
13.8586682984299));
#432700=CARTESIAN_POINT('Ctrl Pts',(-2.64844318997386,0.270037169110867,
13.8587131050557));
#432701=CARTESIAN_POINT('Ctrl Pts',(-2.64837469109747,0.270579112748801,
13.8587357943552));
#432702=CARTESIAN_POINT('Ctrl Pts',(-2.64831955312531,0.271126912995427,
13.8587355499465));
#432703=CARTESIAN_POINT('Ctrl Pts',(-2.64828391613936,0.271480969354972,
13.8587353919793));
#432704=CARTESIAN_POINT('Ctrl Pts',(-2.64825420735979,0.271833639631159,
13.8587257282814));
#432705=CARTESIAN_POINT('Ctrl Pts',(-2.64823028187141,0.272184934900437,
13.8587068136939));
#432706=CARTESIAN_POINT('Ctrl Pts',(-2.64823028187141,0.272184934900437,
13.8587068136939));
#432707=CARTESIAN_POINT('Ctrl Pts',(-2.64815159224441,0.273340325890064,
13.8586446046466));
#432708=CARTESIAN_POINT('Ctrl Pts',(-2.64813538423794,0.274480862310758,
13.858482427929));
#432709=CARTESIAN_POINT('Ctrl Pts',(-2.64817719388495,0.275606786970262,
13.8582284286032));
#432710=CARTESIAN_POINT('Ctrl Pts',(-2.64822008571928,0.276761854697963,
13.8579678548414));
#432711=CARTESIAN_POINT('Ctrl Pts',(-2.64832567286529,0.277904309142861,
13.857615680862));
#432712=CARTESIAN_POINT('Ctrl Pts',(-2.64848014407854,0.278990001618561,
13.8571944833187));
#432713=CARTESIAN_POINT('Ctrl Pts',(-2.64886564278924,0.281699458227203,
13.8561433417727));
#432714=CARTESIAN_POINT('Ctrl Pts',(-2.64956887779495,0.284182814934247,
13.8546163505474));
#432715=CARTESIAN_POINT('Ctrl Pts',(-2.65040285734276,0.286351799711337,
13.8528973491086));
#432716=CARTESIAN_POINT('Ctrl Pts',(-2.65055521310192,0.286748041229711,
13.8525833129072));
#432717=CARTESIAN_POINT('Ctrl Pts',(-2.65071183875195,0.28713389685014,
13.8522628768811));
#432718=CARTESIAN_POINT('Ctrl Pts',(-2.65087149822655,0.287508979248182,
13.851937733538));
#432719=CARTESIAN_POINT('Ctrl Pts',(-2.65184651648625,0.289799555412767,
13.8499521282529));
#432720=CARTESIAN_POINT('Ctrl Pts',(-2.65303532837086,0.291914400563566,
13.847639871647));
#432721=CARTESIAN_POINT('Ctrl Pts',(-2.65430542018226,0.293781734349322,
13.8452109780794));
#432722=CARTESIAN_POINT('Ctrl Pts',(-2.6548768607778,0.294621886471421,
13.8441181685877));
#432723=CARTESIAN_POINT('Ctrl Pts',(-2.65546433748986,0.295412519228075,
13.8430021611332));
#432724=CARTESIAN_POINT('Ctrl Pts',(-2.65605478550131,0.296150250405443,
13.8418824960098));
#432725=CARTESIAN_POINT('Ctrl Pts',(-2.65744619131792,0.297888732763546,
13.8392439765549));
#432726=CARTESIAN_POINT('Ctrl Pts',(-2.65891765954228,0.299418911650689,
13.8364981347964));
#432727=CARTESIAN_POINT('Ctrl Pts',(-2.66044841549995,0.300768553540579,
13.8336931113419));
#432728=CARTESIAN_POINT('Ctrl Pts',(-2.66193927459073,0.302083019031147,
13.8309611966328));
#432729=CARTESIAN_POINT('Ctrl Pts',(-2.66348823843773,0.303227129575497,
13.8281701127186));
#432730=CARTESIAN_POINT('Ctrl Pts',(-2.66508959981538,0.304189622649689,
13.8253580685121));
#432731=CARTESIAN_POINT('Ctrl Pts',(-2.6654367766903,0.304398292186929,
13.8247484142933));
#432732=CARTESIAN_POINT('Ctrl Pts',(-2.66578640770474,0.304598252248951,
13.8241378483365));
#432733=CARTESIAN_POINT('Ctrl Pts',(-2.66613838389344,0.304789073640317,
13.8235269408515));
#432734=CARTESIAN_POINT('',(-2.64833877401582,0.270947596501946,12.5969504640361));
#432735=CARTESIAN_POINT('Origin',(-2.68255463643422,0.274573005056113,12.584524458991));
#432736=CARTESIAN_POINT('Origin',(-2.68255463643422,0.274573005056113,12.584524458991));
#432737=CARTESIAN_POINT('Ctrl Pts',(-2.67260022728041,0.241657374439776,
12.5893111709658));
#432738=CARTESIAN_POINT('Ctrl Pts',(-2.66174861915796,0.244928648765858,
12.5770542771492));
#432739=CARTESIAN_POINT('Ctrl Pts',(-2.6634679191406,0.261202790292361,
12.5737548217797));
#432740=CARTESIAN_POINT('Ctrl Pts',(-2.69632905233628,0.234504195360933,
12.5663937883685));
#432741=CARTESIAN_POINT('Ctrl Pts',(-2.68546360148064,0.237779642651723,
12.5540940315304));
#432742=CARTESIAN_POINT('Ctrl Pts',(-2.68719142264049,0.2541038770703,12.5508374392248));
#432743=CARTESIAN_POINT('Ctrl Pts',(-2.72003393529857,0.227358233752083,
12.5434499600945));
#432744=CARTESIAN_POINT('Ctrl Pts',(-2.70913315699288,0.230644330688506,
12.5311293540533));
#432745=CARTESIAN_POINT('Ctrl Pts',(-2.71089140953306,0.247010769292089,
12.5278936106989));
#432746=CARTESIAN_POINT('Ctrl Pts',(-2.74371675158423,0.22021892425893,
12.5204817579905));
#432747=CARTESIAN_POINT('Ctrl Pts',(-2.73276202187558,0.223521285129382,
12.5081597038247));
#432748=CARTESIAN_POINT('Ctrl Pts',(-2.73456970364935,0.239923002463233,
12.5049254088044));
#432749=CARTESIAN_POINT('Ctrl Pts',(-2.72668989544586,0.225351759568759,
12.5369868989719));
#432750=CARTESIAN_POINT('Ctrl Pts',(-2.727581757252,0.225082903307011,12.5342545179733));
#432751=CARTESIAN_POINT('Ctrl Pts',(-2.72846891440114,0.224945756283421,
12.5314872231885));
#432752=CARTESIAN_POINT('Ctrl Pts',(-2.72930993230297,0.22500328887358,
12.5287124745063));
#432753=CARTESIAN_POINT('Ctrl Pts',(-2.73006840399125,0.225055174619049,
12.5262100684184));
#432754=CARTESIAN_POINT('Ctrl Pts',(-2.73078851669635,0.225266328661584,
12.5237004536639));
#432755=CARTESIAN_POINT('Ctrl Pts',(-2.73146398251014,0.225703988924608,
12.5212220730815));
#432756=CARTESIAN_POINT('Ctrl Pts',(-2.73198111002305,0.226039055716585,
12.5193246583486));
#432757=CARTESIAN_POINT('Ctrl Pts',(-2.73247790432002,0.226511420035291,
12.517417831369));
#432758=CARTESIAN_POINT('Ctrl Pts',(-2.73290258723252,0.227203380386272,
12.5155812248347));
#432759=CARTESIAN_POINT('Ctrl Pts',(-2.73308350443592,0.227498159215093,
12.5147988205793));
#432760=CARTESIAN_POINT('Ctrl Pts',(-2.73325175458264,0.227832944795516,
12.5140295443047));
#432761=CARTESIAN_POINT('Ctrl Pts',(-2.73340545939293,0.228214202692653,
12.5132817086137));
#432762=CARTESIAN_POINT('Ctrl Pts',(-2.73363807083058,0.228791184944568,
12.5121499604604));
#432763=CARTESIAN_POINT('Ctrl Pts',(-2.73383575960262,0.229489735061785,
12.5110494206568));
#432764=CARTESIAN_POINT('Ctrl Pts',(-2.7339678607362,0.230330984967703,
12.5100666561695));
#432765=CARTESIAN_POINT('Ctrl Pts',(-2.7340437129029,0.230814028726455,
12.5095023550641));
#432766=CARTESIAN_POINT('Ctrl Pts',(-2.73409817218707,0.231349803419567,
12.5089719619137));
#432767=CARTESIAN_POINT('Ctrl Pts',(-2.73412386357233,0.23192891242457,
12.5085043804652));
#432768=CARTESIAN_POINT('Ctrl Pts',(-2.73416145956812,0.232776363019137,
12.5078201359221));
#432769=CARTESIAN_POINT('Ctrl Pts',(-2.73413733431634,0.233741244351165,
12.5072563000949));
#432770=CARTESIAN_POINT('Ctrl Pts',(-2.73404465979884,0.234757940087455,
12.5068768744332));
#432771=CARTESIAN_POINT('Ctrl Pts',(-2.73397783509199,0.235491047702893,
12.5066032824114));
#432772=CARTESIAN_POINT('Ctrl Pts',(-2.73387425466085,0.236263980762711,
12.5064197834844));
#432773=CARTESIAN_POINT('Ctrl Pts',(-2.733742264661,0.237033920005263,12.5063282718343));
#432774=CARTESIAN_POINT('Ctrl Pts',(-2.73354960012429,0.238157792932223,
12.5061946931565));
#432775=CARTESIAN_POINT('Ctrl Pts',(-2.73329333237519,0.239299487865532,
12.5062515701262));
#432776=CARTESIAN_POINT('Ctrl Pts',(-2.73300445492327,0.240391536141246,
12.5064436508398));
#432777=CARTESIAN_POINT('',(-2.6634679191406,0.261202790292361,12.5737548217797));
#432778=CARTESIAN_POINT('Origin',(-2.67894999728999,0.262721097302213,12.5893111709658));
#432779=CARTESIAN_POINT('Ctrl Pts',(-2.73300445492327,0.240391536141246,
12.5064436508398));
#432780=CARTESIAN_POINT('Ctrl Pts',(-2.72271137877843,0.243472602714325,
12.5164271754438));
#432781=CARTESIAN_POINT('Ctrl Pts',(-2.71241416254567,0.246554690460763,
12.5264061185523));
#432782=CARTESIAN_POINT('Ctrl Pts',(-2.70211266068599,0.249637836252174,
12.536380305637));
#432783=CARTESIAN_POINT('Ctrl Pts',(-2.68923787273109,0.253491143162093,
12.5488460165097));
#432784=CARTESIAN_POINT('Ctrl Pts',(-2.67635638684673,0.257346103845855,
12.5613043021964));
#432785=CARTESIAN_POINT('Ctrl Pts',(-2.6634679191406,0.261202790292361,
12.5737548217797));
#432786=CARTESIAN_POINT('Ctrl Pts',(-2.66613838389344,0.304789073640317,
12.5893111709658));
#432787=CARTESIAN_POINT('Ctrl Pts',(-2.65617451238041,0.299387231451617,
12.5770542771492));
#432788=CARTESIAN_POINT('Ctrl Pts',(-2.66115509936876,0.283798856677239,
12.5737548217797));
#432789=CARTESIAN_POINT('Ctrl Pts',(-2.65684217843296,0.299749201861002,
12.5928319619712));
#432790=CARTESIAN_POINT('Ctrl Pts',(-2.65169850360042,0.293254894693306,
12.5821634970842));
#432791=CARTESIAN_POINT('Ctrl Pts',(-2.65776421811106,0.281971251231409,
12.5773203894503));
#432792=CARTESIAN_POINT('Ctrl Pts',(-2.64678837658131,0.286351247999782,
12.5969440695591));
#432793=CARTESIAN_POINT('Ctrl Pts',(-2.64717949804393,0.282350552241116,
12.5878292599214));
#432794=CARTESIAN_POINT('Ctrl Pts',(-2.65418247444654,0.277194719077306,
12.5813877129824));
#432795=CARTESIAN_POINT('Ctrl Pts',(-2.64985020398195,0.25590785038207,
12.596957478804));
#432796=CARTESIAN_POINT('Ctrl Pts',(-2.64946205278996,0.259878987725584,
12.5878468778671));
#432797=CARTESIAN_POINT('Ctrl Pts',(-2.65528428009154,0.266299201988851,
12.5814011370086));
#432798=CARTESIAN_POINT('Ctrl Pts',(-2.6624610705918,0.244713876535013,
12.5928371701607));
#432799=CARTESIAN_POINT('Ctrl Pts',(-2.65611683232142,0.250032307363024,
12.5821692192952));
#432800=CARTESIAN_POINT('Ctrl Pts',(-2.65976522429226,0.262308832033917,
12.5773318885715));
#432801=CARTESIAN_POINT('Ctrl Pts',(-2.67260022728039,0.241657374439724,
12.5893111709658));
#432802=CARTESIAN_POINT('Ctrl Pts',(-2.66174861915794,0.244928648765806,
12.5770542771492));
#432803=CARTESIAN_POINT('Ctrl Pts',(-2.66346791914058,0.261202790292308,
12.5737548217797));
#432804=CARTESIAN_POINT('',(-2.66115509936876,0.283798856677239,12.5737548217797));
#432805=CARTESIAN_POINT('Origin',(-2.67662373367068,0.285448509014408,12.5893111709658));
#432806=CARTESIAN_POINT('Ctrl Pts',(-2.66346791914058,0.261202790292308,
12.5737548217797));
#432807=CARTESIAN_POINT('Ctrl Pts',(-2.66249948799061,0.261460590096039,
12.5746934679442));
#432808=CARTESIAN_POINT('Ctrl Pts',(-2.6614749776444,0.261922882199321,
12.5756680099006));
#432809=CARTESIAN_POINT('Ctrl Pts',(-2.66050957865738,0.262534035587474,
12.5765688348656));
#432810=CARTESIAN_POINT('Ctrl Pts',(-2.66025399996289,0.262695831681293,
12.5768073183026));
#432811=CARTESIAN_POINT('Ctrl Pts',(-2.66000248368076,0.26286781682604,
12.5770407398754));
#432812=CARTESIAN_POINT('Ctrl Pts',(-2.65975686203997,0.263048485452194,
12.5772674179684));
#432813=CARTESIAN_POINT('Ctrl Pts',(-2.65874889724505,0.263789900639083,
12.5781976435658));
#432814=CARTESIAN_POINT('Ctrl Pts',(-2.65778963545941,0.264728747969256,
12.5790594849312));
#432815=CARTESIAN_POINT('Ctrl Pts',(-2.65697762396725,0.265836145847293,
12.5797571720116));
#432816=CARTESIAN_POINT('Ctrl Pts',(-2.65644856928278,0.266557655383312,
12.580211740231));
#432817=CARTESIAN_POINT('Ctrl Pts',(-2.65597311843985,0.267394604292317,
12.5806009430798));
#432818=CARTESIAN_POINT('Ctrl Pts',(-2.65560014570566,0.268296825996709,
12.5808812374708));
#432819=CARTESIAN_POINT('Ctrl Pts',(-2.65527963839458,0.269072133749717,
12.5811221033394));
#432820=CARTESIAN_POINT('Ctrl Pts',(-2.65502834998581,0.269911558486257,
12.581287365893));
#432821=CARTESIAN_POINT('Ctrl Pts',(-2.65486845135005,0.270770112916528,
12.581359338449));
#432822=CARTESIAN_POINT('Ctrl Pts',(-2.65484622874146,0.270889434253864,
12.5813693411482));
#432823=CARTESIAN_POINT('Ctrl Pts',(-2.65482571219639,0.271009134368885,
12.5813775999465));
#432824=CARTESIAN_POINT('Ctrl Pts',(-2.65480690080815,0.271129103078795,
12.5813841266931));
#432825=CARTESIAN_POINT('Ctrl Pts',(-2.6547749850128,0.271332644505073,
12.5813952001081));
#432826=CARTESIAN_POINT('Ctrl Pts',(-2.65474836531475,0.271538416630948,
12.5814007534795));
#432827=CARTESIAN_POINT('Ctrl Pts',(-2.65472724888778,0.271746355137143,
12.5814005856065));
#432828=CARTESIAN_POINT('Ctrl Pts',(-2.6546305861411,0.272698216319819,
12.5813998171494));
#432829=CARTESIAN_POINT('Ctrl Pts',(-2.65465558459366,0.273629672533526,
12.58127954464));
#432830=CARTESIAN_POINT('Ctrl Pts',(-2.65477252361255,0.274536229411493,
12.5810700125799));
#432831=CARTESIAN_POINT('Ctrl Pts',(-2.65491377263279,0.275631246900311,
12.5808169217085));
#432832=CARTESIAN_POINT('Ctrl Pts',(-2.65520577317846,0.276687894448358,
12.5804173076348));
#432833=CARTESIAN_POINT('Ctrl Pts',(-2.65559783328823,0.277620505963392,
12.5799304713245));
#432834=CARTESIAN_POINT('Ctrl Pts',(-2.65608371927592,0.278776305433444,
12.5793271277669));
#432835=CARTESIAN_POINT('Ctrl Pts',(-2.65672374331989,0.279825772932485,
12.5785808224116));
#432836=CARTESIAN_POINT('Ctrl Pts',(-2.65746384864562,0.280741185391335,
12.5777485681082));
#432837=CARTESIAN_POINT('Ctrl Pts',(-2.65856668666556,0.282105250245944,
12.576508418016));
#432838=CARTESIAN_POINT('Ctrl Pts',(-2.65987711756026,0.283164490719574,
12.5750928681475));
#432839=CARTESIAN_POINT('Ctrl Pts',(-2.66115509936876,0.283798856677239,
12.5737548217797));
#432840=CARTESIAN_POINT('Ctrl Pts',(-2.66115509936876,0.283798856677239,
12.5737548217797));
#432841=CARTESIAN_POINT('Ctrl Pts',(-2.65617451238041,0.299387231451617,
12.5770542771492));
#432842=CARTESIAN_POINT('Ctrl Pts',(-2.66613838389344,0.304789073640317,
12.5893111709658));
#432843=CARTESIAN_POINT('Ctrl Pts',(-2.68294525065326,0.295554887519686,
12.5508408821982));
#432844=CARTESIAN_POINT('Ctrl Pts',(-2.67794617080864,0.311190581470929,
12.55409748406));
#432845=CARTESIAN_POINT('Ctrl Pts',(-2.68792275366984,0.316599315026769,
12.5663972313419));
#432846=CARTESIAN_POINT('Ctrl Pts',(-2.70471355565376,0.30730047227298,
12.52790050457));
#432847=CARTESIAN_POINT('Ctrl Pts',(-2.69967613132898,0.322971325265517,
12.5311362602938));
#432848=CARTESIAN_POINT('Ctrl Pts',(-2.70968514659679,0.328397641820345,
12.5434568539655));
#432849=CARTESIAN_POINT('Ctrl Pts',(-2.72646170553159,0.319036434919816,
12.5049357605811));
#432850=CARTESIAN_POINT('Ctrl Pts',(-2.721368740735,0.334731819418772,12.5081700652078));
#432851=CARTESIAN_POINT('Ctrl Pts',(-2.73142728390559,0.34018498717437,
12.5204921097672));
#432852=CARTESIAN_POINT('Ctrl Pts',(-2.72503363600676,0.318265807005603,
12.5064436508395));
#432853=CARTESIAN_POINT('Ctrl Pts',(-2.72510023128608,0.319484171835756,
12.5062361689309));
#432854=CARTESIAN_POINT('Ctrl Pts',(-2.72511753114434,0.320754011327717,
12.5061871075061));
#432855=CARTESIAN_POINT('Ctrl Pts',(-2.72506516886799,0.321982129739407,
12.5063648335164));
#432856=CARTESIAN_POINT('Ctrl Pts',(-2.72504138269223,0.322540016875481,
12.5064455676329));
#432857=CARTESIAN_POINT('Ctrl Pts',(-2.72500266959679,0.323097066693645,
12.506574497099));
#432858=CARTESIAN_POINT('Ctrl Pts',(-2.72494964106265,0.323629321706796,
12.5067492519495));
#432859=CARTESIAN_POINT('Ctrl Pts',(-2.72484307816486,0.324698908816405,
12.5071004286051));
#432860=CARTESIAN_POINT('Ctrl Pts',(-2.72467398385993,0.325707613177533,
12.5076537929613));
#432861=CARTESIAN_POINT('Ctrl Pts',(-2.72446437784822,0.326581289986317,
12.5083435010505));
#432862=CARTESIAN_POINT('Ctrl Pts',(-2.72445118189717,0.32663629316256,
12.5083869222964));
#432863=CARTESIAN_POINT('Ctrl Pts',(-2.72443781233519,0.326690764377107,
12.5084308732337));
#432864=CARTESIAN_POINT('Ctrl Pts',(-2.72442426943959,0.326744686821748,
12.5084753333615));
#432865=CARTESIAN_POINT('Ctrl Pts',(-2.72431563754193,0.32717721599888,
12.5088319622689));
#432866=CARTESIAN_POINT('Ctrl Pts',(-2.72419489890408,0.3275835317631,12.509227847131));
#432867=CARTESIAN_POINT('Ctrl Pts',(-2.72406832777229,0.327952349809118,
12.5096423454524));
#432868=CARTESIAN_POINT('Ctrl Pts',(-2.72367170986328,0.329108062333313,
12.5109411997424));
#432869=CARTESIAN_POINT('Ctrl Pts',(-2.72320257217674,0.329969800066465,
12.5124831113042));
#432870=CARTESIAN_POINT('Ctrl Pts',(-2.72271884638541,0.330612394677618,
12.5140723025008));
#432871=CARTESIAN_POINT('Ctrl Pts',(-2.72267352074896,0.330672606496496,
12.5142212114565));
#432872=CARTESIAN_POINT('Ctrl Pts',(-2.72262807576743,0.330730922551065,
12.5143705582413));
#432873=CARTESIAN_POINT('Ctrl Pts',(-2.72258256556837,0.330787420106788,
12.5145201959299));
#432874=CARTESIAN_POINT('Ctrl Pts',(-2.72199791930382,0.331513215326123,
12.5164425148273));
#432875=CARTESIAN_POINT('Ctrl Pts',(-2.72139084050179,0.331970504192687,
12.518463520594));
#432876=CARTESIAN_POINT('Ctrl Pts',(-2.72077139897204,0.33224893366673,
12.5205025929157));
#432877=CARTESIAN_POINT('Ctrl Pts',(-2.72041209833242,0.332410433797589,
12.5216853356836));
#432878=CARTESIAN_POINT('Ctrl Pts',(-2.72004948559046,0.332511906719643,
12.5228750347131));
#432879=CARTESIAN_POINT('Ctrl Pts',(-2.71969136426353,0.332569846030572,
12.5240609649613));
#432880=CARTESIAN_POINT('Ctrl Pts',(-2.71881237467914,0.33271205496091,
12.5269717671326));
#432881=CARTESIAN_POINT('Ctrl Pts',(-2.71793404413007,0.332585744095375,
12.5299036066169));
#432882=CARTESIAN_POINT('Ctrl Pts',(-2.71705798926049,0.332277555854814,
12.5328133004019));
#432883=CARTESIAN_POINT('Ctrl Pts',(-2.71663743191193,0.332129607554079,
12.5342101228451));
#432884=CARTESIAN_POINT('Ctrl Pts',(-2.71621809766108,0.331939434757048,
12.5356023438238));
#432885=CARTESIAN_POINT('Ctrl Pts',(-2.71580314304261,0.331714470150389,
12.5369868989719));
#432886=CARTESIAN_POINT('Origin',(-13.9183178550687,6.41110437652535,-1.24054849490876));
#432887=CARTESIAN_POINT('Ctrl Pts',(-2.72664986841926,0.225363784462659,
12.5369868989719));
#432888=CARTESIAN_POINT('Ctrl Pts',(-2.74134440404376,0.220964474691219,
12.5369868989719));
#432889=CARTESIAN_POINT('Ctrl Pts',(-2.74229760565712,0.205655173258131,
12.5369868989719));
#432890=CARTESIAN_POINT('Ctrl Pts',(-2.73161717717023,0.223876582273657,
12.5218025310015));
#432891=CARTESIAN_POINT('Ctrl Pts',(-2.74153211513278,0.217446195900894,
12.5216901060417));
#432892=CARTESIAN_POINT('Ctrl Pts',(-2.74229471644259,0.205701842107343,
12.5161920673678));
#432893=CARTESIAN_POINT('Ctrl Pts',(-2.73638997309462,0.227558496213283,
12.5042015548895));
#432894=CARTESIAN_POINT('Ctrl Pts',(-2.74104250119392,0.223116500344086,
12.4980677368514));
#432895=CARTESIAN_POINT('Ctrl Pts',(-2.74158781128973,0.216342032348497,
12.4907278922777));
#432896=CARTESIAN_POINT('Ctrl Pts',(-2.73298453076523,0.240389783648551,
12.506463626192));
#432897=CARTESIAN_POINT('Ctrl Pts',(-2.73950210632884,0.240963061163302,
12.4999376786891));
#432898=CARTESIAN_POINT('Ctrl Pts',(-2.73942250361987,0.240956059412004,
12.4906970594712));
#432899=CARTESIAN_POINT('Origin',(-2.72034012543628,0.204288036706323,12.5369868989719));
#432900=CARTESIAN_POINT('Origin',(-2.72034012543628,0.204288036706323,14.));
#432901=CARTESIAN_POINT('Origin',(-2.72034012543628,0.204288036706323,13.7435492065112));
#432902=CARTESIAN_POINT('Ctrl Pts',(-2.70298352541866,0.23249814110276,
13.793642941384));
#432903=CARTESIAN_POINT('Ctrl Pts',(-2.71334351629492,0.229403499273819,
13.8071662555867));
#432904=CARTESIAN_POINT('Ctrl Pts',(-2.71092135293231,0.212546675484043,
13.8103758687955));
#432905=CARTESIAN_POINT('Ctrl Pts',(-2.71889728595751,0.227700857419778,
13.7804579775006));
#432906=CARTESIAN_POINT('Ctrl Pts',(-2.73167767585962,0.223872632546517,
13.7901904343352));
#432907=CARTESIAN_POINT('Ctrl Pts',(-2.73198954862573,0.208119580158416,
13.7927914348263));
#432908=CARTESIAN_POINT('Ctrl Pts',(-2.72826631567795,0.2248765159371,13.7597120340895));
#432909=CARTESIAN_POINT('Ctrl Pts',(-2.74305518169568,0.220440692238788,
13.7635825532444));
#432910=CARTESIAN_POINT('Ctrl Pts',(-2.74440818285361,0.205483911033912,
13.7651073818884));
#432911=CARTESIAN_POINT('Ctrl Pts',(-2.72643164513206,0.2254295866687,13.7381884353898));
#432912=CARTESIAN_POINT('Ctrl Pts',(-2.74087460842012,0.22109845262713,
13.7368803041982));
#432913=CARTESIAN_POINT('Ctrl Pts',(-2.74197614264614,0.205999569904626,
13.7363986145813));
#432914=CARTESIAN_POINT('Origin',(-2.70049520861906,0.210270391225106,13.7902182540695));
#432915=CARTESIAN_POINT('Ctrl Pts',(-2.67259645837988,0.241658509801999,
13.8235227101244));
#432916=CARTESIAN_POINT('Ctrl Pts',(-2.68360551716661,0.238344401633875,
13.8358800583119));
#432917=CARTESIAN_POINT('Ctrl Pts',(-2.68175383533497,0.221876331818285,
13.8390832900376));
#432918=CARTESIAN_POINT('Ctrl Pts',(-2.68401642319661,0.238215901360868,
13.8124254819053));
#432919=CARTESIAN_POINT('Ctrl Pts',(-2.69504686133929,0.234895356975299,
13.8247886449157));
#432920=CARTESIAN_POINT('Ctrl Pts',(-2.69317590227665,0.21840838353296,
13.8279860620657));
#432921=CARTESIAN_POINT('Ctrl Pts',(-2.69543126995668,0.23477483578484,
13.8013225099955));
#432922=CARTESIAN_POINT('Ctrl Pts',(-2.70647788343758,0.231449423865085,
13.8136962257787));
#432923=CARTESIAN_POINT('Ctrl Pts',(-2.70459276011104,0.214942300102144,
13.8168830918626));
#432924=CARTESIAN_POINT('Ctrl Pts',(-2.70684119779572,0.231335253043433,
13.7902140179785));
#432925=CARTESIAN_POINT('Ctrl Pts',(-2.71789912271719,0.228006439745012,
13.802602731458));
#432926=CARTESIAN_POINT('Ctrl Pts',(-2.71600461405122,0.211478010012094,
13.8057746032558));
#432927=CARTESIAN_POINT('Origin',(-2.66625045727084,0.22059365157734,13.8235269408515));
#432928=CARTESIAN_POINT('Ctrl Pts',(-2.66613838389344,0.304789073640317,
13.8235269408515));
#432929=CARTESIAN_POINT('Ctrl Pts',(-2.67651853655451,0.310416599697473,
13.8362179249168));
#432930=CARTESIAN_POINT('Ctrl Pts',(-2.670914504778,0.326549108240942,13.8391868794938));
#432931=CARTESIAN_POINT('Ctrl Pts',(-2.65664099602971,0.299640132249645,
13.8400110824519));
#432932=CARTESIAN_POINT('Ctrl Pts',(-2.66333286786432,0.307159488220104,
13.8494522556836));
#432933=CARTESIAN_POINT('Ctrl Pts',(-2.65533803562189,0.317976629471443,
13.85569149686));
#432934=CARTESIAN_POINT('Ctrl Pts',(-2.64675275490183,0.286693302002753,
13.8586819406588));
#432935=CARTESIAN_POINT('Ctrl Pts',(-2.64632327063174,0.291025920944768,
13.868010383617));
#432936=CARTESIAN_POINT('Ctrl Pts',(-2.63903938795127,0.296396015905721,
13.8744918421245));
#432937=CARTESIAN_POINT('Ctrl Pts',(-2.64988635961401,0.255560489417721,
13.8587686893867));
#432938=CARTESIAN_POINT('Ctrl Pts',(-2.65031196544437,0.251266425189394,
13.8680909899357));
#432939=CARTESIAN_POINT('Ctrl Pts',(-2.64425847956561,0.244569283245145,
13.8745789365163));
#432940=CARTESIAN_POINT('Ctrl Pts',(-2.66223983298432,0.244780569768255,
13.8400379222776));
#432941=CARTESIAN_POINT('Ctrl Pts',(-2.67030993866681,0.238768612667464,
13.8494748685453));
#432942=CARTESIAN_POINT('Ctrl Pts',(-2.66467592518206,0.226561278916095,
13.8557104837033));
#432943=CARTESIAN_POINT('Ctrl Pts',(-2.67260022727837,0.241657374433491,
13.8235269408542));
#432944=CARTESIAN_POINT('Ctrl Pts',(-2.68390520534653,0.238249429353411,
13.8362179249195));
#432945=CARTESIAN_POINT('Ctrl Pts',(-2.68168562294419,0.221316134989481,
13.8391868794965));
#432946=CARTESIAN_POINT('Origin',(-2.6556530341162,0.324129638266227,13.8235269408515));
#432947=CARTESIAN_POINT('Ctrl Pts',(-2.69757821107425,0.321833953560952,
13.7902140241682));
#432948=CARTESIAN_POINT('Ctrl Pts',(-2.70773245741165,0.327333942352926,
13.8026027327198));
#432949=CARTESIAN_POINT('Ctrl Pts',(-2.70252878129016,0.343135831072191,
13.8057746032556));
#432950=CARTESIAN_POINT('Ctrl Pts',(-2.68710169425629,0.316154184359189,
13.8013225161808));
#432951=CARTESIAN_POINT('Ctrl Pts',(-2.69724555279159,0.321648550737635,
13.8136962270464));
#432952=CARTESIAN_POINT('Ctrl Pts',(-2.69205538371422,0.337431476647038,
13.8168830918628));
#432953=CARTESIAN_POINT('Ctrl Pts',(-2.67662066091767,0.310471966557803,
13.8124254880875));
#432954=CARTESIAN_POINT('Ctrl Pts',(-2.68674966563899,0.315958289406157,
13.8247886461867));
#432955=CARTESIAN_POINT('Ctrl Pts',(-2.68157744931327,0.331724352341398,
13.8279860620656));
#432956=CARTESIAN_POINT('Ctrl Pts',(-2.66613492821198,0.304787201027912,
13.8235227163065));
#432957=CARTESIAN_POINT('Ctrl Pts',(-2.67624430081123,0.310262889923955,
13.8358800595848));
#432958=CARTESIAN_POINT('Ctrl Pts',(-2.67109479161606,0.326014346550151,
13.8390832900376));
#432959=CARTESIAN_POINT('Origin',(-2.6870963279192,0.341176396726999,13.7902182540695));
#432960=CARTESIAN_POINT('Ctrl Pts',(-2.7155658915832,0.331585877333848,
13.7382347919292));
#432961=CARTESIAN_POINT('Ctrl Pts',(-2.72884346717415,0.338756920156188,
13.7369371795943));
#432962=CARTESIAN_POINT('Ctrl Pts',(-2.72685357016392,0.353776377100719,
13.7364597369712));
#432963=CARTESIAN_POINT('Ctrl Pts',(-2.71722879230157,0.332487406692799,
13.7595490285573));
#432964=CARTESIAN_POINT('Ctrl Pts',(-2.73082268167875,0.339830429096406,
13.7633824266926));
#432965=CARTESIAN_POINT('Ctrl Pts',(-2.72910296774987,0.354761478768508,
13.7648920890506));
#432966=CARTESIAN_POINT('Ctrl Pts',(-2.7087480897428,0.327889656344912,
13.7803806590111));
#432967=CARTESIAN_POINT('Ctrl Pts',(-2.72050888319893,0.334236358109327,
13.7901039518744));
#432968=CARTESIAN_POINT('Ctrl Pts',(-2.71763678262167,0.349735921964489,
13.7926933640892));
#432969=CARTESIAN_POINT('Ctrl Pts',(-2.69400673552795,0.319897739961045,
13.7936647693663));
#432970=CARTESIAN_POINT('Ctrl Pts',(-2.70352900055552,0.325026073090752,
13.8072068914933));
#432971=CARTESIAN_POINT('Ctrl Pts',(-2.69772592292715,0.341056312012424,
13.8104111085397));
#432972=CARTESIAN_POINT('Origin',(-2.70531779326537,0.351055034776299,13.7435492065112));
#432973=CARTESIAN_POINT('Origin',(-2.70531779326537,0.351055034776299,14.));
#432974=CARTESIAN_POINT('Origin',(-2.70531779326537,0.351055034776299,12.5369868989719));
#432975=CARTESIAN_POINT('Ctrl Pts',(-2.72501537688291,0.318263674450985,
12.506462012331));
#432976=CARTESIAN_POINT('Ctrl Pts',(-2.7315098551323,0.319022186321717,
12.4999388158272));
#432977=CARTESIAN_POINT('Ctrl Pts',(-2.73143301693763,0.319013212131559,
12.4907030323752));
#432978=CARTESIAN_POINT('Ctrl Pts',(-2.72574871736152,0.33151851488371,
12.5042014951932));
#432979=CARTESIAN_POINT('Ctrl Pts',(-2.72940406249579,0.336808084721183,
12.4980716682127));
#432980=CARTESIAN_POINT('Ctrl Pts',(-2.7285677916952,0.343547982077514,
12.4907355092743));
#432981=CARTESIAN_POINT('Ctrl Pts',(-2.7203307813779,0.334158907074822,
12.5218047446509));
#432982=CARTESIAN_POINT('Ctrl Pts',(-2.72873249411198,0.342461322028952,
12.5216906929434));
#432983=CARTESIAN_POINT('Ctrl Pts',(-2.72710454304638,0.354111237464613,
12.5161988840776));
#432984=CARTESIAN_POINT('Ctrl Pts',(-2.71576935481563,0.331696190256002,
12.5369868989719));
#432985=CARTESIAN_POINT('Ctrl Pts',(-2.72925885298006,0.33897897617847,
12.5369868989719));
#432986=CARTESIAN_POINT('Ctrl Pts',(-2.72709817540379,0.354155833690222,
12.5369868989719));
#432987=CARTESIAN_POINT('Origin',(-5.12508596464071E-31,-4.62728456409025E-31,
12.5));
#432988=CARTESIAN_POINT('Origin',(-2.68211016738736,0.0864598836326287,
12.5));
#432989=CARTESIAN_POINT('',(-2.68211016738736,0.0864598836326287,12.5893111709658));
#432990=CARTESIAN_POINT('',(-2.68211016738736,0.0864598836326287,13.8235269408515));
#432991=CARTESIAN_POINT('',(-2.68211016738736,0.0864598836326287,12.5));
#432992=CARTESIAN_POINT('',(-2.71483830529306,0.10088700006064,13.7902182540695));
#432993=CARTESIAN_POINT('',(-2.68211016738736,0.0864598836326287,13.8235269408515));
#432994=CARTESIAN_POINT('',(-2.73380434092628,0.109247549171216,13.7435492065112));
#432995=CARTESIAN_POINT('Origin',(-2.67140646578605,0.0817411550293193,
13.7445212918704));
#432996=CARTESIAN_POINT('',(-2.73380434092628,0.109247549171216,12.5369868989719));
#432997=CARTESIAN_POINT('',(-2.73380434092628,0.109247549171216,12.5));
#432998=CARTESIAN_POINT('Ctrl Pts',(-2.73380434092628,0.109247549171216,
12.5369868989719));
#432999=CARTESIAN_POINT('Ctrl Pts',(-2.71658551727533,0.101657200637442,
12.5544431401645));
#433000=CARTESIAN_POINT('Ctrl Pts',(-2.69935437826406,0.0940614232846584,
12.5718848856037));
#433001=CARTESIAN_POINT('Ctrl Pts',(-2.68211016738736,0.0864598836326287,
12.5893111709658));
#433002=CARTESIAN_POINT('Origin',(-2.93935556317855,-0.0775575831846505,
12.5));
#433003=CARTESIAN_POINT('',(-2.73598532022336,0.00235138034619718,13.7435492065112));
#433004=CARTESIAN_POINT('',(-2.71669405316051,0.00993137402565123,13.7902182540695));
#433005=CARTESIAN_POINT('Origin',(-2.66599993752196,0.0298502873284301,
13.7418732680452));
#433006=CARTESIAN_POINT('',(-2.68340468995259,0.0230115497283134,13.8235269408515));
#433007=CARTESIAN_POINT('',(-2.71669405316051,0.00993137402565123,13.7902182540695));
#433008=CARTESIAN_POINT('',(-2.68340468995259,0.0230115497283134,12.5893111709658));
#433009=CARTESIAN_POINT('',(-2.68340468995259,0.0230115497283134,12.5));
#433010=CARTESIAN_POINT('',(-2.73598532022336,0.00235138034619718,12.5369868989719));
#433011=CARTESIAN_POINT('Ctrl Pts',(-2.68340468995259,0.0230115497283134,
12.5893111709658));
#433012=CARTESIAN_POINT('Ctrl Pts',(-2.70094460623998,0.0161197030619724,
12.5718848856037));
#433013=CARTESIAN_POINT('Ctrl Pts',(-2.71847122650434,0.00923308071658,
12.5544431401645));
#433014=CARTESIAN_POINT('Ctrl Pts',(-2.73598532022336,0.00235138034619718,
12.5369868989719));
#433015=CARTESIAN_POINT('',(-2.73598532022336,0.00235138034619717,12.5));
#433016=CARTESIAN_POINT('Origin',(-2.69597583156671,0.0550054088815593,
12.5));
#433017=CARTESIAN_POINT('',(-2.66160411310814,0.0554239090400246,13.8587068136939));
#433018=CARTESIAN_POINT('Ctrl Pts',(-2.68340468995004,0.0230115497222156,
13.8235269408542));
#433019=CARTESIAN_POINT('Ctrl Pts',(-2.68177377254287,0.0236523756253514,
13.8262006681044));
#433020=CARTESIAN_POINT('Ctrl Pts',(-2.68016830437213,0.0244698717934027,
13.8288634856214));
#433021=CARTESIAN_POINT('Ctrl Pts',(-2.67858784131422,0.0254507112311175,
13.8314912288862));
#433022=CARTESIAN_POINT('Ctrl Pts',(-2.67695854691872,0.0264618555225051,
13.8342001611531));
#433023=CARTESIAN_POINT('Ctrl Pts',(-2.67535375490961,0.0276472935432582,
13.8368750301949));
#433024=CARTESIAN_POINT('Ctrl Pts',(-2.67377771606508,0.0290373765185761,
13.8394886372969));
#433025=CARTESIAN_POINT('Ctrl Pts',(-2.67365599476218,0.0291447359986302,
13.8396904925131));
#433026=CARTESIAN_POINT('Ctrl Pts',(-2.67353445653721,0.029253335040948,
13.8398919674349));
#433027=CARTESIAN_POINT('Ctrl Pts',(-2.67341311016033,0.0293631968235529,
13.8400930404591));
#433028=CARTESIAN_POINT('Ctrl Pts',(-2.67152245197074,0.0310749173079189,
13.8432258934518));
#433029=CARTESIAN_POINT('Ctrl Pts',(-2.66968725826479,0.0330836086591771,
13.8462331177034));
#433030=CARTESIAN_POINT('Ctrl Pts',(-2.66803860146692,0.0353888250842538,
13.8489036603661));
#433031=CARTESIAN_POINT('Ctrl Pts',(-2.66749914177628,0.0361431187256927,
13.849777493004));
#433032=CARTESIAN_POINT('Ctrl Pts',(-2.66697988711977,0.0369290701098329,
13.85061494757));
#433033=CARTESIAN_POINT('Ctrl Pts',(-2.66648609052831,0.0377463941898977,
13.8514076489583));
#433034=CARTESIAN_POINT('Ctrl Pts',(-2.66544163952125,0.0394751524950208,
13.8530843267192));
#433035=CARTESIAN_POINT('Ctrl Pts',(-2.66441102287276,0.0415156062266747,
13.8546805203176));
#433036=CARTESIAN_POINT('Ctrl Pts',(-2.66357584888352,0.04381084417629,
13.8559412814274));
#433037=CARTESIAN_POINT('Ctrl Pts',(-2.66346407551843,0.0441180214502598,
13.8561100121513));
#433038=CARTESIAN_POINT('Ctrl Pts',(-2.66335576478259,0.0444296954105265,
13.8562727473908));
#433039=CARTESIAN_POINT('Ctrl Pts',(-2.66325130656481,0.044745668906959,
13.8564289040185));
#433040=CARTESIAN_POINT('Ctrl Pts',(-2.66277758973886,0.0461786051086078,
13.8571370725437));
#433041=CARTESIAN_POINT('Ctrl Pts',(-2.66237693903039,0.0477258676427366,
13.8577210840554));
#433042=CARTESIAN_POINT('Ctrl Pts',(-2.66209333880873,0.0493346709316656,
13.8581177131616));
#433043=CARTESIAN_POINT('Ctrl Pts',(-2.66201346722509,0.0497877653111516,
13.8582294175695));
#433044=CARTESIAN_POINT('Ctrl Pts',(-2.66194271436159,0.0502456764708526,
13.8583265086086));
#433045=CARTESIAN_POINT('Ctrl Pts',(-2.66188164440383,0.0507070903301426,
13.8584082369006));
#433046=CARTESIAN_POINT('Ctrl Pts',(-2.66179390325108,0.0513700183129284,
13.8585256585398));
#433047=CARTESIAN_POINT('Ctrl Pts',(-2.66172537925685,0.0520484607445389,
13.8586122832068));
#433048=CARTESIAN_POINT('Ctrl Pts',(-2.6616786381655,0.052724873013058,
13.8586682984299));
#433049=CARTESIAN_POINT('Ctrl Pts',(-2.66164124992571,0.0532659357772812,
13.8587131050557));
#433050=CARTESIAN_POINT('Ctrl Pts',(-2.66161715241133,0.0538116594368054,
13.8587357943552));
#433051=CARTESIAN_POINT('Ctrl Pts',(-2.66160684871186,0.054362131179908,
13.8587355499465));
#433052=CARTESIAN_POINT('Ctrl Pts',(-2.66160018918524,0.0547179141912392,
13.8587353919793));
#433053=CARTESIAN_POINT('Ctrl Pts',(-2.66159932516072,0.0550718325274348,
13.8587257282814));
#433054=CARTESIAN_POINT('Ctrl Pts',(-2.66160411310814,0.0554239090400246,
13.8587068136939));
#433055=CARTESIAN_POINT('Ctrl Pts',(-2.66160411310814,0.0554239090400246,
13.8587068136939));
#433056=CARTESIAN_POINT('Ctrl Pts',(-2.66161986040616,0.0565818694966455,
13.8586446046466));
#433057=CARTESIAN_POINT('Ctrl Pts',(-2.661696670637,0.0577199319795604,
13.858482427929));
#433058=CARTESIAN_POINT('Ctrl Pts',(-2.66183011447819,0.0588387023433441,
13.8582284286032));
#433059=CARTESIAN_POINT('Ctrl Pts',(-2.66196701233641,0.0599864305957805,
13.8579678548414));
#433060=CARTESIAN_POINT('Ctrl Pts',(-2.6621653687932,0.0611164772851363,
13.857615680862));
#433061=CARTESIAN_POINT('Ctrl Pts',(-2.66240782003208,0.0621859663707654,
13.8571944833187));
#433062=CARTESIAN_POINT('Ctrl Pts',(-2.66301288189458,0.0648549857623171,
13.8561433417727));
#433063=CARTESIAN_POINT('Ctrl Pts',(-2.6639161935698,0.0672727591232808,
13.8546163505475));
#433064=CARTESIAN_POINT('Ctrl Pts',(-2.66492419051466,0.0693665497070066,
13.8528973491086));
#433065=CARTESIAN_POINT('Ctrl Pts',(-2.66510833668488,0.069749054355661,
13.8525833129072));
#433066=CARTESIAN_POINT('Ctrl Pts',(-2.66529589199116,0.0701208596288435,
13.8522628768812));
#433067=CARTESIAN_POINT('Ctrl Pts',(-2.66548559290958,0.0704816802417791,
13.851937733538));
#433068=CARTESIAN_POINT('Ctrl Pts',(-2.66664407009854,0.0726851616633413,
13.8499521282529));
#433069=CARTESIAN_POINT('Ctrl Pts',(-2.66800130582272,0.0746960706363772,
13.847639871647));
#433070=CARTESIAN_POINT('Ctrl Pts',(-2.66941937654741,0.0764536667494184,
13.8452109780794));
#433071=CARTESIAN_POINT('Ctrl Pts',(-2.67005739591905,0.0772444456211071,
13.8441181685877));
#433072=CARTESIAN_POINT('Ctrl Pts',(-2.67070736176037,0.0779845628065856,
13.8430021611332));
#433073=CARTESIAN_POINT('Ctrl Pts',(-2.67135597704449,0.0786717122499349,
13.8418824960098));
#433074=CARTESIAN_POINT('Ctrl Pts',(-2.67288445552449,0.0802909974601713,
13.8392439765549));
#433075=CARTESIAN_POINT('Ctrl Pts',(-2.67447575134451,0.0816961464825684,
13.8364981347964));
#433076=CARTESIAN_POINT('Ctrl Pts',(-2.6761114221815,0.0829165267290124,
13.8336931113419));
#433077=CARTESIAN_POINT('Ctrl Pts',(-2.67770446170203,0.0841050995877381,
13.8309611966328));
#433078=CARTESIAN_POINT('Ctrl Pts',(-2.67934152713037,0.0851191482652251,
13.8281701127186));
#433079=CARTESIAN_POINT('Ctrl Pts',(-2.68101601223104,0.0859479129045207,
13.8253580685121));
#433080=CARTESIAN_POINT('Ctrl Pts',(-2.68137904240803,0.08612758997275,
13.8247484142933));
#433081=CARTESIAN_POINT('Ctrl Pts',(-2.68174380865551,0.0862983865106671,
13.8241378483365));
#433082=CARTESIAN_POINT('Ctrl Pts',(-2.68211016738736,0.0864598836326288,
13.8235269408515));
#433083=CARTESIAN_POINT('',(-2.66161138968753,0.0541818446662489,12.5969504640361));
#433084=CARTESIAN_POINT('Origin',(-2.69600890610016,0.0550062795408617,
12.584524458991));
#433085=CARTESIAN_POINT('Origin',(-2.69600890610016,0.0550062795408617,
12.584524458991));
#433086=CARTESIAN_POINT('Ctrl Pts',(-2.68340468995259,0.0230115497283134,
12.5893111709658));
#433087=CARTESIAN_POINT('Ctrl Pts',(-2.67285582888757,0.0271564459623303,
12.5770542771492));
#433088=CARTESIAN_POINT('Ctrl Pts',(-2.67589590165752,0.0432362977156396,
12.5737548217797));
#433089=CARTESIAN_POINT('Ctrl Pts',(-2.70647150879878,0.0139480527330364,
12.5663937883685));
#433090=CARTESIAN_POINT('Ctrl Pts',(-2.69590919119647,0.0180982363578279,
12.5540940315304));
#433091=CARTESIAN_POINT('Ctrl Pts',(-2.69896183982587,0.0342273197682056,
12.5508374392248));
#433092=CARTESIAN_POINT('Ctrl Pts',(-2.72951505350752,0.00489370069512543,
12.5434499600945));
#433093=CARTESIAN_POINT('Ctrl Pts',(-2.71891839404936,0.00905737804472826,
12.5311293540533));
#433094=CARTESIAN_POINT('Ctrl Pts',(-2.72200481283406,0.0252260447692931,
12.5278936106989));
#433095=CARTESIAN_POINT('Ctrl Pts',(-2.75253714717388,-0.00415222272246555,
12.5204817579905));
#433096=CARTESIAN_POINT('Ctrl Pts',(-2.74188804149321,3.20619846197456E-5,
12.5081597038247));
#433097=CARTESIAN_POINT('Ctrl Pts',(-2.74502660058381,0.0162318611108275,
12.5049254088044));
#433098=CARTESIAN_POINT('Ctrl Pts',(-2.73598532022336,0.00235138034619827,
12.5369868989719));
#433099=CARTESIAN_POINT('Ctrl Pts',(-2.73685230015164,0.00201072366463625,
12.5342545179733));
#433100=CARTESIAN_POINT('Ctrl Pts',(-2.73772532660293,0.00180172144282968,
12.5314872231885));
#433101=CARTESIAN_POINT('Ctrl Pts',(-2.73856823552727,0.0017905118314122,
12.5287124745063));
#433102=CARTESIAN_POINT('Ctrl Pts',(-2.73932841263351,0.00178040244744051,
12.5262100684184));
#433103=CARTESIAN_POINT('Ctrl Pts',(-2.74006334023772,0.00193215802165255,
12.5237004536639));
#433104=CARTESIAN_POINT('Ctrl Pts',(-2.74077223186921,0.00231330527171363,
12.5212220730815));
#433105=CARTESIAN_POINT('Ctrl Pts',(-2.74131494973713,0.00260510646350231,
12.5193246583486));
#433106=CARTESIAN_POINT('Ctrl Pts',(-2.74184859306926,0.00303540568168749,
12.517417831369));
#433107=CARTESIAN_POINT('Ctrl Pts',(-2.74232826407684,0.00369044799174734,
12.5155812248348));
#433108=CARTESIAN_POINT('Ctrl Pts',(-2.74253260650432,0.00396949953670413,
12.5147988205794));
#433109=CARTESIAN_POINT('Ctrl Pts',(-2.74272758494536,0.00428945719681405,
12.5140295443047));
#433110=CARTESIAN_POINT('Ctrl Pts',(-2.74291185437362,0.00465691812078847,
12.5132817086137));
#433111=CARTESIAN_POINT('Ctrl Pts',(-2.74319072122587,0.00521302052023,
12.5121499604604));
#433112=CARTESIAN_POINT('Ctrl Pts',(-2.74344469052441,0.00589313279938605,
12.5110494206568));
#433113=CARTESIAN_POINT('Ctrl Pts',(-2.74364492177948,0.00672081604688685,
12.5100666561695));
#433114=CARTESIAN_POINT('Ctrl Pts',(-2.74375989410505,0.00719606986161615,
12.5095023550641));
#433115=CARTESIAN_POINT('Ctrl Pts',(-2.74385784279182,0.00772562287140146,
12.5089719619137));
#433116=CARTESIAN_POINT('Ctrl Pts',(-2.74393065145121,0.00830071085255689,
12.5085043804652));
#433117=CARTESIAN_POINT('Ctrl Pts',(-2.74403719744023,0.00914227720249921,
12.5078201359221));
#433118=CARTESIAN_POINT('Ctrl Pts',(-2.74409179924932,0.0101059144034801,
12.5072563000949));
#433119=CARTESIAN_POINT('Ctrl Pts',(-2.74408230323968,0.0111267810021032,
12.5068768744332));
#433120=CARTESIAN_POINT('Ctrl Pts',(-2.74407545596303,0.0118628960964068,
12.5066032824114));
#433121=CARTESIAN_POINT('Ctrl Pts',(-2.74403522140716,0.0126417000519628,
12.5064197834844));
#433122=CARTESIAN_POINT('Ctrl Pts',(-2.74396642778918,0.0134198357955237,
12.5063282718343));
#433123=CARTESIAN_POINT('Ctrl Pts',(-2.7438660104049,0.0145556730763847,
12.5061946931565));
#433124=CARTESIAN_POINT('Ctrl Pts',(-2.74370365410164,0.0157144573146118,
12.5062515701262));
#433125=CARTESIAN_POINT('Ctrl Pts',(-2.74350474993816,0.0168264180839142,
12.5064436508398));
#433126=CARTESIAN_POINT('',(-2.67589590165752,0.0432362977156397,12.5737548217797));
#433127=CARTESIAN_POINT('Origin',(-2.69145022058562,0.0434876195863907,
12.5893111709658));
#433128=CARTESIAN_POINT('Ctrl Pts',(-2.74350474993816,0.0168264180839145,
12.5064436508398));
#433129=CARTESIAN_POINT('Ctrl Pts',(-2.733497058684,0.0207362139242025,
12.5164271754438));
#433130=CARTESIAN_POINT('Ctrl Pts',(-2.72348532435284,0.0246473649955796,
12.5264061185523));
#433131=CARTESIAN_POINT('Ctrl Pts',(-2.71346940489532,0.0285599199097525,
12.536380305637));
#433132=CARTESIAN_POINT('Ctrl Pts',(-2.70095153702076,0.033449820000828,
12.5488460165097));
#433133=CARTESIAN_POINT('Ctrl Pts',(-2.68842712830146,0.0383419143063837,
12.5613043021964));
#433134=CARTESIAN_POINT('Ctrl Pts',(-2.67589590165752,0.0432362977156394,
12.5737548217797));
#433135=CARTESIAN_POINT('Ctrl Pts',(-2.68211016738736,0.0864598836326288,
12.5893111709658));
#433136=CARTESIAN_POINT('Ctrl Pts',(-2.6717391495482,0.0818881636565727,
12.5770542771492));
#433137=CARTESIAN_POINT('Ctrl Pts',(-2.67543256678469,0.0659456938362415,
12.5737548217797));
#433138=CARTESIAN_POINT('Ctrl Pts',(-2.67243409794577,0.0821945086576885,
12.5928319619712));
#433139=CARTESIAN_POINT('Ctrl Pts',(-2.66677819194253,0.0761410680117523,
12.5821634970842));
#433140=CARTESIAN_POINT('Ctrl Pts',(-2.67190400159415,0.0644005578986747,
12.5773203894503));
#433141=CARTESIAN_POINT('Ctrl Pts',(-2.66132169167018,0.06966061356854,
12.5969440695591));
#433142=CARTESIAN_POINT('Ctrl Pts',(-2.66138541786341,0.0656413497647797,
12.5878292599214));
#433143=CARTESIAN_POINT('Ctrl Pts',(-2.66794484417248,0.0599318646212225,
12.5813877129824));
#433144=CARTESIAN_POINT('Ctrl Pts',(-2.66189191156417,0.0390689464872274,
12.596957478804));
#433145=CARTESIAN_POINT('Ctrl Pts',(-2.66182873647298,0.0430585081243937,
12.5878468778671));
#433146=CARTESIAN_POINT('Ctrl Pts',(-2.66815489785834,0.0489827940783303,
12.5814011370086));
#433147=CARTESIAN_POINT('Ctrl Pts',(-2.67354840376738,0.0268843169624308,
12.5928371701607));
#433148=CARTESIAN_POINT('Ctrl Pts',(-2.66765877691286,0.0327021654666717,
12.5821692192952));
#433149=CARTESIAN_POINT('Ctrl Pts',(-2.67229567989076,0.0446404631988242,
12.5773318885715));
#433150=CARTESIAN_POINT('Ctrl Pts',(-2.68340468995256,0.0230115497282627,
12.5893111709658));
#433151=CARTESIAN_POINT('Ctrl Pts',(-2.67285582888755,0.0271564459622794,
12.5770542771492));
#433152=CARTESIAN_POINT('Ctrl Pts',(-2.6758959016575,0.0432362977155884,
12.5737548217797));
#433153=CARTESIAN_POINT('',(-2.67543256678469,0.0659456938362415,12.5737548217797));
#433154=CARTESIAN_POINT('Origin',(-2.69098419246214,0.0663290197919444,
12.5893111709658));
#433155=CARTESIAN_POINT('Ctrl Pts',(-2.6758959016575,0.0432362977155884,
12.5737548217797));
#433156=CARTESIAN_POINT('Ctrl Pts',(-2.67495170595959,0.0435721758409372,
12.5746934679442));
#433157=CARTESIAN_POINT('Ctrl Pts',(-2.67396828568517,0.044116436809687,
12.5756680099006));
#433158=CARTESIAN_POINT('Ctrl Pts',(-2.67305591365844,0.0448042456151264,
12.5765688348656));
#433159=CARTESIAN_POINT('Ctrl Pts',(-2.67281437326466,0.0449863353820681,
12.5768073183026));
#433160=CARTESIAN_POINT('Ctrl Pts',(-2.67257771226814,0.0451782491723921,
12.5770407398754));
#433161=CARTESIAN_POINT('Ctrl Pts',(-2.67234763408338,0.0453783370825612,
12.5772674179684));
#433162=CARTESIAN_POINT('Ctrl Pts',(-2.67140345542886,0.0461994437598534,
12.5781976435658));
#433163=CARTESIAN_POINT('Ctrl Pts',(-2.67052391028091,0.0472133558938664,
12.5790594849312));
#433164=CARTESIAN_POINT('Ctrl Pts',(-2.66980486389765,0.0483832554717753,
12.5797571720116));
#433165=CARTESIAN_POINT('Ctrl Pts',(-2.66933637932435,0.0491454871126227,
12.580211740231));
#433166=CARTESIAN_POINT('Ctrl Pts',(-2.66893072961081,0.0500184048007455,
12.5806009430798));
#433167=CARTESIAN_POINT('Ctrl Pts',(-2.66863253735736,0.0509480251771897,
12.5808812374708));
#433168=CARTESIAN_POINT('Ctrl Pts',(-2.66837629128739,0.0517468774789039,
12.5811221033394));
#433169=CARTESIAN_POINT('Ctrl Pts',(-2.66819425992894,0.0526039914370422,
12.581287365893));
#433170=CARTESIAN_POINT('Ctrl Pts',(-2.6681048734992,0.0534727223215106,
12.581359338449));
#433171=CARTESIAN_POINT('Ctrl Pts',(-2.66809245063123,0.0535934579758461,
12.5813693411482));
#433172=CARTESIAN_POINT('Ctrl Pts',(-2.66808175902388,0.0537144320875003,
12.5813775999465));
#433173=CARTESIAN_POINT('Ctrl Pts',(-2.66807278879257,0.0538355349142049,
12.5813841266931));
#433174=CARTESIAN_POINT('Ctrl Pts',(-2.66805756971023,0.0540410005067911,
12.5813952001081));
#433175=CARTESIAN_POINT('Ctrl Pts',(-2.66804781092558,0.0542482576954088,
12.5814007534795));
#433176=CARTESIAN_POINT('Ctrl Pts',(-2.66804371368044,0.0544572254882118,
12.5814005856065));
#433177=CARTESIAN_POINT('Ctrl Pts',(-2.66802495809412,0.0554137983425526,
12.5813998171494));
#433178=CARTESIAN_POINT('Ctrl Pts',(-2.66812579569502,0.0563401176065905,
12.58127954464));
#433179=CARTESIAN_POINT('Ctrl Pts',(-2.66831623841059,0.0572341263756829,
12.5810700125799));
#433180=CARTESIAN_POINT('Ctrl Pts',(-2.66854627152736,0.0583139871776976,
12.5808169217085));
#433181=CARTESIAN_POINT('Ctrl Pts',(-2.66892342704989,0.0593433180629238,
12.5804173076348));
#433182=CARTESIAN_POINT('Ctrl Pts',(-2.66939019910842,0.0602408698514211,
12.5799304713245));
#433183=CARTESIAN_POINT('Ctrl Pts',(-2.66996867673729,0.0613532192753413,
12.5793271277669));
#433184=CARTESIAN_POINT('Ctrl Pts',(-2.670692112498,0.0623470268565772,
12.5785808224116));
#433185=CARTESIAN_POINT('Ctrl Pts',(-2.67150436979799,0.0631990679011367,
12.5777485681082));
#433186=CARTESIAN_POINT('Ctrl Pts',(-2.67271472216441,0.0644687024055957,
12.576508418016));
#433187=CARTESIAN_POINT('Ctrl Pts',(-2.67410713064052,0.0654176060605656,
12.5750928681475));
#433188=CARTESIAN_POINT('Ctrl Pts',(-2.67543256678469,0.0659456938362415,
12.5737548217797));
#433189=CARTESIAN_POINT('Ctrl Pts',(-2.67543256678469,0.0659456938362415,
12.5737548217797));
#433190=CARTESIAN_POINT('Ctrl Pts',(-2.6717391495482,0.0818881636565725,
12.5770542771492));
#433191=CARTESIAN_POINT('Ctrl Pts',(-2.68211016738736,0.0864598836326287,
12.5893111709658));
#433192=CARTESIAN_POINT('Ctrl Pts',(-2.69810843878968,0.0758865078362841,
12.5508408821982));
#433193=CARTESIAN_POINT('Ctrl Pts',(-2.69440044718258,0.0918776467222681,
12.55409748406));
#433194=CARTESIAN_POINT('Ctrl Pts',(-2.70478469578434,0.0964551990421396,
12.5663972313419));
#433195=CARTESIAN_POINT('Ctrl Pts',(-2.72076168574913,0.0858186911806309,
12.52790050457));
#433196=CARTESIAN_POINT('Ctrl Pts',(-2.71701834303816,0.101847997550193,
12.5311362602938));
#433197=CARTESIAN_POINT('Ctrl Pts',(-2.7274363493081,0.106440430820861,
12.5434568539655));
#433198=CARTESIAN_POINT('Ctrl Pts',(-2.74339406035942,0.0957429272648899,
12.5049357605811));
#433199=CARTESIAN_POINT('Ctrl Pts',(-2.73959736152855,0.111801210578403,
12.5081700652078));
#433200=CARTESIAN_POINT('Ctrl Pts',(-2.75006691952333,0.116416368720788,
12.5204921097672));
#433201=CARTESIAN_POINT('Ctrl Pts',(-2.74190792928895,0.0950912644753132,
12.5064436508395));
#433202=CARTESIAN_POINT('Ctrl Pts',(-2.74207361102238,0.0963001471634963,
12.5062361689309));
#433203=CARTESIAN_POINT('Ctrl Pts',(-2.742194357024,0.0975643512702508,
12.5061871075061));
#433204=CARTESIAN_POINT('Ctrl Pts',(-2.74224227203065,0.0987926512308685,
12.5063648335164));
#433205=CARTESIAN_POINT('Ctrl Pts',(-2.74226403798219,0.099350620837665,
12.5064455676329));
#433206=CARTESIAN_POINT('Ctrl Pts',(-2.74227085843297,0.0999089725951846,
12.506574497099));
#433207=CARTESIAN_POINT('Ctrl Pts',(-2.74226139007168,0.100443778891512,
12.5067492519495));
#433208=CARTESIAN_POINT('Ctrl Pts',(-2.74224236303213,0.101518492903706,
12.5071004286051));
#433209=CARTESIAN_POINT('Ctrl Pts',(-2.74215605014434,0.102537623639935,
12.5076537929613));
#433210=CARTESIAN_POINT('Ctrl Pts',(-2.74201835435008,0.103425478197055,
12.5083435010505));
#433211=CARTESIAN_POINT('Ctrl Pts',(-2.74200968557695,0.10348137394728,
12.5083869222964));
#433212=CARTESIAN_POINT('Ctrl Pts',(-2.74200080041076,0.103536753656767,
12.5084308732337));
#433213=CARTESIAN_POINT('Ctrl Pts',(-2.74199169775787,0.103591600550636,
12.5084753333615));
#433214=CARTESIAN_POINT('Ctrl Pts',(-2.74191868246723,0.10403154503076,
12.5088319622689));
#433215=CARTESIAN_POINT('Ctrl Pts',(-2.74183146408406,0.104446350132662,
12.509227847131));
#433216=CARTESIAN_POINT('Ctrl Pts',(-2.74173537620196,0.104824257689328,
12.5096423454524));
#433217=CARTESIAN_POINT('Ctrl Pts',(-2.74143427930616,0.106008452717044,
12.5109411997424));
#433218=CARTESIAN_POINT('Ctrl Pts',(-2.74103694226181,0.106905562165694,
12.5124831113042));
#433219=CARTESIAN_POINT('Ctrl Pts',(-2.74060720345451,0.107585446738974,
12.5140723025008));
#433220=CARTESIAN_POINT('Ctrl Pts',(-2.74056693645759,0.107649152668145,
12.5142212114565));
#433221=CARTESIAN_POINT('Ctrl Pts',(-2.74052639599032,0.107710978868737,
12.5143705582413));
#433222=CARTESIAN_POINT('Ctrl Pts',(-2.74048564229798,0.107770997937223,
12.5145201959299));
#433223=CARTESIAN_POINT('Ctrl Pts',(-2.73996210044397,0.108542032230993,
12.5164425148273));
#433224=CARTESIAN_POINT('Ctrl Pts',(-2.73939431493446,0.109047282064788,
12.5184635205941));
#433225=CARTESIAN_POINT('Ctrl Pts',(-2.73879962913225,0.109375275323014,
12.5205025929157));
#433226=CARTESIAN_POINT('Ctrl Pts',(-2.73845468779583,0.109565524413223,
12.5216853356836));
#433227=CARTESIAN_POINT('Ctrl Pts',(-2.73810155260303,0.109696215997301,
12.5228750347131));
#433228=CARTESIAN_POINT('Ctrl Pts',(-2.73774934548699,0.109783152732733,
12.5240609649613));
#433229=CARTESIAN_POINT('Ctrl Pts',(-2.73688487201596,0.109996534285856,
12.5269717671326));
#433230=CARTESIAN_POINT('Ctrl Pts',(-2.73599916853119,0.109942235803077,
12.5299036066169));
#433231=CARTESIAN_POINT('Ctrl Pts',(-2.73510090845922,0.10970647963823,
12.5328133004019));
#433232=CARTESIAN_POINT('Ctrl Pts',(-2.73466969132056,0.109593302951431,
12.5342101228451));
#433233=CARTESIAN_POINT('Ctrl Pts',(-2.7342362515214,0.109437942573048,
12.5356023438238));
#433234=CARTESIAN_POINT('Ctrl Pts',(-2.73380434092628,0.109247549171216,
12.5369868989719));
#433235=CARTESIAN_POINT('Origin',(-14.394554771405,5.25529295237477,-1.24053018555564));
#433236=CARTESIAN_POINT('Ctrl Pts',(-2.73594640652385,0.00236662780252761,
12.5369868989719));
#433237=CARTESIAN_POINT('Ctrl Pts',(-2.75023346270574,-0.00321578469936245,
12.5369868989719));
#433238=CARTESIAN_POINT('Ctrl Pts',(-2.74993564242795,-0.0185518404754673,
12.5369868989719));
#433239=CARTESIAN_POINT('Ctrl Pts',(-2.74077596617979,0.000479492378690292,
12.5218025310016));
#433240=CARTESIAN_POINT('Ctrl Pts',(-2.75013377681806,-0.00673765690360874,
12.5216901060418));
#433241=CARTESIAN_POINT('Ctrl Pts',(-2.7499365667715,-0.0185050914151908,
12.5161920673678));
#433242=CARTESIAN_POINT('Ctrl Pts',(-2.74583299118687,0.0037601278770949,
12.5042015548894));
#433243=CARTESIAN_POINT('Ctrl Pts',(-2.75010797448188,-0.00104631184936697,
12.4980677368513));
#433244=CARTESIAN_POINT('Ctrl Pts',(-2.75009928807058,-0.00784268619677183,
12.4907278922777));
#433245=CARTESIAN_POINT('Ctrl Pts',(-2.74348474923167,0.0168262954263408,
12.506463626192));
#433246=CARTESIAN_POINT('Ctrl Pts',(-2.75002736553977,0.0168664224927999,
12.4999376786891));
#433247=CARTESIAN_POINT('Ctrl Pts',(-2.74994745699453,0.0168659323990281,
12.4906970594712));
#433248=CARTESIAN_POINT('Origin',(-2.72793978959033,-0.0181246895118802,
12.5369868989719));
#433249=CARTESIAN_POINT('Origin',(-2.72793978959033,-0.0181246895118802,
14.));
#433250=CARTESIAN_POINT('Origin',(-2.72793978959033,-0.0181246895118801,
13.7435492065112));
#433251=CARTESIAN_POINT('Ctrl Pts',(-2.71294032762559,0.0114062721215966,
13.793642941384));
#433252=CARTESIAN_POINT('Ctrl Pts',(-2.72301360444854,0.00747749202417046,
13.8071662555867));
#433253=CARTESIAN_POINT('Ctrl Pts',(-2.71922551300471,-0.00912581327471074,
13.8103758687955));
#433254=CARTESIAN_POINT('Ctrl Pts',(-2.72841011328307,0.00532783178425798,
13.7804579775006));
#433255=CARTESIAN_POINT('Ctrl Pts',(-2.74083594162536,0.000470624589080533,
13.7901904343351));
#433256=CARTESIAN_POINT('Ctrl Pts',(-2.73986275664679,-0.0152554313424525,
13.7927914348263));
#433257=CARTESIAN_POINT('Ctrl Pts',(-2.73751775827926,0.00174922516482727,
13.7597120340895));
#433258=CARTESIAN_POINT('Ctrl Pts',(-2.7518958547537,-0.00387726856962336,
13.7635825532445));
#433259=CARTESIAN_POINT('Ctrl Pts',(-2.75202523739173,-0.0188945644739232,
13.7651073818884));
#433260=CARTESIAN_POINT('Ctrl Pts',(-2.73573427284735,0.00244999828093495,
13.7381884353898));
#433261=CARTESIAN_POINT('Ctrl Pts',(-2.74977615073385,-0.00304395985931783,
13.7368803041982));
#433262=CARTESIAN_POINT('Ctrl Pts',(-2.74964332058253,-0.0181823875606896,
13.7363986145813));
#433263=CARTESIAN_POINT('Origin',(-2.70864852252747,-0.0105446958324261,
13.7902182540695));
#433264=CARTESIAN_POINT('Ctrl Pts',(-2.68340102613533,0.0230129885130929,
13.8235227101244));
#433265=CARTESIAN_POINT('Ctrl Pts',(-2.69410332260474,0.0188125672722698,
13.8358800583119));
#433266=CARTESIAN_POINT('Ctrl Pts',(-2.69091550151957,0.00255022285992592,
13.8390832900376));
#433267=CARTESIAN_POINT('Ctrl Pts',(-2.69450238741364,0.0186510019172073,
13.8124254819052));
#433268=CARTESIAN_POINT('Ctrl Pts',(-2.70522546748948,0.0144424232589427,
13.8247886449157));
#433269=CARTESIAN_POINT('Ctrl Pts',(-2.70201689249565,-0.00183719060661301,
13.8279860620657));
#433270=CARTESIAN_POINT('Ctrl Pts',(-2.70559877342302,0.0142909702218092,
13.8013225099955));
#433271=CARTESIAN_POINT('Ctrl Pts',(-2.71633757826577,0.0100762217854295,
13.8136962257787));
#433272=CARTESIAN_POINT('Ctrl Pts',(-2.71311324370024,-0.00622232083317992,
13.8168830918626));
#433273=CARTESIAN_POINT('Ctrl Pts',(-2.71669037774349,0.00993281736474199,
13.7902140179785));
#433274=CARTESIAN_POINT('Ctrl Pts',(-2.72744017914498,0.00571375688009667,
13.802602731458));
#433275=CARTESIAN_POINT('Ctrl Pts',(-2.72420475383462,-0.0106052558223468,
13.8057746032558));
#433276=CARTESIAN_POINT('Origin',(-2.67535915931955,0.00253547987023609,
13.8235269408515));
#433277=CARTESIAN_POINT('Ctrl Pts',(-2.68211016738736,0.0864598836326288,
13.8235269408515));
#433278=CARTESIAN_POINT('Ctrl Pts',(-2.69291447656381,0.0912226057545551,
13.8362179249168));
#433279=CARTESIAN_POINT('Ctrl Pts',(-2.68864404095394,0.107758215321761,
13.8391868794938));
#433280=CARTESIAN_POINT('Ctrl Pts',(-2.67222469477449,0.0821022002000186,
13.8400110824519));
#433281=CARTESIAN_POINT('Ctrl Pts',(-2.67950719727548,0.0890510864549605,
13.8494522556836));
#433282=CARTESIAN_POINT('Ctrl Pts',(-2.67242066461126,0.100483887609305,
13.85569149686));
#433283=CARTESIAN_POINT('Ctrl Pts',(-2.66131406909561,0.0700044329126074,
13.8586819406588));
#433284=CARTESIAN_POINT('Ctrl Pts',(-2.66123916256485,0.0743576423776596,
13.868010383617));
#433285=CARTESIAN_POINT('Ctrl Pts',(-2.65441722899596,0.0803035728493568,
13.8744918421245));
#433286=CARTESIAN_POINT('Ctrl Pts',(-2.661899633748,0.0387197943181669,
13.8587686893867));
#433287=CARTESIAN_POINT('Ctrl Pts',(-2.66197381731131,0.0344053274080189,
13.8680909899357));
#433288=CARTESIAN_POINT('Ctrl Pts',(-2.65539459466576,0.0282238849480537,
13.8745789365163));
#433289=CARTESIAN_POINT('Ctrl Pts',(-2.67333333842744,0.02696882119832,
13.8400379222776));
#433290=CARTESIAN_POINT('Ctrl Pts',(-2.68088656118302,0.0203190798565372,
13.8494748685453));
#433291=CARTESIAN_POINT('Ctrl Pts',(-2.67427628338526,0.00861158940378663,
13.8557104837033));
#433292=CARTESIAN_POINT('Ctrl Pts',(-2.68340468995004,0.0230115497222156,
13.8235269408542));
#433293=CARTESIAN_POINT('Ctrl Pts',(-2.69439427247443,0.0186934836354026,
13.8362179249195));
#433294=CARTESIAN_POINT('Ctrl Pts',(-2.69080185485773,0.00199744998295956,
13.8391868794965));
#433295=CARTESIAN_POINT('Origin',(-2.67323614231258,0.106590747473313,13.8235269408515));
#433296=CARTESIAN_POINT('Ctrl Pts',(-2.7148346970873,0.100885410333076,
13.7902140241682));
#433297=CARTESIAN_POINT('Ctrl Pts',(-2.72540345615365,0.105539433022133,
13.8026027327198));
#433298=CARTESIAN_POINT('Ctrl Pts',(-2.72150509546337,0.121712890172733,
13.8057746032556));
#433299=CARTESIAN_POINT('Ctrl Pts',(-2.70393008609646,0.0960784734746837,
13.8013225161808));
#433300=CARTESIAN_POINT('Ctrl Pts',(-2.71448803364637,0.10072773916065,
13.8136962270464));
#433301=CARTESIAN_POINT('Ctrl Pts',(-2.71060158941156,0.116881195649068,
13.8168830918628));
#433302=CARTESIAN_POINT('Ctrl Pts',(-2.69302077402973,0.0912694643025583,
13.8124254880875));
#433303=CARTESIAN_POINT('Ctrl Pts',(-2.70356326156808,0.0959119239463373,
13.8247886461868));
#433304=CARTESIAN_POINT('Ctrl Pts',(-2.69969333585972,0.112047110254848,
13.8279860620656));
#433305=CARTESIAN_POINT('Ctrl Pts',(-2.68210657056909,0.0864582989213033,
13.8235227163065));
#433306=CARTESIAN_POINT('Ctrl Pts',(-2.69262862454384,0.0910917601965746,
13.8358800595847));
#433307=CARTESIAN_POINT('Ctrl Pts',(-2.68878013986014,0.107210537955378,
13.8390832900376));
#433308=CARTESIAN_POINT('Origin',(-2.70596428021828,0.121017863901323,13.7902182540695));
#433309=CARTESIAN_POINT('Ctrl Pts',(-2.73355739739318,0.109138722433136,
13.7382347919292));
#433310=CARTESIAN_POINT('Ctrl Pts',(-2.74737529950942,0.115203658528389,
13.7369371795942));
#433311=CARTESIAN_POINT('Ctrl Pts',(-2.74661624889214,0.130335334548605,
13.7364597369711));
#433312=CARTESIAN_POINT('Ctrl Pts',(-2.73528824795873,0.109901710181357,
13.7595490285574));
#433313=CARTESIAN_POINT('Ctrl Pts',(-2.74943542928561,0.116112271099933,
13.7633824266926));
#433314=CARTESIAN_POINT('Ctrl Pts',(-2.74893845672435,0.131133811586217,
13.7648920890506));
#433315=CARTESIAN_POINT('Ctrl Pts',(-2.72646100490131,0.10601051445799,
13.780380659011));
#433316=CARTESIAN_POINT('Ctrl Pts',(-2.73869998040111,0.111377484247306,
13.7901039518744));
#433317=CARTESIAN_POINT('Ctrl Pts',(-2.73710079484676,0.127059577442688,
13.7926933640892));
#433318=CARTESIAN_POINT('Ctrl Pts',(-2.71111728594794,0.0992467477371861,
13.7936647693663));
#433319=CARTESIAN_POINT('Ctrl Pts',(-2.72102587318337,0.103581863761312,
13.8072068914933));
#433320=CARTESIAN_POINT('Ctrl Pts',(-2.71654871810667,0.120031768085242,
13.8104111085397));
#433321=CARTESIAN_POINT('Origin',(-2.7249303158515,0.1293784130119,13.7435492065112));
#433322=CARTESIAN_POINT('Origin',(-2.7249303158515,0.1293784130119,14.));
#433323=CARTESIAN_POINT('Origin',(-2.7249303158515,0.1293784130119,12.5369868989719));
#433324=CARTESIAN_POINT('Ctrl Pts',(-2.74188955709783,0.0950906273046976,
12.506462012331));
#433325=CARTESIAN_POINT('Ctrl Pts',(-2.74842425126575,0.0953172550206331,
12.4999388158272));
#433326=CARTESIAN_POINT('Ctrl Pts',(-2.74834693726402,0.0953145737175499,
12.4907030323752));
#433327=CARTESIAN_POINT('Ctrl Pts',(-2.74370084999371,0.108241589292313,
12.5042014951932));
#433328=CARTESIAN_POINT('Ctrl Pts',(-2.74777518131633,0.113215613959498,
12.4980716682127));
#433329=CARTESIAN_POINT('Ctrl Pts',(-2.74749105734251,0.120001248697188,
12.4907355092743));
#433330=CARTESIAN_POINT('Ctrl Pts',(-2.73851615822091,0.111314807876567,
12.5218047446509));
#433331=CARTESIAN_POINT('Ctrl Pts',(-2.74756663884357,0.11890477964432,
12.5216906929434));
#433332=CARTESIAN_POINT('Ctrl Pts',(-2.74689368091139,0.130648624072426,
12.5161988840776));
#433333=CARTESIAN_POINT('Ctrl Pts',(-2.73376917514574,0.10923208415584,
12.5369868989719));
#433334=CARTESIAN_POINT('Ctrl Pts',(-2.7478074027806,0.115391117878143,
12.5369868989719));
#433335=CARTESIAN_POINT('Ctrl Pts',(-2.746890969463,0.130693590929748,12.5369868989719));
#433336=CARTESIAN_POINT('Origin',(-5.15079064385546E-31,-5.04677213932918E-31,
12.5));
#433337=CARTESIAN_POINT('Origin',(-2.68023295023435,-0.132444682635759,
12.5));
#433338=CARTESIAN_POINT('',(-2.68023295023435,-0.132444682635759,12.5893111709658));
#433339=CARTESIAN_POINT('',(-2.68023295023435,-0.132444682635759,13.8235269408515));
#433340=CARTESIAN_POINT('',(-2.68023295023435,-0.132444682635759,12.5));
#433341=CARTESIAN_POINT('',(-2.71402813188475,-0.120733218320032,13.7902182540695));
#433342=CARTESIAN_POINT('',(-2.68023295023435,-0.132444682635759,13.8235269408515));
#433343=CARTESIAN_POINT('',(-2.73361252196705,-0.113946396223116,13.7435492065112));
#433344=CARTESIAN_POINT('Origin',(-2.66918024413258,-0.136275259008993,
13.7445212918717));
#433345=CARTESIAN_POINT('',(-2.73361252196705,-0.113946396223116,12.5369868989719));
#433346=CARTESIAN_POINT('',(-2.73361252196705,-0.113946396223116,12.5));
#433347=CARTESIAN_POINT('Ctrl Pts',(-2.73361252196705,-0.113946396223116,
12.5369868989719));
#433348=CARTESIAN_POINT('Ctrl Pts',(-2.71583230866048,-0.120107994518991,
12.5544431401645));
#433349=CARTESIAN_POINT('Ctrl Pts',(-2.69803937847279,-0.126273999753732,
12.5718848856037));
#433350=CARTESIAN_POINT('Ctrl Pts',(-2.68023295023435,-0.132444682635759,
12.5893111709658));
#433351=CARTESIAN_POINT('Origin',(-2.92325343698282,-0.316884282769413,
12.5));
#433352=CARTESIAN_POINT('',(-2.72707321410059,-0.220664646924619,13.7435492065112));
#433353=CARTESIAN_POINT('',(-2.70846397699157,-0.211537457691819,13.7902182540695));
#433354=CARTESIAN_POINT('Origin',(-2.65956211819432,-0.187552781884673,
13.7418732680455));
#433355=CARTESIAN_POINT('',(-2.67635153714374,-0.195787413049954,13.8235269408515));
#433356=CARTESIAN_POINT('',(-2.70846397699157,-0.211537457691819,13.7902182540695));
#433357=CARTESIAN_POINT('',(-2.67635153714374,-0.195787413049954,12.5893111709658));
#433358=CARTESIAN_POINT('',(-2.67635153714374,-0.195787413049954,12.5));
#433359=CARTESIAN_POINT('',(-2.72707321410059,-0.220664646924619,12.5369868989719));
#433360=CARTESIAN_POINT('Ctrl Pts',(-2.67635153714374,-0.195787413049954,
12.5893111709658));
#433361=CARTESIAN_POINT('Ctrl Pts',(-2.69327134132254,-0.204085993675111,
12.5718848856037));
#433362=CARTESIAN_POINT('Ctrl Pts',(-2.71017831955037,-0.212378283613504,
12.5544431401645));
#433363=CARTESIAN_POINT('Ctrl Pts',(-2.72707321410059,-0.220664646924619,
12.5369868989719));
#433364=CARTESIAN_POINT('',(-2.72707321410059,-0.220664646924619,12.5));
#433365=CARTESIAN_POINT('Origin',(-2.69148864585867,-0.164924675570068,
12.5));
#433366=CARTESIAN_POINT('',(-2.65726540810591,-0.161705953790234,13.8587068136939));
#433367=CARTESIAN_POINT('Ctrl Pts',(-2.6763515371407,-0.195787413055823,
13.8235269408542));
#433368=CARTESIAN_POINT('Ctrl Pts',(-2.67477827973691,-0.195015784538633,
13.8262006681044));
#433369=CARTESIAN_POINT('Ctrl Pts',(-2.67324478715602,-0.194070147961288,
13.8288634856214));
#433370=CARTESIAN_POINT('Ctrl Pts',(-2.6717495304784,-0.192963749774365,
13.8314912288862));
#433371=CARTESIAN_POINT('Ctrl Pts',(-2.67020807507234,-0.191823167363328,
13.8342001611531));
#433372=CARTESIAN_POINT('Ctrl Pts',(-2.66870524708003,-0.190510868342892,
13.8368750301949));
#433373=CARTESIAN_POINT('Ctrl Pts',(-2.66724775704212,-0.18899694895694,
13.8394886372969));
#433374=CARTESIAN_POINT('Ctrl Pts',(-2.66713519155111,-0.188880025290508,
13.8396904925131));
#433375=CARTESIAN_POINT('Ctrl Pts',(-2.6670229095647,-0.188761881108905,
13.8398919674349));
#433376=CARTESIAN_POINT('Ctrl Pts',(-2.66691092171307,-0.188642494026079,
13.8400930404591));
#433377=CARTESIAN_POINT('Ctrl Pts',(-2.66516607564295,-0.186782362955953,
13.8432258934518));
#433378=CARTESIAN_POINT('Ctrl Pts',(-2.66350071538557,-0.184630770035319,
13.8462331177034));
#433379=CARTESIAN_POINT('Ctrl Pts',(-2.66204544089643,-0.182198843193322,
13.8489036603661));
#433380=CARTESIAN_POINT('Ctrl Pts',(-2.66156925814769,-0.181403088428862,
13.849777493004));
#433381=CARTESIAN_POINT('Ctrl Pts',(-2.66111579360245,-0.180577428158085,
13.85061494757));
#433382=CARTESIAN_POINT('Ctrl Pts',(-2.66069025957861,-0.179722574650084,
13.8514076489583));
#433383=CARTESIAN_POINT('Ctrl Pts',(-2.65979019374699,-0.177914436192341,
13.8530843267192));
#433384=CARTESIAN_POINT('Ctrl Pts',(-2.65892932231216,-0.175796767077549,
13.8546805203176));
#433385=CARTESIAN_POINT('Ctrl Pts',(-2.65828401049632,-0.173441091909396,
13.8559412814273));
#433386=CARTESIAN_POINT('Ctrl Pts',(-2.6581976468474,-0.173125826175534,
13.8561100121513));
#433387=CARTESIAN_POINT('Ctrl Pts',(-2.65811510082779,-0.172806360954155,
13.8562727473908));
#433388=CARTESIAN_POINT('Ctrl Pts',(-2.65803674495943,-0.17248292451895,
13.8564289040185));
#433389=CARTESIAN_POINT('Ctrl Pts',(-2.6576814019903,-0.171016143975212,
13.8571370725437));
#433390=CARTESIAN_POINT('Ctrl Pts',(-2.65740820067463,-0.169441373077321,
13.8577210840554));
#433391=CARTESIAN_POINT('Ctrl Pts',(-2.65725667651276,-0.167814806897733,
13.8581177131616));
#433392=CARTESIAN_POINT('Ctrl Pts',(-2.65721400209347,-0.167356709876862,
13.8582294175695));
#433393=CARTESIAN_POINT('Ctrl Pts',(-2.65718080866484,-0.166894555363562,
13.8583265086086));
#433394=CARTESIAN_POINT('Ctrl Pts',(-2.65715755142542,-0.166429699052326,
13.8584082369006));
#433395=CARTESIAN_POINT('Ctrl Pts',(-2.65712413700904,-0.165761825189217,
13.8585256585398));
#433396=CARTESIAN_POINT('Ctrl Pts',(-2.65711114037927,-0.165080054877154,
13.8586122832068));
#433397=CARTESIAN_POINT('Ctrl Pts',(-2.65711968869444,-0.16440208348179,
13.8586682984299));
#433398=CARTESIAN_POINT('Ctrl Pts',(-2.6571265264992,-0.163859773570642,
13.8587131050557));
#433399=CARTESIAN_POINT('Ctrl Pts',(-2.65714699071182,-0.163313901590444,
13.8587357943552));
#433400=CARTESIAN_POINT('Ctrl Pts',(-2.65718158985444,-0.162764421649494,
13.8587355499465));
#433401=CARTESIAN_POINT('Ctrl Pts',(-2.65720395210521,-0.162409279663444,
13.8587353919793));
#433402=CARTESIAN_POINT('Ctrl Pts',(-2.65723193858569,-0.162056468535203,
13.8587257282814));
#433403=CARTESIAN_POINT('Ctrl Pts',(-2.65726540810591,-0.161705953790234,
13.8587068136939));
#433404=CARTESIAN_POINT('Ctrl Pts',(-2.65726540810591,-0.161705953790234,
13.8587068136939));
#433405=CARTESIAN_POINT('Ctrl Pts',(-2.65737548753329,-0.160553129902586,
13.8586446046466));
#433406=CARTESIAN_POINT('Ctrl Pts',(-2.65754480484203,-0.159425114975678,
13.858482427929));
#433407=CARTESIAN_POINT('Ctrl Pts',(-2.65776899483064,-0.158320944139967,
13.8582284286032));
#433408=CARTESIAN_POINT('Ctrl Pts',(-2.65799898768009,-0.157188193304953,
13.8579678548414));
#433409=CARTESIAN_POINT('Ctrl Pts',(-2.65828879341816,-0.156078074645413,
13.857615680862));
#433410=CARTESIAN_POINT('Ctrl Pts',(-2.65861761120967,-0.155031906223266,
13.8571944833187));
#433411=CARTESIAN_POINT('Ctrl Pts',(-2.65943820963712,-0.152421085932469,
13.8561433417727));
#433412=CARTESIAN_POINT('Ctrl Pts',(-2.66053558659169,-0.150084985800373,
13.8546163505474));
#433413=CARTESIAN_POINT('Ctrl Pts',(-2.66171089288025,-0.148080323240879,
13.8528973491086));
#433414=CARTESIAN_POINT('Ctrl Pts',(-2.66192560399914,-0.147714100967296,
13.8525833129072));
#433415=CARTESIAN_POINT('Ctrl Pts',(-2.66214284081204,-0.147358820344133,
13.8522628768812));
#433416=CARTESIAN_POINT('Ctrl Pts',(-2.66236132074595,-0.147014662717974,
13.851937733538));
#433417=CARTESIAN_POINT('Ctrl Pts',(-2.66369554738961,-0.144912939844747,
13.8499521282529));
#433418=CARTESIAN_POINT('Ctrl Pts',(-2.66521217477356,-0.143019349316914,
13.847639871647));
#433419=CARTESIAN_POINT('Ctrl Pts',(-2.66676878738483,-0.141383187388737,
13.8452109780794));
#433420=CARTESIAN_POINT('Ctrl Pts',(-2.66746913961893,-0.140647044270379,
13.8441181685877));
#433421=CARTESIAN_POINT('Ctrl Pts',(-2.66817726917405,-0.139962368013835,
13.8430021611332));
#433422=CARTESIAN_POINT('Ctrl Pts',(-2.66887973530314,-0.139330373170678,
13.8418824960098));
#433423=CARTESIAN_POINT('Ctrl Pts',(-2.67053511467444,-0.13784106118422,
13.8392439765549));
#433424=CARTESIAN_POINT('Ctrl Pts',(-2.67223564827898,-0.136570293061481,
13.8364981347964));
#433425=CARTESIAN_POINT('Ctrl Pts',(-2.67396534887573,-0.135487295887676,
13.8336931113419));
#433426=CARTESIAN_POINT('Ctrl Pts',(-2.67564996741083,-0.134432525417069,
13.8309611966328));
#433427=CARTESIAN_POINT('Ctrl Pts',(-2.67736424002019,-0.133555286933089,
13.8281701127186));
#433428=CARTESIAN_POINT('Ctrl Pts',(-2.6791007054218,-0.132865766020628,
13.8253580685121));
#433429=CARTESIAN_POINT('Ctrl Pts',(-2.67947717299492,-0.132716277142651,
13.8247484142933));
#433430=CARTESIAN_POINT('Ctrl Pts',(-2.67985464701624,-0.132575780751616,
13.8241378483365));
#433431=CARTESIAN_POINT('Ctrl Pts',(-2.68023295023436,-0.132444682635759,
13.8235269408515));
#433432=CARTESIAN_POINT('',(-2.65717142069583,-0.162944478406341,12.5969504640361));
#433433=CARTESIAN_POINT('Origin',(-2.69152168130615,-0.164926503689338,
12.584524458991));
#433434=CARTESIAN_POINT('Origin',(-2.69152168130615,-0.164926503689338,
12.584524458991));
#433435=CARTESIAN_POINT('Ctrl Pts',(-2.67635153714374,-0.195787413049954,
12.5893111709658));
#433436=CARTESIAN_POINT('Ctrl Pts',(-2.66617562406611,-0.190796478508579,
12.5770542771492));
#433437=CARTESIAN_POINT('Ctrl Pts',(-2.67051623844065,-0.175017925288893,
12.5737548217797));
#433438=CARTESIAN_POINT('Ctrl Pts',(-2.69860284390658,-0.206700911884528,
12.5663937883685));
#433439=CARTESIAN_POINT('Ctrl Pts',(-2.68841395003863,-0.201703610713006,
12.5540940315304));
#433440=CARTESIAN_POINT('Ctrl Pts',(-2.69277111126456,-0.185877014699834,
12.5508374392248));
#433441=CARTESIAN_POINT('Ctrl Pts',(-2.72083169937371,-0.217603399132581,
12.5434499600945));
#433442=CARTESIAN_POINT('Ctrl Pts',(-2.71060967778341,-0.212589849955346,
12.5311293540533));
#433443=CARTESIAN_POINT('Ctrl Pts',(-2.71500372320481,-0.196726554919452,
12.5278936106989));
#433444=CARTESIAN_POINT('Ctrl Pts',(-2.74303986218576,-0.228495737346712,
12.5204817579905));
#433445=CARTESIAN_POINT('Ctrl Pts',(-2.73276724857437,-0.223457374527361,
12.5081597038247));
#433446=CARTESIAN_POINT('Ctrl Pts',(-2.73721579838891,-0.207567300599202,
12.5049254088044));
#433447=CARTESIAN_POINT('Ctrl Pts',(-2.72707321410058,-0.220664646924618,
12.5369868989719));
#433448=CARTESIAN_POINT('Ctrl Pts',(-2.72790954254262,-0.221074837011971,
12.5342545179733));
#433449=CARTESIAN_POINT('Ctrl Pts',(-2.72876262844905,-0.221354303556684,
12.5314872231885));
#433450=CARTESIAN_POINT('Ctrl Pts',(-2.72960181897609,-0.221434180771564,
12.5287124745063));
#433451=CARTESIAN_POINT('Ctrl Pts',(-2.73035864264708,-0.221506218008694,
12.5262100684184));
#433452=CARTESIAN_POINT('Ctrl Pts',(-2.73110349432844,-0.221414870811116,
12.5237004536639));
#433453=CARTESIAN_POINT('Ctrl Pts',(-2.73184109422079,-0.221092773046081,
12.5212220730815));
#433454=CARTESIAN_POINT('Ctrl Pts',(-2.73240579074586,-0.22084617934327,
12.5193246583486));
#433455=CARTESIAN_POINT('Ctrl Pts',(-2.7329727318048,-0.220460808795907,
12.517417831369));
#433456=CARTESIAN_POINT('Ctrl Pts',(-2.73350419877607,-0.219847043725262,
12.5155812248348));
#433457=CARTESIAN_POINT('Ctrl Pts',(-2.73373060656248,-0.219585576506165,
12.5147988205793));
#433458=CARTESIAN_POINT('Ctrl Pts',(-2.73395101574848,-0.219282576031812,
12.5140295443047));
#433459=CARTESIAN_POINT('Ctrl Pts',(-2.73416462351205,-0.218931357472827,
12.5132817086137));
#433460=CARTESIAN_POINT('Ctrl Pts',(-2.73448788996602,-0.218399835695578,
12.5121499604604));
#433461=CARTESIAN_POINT('Ctrl Pts',(-2.73479644966733,-0.217742687289853,
12.511049420657));
#433462=CARTESIAN_POINT('Ctrl Pts',(-2.73506347853791,-0.216934078796233,
12.5100666561697));
#433463=CARTESIAN_POINT('Ctrl Pts',(-2.73521680590049,-0.216469777661257,
12.5095023550643));
#433464=CARTESIAN_POINT('Ctrl Pts',(-2.73535759215747,-0.215949970422336,
12.5089719619137));
#433465=CARTESIAN_POINT('Ctrl Pts',(-2.73547703356137,-0.21538273058066,
12.5085043804652));
#433466=CARTESIAN_POINT('Ctrl Pts',(-2.73565182049765,-0.214552648960552,
12.5078201359221));
#433467=CARTESIAN_POINT('Ctrl Pts',(-2.73578478600157,-0.213596668737202,
12.5072563000949));
#433468=CARTESIAN_POINT('Ctrl Pts',(-2.73585853169418,-0.212578424975029,
12.5068768744332));
#433469=CARTESIAN_POINT('Ctrl Pts',(-2.73591170741522,-0.211844201126362,
12.5066032824114));
#433470=CARTESIAN_POINT('Ctrl Pts',(-2.73593508648895,-0.211064709086899,
12.5064197834844));
#433471=CARTESIAN_POINT('Ctrl Pts',(-2.73592994706302,-0.210283555207319,
12.5063282718343));
#433472=CARTESIAN_POINT('Ctrl Pts',(-2.73592244509229,-0.209143312382261,
12.5061946931565));
#433473=CARTESIAN_POINT('Ctrl Pts',(-2.73585508068928,-0.207975150357036,
12.5062515701262));
#433474=CARTESIAN_POINT('Ctrl Pts',(-2.73574747348863,-0.206850677009604,
12.5064436508398));
#433475=CARTESIAN_POINT('',(-2.67051623844065,-0.175017925288893,12.5737548217797));
#433476=CARTESIAN_POINT('Origin',(-2.68603928672129,-0.176035261062827,
12.5893111709658));
#433477=CARTESIAN_POINT('Ctrl Pts',(-2.73574747348863,-0.206850677009604,
12.5064436508398));
#433478=CARTESIAN_POINT('Ctrl Pts',(-2.72609176665931,-0.202138170948357,
12.5164271754438));
#433479=CARTESIAN_POINT('Ctrl Pts',(-2.7164321406699,-0.197423984617126,
12.5264061185523));
#433480=CARTESIAN_POINT('Ctrl Pts',(-2.706768457906,-0.192708057987618,
12.536380305637));
#433481=CARTESIAN_POINT('Ctrl Pts',(-2.69469081445718,-0.186814106193713,
12.5488460165097));
#433482=CARTESIAN_POINT('Ctrl Pts',(-2.6826068307766,-0.180917434346827,
12.5613043021964));
#433483=CARTESIAN_POINT('Ctrl Pts',(-2.67051623844065,-0.175017925288894,
12.5737548217797));
#433484=CARTESIAN_POINT('Ctrl Pts',(-2.68023295023435,-0.132444682635759,
12.5893111709658));
#433485=CARTESIAN_POINT('Ctrl Pts',(-2.66952380348168,-0.136155856357012,
12.5770542771492));
#433486=CARTESIAN_POINT('Ctrl Pts',(-2.67190547188397,-0.152346326716963,
12.5737548217797));
#433487=CARTESIAN_POINT('Ctrl Pts',(-2.67024140945735,-0.135907175439603,
12.5928319619712));
#433488=CARTESIAN_POINT('Ctrl Pts',(-2.66411091140471,-0.141479464915032,
12.5821634970842));
#433489=CARTESIAN_POINT('Ctrl Pts',(-2.66826270477977,-0.153598710521533,
12.5773203894503));
#433490=CARTESIAN_POINT('Ctrl Pts',(-2.65814434998816,-0.147493600752807,
12.5969440695591));
#433491=CARTESIAN_POINT('Ctrl Pts',(-2.6578802568247,-0.15150468506418,
12.5878292599214));
#433492=CARTESIAN_POINT('Ctrl Pts',(-2.66395248114037,-0.157729826505854,
12.5813877129824));
#433493=CARTESIAN_POINT('Ctrl Pts',(-2.65621916765618,-0.178029954800566,
12.596957478804));
#433494=CARTESIAN_POINT('Ctrl Pts',(-2.65648138908561,-0.174048518744211,
12.5878468778671));
#433495=CARTESIAN_POINT('Ctrl Pts',(-2.66326938499446,-0.168659586245191,
12.5814011370086));
#433496=CARTESIAN_POINT('Ctrl Pts',(-2.66684371342032,-0.191124153303934,
12.5928371701607));
#433497=CARTESIAN_POINT('Ctrl Pts',(-2.66144789247666,-0.18484560394538,
12.5821692192952));
#433498=CARTESIAN_POINT('Ctrl Pts',(-2.66704244863735,-0.173324980553701,
12.5773318885715));
#433499=CARTESIAN_POINT('Ctrl Pts',(-2.67635153714371,-0.195787413050002,
12.5893111709658));
#433500=CARTESIAN_POINT('Ctrl Pts',(-2.66617562406608,-0.190796478508627,
12.5770542771492));
#433501=CARTESIAN_POINT('Ctrl Pts',(-2.67051623844063,-0.175017925288943,
12.5737548217797));
#433502=CARTESIAN_POINT('',(-2.67190547188397,-0.152346326716963,12.5737548217797));
#433503=CARTESIAN_POINT('Origin',(-2.68743659543392,-0.153231878113717,
12.5893111709658));
#433504=CARTESIAN_POINT('Ctrl Pts',(-2.67051623844063,-0.175017925288943,
12.5737548217797));
#433505=CARTESIAN_POINT('Ctrl Pts',(-2.66960256166138,-0.174606204055485,
12.5746934679442));
#433506=CARTESIAN_POINT('Ctrl Pts',(-2.66866677595842,-0.17398359618822,
12.5756680099006));
#433507=CARTESIAN_POINT('Ctrl Pts',(-2.6678135025773,-0.173223709219617,
12.5765688348656));
#433508=CARTESIAN_POINT('Ctrl Pts',(-2.6675876078957,-0.173022537556906,
12.5768073183026));
#433509=CARTESIAN_POINT('Ctrl Pts',(-2.66736737712466,-0.172811972275615,
12.5770407398754));
#433510=CARTESIAN_POINT('Ctrl Pts',(-2.66715437352828,-0.172593796633459,
12.5772674179684));
#433511=CARTESIAN_POINT('Ctrl Pts',(-2.66628026436733,-0.171698462795228,
12.5781976435658));
#433512=CARTESIAN_POINT('Ctrl Pts',(-2.66548628908493,-0.170616233275343,
12.5790594849312));
#433513=CARTESIAN_POINT('Ctrl Pts',(-2.66486499294561,-0.169391617486232,
12.5797571720116));
#433514=CARTESIAN_POINT('Ctrl Pts',(-2.66446019617102,-0.168593736266367,
12.580211740231));
#433515=CARTESIAN_POINT('Ctrl Pts',(-2.6641270471188,-0.16769065892232,
12.5806009430798));
#433516=CARTESIAN_POINT('Ctrl Pts',(-2.66390561976632,-0.166739826344052,
12.5808812374708));
#433517=CARTESIAN_POINT('Ctrl Pts',(-2.66371534021279,-0.165922745723894,
12.5811221033394));
#433518=CARTESIAN_POINT('Ctrl Pts',(-2.66360377729331,-0.165053646496132,
12.581287365893));
#433519=CARTESIAN_POINT('Ctrl Pts',(-2.66358549792153,-0.164180520418168,
12.581359338449));
#433520=CARTESIAN_POINT('Ctrl Pts',(-2.66358295746631,-0.164059173922696,
12.5813693411482));
#433521=CARTESIAN_POINT('Ctrl Pts',(-2.66358216194757,-0.163937730877166,
12.5813775999465));
#433522=CARTESIAN_POINT('Ctrl Pts',(-2.66358309256861,-0.163816299853001,
12.5813841266931));
#433523=CARTESIAN_POINT('Ctrl Pts',(-2.66358467147975,-0.163610277433727,
12.5813952001081));
#433524=CARTESIAN_POINT('Ctrl Pts',(-2.66359183855161,-0.163402914444762,
12.5814007534795));
#433525=CARTESIAN_POINT('Ctrl Pts',(-2.66360478775479,-0.163194308011535,
12.5814005856065));
#433526=CARTESIAN_POINT('Ctrl Pts',(-2.66366406414415,-0.162239389320051,
12.5813998171494));
#433527=CARTESIAN_POINT('Ctrl Pts',(-2.6638400698358,-0.161324371507552,
12.58127954464));
#433528=CARTESIAN_POINT('Ctrl Pts',(-2.6641027488832,-0.160448860328191,
12.5810700125799));
#433529=CARTESIAN_POINT('Ctrl Pts',(-2.66442003526405,-0.159391342508453,
12.5808169217085));
#433530=CARTESIAN_POINT('Ctrl Pts',(-2.66487983585568,-0.158396178313262,
12.5804173076348));
#433531=CARTESIAN_POINT('Ctrl Pts',(-2.66541821357192,-0.157539659310368,
12.5799304713245));
#433532=CARTESIAN_POINT('Ctrl Pts',(-2.6660854331688,-0.156478162434471,
12.5793271277669));
#433533=CARTESIAN_POINT('Ctrl Pts',(-2.66688746630062,-0.155546628396526,
12.5785808224116));
#433534=CARTESIAN_POINT('Ctrl Pts',(-2.66776647013655,-0.154763628958832,
12.5777485681082));
#433535=CARTESIAN_POINT('Ctrl Pts',(-2.66907628215414,-0.153596874012674,
12.576508418016));
#433536=CARTESIAN_POINT('Ctrl Pts',(-2.67054140196298,-0.15276462197363,
12.5750928681475));
#433537=CARTESIAN_POINT('Ctrl Pts',(-2.67190547188397,-0.152346326716963,
12.5737548217797));
#433538=CARTESIAN_POINT('Ctrl Pts',(-2.67190547188397,-0.152346326716963,
12.5737548217797));
#433539=CARTESIAN_POINT('Ctrl Pts',(-2.66952380348168,-0.136155856357012,
12.5770542771492));
#433540=CARTESIAN_POINT('Ctrl Pts',(-2.68023295023435,-0.132444682635759,
12.5893111709658));
#433541=CARTESIAN_POINT('Ctrl Pts',(-2.69531616042252,-0.144286884036376,
12.5508408821982));
#433542=CARTESIAN_POINT('Ctrl Pts',(-2.69292393312528,-0.12804671860655,
12.55409748406));
#433543=CARTESIAN_POINT('Ctrl Pts',(-2.70364674200648,-0.124330810378115,
12.5663972313419));
#433544=CARTESIAN_POINT('Ctrl Pts',(-2.71870359571991,-0.136234199142437,
12.52790050457));
#433545=CARTESIAN_POINT('Ctrl Pts',(-2.71627924595099,-0.119953111785028,
12.5311362602938));
#433546=CARTESIAN_POINT('Ctrl Pts',(-2.72703691311007,-0.116225123684305,
12.5434568539655));
#433547=CARTESIAN_POINT('Ctrl Pts',(-2.74206958034371,-0.128187733774514,
12.5049357605811));
#433548=CARTESIAN_POINT('Ctrl Pts',(-2.73959441388288,-0.111873416872463,
12.5081700652078));
#433549=CARTESIAN_POINT('Ctrl Pts',(-2.75040531352075,-0.108126981459283,
12.5204921097672));
#433550=CARTESIAN_POINT('Ctrl Pts',(-2.74053527768469,-0.128716094731106,
12.5064436508395));
#433551=CARTESIAN_POINT('Ctrl Pts',(-2.74079894328763,-0.127524739099731,
12.5062361689309));
#433552=CARTESIAN_POINT('Ctrl Pts',(-2.74102233188788,-0.126274583447935,
12.5061871075061));
#433553=CARTESIAN_POINT('Ctrl Pts',(-2.74117020531107,-0.125054276071972,
12.5063648335164));
#433554=CARTESIAN_POINT('Ctrl Pts',(-2.74123737854109,-0.124499937190128,
12.5064455676329));
#433555=CARTESIAN_POINT('Ctrl Pts',(-2.74128968714911,-0.123943999232077,
12.506574497099));
#433556=CARTESIAN_POINT('Ctrl Pts',(-2.74132384197106,-0.123410200700237,
12.5067492519495));
#433557=CARTESIAN_POINT('Ctrl Pts',(-2.74139247741156,-0.122337511830006,
12.5071004286051));
#433558=CARTESIAN_POINT('Ctrl Pts',(-2.74138952033895,-0.121314736865664,
12.5076537929612));
#433559=CARTESIAN_POINT('Ctrl Pts',(-2.74132465110495,-0.120418613085864,
12.5083435010503));
#433560=CARTESIAN_POINT('Ctrl Pts',(-2.741320567199,-0.120362196738561,
12.5083869222963));
#433561=CARTESIAN_POINT('Ctrl Pts',(-2.74131622555791,-0.120306277076869,
12.5084308732336));
#433562=CARTESIAN_POINT('Ctrl Pts',(-2.74131162372435,-0.120250870730712,
12.5084753333615));
#433563=CARTESIAN_POINT('Ctrl Pts',(-2.74127471094544,-0.119806438705525,
12.508831962269));
#433564=CARTESIAN_POINT('Ctrl Pts',(-2.74122159324092,-0.119385904725475,
12.509227847131));
#433565=CARTESIAN_POINT('Ctrl Pts',(-2.74115662805751,-0.119001422570601,
12.5096423454524));
#433566=CARTESIAN_POINT('Ctrl Pts',(-2.74095305592508,-0.117796625661898,
12.5109411997424));
#433567=CARTESIAN_POINT('Ctrl Pts',(-2.74063016373539,-0.116870114613123,
12.5124831113042));
#433568=CARTESIAN_POINT('Ctrl Pts',(-2.74025727175298,-0.11615746459738,
12.5140723025008));
#433569=CARTESIAN_POINT('Ctrl Pts',(-2.74022233136581,-0.116090688510361,
12.5142212114565));
#433570=CARTESIAN_POINT('Ctrl Pts',(-2.74018696520292,-0.116025763606908,
12.5143705582413));
#433571=CARTESIAN_POINT('Ctrl Pts',(-2.7401512392264,-0.115962622442655,
12.5145201959299));
#433572=CARTESIAN_POINT('Ctrl Pts',(-2.73969228586759,-0.115151480180464,
12.5164425148273));
#433573=CARTESIAN_POINT('Ctrl Pts',(-2.73916757216949,-0.114601631733722,
12.5184635205941));
#433574=CARTESIAN_POINT('Ctrl Pts',(-2.73860159963072,-0.114226257432332,
12.5205025929158));
#433575=CARTESIAN_POINT('Ctrl Pts',(-2.73827331312518,-0.114008525459078,
12.5216853356836));
#433576=CARTESIAN_POINT('Ctrl Pts',(-2.73793200553798,-0.113849484943904,
12.5228750347131));
#433577=CARTESIAN_POINT('Ctrl Pts',(-2.73758805651309,-0.113734129333599,
12.5240609649613));
#433578=CARTESIAN_POINT('Ctrl Pts',(-2.73674385208373,-0.11345099517672,
12.5269717671327));
#433579=CARTESIAN_POINT('Ctrl Pts',(-2.7358566698738,-0.113432919929299,
12.5299036066169));
#433580=CARTESIAN_POINT('Ctrl Pts',(-2.73494218237204,-0.113594675100055,
12.5328133004019));
#433581=CARTESIAN_POINT('Ctrl Pts',(-2.73450317512218,-0.113672327000739,
12.5342101228452));
#433582=CARTESIAN_POINT('Ctrl Pts',(-2.73405851424506,-0.113791841062789,
12.5356023438238));
#433583=CARTESIAN_POINT('Ctrl Pts',(-2.73361252196705,-0.113946396223116,
12.5369868989719));
#433584=CARTESIAN_POINT('Origin',(-14.7751638741716,4.06456903460374,-1.24070212061166));
#433585=CARTESIAN_POINT('Ctrl Pts',(-2.72703567269247,-0.220646278375188,
12.5369868989719));
#433586=CARTESIAN_POINT('Ctrl Pts',(-2.74082017142999,-0.227374643573386,
12.5369868989719));
#433587=CARTESIAN_POINT('Ctrl Pts',(-2.73927331120585,-0.242635394771541,
12.5369868989719));
#433588=CARTESIAN_POINT('Ctrl Pts',(-2.73169534333072,-0.222920788458994,
12.5218025310016));
#433589=CARTESIAN_POINT('Ctrl Pts',(-2.74043375195878,-0.230876671713106,
12.5216901060418));
#433590=CARTESIAN_POINT('Ctrl Pts',(-2.73927804295614,-0.242588876607485,
12.5161920673677));
#433591=CARTESIAN_POINT('Ctrl Pts',(-2.73700294375324,-0.220063263489773,
12.5042015548895));
#433592=CARTESIAN_POINT('Ctrl Pts',(-2.74087193293557,-0.225202161010103,
12.4980677368512));
#433593=CARTESIAN_POINT('Ctrl Pts',(-2.74030930782376,-0.231975212959352,
12.4907278922778));
#433594=CARTESIAN_POINT('Ctrl Pts',(-2.73572752933513,-0.206849169015788,
12.506463626192));
#433595=CARTESIAN_POINT('Ctrl Pts',(-2.74225164635562,-0.207342459436628,
12.4999376786891));
#433596=CARTESIAN_POINT('Ctrl Pts',(-2.74217196375227,-0.207336434611381,
12.4906970594712));
#433597=CARTESIAN_POINT('Origin',(-2.71738546452303,-0.240416798911745,
12.5369868989719));
#433598=CARTESIAN_POINT('Origin',(-2.71738546452303,-0.240416798911746,
14.));
#433599=CARTESIAN_POINT('Origin',(-2.71738546452303,-0.240416798911745,
13.7435492065112));
#433600=CARTESIAN_POINT('Ctrl Pts',(-2.70484295955581,-0.209761503718633,
13.793642941384));
#433601=CARTESIAN_POINT('Ctrl Pts',(-2.71456248633017,-0.214498276701194,
13.8071662555867));
#433602=CARTESIAN_POINT('Ctrl Pts',(-2.70943367592869,-0.230737571251773,
13.8103758687955));
#433603=CARTESIAN_POINT('Ctrl Pts',(-2.71976582146069,-0.217080649692748,
13.7804579775006));
#433604=CARTESIAN_POINT('Ctrl Pts',(-2.73175439640573,-0.222934515297326,
13.7901904343352));
#433605=CARTESIAN_POINT('Ctrl Pts',(-2.72950263006789,-0.238528920464716,
13.7927914348262));
#433606=CARTESIAN_POINT('Ctrl Pts',(-2.72855147185785,-0.221389706412309,
13.7597120340895));
#433607=CARTESIAN_POINT('Ctrl Pts',(-2.74242311492923,-0.228169426795429,
13.7635825532445));
#433608=CARTESIAN_POINT('Ctrl Pts',(-2.74132801802721,-0.243147299772559,
13.7651073818884));
#433609=CARTESIAN_POINT('Ctrl Pts',(-2.7268310403412,-0.220545894441165,
13.7381884353898));
#433610=CARTESIAN_POINT('Ctrl Pts',(-2.74037838644556,-0.227166115295103,
13.7368803041982));
#433611=CARTESIAN_POINT('Ctrl Pts',(-2.73901207587965,-0.242243344236675,
13.7363986145813));
#433612=CARTESIAN_POINT('Origin',(-2.69877622741401,-0.231289609678946,
13.7902182540695));
#433613=CARTESIAN_POINT('Ctrl Pts',(-2.67634800279185,-0.195785680417494,
13.8235227101244));
#433614=CARTESIAN_POINT('Ctrl Pts',(-2.68667231492669,-0.200844461620682,
13.8358800583119));
#433615=CARTESIAN_POINT('Ctrl Pts',(-2.68216956901137,-0.216792857410809,
13.8390832900376));
#433616=CARTESIAN_POINT('Ctrl Pts',(-2.68705688280404,-0.201038016867016,
13.8124254819053));
#433617=CARTESIAN_POINT('Ctrl Pts',(-2.69740124448431,-0.206106622401379,
13.8247886449158));
#433618=CARTESIAN_POINT('Ctrl Pts',(-2.69287640609648,-0.222070538545803,
13.8279860620657));
#433619=CARTESIAN_POINT('Ctrl Pts',(-2.6977609634446,-0.2062879993902,13.8013225099955));
#433620=CARTESIAN_POINT('Ctrl Pts',(-2.70812049467478,-0.211364035887708,
13.8136962257787));
#433621=CARTESIAN_POINT('Ctrl Pts',(-2.70357840628482,-0.227345533249965,
13.8168830918626));
#433622=CARTESIAN_POINT('Ctrl Pts',(-2.70846043144973,-0.211535719574715,
13.7902140179785));
#433623=CARTESIAN_POINT('Ctrl Pts',(-2.71883057117651,-0.216616950094158,
13.802602731458));
#433624=CARTESIAN_POINT('Ctrl Pts',(-2.71427576044339,-0.232617945429034,
13.8057746032558));
#433625=CARTESIAN_POINT('Origin',(-2.66666378756618,-0.21553956503708,13.8235269408515));
#433626=CARTESIAN_POINT('Ctrl Pts',(-2.68023295023436,-0.132444682635759,
13.8235269408515));
#433627=CARTESIAN_POINT('Ctrl Pts',(-2.69138951503121,-0.128578459578989,
13.8362179249168));
#433628=CARTESIAN_POINT('Ctrl Pts',(-2.68848109463237,-0.111749790741529,
13.8391868794938));
#433629=CARTESIAN_POINT('Ctrl Pts',(-2.67002517906158,-0.135982108446035,
13.8400110824519));
#433630=CARTESIAN_POINT('Ctrl Pts',(-2.67784984837637,-0.12964993559815,
13.8494522556836));
#433631=CARTESIAN_POINT('Ctrl Pts',(-2.67171877499601,-0.11767755794622,
13.85569149686));
#433632=CARTESIAN_POINT('Ctrl Pts',(-2.65816477724548,-0.147150304128653,
13.8586819406588));
#433633=CARTESIAN_POINT('Ctrl Pts',(-2.65844494694465,-0.142805474031326,
13.868010383617));
#433634=CARTESIAN_POINT('Ctrl Pts',(-2.65213036132971,-0.136323277235162,
13.8744918421245));
#433635=CARTESIAN_POINT('Ctrl Pts',(-2.65619840500193,-0.178378574624259,
13.8587686893867));
#433636=CARTESIAN_POINT('Ctrl Pts',(-2.65592067261882,-0.18268473215078,
13.8680909899357));
#433637=CARTESIAN_POINT('Ctrl Pts',(-2.64885949684767,-0.188309338646756,
13.8745789365163));
#433638=CARTESIAN_POINT('Ctrl Pts',(-2.66663625157229,-0.191022400427148,
13.8400379222776));
#433639=CARTESIAN_POINT('Ctrl Pts',(-2.6736223259497,-0.198265673078453,
13.8494748685453));
#433640=CARTESIAN_POINT('Ctrl Pts',(-2.66607977414707,-0.209395408815177,
13.8557104837033));
#433641=CARTESIAN_POINT('Ctrl Pts',(-2.6763515371407,-0.195787413055823,
13.8235269408542));
#433642=CARTESIAN_POINT('Ctrl Pts',(-2.68695259026277,-0.200986864131993,
13.8362179249195));
#433643=CARTESIAN_POINT('Ctrl Pts',(-2.68201124437825,-0.217334527723647,
13.8391868794965));
#433644=CARTESIAN_POINT('Origin',(-2.67302930503479,-0.111657487157801,
13.8235269408515));
#433645=CARTESIAN_POINT('Ctrl Pts',(-2.71402440610745,-0.120734508655639,
13.7902140241683));
#433646=CARTESIAN_POINT('Ctrl Pts',(-2.72493734455485,-0.116957423822622,
13.8026027327198));
#433647=CARTESIAN_POINT('Ctrl Pts',(-2.722370242243,-0.100520029929612,
13.8057746032556));
#433648=CARTESIAN_POINT('Ctrl Pts',(-2.70276426933073,-0.124636623798955,
13.8013225161808));
#433649=CARTESIAN_POINT('Ctrl Pts',(-2.71366604449621,-0.120863398901542,
13.8136962270464));
#433650=CARTESIAN_POINT('Ctrl Pts',(-2.71110918874919,-0.104446910421896,
13.8168830918628));
#433651=CARTESIAN_POINT('Ctrl Pts',(-2.69149927820773,-0.128540421179234,
13.8124254880875));
#433652=CARTESIAN_POINT('Ctrl Pts',(-2.70238509004795,-0.124772719542996,
13.8247886461868));
#433653=CARTESIAN_POINT('Ctrl Pts',(-2.69984320867404,-0.108375786864016,
13.8279860620656));
#433654=CARTESIAN_POINT('Ctrl Pts',(-2.68022923621552,-0.132445968900005,
13.8235227163065));
#433655=CARTESIAN_POINT('Ctrl Pts',(-2.69109394903256,-0.128685570165813,
13.8358800595847));
#433656=CARTESIAN_POINT('Ctrl Pts',(-2.68857209989094,-0.112306739080995,
13.8390832900376));
#433657=CARTESIAN_POINT('Origin',(-2.70682448668518,-0.0999460228420741,
13.7902182540695));
#433658=CARTESIAN_POINT('Ctrl Pts',(-2.73335752972873,-0.114034732658743,
13.7382347919292));
#433659=CARTESIAN_POINT('Ctrl Pts',(-2.74762380251145,-0.109116264439644,
13.7369371795942));
#433660=CARTESIAN_POINT('Ctrl Pts',(-2.74810064964376,-0.0939730681511174,
13.7364597369712));
#433661=CARTESIAN_POINT('Ctrl Pts',(-2.73514481161654,-0.113415364078833,
13.7595490285574));
#433662=CARTESIAN_POINT('Ctrl Pts',(-2.74975113773552,-0.108378594903541,
13.7633824266926));
#433663=CARTESIAN_POINT('Ctrl Pts',(-2.75048021381224,-0.0933665294766319,
13.7648920890506));
#433664=CARTESIAN_POINT('Ctrl Pts',(-2.72602977190662,-0.11657410991213,
13.7803806590111));
#433665=CARTESIAN_POINT('Ctrl Pts',(-2.73866548108742,-0.112222588396372,
13.7901039518744));
#433666=CARTESIAN_POINT('Ctrl Pts',(-2.73834985287197,-0.096462327603629,
13.7926933640891));
#433667=CARTESIAN_POINT('Ctrl Pts',(-2.71018579813282,-0.122064715218304,
13.7936647693663));
#433668=CARTESIAN_POINT('Ctrl Pts',(-2.72041476756285,-0.118551665781653,
13.8072068914933));
#433669=CARTESIAN_POINT('Ctrl Pts',(-2.71729332976618,-0.101791567454706,
13.8104111085397));
#433670=CARTESIAN_POINT('Origin',(-2.72640887676748,-0.0931592007451578,
13.7435492065112));
#433671=CARTESIAN_POINT('Origin',(-2.72640887676748,-0.0931592007451578,
14.));
#433672=CARTESIAN_POINT('Origin',(-2.72640887676748,-0.093159200745158,
12.5369868989719));
#433673=CARTESIAN_POINT('Ctrl Pts',(-2.7405169146902,-0.128715232277453,
12.506462012331));
#433674=CARTESIAN_POINT('Ctrl Pts',(-2.74704833746511,-0.129021996886374,
12.4999388158272));
#433675=CARTESIAN_POINT('Ctrl Pts',(-2.74697106216825,-0.129018367458753,
12.4907030323752));
#433676=CARTESIAN_POINT('Ctrl Pts',(-2.74339410614793,-0.115755666217203,
12.5042014951932));
#433677=CARTESIAN_POINT('Ctrl Pts',(-2.7478603096561,-0.111130288033808,
12.4980716682127));
#433678=CARTESIAN_POINT('Ctrl Pts',(-2.74813022330732,-0.104344073194392,
12.4907355092743));
#433679=CARTESIAN_POINT('Ctrl Pts',(-2.73847716185432,-0.112270073002454,
12.5218047446509));
#433680=CARTESIAN_POINT('Ctrl Pts',(-2.74811618091026,-0.105443054430946,
12.5216906929434));
#433681=CARTESIAN_POINT('Ctrl Pts',(-2.74840269453549,-0.0936834343574711,
12.5161988840776));
#433682=CARTESIAN_POINT('Ctrl Pts',(-2.73357621265543,-0.113958943442349,
12.5369868989719));
#433683=CARTESIAN_POINT('Ctrl Pts',(-2.74806974767195,-0.108964649273456,
12.5369868989719));
#433684=CARTESIAN_POINT('Ctrl Pts',(-2.74840365732554,-0.0936383961154349,
12.5369868989719));
#433685=CARTESIAN_POINT('Origin',(-5.14221766115599E-31,-5.4669590742534E-31,
12.5));
#433686=CARTESIAN_POINT('Origin',(-2.66051922500485,-0.35046785139304,12.5));
#433687=CARTESIAN_POINT('',(-2.66051922500485,-0.35046785139304,12.5893111709658));
#433688=CARTESIAN_POINT('',(-2.66051922500485,-0.35046785139304,13.8235269408515));
#433689=CARTESIAN_POINT('',(-2.66051922500485,-0.35046785139304,12.5));
#433690=CARTESIAN_POINT('',(-2.69515654904186,-0.341549977052361,13.7902182540695));
#433691=CARTESIAN_POINT('',(-2.66051922500485,-0.35046785139304,13.8235269408515));
#433692=CARTESIAN_POINT('',(-2.71522896268844,-0.336382047150414,13.7435492065112));
#433693=CARTESIAN_POINT('Origin',(-2.64919106833208,-0.35338478368455,13.7445212918706));
#433694=CARTESIAN_POINT('',(-2.71522896268844,-0.336382047150414,12.5369868989719));
#433695=CARTESIAN_POINT('',(-2.71522896268844,-0.336382047150414,12.5));
#433696=CARTESIAN_POINT('Ctrl Pts',(-2.71522896268844,-0.336382047150414,
12.5369868989719));
#433697=CARTESIAN_POINT('Ctrl Pts',(-2.69700568411229,-0.341073890788324,
12.5544431401645));
#433698=CARTESIAN_POINT('Ctrl Pts',(-2.67876937176296,-0.345769090157505,
12.5718848856037));
#433699=CARTESIAN_POINT('Ctrl Pts',(-2.66051922500485,-0.35046785139304,
12.5893111709658));
#433700=CARTESIAN_POINT('Origin',(-2.88769754146683,-0.554102169734571,
12.5));
#433701=CARTESIAN_POINT('',(-2.70001288567338,-0.442212187377255,13.7435492065112));
#433702=CARTESIAN_POINT('',(-2.68220951992085,-0.431598542529574,13.7902182540695));
#433703=CARTESIAN_POINT('Origin',(-2.63542535176389,-0.403707718276761,
13.7418732680449));
#433704=CARTESIAN_POINT('',(-2.65148770642212,-0.413283442897022,13.8235269408515));
#433705=CARTESIAN_POINT('',(-2.68220951992085,-0.431598542529574,13.7902182540695));
#433706=CARTESIAN_POINT('',(-2.65148770642212,-0.413283442897022,12.5893111709658));
#433707=CARTESIAN_POINT('',(-2.65148770642212,-0.413283442897022,12.5));
#433708=CARTESIAN_POINT('',(-2.70001288567338,-0.442212187377255,12.5369868989719));
#433709=CARTESIAN_POINT('Ctrl Pts',(-2.65148770642212,-0.413283442897022,
12.5893111709658));
#433710=CARTESIAN_POINT('Ctrl Pts',(-2.66767479998709,-0.422933531796104,
12.5718848856037));
#433711=CARTESIAN_POINT('Ctrl Pts',(-2.68384962302775,-0.43257630550609,
12.5544431401645));
#433712=CARTESIAN_POINT('Ctrl Pts',(-2.70001288567338,-0.442212187377255,
12.5369868989719));
#433713=CARTESIAN_POINT('',(-2.70001288567338,-0.442212187377255,12.5));
#433714=CARTESIAN_POINT('Origin',(-2.66909004727681,-0.383757213516432,
12.5));
#433715=CARTESIAN_POINT('',(-2.63524304023065,-0.377759690177983,13.8587068136939));
#433716=CARTESIAN_POINT('Ctrl Pts',(-2.65148770641861,-0.413283442902624,
13.8235269408542));
#433717=CARTESIAN_POINT('Ctrl Pts',(-2.64998257878664,-0.412386146831852,
13.8262006681044));
#433718=CARTESIAN_POINT('Ctrl Pts',(-2.64853126693574,-0.411318662900615,
13.8288634856214));
#433719=CARTESIAN_POINT('Ctrl Pts',(-2.64713116732489,-0.410094068861876,
13.8314912288862));
#433720=CARTESIAN_POINT('Ctrl Pts',(-2.64568780903969,-0.408831638718954,
13.8342001611531));
#433721=CARTESIAN_POINT('Ctrl Pts',(-2.64429694613649,-0.407401211832304,
13.8368750301949));
#433722=CARTESIAN_POINT('Ctrl Pts',(-2.64296770426095,-0.405773530919453,
13.8394886372969));
#433723=CARTESIAN_POINT('Ctrl Pts',(-2.64286504368661,-0.405647821174351,
13.8396904925131));
#433724=CARTESIAN_POINT('Ctrl Pts',(-2.64276276515684,-0.405520918083497,
13.8398919674349));
#433725=CARTESIAN_POINT('Ctrl Pts',(-2.64266088109114,-0.405392800201788,
13.8400930404591));
#433726=CARTESIAN_POINT('Ctrl Pts',(-2.64107345880321,-0.403396637411273,
13.8432258934518));
#433727=CARTESIAN_POINT('Ctrl Pts',(-2.63958901469215,-0.401116461417161,
13.8462331177034));
#433728=CARTESIAN_POINT('Ctrl Pts',(-2.63833680712334,-0.398574008230136,
13.8489036603661));
#433729=CARTESIAN_POINT('Ctrl Pts',(-2.63792707023415,-0.397742087959324,
13.849777493004));
#433730=CARTESIAN_POINT('Ctrl Pts',(-2.6375424135319,-0.396882213434789,
13.85061494757));
#433731=CARTESIAN_POINT('Ctrl Pts',(-2.63718797393439,-0.395995519407907,
13.8514076489583));
#433732=CARTESIAN_POINT('Ctrl Pts',(-2.63643828306783,-0.394120033660651,
13.8530843267192));
#433733=CARTESIAN_POINT('Ctrl Pts',(-2.63575288580402,-0.391939241901277,
13.8546805203176));
#433734=CARTESIAN_POINT('Ctrl Pts',(-2.63530173060524,-0.389538806144157,
13.8559412814273));
#433735=CARTESIAN_POINT('Ctrl Pts',(-2.63524135140833,-0.389217549991856,
13.8561100121513));
#433736=CARTESIAN_POINT('Ctrl Pts',(-2.6351851194351,-0.388892419497718,
13.8562727473908));
#433737=CARTESIAN_POINT('Ctrl Pts',(-2.63513338736153,-0.388563672539864,
13.8564289040185));
#433738=CARTESIAN_POINT('Ctrl Pts',(-2.63489878299806,-0.387072808836557,
13.8571370725437));
#433739=CARTESIAN_POINT('Ctrl Pts',(-2.63475484918487,-0.385481009415416,
13.8577210840554));
#433740=CARTESIAN_POINT('Ctrl Pts',(-2.63473640945108,-0.383847504874734,
13.8581177131616));
#433741=CARTESIAN_POINT('Ctrl Pts',(-2.63473121618737,-0.383387453772568,
13.8582294175695));
#433742=CARTESIAN_POINT('Ctrl Pts',(-2.63473580309041,-0.382924131467699,
13.8583265086086));
#433743=CARTESIAN_POINT('Ctrl Pts',(-2.63475051334241,-0.382458926246567,
13.8584082369006));
#433744=CARTESIAN_POINT('Ctrl Pts',(-2.63477164802983,-0.381790551093503,
13.8585256585398));
#433745=CARTESIAN_POINT('Ctrl Pts',(-2.63481426525496,-0.381109989969931,
13.8586122832068));
#433746=CARTESIAN_POINT('Ctrl Pts',(-2.63487804608901,-0.380434971235501,
13.8586682984299));
#433747=CARTESIAN_POINT('Ctrl Pts',(-2.63492906443386,-0.379895023160412,
13.8587131050557));
#433748=CARTESIAN_POINT('Ctrl Pts',(-2.63499395418751,-0.379352635547506,
13.8587357943552));
#433749=CARTESIAN_POINT('Ctrl Pts',(-2.63507322592065,-0.378807804107057,
13.8587355499465));
#433750=CARTESIAN_POINT('Ctrl Pts',(-2.63512446113171,-0.378455666557732,
13.8587353919793));
#433751=CARTESIAN_POINT('Ctrl Pts',(-2.63518111187177,-0.378106310537414,
13.8587257282814));
#433752=CARTESIAN_POINT('Ctrl Pts',(-2.63524304023065,-0.377759690177983,
13.8587068136939));
#433753=CARTESIAN_POINT('Ctrl Pts',(-2.63524304023065,-0.377759690177983,
13.8587068136939));
#433754=CARTESIAN_POINT('Ctrl Pts',(-2.63544671922696,-0.376619674711952,
13.8586446046466));
#433755=CARTESIAN_POINT('Ctrl Pts',(-2.63570741683485,-0.375509214094161,
13.858482427929));
#433756=CARTESIAN_POINT('Ctrl Pts',(-2.6360208610235,-0.374426990861144,
13.8582284286032));
#433757=CARTESIAN_POINT('Ctrl Pts',(-2.63634241829973,-0.373316755713468,
13.8579678548414));
#433758=CARTESIAN_POINT('Ctrl Pts',(-2.63672174470969,-0.372233952740267,
13.857615680862));
#433759=CARTESIAN_POINT('Ctrl Pts',(-2.63713474082569,-0.371218067059845,
13.8571944833187));
#433760=CARTESIAN_POINT('Ctrl Pts',(-2.63816541487094,-0.368682820448085,
13.8561433417727));
#433761=CARTESIAN_POINT('Ctrl Pts',(-2.63944955424229,-0.366443939905809,
13.8546163505474));
#433762=CARTESIAN_POINT('Ctrl Pts',(-2.64078434840511,-0.364541746069135,
13.8528973491086));
#433763=CARTESIAN_POINT('Ctrl Pts',(-2.6410281956056,-0.364194243319431,
13.8525833129072));
#433764=CARTESIAN_POINT('Ctrl Pts',(-2.64127366824998,-0.363857851680216,
13.8522628768812));
#433765=CARTESIAN_POINT('Ctrl Pts',(-2.64151947325147,-0.363532647353053,
13.851937733538));
#433766=CARTESIAN_POINT('Ctrl Pts',(-2.64302057029165,-0.361546669647119,
13.8499521282529));
#433767=CARTESIAN_POINT('Ctrl Pts',(-2.64468649643034,-0.35978299909703,
13.847639871647));
#433768=CARTESIAN_POINT('Ctrl Pts',(-2.6463712919281,-0.3582791597414,13.8452109780794));
#433769=CARTESIAN_POINT('Ctrl Pts',(-2.64712931629607,-0.357602551287374,
13.8441181685877));
#433770=CARTESIAN_POINT('Ctrl Pts',(-2.64789089707965,-0.356977872367289,
13.8430021611332));
#433771=CARTESIAN_POINT('Ctrl Pts',(-2.64864253925751,-0.356405237945735,
13.8418824960098));
#433772=CARTESIAN_POINT('Ctrl Pts',(-2.65041380324351,-0.355055810308606,
13.8392439765549));
#433773=CARTESIAN_POINT('Ctrl Pts',(-2.652212257862,-0.353927879837718,
13.8364981347964));
#433774=CARTESIAN_POINT('Ctrl Pts',(-2.65402447734643,-0.35298947290406,
13.8336931113419));
#433775=CARTESIAN_POINT('Ctrl Pts',(-2.65578946403768,-0.352075524145027,
13.8309611966328));
#433776=CARTESIAN_POINT('Ctrl Pts',(-2.65756953562669,-0.351340933731929,
13.8281701127186));
#433777=CARTESIAN_POINT('Ctrl Pts',(-2.65935642543848,-0.350795245194212,
13.8253580685121));
#433778=CARTESIAN_POINT('Ctrl Pts',(-2.65974382507816,-0.350676939330308,
13.8247484142933));
#433779=CARTESIAN_POINT('Ctrl Pts',(-2.66013149484599,-0.35056767806646,
13.8241378483365));
#433780=CARTESIAN_POINT('Ctrl Pts',(-2.66051922500485,-0.35046785139304,
13.8235269408515));
#433781=CARTESIAN_POINT('',(-2.63504841430183,-0.378986432859003,12.5969504640361));
#433782=CARTESIAN_POINT('Origin',(-2.66912282379287,-0.383761728248441,
12.584524458991));
#433783=CARTESIAN_POINT('Origin',(-2.66912282379287,-0.383761728248441,
12.584524458991));
#433784=CARTESIAN_POINT('Ctrl Pts',(-2.65148770642212,-0.413283442897022,
12.5893111709658));
#433785=CARTESIAN_POINT('Ctrl Pts',(-2.6417524603545,-0.407479683894216,
12.5770542771492));
#433786=CARTESIAN_POINT('Ctrl Pts',(-2.64736473026113,-0.392107432876553,
12.5737548217797));
#433787=CARTESIAN_POINT('Ctrl Pts',(-2.67277542232632,-0.425974316036751,
12.5663937883685));
#433788=CARTESIAN_POINT('Ctrl Pts',(-2.66302775760034,-0.420163153533316,
12.5540940315304));
#433789=CARTESIAN_POINT('Ctrl Pts',(-2.66866043523377,-0.404744368302604,
12.5508374392248));
#433790=CARTESIAN_POINT('Ctrl Pts',(-2.69404165918613,-0.438652384241057,
12.5434499600945));
#433791=CARTESIAN_POINT('Ctrl Pts',(-2.68426230133086,-0.432822327578891,
12.5311293540533));
#433792=CARTESIAN_POINT('Ctrl Pts',(-2.68993473174172,-0.417369971842775,
12.5278936106989));
#433793=CARTESIAN_POINT('Ctrl Pts',(-2.71528809948451,-0.451318650538058,
12.5204817579905));
#433794=CARTESIAN_POINT('Ctrl Pts',(-2.70546034049114,-0.445459739079734,
12.5081597038247));
#433795=CARTESIAN_POINT('Ctrl Pts',(-2.71118927666454,-0.429985136169938,
12.5049254088044));
#433796=CARTESIAN_POINT('Ctrl Pts',(-2.70001288567338,-0.442212187377255,
12.5369868989719));
#433797=CARTESIAN_POINT('Ctrl Pts',(-2.70081299700138,-0.442689181123054,
12.5342545179733));
#433798=CARTESIAN_POINT('Ctrl Pts',(-2.701640465217,-0.443037252186933,
12.5314872231885));
#433799=CARTESIAN_POINT('Ctrl Pts',(-2.70247035267223,-0.443185265435587,
12.5287124745063));
#433800=CARTESIAN_POINT('Ctrl Pts',(-2.70321878637129,-0.443318751129947,
12.5262100684184));
#433801=CARTESIAN_POINT('Ctrl Pts',(-2.70396860526476,-0.443288420209528,
12.5237004536639));
#433802=CARTESIAN_POINT('Ctrl Pts',(-2.70473000481237,-0.443027515437006,
12.5212220730815));
#433803=CARTESIAN_POINT('Ctrl Pts',(-2.70531292203238,-0.442827770263577,
12.5193246583486));
#433804=CARTESIAN_POINT('Ctrl Pts',(-2.70590938791894,-0.442489892964446,
12.517417831369));
#433805=CARTESIAN_POINT('Ctrl Pts',(-2.70648911402888,-0.441921489638494,
12.5155812248347));
#433806=CARTESIAN_POINT('Ctrl Pts',(-2.70673608046776,-0.441679346766459,
12.5147988205793));
#433807=CARTESIAN_POINT('Ctrl Pts',(-2.70698045361195,-0.441395319896029,
12.5140295443047));
#433808=CARTESIAN_POINT('Ctrl Pts',(-2.70722197818642,-0.441062681003598,
12.5132817086137));
#433809=CARTESIAN_POINT('Ctrl Pts',(-2.70758749295719,-0.440559277038272,
12.5121499604604));
#433810=CARTESIAN_POINT('Ctrl Pts',(-2.70794858964725,-0.439929465719476,
12.5110494206568));
#433811=CARTESIAN_POINT('Ctrl Pts',(-2.7082806391003,-0.439145313135833,
12.5100666561695));
#433812=CARTESIAN_POINT('Ctrl Pts',(-2.70847130113159,-0.438695054528048,
12.5095023550641));
#433813=CARTESIAN_POINT('Ctrl Pts',(-2.70865398804955,-0.438188452292117,
12.5089719619137));
#433814=CARTESIAN_POINT('Ctrl Pts',(-2.70881926733513,-0.437632835477477,
12.5085043804652));
#433815=CARTESIAN_POINT('Ctrl Pts',(-2.70906113204043,-0.436819762643432,
12.5078201359221));
#433816=CARTESIAN_POINT('Ctrl Pts',(-2.7092715763757,-0.435877801288408,
12.5072563000949));
#433817=CARTESIAN_POINT('Ctrl Pts',(-2.70942807300513,-0.434868956606923,
12.5068768744332));
#433818=CARTESIAN_POINT('Ctrl Pts',(-2.70954091784821,-0.434141510142467,
12.5066032824114));
#433819=CARTESIAN_POINT('Ctrl Pts',(-2.70962775496767,-0.433366517410012,
12.5064197834844));
#433820=CARTESIAN_POINT('Ctrl Pts',(-2.70968630393582,-0.4325875438446,
12.5063282718343));
#433821=CARTESIAN_POINT('Ctrl Pts',(-2.70977176730302,-0.43145048360322,
12.5061946931565));
#433822=CARTESIAN_POINT('Ctrl Pts',(-2.70979984309925,-0.430280717716541,
12.5062515701262));
#433823=CARTESIAN_POINT('Ctrl Pts',(-2.7097842489696,-0.429151214975581,
12.5064436508398));
#433824=CARTESIAN_POINT('',(-2.64736473026113,-0.392107432876553,12.5737548217797));
#433825=CARTESIAN_POINT('Origin',(-2.66275320456912,-0.394386656093445,
12.5893111709658));
#433826=CARTESIAN_POINT('Ctrl Pts',(-2.7097842489696,-0.42915121497558,
12.5064436508398));
#433827=CARTESIAN_POINT('Ctrl Pts',(-2.70054478370098,-0.423667359643695,
12.5164271754438));
#433828=CARTESIAN_POINT('Ctrl Pts',(-2.69130154927055,-0.418181510184859,
12.5264061185523));
#433829=CARTESIAN_POINT('Ctrl Pts',(-2.68205441341468,-0.412693595553663,
12.536380305637));
#433830=CARTESIAN_POINT('Ctrl Pts',(-2.67049736911609,-0.405834815333688,
12.5488460165097));
#433831=CARTESIAN_POINT('Ctrl Pts',(-2.6589342273919,-0.398972807323734,
12.5613043021964));
#433832=CARTESIAN_POINT('Ctrl Pts',(-2.64736473026113,-0.392107432876553,
12.5737548217797));
#433833=CARTESIAN_POINT('Ctrl Pts',(-2.66051922500485,-0.35046785139304,
12.5893111709658));
#433834=CARTESIAN_POINT('Ctrl Pts',(-2.64954321694341,-0.353293781610674,
12.5770542771492));
#433835=CARTESIAN_POINT('Ctrl Pts',(-2.65059728690124,-0.36962450760124,
12.5737548217797));
#433836=CARTESIAN_POINT('Ctrl Pts',(-2.6502787049478,-0.353104419707449,
12.5928319619712));
#433837=CARTESIAN_POINT('Ctrl Pts',(-2.64371441229884,-0.358158475345272,
12.5821634970843));
#433838=CARTESIAN_POINT('Ctrl Pts',(-2.64686455989743,-0.37057580486522,
12.5773203894503));
#433839=CARTESIAN_POINT('Ctrl Pts',(-2.63727749621991,-0.363666269495877,
12.5969440695591));
#433840=CARTESIAN_POINT('Ctrl Pts',(-2.6366873411962,-0.367642481210552,
12.5878292599214));
#433841=CARTESIAN_POINT('Ctrl Pts',(-2.64223195386749,-0.374341851661124,
12.5813877129824));
#433842=CARTESIAN_POINT('Ctrl Pts',(-2.63286972343275,-0.393944096112038,
12.596957478804));
#433843=CARTESIAN_POINT('Ctrl Pts',(-2.63345559634244,-0.389997281436558,
12.5878468778671));
#433844=CARTESIAN_POINT('Ctrl Pts',(-2.64066025378196,-0.385179564849123,
12.5814011370086));
#433845=CARTESIAN_POINT('Ctrl Pts',(-2.64239161815869,-0.407860723863328,
12.5928371701607));
#433846=CARTESIAN_POINT('Ctrl Pts',(-2.63752551142403,-0.401163256360554,
12.5821692192952));
#433847=CARTESIAN_POINT('Ctrl Pts',(-2.64404048991929,-0.390136975157249,
12.5773318885715));
#433848=CARTESIAN_POINT('Ctrl Pts',(-2.65148770642209,-0.413283442897068,
12.5893111709658));
#433849=CARTESIAN_POINT('Ctrl Pts',(-2.64175246035447,-0.407479683894262,
12.5770542771492));
#433850=CARTESIAN_POINT('Ctrl Pts',(-2.6473647302611,-0.3921074328766,12.5737548217797));
#433851=CARTESIAN_POINT('',(-2.65059728690124,-0.36962450760124,12.5737548217797));
#433852=CARTESIAN_POINT('Origin',(-2.6660045512589,-0.371773043152011,12.5893111709658));
#433853=CARTESIAN_POINT('Ctrl Pts',(-2.6473647302611,-0.3921074328766,12.5737548217797));
#433854=CARTESIAN_POINT('Ctrl Pts',(-2.64648765276873,-0.391622608471913,
12.5746934679442));
#433855=CARTESIAN_POINT('Ctrl Pts',(-2.6456057291367,-0.390925797058764,
12.5756680099006));
#433856=CARTESIAN_POINT('Ctrl Pts',(-2.64481723279475,-0.390098888849399,
12.5765688348656));
#433857=CARTESIAN_POINT('Ctrl Pts',(-2.64460848711716,-0.389879974055145,
12.5768073183026));
#433858=CARTESIAN_POINT('Ctrl Pts',(-2.64440615217106,-0.389652158560094,
12.5770407398754));
#433859=CARTESIAN_POINT('Ctrl Pts',(-2.64421164066685,-0.389417347108852,
12.5772674179684));
#433860=CARTESIAN_POINT('Ctrl Pts',(-2.64341341805172,-0.388453744408658,
12.5781976435658));
#433861=CARTESIAN_POINT('Ctrl Pts',(-2.64271029640937,-0.3873103995618,
12.5790594849312));
#433862=CARTESIAN_POINT('Ctrl Pts',(-2.64219088513729,-0.386039217177518,
12.5797571720115));
#433863=CARTESIAN_POINT('Ctrl Pts',(-2.64185247001716,-0.385210996146513,
12.580211740231));
#433864=CARTESIAN_POINT('Ctrl Pts',(-2.64159403867823,-0.384283768977268,
12.5806009430798));
#433865=CARTESIAN_POINT('Ctrl Pts',(-2.64145084978923,-0.383318051831108,
12.5808812374708));
#433866=CARTESIAN_POINT('Ctrl Pts',(-2.64132780303116,-0.38248818042923,
12.5811221033394));
#433867=CARTESIAN_POINT('Ctrl Pts',(-2.64128745098348,-0.381612879643817,
12.581287365893));
#433868=CARTESIAN_POINT('Ctrl Pts',(-2.64134040031586,-0.380741168882355,
12.581359338449));
#433869=CARTESIAN_POINT('Ctrl Pts',(-2.6413477591797,-0.380620019086649,
12.5813693411482));
#433870=CARTESIAN_POINT('Ctrl Pts',(-2.64135686504362,-0.380498915290669,
12.5813775999465));
#433871=CARTESIAN_POINT('Ctrl Pts',(-2.64136769032387,-0.380377964172472,
12.5813841266931));
#433872=CARTESIAN_POINT('Ctrl Pts',(-2.64138605672111,-0.380172755971718,
12.5813952001081));
#433873=CARTESIAN_POINT('Ctrl Pts',(-2.64141010195379,-0.379966667148885,
12.5814007534795));
#433874=CARTESIAN_POINT('Ctrl Pts',(-2.64144001143049,-0.37975981031663,
12.5814005856065));
#433875=CARTESIAN_POINT('Ctrl Pts',(-2.64157692532093,-0.378812900614344,
12.5813998171494));
#433876=CARTESIAN_POINT('Ctrl Pts',(-2.6418269278145,-0.377915273545959,
12.58127954464));
#433877=CARTESIAN_POINT('Ctrl Pts',(-2.642160095108,-0.37706408633878,12.5810700125799));
#433878=CARTESIAN_POINT('Ctrl Pts',(-2.64256252326442,-0.37603594910793,
12.5808169217085));
#433879=CARTESIAN_POINT('Ctrl Pts',(-2.64310190902808,-0.375081574256301,
12.5804173076348));
#433880=CARTESIAN_POINT('Ctrl Pts',(-2.64370830958714,-0.37427178803166,
12.5799304713245));
#433881=CARTESIAN_POINT('Ctrl Pts',(-2.6444598309157,-0.37326820779036,
12.5793271277669));
#433882=CARTESIAN_POINT('Ctrl Pts',(-2.64533512402048,-0.372405146501036,
12.5785808224116));
#433883=CARTESIAN_POINT('Ctrl Pts',(-2.64627502476683,-0.37169639940228,
12.5777485681082));
#433884=CARTESIAN_POINT('Ctrl Pts',(-2.64767557985272,-0.37064028857609,
12.576508418016));
#433885=CARTESIAN_POINT('Ctrl Pts',(-2.6492036608637,-0.36993022665298,
12.5750928681475));
#433886=CARTESIAN_POINT('Ctrl Pts',(-2.65059728690124,-0.36962450760124,
12.5737548217797));
#433887=CARTESIAN_POINT('Ctrl Pts',(-2.65059728690124,-0.36962450760124,
12.5737548217797));
#433888=CARTESIAN_POINT('Ctrl Pts',(-2.64954321694341,-0.353293781610674,
12.5770542771492));
#433889=CARTESIAN_POINT('Ctrl Pts',(-2.66051922500485,-0.350467851393039,
12.5893111709658));
#433890=CARTESIAN_POINT('Ctrl Pts',(-2.6745869977036,-0.363500070501432,
12.5508408821982));
#433891=CARTESIAN_POINT('Ctrl Pts',(-2.67352645459423,-0.347118954149279,
12.55409748406));
#433892=CARTESIAN_POINT('Ctrl Pts',(-2.68451646523087,-0.34428941876845,
12.5663972313419));
#433893=CARTESIAN_POINT('Ctrl Pts',(-2.6985529818157,-0.357380473347283,
12.52790050457));
#433894=CARTESIAN_POINT('Ctrl Pts',(-2.69746375863649,-0.340955952952226,
12.5311362602938));
#433895=CARTESIAN_POINT('Ctrl Pts',(-2.70848949618474,-0.338117219167138,
12.5434568539655));
#433896=CARTESIAN_POINT('Ctrl Pts',(-2.72249707968045,-0.351265326595135,
12.5049357605811));
#433897=CARTESIAN_POINT('Ctrl Pts',(-2.72135991741408,-0.334803545191858,
12.5081700652078));
#433898=CARTESIAN_POINT('Ctrl Pts',(-2.73244021394163,-0.331950764417438,
12.5204921097672));
#433899=CARTESIAN_POINT('Ctrl Pts',(-2.72092481596393,-0.35166686956375,
12.5064436508395));
#433900=CARTESIAN_POINT('Ctrl Pts',(-2.72128471078529,-0.35050096926435,
12.5062361689309));
#433901=CARTESIAN_POINT('Ctrl Pts',(-2.72160925536991,-0.349273181647114,
12.5061871075061));
#433902=CARTESIAN_POINT('Ctrl Pts',(-2.7218561031364,-0.348068987800056,
12.5063648335164));
#433903=CARTESIAN_POINT('Ctrl Pts',(-2.72196823661814,-0.347521968676965,
12.5064455676329));
#433904=CARTESIAN_POINT('Ctrl Pts',(-2.72206568527824,-0.34697214419377,
12.506574497099));
#433905=CARTESIAN_POINT('Ctrl Pts',(-2.72214323598872,-0.346442905767576,
12.5067492519495));
#433906=CARTESIAN_POINT('Ctrl Pts',(-2.72229907715176,-0.345379380606543,
12.5071004286051));
#433907=CARTESIAN_POINT('Ctrl Pts',(-2.72237949557313,-0.344359767812568,
12.5076537929613));
#433908=CARTESIAN_POINT('Ctrl Pts',(-2.7223878845934,-0.343461338365866,
12.5083435010505));
#433909=CARTESIAN_POINT('Ctrl Pts',(-2.72238841273236,-0.34340477686315,
12.5083869222964));
#433910=CARTESIAN_POINT('Ctrl Pts',(-2.72238864350928,-0.343348689385558,
12.5084308732337));
#433911=CARTESIAN_POINT('Ctrl Pts',(-2.72238857311952,-0.343293092307382,
12.5084753333615));
#433912=CARTESIAN_POINT('Ctrl Pts',(-2.7223880085008,-0.342847130358932,
12.5088319622689));
#433913=CARTESIAN_POINT('Ctrl Pts',(-2.72236934496448,-0.342423666084951,
12.509227847131));
#433914=CARTESIAN_POINT('Ctrl Pts',(-2.72233593481234,-0.342035167997174,
12.5096423454524));
#433915=CARTESIAN_POINT('Ctrl Pts',(-2.72223124218224,-0.340817786932132,
12.5109411997424));
#433916=CARTESIAN_POINT('Ctrl Pts',(-2.72198494364145,-0.339868040061396,
12.5124831113042));
#433917=CARTESIAN_POINT('Ctrl Pts',(-2.72167138001856,-0.339127367171464,
12.5140723025008));
#433918=CARTESIAN_POINT('Ctrl Pts',(-2.72164199876366,-0.339057965310441,
12.5142212114565));
#433919=CARTESIAN_POINT('Ctrl Pts',(-2.72161204226112,-0.338990373768649,
12.5143705582413));
#433920=CARTESIAN_POINT('Ctrl Pts',(-2.7215815817509,-0.338924530702661,
12.5145201959299));
#433921=CARTESIAN_POINT('Ctrl Pts',(-2.72119027114618,-0.338078678489976,
12.5164425148273));
#433922=CARTESIAN_POINT('Ctrl Pts',(-2.72071212114258,-0.337487890580984,
12.518463520594));
#433923=CARTESIAN_POINT('Ctrl Pts',(-2.72017862832111,-0.337067633290473,
12.5205025929157));
#433924=CARTESIAN_POINT('Ctrl Pts',(-2.71986918133898,-0.336823867404533,
12.5216853356836));
#433925=CARTESIAN_POINT('Ctrl Pts',(-2.71954197270307,-0.336637536346651,
12.5228750347131));
#433926=CARTESIAN_POINT('Ctrl Pts',(-2.71920857069333,-0.336494529534027,
12.5240609649613));
#433927=CARTESIAN_POINT('Ctrl Pts',(-2.71839025334684,-0.336143526984493,
12.5269717671327));
#433928=CARTESIAN_POINT('Ctrl Pts',(-2.717507496463,-0.33605319829466,12.5299036066169));
#433929=CARTESIAN_POINT('Ctrl Pts',(-2.71658286729487,-0.336139876017347,
12.5328133004019));
#433930=CARTESIAN_POINT('Ctrl Pts',(-2.71613899145463,-0.336181486371329,
12.5342101228451));
#433931=CARTESIAN_POINT('Ctrl Pts',(-2.71568606864433,-0.336264358770682,
12.5356023438238));
#433932=CARTESIAN_POINT('Ctrl Pts',(-2.71522896268844,-0.336382047150414,
12.5369868989719));
#433933=CARTESIAN_POINT('Origin',(-15.0568630004311,2.84661798304233,-1.24021445932235));
#433934=CARTESIAN_POINT('Ctrl Pts',(-2.69997696638848,-0.442190819974361,
12.5369868989719));
#433935=CARTESIAN_POINT('Ctrl Pts',(-2.71316717411687,-0.450020361708556,
12.5369868989719));
#433936=CARTESIAN_POINT('Ctrl Pts',(-2.71038156804597,-0.46510425054743,
12.5369868989719));
#433937=CARTESIAN_POINT('Ctrl Pts',(-2.70443573866972,-0.444837568228778,
12.5218025310016));
#433938=CARTESIAN_POINT('Ctrl Pts',(-2.71249659261995,-0.453479240364314,
12.5216901060418));
#433939=CARTESIAN_POINT('Ctrl Pts',(-2.71039007571397,-0.465058272850304,
12.5161920673678));
#433940=CARTESIAN_POINT('Ctrl Pts',(-2.70995859330271,-0.442422170145969,
12.5042015548894));
#433941=CARTESIAN_POINT('Ctrl Pts',(-2.71339584088752,-0.447859326945022,
12.4980677368514));
#433942=CARTESIAN_POINT('Ctrl Pts',(-2.71228302125259,-0.454563982952899,
12.4907278922777));
#433943=CARTESIAN_POINT('Ctrl Pts',(-2.70976449409411,-0.429148086365825,
12.506463626192));
#433944=CARTESIAN_POINT('Ctrl Pts',(-2.71622669490464,-0.430171511507603,
12.4999376786891));
#433945=CARTESIAN_POINT('Ctrl Pts',(-2.71614776851777,-0.430159011857555,
12.4906970594712));
#433946=CARTESIAN_POINT('Origin',(-2.68874738752638,-0.461108974180832,
12.5369868989719));
#433947=CARTESIAN_POINT('Origin',(-2.68874738752638,-0.461108974180832,
14.));
#433948=CARTESIAN_POINT('Origin',(-2.68874738752638,-0.461108974180832,
13.7435492065112));
#433949=CARTESIAN_POINT('Ctrl Pts',(-2.67874530785786,-0.429533351359827,
13.793642941384));
#433950=CARTESIAN_POINT('Ctrl Pts',(-2.68804640273655,-0.435046594784841,
13.8071662555867));
#433951=CARTESIAN_POINT('Ctrl Pts',(-2.68161100476447,-0.450813808761179,
13.8103758687955));
#433952=CARTESIAN_POINT('Ctrl Pts',(-2.6930219368263,-0.438044495261849,
13.7804579775006));
#433953=CARTESIAN_POINT('Ctrl Pts',(-2.70449347638579,-0.444856062766058,
13.7901904343352));
#433954=CARTESIAN_POINT('Ctrl Pts',(-2.70097811382212,-0.460215038975772,
13.7927914348262));
#433955=CARTESIAN_POINT('Ctrl Pts',(-2.70142712557053,-0.443055326020003,
13.7597120340895));
#433956=CARTESIAN_POINT('Ctrl Pts',(-2.71470000174282,-0.450943155131201,
13.7635825532445));
#433957=CARTESIAN_POINT('Ctrl Pts',(-2.71238771299,-0.465781929907696,13.7651073818884));
#433958=CARTESIAN_POINT('Ctrl Pts',(-2.69978119715705,-0.442074090623276,
13.7381884353898));
#433959=CARTESIAN_POINT('Ctrl Pts',(-2.7127438561261,-0.449776517713384,
13.7368803041982));
#433960=CARTESIAN_POINT('Ctrl Pts',(-2.71015315771698,-0.464692211424101,
13.7363986145813));
#433961=CARTESIAN_POINT('Origin',(-2.67094402177385,-0.450495329333152,
13.7902182540695));
#433962=CARTESIAN_POINT('Ctrl Pts',(-2.65148432505612,-0.41328142794726,
13.8235227101244));
#433963=CARTESIAN_POINT('Ctrl Pts',(-2.66136194626255,-0.419164903758537,
13.8358800583119));
#433964=CARTESIAN_POINT('Ctrl Pts',(-2.65557424054822,-0.434693216983779,
13.8390832900376));
#433965=CARTESIAN_POINT('Ctrl Pts',(-2.66172945797254,-0.419389160817917,
13.8124254819052));
#433966=CARTESIAN_POINT('Ctrl Pts',(-2.671626261237,-0.425284062494811,
13.8247886449158));
#433967=CARTESIAN_POINT('Ctrl Pts',(-2.66581527150809,-0.440826043690033,
13.8279860620657));
#433968=CARTESIAN_POINT('Ctrl Pts',(-2.67196999935371,-0.4254941564014,
13.8013225099955));
#433969=CARTESIAN_POINT('Ctrl Pts',(-2.68188131600011,-0.43139770077468,
13.8136962257787));
#433970=CARTESIAN_POINT('Ctrl Pts',(-2.67605170063459,-0.446955798652356,
13.8168830918626));
#433971=CARTESIAN_POINT('Ctrl Pts',(-2.68220612784919,-0.431596521201332,
13.7902140179785));
#433972=CARTESIAN_POINT('Ctrl Pts',(-2.69212759433233,-0.437506107004801,
13.802602731458));
#433973=CARTESIAN_POINT('Ctrl Pts',(-2.6862837096904,-0.45308260098815,
13.8057746032558));
#433974=CARTESIAN_POINT('Origin',(-2.64022220827511,-0.432180229700599,
13.8235269408515));
#433975=CARTESIAN_POINT('Ctrl Pts',(-2.66051922500485,-0.35046785139304,
13.8235269408515));
#433976=CARTESIAN_POINT('Ctrl Pts',(-2.67195380032408,-0.347523856477988,
13.8362179249168));
#433977=CARTESIAN_POINT('Ctrl Pts',(-2.67042675019419,-0.330514120384856,
13.8391868794938));
#433978=CARTESIAN_POINT('Ctrl Pts',(-2.65005708630518,-0.353161478595842,
13.8400110824519));
#433979=CARTESIAN_POINT('Ctrl Pts',(-2.65837185055042,-0.347488158720583,
13.8494522556836));
#433980=CARTESIAN_POINT('Ctrl Pts',(-2.65323703773573,-0.335055878769023,
13.85569149686));
#433981=CARTESIAN_POINT('Ctrl Pts',(-2.63732583736909,-0.363325780174028,
13.8586819406588));
#433982=CARTESIAN_POINT('Ctrl Pts',(-2.63795921881506,-0.359018243571877,
13.868010383617));
#433983=CARTESIAN_POINT('Ctrl Pts',(-2.63219400367951,-0.352042918401439,
13.8744918421245));
#433984=CARTESIAN_POINT('Ctrl Pts',(-2.63282061411247,-0.394289863582954,
13.8587686893867));
#433985=CARTESIAN_POINT('Ctrl Pts',(-2.63219281404613,-0.398559054957974,
13.8680909899357));
#433986=CARTESIAN_POINT('Ctrl Pts',(-2.62469667610912,-0.403589394661724,
13.8745789365163));
#433987=CARTESIAN_POINT('Ctrl Pts',(-2.64219314042693,-0.407742399494244,
13.8400379222776));
#433988=CARTESIAN_POINT('Ctrl Pts',(-2.64856557525381,-0.41553100067065,
13.8494748685453));
#433989=CARTESIAN_POINT('Ctrl Pts',(-2.64014094388412,-0.426008915136298,
13.8557104837033));
#433990=CARTESIAN_POINT('Ctrl Pts',(-2.65148770641861,-0.413283442902624,
13.8235269408542));
#433991=CARTESIAN_POINT('Ctrl Pts',(-2.66162968187889,-0.419329677479087,
13.8362179249195));
#433992=CARTESIAN_POINT('Ctrl Pts',(-2.65537229156814,-0.43522018000592,
13.8391868794965));
#433993=CARTESIAN_POINT('Origin',(-2.65503389875079,-0.329162659634068,
13.8235269408515));
#433994=CARTESIAN_POINT('Ctrl Pts',(-2.69515273048745,-0.341550959409045,
13.7902140241682));
#433995=CARTESIAN_POINT('Ctrl Pts',(-2.70633722451106,-0.338675948308463,
13.8026027327198));
#433996=CARTESIAN_POINT('Ctrl Pts',(-2.70511846421998,-0.322084005817412,
13.8057746032556));
#433997=CARTESIAN_POINT('Ctrl Pts',(-2.68361200227733,-0.344522284904809,
13.8013225161808));
#433998=CARTESIAN_POINT('Ctrl Pts',(-2.69478505554331,-0.341650210985101,
13.8136962270464));
#433999=CARTESIAN_POINT('Ctrl Pts',(-2.69357480373718,-0.325079939536543,
13.8168830918628));
#434000=CARTESIAN_POINT('Ctrl Pts',(-2.67206629875538,-0.347494891365753,
13.8124254880875));
#434001=CARTESIAN_POINT('Ctrl Pts',(-2.68322299161573,-0.344627021169827,
13.8247886461867));
#434002=CARTESIAN_POINT('Ctrl Pts',(-2.68202607037744,-0.328077461002025,
13.8279860620656));
#434003=CARTESIAN_POINT('Ctrl Pts',(-2.66051541850163,-0.350468830650333,
13.8235227163065));
#434004=CARTESIAN_POINT('Ctrl Pts',(-2.67165048728972,-0.347606519290379,
13.8358800595847));
#434005=CARTESIAN_POINT('Ctrl Pts',(-2.67047205618014,-0.33107663329809,
13.8390832900376));
#434006=CARTESIAN_POINT('Origin',(-2.6896712227878,-0.32024478529339,13.7902182540695));
#434007=CARTESIAN_POINT('Ctrl Pts',(-2.7149676186762,-0.33644930541918,
13.7382347919292));
#434008=CARTESIAN_POINT('Ctrl Pts',(-2.72958732243381,-0.332710036670744,
13.7369371795943));
#434009=CARTESIAN_POINT('Ctrl Pts',(-2.7312968939767,-0.317656095586762,
13.7364597369711));
#434010=CARTESIAN_POINT('Ctrl Pts',(-2.71679943782014,-0.335977677803303,
13.7595490285573));
#434011=CARTESIAN_POINT('Ctrl Pts',(-2.73176770604075,-0.332148219239129,
13.7633824266926));
#434012=CARTESIAN_POINT('Ctrl Pts',(-2.73371797887451,-0.317245531690206,
13.7648920890506));
#434013=CARTESIAN_POINT('Ctrl Pts',(-2.70745726054319,-0.338382952814148,
13.7803806590111));
#434014=CARTESIAN_POINT('Ctrl Pts',(-2.72040561484516,-0.3350758382297,
13.7901039518744));
#434015=CARTESIAN_POINT('Ctrl Pts',(-2.72137564442225,-0.319342291774907,
13.7926933640892));
#434016=CARTESIAN_POINT('Ctrl Pts',(-2.6912184709803,-0.342563857633278,
13.7936647693663));
#434017=CARTESIAN_POINT('Ctrl Pts',(-2.70169975050101,-0.33989625354848,
13.8072068914933));
#434018=CARTESIAN_POINT('Ctrl Pts',(-2.69995480263794,-0.322937496907673,
13.8104111085397));
#434019=CARTESIAN_POINT('Origin',(-2.70974363643439,-0.315076855391442,
13.7435492065112));
#434020=CARTESIAN_POINT('Origin',(-2.70974363643439,-0.315076855391442,
14.));
#434021=CARTESIAN_POINT('Origin',(-2.70974363643439,-0.315076855391443,
12.5369868989719));
#434022=CARTESIAN_POINT('Ctrl Pts',(-2.72090658436879,-0.351664513225318,
12.506462012331));
#434023=CARTESIAN_POINT('Ctrl Pts',(-2.72739127020971,-0.352502628691232,
12.4999388158272));
#434024=CARTESIAN_POINT('Ctrl Pts',(-2.72731454787207,-0.352492712686149,
12.4907030323752));
#434025=CARTESIAN_POINT('Ctrl Pts',(-2.72483052715391,-0.338982586866375,
12.5042014951932));
#434026=CARTESIAN_POINT('Ctrl Pts',(-2.72965888100028,-0.33473663629545,
12.4980716682128));
#434027=CARTESIAN_POINT('Ctrl Pts',(-2.73048103604559,-0.327995002494423,
12.4907355092744));
#434028=CARTESIAN_POINT('Ctrl Pts',(-2.72021405179254,-0.335107815068892,
12.5218047446509));
#434029=CARTESIAN_POINT('Ctrl Pts',(-2.73037746320019,-0.329089182375839,
12.5216906929433));
#434030=CARTESIAN_POINT('Ctrl Pts',(-2.73162154168198,-0.317392044988393,
12.5161988840775));
#434031=CARTESIAN_POINT('Ctrl Pts',(-2.71519175147824,-0.336391593073828,
12.5369868989719));
#434032=CARTESIAN_POINT('Ctrl Pts',(-2.73004414179213,-0.33259527466203,
12.5369868989719));
#434033=CARTESIAN_POINT('Ctrl Pts',(-2.73162617230327,-0.317347235083714,
12.5369868989719));
#434034=CARTESIAN_POINT('Origin',(-5.09942406832773E-31,-5.88504909413694E-31,
12.5));
#434035=CARTESIAN_POINT('Origin',(-2.6231001832877,-0.566158714422425,12.5));
#434036=CARTESIAN_POINT('',(-2.6231001832877,-0.566158714422425,12.5893111709658));
#434037=CARTESIAN_POINT('',(-2.6231001832877,-0.566158714422425,13.8235269408515));
#434038=CARTESIAN_POINT('',(-2.6231001832877,-0.566158714422425,12.5));
#434039=CARTESIAN_POINT('',(-2.65834914403464,-0.560093777039188,13.7902182540695));
#434040=CARTESIAN_POINT('',(-2.6231001832877,-0.566158714422425,13.8235269408515));
#434041=CARTESIAN_POINT('',(-2.6787760026444,-0.556579131053058,13.7435492065112));
#434042=CARTESIAN_POINT('Origin',(-2.61157196305983,-0.568142590928179,
13.7445212918702));
#434043=CARTESIAN_POINT('',(-2.6787760026444,-0.556579131053058,12.5369868989719));
#434044=CARTESIAN_POINT('',(-2.6787760026444,-0.556579131053058,12.5));
#434045=CARTESIAN_POINT('Ctrl Pts',(-2.6787760026444,-0.556579131053058,
12.5369868989719));
#434046=CARTESIAN_POINT('Ctrl Pts',(-2.66023093171095,-0.559769996587692,
12.5544431401645));
#434047=CARTESIAN_POINT('Ctrl Pts',(-2.64167259684988,-0.562963144314164,
12.5718848856037));
#434048=CARTESIAN_POINT('Ctrl Pts',(-2.6231001832877,-0.566158714422425,
12.5893111709658));
#434049=CARTESIAN_POINT('Origin',(-2.83292449524894,-0.787632598180569,
12.5));
#434050=CARTESIAN_POINT('',(-2.65498441696279,-0.660816878682771,13.7435492065112));
#434051=CARTESIAN_POINT('',(-2.63810540102849,-0.648787410275543,13.7902182540695));
#434052=CARTESIAN_POINT('Origin',(-2.59375026443174,-0.617176046410157,
13.7418732680438));
#434053=CARTESIAN_POINT('',(-2.60897866247894,-0.62802913961858,13.8235269408515));
#434054=CARTESIAN_POINT('',(-2.63810540102849,-0.648787410275543,13.7902182540695));
#434055=CARTESIAN_POINT('',(-2.60897866247894,-0.62802913961858,12.5893111709658));
#434056=CARTESIAN_POINT('',(-2.60897866247894,-0.62802913961858,12.5));
#434057=CARTESIAN_POINT('',(-2.65498441696279,-0.660816878682771,12.5369868989719));
#434058=CARTESIAN_POINT('Ctrl Pts',(-2.60897866247894,-0.62802913961858,
12.5893111709658));
#434059=CARTESIAN_POINT('Ctrl Pts',(-2.62432532299308,-0.638966517042117,
12.5718848856037));
#434060=CARTESIAN_POINT('Ctrl Pts',(-2.6396603500679,-0.6498956034556,12.5544431401645));
#434061=CARTESIAN_POINT('Ctrl Pts',(-2.65498441696279,-0.660816878682771,
12.5369868989719));
#434062=CARTESIAN_POINT('',(-2.65498441696279,-0.660816878682771,12.5));
#434063=CARTESIAN_POINT('Origin',(-2.62892909479919,-0.600035910522329,
12.5));
#434064=CARTESIAN_POINT('',(-2.59568356470713,-0.591299498153624,13.8587068136939));
#434065=CARTESIAN_POINT('Ctrl Pts',(-2.60897866247499,-0.628029139623877,
13.8235269408542));
#434066=CARTESIAN_POINT('Ctrl Pts',(-2.60755168099091,-0.62701214735683,
13.8262006681044));
#434067=CARTESIAN_POINT('Ctrl Pts',(-2.60619220811089,-0.625829920001143,
13.8288634856214));
#434068=CARTESIAN_POINT('Ctrl Pts',(-2.60489658299874,-0.624495279581872,
13.8314912288862));
#434069=CARTESIAN_POINT('Ctrl Pts',(-2.60356092714564,-0.62311940297138,
13.8342001611531));
#434070=CARTESIAN_POINT('Ctrl Pts',(-2.60229128529472,-0.621580367473445,
13.8368750301949));
#434071=CARTESIAN_POINT('Ctrl Pts',(-2.60109913746691,-0.619849756981623,
13.8394886372968));
#434072=CARTESIAN_POINT('Ctrl Pts',(-2.60100706499842,-0.619716097735462,
13.8396904925131));
#434073=CARTESIAN_POINT('Ctrl Pts',(-2.60091547057203,-0.619581280254489,
13.8398919674349));
#434074=CARTESIAN_POINT('Ctrl Pts',(-2.6008243683139,-0.619445284177259,
13.8400930404591));
#434075=CARTESIAN_POINT('Ctrl Pts',(-2.59940493384158,-0.61732637380038,
13.8432258934518));
#434076=CARTESIAN_POINT('Ctrl Pts',(-2.59811128460748,-0.614932788927828,
13.8462331177034));
#434077=CARTESIAN_POINT('Ctrl Pts',(-2.59707047719378,-0.612296729002257,
13.8489036603661));
#434078=CARTESIAN_POINT('Ctrl Pts',(-2.59672991289554,-0.611434179517238,
13.8497774930041));
#434079=CARTESIAN_POINT('Ctrl Pts',(-2.59641662386316,-0.610545813062039,
13.85061494757));
#434080=CARTESIAN_POINT('Ctrl Pts',(-2.59613563742903,-0.609633179318732,
13.8514076489583));
#434081=CARTESIAN_POINT('Ctrl Pts',(-2.59554131059654,-0.607702827330148,
13.8530843267192));
#434082=CARTESIAN_POINT('Ctrl Pts',(-2.59503594870946,-0.605473425735505,
13.8546805203176));
#434083=CARTESIAN_POINT('Ctrl Pts',(-2.59478195249114,-0.603044203893294,
13.8559412814273));
#434084=CARTESIAN_POINT('Ctrl Pts',(-2.59474795955984,-0.602719095229282,
13.8561100121513));
#434085=CARTESIAN_POINT('Ctrl Pts',(-2.59471841584751,-0.602390463152217,
13.8562727473908));
#434086=CARTESIAN_POINT('Ctrl Pts',(-2.59469365183714,-0.602058593428518,
13.8564289040185));
#434087=CARTESIAN_POINT('Ctrl Pts',(-2.59458134733266,-0.60055356801762,
13.8571370725437));
#434088=CARTESIAN_POINT('Ctrl Pts',(-2.59456763887773,-0.598955333235754,
13.8577210840553));
#434089=CARTESIAN_POINT('Ctrl Pts',(-2.59468240628542,-0.597325761037194,
13.8581177131616));
#434090=CARTESIAN_POINT('Ctrl Pts',(-2.5947147287376,-0.596866817417908,
13.8582294175695));
#434091=CARTESIAN_POINT('Ctrl Pts',(-2.59475706544722,-0.596405410654961,
13.8583265086086));
#434092=CARTESIAN_POINT('Ctrl Pts',(-2.59480964529635,-0.59594295238792,
13.8584082369006));
#434093=CARTESIAN_POINT('Ctrl Pts',(-2.5948851884397,-0.59527852387127,
13.8585256585398));
#434094=CARTESIAN_POINT('Ctrl Pts',(-2.59498313590912,-0.594603700958181,
13.8586122832068));
#434095=CARTESIAN_POINT('Ctrl Pts',(-2.59510172481113,-0.593936127022992,
13.8586682984299));
#434096=CARTESIAN_POINT('Ctrl Pts',(-2.5951965841774,-0.593402134049317,
13.8587131050557));
#434097=CARTESIAN_POINT('Ctrl Pts',(-2.59530546764148,-0.592866840303779,
13.8587357943552));
#434098=CARTESIAN_POINT('Ctrl Pts',(-2.59542888442484,-0.592330283127177,
13.8587355499465));
#434099=CARTESIAN_POINT('Ctrl Pts',(-2.5955086516343,-0.591983493431892,
13.8587353919793));
#434100=CARTESIAN_POINT('Ctrl Pts',(-2.59559358963261,-0.591639917426194,
13.8587257282814));
#434101=CARTESIAN_POINT('Ctrl Pts',(-2.59568356470713,-0.591299498153624,
13.8587068136939));
#434102=CARTESIAN_POINT('Ctrl Pts',(-2.59568356470713,-0.591299498153624,
13.8587068136939));
#434103=CARTESIAN_POINT('Ctrl Pts',(-2.59597948782226,-0.590179877724025,
13.8586446046466));
#434104=CARTESIAN_POINT('Ctrl Pts',(-2.59632983082974,-0.589094361347527,
13.858482427929));
#434105=CARTESIAN_POINT('Ctrl Pts',(-2.59673044329909,-0.588041287734245,
13.8582284286032));
#434106=CARTESIAN_POINT('Ctrl Pts',(-2.59714142509146,-0.58696095670564,
13.8579678548414));
#434107=CARTESIAN_POINT('Ctrl Pts',(-2.59760774781866,-0.585912675293914,
13.857615680862));
#434108=CARTESIAN_POINT('Ctrl Pts',(-2.59810217383812,-0.584933832906813,
13.8571944833187));
#434109=CARTESIAN_POINT('Ctrl Pts',(-2.59933606453546,-0.582491031621999,
13.8561433417727));
#434110=CARTESIAN_POINT('Ctrl Pts',(-2.60079842058794,-0.580364270050159,
13.8546163505474));
#434111=CARTESIAN_POINT('Ctrl Pts',(-2.6022838197901,-0.578577203722447,
13.8528973491086));
#434112=CARTESIAN_POINT('Ctrl Pts',(-2.6025551803093,-0.578250733070091,
13.8525833129072));
#434113=CARTESIAN_POINT('Ctrl Pts',(-2.6028272552052,-0.577935469045686,
13.8522628768812));
#434114=CARTESIAN_POINT('Ctrl Pts',(-2.60309874948253,-0.577631382198665,
13.851937733538));
#434115=CARTESIAN_POINT('Ctrl Pts',(-2.60475672736609,-0.575774366013995,
13.8499521282529));
#434116=CARTESIAN_POINT('Ctrl Pts',(-2.60656086579594,-0.574152352378175,
13.847639871647));
#434117=CARTESIAN_POINT('Ctrl Pts',(-2.60836263214411,-0.572790843397887,
13.8452109780794));
#434118=CARTESIAN_POINT('Ctrl Pts',(-2.60917328411886,-0.572178272325822,
13.8441181685877));
#434119=CARTESIAN_POINT('Ctrl Pts',(-2.60998324793643,-0.571617747877346,
13.8430021611332));
#434120=CARTESIAN_POINT('Ctrl Pts',(-2.61077906410839,-0.571108284664993,
13.8418824960098));
#434121=CARTESIAN_POINT('Ctrl Pts',(-2.6126544252395,-0.569907721595472,
13.8392439765549));
#434122=CARTESIAN_POINT('Ctrl Pts',(-2.61453883245319,-0.568930134967618,
13.8364981347964));
#434123=CARTESIAN_POINT('Ctrl Pts',(-2.61642151080363,-0.568142563217421,
13.8336931113419));
#434124=CARTESIAN_POINT('Ctrl Pts',(-2.61825511995583,-0.567375518348159,
13.8309611966327));
#434125=CARTESIAN_POINT('Ctrl Pts',(-2.62008914444175,-0.566788464583941,
13.8281701127185));
#434126=CARTESIAN_POINT('Ctrl Pts',(-2.62191456720686,-0.566390239888157,
13.825358068512));
#434127=CARTESIAN_POINT('Ctrl Pts',(-2.62231032083238,-0.566303904344336,
13.8247484142932));
#434128=CARTESIAN_POINT('Ctrl Pts',(-2.62270560646835,-0.566226605323364,
13.8241378483365));
#434129=CARTESIAN_POINT('Ctrl Pts',(-2.6231001832877,-0.566158714422425,
13.8235269408515));
#434130=CARTESIAN_POINT('',(-2.59538959546303,-0.592506295129496,12.5969504640361));
#434131=CARTESIAN_POINT('Origin',(-2.62896139426152,-0.60004308182228,12.584524458991));
#434132=CARTESIAN_POINT('Origin',(-2.62896139426152,-0.60004308182228,12.584524458991));
#434133=CARTESIAN_POINT('Ctrl Pts',(-2.60897866247894,-0.62802913961858,
12.5893111709658));
#434134=CARTESIAN_POINT('Ctrl Pts',(-2.59974886987771,-0.621451179212954,
12.5770542771492));
#434135=CARTESIAN_POINT('Ctrl Pts',(-2.60659544658616,-0.606587530191593,
12.5737548217797));
#434136=CARTESIAN_POINT('Ctrl Pts',(-2.62916112128738,-0.642412931396569,
12.5663937883685));
#434137=CARTESIAN_POINT('Ctrl Pts',(-2.61991955480387,-0.635826579888902,
12.5540940315304));
#434138=CARTESIAN_POINT('Ctrl Pts',(-2.62679026430446,-0.620918214912444,
12.5508374392248));
#434139=CARTESIAN_POINT('Ctrl Pts',(-2.64932321624227,-0.656782210104961,
12.5434499600945));
#434140=CARTESIAN_POINT('Ctrl Pts',(-2.64005160213515,-0.650174444023033,
12.5311293540533));
#434141=CARTESIAN_POINT('Ctrl Pts',(-2.64696466844689,-0.635235860464691,
12.5278936106989));
#434142=CARTESIAN_POINT('Ctrl Pts',(-2.66946654247219,-0.67113811257241,
12.5204817579905));
#434143=CARTESIAN_POINT('Ctrl Pts',(-2.66014904021147,-0.664497642564215,
12.5081597038247));
#434144=CARTESIAN_POINT('Ctrl Pts',(-2.66712023761871,-0.649541491602016,
12.5049254088044));
#434145=CARTESIAN_POINT('Ctrl Pts',(-2.65498441696279,-0.660816878682772,
12.5369868989719));
#434146=CARTESIAN_POINT('Ctrl Pts',(-2.65574298656787,-0.661357501772333,
12.5342545179733));
#434147=CARTESIAN_POINT('Ctrl Pts',(-2.65653933042822,-0.661771860999872,
12.5314872231885));
#434148=CARTESIAN_POINT('Ctrl Pts',(-2.65735439204755,-0.661987025278552,
12.5287124745063));
#434149=CARTESIAN_POINT('Ctrl Pts',(-2.65808945507192,-0.662181071104868,
12.5262100684184));
#434150=CARTESIAN_POINT('Ctrl Pts',(-2.65883925125646,-0.662211958308881,
12.5237004536639));
#434151=CARTESIAN_POINT('Ctrl Pts',(-2.65961938347097,-0.662013982807086,
12.5212220730815));
#434152=CARTESIAN_POINT('Ctrl Pts',(-2.660216642168,-0.661862415434214,
12.5193246583486));
#434153=CARTESIAN_POINT('Ctrl Pts',(-2.66083866350011,-0.661574279900998,
12.517417831369));
#434154=CARTESIAN_POINT('Ctrl Pts',(-2.6614627907671,-0.661055020950102,
12.5155812248347));
#434155=CARTESIAN_POINT('Ctrl Pts',(-2.66172867233754,-0.66083381384599,
12.5147988205793));
#434156=CARTESIAN_POINT('Ctrl Pts',(-2.66199538317697,-0.66057065073144,
12.5140295443047));
#434157=CARTESIAN_POINT('Ctrl Pts',(-2.66226321725615,-0.660258805162506,
12.5132817086137));
#434158=CARTESIAN_POINT('Ctrl Pts',(-2.66266854790322,-0.659786869079438,
12.5121499604604));
#434159=CARTESIAN_POINT('Ctrl Pts',(-2.6630797785432,-0.659188586138715,
12.511049420657));
#434160=CARTESIAN_POINT('Ctrl Pts',(-2.66347463884435,-0.658434107871132,
12.5100666561697));
#434161=CARTESIAN_POINT('Ctrl Pts',(-2.66370136671998,-0.658000888187295,
12.5095023550643));
#434162=CARTESIAN_POINT('Ctrl Pts',(-2.66392473854761,-0.657510862307966,
12.5089719619137));
#434163=CARTESIAN_POINT('Ctrl Pts',(-2.66413475580849,-0.656970566058595,
12.5085043804652));
#434164=CARTESIAN_POINT('Ctrl Pts',(-2.66444208871311,-0.656179912876177,
12.5078201359221));
#434165=CARTESIAN_POINT('Ctrl Pts',(-2.66472861140739,-0.655258238986815,
12.5072563000949));
#434166=CARTESIAN_POINT('Ctrl Pts',(-2.6649668175144,-0.654265507080926,
12.5068768744332));
#434167=CARTESIAN_POINT('Ctrl Pts',(-2.66513858051571,-0.653549679036882,
12.5066032824114));
#434168=CARTESIAN_POINT('Ctrl Pts',(-2.6652882977942,-0.652784343060205,
12.5064197834844));
#434169=CARTESIAN_POINT('Ctrl Pts',(-2.66541014552271,-0.652012733749517,
12.5063282718343));
#434170=CARTESIAN_POINT('Ctrl Pts',(-2.66558800548322,-0.650886423040119,
12.5061946931565));
#434171=CARTESIAN_POINT('Ctrl Pts',(-2.66571133463889,-0.649722837890964,
12.5062515701262));
#434172=CARTESIAN_POINT('Ctrl Pts',(-2.66578785735661,-0.648595822410862,
12.5064436508398));
#434173=CARTESIAN_POINT('',(-2.60659544658616,-0.606587530191593,12.5737548217797));
#434174=CARTESIAN_POINT('Origin',(-2.6217469391639,-0.610113472996979,12.5893111709658));
#434175=CARTESIAN_POINT('Ctrl Pts',(-2.66578785735661,-0.648595822410862,
12.5064436508398));
#434176=CARTESIAN_POINT('Ctrl Pts',(-2.65702612076564,-0.642377111960802,
12.5164271754438));
#434177=CARTESIAN_POINT('Ctrl Pts',(-2.6482607900943,-0.636156106797407,
12.5264061185523));
#434178=CARTESIAN_POINT('Ctrl Pts',(-2.63949173930992,-0.629932725330953,
12.536380305637));
#434179=CARTESIAN_POINT('Ctrl Pts',(-2.62853220438458,-0.622154760735652,
12.5488460165097));
#434180=CARTESIAN_POINT('Ctrl Pts',(-2.61756685541717,-0.614373082093783,
12.5613043021964));
#434181=CARTESIAN_POINT('Ctrl Pts',(-2.60659544658616,-0.606587530191593,
12.5737548217797));
#434182=CARTESIAN_POINT('Ctrl Pts',(-2.6231001832877,-0.566158714422425,
12.5893111709658));
#434183=CARTESIAN_POINT('Ctrl Pts',(-2.61193035744024,-0.568080595037089,
12.5770542771492));
#434184=CARTESIAN_POINT('Ctrl Pts',(-2.61164981429194,-0.584442898371182,
12.5737548217797));
#434185=CARTESIAN_POINT('Ctrl Pts',(-2.61267883292203,-0.567951812320271,
12.5928319619712));
#434186=CARTESIAN_POINT('Ctrl Pts',(-2.6057244299613,-0.572454000214079,
12.5821634970843));
#434187=CARTESIAN_POINT('Ctrl Pts',(-2.60785196807089,-0.585086778368237,
12.5773203894503));
#434188=CARTESIAN_POINT('Ctrl Pts',(-2.59885999583447,-0.577418799216162,
12.5969440695591));
#434189=CARTESIAN_POINT('Ctrl Pts',(-2.59794770633483,-0.581333677301208,
12.5878292599214));
#434190=CARTESIAN_POINT('Ctrl Pts',(-2.60292780887921,-0.588462693555647,
12.5813877129824));
#434191=CARTESIAN_POINT('Ctrl Pts',(-2.5919989655928,-0.607236604460083,
12.596957478804));
#434192=CARTESIAN_POINT('Ctrl Pts',(-2.59290459109521,-0.603350676565965,
12.5878468778671));
#434193=CARTESIAN_POINT('Ctrl Pts',(-2.60047796425882,-0.599136236999139,
12.5814011370086));
#434194=CARTESIAN_POINT('Ctrl Pts',(-2.60035484264215,-0.621883048597696,
12.5928371701607));
#434195=CARTESIAN_POINT('Ctrl Pts',(-2.59605083325396,-0.614811233491929,
12.5821692192952));
#434196=CARTESIAN_POINT('Ctrl Pts',(-2.60344287797678,-0.604352672559195,
12.5773318885715));
#434197=CARTESIAN_POINT('Ctrl Pts',(-2.6089786624789,-0.628029139618622,
12.5893111709658));
#434198=CARTESIAN_POINT('Ctrl Pts',(-2.59974886987767,-0.621451179212996,
12.5770542771492));
#434199=CARTESIAN_POINT('Ctrl Pts',(-2.60659544658613,-0.606587530191637,
12.5737548217797));
#434200=CARTESIAN_POINT('',(-2.61164981429194,-0.584442898371182,12.5737548217797));
#434201=CARTESIAN_POINT('Origin',(-2.62683068665505,-0.587840119926364,
12.5893111709658));
#434202=CARTESIAN_POINT('Ctrl Pts',(-2.60659544658613,-0.606587530191637,
12.5737548217797));
#434203=CARTESIAN_POINT('Ctrl Pts',(-2.60576080518662,-0.60603282904214,
12.5746934679442));
#434204=CARTESIAN_POINT('Ctrl Pts',(-2.60493861268177,-0.605266451248091,
12.5756680099006));
#434205=CARTESIAN_POINT('Ctrl Pts',(-2.60422014069206,-0.60437802473566,
12.5765688348656));
#434206=CARTESIAN_POINT('Ctrl Pts',(-2.60402993318653,-0.604142823651705,
12.5768073183026));
#434207=CARTESIAN_POINT('Ctrl Pts',(-2.60384684057106,-0.603899274017432,
12.5770407398754));
#434208=CARTESIAN_POINT('Ctrl Pts',(-2.603672115601,-0.603649389388578,
12.5772674179684));
#434209=CARTESIAN_POINT('Ctrl Pts',(-2.60295509157148,-0.602623930443406,
12.5781976435658));
#434210=CARTESIAN_POINT('Ctrl Pts',(-2.60234750272771,-0.601427079040893,
12.5790594849312));
#434211=CARTESIAN_POINT('Ctrl Pts',(-2.60193343291919,-0.600117789570475,
12.5797571720116));
#434212=CARTESIAN_POINT('Ctrl Pts',(-2.60166365155031,-0.599264740402644,
12.580211740231));
#434213=CARTESIAN_POINT('Ctrl Pts',(-2.60148165774259,-0.598319533952032,
12.5806009430798));
#434214=CARTESIAN_POINT('Ctrl Pts',(-2.6014176602155,-0.597345358926255,
12.5808812374708));
#434215=CARTESIAN_POINT('Ctrl Pts',(-2.60136266510878,-0.596508219399915,
12.5811221033394));
#434216=CARTESIAN_POINT('Ctrl Pts',(-2.60139379246911,-0.595632542039162,
12.581287365893));
#434217=CARTESIAN_POINT('Ctrl Pts',(-2.60151761813658,-0.594768047685495,
12.581359338449));
#434218=CARTESIAN_POINT('Ctrl Pts',(-2.60153482734746,-0.594647900821458,
12.5813693411482));
#434219=CARTESIAN_POINT('Ctrl Pts',(-2.60155377399602,-0.594527942200814,
12.5813775999465));
#434220=CARTESIAN_POINT('Ctrl Pts',(-2.60157442189503,-0.594408275898322,
12.5813841266931));
#434221=CARTESIAN_POINT('Ctrl Pts',(-2.60160945355302,-0.594205247542808,
12.5813952001081));
#434222=CARTESIAN_POINT('Ctrl Pts',(-2.60165021692947,-0.59400180437322,
12.5814007534795));
#434223=CARTESIAN_POINT('Ctrl Pts',(-2.60169688763704,-0.593798073740026,
12.5814005856065));
#434224=CARTESIAN_POINT('Ctrl Pts',(-2.60191052788922,-0.592865474554778,
12.5813998171494));
#434225=CARTESIAN_POINT('Ctrl Pts',(-2.60223286345935,-0.59199121179055,
12.58127954464));
#434226=CARTESIAN_POINT('Ctrl Pts',(-2.60263430182559,-0.591170013065979,
12.5810700125799));
#434227=CARTESIAN_POINT('Ctrl Pts',(-2.60311919366459,-0.590178098507659,
12.5808169217085));
#434228=CARTESIAN_POINT('Ctrl Pts',(-2.60373457507701,-0.58927086420677,
12.5804173076348));
#434229=CARTESIAN_POINT('Ctrl Pts',(-2.60440496298324,-0.588513199754099,
12.5799304713245));
#434230=CARTESIAN_POINT('Ctrl Pts',(-2.60523578479302,-0.587574214808325,
12.5793271277669));
#434231=CARTESIAN_POINT('Ctrl Pts',(-2.60617851293955,-0.586785369798107,
12.5785808224116));
#434232=CARTESIAN_POINT('Ctrl Pts',(-2.60717305571194,-0.586155591633295,
12.5777485681082));
#434233=CARTESIAN_POINT('Ctrl Pts',(-2.60865503340311,-0.585217153170376,
12.576508418016));
#434234=CARTESIAN_POINT('Ctrl Pts',(-2.61023590648921,-0.584634006708146,
12.5750928681475));
#434235=CARTESIAN_POINT('Ctrl Pts',(-2.61164981429194,-0.584442898371182,
12.5737548217797));
#434236=CARTESIAN_POINT('Ctrl Pts',(-2.61164981429194,-0.584442898371182,
12.5737548217797));
#434237=CARTESIAN_POINT('Ctrl Pts',(-2.61193035744024,-0.568080595037088,
12.5770542771492));
#434238=CARTESIAN_POINT('Ctrl Pts',(-2.6231001832877,-0.566158714422425,
12.5893111709658));
#434239=CARTESIAN_POINT('Ctrl Pts',(-2.63605889979076,-0.580294223970602,
12.5508408821982));
#434240=CARTESIAN_POINT('Ctrl Pts',(-2.63633709860868,-0.563881170322734,
12.55409748406));
#434241=CARTESIAN_POINT('Ctrl Pts',(-2.64752117429318,-0.56195683788064,
12.5663972313419));
#434242=CARTESIAN_POINT('Ctrl Pts',(-2.66044394304741,-0.57614843946563,
12.52790050457));
#434243=CARTESIAN_POINT('Ctrl Pts',(-2.66069709505851,-0.559689788506306,
12.5311362602938));
#434244=CARTESIAN_POINT('Ctrl Pts',(-2.6719175285316,-0.557759200341832,
12.5434568539655));
#434245=CARTESIAN_POINT('Ctrl Pts',(-2.68480681013232,-0.572005306621965,
12.5049357605811));
#434246=CARTESIAN_POINT('Ctrl Pts',(-2.68501521968767,-0.555505611156697,
12.5081700652078));
#434247=CARTESIAN_POINT('Ctrl Pts',(-2.69629117555962,-0.553565469806416,
12.5204921097672));
#434248=CARTESIAN_POINT('Ctrl Pts',(-2.68320704851393,-0.572277359400397,
12.5064436508395));
#434249=CARTESIAN_POINT('Ctrl Pts',(-2.68366077751305,-0.571144673307105,
12.5062361689309));
#434250=CARTESIAN_POINT('Ctrl Pts',(-2.68408431829136,-0.56994742444845,
12.5061871075062));
#434251=CARTESIAN_POINT('Ctrl Pts',(-2.68442849767,-0.568767357841671,12.5063648335164));
#434252=CARTESIAN_POINT('Ctrl Pts',(-2.68458484517365,-0.568231298799345,
12.5064455676329));
#434253=CARTESIAN_POINT('Ctrl Pts',(-2.68472678538106,-0.567691246782228,
12.506574497099));
#434254=CARTESIAN_POINT('Ctrl Pts',(-2.6848472158929,-0.567170090456088,
12.5067492519495));
#434255=CARTESIAN_POINT('Ctrl Pts',(-2.68508922568121,-0.566122806588952,
12.5071004286051));
#434256=CARTESIAN_POINT('Ctrl Pts',(-2.68525248442525,-0.565113141320434,
12.5076537929612));
#434257=CARTESIAN_POINT('Ctrl Pts',(-2.68533407587227,-0.564218385106703,
12.5083435010503));
#434258=CARTESIAN_POINT('Ctrl Pts',(-2.68533921254146,-0.564162054855853,
12.5083869222963));
#434259=CARTESIAN_POINT('Ctrl Pts',(-2.68534401420061,-0.56410617281508,
12.5084308732336));
#434260=CARTESIAN_POINT('Ctrl Pts',(-2.68534847572309,-0.564050754994082,
12.5084753333615));
#434261=CARTESIAN_POINT('Ctrl Pts',(-2.685384263022,-0.563606230925559,
12.508831962269));
#434262=CARTESIAN_POINT('Ctrl Pts',(-2.68540017785663,-0.563182654442561,
12.509227847131));
#434263=CARTESIAN_POINT('Ctrl Pts',(-2.68539854507481,-0.562792725812558,
12.5096423454524));
#434264=CARTESIAN_POINT('Ctrl Pts',(-2.68539342865921,-0.561570862061311,
12.5109411997424));
#434265=CARTESIAN_POINT('Ctrl Pts',(-2.68522536284349,-0.560604199777341,
12.5124831113042));
#434266=CARTESIAN_POINT('Ctrl Pts',(-2.68497321429429,-0.559840433069102,
12.5140723025008));
#434267=CARTESIAN_POINT('Ctrl Pts',(-2.68494958769906,-0.559768867292009,
12.5142212114565));
#434268=CARTESIAN_POINT('Ctrl Pts',(-2.68492524021245,-0.559699058922436,
12.5143705582413));
#434269=CARTESIAN_POINT('Ctrl Pts',(-2.6849002478782,-0.559630952129454,
12.5145201959299));
#434270=CARTESIAN_POINT('Ctrl Pts',(-2.68457918413508,-0.558756018973192,
12.5164425148273));
#434271=CARTESIAN_POINT('Ctrl Pts',(-2.68415077983536,-0.558128223198006,
12.5184635205941));
#434272=CARTESIAN_POINT('Ctrl Pts',(-2.6836533170379,-0.557665879661304,
12.5205025929158));
#434273=CARTESIAN_POINT('Ctrl Pts',(-2.68336476889779,-0.557397702084433,
12.5216853356836));
#434274=CARTESIAN_POINT('Ctrl Pts',(-2.68305383673265,-0.557185320486293,
12.5228750347131));
#434275=CARTESIAN_POINT('Ctrl Pts',(-2.68273320047344,-0.557015614158095,
12.5240609649613));
#434276=CARTESIAN_POINT('Ctrl Pts',(-2.68194621597675,-0.556599079079963,
12.5269717671327));
#434277=CARTESIAN_POINT('Ctrl Pts',(-2.68107375902041,-0.556437098070245,
12.5299036066169));
#434278=CARTESIAN_POINT('Ctrl Pts',(-2.68014514144049,-0.55644812151892,
12.5328133004019));
#434279=CARTESIAN_POINT('Ctrl Pts',(-2.67969935093035,-0.55645341341616,
12.5342101228451));
#434280=CARTESIAN_POINT('Ctrl Pts',(-2.67924118031344,-0.55649909265067,
12.5356023438238));
#434281=CARTESIAN_POINT('Ctrl Pts',(-2.67877600264439,-0.556579131053058,
12.5369868989719));
#434282=CARTESIAN_POINT('Origin',(-15.2392792397904,1.6099572959598,-1.24075170958192));
#434283=CARTESIAN_POINT('Ctrl Pts',(-2.65495035883805,-0.660792654622976,
12.5369868989719));
#434284=CARTESIAN_POINT('Ctrl Pts',(-2.66745849690108,-0.669671268584721,
12.5369868989719));
#434285=CARTESIAN_POINT('Ctrl Pts',(-2.66345268273223,-0.684477914272724,
12.5369868989719));
#434286=CARTESIAN_POINT('Ctrl Pts',(-2.65917856036841,-0.663794027375063,
12.5218025310016));
#434287=CARTESIAN_POINT('Ctrl Pts',(-2.66650821598767,-0.673063979489715,
12.5216901060418));
#434288=CARTESIAN_POINT('Ctrl Pts',(-2.66346490970081,-0.684432783016522,
12.5161920673677));
#434289=CARTESIAN_POINT('Ctrl Pts',(-2.66487991552539,-0.661836830254383,
12.5042015548895));
#434290=CARTESIAN_POINT('Ctrl Pts',(-2.66786254719726,-0.667536062950742,
12.4980677368513));
#434291=CARTESIAN_POINT('Ctrl Pts',(-2.66620693867018,-0.67412770463767,
12.4907278922778));
#434292=CARTESIAN_POINT('Ctrl Pts',(-2.66576842322458,-0.648591094005551,
12.506463626192));
#434293=CARTESIAN_POINT('Ctrl Pts',(-2.67212570294493,-0.650137843142798,
12.4999376786891));
#434294=CARTESIAN_POINT('Ctrl Pts',(-2.67204805801663,-0.650118951851058,
12.4906970594712));
#434295=CARTESIAN_POINT('Origin',(-2.64221614027783,-0.678732545304372,
12.5369868989719));
#434296=CARTESIAN_POINT('Origin',(-2.64221614027783,-0.678732545304372,
14.));
#434297=CARTESIAN_POINT('Origin',(-2.64221614027783,-0.678732545304372,
13.7435492065112));
#434298=CARTESIAN_POINT('Ctrl Pts',(-2.63482104809799,-0.646446725415739,
13.793642941384));
#434299=CARTESIAN_POINT('Ctrl Pts',(-2.64364181382917,-0.652699749557833,
13.8071662555867));
#434300=CARTESIAN_POINT('Ctrl Pts',(-2.63594265479821,-0.66788995475232,
13.8103758687955));
#434301=CARTESIAN_POINT('Ctrl Pts',(-2.64835643551964,-0.656093226987222,
13.7804579775006));
#434302=CARTESIAN_POINT('Ctrl Pts',(-2.65923459849045,-0.663817166533145,
13.7901904343351));
#434303=CARTESIAN_POINT('Ctrl Pts',(-2.65447903385889,-0.678838502332587,
13.7927914348263));
#434304=CARTESIAN_POINT('Ctrl Pts',(-2.65632522746666,-0.66177248553203,
13.7597120340895));
#434305=CARTESIAN_POINT('Ctrl Pts',(-2.66891100793882,-0.670715931169972,
13.7635825532445));
#434306=CARTESIAN_POINT('Ctrl Pts',(-2.66539691523532,-0.685316858147909,
13.7651073818884));
#434307=CARTESIAN_POINT('Ctrl Pts',(-2.65476475553836,-0.660660356669375,
13.7381884353898));
#434308=CARTESIAN_POINT('Ctrl Pts',(-2.66705646301534,-0.669393731614178,
13.7368803041982));
#434309=CARTESIAN_POINT('Ctrl Pts',(-2.66325861743349,-0.684048628613317,
13.7363986145813));
#434310=CARTESIAN_POINT('Origin',(-2.62533712434353,-0.666703076897143,
13.7902182540695));
#434311=CARTESIAN_POINT('Ctrl Pts',(-2.60897545660127,-0.628026855760681,
13.8235227101244));
#434312=CARTESIAN_POINT('Ctrl Pts',(-2.61834065293983,-0.634695872619238,
13.8358800583119));
#434313=CARTESIAN_POINT('Ctrl Pts',(-2.61130650365314,-0.649700764917055,
13.8390832900376));
#434314=CARTESIAN_POINT('Ctrl Pts',(-2.61868866275269,-0.634949339097926,
13.8124254819052));
#434315=CARTESIAN_POINT('Ctrl Pts',(-2.62807204600843,-0.641631307319277,
13.8247886449157));
#434316=CARTESIAN_POINT('Ctrl Pts',(-2.62101357611637,-0.656647924244691,
13.8279860620657));
#434317=CARTESIAN_POINT('Ctrl Pts',(-2.62839751576113,-0.641868720003337,
13.8013225099955));
#434318=CARTESIAN_POINT('Ctrl Pts',(-2.63779465964678,-0.648560485138564,
13.8136962257787));
#434319=CARTESIAN_POINT('Ctrl Pts',(-2.6307163124341,-0.663591646957212,
13.8168830918626));
#434320=CARTESIAN_POINT('Ctrl Pts',(-2.63810218500068,-0.648785119187777,
13.7902140179785));
#434321=CARTESIAN_POINT('Ctrl Pts',(-2.64750895251766,-0.655483732956772,
13.802602731458));
#434322=CARTESIAN_POINT('Ctrl Pts',(-2.64041488405503,-0.670532066591058,
13.8057746032558));
#434323=CARTESIAN_POINT('Origin',(-2.59621038579398,-0.64594480624018,13.8235269408515));
#434324=CARTESIAN_POINT('Ctrl Pts',(-2.6231001832877,-0.566158714422425,
13.8235269408515));
#434325=CARTESIAN_POINT('Ctrl Pts',(-2.63473667391714,-0.564156539449527,
13.8362179249168));
#434326=CARTESIAN_POINT('Ctrl Pts',(-2.63460115632286,-0.547078933088014,
13.8391868794938));
#434327=CARTESIAN_POINT('Ctrl Pts',(-2.61245330086808,-0.567990617373133,
13.8400110824519));
#434328=CARTESIAN_POINT('Ctrl Pts',(-2.62120282665965,-0.563013905478216,
13.8494522556837));
#434329=CARTESIAN_POINT('Ctrl Pts',(-2.61709844574261,-0.550204457998946,
13.85569149686));
#434330=CARTESIAN_POINT('Ctrl Pts',(-2.59893592917315,-0.57708338309688,
13.8586819406588));
#434331=CARTESIAN_POINT('Ctrl Pts',(-2.59991830731691,-0.572841805935299,
13.868010383617));
#434332=CARTESIAN_POINT('Ctrl Pts',(-2.59474082921627,-0.565419772028747,
13.8744918421245));
#434333=CARTESIAN_POINT('Ctrl Pts',(-2.5919218364209,-0.607577218552753,
13.8587686893867));
#434334=CARTESIAN_POINT('Ctrl Pts',(-2.59094814657719,-0.611781033012038,
13.8680909899357));
#434335=CARTESIAN_POINT('Ctrl Pts',(-2.58306693203553,-0.616183629842783,
13.8745789365163));
#434336=CARTESIAN_POINT('Ctrl Pts',(-2.60016666986321,-0.621748940165471,
13.8400379222776));
#434337=CARTESIAN_POINT('Ctrl Pts',(-2.60588305763718,-0.630031038011176,
13.8494748685453));
#434338=CARTESIAN_POINT('Ctrl Pts',(-2.59663241123223,-0.639787402413708,
13.8557104837033));
#434339=CARTESIAN_POINT('Ctrl Pts',(-2.60897866247499,-0.628029139623877,
13.8235269408542));
#434340=CARTESIAN_POINT('Ctrl Pts',(-2.61859406710009,-0.634881921007085,
13.8362179249195));
#434341=CARTESIAN_POINT('Ctrl Pts',(-2.61106227426324,-0.65020951379653,
13.8391868794965));
#434342=CARTESIAN_POINT('Origin',(-2.61936967992036,-0.544477308918487,
13.8235269408515));
#434343=CARTESIAN_POINT('Ctrl Pts',(-2.65834525811495,-0.560094444879529,
13.7902140241682));
#434344=CARTESIAN_POINT('Ctrl Pts',(-2.66972687675236,-0.558140640235927,
13.8026027327198));
#434345=CARTESIAN_POINT('Ctrl Pts',(-2.66986456913071,-0.541504565786618,
13.8057746032556));
#434346=CARTESIAN_POINT('Ctrl Pts',(-2.64660074011354,-0.562115207046805,
13.8013225161807));
#434347=CARTESIAN_POINT('Ctrl Pts',(-2.65797071665401,-0.560163397282895,
13.8136962270464));
#434348=CARTESIAN_POINT('Ctrl Pts',(-2.65811512281489,-0.543549615287982,
13.8168830918628));
#434349=CARTESIAN_POINT('Ctrl Pts',(-2.63485115894477,-0.564136840382844,
13.8124254880876));
#434350=CARTESIAN_POINT('Ctrl Pts',(-2.64620448687496,-0.562187886830223,
13.8247886461868));
#434351=CARTESIAN_POINT('Ctrl Pts',(-2.64636049108562,-0.545595833766026,
13.8279860620656));
#434352=CARTESIAN_POINT('Ctrl Pts',(-2.62309630963174,-0.566159380155974,
13.8235227163065));
#434353=CARTESIAN_POINT('Ctrl Pts',(-2.63442763234527,-0.564214204380124,
13.8358800595847));
#434354=CARTESIAN_POINT('Ctrl Pts',(-2.63460046153234,-0.547643267144387,
13.8390832900376));
#434355=CARTESIAN_POINT('Origin',(-2.65461864066729,-0.538412371535249,
13.7902182540695));
#434356=CARTESIAN_POINT('Ctrl Pts',(-2.67851004605948,-0.556624863562287,
13.7382347919292));
#434357=CARTESIAN_POINT('Ctrl Pts',(-2.69338588907555,-0.554089678501094,
13.7369371795943));
#434358=CARTESIAN_POINT('Ctrl Pts',(-2.69631680811249,-0.539225174115846,
13.7364597369711));
#434359=CARTESIAN_POINT('Ctrl Pts',(-2.68037421200545,-0.5563041155144,
13.7595490285573));
#434360=CARTESIAN_POINT('Ctrl Pts',(-2.69560481097229,-0.553707451976304,
13.7633824266925));
#434361=CARTESIAN_POINT('Ctrl Pts',(-2.69876330181909,-0.5390133172322,
13.7648920890506));
#434362=CARTESIAN_POINT('Ctrl Pts',(-2.6708670678098,-0.557939912994462,
13.7803806590111));
#434363=CARTESIAN_POINT('Ctrl Pts',(-2.68404189807138,-0.55569921364324,
13.7901039518745));
#434364=CARTESIAN_POINT('Ctrl Pts',(-2.68629113005427,-0.540097085682201,
13.7926933640892));
#434365=CARTESIAN_POINT('Ctrl Pts',(-2.65434152892321,-0.56078329409476,
13.7936647693663));
#434366=CARTESIAN_POINT('Ctrl Pts',(-2.6650053673487,-0.558978887826884,
13.8072068914932));
#434367=CARTESIAN_POINT('Ctrl Pts',(-2.66464852175933,-0.541934330599655,
13.8104111085397));
#434368=CARTESIAN_POINT('Origin',(-2.67504549927705,-0.53489772554912,13.7435492065112));
#434369=CARTESIAN_POINT('Origin',(-2.67504549927705,-0.53489772554912,14.));
#434370=CARTESIAN_POINT('Origin',(-2.67504549927705,-0.53489772554912,12.5369868989719));
#434371=CARTESIAN_POINT('Ctrl Pts',(-2.68318906964636,-0.572273524858225,
12.506462012331));
#434372=CARTESIAN_POINT('Ctrl Pts',(-2.68958386403895,-0.573637413660991,
12.4999388158272));
#434373=CARTESIAN_POINT('Ctrl Pts',(-2.68950820523503,-0.573621277067824,
12.4907030323752));
#434374=CARTESIAN_POINT('Ctrl Pts',(-2.68813365056713,-0.559953634328176,
12.5042014951932));
#434375=CARTESIAN_POINT('Ctrl Pts',(-2.69329202285334,-0.55611536747025,
12.4980716682127));
#434376=CARTESIAN_POINT('Ctrl Pts',(-2.69466094798664,-0.549463179168228,
12.4907355092744));
#434377=CARTESIAN_POINT('Ctrl Pts',(-2.68384836601972,-0.55571546991498,
12.5218047446509));
#434378=CARTESIAN_POINT('Ctrl Pts',(-2.69446853395318,-0.550545276107923,
12.5216906929434));
#434379=CARTESIAN_POINT('Ctrl Pts',(-2.6966618981544,-0.538988463925912,
12.5161988840775));
#434380=CARTESIAN_POINT('Ctrl Pts',(-2.67873813717001,-0.55658561215412,
12.5369868989719));
#434381=CARTESIAN_POINT('Ctrl Pts',(-2.69385054257426,-0.554012533372128,
12.5369868989719));
#434382=CARTESIAN_POINT('Ctrl Pts',(-2.69667016579091,-0.538944180561122,
12.5369868989719));
#434383=CARTESIAN_POINT('Origin',(-5.02269464967049E-31,-6.29825987887749E-31,
12.5));
#434384=CARTESIAN_POINT('Origin',(-2.56822484263185,-0.778081884616942,
12.5));
#434385=CARTESIAN_POINT('',(-2.56822484263185,-0.778081884616942,12.5893111709658));
#434386=CARTESIAN_POINT('',(-2.56822484263185,-0.778081884616942,13.8235269408515));
#434387=CARTESIAN_POINT('',(-2.56822484263185,-0.778081884616942,12.5));
#434388=CARTESIAN_POINT('',(-2.6038508640706,-0.774910245348786,13.7902182540695));
#434389=CARTESIAN_POINT('',(-2.56822484263185,-0.778081884616942,13.8235269408515));
#434390=CARTESIAN_POINT('',(-2.62449623026968,-0.773072272667636,13.7435492065112));
#434391=CARTESIAN_POINT('Origin',(-2.55657327724839,-0.779119502966356,
13.7445212918686));
#434392=CARTESIAN_POINT('',(-2.62449623026968,-0.773072272667636,12.5369868989719));
#434393=CARTESIAN_POINT('',(-2.62449623026968,-0.773072272667636,12.5));
#434394=CARTESIAN_POINT('Ctrl Pts',(-2.62449623026968,-0.773072272667636,
12.5369868989719));
#434395=CARTESIAN_POINT('Ctrl Pts',(-2.60575278136628,-0.774740925415317,
12.5544431401645));
#434396=CARTESIAN_POINT('Ctrl Pts',(-2.58699592665006,-0.776410771627792,
12.5718848856037));
#434397=CARTESIAN_POINT('Ctrl Pts',(-2.56822484263185,-0.778081884616942,
12.5893111709658));
#434398=CARTESIAN_POINT('Origin',(-2.75929880391481,-1.01592146163591,12.5));
#434399=CARTESIAN_POINT('',(-2.5922874649989,-0.875023942687764,13.7435492065112));
#434400=CARTESIAN_POINT('',(-2.57644512594903,-0.861658704848515,13.7902182540695));
#434401=CARTESIAN_POINT('Origin',(-2.5348141970342,-0.826537169785806,13.7418732680453));
#434402=CARTESIAN_POINT('',(-2.54910729598814,-0.83859540603349,13.8235269408515));
#434403=CARTESIAN_POINT('',(-2.57644512594903,-0.861658704848515,13.7902182540695));
#434404=CARTESIAN_POINT('',(-2.54910729598814,-0.83859540603349,12.5893111709658));
#434405=CARTESIAN_POINT('',(-2.54910729598814,-0.83859540603349,12.5));
#434406=CARTESIAN_POINT('',(-2.5922874649989,-0.875023942687764,12.5369868989719));
#434407=CARTESIAN_POINT('Ctrl Pts',(-2.54910729598814,-0.83859540603349,
12.5893111709658));
#434408=CARTESIAN_POINT('Ctrl Pts',(-2.56351139395776,-0.850747285539268,
12.5718848856037));
#434409=CARTESIAN_POINT('Ctrl Pts',(-2.57790457299165,-0.86288995338934,
12.5544431401645));
#434410=CARTESIAN_POINT('Ctrl Pts',(-2.5922874649989,-0.875023942687764,
12.5369868989719));
#434411=CARTESIAN_POINT('',(-2.5922874649989,-0.875023942687764,12.5));
#434412=CARTESIAN_POINT('Origin',(-2.57127305293844,-0.812321467542656,
12.5));
#434413=CARTESIAN_POINT('',(-2.53885024331821,-0.800904305526286,13.8587068136939));
#434414=CARTESIAN_POINT('Ctrl Pts',(-2.54910729598377,-0.838595406038448,
13.8235269408542));
#434415=CARTESIAN_POINT('Ctrl Pts',(-2.54776795697393,-0.837465485490875,
13.8262006681044));
#434416=CARTESIAN_POINT('Ctrl Pts',(-2.54650937013253,-0.83617638223874,
13.8288634856214));
#434417=CARTESIAN_POINT('Ctrl Pts',(-2.54532684169042,-0.834740577250732,
13.8314912288862));
#434418=CARTESIAN_POINT('Ctrl Pts',(-2.54410777683876,-0.833260410404508,
13.834200161153));
#434419=CARTESIAN_POINT('Ctrl Pts',(-2.54296780529715,-0.831623008322601,
13.8368750301949));
#434420=CARTESIAN_POINT('Ctrl Pts',(-2.54192068506418,-0.829800985179098,
13.8394886372968));
#434421=CARTESIAN_POINT('Ctrl Pts',(-2.54183981342862,-0.829660265912108,
13.839690492513));
#434422=CARTESIAN_POINT('Ctrl Pts',(-2.54175951265142,-0.829518431229104,
13.8398919674349));
#434423=CARTESIAN_POINT('Ctrl Pts',(-2.54167979847135,-0.829375461987807,
13.8400930404591));
#434424=CARTESIAN_POINT('Ctrl Pts',(-2.54043779791686,-0.82714790502353,
13.8432258934518));
#434425=CARTESIAN_POINT('Ctrl Pts',(-2.53934355258194,-0.824656840184953,
13.8462331177034));
#434426=CARTESIAN_POINT('Ctrl Pts',(-2.53852107172497,-0.821944716064727,
13.8489036603661));
#434427=CARTESIAN_POINT('Ctrl Pts',(-2.53825194641688,-0.821057277490011,
13.849777493004));
#434428=CARTESIAN_POINT('Ctrl Pts',(-2.53801210994121,-0.820146331036332,
13.85061494757));
#434429=CARTESIAN_POINT('Ctrl Pts',(-2.53780644658882,-0.819213831003585,
13.8514076489583));
#434430=CARTESIAN_POINT('Ctrl Pts',(-2.53737143893741,-0.817241458947682,
13.8530843267192));
#434431=CARTESIAN_POINT('Ctrl Pts',(-2.53704947552703,-0.814978283817573,
13.8546805203176));
#434432=CARTESIAN_POINT('Ctrl Pts',(-2.53699432859212,-0.812536441960855,
13.8559412814274));
#434433=CARTESIAN_POINT('Ctrl Pts',(-2.53698694814377,-0.812209644329637,
13.8561100121513));
#434434=CARTESIAN_POINT('Ctrl Pts',(-2.53698428930086,-0.811879697661884,
13.8562727473908));
#434435=CARTESIAN_POINT('Ctrl Pts',(-2.53698665815411,-0.811546913710582,
13.8564289040185));
#434436=CARTESIAN_POINT('Ctrl Pts',(-2.53699740087656,-0.810037742287886,
13.8571370725437));
#434437=CARTESIAN_POINT('Ctrl Pts',(-2.53711400900739,-0.808443708134074,
13.8577210840553));
#434438=CARTESIAN_POINT('Ctrl Pts',(-2.53736121979839,-0.806828912811752,
13.8581177131616));
#434439=CARTESIAN_POINT('Ctrl Pts',(-2.53743084286587,-0.806374130869416,
13.8582294175695));
#434440=CARTESIAN_POINT('Ctrl Pts',(-2.53751064763825,-0.805917710234276,
13.8583265086086));
#434441=CARTESIAN_POINT('Ctrl Pts',(-2.53760074717429,-0.805461076504797,
13.8584082369006));
#434442=CARTESIAN_POINT('Ctrl Pts',(-2.53773019604643,-0.804805016286717,
13.8585256585398));
#434443=CARTESIAN_POINT('Ctrl Pts',(-2.53788282193589,-0.80414042241926,
13.8586122832068));
#434444=CARTESIAN_POINT('Ctrl Pts',(-2.53805542971628,-0.803484735877709,
13.8586682984299));
#434445=CARTESIAN_POINT('Ctrl Pts',(-2.53819349883054,-0.802960251640585,
13.8587131050557));
#434446=CARTESIAN_POINT('Ctrl Pts',(-2.53834565140356,-0.802435614053973,
13.8587357943552));
#434447=CARTESIAN_POINT('Ctrl Pts',(-2.5385123919188,-0.801910901840702,
13.8587355499465));
#434448=CARTESIAN_POINT('Ctrl Pts',(-2.53862016028908,-0.801571767827555,
13.8587353919793));
#434449=CARTESIAN_POINT('Ctrl Pts',(-2.53873282029729,-0.801236258278003,
13.8587257282814));
#434450=CARTESIAN_POINT('Ctrl Pts',(-2.53885024331821,-0.800904305526286,
13.8587068136939));
#434451=CARTESIAN_POINT('Ctrl Pts',(-2.53885024331821,-0.800904305526286,
13.8587068136939));
#434452=CARTESIAN_POINT('Ctrl Pts',(-2.53923644123263,-0.799812531022465,
13.8586446046466));
#434453=CARTESIAN_POINT('Ctrl Pts',(-2.53967409816476,-0.798759182819753,
13.858482427929));
#434454=CARTESIAN_POINT('Ctrl Pts',(-2.54015921290488,-0.797742266857458,
13.8582284286032));
#434455=CARTESIAN_POINT('Ctrl Pts',(-2.54065688419738,-0.796699029372676,
13.8579678548414));
#434456=CARTESIAN_POINT('Ctrl Pts',(-2.541207099941,-0.795692245662266,
13.857615680862));
#434457=CARTESIAN_POINT('Ctrl Pts',(-2.54177966554035,-0.794756960603073,
13.8571944833187));
#434458=CARTESIAN_POINT('Ctrl Pts',(-2.54320856155074,-0.792422861084746,
13.8561433417727));
#434459=CARTESIAN_POINT('Ctrl Pts',(-2.54483940254608,-0.790422371730728,
13.8546163505474));
#434460=CARTESIAN_POINT('Ctrl Pts',(-2.54646552170094,-0.788762325543555,
13.8528973491086));
#434461=CARTESIAN_POINT('Ctrl Pts',(-2.54676258967939,-0.788459059596855,
13.8525833129072));
#434462=CARTESIAN_POINT('Ctrl Pts',(-2.54705945621328,-0.788167021217311,
13.8522628768812));
#434463=CARTESIAN_POINT('Ctrl Pts',(-2.54735483301685,-0.787886075498211,
13.851937733538));
#434464=CARTESIAN_POINT('Ctrl Pts',(-2.54915865817453,-0.786170378971128,
13.8499521282529));
#434465=CARTESIAN_POINT('Ctrl Pts',(-2.55108900265194,-0.784700816482711,
13.847639871647));
#434466=CARTESIAN_POINT('Ctrl Pts',(-2.55299574939275,-0.783490698495397,
13.8452109780794));
#434467=CARTESIAN_POINT('Ctrl Pts',(-2.55385363421913,-0.782946241364709,
13.8441181685877));
#434468=CARTESIAN_POINT('Ctrl Pts',(-2.55470659089512,-0.782453601585564,
13.8430021611332));
#434469=CARTESIAN_POINT('Ctrl Pts',(-2.55554128503584,-0.782010699976034,
13.8418824960098));
#434470=CARTESIAN_POINT('Ctrl Pts',(-2.55750826309315,-0.780966991023276,
13.8392439765549));
#434471=CARTESIAN_POINT('Ctrl Pts',(-2.55946608248293,-0.78014625391618,
13.8364981347964));
#434472=CARTESIAN_POINT('Ctrl Pts',(-2.56140669078557,-0.779514758509505,
13.8336931113419));
#434473=CARTESIAN_POINT('Ctrl Pts',(-2.56329672003233,-0.778899722087069,
13.8309611966327));
#434474=CARTESIAN_POINT('Ctrl Pts',(-2.56517249228479,-0.778464111717678,
13.8281701127185));
#434475=CARTESIAN_POINT('Ctrl Pts',(-2.56702430011589,-0.778216000983472,
13.825358068512));
#434476=CARTESIAN_POINT('Ctrl Pts',(-2.56742577405218,-0.77816221030853,
13.8247484142932));
#434477=CARTESIAN_POINT('Ctrl Pts',(-2.56782604499562,-0.778117387942658,
13.8241378483365));
#434478=CARTESIAN_POINT('Ctrl Pts',(-2.56822484263185,-0.778081884616942,
13.8235269408515));
#434479=CARTESIAN_POINT('',(-2.53845888707557,-0.802083125762464,12.5969504640361));
#434480=CARTESIAN_POINT('Origin',(-2.57130466039945,-0.81233124768673,12.584524458991));
#434481=CARTESIAN_POINT('Origin',(-2.57130466039945,-0.81233124768673,12.584524458991));
#434482=CARTESIAN_POINT('Ctrl Pts',(-2.54910729598814,-0.83859540603349,
12.5893111709658));
#434483=CARTESIAN_POINT('Ctrl Pts',(-2.54044437960025,-0.831287019466255,
12.5770542771492));
#434484=CARTESIAN_POINT('Ctrl Pts',(-2.54847970027214,-0.817030887573105,
12.5737548217797));
#434485=CARTESIAN_POINT('Ctrl Pts',(-2.56805018676731,-0.854576394688601,
12.5663937883685));
#434486=CARTESIAN_POINT('Ctrl Pts',(-2.55937621962647,-0.847258685259328,
12.5540940315304));
#434487=CARTESIAN_POINT('Ctrl Pts',(-2.5674392375561,-0.83295995324631,
12.5508374392248));
#434488=CARTESIAN_POINT('Ctrl Pts',(-2.58697396440188,-0.870541258722054,
12.5434499600944));
#434489=CARTESIAN_POINT('Ctrl Pts',(-2.57827179510498,-0.863199756813581,
12.5311293540533));
#434490=CARTESIAN_POINT('Ctrl Pts',(-2.58637949200197,-0.848874359241767,
12.5278936106989));
#434491=CARTESIAN_POINT('Ctrl Pts',(-2.6058801260507,-0.886491261197587,
12.5204817579905));
#434492=CARTESIAN_POINT('Ctrl Pts',(-2.5971348869629,-0.879113423871825,
12.5081597038247));
#434493=CARTESIAN_POINT('Ctrl Pts',(-2.60530195343539,-0.864775255574287,
12.5049254088044));
#434494=CARTESIAN_POINT('Ctrl Pts',(-2.5922874649989,-0.875023942687763,
12.5369868989719));
#434495=CARTESIAN_POINT('Ctrl Pts',(-2.5929994447255,-0.875624597363629,
12.5342545179733));
#434496=CARTESIAN_POINT('Ctrl Pts',(-2.59375936469358,-0.876102487262538,
12.5314872231885));
#434497=CARTESIAN_POINT('Ctrl Pts',(-2.59455417637642,-0.87638337068847,
12.5287124745063));
#434498=CARTESIAN_POINT('Ctrl Pts',(-2.59527097700292,-0.876636685303784,
12.5262100684184));
#434499=CARTESIAN_POINT('Ctrl Pts',(-2.59601576070864,-0.876728585082981,
12.5237004536639));
#434500=CARTESIAN_POINT('Ctrl Pts',(-2.59680943393888,-0.876594856346212,
12.5212220730815));
#434501=CARTESIAN_POINT('Ctrl Pts',(-2.59741705945484,-0.876492475429756,
12.5193246583486));
#434502=CARTESIAN_POINT('Ctrl Pts',(-2.59806049678315,-0.876255999156885,
12.517417831369));
#434503=CARTESIAN_POINT('Ctrl Pts',(-2.59872487174322,-0.875789340163682,
12.5155812248347));
#434504=CARTESIAN_POINT('Ctrl Pts',(-2.59900789904724,-0.875590540924276,
12.5147988205793));
#434505=CARTESIAN_POINT('Ctrl Pts',(-2.59929517266528,-0.875349992872718,
12.5140295443047));
#434506=CARTESIAN_POINT('Ctrl Pts',(-2.59958753385755,-0.875061015908095,
12.5132817086137));
#434507=CARTESIAN_POINT('Ctrl Pts',(-2.60002998297234,-0.874623688364053,
12.5121499604604));
#434508=CARTESIAN_POINT('Ctrl Pts',(-2.60048861089017,-0.874060915274934,
12.5110494206568));
#434509=CARTESIAN_POINT('Ctrl Pts',(-2.6009436543093,-0.873341132251789,
12.5100666561695));
#434510=CARTESIAN_POINT('Ctrl Pts',(-2.60120493919269,-0.872927834497413,
12.5095023550641));
#434511=CARTESIAN_POINT('Ctrl Pts',(-2.60146750942728,-0.872457646016778,
12.5089719619137));
#434512=CARTESIAN_POINT('Ctrl Pts',(-2.60172086703324,-0.871936265915072,
12.5085043804652));
#434513=CARTESIAN_POINT('Ctrl Pts',(-2.60209162288741,-0.87117329405076,
12.5078201359221));
#434514=CARTESIAN_POINT('Ctrl Pts',(-2.60245231717916,-0.870278041215723,
12.5072563000953));
#434515=CARTESIAN_POINT('Ctrl Pts',(-2.60277064754136,-0.869308028552474,
12.5068768744336));
#434516=CARTESIAN_POINT('Ctrl Pts',(-2.60300018564644,-0.868608582646373,
12.5066032824118));
#434517=CARTESIAN_POINT('Ctrl Pts',(-2.60321178674052,-0.867857996609167,
12.5064197834844));
#434518=CARTESIAN_POINT('Ctrl Pts',(-2.60339612235286,-0.86709888648586,
12.5063282718343));
#434519=CARTESIAN_POINT('Ctrl Pts',(-2.603665195278,-0.865990820720387,
12.5061946931565));
#434520=CARTESIAN_POINT('Ctrl Pts',(-2.60388295705793,-0.864841159775945,
12.5062515701262));
#434521=CARTESIAN_POINT('Ctrl Pts',(-2.60405108737695,-0.863724131658777,
12.5064436508398));
#434522=CARTESIAN_POINT('',(-2.54847970027214,-0.817030887573105,12.5737548217797));
#434523=CARTESIAN_POINT('Origin',(-2.56329338043633,-0.821780085399356,
12.5893111709658));
#434524=CARTESIAN_POINT('Ctrl Pts',(-2.60405108737695,-0.863724131658777,
12.5064436508398));
#434525=CARTESIAN_POINT('Ctrl Pts',(-2.59582538737506,-0.856811950582574,
12.5164271754438));
#434526=CARTESIAN_POINT('Ctrl Pts',(-2.58759629229226,-0.849897189477589,
12.5264061185523));
#434527=CARTESIAN_POINT('Ctrl Pts',(-2.57936368316554,-0.842979756752747,
12.536380305637));
#434528=CARTESIAN_POINT('Ctrl Pts',(-2.56907459151018,-0.834334368853223,
12.5488460165097));
#434529=CARTESIAN_POINT('Ctrl Pts',(-2.55878000788777,-0.82568480536692,
12.5613043021964));
#434530=CARTESIAN_POINT('Ctrl Pts',(-2.54847970027214,-0.817030887573105,
12.5737548217797));
#434531=CARTESIAN_POINT('Ctrl Pts',(-2.56822484263185,-0.778081884616942,
12.5893111709658));
#434532=CARTESIAN_POINT('Ctrl Pts',(-2.55693553234648,-0.779086925830232,
12.5770542771492));
#434533=CARTESIAN_POINT('Ctrl Pts',(-2.55532224306043,-0.795371918078755,
12.5737548217797));
#434534=CARTESIAN_POINT('Ctrl Pts',(-2.55769201432484,-0.779019579327555,
12.5928319619712));
#434535=CARTESIAN_POINT('Ctrl Pts',(-2.55039378145664,-0.782939938159727,
12.5821634970842));
#434536=CARTESIAN_POINT('Ctrl Pts',(-2.55148455166212,-0.795704095893736,
12.5773203894503));
#434537=CARTESIAN_POINT('Ctrl Pts',(-2.54314751095848,-0.787328702095061,
12.5969440695591));
#434538=CARTESIAN_POINT('Ctrl Pts',(-2.541919158119,-0.79115619368273,12.5878292599214));
#434539=CARTESIAN_POINT('Ctrl Pts',(-2.5463016087757,-0.798667413314068,
12.5813877129824));
#434540=CARTESIAN_POINT('Ctrl Pts',(-2.53387888228656,-0.816488053392434,
12.596957478804));
#434541=CARTESIAN_POINT('Ctrl Pts',(-2.53509823359339,-0.812688872488681,
12.5878468778671));
#434542=CARTESIAN_POINT('Ctrl Pts',(-2.54298992293219,-0.809105756342446,
12.5814011370086));
#434543=CARTESIAN_POINT('Ctrl Pts',(-2.54101313467616,-0.831766844247121,
12.5928371701607));
#434544=CARTESIAN_POINT('Ctrl Pts',(-2.53729986510681,-0.824367743301106,
12.5821692192951));
#434545=CARTESIAN_POINT('Ctrl Pts',(-2.54551978321918,-0.81454650263643,
12.5773318885715));
#434546=CARTESIAN_POINT('Ctrl Pts',(-2.5491072959881,-0.83859540603353,
12.5893111709658));
#434547=CARTESIAN_POINT('Ctrl Pts',(-2.54044437960021,-0.831287019466295,
12.5770542771492));
#434548=CARTESIAN_POINT('Ctrl Pts',(-2.5484797002721,-0.817030887573146,
12.5737548217797));
#434549=CARTESIAN_POINT('',(-2.55532224306043,-0.795371918078755,12.5737548217797));
#434550=CARTESIAN_POINT('Origin',(-2.57017569722807,-0.799995217689399,
12.5893111709658));
#434551=CARTESIAN_POINT('Ctrl Pts',(-2.5484797002721,-0.817030887573146,
12.5737548217797));
#434552=CARTESIAN_POINT('Ctrl Pts',(-2.54769304936628,-0.816410001123474,
12.5746934679442));
#434553=CARTESIAN_POINT('Ctrl Pts',(-2.54693605954408,-0.815579157066309,
12.5756680099006));
#434554=CARTESIAN_POINT('Ctrl Pts',(-2.54629239321916,-0.814635124582682,
12.5765688348656));
#434555=CARTESIAN_POINT('Ctrl Pts',(-2.54612198968525,-0.814385202433427,
12.5768073183026));
#434556=CARTESIAN_POINT('Ctrl Pts',(-2.54595935785156,-0.814127539442557,
12.5770407398754));
#434557=CARTESIAN_POINT('Ctrl Pts',(-2.54580558218149,-0.813864244577062,
12.5772674179684));
#434558=CARTESIAN_POINT('Ctrl Pts',(-2.5451745284142,-0.812783753647002,
12.5781976435658));
#434559=CARTESIAN_POINT('Ctrl Pts',(-2.54466651577252,-0.811541360537451,
12.5790594849312));
#434560=CARTESIAN_POINT('Ctrl Pts',(-2.54436054299381,-0.810202677086306,
12.5797571720116));
#434561=CARTESIAN_POINT('Ctrl Pts',(-2.54416119072669,-0.809330476683118,
12.580211740231));
#434562=CARTESIAN_POINT('Ctrl Pts',(-2.54405684558894,-0.808373581144119,
12.5806009430798));
#434563=CARTESIAN_POINT('Ctrl Pts',(-2.54407246531675,-0.807397431212796,
12.5808812374708));
#434564=CARTESIAN_POINT('Ctrl Pts',(-2.54408588784472,-0.80655859458742,
12.5811221033394));
#434565=CARTESIAN_POINT('Ctrl Pts',(-2.54418828746562,-0.805688368139684,
12.581287365893));
#434566=CARTESIAN_POINT('Ctrl Pts',(-2.5443821654288,-0.804836843261101,
12.581359338449));
#434567=CARTESIAN_POINT('Ctrl Pts',(-2.54440911046226,-0.804718498886295,
12.5813693411482));
#434568=CARTESIAN_POINT('Ctrl Pts',(-2.54443777180863,-0.804600483745816,
12.5813775999465));
#434569=CARTESIAN_POINT('Ctrl Pts',(-2.54446810491804,-0.804482898618531,
12.5813841266931));
#434570=CARTESIAN_POINT('Ctrl Pts',(-2.54451956870687,-0.804283401228465,
12.5813952001081));
#434571=CARTESIAN_POINT('Ctrl Pts',(-2.54457677895355,-0.804083957592851,
12.5814007534795));
#434572=CARTESIAN_POINT('Ctrl Pts',(-2.54463990030613,-0.803884708952469,
12.5814005856065));
#434573=CARTESIAN_POINT('Ctrl Pts',(-2.54492884517943,-0.802972626577968,
12.5813998171494));
#434574=CARTESIAN_POINT('Ctrl Pts',(-2.54532136873609,-0.802127546192349,
12.58127954464));
#434575=CARTESIAN_POINT('Ctrl Pts',(-2.54578840666897,-0.801341800892411,
12.5810700125799));
#434576=CARTESIAN_POINT('Ctrl Pts',(-2.54635253531537,-0.800392710034351,
12.5808169217085));
#434577=CARTESIAN_POINT('Ctrl Pts',(-2.54703981711477,-0.799538653778791,
12.5804173076348));
#434578=CARTESIAN_POINT('Ctrl Pts',(-2.54776973104725,-0.798838153230019,
12.5799304713245));
#434579=CARTESIAN_POINT('Ctrl Pts',(-2.54867432435619,-0.797970012369661,
12.5793271277669));
#434580=CARTESIAN_POINT('Ctrl Pts',(-2.54967821384419,-0.797260633271943,
12.5785808224116));
#434581=CARTESIAN_POINT('Ctrl Pts',(-2.55072078012457,-0.796714015110856,
12.5777485681082));
#434582=CARTESIAN_POINT('Ctrl Pts',(-2.55227431810398,-0.795899494164346,
12.576508418016));
#434583=CARTESIAN_POINT('Ctrl Pts',(-2.55389746281564,-0.79544714390649,
12.5750928681475));
#434584=CARTESIAN_POINT('Ctrl Pts',(-2.55532224306043,-0.795371918078755,
12.5737548217797));
#434585=CARTESIAN_POINT('Ctrl Pts',(-2.55532224306043,-0.795371918078755,
12.5737548217797));
#434586=CARTESIAN_POINT('Ctrl Pts',(-2.55693553234648,-0.779086925830232,
12.5770542771492));
#434587=CARTESIAN_POINT('Ctrl Pts',(-2.56822484263185,-0.778081884616942,
12.5893111709658));
#434588=CARTESIAN_POINT('Ctrl Pts',(-2.57998826481891,-0.793226615121052,
12.5508408821982));
#434589=CARTESIAN_POINT('Ctrl Pts',(-2.58160335419684,-0.77689085034156,
12.55409748406));
#434590=CARTESIAN_POINT('Ctrl Pts',(-2.59290706675081,-0.775884526953087,
12.5663972313419));
#434591=CARTESIAN_POINT('Ctrl Pts',(-2.60463008878051,-0.791082232777121,
12.52790050457));
#434592=CARTESIAN_POINT('Ctrl Pts',(-2.60622393129696,-0.774698980860186,
12.5311362602937));
#434593=CARTESIAN_POINT('Ctrl Pts',(-2.61756439056145,-0.77368938606204,
12.5434568539655));
#434594=CARTESIAN_POINT('Ctrl Pts',(-2.6292495942247,-0.788938685707459,
12.5049357605811));
#434595=CARTESIAN_POINT('Ctrl Pts',(-2.63080218867057,-0.772510878931263,
12.5081700652078));
#434596=CARTESIAN_POINT('Ctrl Pts',(-2.642198764261,-0.771496288325706,
12.5204921097672));
#434597=CARTESIAN_POINT('Ctrl Pts',(-2.62763298085407,-0.789079437829352,
12.5064436508395));
#434598=CARTESIAN_POINT('Ctrl Pts',(-2.62817752453933,-0.787987503781238,
12.5062361689309));
#434599=CARTESIAN_POINT('Ctrl Pts',(-2.62869724291733,-0.786828761174787,
12.5061871075061));
#434600=CARTESIAN_POINT('Ctrl Pts',(-2.62913646345114,-0.785680674956858,
12.5063648335164));
#434601=CARTESIAN_POINT('Ctrl Pts',(-2.62933598450984,-0.78515914337978,
12.5064455676329));
#434602=CARTESIAN_POINT('Ctrl Pts',(-2.62952147167592,-0.784632457785811,
12.506574497099));
#434603=CARTESIAN_POINT('Ctrl Pts',(-2.62968398054393,-0.784122851769093,
12.5067492519495));
#434604=CARTESIAN_POINT('Ctrl Pts',(-2.63001054842234,-0.783098778696979,
12.5071004286051));
#434605=CARTESIAN_POINT('Ctrl Pts',(-2.63025556102904,-0.782105780109526,
12.5076537929613));
#434606=CARTESIAN_POINT('Ctrl Pts',(-2.63040981192518,-0.781220651583605,
12.5083435010505));
#434607=CARTESIAN_POINT('Ctrl Pts',(-2.6304195229409,-0.781164927453336,
12.5083869222964));
#434608=CARTESIAN_POINT('Ctrl Pts',(-2.63042886352802,-0.781109622735334,
12.5084308732337));
#434609=CARTESIAN_POINT('Ctrl Pts',(-2.63043782727202,-0.781054752968155,
12.5084753333615));
#434610=CARTESIAN_POINT('Ctrl Pts',(-2.63050972832999,-0.780614625013893,
12.5088319622689));
#434611=CARTESIAN_POINT('Ctrl Pts',(-2.63056011562499,-0.780193755153452,
12.509227847131));
#434612=CARTESIAN_POINT('Ctrl Pts',(-2.63059027107938,-0.779804990891921,
12.5096423454524));
#434613=CARTESIAN_POINT('Ctrl Pts',(-2.63068476492719,-0.778586775756137,
12.5109411997424));
#434614=CARTESIAN_POINT('Ctrl Pts',(-2.6305960502868,-0.777609631036941,
12.5124831113042));
#434615=CARTESIAN_POINT('Ctrl Pts',(-2.63040699481828,-0.776827853251822,
12.5140723025008));
#434616=CARTESIAN_POINT('Ctrl Pts',(-2.63038928011381,-0.776754599817102,
12.5142212114565));
#434617=CARTESIAN_POINT('Ctrl Pts',(-2.63037070367165,-0.776683039182932,
12.5143705582413));
#434618=CARTESIAN_POINT('Ctrl Pts',(-2.63035134583323,-0.776613121902429,
12.5145201959299));
#434619=CARTESIAN_POINT('Ctrl Pts',(-2.63010266557795,-0.775714930338395,
12.5164425148273));
#434620=CARTESIAN_POINT('Ctrl Pts',(-2.62972685794205,-0.775054304574326,
12.518463520594));
#434621=CARTESIAN_POINT('Ctrl Pts',(-2.62926873570144,-0.774552951611391,
12.5205025929157));
#434622=CARTESIAN_POINT('Ctrl Pts',(-2.62900300664362,-0.774262147021112,
12.5216853356836));
#434623=CARTESIAN_POINT('Ctrl Pts',(-2.62871042015151,-0.774025128247206,
12.5228750347131));
#434624=CARTESIAN_POINT('Ctrl Pts',(-2.62840468342422,-0.773829851771047,
12.5240609649613));
#434625=CARTESIAN_POINT('Ctrl Pts',(-2.62765426902932,-0.773350556136539,
12.5269717671326));
#434626=CARTESIAN_POINT('Ctrl Pts',(-2.62679791805758,-0.773118000763833,
12.5299036066169));
#434627=CARTESIAN_POINT('Ctrl Pts',(-2.62587149186265,-0.773053296579262,
12.5328133004019));
#434628=CARTESIAN_POINT('Ctrl Pts',(-2.6254267533449,-0.773022234803056,
12.5342101228451));
#434629=CARTESIAN_POINT('Ctrl Pts',(-2.62496638397125,-0.773030416884956,
12.5356023438238));
#434630=CARTESIAN_POINT('Ctrl Pts',(-2.62449623026968,-0.773072272667636,
12.5369868989719));
#434631=CARTESIAN_POINT('Origin',(-15.3184123001101,0.362331832531667,-1.23925115604868));
#434632=CARTESIAN_POINT('Ctrl Pts',(-2.59225549468539,-0.874997023178067,
12.5369868989719));
#434633=CARTESIAN_POINT('Ctrl Pts',(-2.60399832348813,-0.884865623656304,
12.5369868989719));
#434634=CARTESIAN_POINT('Ctrl Pts',(-2.59879895925366,-0.899296490409444,
12.5369868989719));
#434635=CARTESIAN_POINT('Ctrl Pts',(-2.5962249874813,-0.87833304678732,
12.5218025310016));
#434636=CARTESIAN_POINT('Ctrl Pts',(-2.60277466712086,-0.88816958887924,
12.5216901060418));
#434637=CARTESIAN_POINT('Ctrl Pts',(-2.59881482415437,-0.899252505935221,
12.5161920673678));
#434638=CARTESIAN_POINT('Ctrl Pts',(-2.6020669015845,-0.876847075452772,
12.5042015548895));
#434639=CARTESIAN_POINT('Ctrl Pts',(-2.60457506842166,-0.882770456593155,
12.4980677368514));
#434640=CARTESIAN_POINT('Ctrl Pts',(-2.6023876888041,-0.889205217671326,
12.4907278922777));
#434641=CARTESIAN_POINT('Ctrl Pts',(-2.60403210331923,-0.863717834924639,
12.5064636261921));
#434642=CARTESIAN_POINT('Ctrl Pts',(-2.61024215530184,-0.865777614697072,
12.4999376786892));
#434643=CARTESIAN_POINT('Ctrl Pts',(-2.61016630854628,-0.865752457482069,
12.4906970594712));
#434644=CARTESIAN_POINT('Origin',(-2.57810138055071,-0.891839263321898,
12.5369868989719));
#434645=CARTESIAN_POINT('Origin',(-2.57810138055071,-0.891839263321898,
14.));
#434646=CARTESIAN_POINT('Origin',(-2.57810138055071,-0.891839263321898,
13.7435492065112));
#434647=CARTESIAN_POINT('Ctrl Pts',(-2.5733624889779,-0.859058103170204,
13.793642941384));
#434648=CARTESIAN_POINT('Ctrl Pts',(-2.58164422482094,-0.866009295185383,
13.8071662555867));
#434649=CARTESIAN_POINT('Ctrl Pts',(-2.57273254136418,-0.880521403288669,
13.8103758687955));
#434650=CARTESIAN_POINT('Ctrl Pts',(-2.58606655908268,-0.869775766534773,
13.7804579775006));
#434651=CARTESIAN_POINT('Ctrl Pts',(-2.59627895308506,-0.878360676579107,
13.7901904343351));
#434652=CARTESIAN_POINT('Ctrl Pts',(-2.59031483388354,-0.892944407456857,
13.7927914348262));
#434653=CARTESIAN_POINT('Ctrl Pts',(-2.59354592323677,-0.876085658337585,
13.7597120340895));
#434654=CARTESIAN_POINT('Ctrl Pts',(-2.60536085171629,-0.88602520334712,
13.7635825532445));
#434655=CARTESIAN_POINT('Ctrl Pts',(-2.60066834076928,-0.900291115766461,
13.7651073818884));
#434656=CARTESIAN_POINT('Ctrl Pts',(-2.59208129247692,-0.874850037043129,
13.7381884353898));
#434657=CARTESIAN_POINT('Ctrl Pts',(-2.60362024917657,-0.884556240673273,
13.7368803041982));
#434658=CARTESIAN_POINT('Ctrl Pts',(-2.59864053045773,-0.898852815039194,
13.7363986145813));
#434659=CARTESIAN_POINT('Origin',(-2.56225904150083,-0.878474025482649,
13.7902182540695));
#434660=CARTESIAN_POINT('Ctrl Pts',(-2.54910428693338,-0.838592868466142,
13.8235227101244));
#434661=CARTESIAN_POINT('Ctrl Pts',(-2.5578947345676,-0.846003045165089,
13.8358800583119));
#434662=CARTESIAN_POINT('Ctrl Pts',(-2.54966095281149,-0.860384661452888,
13.8390832900376));
#434663=CARTESIAN_POINT('Ctrl Pts',(-2.55822092653545,-0.846284034285507,
13.8124254819053));
#434664=CARTESIAN_POINT('Ctrl Pts',(-2.5670284449151,-0.853708601655244,
13.8247886449158));
#434665=CARTESIAN_POINT('Ctrl Pts',(-2.55876946781238,-0.868099921202787,
13.8279860620657));
#434666=CARTESIAN_POINT('Ctrl Pts',(-2.56733348035622,-0.853971753174535,
13.8013225099954));
#434667=CARTESIAN_POINT('Ctrl Pts',(-2.57615391503897,-0.861407206478814,
13.8136962257787));
#434668=CARTESIAN_POINT('Ctrl Pts',(-2.567873941212,-0.875811402336499,
13.8168830918626));
#434669=CARTESIAN_POINT('Ctrl Pts',(-2.57644210736721,-0.861656159248027,
13.7902140179785));
#434670=CARTESIAN_POINT('Ctrl Pts',(-2.58527157543221,-0.869099222813102,
13.802602731458));
#434671=CARTESIAN_POINT('Ctrl Pts',(-2.57697453300406,-0.883519251920806,
13.8057746032558));
#434672=CARTESIAN_POINT('Origin',(-2.53492121153995,-0.855410726667624,
13.8235269408515));
#434673=CARTESIAN_POINT('Ctrl Pts',(-2.56822484263185,-0.778081884616942,
13.8235269408515));
#434674=CARTESIAN_POINT('Ctrl Pts',(-2.57998580964624,-0.777034853730306,
13.8362179249168));
#434675=CARTESIAN_POINT('Ctrl Pts',(-2.5812427264348,-0.760003025753138,
13.8391868794938));
#434676=CARTESIAN_POINT('Ctrl Pts',(-2.55746406973814,-0.77903987230367,
13.8400110824519));
#434677=CARTESIAN_POINT('Ctrl Pts',(-2.56659013042535,-0.774792887585658,
13.8494522556837));
#434678=CARTESIAN_POINT('Ctrl Pts',(-2.56354349538393,-0.761691517338244,
13.85569149686));
#434679=CARTESIAN_POINT('Ctrl Pts',(-2.54325053116281,-0.787000591317278,
13.8586819406588));
#434680=CARTESIAN_POINT('Ctrl Pts',(-2.54457536843989,-0.78285320059247,
13.868010383617));
#434681=CARTESIAN_POINT('Ctrl Pts',(-2.54002008263671,-0.775033850360904,
13.8744918421245));
#434682=CARTESIAN_POINT('Ctrl Pts',(-2.53377424654496,-0.816821247376267,
13.8587686893867));
#434683=CARTESIAN_POINT('Ctrl Pts',(-2.53246114666913,-0.820931709228164,
13.8680909899357));
#434684=CARTESIAN_POINT('Ctrl Pts',(-2.52424730370528,-0.824677264630375,
13.8745789365163));
#434685=CARTESIAN_POINT('Ctrl Pts',(-2.54083651910886,-0.831617844221254,
13.8400379222776));
#434686=CARTESIAN_POINT('Ctrl Pts',(-2.54585881821242,-0.840338322741523,
13.8494748685452));
#434687=CARTESIAN_POINT('Ctrl Pts',(-2.53584371829778,-0.849308210085531,
13.8557104837033));
#434688=CARTESIAN_POINT('Ctrl Pts',(-2.54910729598377,-0.838595406038448,
13.8235269408542));
#434689=CARTESIAN_POINT('Ctrl Pts',(-2.55813214084235,-0.846209130098926,
13.8362179249195));
#434690=CARTESIAN_POINT('Ctrl Pts',(-2.54937606831806,-0.860871810549845,
13.8391868794965));
#434691=CARTESIAN_POINT('Origin',(-2.56627398803563,-0.756168551544486,
13.8235269408515));
#434692=CARTESIAN_POINT('Ctrl Pts',(-2.60384693664582,-0.774910594228413,
13.7902140241682));
#434693=CARTESIAN_POINT('Ctrl Pts',(-2.6153499371028,-0.77389099828931,
13.8026027327198));
#434694=CARTESIAN_POINT('Ctrl Pts',(-2.61684316583052,-0.757321502212479,
13.8057746032556));
#434695=CARTESIAN_POINT('Ctrl Pts',(-2.59197678668273,-0.775967345228378,
13.8013225161808));
#434696=CARTESIAN_POINT('Ctrl Pts',(-2.60346802117969,-0.774948788592186,
13.8136962270464));
#434697=CARTESIAN_POINT('Ctrl Pts',(-2.60496612430837,-0.758402058029048,
13.8168830918628));
#434698=CARTESIAN_POINT('Ctrl Pts',(-2.58010151939116,-0.777024551803223,
13.8124254880875));
#434699=CARTESIAN_POINT('Ctrl Pts',(-2.59157592786698,-0.776007484858214,
13.8247886461867));
#434700=CARTESIAN_POINT('Ctrl Pts',(-2.59308381934438,-0.759483356273309,
13.8279860620656));
#434701=CARTESIAN_POINT('Ctrl Pts',(-2.56822092760171,-0.778082232396394,
13.8235227163065));
#434702=CARTESIAN_POINT('Ctrl Pts',(-2.57967309615752,-0.777067137028476,
13.8358800595847));
#434703=CARTESIAN_POINT('Ctrl Pts',(-2.58119603549152,-0.760565425402617,
13.8390832900376));
#434704=CARTESIAN_POINT('Origin',(-2.60190000947438,-0.75299691227633,13.7902182540695));
#434705=CARTESIAN_POINT('Ctrl Pts',(-2.6242274310093,-0.773096175075023,
13.7382347919292));
#434706=CARTESIAN_POINT('Ctrl Pts',(-2.63926041700291,-0.771781944939381,
13.7369371795943));
#434707=CARTESIAN_POINT('Ctrl Pts',(-2.64339317875125,-0.757205798077073,
13.7364597369711));
#434708=CARTESIAN_POINT('Ctrl Pts',(-2.62611153804043,-0.772928441120475,
13.7595490285574));
#434709=CARTESIAN_POINT('Ctrl Pts',(-2.64150311063024,-0.771581852975879,
13.7633824266925));
#434710=CARTESIAN_POINT('Ctrl Pts',(-2.64584880025467,-0.757194058078969,
13.7648920890506));
#434711=CARTESIAN_POINT('Ctrl Pts',(-2.61650269540219,-0.773783875107399,
13.7803806590111));
#434712=CARTESIAN_POINT('Ctrl Pts',(-2.62981632530171,-0.772624502473894,
13.7901039518744));
#434713=CARTESIAN_POINT('Ctrl Pts',(-2.63332979142262,-0.757257622594016,
13.7926933640892));
#434714=CARTESIAN_POINT('Ctrl Pts',(-2.59980038192665,-0.775270810256772,
13.7936647693663));
#434715=CARTESIAN_POINT('Ctrl Pts',(-2.61057581317161,-0.774341609831827,
13.8072068914933));
#434716=CARTESIAN_POINT('Ctrl Pts',(-2.61160944460447,-0.757324680734365,
13.8104111085397));
#434717=CARTESIAN_POINT('Origin',(-2.62254537567346,-0.75115893959518,13.7435492065112));
#434718=CARTESIAN_POINT('Origin',(-2.62254537567346,-0.75115893959518,14.));
#434719=CARTESIAN_POINT('Origin',(-2.62254537567346,-0.75115893959518,12.5369868989719));
#434720=CARTESIAN_POINT('Ctrl Pts',(-2.62761537436049,-0.78907415060169,
12.506462012331));
#434721=CARTESIAN_POINT('Ctrl Pts',(-2.63387772100312,-0.790954736286347,
12.4999388158272));
#434722=CARTESIAN_POINT('Ctrl Pts',(-2.63380362922977,-0.790932486491461,
12.4907030323752));
#434723=CARTESIAN_POINT('Ctrl Pts',(-2.6335476880466,-0.777198282739337,
12.5042014951932));
#434724=CARTESIAN_POINT('Ctrl Pts',(-2.63900175065624,-0.773793242627058,
12.4980716682127));
#434725=CARTESIAN_POINT('Ctrl Pts',(-2.6409083359066,-0.767274769039712,
12.4907355092743));
#434726=CARTESIAN_POINT('Ctrl Pts',(-2.62962211217494,-0.772624929995355,
12.5218047446509));
#434727=CARTESIAN_POINT('Ctrl Pts',(-2.64062836116866,-0.768337581861103,
12.5216906929434));
#434728=CARTESIAN_POINT('Ctrl Pts',(-2.64375641461251,-0.756998003562851,
12.5161988840776));
#434729=CARTESIAN_POINT('Ctrl Pts',(-2.62445796251965,-0.77307564581568,
12.5369868989719));
#434730=CARTESIAN_POINT('Ctrl Pts',(-2.63972981244962,-0.771742930078233,
12.5369868989719));
#434731=CARTESIAN_POINT('Ctrl Pts',(-2.64376826424447,-0.756954541436434,
12.5369868989719));
#434732=CARTESIAN_POINT('Origin',(-4.91254002680598E-31,-6.70384157887756E-31,
12.5));
#434733=CARTESIAN_POINT('Origin',(-2.49625838937555,-0.984827048243808,
12.5));
#434734=CARTESIAN_POINT('',(-2.49625838937555,-0.984827048243808,12.5893111709658));
#434735=CARTESIAN_POINT('',(-2.49625838937555,-0.984827048243808,13.8235269408515));
#434736=CARTESIAN_POINT('',(-2.49625838937555,-0.984827048243808,12.5));
#434737=CARTESIAN_POINT('',(-2.53202438621132,-0.98456981382678,13.7902182540695));
#434738=CARTESIAN_POINT('',(-2.49625838937555,-0.984827048243808,13.8235269408515));
#434739=CARTESIAN_POINT('',(-2.55275086849392,-0.984420745855558,13.7435492065112));
#434740=CARTESIAN_POINT('Origin',(-2.48456101808811,-0.984911503257141,
13.7445212918691));
#434741=CARTESIAN_POINT('',(-2.55275086849392,-0.984420745855558,12.5369868989719));
#434742=CARTESIAN_POINT('',(-2.55275086849392,-0.984420745855558,12.5));
#434743=CARTESIAN_POINT('Ctrl Pts',(-2.55275086849392,-0.984420745855558,
12.5369868989719));
#434744=CARTESIAN_POINT('Ctrl Pts',(-2.53393377618057,-0.984556081207558,
12.5544431401645));
#434745=CARTESIAN_POINT('Ctrl Pts',(-2.51510322538267,-0.984691513354999,
12.5718848856037));
#434746=CARTESIAN_POINT('Ctrl Pts',(-2.49625838937555,-0.984827048243808,
12.5893111709658));
#434747=CARTESIAN_POINT('Origin',(-2.66731043429289,-1.2374495353793,12.5));
#434748=CARTESIAN_POINT('',(-2.51233926765277,-1.08340786672296,13.7435492065112));
#434749=CARTESIAN_POINT('',(-2.4976390336399,-1.0687958029044,13.7902182540695));
#434750=CARTESIAN_POINT('Origin',(-2.45900935936426,-1.03039782466055,13.7418732680442));
#434751=CARTESIAN_POINT('',(-2.47227204101564,-1.04358095837975,13.8235269408515));
#434752=CARTESIAN_POINT('',(-2.4976390336399,-1.0687958029044,13.7902182540695));
#434753=CARTESIAN_POINT('',(-2.47227204101564,-1.04358095837975,12.5893111709658));
#434754=CARTESIAN_POINT('',(-2.47227204101564,-1.04358095837975,12.5));
#434755=CARTESIAN_POINT('',(-2.51233926765277,-1.08340786672296,12.5369868989719));
#434756=CARTESIAN_POINT('Ctrl Pts',(-2.47227204101564,-1.04358095837975,
12.5893111709658));
#434757=CARTESIAN_POINT('Ctrl Pts',(-2.48563771954525,-1.05686647121458,
12.5718848856037));
#434758=CARTESIAN_POINT('Ctrl Pts',(-2.49899326630645,-1.0701419130501,
12.5544431401645));
#434759=CARTESIAN_POINT('Ctrl Pts',(-2.51233926765277,-1.08340786672296,
12.5369868989719));
#434760=CARTESIAN_POINT('',(-2.51233926765277,-1.08340786672296,12.5));
#434761=CARTESIAN_POINT('Origin',(-2.49650561314058,-1.01920115922009,12.5));
#434762=CARTESIAN_POINT('',(-2.4651212924408,-1.00517922688567,13.8587068136939));
#434763=CARTESIAN_POINT('Ctrl Pts',(-2.47227204101088,-1.04358095838433,
13.8235269408542));
#434764=CARTESIAN_POINT('Ctrl Pts',(-2.4710292575554,-1.04234562899105,
13.8262006681044));
#434765=CARTESIAN_POINT('Ctrl Pts',(-2.46987993244038,-1.04095822861191,
13.8288634856214));
#434766=CARTESIAN_POINT('Ctrl Pts',(-2.4688183702,-1.03943081410046,13.8314912288862));
#434767=CARTESIAN_POINT('Ctrl Pts',(-2.46772400902523,-1.03785620728465,
13.8342001611531));
#434768=CARTESIAN_POINT('Ctrl Pts',(-2.46672129411546,-1.03613133525948,
13.8368750301949));
#434769=CARTESIAN_POINT('Ctrl Pts',(-2.46582616988972,-1.0342300247277,
13.8394886372969));
#434770=CARTESIAN_POINT('Ctrl Pts',(-2.4657570372745,-1.03408318190339,
13.8396904925131));
#434771=CARTESIAN_POINT('Ctrl Pts',(-2.4656885645349,-1.03393527390479,
13.8398919674349));
#434772=CARTESIAN_POINT('Ctrl Pts',(-2.46562076891762,-1.03378628293615,
13.8400930404591));
#434773=CARTESIAN_POINT('Ctrl Pts',(-2.46456446758973,-1.03146490340854,
13.8432258934518));
#434774=CARTESIAN_POINT('Ctrl Pts',(-2.46367690817616,-1.02889293622944,
13.8462331177034));
#434775=CARTESIAN_POINT('Ctrl Pts',(-2.46307822735032,-1.02612279665311,
13.8489036603661));
#434776=CARTESIAN_POINT('Ctrl Pts',(-2.46288233201691,-1.02521637474599,
13.849777493004));
#434777=CARTESIAN_POINT('Ctrl Pts',(-2.46271754417012,-1.02428891049219,
13.85061494757));
#434778=CARTESIAN_POINT('Ctrl Pts',(-2.46258857255514,-1.02334274980388,
13.8514076489583));
#434779=CARTESIAN_POINT('Ctrl Pts',(-2.46231577898897,-1.0213414834913,
13.8530843267192));
#434780=CARTESIAN_POINT('Ctrl Pts',(-2.46217935666868,-1.01905959588286,
13.8546805203176));
#434781=CARTESIAN_POINT('Ctrl Pts',(-2.46232342601092,-1.01662138406636,
13.8559412814273));
#434782=CARTESIAN_POINT('Ctrl Pts',(-2.46234270716119,-1.01629507225221,
13.8561100121513));
#434783=CARTESIAN_POINT('Ctrl Pts',(-2.46236695088185,-1.01596600673437,
13.8562727473908));
#434784=CARTESIAN_POINT('Ctrl Pts',(-2.46239643683439,-1.01563452317772,
13.8564289040185));
#434785=CARTESIAN_POINT('Ctrl Pts',(-2.46253015529273,-1.01413124903004,
13.8571370725437));
#434786=CARTESIAN_POINT('Ctrl Pts',(-2.46277630400145,-1.01255202353858,
13.8577210840554));
#434787=CARTESIAN_POINT('Ctrl Pts',(-2.46315431302874,-1.01096275128894,
13.8581177131616));
#434788=CARTESIAN_POINT('Ctrl Pts',(-2.46326077338149,-1.01051515752235,
13.8582294175695));
#434789=CARTESIAN_POINT('Ctrl Pts',(-2.46337751512905,-1.01006676041904,
13.8583265086086));
#434790=CARTESIAN_POINT('Ctrl Pts',(-2.46350453475444,-1.00961899004926,
13.8584082369006));
#434791=CARTESIAN_POINT('Ctrl Pts',(-2.46368702789447,-1.00897566410226,
13.8585256585398));
#434792=CARTESIAN_POINT('Ctrl Pts',(-2.46389331650387,-1.00832572204297,
13.8586122832068));
#434793=CARTESIAN_POINT('Ctrl Pts',(-2.46411879448634,-1.00768628638081,
13.8586682984299));
#434794=CARTESIAN_POINT('Ctrl Pts',(-2.46429915452141,-1.0071748012363,
13.8587131050557));
#434795=CARTESIAN_POINT('Ctrl Pts',(-2.46449356365311,-1.00666431118519,
13.8587357943552));
#434796=CARTESIAN_POINT('Ctrl Pts',(-2.46470251826961,-1.00615493580846,
13.8587355499465));
#434797=CARTESIAN_POINT('Ctrl Pts',(-2.46483757061997,-1.00582571435839,
13.8587353919793));
#434798=CARTESIAN_POINT('Ctrl Pts',(-2.46497720290432,-1.00550050402571,
13.8587257282814));
#434799=CARTESIAN_POINT('Ctrl Pts',(-2.4651212924408,-1.00517922688567,
13.8587068136939));
#434800=CARTESIAN_POINT('Ctrl Pts',(-2.4651212924408,-1.00517922688567,
13.8587068136939));
#434801=CARTESIAN_POINT('Ctrl Pts',(-2.46559519507111,-1.00412256388679,
13.8586446046466));
#434802=CARTESIAN_POINT('Ctrl Pts',(-2.46611725339322,-1.00310839371633,
13.858482427929));
#434803=CARTESIAN_POINT('Ctrl Pts',(-2.46668364204556,-1.00213440281294,
13.8582284286032));
#434804=CARTESIAN_POINT('Ctrl Pts',(-2.46726469091784,-1.00113520144532,
13.8579678548414));
#434805=CARTESIAN_POINT('Ctrl Pts',(-2.46789513808288,-1.00017661541572,
13.857615680862));
#434806=CARTESIAN_POINT('Ctrl Pts',(-2.46854203293253,-0.999291111852187,
13.8571944833187));
#434807=CARTESIAN_POINT('Ctrl Pts',(-2.47015642518878,-0.997081247147531,
13.8561433417727));
#434808=CARTESIAN_POINT('Ctrl Pts',(-2.47194489814923,-0.99522034293792,
13.8546163505474));
#434809=CARTESIAN_POINT('Ctrl Pts',(-2.47370091570212,-0.993698364224767,
13.8528973491086));
#434810=CARTESIAN_POINT('Ctrl Pts',(-2.47402171420141,-0.993420321168572,
13.8525833129072));
#434811=CARTESIAN_POINT('Ctrl Pts',(-2.47434139677549,-0.993153451901128,
13.8522628768812));
#434812=CARTESIAN_POINT('Ctrl Pts',(-2.47465869042139,-0.992897516957365,
13.851937733538));
#434813=CARTESIAN_POINT('Ctrl Pts',(-2.47659635869437,-0.991334557765187,
13.8499521282529));
#434814=CARTESIAN_POINT('Ctrl Pts',(-2.47864006309533,-0.990027226120073,
13.847639871647));
#434815=CARTESIAN_POINT('Ctrl Pts',(-2.48063910114381,-0.988976552261284,
13.8452109780794));
#434816=CARTESIAN_POINT('Ctrl Pts',(-2.48153850973985,-0.988503832344347,
13.8441181685877));
#434817=CARTESIAN_POINT('Ctrl Pts',(-2.48242878298831,-0.988082355670984,
13.8430021611332));
#434818=CARTESIAN_POINT('Ctrl Pts',(-2.48329680034602,-0.987708963101414,
13.8418824960098));
#434819=CARTESIAN_POINT('Ctrl Pts',(-2.48534230541506,-0.986829053976304,
13.8392439765549));
#434820=CARTESIAN_POINT('Ctrl Pts',(-2.4873605080159,-0.986170628260006,
13.8364981347964));
#434821=CARTESIAN_POINT('Ctrl Pts',(-2.48934613184266,-0.985699411694597,
13.8336931113419));
#434822=CARTESIAN_POINT('Ctrl Pts',(-2.49128000335114,-0.985240476684907,
13.8309611966328));
#434823=CARTESIAN_POINT('Ctrl Pts',(-2.49318504041528,-0.984959208625481,
13.8281701127186));
#434824=CARTESIAN_POINT('Ctrl Pts',(-2.49505090983676,-0.984862862988851,
13.8253580685121));
#434825=CARTESIAN_POINT('Ctrl Pts',(-2.49545543234105,-0.98484197515085,
13.8247484142933));
#434826=CARTESIAN_POINT('Ctrl Pts',(-2.4958580248549,-0.984829927725528,
13.8241378483365));
#434827=CARTESIAN_POINT('Ctrl Pts',(-2.49625838937555,-0.984827048243808,
13.8235269408515));
#434828=CARTESIAN_POINT('',(-2.46463515361085,-1.0063222255279,12.5969504640361));
#434829=CARTESIAN_POINT('Origin',(-2.49653631825785,-1.01921348312305,12.584524458991));
#434830=CARTESIAN_POINT('Origin',(-2.49653631825785,-1.01921348312305,12.584524458991));
#434831=CARTESIAN_POINT('Ctrl Pts',(-2.47227204101564,-1.04358095837975,
12.5893111709658));
#434832=CARTESIAN_POINT('Ctrl Pts',(-2.46423365112037,-1.03559078175771,
12.5770542771492));
#434833=CARTESIAN_POINT('Ctrl Pts',(-2.47340424202235,-1.02203703919843,
12.5737548217797));
#434834=CARTESIAN_POINT('Ctrl Pts',(-2.48984930195276,-1.06105279306917,
12.5663937883685));
#434835=CARTESIAN_POINT('Ctrl Pts',(-2.48180065797481,-1.0530524238672,
12.5540940315304));
#434836=CARTESIAN_POINT('Ctrl Pts',(-2.49100232627946,-1.03945848052007,
12.5508374392248));
#434837=CARTESIAN_POINT('Ctrl Pts',(-2.50740882764907,-1.07850699889156,
12.5434499600945));
#434838=CARTESIAN_POINT('Ctrl Pts',(-2.49933401466334,-1.07048061764037,
12.5311293540533));
#434839=CARTESIAN_POINT('Ctrl Pts',(-2.50858238676034,-1.0568637392125,
12.5278936106989));
#434840=CARTESIAN_POINT('Ctrl Pts',(-2.52495200733029,-1.09594495674026,
12.5204817579905));
#434841=CARTESIAN_POINT('Ctrl Pts',(-2.51683722953868,-1.08787885038707,
12.5081597038247));
#434842=CARTESIAN_POINT('Ctrl Pts',(-2.52614581459653,-1.07425408289858,
12.5049254088044));
#434843=CARTESIAN_POINT('Ctrl Pts',(-2.51233926765277,-1.08340786672296,
12.5369868989719));
#434844=CARTESIAN_POINT('Ctrl Pts',(-2.51299991939328,-1.08406455572736,
12.5342545179733));
#434845=CARTESIAN_POINT('Ctrl Pts',(-2.51371835832708,-1.0846027960192,
12.5314872231885));
#434846=CARTESIAN_POINT('Ctrl Pts',(-2.5144876307328,-1.08494752935953,
12.5287124745062));
#434847=CARTESIAN_POINT('Ctrl Pts',(-2.51518139877155,-1.08525842699687,
12.5262100684184));
#434848=CARTESIAN_POINT('Ctrl Pts',(-2.51591621358577,-1.08541072777338,
12.5237004536639));
#434849=CARTESIAN_POINT('Ctrl Pts',(-2.51671814606732,-1.08534213574432,
12.5212220730815));
#434850=CARTESIAN_POINT('Ctrl Pts',(-2.51733209475465,-1.08528962261239,
12.5193246583486));
#434851=CARTESIAN_POINT('Ctrl Pts',(-2.51799266610991,-1.08510637931045,
12.517417831369));
#434852=CARTESIAN_POINT('Ctrl Pts',(-2.5186928674573,-1.08469542581355,
12.5155812248348));
#434853=CARTESIAN_POINT('Ctrl Pts',(-2.51899115699489,-1.08452035741499,
12.5147988205793));
#434854=CARTESIAN_POINT('Ctrl Pts',(-2.519297081633,-1.08430402523402,12.5140295443047));
#434855=CARTESIAN_POINT('Ctrl Pts',(-2.51961202432288,-1.08403983996772,
12.5132817086137));
#434856=CARTESIAN_POINT('Ctrl Pts',(-2.52008864747953,-1.08364003130536,
12.5121499604604));
#434857=CARTESIAN_POINT('Ctrl Pts',(-2.5205916205821,-1.08311651323026,
12.5110494206568));
#434858=CARTESIAN_POINT('Ctrl Pts',(-2.52110381888031,-1.08243621548882,
12.5100666561695));
#434859=CARTESIAN_POINT('Ctrl Pts',(-2.52139792196366,-1.08204559009228,
12.5095023550641));
#434860=CARTESIAN_POINT('Ctrl Pts',(-2.52169794324365,-1.0815983680367,
12.5089719619137));
#434861=CARTESIAN_POINT('Ctrl Pts',(-2.52199295514162,-1.08109937378121,
12.5085043804652));
#434862=CARTESIAN_POINT('Ctrl Pts',(-2.5224246666263,-1.08036916068688,
12.5078201359221));
#434863=CARTESIAN_POINT('Ctrl Pts',(-2.52285713215508,-1.0795062866642,
12.5072563000949));
#434864=CARTESIAN_POINT('Ctrl Pts',(-2.52325346833651,-1.07856544851782,
12.5068768744332));
#434865=CARTESIAN_POINT('Ctrl Pts',(-2.5235392540072,-1.07788703944677,
12.5066032824114));
#434866=CARTESIAN_POINT('Ctrl Pts',(-2.52381133074579,-1.07715619837718,
12.5064197834844));
#434867=CARTESIAN_POINT('Ctrl Pts',(-2.52405692751887,-1.07641463919388,
12.5063282718343));
#434868=CARTESIAN_POINT('Ctrl Pts',(-2.52441542277272,-1.07533219236719,
12.5061946931565));
#434869=CARTESIAN_POINT('Ctrl Pts',(-2.5247261680082,-1.07420410643136,
12.5062515701262));
#434870=CARTESIAN_POINT('Ctrl Pts',(-2.52498478704898,-1.07310449931496,
12.5064436508398));
#434871=CARTESIAN_POINT('',(-2.47340424202235,-1.02203703919843,12.5737548217797));
#434872=CARTESIAN_POINT('Origin',(-2.4877815271756,-1.02797788691757,12.5893111709658));
#434873=CARTESIAN_POINT('Ctrl Pts',(-2.52498478704898,-1.07310449931495,
12.5064436508398));
#434874=CARTESIAN_POINT('Ctrl Pts',(-2.51734986431254,-1.06554484703725,
12.5164271754438));
#434875=CARTESIAN_POINT('Ctrl Pts',(-2.50971176808834,-1.05798234658497,
12.5264061185523));
#434876=CARTESIAN_POINT('Ctrl Pts',(-2.50207038727473,-1.05041689697523,
12.536380305637));
#434877=CARTESIAN_POINT('Ctrl Pts',(-2.49252021109674,-1.04096161940157,
12.5488460165097));
#434878=CARTESIAN_POINT('Ctrl Pts',(-2.48296490157486,-1.03150173248874,
12.5613043021964));
#434879=CARTESIAN_POINT('Ctrl Pts',(-2.47340424202235,-1.02203703919843,
12.5737548217797));
#434880=CARTESIAN_POINT('Ctrl Pts',(-2.49625838937555,-0.984827048243808,
12.5893111709658));
#434881=CARTESIAN_POINT('Ctrl Pts',(-2.48492472314963,-0.984908561672269,
12.5770542771492));
#434882=CARTESIAN_POINT('Ctrl Pts',(-2.48198942389984,-1.00100786889864,
12.5737548217797));
#434883=CARTESIAN_POINT('Ctrl Pts',(-2.48568417736179,-0.984903099563596,
12.5928319619712));
#434884=CARTESIAN_POINT('Ctrl Pts',(-2.47809068312174,-0.988215539992912,
12.5821634970843));
#434885=CARTESIAN_POINT('Ctrl Pts',(-2.47813742652736,-1.001026133943,12.5773203894503));
#434886=CARTESIAN_POINT('Ctrl Pts',(-2.47051079898685,-0.991999062361609,
12.5969440695591));
#434887=CARTESIAN_POINT('Ctrl Pts',(-2.46897455729303,-0.995713696126876,
12.5878292599214));
#434888=CARTESIAN_POINT('Ctrl Pts',(-2.47273019157598,-1.00355713320773,
12.5813877129824));
#434889=CARTESIAN_POINT('Ctrl Pts',(-2.4588962530793,-1.02030590904051,
12.596957478804));
#434890=CARTESIAN_POINT('Ctrl Pts',(-2.46042121560877,-1.01661875804921,
12.5878468778671));
#434891=CARTESIAN_POINT('Ctrl Pts',(-2.46857870323226,-1.01369081037035,
12.5814011370086));
#434892=CARTESIAN_POINT('Ctrl Pts',(-2.46476140353657,-1.03611536877996,
12.5928371701607));
#434893=CARTESIAN_POINT('Ctrl Pts',(-2.46166358498239,-1.02843822178975,
12.5821692192951));
#434894=CARTESIAN_POINT('Ctrl Pts',(-2.47065667428546,-1.01931966012934,
12.5773318885715));
#434895=CARTESIAN_POINT('Ctrl Pts',(-2.4722720410156,-1.04358095837979,
12.5893111709658));
#434896=CARTESIAN_POINT('Ctrl Pts',(-2.46423365112033,-1.03559078175775,
12.5770542771492));
#434897=CARTESIAN_POINT('Ctrl Pts',(-2.47340424202231,-1.02203703919846,
12.5737548217797));
#434898=CARTESIAN_POINT('',(-2.48198942389984,-1.00100786889864,12.5737548217797));
#434899=CARTESIAN_POINT('Origin',(-2.49641661258517,-1.00682647926863,12.5893111709658));
#434900=CARTESIAN_POINT('Ctrl Pts',(-2.47340424202231,-1.02203703919846,
12.5737548217797));
#434901=CARTESIAN_POINT('Ctrl Pts',(-2.47267081664216,-1.0213540993455,
12.5746934679442));
#434902=CARTESIAN_POINT('Ctrl Pts',(-2.47198406714499,-1.02046431815534,
12.5756680099006));
#434903=CARTESIAN_POINT('Ctrl Pts',(-2.47141948997805,-1.01947096208094,
12.5765688348656));
#434904=CARTESIAN_POINT('Ctrl Pts',(-2.47127002442318,-1.01920798205705,
12.5768073183026));
#434905=CARTESIAN_POINT('Ctrl Pts',(-2.47112893565927,-1.01893792041428,
12.5770407398754));
#434906=CARTESIAN_POINT('Ctrl Pts',(-2.4709971326409,-1.01866296749603,
12.5772674179684));
#434907=CARTESIAN_POINT('Ctrl Pts',(-2.47045624869456,-1.01753463506996,
12.5781976435658));
#434908=CARTESIAN_POINT('Ctrl Pts',(-2.47005119299528,-1.01625496817453,
12.5790594849312));
#434909=CARTESIAN_POINT('Ctrl Pts',(-2.46985535344476,-1.01489579946016,
12.5797571720116));
#434910=CARTESIAN_POINT('Ctrl Pts',(-2.46972775693583,-1.0140102521714,
12.580211740231));
#434911=CARTESIAN_POINT('Ctrl Pts',(-2.46970175486773,-1.01304803552594,
12.5806009430798));
#434912=CARTESIAN_POINT('Ctrl Pts',(-2.46979688790372,-1.01207640680581,
12.5808812374708));
#434913=CARTESIAN_POINT('Ctrl Pts',(-2.46987863874168,-1.01124145540075,
12.5811221033394));
#434914=CARTESIAN_POINT('Ctrl Pts',(-2.47005162917057,-1.01038247107947,
12.581287365893));
#434915=CARTESIAN_POINT('Ctrl Pts',(-2.4703142692036,-1.00954958243355,
12.581359338449));
#434916=CARTESIAN_POINT('Ctrl Pts',(-2.47035077074488,-1.00943382811026,
12.5813693411482));
#434917=CARTESIAN_POINT('Ctrl Pts',(-2.47038895605253,-1.00931854182123,
12.5813775999465));
#434918=CARTESIAN_POINT('Ctrl Pts',(-2.47042877251051,-1.00920382037877,
12.5813841266931));
#434919=CARTESIAN_POINT('Ctrl Pts',(-2.47049632594716,-1.00900918157637,
12.5813952001081));
#434920=CARTESIAN_POINT('Ctrl Pts',(-2.47056960233931,-1.00881506473922,
12.5814007534795));
#434921=CARTESIAN_POINT('Ctrl Pts',(-2.47064875427473,-1.00862162405847,
12.5814005856065));
#434922=CARTESIAN_POINT('Ctrl Pts',(-2.47101108088868,-1.00773612825244,
12.5813998171494));
#434923=CARTESIAN_POINT('Ctrl Pts',(-2.47147118025235,-1.00692585411597,
12.58127954464));
#434924=CARTESIAN_POINT('Ctrl Pts',(-2.47200070969148,-1.00618079124599,
12.5810700125799));
#434925=CARTESIAN_POINT('Ctrl Pts',(-2.47264032096221,-1.00528084013127,
12.5808169217085));
#434926=CARTESIAN_POINT('Ctrl Pts',(-2.47339492940163,-1.00448564552451,
12.5804173076348));
#434927=CARTESIAN_POINT('Ctrl Pts',(-2.47417951190356,-1.00384697059521,
12.5799304713245));
#434928=CARTESIAN_POINT('Ctrl Pts',(-2.47515185679244,-1.00305545115446,
12.5793271277669));
#434929=CARTESIAN_POINT('Ctrl Pts',(-2.476210226903,-1.0024302587701,12.5785808224116));
#434930=CARTESIAN_POINT('Ctrl Pts',(-2.47729387858476,-1.00197043826641,
12.5777485681082));
#434931=CARTESIAN_POINT('Ctrl Pts',(-2.4789086383135,-1.00128525533883,
12.576508418016));
#434932=CARTESIAN_POINT('Ctrl Pts',(-2.48056325289046,-1.00096671160168,
12.5750928681475));
#434933=CARTESIAN_POINT('Ctrl Pts',(-2.48198942389984,-1.00100786889864,
12.5737548217797));
#434934=CARTESIAN_POINT('Ctrl Pts',(-2.48198942389984,-1.00100786889864,
12.5737548217797));
#434935=CARTESIAN_POINT('Ctrl Pts',(-2.48492472314963,-0.984908561672269,
12.5770542771492));
#434936=CARTESIAN_POINT('Ctrl Pts',(-2.49625838937555,-0.984827048243808,
12.5893111709658));
#434937=CARTESIAN_POINT('Ctrl Pts',(-2.5067482336128,-1.00088021402104,
12.5508408821982));
#434938=CARTESIAN_POINT('Ctrl Pts',(-2.50968946539744,-0.984730449929319,
12.5540974840599));
#434939=CARTESIAN_POINT('Ctrl Pts',(-2.52103759047877,-0.984648832510594,
12.5663972313419));
#434940=CARTESIAN_POINT('Ctrl Pts',(-2.53148285100647,-1.00075150434887,
12.52790050457));
#434941=CARTESIAN_POINT('Ctrl Pts',(-2.53440677726936,-0.984552679312757,
12.5311362602938));
#434942=CARTESIAN_POINT('Ctrl Pts',(-2.54579179343984,-0.98447079656777,
12.5434568539655));
#434943=CARTESIAN_POINT('Ctrl Pts',(-2.55619515606317,-1.00062180800529,
12.5049357605811));
#434944=CARTESIAN_POINT('Ctrl Pts',(-2.55908160313967,-0.984375214261865,
12.5081700652078));
#434945=CARTESIAN_POINT('Ctrl Pts',(-2.57052295611833,-0.984292926334116,
12.5204921097672));
#434946=CARTESIAN_POINT('Ctrl Pts',(-2.55457244923555,-1.0006303227885,
12.5064436508395));
#434947=CARTESIAN_POINT('Ctrl Pts',(-2.55520418375856,-0.999586407426494,
12.5062361689309));
#434948=CARTESIAN_POINT('Ctrl Pts',(-2.5558166210962,-0.998473882313115,
12.5061871075061));
#434949=CARTESIAN_POINT('Ctrl Pts',(-2.55634795984499,-0.997365416808395,
12.5063648335164));
#434950=CARTESIAN_POINT('Ctrl Pts',(-2.55658932667902,-0.996861883403164,
12.5064455676329));
#434951=CARTESIAN_POINT('Ctrl Pts',(-2.55681712641728,-0.996352069238074,
12.506574497099));
#434952=CARTESIAN_POINT('Ctrl Pts',(-2.55702063217175,-0.995857404874738,
12.5067492519495));
#434953=CARTESIAN_POINT('Ctrl Pts',(-2.5574295848849,-0.994863357635075,
12.5071004286051));
#434954=CARTESIAN_POINT('Ctrl Pts',(-2.5577547208358,-0.993893633970525,
12.5076537929613));
#434955=CARTESIAN_POINT('Ctrl Pts',(-2.5579806046668,-0.993024023516777,
12.5083435010505));
#434956=CARTESIAN_POINT('Ctrl Pts',(-2.55799482540385,-0.992969276341902,
12.5083869222964));
#434957=CARTESIAN_POINT('Ctrl Pts',(-2.55800864275887,-0.992914916990364,
12.5084308732337));
#434958=CARTESIAN_POINT('Ctrl Pts',(-2.55802204907216,-0.992860960426174,
12.5084753333615));
#434959=CARTESIAN_POINT('Ctrl Pts',(-2.55812958539951,-0.992428157565093,
12.5088319622689));
#434960=CARTESIAN_POINT('Ctrl Pts',(-2.55821410983573,-0.992012795146706,
12.509227847131));
#434961=CARTESIAN_POINT('Ctrl Pts',(-2.55827585284676,-0.991627782415668,
12.5096423454524));
#434962=CARTESIAN_POINT('Ctrl Pts',(-2.55846932811701,-0.990421322916091,
12.5109411997424));
#434963=CARTESIAN_POINT('Ctrl Pts',(-2.55846055503325,-0.989440198498566,
12.5124831113042));
#434964=CARTESIAN_POINT('Ctrl Pts',(-2.55833585077837,-0.988645612238747,
12.5140723025007));
#434965=CARTESIAN_POINT('Ctrl Pts',(-2.5583241658531,-0.988571158635915,
12.5142212114565));
#434966=CARTESIAN_POINT('Ctrl Pts',(-2.55831148407854,-0.988498321961358,
12.5143705582413));
#434967=CARTESIAN_POINT('Ctrl Pts',(-2.55829788955917,-0.988427059481295,
12.5145201959299));
#434968=CARTESIAN_POINT('Ctrl Pts',(-2.5581232477178,-0.98751158682615,
12.5164425148273));
#434969=CARTESIAN_POINT('Ctrl Pts',(-2.55780253768352,-0.986822527428655,
12.5184635205941));
#434970=CARTESIAN_POINT('Ctrl Pts',(-2.55738680472768,-0.986285501460735,
12.5205025929158));
#434971=CARTESIAN_POINT('Ctrl Pts',(-2.55714566313518,-0.985974005113623,
12.5216853356836));
#434972=CARTESIAN_POINT('Ctrl Pts',(-2.55687336943095,-0.985713926484789,
12.5228750347131));
#434973=CARTESIAN_POINT('Ctrl Pts',(-2.55658456686307,-0.985494379393402,
12.5240609649613));
#434974=CARTESIAN_POINT('Ctrl Pts',(-2.55587571645393,-0.984955512835885,
12.5269717671327));
#434975=CARTESIAN_POINT('Ctrl Pts',(-2.55504117034121,-0.984653930717825,
12.5299036066169));
#434976=CARTESIAN_POINT('Ctrl Pts',(-2.55412310074475,-0.984513929495684,
12.5328133004019));
#434977=CARTESIAN_POINT('Ctrl Pts',(-2.55368237388086,-0.98444672075703,
12.5342101228452));
#434978=CARTESIAN_POINT('Ctrl Pts',(-2.55322286943268,-0.984417351235913,
12.5356023438238));
#434979=CARTESIAN_POINT('Ctrl Pts',(-2.55275086849392,-0.984420745855558,
12.5369868989719));
#434980=CARTESIAN_POINT('Origin',(-15.2975147215125,-0.887461820663325,
-1.23983318115551));
#434981=CARTESIAN_POINT('Ctrl Pts',(-2.51230959790793,-1.0833784309085,
12.5369868989719));
#434982=CARTESIAN_POINT('Ctrl Pts',(-2.52320897086175,-1.09417134399527,
12.5369868989719));
#434983=CARTESIAN_POINT('Ctrl Pts',(-2.5168506574729,-1.10813039677596,
12.5369868989719));
#434984=CARTESIAN_POINT('Ctrl Pts',(-2.51599396564969,-1.08702690468825,
12.5218025310016));
#434985=CARTESIAN_POINT('Ctrl Pts',(-2.52172008227195,-1.09736457619265,
12.5216901060418));
#434986=CARTESIAN_POINT('Ctrl Pts',(-2.51687005472745,-1.10808785179314,
12.5161920673678));
#434987=CARTESIAN_POINT('Ctrl Pts',(-2.52193756172439,-1.08602204803375,
12.5042015548895));
#434988=CARTESIAN_POINT('Ctrl Pts',(-2.52395457229035,-1.09213015849392,
12.4980677368514));
#434989=CARTESIAN_POINT('Ctrl Pts',(-2.52124997823278,-1.09836521668991,
12.4907278922776));
#434990=CARTESIAN_POINT('Ctrl Pts',(-2.52496637940152,-1.07309667615577,
12.506463626192));
#434991=CARTESIAN_POINT('Ctrl Pts',(-2.53098787677485,-1.07565577906879,
12.4999376786891));
#434992=CARTESIAN_POINT('Ctrl Pts',(-2.53091433293968,-1.07562452334764,
12.4906970594712));
#434993=CARTESIAN_POINT('Origin',(-2.49682978149281,-1.09901093818514,12.5369868989719));
#434994=CARTESIAN_POINT('Origin',(-2.49682978149281,-1.09901093818514,14.));
#434995=CARTESIAN_POINT('Origin',(-2.49682978149281,-1.09901093818514,13.7435492065112));
#434996=CARTESIAN_POINT('Ctrl Pts',(-2.49477862706859,-1.06595259098269,
13.793642941384));
#434997=CARTESIAN_POINT('Ctrl Pts',(-2.50246621943784,-1.07355569183496,
13.8071662555867));
#434998=CARTESIAN_POINT('Ctrl Pts',(-2.49240131733838,-1.08729312716194,
13.8103758687955));
#434999=CARTESIAN_POINT('Ctrl Pts',(-2.50656683636598,-1.07767009185895,
13.7804579775007));
#435000=CARTESIAN_POINT('Ctrl Pts',(-2.51604549960272,-1.08705884124179,
13.7901904343352));
#435001=CARTESIAN_POINT('Ctrl Pts',(-2.50891251606055,-1.10110791487494,
13.7927914348263));
#435002=CARTESIAN_POINT('Ctrl Pts',(-2.51350699879274,-1.0845686256309,
13.7597120340894));
#435003=CARTESIAN_POINT('Ctrl Pts',(-2.52447244887986,-1.0954381239799,
13.7635825532444));
#435004=CARTESIAN_POINT('Ctrl Pts',(-2.51863274757549,-1.10927408454719,
13.7651073818884));
#435005=CARTESIAN_POINT('Ctrl Pts',(-2.51214795607736,-1.08321773476046,
13.7381884353898));
#435006=CARTESIAN_POINT('Ctrl Pts',(-2.52285737214662,-1.0938321738922,
13.7368803041982));
#435007=CARTESIAN_POINT('Ctrl Pts',(-2.51672891949728,-1.10767528428125,
13.7363986145813));
#435008=CARTESIAN_POINT('Origin',(-2.48212954747994,-1.08439887436658,13.7902182540695));
#435009=CARTESIAN_POINT('Ctrl Pts',(-2.47226924880857,-1.04357818399006,
13.8235227101244));
#435010=CARTESIAN_POINT('Ctrl Pts',(-2.48042644875974,-1.05168020702606,
13.8358800583119));
#435011=CARTESIAN_POINT('Ctrl Pts',(-2.47104782899332,-1.06534284002023,
13.8390832900376));
#435012=CARTESIAN_POINT('Ctrl Pts',(-2.48072865212883,-1.05198684885194,
13.8124254819053));
#435013=CARTESIAN_POINT('Ctrl Pts',(-2.48890169305066,-1.06010460609919,
13.8247886449158));
#435014=CARTESIAN_POINT('Ctrl Pts',(-2.47949717086737,-1.07377485641168,
13.8279860620657));
#435015=CARTESIAN_POINT('Ctrl Pts',(-2.48918426421976,-1.06039174522379,
13.8013225099955));
#435016=CARTESIAN_POINT('Ctrl Pts',(-2.49736929116205,-1.06852140498214,
13.8136962257787));
#435017=CARTESIAN_POINT('Ctrl Pts',(-2.48794279258049,-1.08220277733194,
13.8168830918626));
#435018=CARTESIAN_POINT('Ctrl Pts',(-2.49763623259224,-1.06879301973175,
13.7902140179785));
#435019=CARTESIAN_POINT('Ctrl Pts',(-2.50582964255204,-1.07693100073291,
13.802602731458));
#435020=CARTESIAN_POINT('Ctrl Pts',(-2.49638484160682,-1.09062676239944,
13.8057746032558));
#435021=CARTESIAN_POINT('Origin',(-2.45676255485568,-1.05918402984193,13.8235269408515));
#435022=CARTESIAN_POINT('Ctrl Pts',(-2.49625838937555,-0.984827048243808,
13.8235269408515));
#435023=CARTESIAN_POINT('Ctrl Pts',(-2.50806556547983,-0.984742129261236,
13.8362179249168));
#435024=CARTESIAN_POINT('Ctrl Pts',(-2.51070655207738,-0.967869423673549,
13.8391868794938));
#435025=CARTESIAN_POINT('Ctrl Pts',(-2.48545533717591,-0.984904745416557,
13.8400110824519));
#435026=CARTESIAN_POINT('Ctrl Pts',(-2.49489720033065,-0.981415750858121,
13.8494522556837));
#435027=CARTESIAN_POINT('Ctrl Pts',(-2.49292858601838,-0.968109645299923,
13.85569149686));
#435028=CARTESIAN_POINT('Ctrl Pts',(-2.47064022047438,-0.991680440448419,
13.8586819406588));
#435029=CARTESIAN_POINT('Ctrl Pts',(-2.47229870031127,-0.987654836361377,
13.868010383617));
#435030=CARTESIAN_POINT('Ctrl Pts',(-2.46839592148099,-0.979490206290489,
13.8744918421245));
#435031=CARTESIAN_POINT('Ctrl Pts',(-2.45876480710159,-1.02062946556451,
13.8587686893867));
#435032=CARTESIAN_POINT('Ctrl Pts',(-2.45712103565668,-1.02461922036359,
13.8680909899357));
#435033=CARTESIAN_POINT('Ctrl Pts',(-2.44862922604038,-1.02768280828403,
13.8745789365163));
#435034=CARTESIAN_POINT('Ctrl Pts',(-2.46459752052836,-1.03595246873103,
13.8400379222776));
#435035=CARTESIAN_POINT('Ctrl Pts',(-2.46889230838958,-1.0450532945801,
13.8494748685453));
#435036=CARTESIAN_POINT('Ctrl Pts',(-2.4581794038028,-1.05317701174524,
13.8557104837033));
#435037=CARTESIAN_POINT('Ctrl Pts',(-2.47227204101088,-1.04358095838433,
13.8235269408542));
#435038=CARTESIAN_POINT('Ctrl Pts',(-2.4806462672494,-1.05190495704464,
13.8362179249195));
#435039=CARTESIAN_POINT('Ctrl Pts',(-2.47072418525568,-1.0658051474378,
13.8391868794965));
#435040=CARTESIAN_POINT('Origin',(-2.49610016616593,-0.962827617218985,
13.8235269408515));
#435041=CARTESIAN_POINT('Ctrl Pts',(-2.53202044341779,-0.984569841423958,
13.7902140241683));
#435042=CARTESIAN_POINT('Ctrl Pts',(-2.54356827512419,-0.984491239432124,
13.8026027327198));
#435043=CARTESIAN_POINT('Ctrl Pts',(-2.54640710301046,-0.968098588990368,
13.8057746032556));
#435044=CARTESIAN_POINT('Ctrl Pts',(-2.52010365538259,-0.98465554875306,
13.8013225161808));
#435045=CARTESIAN_POINT('Ctrl Pts',(-2.53163967556639,-0.984577023570956,
13.8136962270464));
#435046=CARTESIAN_POINT('Ctrl Pts',(-2.53448150603375,-0.96820746020147,
13.8168830918628));
#435047=CARTESIAN_POINT('Ctrl Pts',(-2.50818172991283,-0.984741293031374,
13.8124254880875));
#435048=CARTESIAN_POINT('Ctrl Pts',(-2.51970085863903,-0.984662881106717,
13.8247886461868));
#435049=CARTESIAN_POINT('Ctrl Pts',(-2.52255060261411,-0.968316642350521,
13.8279860620656));
#435050=CARTESIAN_POINT('Ctrl Pts',(-2.49625445902509,-0.98482707575475,
13.8235227163065));
#435051=CARTESIAN_POINT('Ctrl Pts',(-2.50775126113095,-0.984748816086976,
13.8358800595847));
#435052=CARTESIAN_POINT('Ctrl Pts',(-2.51061417570187,-0.968426146239254,
13.8390832900376));
#435053=CARTESIAN_POINT('Origin',(-2.5318661630017,-0.962570382801957,13.7902182540695));
#435054=CARTESIAN_POINT('Ctrl Pts',(-2.55248101537279,-0.984422659094525,
13.7382347919292));
#435055=CARTESIAN_POINT('Ctrl Pts',(-2.56757110230241,-0.984338129869166,
13.7369371795943));
#435056=CARTESIAN_POINT('Ctrl Pts',(-2.5728782039146,-0.970147342382266,
13.7364597369711));
#435057=CARTESIAN_POINT('Ctrl Pts',(-2.55437252506769,-0.984409055475106,
13.7595490285574));
#435058=CARTESIAN_POINT('Ctrl Pts',(-2.56982264290434,-0.984321504045932,
13.7633824266926));
#435059=CARTESIAN_POINT('Ctrl Pts',(-2.57532661145888,-0.970335797397424,
13.7648920890506));
#435060=CARTESIAN_POINT('Ctrl Pts',(-2.5447259292492,-0.984478433196848,
13.7803806590111));
#435061=CARTESIAN_POINT('Ctrl Pts',(-2.55808975877626,-0.984408102714666,
13.7901039518744));
#435062=CARTESIAN_POINT('Ctrl Pts',(-2.56284407749788,-0.969378734966195,
13.7926933640892));
#435063=CARTESIAN_POINT('Ctrl Pts',(-2.52795799232525,-0.984599027087206,
13.7936647693663));
#435064=CARTESIAN_POINT('Ctrl Pts',(-2.53877330767256,-0.984551216180718,
13.8072068914933));
#435065=CARTESIAN_POINT('Ctrl Pts',(-2.541190537481,-0.967675160068563,
13.8104111085397));
#435066=CARTESIAN_POINT('Origin',(-2.5525926452843,-0.962421314830735,13.7435492065112));
#435067=CARTESIAN_POINT('Origin',(-2.5525926452843,-0.962421314830735,14.));
#435068=CARTESIAN_POINT('Origin',(-2.5525926452843,-0.962421314830735,12.5369868989719));
#435069=CARTESIAN_POINT('Ctrl Pts',(-2.55455533228426,-1.00062361806097,
12.506462012331));
#435070=CARTESIAN_POINT('Ctrl Pts',(-2.56064355629324,-1.00300838564006,
12.4999388158272));
#435071=CARTESIAN_POINT('Ctrl Pts',(-2.560571524619,-1.00298017071217,12.4907030323752));
#435072=CARTESIAN_POINT('Ctrl Pts',(-2.56143590016693,-0.989270804807574,
12.5042014951932));
#435073=CARTESIAN_POINT('Ctrl Pts',(-2.56714935721315,-0.986321651421119,
12.4980716682127));
#435074=CARTESIAN_POINT('Ctrl Pts',(-2.56958091457031,-0.979980271914656,
12.4907355092743));
#435075=CARTESIAN_POINT('Ctrl Pts',(-2.55789615703068,-0.984392698640763,
12.5218047446509));
#435076=CARTESIAN_POINT('Ctrl Pts',(-2.56921524231361,-0.981016727773746,
12.5216906929434));
#435077=CARTESIAN_POINT('Ctrl Pts',(-2.57325716832047,-0.969969846381957,
12.5161988840776));
#435078=CARTESIAN_POINT('Ctrl Pts',(-2.55271245313378,-0.984420988602842,
12.5369868989719));
#435079=CARTESIAN_POINT('Ctrl Pts',(-2.56804211594788,-0.984337504913307,
12.5369868989719));
#435080=CARTESIAN_POINT('Ctrl Pts',(-2.57327252109055,-0.969927494727188,
12.5369868989719));
#435081=CARTESIAN_POINT('Origin',(-4.76969326057513E-31,-7.09909511483994E-31,
12.5));
#435082=CARTESIAN_POINT('Origin',(-2.40767974839161,-1.18501835034964,12.5));
#435083=CARTESIAN_POINT('',(-2.40767974839161,-1.18501835034964,12.5893111709658));
#435084=CARTESIAN_POINT('',(-2.40767974839161,-1.18501835034964,13.8235269408515));
#435085=CARTESIAN_POINT('',(-2.40767974839161,-1.18501835034964,12.5));
#435086=CARTESIAN_POINT('',(-2.44334770381643,-1.18767723263634,13.7902182540695));
#435087=CARTESIAN_POINT('',(-2.40767974839161,-1.18501835034964,13.8235269408515));
#435088=CARTESIAN_POINT('',(-2.46401737086258,-1.1892180613978,13.7435492065112));
#435089=CARTESIAN_POINT('Origin',(-2.39601441527465,-1.18414907999287,13.7445212918693));
#435090=CARTESIAN_POINT('',(-2.46401737086258,-1.1892180613978,12.5369868989719));
#435091=CARTESIAN_POINT('',(-2.46401737086258,-1.1892180613978,12.5));
#435092=CARTESIAN_POINT('Ctrl Pts',(-2.46401737086258,-1.1892180613978,
12.5369868989719));
#435093=CARTESIAN_POINT('Ctrl Pts',(-2.44525185978402,-1.18781917871968,
12.5544431401645));
#435094=CARTESIAN_POINT('Ctrl Pts',(-2.42647292711318,-1.18641929552349,
12.5718848856037));
#435095=CARTESIAN_POINT('Ctrl Pts',(-2.40767974839161,-1.18501835034964,
12.5893111709658));
#435096=CARTESIAN_POINT('Origin',(-2.55757155380599,-1.45074258662954,12.5));
#435097=CARTESIAN_POINT('',(-2.41567186698722,-1.28458189015483,13.7435492065112));
#435098=CARTESIAN_POINT('',(-2.40221156564333,-1.26882024123085,13.7902182540695));
#435099=CARTESIAN_POINT('Origin',(-2.36684022012061,-1.22740135202068,13.7418732680454));
#435100=CARTESIAN_POINT('',(-2.37898422350636,-1.24162165162673,13.8235269408515));
#435101=CARTESIAN_POINT('',(-2.40221156564333,-1.26882024123085,13.7902182540695));
#435102=CARTESIAN_POINT('',(-2.37898422350636,-1.24162165162673,12.5893111709658));
#435103=CARTESIAN_POINT('',(-2.37898422350636,-1.24162165162673,12.5));
#435104=CARTESIAN_POINT('',(-2.41567186698722,-1.28458189015483,12.5369868989719));
#435105=CARTESIAN_POINT('Ctrl Pts',(-2.37898422350636,-1.24162165162673,
12.5893111709658));
#435106=CARTESIAN_POINT('Ctrl Pts',(-2.39122253621053,-1.25595238489465,
12.5718848856037));
#435107=CARTESIAN_POINT('Ctrl Pts',(-2.40345157173885,-1.27027225484049,
12.5544431401645));
#435108=CARTESIAN_POINT('Ctrl Pts',(-2.41567186698722,-1.28458189015483,
12.5369868989719));
#435109=CARTESIAN_POINT('',(-2.41567186698722,-1.28458189015483,12.5));
#435110=CARTESIAN_POINT('Origin',(-2.40512434038171,-1.21929823533928,12.5));
#435111=CARTESIAN_POINT('',(-2.37498736607852,-1.20276484633319,13.8587068136939));
#435112=CARTESIAN_POINT('Ctrl Pts',(-2.37898422350124,-1.24162165163091,
13.8235269408542));
#435113=CARTESIAN_POINT('Ctrl Pts',(-2.37784626611898,-1.24028913430522,
13.8262006681044));
#435114=CARTESIAN_POINT('Ctrl Pts',(-2.37681385129937,-1.2388126697197,
13.8288634856214));
#435115=CARTESIAN_POINT('Ctrl Pts',(-2.37588031978227,-1.23720381037638,
13.8314912288862));
#435116=CARTESIAN_POINT('Ctrl Pts',(-2.37491794507746,-1.23554524233957,
13.834200161153));
#435117=CARTESIAN_POINT('Ctrl Pts',(-2.37405915970181,-1.23374437910986,
13.8368750301949));
#435118=CARTESIAN_POINT('Ctrl Pts',(-2.37332198838734,-1.23177643409771,
13.8394886372968));
#435119=CARTESIAN_POINT('Ctrl Pts',(-2.37326505485859,-1.23162444493085,
13.8396904925131));
#435120=CARTESIAN_POINT('Ctrl Pts',(-2.37320886583138,-1.23147144791995,
13.8398919674349));
#435121=CARTESIAN_POINT('Ctrl Pts',(-2.37315343994553,-1.23131742673428,
13.8400930404591));
#435122=CARTESIAN_POINT('Ctrl Pts',(-2.37228986735531,-1.22891767304111,
13.8432258934518));
#435123=CARTESIAN_POINT('Ctrl Pts',(-2.37161490042454,-1.22628191953871,
13.8462331177034));
#435124=CARTESIAN_POINT('Ctrl Pts',(-2.37124400375196,-1.22347219932811,
13.8489036603661));
#435125=CARTESIAN_POINT('Ctrl Pts',(-2.37112264204435,-1.22255282617684,
13.8497774930041));
#435126=CARTESIAN_POINT('Ctrl Pts',(-2.37103399946237,-1.22161501624451,
13.85061494757));
#435127=CARTESIAN_POINT('Ctrl Pts',(-2.37098257786962,-1.22066149144389,
13.8514076489583));
#435128=CARTESIAN_POINT('Ctrl Pts',(-2.37087381378487,-1.21864464897173,
13.8530843267192));
#435129=CARTESIAN_POINT('Ctrl Pts',(-2.3709238404227,-1.21635923447046,
13.8546805203176));
#435130=CARTESIAN_POINT('Ctrl Pts',(-2.37126616728438,-1.21394087859148,
13.8559412814274));
#435131=CARTESIAN_POINT('Ctrl Pts',(-2.3713119817204,-1.21361722414575,
13.8561100121513));
#435132=CARTESIAN_POINT('Ctrl Pts',(-2.37136296666668,-1.21329122965459,
13.8562727473908));
#435133=CARTESIAN_POINT('Ctrl Pts',(-2.37141937349435,-1.21296325246101,
13.8564289040185));
#435134=CARTESIAN_POINT('Ctrl Pts',(-2.37167517781431,-1.21147587962978,
13.8571370725437));
#435135=CARTESIAN_POINT('Ctrl Pts',(-2.37204922902188,-1.20992197228575,
13.8577210840554));
#435136=CARTESIAN_POINT('Ctrl Pts',(-2.37255552069773,-1.2083687994534,
13.8581177131616));
#435137=CARTESIAN_POINT('Ctrl Pts',(-2.37269810985969,-1.20793137252523,
13.8582294175695));
#435138=CARTESIAN_POINT('Ctrl Pts',(-2.37285101168534,-1.2074939829625,
13.8583265086086));
#435139=CARTESIAN_POINT('Ctrl Pts',(-2.37301410610544,-1.20705805579035,
13.8584082369006));
#435140=CARTESIAN_POINT('Ctrl Pts',(-2.37324842905163,-1.20643174534246,
13.8585256585398));
#435141=CARTESIAN_POINT('Ctrl Pts',(-2.37350700756429,-1.20580078034851,
13.8586122832068));
#435142=CARTESIAN_POINT('Ctrl Pts',(-2.37378385523008,-1.20518185090458,
13.8586682984299));
#435143=CARTESIAN_POINT('Ctrl Pts',(-2.37400530591969,-1.20468676870193,
13.8587131050557));
#435144=CARTESIAN_POINT('Ctrl Pts',(-2.37424067784936,-1.2041938234134,
13.8587357943552));
#435145=CARTESIAN_POINT('Ctrl Pts',(-2.37449045600862,-1.2037031746823,
13.8587355499465));
#435146=CARTESIAN_POINT('Ctrl Pts',(-2.37465189358794,-1.20338605670978,
13.8587353919793));
#435147=CARTESIAN_POINT('Ctrl Pts',(-2.37481756891859,-1.20307330981514,
13.8587257282814));
#435148=CARTESIAN_POINT('Ctrl Pts',(-2.37498736607852,-1.20276484633319,
13.8587068136939));
#435149=CARTESIAN_POINT('Ctrl Pts',(-2.37498736607852,-1.20276484633319,
13.8587068136939));
#435150=CARTESIAN_POINT('Ctrl Pts',(-2.37554581968092,-1.20175032675711,
13.8586446046466));
#435151=CARTESIAN_POINT('Ctrl Pts',(-2.37614880518103,-1.20078208375401,
13.858482427929));
#435152=CARTESIAN_POINT('Ctrl Pts',(-2.37679269852259,-1.19985749965825,
13.8582284286032));
#435153=CARTESIAN_POINT('Ctrl Pts',(-2.37745325819027,-1.19890898392803,
13.8579678548414));
#435154=CARTESIAN_POINT('Ctrl Pts',(-2.37815974125487,-1.1980049748111,
13.857615680862));
#435155=CARTESIAN_POINT('Ctrl Pts',(-2.37887666037631,-1.19717514562335,
13.8571944833187));
#435156=CARTESIAN_POINT('Ctrl Pts',(-2.38066580536432,-1.19510422201738,
13.8561433417727));
#435157=CARTESIAN_POINT('Ctrl Pts',(-2.38260000829739,-1.19339528696266,
13.8546163505475));
#435158=CARTESIAN_POINT('Ctrl Pts',(-2.38447423824122,-1.19202150424076,
13.8528973491086));
#435159=CARTESIAN_POINT('Ctrl Pts',(-2.38481663240028,-1.19177053440573,
13.8525833129073));
#435160=CARTESIAN_POINT('Ctrl Pts',(-2.38515700357976,-1.19153061022133,
13.8522628768812));
#435161=CARTESIAN_POINT('Ctrl Pts',(-2.38549410253113,-1.19130138925773,
13.851937733538));
#435162=CARTESIAN_POINT('Ctrl Pts',(-2.38755271905675,-1.18990156863601,
13.8499521282529));
#435163=CARTESIAN_POINT('Ctrl Pts',(-2.38969618286566,-1.1887651679106,
13.847639871647));
#435164=CARTESIAN_POINT('Ctrl Pts',(-2.39177420895342,-1.18788093024152,
13.8452109780794));
#435165=CARTESIAN_POINT('Ctrl Pts',(-2.3927091559033,-1.18748309341139,
13.8441181685877));
#435166=CARTESIAN_POINT('Ctrl Pts',(-2.39363082110264,-1.18713558470153,
13.8430021611332));
#435167=CARTESIAN_POINT('Ctrl Pts',(-2.39452638516502,-1.18683418603786,
13.8418824960098));
#435168=CARTESIAN_POINT('Ctrl Pts',(-2.39663680474706,-1.18612393239045,
13.8392439765549));
#435169=CARTESIAN_POINT('Ctrl Pts',(-2.39870195975365,-1.18563219977946,
13.8364981347964));
#435170=CARTESIAN_POINT('Ctrl Pts',(-2.40071938510556,-1.18532439792381,
13.8336931113419));
#435171=CARTESIAN_POINT('Ctrl Pts',(-2.40268422927996,-1.18502461846363,
13.8309611966328));
#435172=CARTESIAN_POINT('Ctrl Pts',(-2.40460585344843,-1.1848995645067,
13.8281701127186));
#435173=CARTESIAN_POINT('Ctrl Pts',(-2.40647336740714,-1.18495562513197,
13.8253580685121));
#435174=CARTESIAN_POINT('Ctrl Pts',(-2.40687824644888,-1.18496777913603,
13.8247484142933));
#435175=CARTESIAN_POINT('Ctrl Pts',(-2.40728048134637,-1.18498858682488,
13.8241378483365));
#435176=CARTESIAN_POINT('Ctrl Pts',(-2.40767974839161,-1.18501835034964,
13.8235269408515));
#435177=CARTESIAN_POINT('',(-2.37440967983503,-1.20386441691394,12.5969504640361));
#435178=CARTESIAN_POINT('Origin',(-2.40515393881772,-1.21931302098757,12.584524458991));
#435179=CARTESIAN_POINT('Origin',(-2.40515393881772,-1.21931302098757,12.584524458991));
#435180=CARTESIAN_POINT('Ctrl Pts',(-2.37898422350636,-1.24162165162673,
12.5893111709658));
#435181=CARTESIAN_POINT('Ctrl Pts',(-2.37162385426222,-1.23300285825703,
12.5770542771492));
#435182=CARTESIAN_POINT('Ctrl Pts',(-2.38186868662488,-1.22024170295212,
12.5737548217797));
#435183=CARTESIAN_POINT('Ctrl Pts',(-2.39507888082995,-1.26046806017326,
12.5663937883685));
#435184=CARTESIAN_POINT('Ctrl Pts',(-2.38770912241267,-1.25183827233565,
12.5540940315304));
#435185=CARTESIAN_POINT('Ctrl Pts',(-2.39798820550788,-1.23903958310452,
12.5508374392248));
#435186=CARTESIAN_POINT('Ctrl Pts',(-2.41115729884161,-1.27929545292459,
12.5434499600945));
#435187=CARTESIAN_POINT('Ctrl Pts',(-2.40376357871525,-1.27063760657353,
12.5311293540533));
#435188=CARTESIAN_POINT('Ctrl Pts',(-2.41409107962181,-1.25781986536901,
12.5278936106989));
#435189=CARTESIAN_POINT('Ctrl Pts',(-2.42722074958886,-1.29810531941401,
12.5204817579905));
#435190=CARTESIAN_POINT('Ctrl Pts',(-2.41979043560079,-1.28940462264037,
12.5081597038247));
#435191=CARTESIAN_POINT('Ctrl Pts',(-2.43017859214625,-1.27658392654064,
12.5049254088044));
#435192=CARTESIAN_POINT('Ctrl Pts',(-2.41567186698722,-1.28458189015483,
12.5369868989719));
#435193=CARTESIAN_POINT('Ctrl Pts',(-2.4162767942133,-1.28529024333077,
12.5342545179733));
#435194=CARTESIAN_POINT('Ctrl Pts',(-2.41694897102025,-1.28588525211521,
12.5314872231885));
#435195=CARTESIAN_POINT('Ctrl Pts',(-2.41768758476792,-1.28629154122643,
12.5287124745063));
#435196=CARTESIAN_POINT('Ctrl Pts',(-2.41835370330707,-1.28665795291332,
12.5262100684184));
#435197=CARTESIAN_POINT('Ctrl Pts',(-2.41907365915844,-1.28686964115061,
12.5237004536639));
#435198=CARTESIAN_POINT('Ctrl Pts',(-2.41987851416296,-1.28686664229789,
12.5212220730815));
#435199=CARTESIAN_POINT('Ctrl Pts',(-2.42049470029444,-1.28686434641671,
12.5193246583486));
#435200=CARTESIAN_POINT('Ctrl Pts',(-2.42116800968327,-1.28673555553964,
12.517417831369));
#435201=CARTESIAN_POINT('Ctrl Pts',(-2.42189937769354,-1.28638304236677,
12.5155812248347));
#435202=CARTESIAN_POINT('Ctrl Pts',(-2.42221094439704,-1.28623286986036,
12.5147988205793));
#435203=CARTESIAN_POINT('Ctrl Pts',(-2.42253348417723,-1.28604219320495,
12.5140295443047));
#435204=CARTESIAN_POINT('Ctrl Pts',(-2.42286891247307,-1.28580455774634,
12.5132817086137));
#435205=CARTESIAN_POINT('Ctrl Pts',(-2.42337653782311,-1.28544492862634,
12.5121499604604));
#435206=CARTESIAN_POINT('Ctrl Pts',(-2.42392050890739,-1.28496414949169,
12.5110494206568));
#435207=CARTESIAN_POINT('Ctrl Pts',(-2.42448645348953,-1.28432786430119,
12.5100666561695));
#435208=CARTESIAN_POINT('Ctrl Pts',(-2.42481141756533,-1.28396251081004,
12.5095023550641));
#435209=CARTESIAN_POINT('Ctrl Pts',(-2.42514689329859,-1.28354123136856,
12.5089719619137));
#435210=CARTESIAN_POINT('Ctrl Pts',(-2.42548159623306,-1.28306794368374,
12.5085043804652));
#435211=CARTESIAN_POINT('Ctrl Pts',(-2.42597139037954,-1.28237534880706,
12.5078201359221));
#435212=CARTESIAN_POINT('Ctrl Pts',(-2.42647274915835,-1.28155059588188,
12.5072563000949));
#435213=CARTESIAN_POINT('Ctrl Pts',(-2.42694445360708,-1.28064519337502,
12.5068768744332));
#435214=CARTESIAN_POINT('Ctrl Pts',(-2.42728458498685,-1.27999233583945,
12.5066032824114));
#435215=CARTESIAN_POINT('Ctrl Pts',(-2.42761532674451,-1.27928610336327,
12.5064197834844));
#435216=CARTESIAN_POINT('Ctrl Pts',(-2.42792055027233,-1.27856703007399,
12.5063282718343));
#435217=CARTESIAN_POINT('Ctrl Pts',(-2.42836608212811,-1.27751740569111,
12.5061946931565));
#435218=CARTESIAN_POINT('Ctrl Pts',(-2.42876774286086,-1.27641840198969,
12.5062515701262));
#435219=CARTESIAN_POINT('Ctrl Pts',(-2.42911512955636,-1.27534353357797,
12.5064436508398));
#435220=CARTESIAN_POINT('',(-2.38186868662489,-1.22024170295212,12.5737548217797));
#435221=CARTESIAN_POINT('Origin',(-2.39571389830658,-1.22733466520276,12.5893111709658));
#435222=CARTESIAN_POINT('Ctrl Pts',(-2.42911512955636,-1.27534353357797,
12.5064436508398));
#435223=CARTESIAN_POINT('Ctrl Pts',(-2.42212179323652,-1.2671867183374,
12.5164271754438));
#435224=CARTESIAN_POINT('Ctrl Pts',(-2.41512552614109,-1.25902680573062,
12.5264061185523));
#435225=CARTESIAN_POINT('Ctrl Pts',(-2.40812622576917,-1.25086368605492,
12.536380305637));
#435226=CARTESIAN_POINT('Ctrl Pts',(-2.39937851991535,-1.24066144211936,
12.5488460165097));
#435227=CARTESIAN_POINT('Ctrl Pts',(-2.39062607350234,-1.23045418576666,
12.5613043021964));
#435228=CARTESIAN_POINT('Ctrl Pts',(-2.38186868662488,-1.22024170295212,
12.5737548217797));
#435229=CARTESIAN_POINT('Ctrl Pts',(-2.40767974839161,-1.18501835034964,
12.5893111709658));
#435230=CARTESIAN_POINT('Ctrl Pts',(-2.39637714990393,-1.18417579353485,
12.5770542771492));
#435231=CARTESIAN_POINT('Ctrl Pts',(-2.39213937462263,-1.19998227750568,
12.5737548217797));
#435232=CARTESIAN_POINT('Ctrl Pts',(-2.39713452230741,-1.18423225216962,
12.5928319619712));
#435233=CARTESIAN_POINT('Ctrl Pts',(-2.38929630014685,-1.18691473045154,
12.5821634970843));
#435234=CARTESIAN_POINT('Ctrl Pts',(-2.38829870568296,-1.19968650822855,
12.5773203894503));
#435235=CARTESIAN_POINT('Ctrl Pts',(-2.38143324525357,-1.19006783253646,
12.5969440695591));
#435236=CARTESIAN_POINT('Ctrl Pts',(-2.3795993381404,-1.19364488820449,
12.5878292599214));
#435237=CARTESIAN_POINT('Ctrl Pts',(-2.38270316292309,-1.20176834595517,
12.5813877129824));
#435238=CARTESIAN_POINT('Ctrl Pts',(-2.36755007499711,-1.21733379720254,
12.596957478804));
#435239=CARTESIAN_POINT('Ctrl Pts',(-2.3693705003752,-1.21378321350521,
12.5878468778671));
#435240=CARTESIAN_POINT('Ctrl Pts',(-2.37773949954914,-1.21152991930245,
12.5814011370086));
#435241=CARTESIAN_POINT('Ctrl Pts',(-2.37210709191346,-1.23356871648057,
12.5928371701607));
#435242=CARTESIAN_POINT('Ctrl Pts',(-2.36964533984581,-1.22566461359273,
12.5821692192951));
#435243=CARTESIAN_POINT('Ctrl Pts',(-2.37935175281402,-1.21730941345999,
12.5773318885715));
#435244=CARTESIAN_POINT('Ctrl Pts',(-2.37898422350631,-1.24162165162676,
12.5893111709658));
#435245=CARTESIAN_POINT('Ctrl Pts',(-2.37162385426218,-1.23300285825706,
12.5770542771492));
#435246=CARTESIAN_POINT('Ctrl Pts',(-2.38186868662484,-1.22024170295216,
12.5737548217797));
#435247=CARTESIAN_POINT('',(-2.39213937462263,-1.19998227750568,12.5737548217797));
#435248=CARTESIAN_POINT('Origin',(-2.40604428726527,-1.20695747674301,12.5893111709658));
#435249=CARTESIAN_POINT('Ctrl Pts',(-2.38186868662484,-1.22024170295216,
12.5737548217797));
#435250=CARTESIAN_POINT('Ctrl Pts',(-2.38119336759526,-1.21950125454794,
12.5746934679442));
#435251=CARTESIAN_POINT('Ctrl Pts',(-2.38058142862772,-1.2185584575718,
12.5756680099006));
#435252=CARTESIAN_POINT('Ctrl Pts',(-2.38009969778665,-1.2175223885274,
12.5765688348656));
#435253=CARTESIAN_POINT('Ctrl Pts',(-2.37997216487942,-1.21724810071756,
12.5768073183026));
#435254=CARTESIAN_POINT('Ctrl Pts',(-2.37985355810775,-1.21696743763857,
12.5770407398754));
#435255=CARTESIAN_POINT('Ctrl Pts',(-2.37974460486843,-1.21668265643388,
12.5772674179684));
#435256=CARTESIAN_POINT('Ctrl Pts',(-2.37929749023645,-1.21551399137792,
12.5781976435658));
#435257=CARTESIAN_POINT('Ctrl Pts',(-2.37899808705842,-1.21420556666868,
12.5790594849312));
#435258=CARTESIAN_POINT('Ctrl Pts',(-2.37891368401597,-1.21283495773463,
12.5797571720116));
#435259=CARTESIAN_POINT('Ctrl Pts',(-2.37885869239895,-1.21194195673139,
12.580211740231));
#435260=CARTESIAN_POINT('Ctrl Pts',(-2.37891120643998,-1.21098082237251,
12.5806009430798));
#435261=CARTESIAN_POINT('Ctrl Pts',(-2.37908521968949,-1.21002018089239,
12.5808812374708));
#435262=CARTESIAN_POINT('Ctrl Pts',(-2.37923475479911,-1.20919467117148,
12.5811221033394));
#435263=CARTESIAN_POINT('Ctrl Pts',(-2.37947718481323,-1.20835264537558,
12.581287365893));
#435264=CARTESIAN_POINT('Ctrl Pts',(-2.37980683909001,-1.20754393569884,
12.581359338449));
#435265=CARTESIAN_POINT('Ctrl Pts',(-2.37985265422739,-1.20743154175299,
12.5813693411482));
#435266=CARTESIAN_POINT('Ctrl Pts',(-2.3799001093794,-1.20731975152665,
12.5813775999465));
#435267=CARTESIAN_POINT('Ctrl Pts',(-2.37994914421397,-1.2072086572213,
12.5813841266931));
#435268=CARTESIAN_POINT('Ctrl Pts',(-2.38003233774148,-1.20702017229568,
12.5813952001081));
#435269=CARTESIAN_POINT('Ctrl Pts',(-2.38012119263679,-1.20683267407251,
12.5814007534795));
#435270=CARTESIAN_POINT('Ctrl Pts',(-2.38021584841197,-1.20664632866722,
12.5814005856065));
#435271=CARTESIAN_POINT('Ctrl Pts',(-2.38064914554274,-1.20579331225815,
12.5813998171494));
#435272=CARTESIAN_POINT('Ctrl Pts',(-2.38117375882807,-1.20502323661152,
12.58127954464));
#435273=CARTESIAN_POINT('Ctrl Pts',(-2.38176225584241,-1.20432381444198,
12.5810700125799));
#435274=CARTESIAN_POINT('Ctrl Pts',(-2.38247309322999,-1.20347899209677,
12.5808169217085));
#435275=CARTESIAN_POINT('Ctrl Pts',(-2.38329000651475,-1.20274795102772,
12.5804173076348));
#435276=CARTESIAN_POINT('Ctrl Pts',(-2.38412403631904,-1.20217535199418,
12.5799304713245));
#435277=CARTESIAN_POINT('Ctrl Pts',(-2.38515766199304,-1.20146572140433,
12.5793271277669));
#435278=CARTESIAN_POINT('Ctrl Pts',(-2.3862634694477,-1.20092887628549,
12.5785808224116));
#435279=CARTESIAN_POINT('Ctrl Pts',(-2.3873809950077,-1.2005589134688,12.5777485681082));
#435280=CARTESIAN_POINT('Ctrl Pts',(-2.38904623052617,-1.20000762833946,
12.576508418016));
#435281=CARTESIAN_POINT('Ctrl Pts',(-2.39072130378142,-1.19982501097904,
12.5750928681475));
#435282=CARTESIAN_POINT('Ctrl Pts',(-2.39213937462263,-1.19998227750568,
12.5737548217797));
#435283=CARTESIAN_POINT('Ctrl Pts',(-2.39213937462263,-1.19998227750568,
12.5737548217797));
#435284=CARTESIAN_POINT('Ctrl Pts',(-2.39637714990393,-1.18417579353485,
12.5770542771492));
#435285=CARTESIAN_POINT('Ctrl Pts',(-2.40767974839161,-1.18501835034964,
12.5893111709658));
#435286=CARTESIAN_POINT('Ctrl Pts',(-2.41682620649634,-1.20187312023033,
12.5508408821982));
#435287=CARTESIAN_POINT('Ctrl Pts',(-2.42107400727543,-1.18601683084187,
12.55409748406));
#435288=CARTESIAN_POINT('Ctrl Pts',(-2.43239102498403,-1.18686046254337,
12.5663972313419));
#435289=CARTESIAN_POINT('Ctrl Pts',(-2.44148901252426,-1.20376093977156,
12.52790050457));
#435290=CARTESIAN_POINT('Ctrl Pts',(-2.44572356428675,-1.18785434212425,
12.5311362602938));
#435291=CARTESIAN_POINT('Ctrl Pts',(-2.45707737195896,-1.18870071634859,
12.5434568539655));
#435292=CARTESIAN_POINT('Ctrl Pts',(-2.46612966088055,-1.20564595726182,
12.5049357605811));
#435293=CARTESIAN_POINT('Ctrl Pts',(-2.47033075175862,-1.18968869495203,
12.5081700652078));
#435294=CARTESIAN_POINT('Ctrl Pts',(-2.48174074180913,-1.19053925731467,
12.5204921097672));
#435295=CARTESIAN_POINT('Ctrl Pts',(-2.46451165944216,-1.20552217804186,
12.5064436508395));
#435296=CARTESIAN_POINT('Ctrl Pts',(-2.46522638071389,-1.20453322845048,
12.5062361689309));
#435297=CARTESIAN_POINT('Ctrl Pts',(-2.46592746134174,-1.20347432450124,
12.5061871075061));
#435298=CARTESIAN_POINT('Ctrl Pts',(-2.4665473823338,-1.20241285636478,
12.5063648335164));
#435299=CARTESIAN_POINT('Ctrl Pts',(-2.4668289886867,-1.20193067206313,
12.5064455676329));
#435300=CARTESIAN_POINT('Ctrl Pts',(-2.46709758502746,-1.20144112205608,
12.506574497099));
#435301=CARTESIAN_POINT('Ctrl Pts',(-2.46734073337117,-1.20096469125585,
12.5067492519495));
#435302=CARTESIAN_POINT('Ctrl Pts',(-2.46782934940616,-1.20000728506915,
12.5071004286051));
#435303=CARTESIAN_POINT('Ctrl Pts',(-2.46823244497511,-1.1990672896786,
12.5076537929612));
#435304=CARTESIAN_POINT('Ctrl Pts',(-2.46852845852134,-1.19821898441121,
12.5083435010503));
#435305=CARTESIAN_POINT('Ctrl Pts',(-2.4685470943431,-1.19816557852503,
12.5083869222963));
#435306=CARTESIAN_POINT('Ctrl Pts',(-2.46856529651385,-1.19811252629235,
12.5084308732336));
#435307=CARTESIAN_POINT('Ctrl Pts',(-2.46858305617966,-1.19805984200306,
12.5084753333616));
#435308=CARTESIAN_POINT('Ctrl Pts',(-2.46872551213987,-1.1976372444668,
12.508831962269));
#435309=CARTESIAN_POINT('Ctrl Pts',(-2.46884361122113,-1.19723015365885,
12.509227847131));
#435310=CARTESIAN_POINT('Ctrl Pts',(-2.46893653089925,-1.1968514546545,
12.5096423454524));
#435311=CARTESIAN_POINT('Ctrl Pts',(-2.46922770004594,-1.19566477958005,
12.5109411997424));
#435312=CARTESIAN_POINT('Ctrl Pts',(-2.46929892690224,-1.19468620468532,
12.5124831113042));
#435313=CARTESIAN_POINT('Ctrl Pts',(-2.46923940374723,-1.19388409779126,
12.5140723025007));
#435314=CARTESIAN_POINT('Ctrl Pts',(-2.46923382636241,-1.19380893949676,
12.5142212114565));
#435315=CARTESIAN_POINT('Ctrl Pts',(-2.46922712365056,-1.19373531149787,
12.5143705582413));
#435316=CARTESIAN_POINT('Ctrl Pts',(-2.46921938291953,-1.1936631780583,
12.5145201959299));
#435317=CARTESIAN_POINT('Ctrl Pts',(-2.4691199417047,-1.19273651663152,
12.5164425148273));
#435318=CARTESIAN_POINT('Ctrl Pts',(-2.46885646354442,-1.19202360917721,
12.5184635205941));
#435319=CARTESIAN_POINT('Ctrl Pts',(-2.4684858865076,-1.19145448402352,
12.5205025929158));
#435320=CARTESIAN_POINT('Ctrl Pts',(-2.46827093713793,-1.19112436887637,
12.5216853356836));
#435321=CARTESIAN_POINT('Ctrl Pts',(-2.46802074829123,-1.19084296117297,
12.5228750347131));
#435322=CARTESIAN_POINT('Ctrl Pts',(-2.4677508018162,-1.19060060451602,
12.5240609649613));
#435323=CARTESIAN_POINT('Ctrl Pts',(-2.46708823267535,-1.19000575310353,
12.5269717671327));
#435324=CARTESIAN_POINT('Ctrl Pts',(-2.46628104518835,-1.18963715121935,
12.5299036066169));
#435325=CARTESIAN_POINT('Ctrl Pts',(-2.46537744179204,-1.18942278464467,
12.532813300402));
#435326=CARTESIAN_POINT('Ctrl Pts',(-2.46494365954657,-1.18931987620664,
12.5342101228452));
#435327=CARTESIAN_POINT('Ctrl Pts',(-2.46448807795016,-1.18925315053182,
12.5356023438239));
#435328=CARTESIAN_POINT('Ctrl Pts',(-2.46401737086258,-1.1892180613978,
12.5369868989719));
#435329=CARTESIAN_POINT('Origin',(-15.1745209143218,-2.13141609154649,-1.24009674915699));
#435330=CARTESIAN_POINT('Ctrl Pts',(-2.41564469525815,-1.28455013392597,
12.5369868989719));
#435331=CARTESIAN_POINT('Ctrl Pts',(-2.42562807883452,-1.29619553456537,
12.5369868989719));
#435332=CARTESIAN_POINT('Ctrl Pts',(-2.41815312981779,-1.30958987818059,
12.5369868989719));
#435333=CARTESIAN_POINT('Ctrl Pts',(-2.41901941908637,-1.28848677788516,
12.5218025310015));
#435334=CARTESIAN_POINT('Ctrl Pts',(-2.42388386633006,-1.29925678330379,
12.5216901060418));
#435335=CARTESIAN_POINT('Ctrl Pts',(-2.41817593034064,-1.30954905581901,
12.5161920673677));
#435336=CARTESIAN_POINT('Ctrl Pts',(-2.42502514348139,-1.287969723066,12.5042015548895));
#435337=CARTESIAN_POINT('Ctrl Pts',(-2.42653757490369,-1.29422191437866,
12.4980677368513));
#435338=CARTESIAN_POINT('Ctrl Pts',(-2.42333376503328,-1.30021577640893,
12.4907278922778));
#435339=CARTESIAN_POINT('Ctrl Pts',(-2.42909742081894,-1.27533423605555,
12.506463626192));
#435340=CARTESIAN_POINT('Ctrl Pts',(-2.43489029151153,-1.27837563170151,
12.4999376786891));
#435341=CARTESIAN_POINT('Ctrl Pts',(-2.43481954001884,-1.27833848547588,
12.4906970594712));
#435342=CARTESIAN_POINT('Origin',(-2.39894219218699,-1.2988688765788,12.5369868989719));
#435343=CARTESIAN_POINT('Origin',(-2.39894219218699,-1.2988688765788,14.));
#435344=CARTESIAN_POINT('Origin',(-2.39894219218699,-1.2988688765788,13.7435492065112));
#435345=CARTESIAN_POINT('Ctrl Pts',(-2.39959242500563,-1.26575334017198,
13.793642941384));
#435346=CARTESIAN_POINT('Ctrl Pts',(-2.40663471424226,-1.27395775247959,
13.8071662555867));
#435347=CARTESIAN_POINT('Ctrl Pts',(-2.39548357376296,-1.28682909466469,
13.8103758687955));
#435348=CARTESIAN_POINT('Ctrl Pts',(-2.41038632490764,-1.2783927005248,
13.7804579775006));
#435349=CARTESIAN_POINT('Ctrl Pts',(-2.41906817843885,-1.288522808668,13.7901904343352));
#435350=CARTESIAN_POINT('Ctrl Pts',(-2.41081379938462,-1.30194373078957,
13.7927914348263));
#435351=CARTESIAN_POINT('Ctrl Pts',(-2.41674109997117,-1.28583396766183,
13.7597120340895));
#435352=CARTESIAN_POINT('Ctrl Pts',(-2.42678409840478,-1.2975610846321,
13.7635825532444));
#435353=CARTESIAN_POINT('Ctrl Pts',(-2.41983606899175,-1.31087501731256,
13.7651073818884));
#435354=CARTESIAN_POINT('Ctrl Pts',(-2.41549668950532,-1.2843767971713,
13.7381884353898));
#435355=CARTESIAN_POINT('Ctrl Pts',(-2.42530529554721,-1.29582883446347,
13.7368803041982));
#435356=CARTESIAN_POINT('Ctrl Pts',(-2.41806889280862,-1.30912635725999,
13.7363986145813));
#435357=CARTESIAN_POINT('Origin',(-2.38548189084311,-1.28310722765482,13.7902182540695));
#435358=CARTESIAN_POINT('Ctrl Pts',(-2.37898166672864,-1.24161865887779,
13.8235227101244));
#435359=CARTESIAN_POINT('Ctrl Pts',(-2.38645133417696,-1.25035861062428,
13.8358800583119));
#435360=CARTESIAN_POINT('Ctrl Pts',(-2.3759902895674,-1.26321133775643,
13.8390832900376));
#435361=CARTESIAN_POINT('Ctrl Pts',(-2.38672753783373,-1.25068886450489,
13.8124254819052));
#435362=CARTESIAN_POINT('Ctrl Pts',(-2.3942117110589,-1.25944578929451,
13.8247886449157));
#435363=CARTESIAN_POINT('Ctrl Pts',(-2.38372422933846,-1.27230399711153,
13.8279860620657));
#435364=CARTESIAN_POINT('Ctrl Pts',(-2.3944699374914,-1.25975500516089,
13.8013225099955));
#435365=CARTESIAN_POINT('Ctrl Pts',(-2.40196508668937,-1.26852476982893,
13.8136962257787));
#435366=CARTESIAN_POINT('Ctrl Pts',(-2.39145479514605,-1.28139227139512,
13.8168830918626));
#435367=CARTESIAN_POINT('Ctrl Pts',(-2.40220900077034,-1.26881723900759,
13.7902140179785));
#435368=CARTESIAN_POINT('Ctrl Pts',(-2.40971182683348,-1.27759598052393,
13.802602731458));
#435369=CARTESIAN_POINT('Ctrl Pts',(-2.3991821209632,-1.29047633171505,
13.8057746032558));
#435370=CARTESIAN_POINT('Origin',(-2.36225454870613,-1.2559086380507,13.8235269408515));
#435371=CARTESIAN_POINT('Ctrl Pts',(-2.40767974839161,-1.18501835034964,
13.8235269408515));
#435372=CARTESIAN_POINT('Ctrl Pts',(-2.41945455877684,-1.18589610839295,
13.8362179249168));
#435373=CARTESIAN_POINT('Ctrl Pts',(-2.42346203985331,-1.16929481026663,
13.8391868794938));
#435374=CARTESIAN_POINT('Ctrl Pts',(-2.39690630941608,-1.18421523994654,
13.8400110824519));
#435375=CARTESIAN_POINT('Ctrl Pts',(-2.4066011409968,-1.18150745423075,
13.8494522556836));
#435376=CARTESIAN_POINT('Ctrl Pts',(-2.40572364821714,-1.16808516329897,
13.85569149686));
#435377=CARTESIAN_POINT('Ctrl Pts',(-2.38158820674563,-1.18976081986413,
13.8586819406588));
#435378=CARTESIAN_POINT('Ctrl Pts',(-2.38356929223266,-1.18588379214588,
13.868010383617));
#435379=CARTESIAN_POINT('Ctrl Pts',(-2.38034499272449,-1.17742821650172,
13.8744918421245));
#435380=CARTESIAN_POINT('Ctrl Pts',(-2.36739269353459,-1.21764556305143,
13.8587686893867));
#435381=CARTESIAN_POINT('Ctrl Pts',(-2.36542918954836,-1.22148805963776,
13.8680909899357));
#435382=CARTESIAN_POINT('Ctrl Pts',(-2.35671592487156,-1.22384929240428,
13.8745789365163));
#435383=CARTESIAN_POINT('Ctrl Pts',(-2.3719570320787,-1.23339300048152,
13.8400379222776));
#435384=CARTESIAN_POINT('Ctrl Pts',(-2.37549572759296,-1.24281360916491,
13.8494748685453));
#435385=CARTESIAN_POINT('Ctrl Pts',(-2.36415631094658,-1.25003709415377,
13.8557104837033));
#435386=CARTESIAN_POINT('Ctrl Pts',(-2.37898422350124,-1.24162165163091,
13.8235269408542));
#435387=CARTESIAN_POINT('Ctrl Pts',(-2.38665210202572,-1.25060053005331,
13.8362179249195));
#435388=CARTESIAN_POINT('Ctrl Pts',(-2.37563004038121,-1.26364572691502,
13.8391868794965));
#435389=CARTESIAN_POINT('Origin',(-2.40931520951794,-1.16307922395627,13.8235269408515));
#435390=CARTESIAN_POINT('Ctrl Pts',(-2.44334377189279,-1.18767693876742,
13.7902140241683));
#435391=CARTESIAN_POINT('Ctrl Pts',(-2.45485958593386,-1.18853985380613,
13.8026027327198));
#435392=CARTESIAN_POINT('Ctrl Pts',(-2.45902512104747,-1.17243313938355,
13.8057746032556));
#435393=CARTESIAN_POINT('Ctrl Pts',(-2.43145965004371,-1.18679103205752,
13.8013225161808));
#435394=CARTESIAN_POINT('Ctrl Pts',(-2.44296368560333,-1.18765306090166,
13.8136962270464));
#435395=CARTESIAN_POINT('Ctrl Pts',(-2.44713033149648,-1.17156960146924,
13.8168830918628));
#435396=CARTESIAN_POINT('Ctrl Pts',(-2.41957040484278,-1.18590474342528,
13.8124254880875));
#435397=CARTESIAN_POINT('Ctrl Pts',(-2.4310575959182,-1.1867655083394,13.8247886461867));
#435398=CARTESIAN_POINT('Ctrl Pts',(-2.435230227815,-1.17070594093389,13.8279860620656));
#435399=CARTESIAN_POINT('Ctrl Pts',(-2.40767582887667,-1.18501805740899,
13.8235227163066));
#435400=CARTESIAN_POINT('Ctrl Pts',(-2.41914075521139,-1.18587715424653,
13.8358800595848));
#435401=CARTESIAN_POINT('Ctrl Pts',(-2.42332459279511,-1.16984215085174,
13.8390832900376));
#435402=CARTESIAN_POINT('Origin',(-2.44498316494276,-1.16573810624297,13.7902182540695));
#435403=CARTESIAN_POINT('Ctrl Pts',(-2.46374825970872,-1.18919797273606,
13.7382347919292));
#435404=CARTESIAN_POINT('Ctrl Pts',(-2.47879502553553,-1.19034370694901,
13.7369371795942));
#435405=CARTESIAN_POINT('Ctrl Pts',(-2.48524114912593,-1.17663271618693,
13.7364597369712));
#435406=CARTESIAN_POINT('Ctrl Pts',(-2.46563458438239,-1.18933858998161,
13.7595490285574));
#435407=CARTESIAN_POINT('Ctrl Pts',(-2.48104042948073,-1.1905106579082,
13.7633824266926));
#435408=CARTESIAN_POINT('Ctrl Pts',(-2.4876660489628,-1.17702011207837,
13.7648920890506));
#435409=CARTESIAN_POINT('Ctrl Pts',(-2.45601443188735,-1.18862144974088,
13.780380659011));
#435410=CARTESIAN_POINT('Ctrl Pts',(-2.46933952696129,-1.18964062944777,
13.7901039518744));
#435411=CARTESIAN_POINT('Ctrl Pts',(-2.47530305907691,-1.17504879179339,
13.7926933640892));
#435412=CARTESIAN_POINT('Ctrl Pts',(-2.43929245936862,-1.18737489983978,
13.7936647693663));
#435413=CARTESIAN_POINT('Ctrl Pts',(-2.45007568467906,-1.18820879662543,
13.8072068914933));
#435414=CARTESIAN_POINT('Ctrl Pts',(-2.45386042659752,-1.17158592086766,
13.8104111085397));
#435415=CARTESIAN_POINT('Origin',(-2.46565283198891,-1.16727893500443,13.7435492065112));
#435416=CARTESIAN_POINT('Origin',(-2.46565283198891,-1.16727893500443,14.));
#435417=CARTESIAN_POINT('Origin',(-2.46565283198891,-1.16727893500443,12.5369868989719));
#435418=CARTESIAN_POINT('Ctrl Pts',(-2.46449514594364,-1.20551410043333,
12.506462012331));
#435419=CARTESIAN_POINT('Ctrl Pts',(-2.47036873119268,-1.20838717967208,
12.4999388158272));
#435420=CARTESIAN_POINT('Ctrl Pts',(-2.47029923897645,-1.20835318737687,
12.4907030323752));
#435421=CARTESIAN_POINT('Ctrl Pts',(-2.47227817897883,-1.19475989288802,
12.5042014951932));
#435422=CARTESIAN_POINT('Ctrl Pts',(-2.47821300834767,-1.19228625235656,
12.4980716682127));
#435423=CARTESIAN_POINT('Ctrl Pts',(-2.48115335619857,-1.18616416776537,
12.4907355092744));
#435424=CARTESIAN_POINT('Ctrl Pts',(-2.46914782498458,-1.18960949629008,
12.5218047446509));
#435425=CARTESIAN_POINT('Ctrl Pts',(-2.4807044199116,-1.18716736921946,
12.5216906929434));
#435426=CARTESIAN_POINT('Ctrl Pts',(-2.48563332013081,-1.17648669990714,
12.5161988840775));
#435427=CARTESIAN_POINT('Ctrl Pts',(-2.46397906354022,-1.18921517212888,
12.5369868989719));
#435428=CARTESIAN_POINT('Ctrl Pts',(-2.47926452286165,-1.19038147605744,
12.5369868989719));
#435429=CARTESIAN_POINT('Ctrl Pts',(-2.48565207386886,-1.1764457405673,
12.5369868989719));
#435430=CARTESIAN_POINT('Origin',(-4.59510497263915E-31,-7.48139013969503E-31,
12.5));
#435431=CARTESIAN_POINT('Origin',(-2.30307839592131,-1.37732355084816,12.5));
#435432=CARTESIAN_POINT('',(-2.30307839592131,-1.37732355084816,12.5893111709658));
#435433=CARTESIAN_POINT('',(-2.30307839592131,-1.37732355084816,13.8235269408515));
#435434=CARTESIAN_POINT('',(-2.30307839592131,-1.37732355084816,12.5));
#435435=CARTESIAN_POINT('',(-2.33841094557663,-1.38288085541566,13.7902182540695));
#435436=CARTESIAN_POINT('',(-2.30307839592131,-1.37732355084816,13.8235269408515));
#435437=CARTESIAN_POINT('',(-2.35888624416239,-1.38610132694861,13.7435492065112));
#435438=CARTESIAN_POINT('Origin',(-2.29152273184205,-1.3755063399721,13.7445212918693));
#435439=CARTESIAN_POINT('',(-2.35888624416239,-1.38610132694861,12.5369868989719));
#435440=CARTESIAN_POINT('',(-2.35888624416239,-1.38610132694861,12.5));
#435441=CARTESIAN_POINT('Ctrl Pts',(-2.35888624416239,-1.38610132694861,
12.5369868989719));
#435442=CARTESIAN_POINT('Ctrl Pts',(-2.34029719569876,-1.3831775355738,
12.5544431401645));
#435443=CARTESIAN_POINT('Ctrl Pts',(-2.32169485185361,-1.38025165302568,
12.5718848856037));
#435444=CARTESIAN_POINT('Ctrl Pts',(-2.30307839592131,-1.37732355084816,
12.5893111709658));
#435445=CARTESIAN_POINT('Origin',(-2.43081245659811,-1.65438118532145,12.5));
#435446=CARTESIAN_POINT('',(-2.30292856860467,-1.47720723304881,13.7435492065112));
#435447=CARTESIAN_POINT('',(-2.29079777601442,-1.46040089019251,13.7902182540695));
#435448=CARTESIAN_POINT('Origin',(-2.2589201497101,-1.41623672588671,13.7418732680448));
#435449=CARTESIAN_POINT('',(-2.26986465849441,-1.43139955763529,13.8235269408515));
#435450=CARTESIAN_POINT('',(-2.29079777601442,-1.46040089019251,13.7902182540695));
#435451=CARTESIAN_POINT('',(-2.26986465849441,-1.43139955763529,12.5893111709658));
#435452=CARTESIAN_POINT('',(-2.26986465849441,-1.43139955763529,12.5));
#435453=CARTESIAN_POINT('',(-2.30292856860467,-1.47720723304881,12.5369868989719));
#435454=CARTESIAN_POINT('Ctrl Pts',(-2.26986465849441,-1.43139955763529,
12.5893111709658));
#435455=CARTESIAN_POINT('Ctrl Pts',(-2.28089416142127,-1.4466801426708,
12.5718848856037));
#435456=CARTESIAN_POINT('Ctrl Pts',(-2.29191530350293,-1.46194914435509,
12.5544431401645));
#435457=CARTESIAN_POINT('Ctrl Pts',(-2.30292856860467,-1.47720723304881,
12.5369868989719));
#435458=CARTESIAN_POINT('',(-2.30292856860467,-1.47720723304881,12.5));
#435459=CARTESIAN_POINT('Origin',(-2.29773736195518,-1.41128108287233,12.5));
#435460=CARTESIAN_POINT('',(-2.26904829064012,-1.39234626417087,13.8587068136939));
#435461=CARTESIAN_POINT('Ctrl Pts',(-2.26986465848896,-1.43139955763904,
13.8235269408542));
#435462=CARTESIAN_POINT('Ctrl Pts',(-2.26883910009855,-1.42997872006389,
13.8262006681044));
#435463=CARTESIAN_POINT('Ctrl Pts',(-2.26793046612463,-1.42842301690021,
13.8288634856214));
#435464=CARTESIAN_POINT('Ctrl Pts',(-2.26713117782905,-1.42674341941851,
13.8314912288862));
#435465=CARTESIAN_POINT('Ctrl Pts',(-2.26630719403907,-1.42501192765731,
13.8342001611531));
#435466=CARTESIAN_POINT('Ctrl Pts',(-2.26559805327254,-1.42314705767076,
13.8368750301949));
#435467=CARTESIAN_POINT('Ctrl Pts',(-2.2650237406228,-1.42112557452759,
13.8394886372969));
#435468=CARTESIAN_POINT('Ctrl Pts',(-2.26497938506377,-1.42096945048101,
13.8396904925131));
#435469=CARTESIAN_POINT('Ctrl Pts',(-2.26493585367766,-1.4208123826277,
13.8398919674349));
#435470=CARTESIAN_POINT('Ctrl Pts',(-2.26489316637337,-1.42065435621056,
13.8400930404591));
#435471=CARTESIAN_POINT('Ctrl Pts',(-2.26422806945392,-1.41819219831672,
13.8432258934518));
#435472=CARTESIAN_POINT('Ctrl Pts',(-2.26377018679952,-1.41551019899573,
13.8462331177034));
#435473=CARTESIAN_POINT('Ctrl Pts',(-2.26362954253635,-1.4126795963753,
13.8489036603661));
#435474=CARTESIAN_POINT('Ctrl Pts',(-2.26358352209669,-1.41175339025651,
13.8497774930041));
#435475=CARTESIAN_POINT('Ctrl Pts',(-2.26357161468127,-1.41081147561601,
13.85061494757));
#435476=CARTESIAN_POINT('Ctrl Pts',(-2.26359808531297,-1.40985693225332,
13.8514076489583));
#435477=CARTESIAN_POINT('Ctrl Pts',(-2.26365407451668,-1.40783793537547,
13.8530843267192));
#435478=CARTESIAN_POINT('Ctrl Pts',(-2.2638902171936,-1.40556420303781,
13.8546805203176));
#435479=CARTESIAN_POINT('Ctrl Pts',(-2.26442852344596,-1.40318179685575,
13.8559412814274));
#435480=CARTESIAN_POINT('Ctrl Pts',(-2.26450056628021,-1.40286295364535,
13.8561100121513));
#435481=CARTESIAN_POINT('Ctrl Pts',(-2.26457795315569,-1.40254219962042,
13.8562727473908));
#435482=CARTESIAN_POINT('Ctrl Pts',(-2.26466090548036,-1.40221991142402,
13.8564289040185));
#435483=CARTESIAN_POINT('Ctrl Pts',(-2.26503709332639,-1.40075833813004,
13.8571370725437));
#435484=CARTESIAN_POINT('Ctrl Pts',(-2.26553655778373,-1.39924008993045,
13.8577210840553));
#435485=CARTESIAN_POINT('Ctrl Pts',(-2.26616776282059,-1.39773335262434,
13.8581177131616));
#435486=CARTESIAN_POINT('Ctrl Pts',(-2.26634553188439,-1.39730900353862,
13.8582294175695));
#435487=CARTESIAN_POINT('Ctrl Pts',(-2.26653357625172,-1.39688553227183,
13.8583265086086));
#435488=CARTESIAN_POINT('Ctrl Pts',(-2.26673166010008,-1.39646434932072,
13.8584082369006));
#435489=CARTESIAN_POINT('Ctrl Pts',(-2.26701625347188,-1.39585922236464,
13.8585256585398));
#435490=CARTESIAN_POINT('Ctrl Pts',(-2.26732540109047,-1.39525143340397,
13.8586122832068));
#435491=CARTESIAN_POINT('Ctrl Pts',(-2.26765177606403,-1.39465712905159,
13.8586682984299));
#435492=CARTESIAN_POINT('Ctrl Pts',(-2.26791284369037,-1.39418174448118,
13.8587131050557));
#435493=CARTESIAN_POINT('Ctrl Pts',(-2.26818761205666,-1.39370962442479,
13.8587357943552));
#435494=CARTESIAN_POINT('Ctrl Pts',(-2.26847655152625,-1.39324096752567,
13.8587355499465));
#435495=CARTESIAN_POINT('Ctrl Pts',(-2.26866329999401,-1.39293806339859,
13.8587353919793));
#435496=CARTESIAN_POINT('Ctrl Pts',(-2.2688539158289,-1.39263986122106,
13.8587257282814));
#435497=CARTESIAN_POINT('Ctrl Pts',(-2.26904829064012,-1.39234626417087,
13.8587068136939));
#435498=CARTESIAN_POINT('Ctrl Pts',(-2.26904829064012,-1.39234626417087,
13.8587068136939));
#435499=CARTESIAN_POINT('Ctrl Pts',(-2.26968757879808,-1.39138063947788,
13.8586446046467));
#435500=CARTESIAN_POINT('Ctrl Pts',(-2.27036747870724,-1.39046476713949,
13.858482427929));
#435501=CARTESIAN_POINT('Ctrl Pts',(-2.27108459173413,-1.38959574280588,
13.8582284286032));
#435502=CARTESIAN_POINT('Ctrl Pts',(-2.27182026628162,-1.38870422492876,
13.8579678548414));
#435503=CARTESIAN_POINT('Ctrl Pts',(-2.27259808371754,-1.38786080875602,
13.857615680862));
#435504=CARTESIAN_POINT('Ctrl Pts',(-2.2733802561323,-1.38709217632039,
13.8571944833187));
#435505=CARTESIAN_POINT('Ctrl Pts',(-2.27533224738737,-1.38517397546801,
13.8561433417727));
#435506=CARTESIAN_POINT('Ctrl Pts',(-2.2773993084917,-1.38362838224901,
13.8546163505474));
#435507=CARTESIAN_POINT('Ctrl Pts',(-2.27937927813542,-1.38241193781571,
13.8528973491086));
#435508=CARTESIAN_POINT('Ctrl Pts',(-2.2797409893776,-1.3821897113647,13.8525833129072));
#435509=CARTESIAN_POINT('Ctrl Pts',(-2.28009978404843,-1.38197832891922,
13.8522628768812));
#435510=CARTESIAN_POINT('Ctrl Pts',(-2.28045444496735,-1.38177734736348,
13.851937733538));
#435511=CARTESIAN_POINT('Ctrl Pts',(-2.28262030999228,-1.38054998088751,
13.8499521282529));
#435512=CARTESIAN_POINT('Ctrl Pts',(-2.28484926881114,-1.37959207364114,
13.847639871647));
#435513=CARTESIAN_POINT('Ctrl Pts',(-2.2869924540174,-1.37888015661756,
13.8452109780794));
#435514=CARTESIAN_POINT('Ctrl Pts',(-2.28795671740343,-1.3785598504127,
13.8441181685877));
#435515=CARTESIAN_POINT('Ctrl Pts',(-2.28890364102382,-1.37828862227948,
13.8430021611332));
#435516=CARTESIAN_POINT('Ctrl Pts',(-2.2898207919598,-1.3780612232801,13.8418824960098));
#435517=CARTESIAN_POINT('Ctrl Pts',(-2.29198208156072,-1.37752535173122,
13.8392439765549));
#435518=CARTESIAN_POINT('Ctrl Pts',(-2.29408044570721,-1.37720358462492,
13.8364981347964));
#435519=CARTESIAN_POINT('Ctrl Pts',(-2.29611624695142,-1.3770612458496,
13.8336931113419));
#435520=CARTESIAN_POINT('Ctrl Pts',(-2.29809898807794,-1.37692261692179,
13.8309611966328));
#435521=CARTESIAN_POINT('Ctrl Pts',(-2.30002441125895,-1.3769546092808,
13.8281701127186));
#435522=CARTESIAN_POINT('Ctrl Pts',(-2.30188114175763,-1.37716270309375,
13.8253580685121));
#435523=CARTESIAN_POINT('Ctrl Pts',(-2.30228368293359,-1.37720781805697,
13.8247484142933));
#435524=CARTESIAN_POINT('Ctrl Pts',(-2.30268288340781,-1.37726134238827,
13.8241378483365));
#435525=CARTESIAN_POINT('Ctrl Pts',(-2.30307839592131,-1.37732355084816,
13.8235269408515));
#435526=CARTESIAN_POINT('',(-2.26838290138995,-1.39339508922901,12.5969504640361));
#435527=CARTESIAN_POINT('Origin',(-2.29776565673724,-1.41129823186991,12.584524458991));
#435528=CARTESIAN_POINT('Origin',(-2.29776565673724,-1.41129823186991,12.584524458991));
#435529=CARTESIAN_POINT('Ctrl Pts',(-2.26986465849441,-1.43139955763529,
12.5893111709658));
#435530=CARTESIAN_POINT('Ctrl Pts',(-2.26323129194435,-1.42220950416579,
12.5770542771492));
#435531=CARTESIAN_POINT('Ctrl Pts',(-2.2744821880986,-1.41032585949838,
12.5737548217797));
#435532=CARTESIAN_POINT('Ctrl Pts',(-2.28436960491541,-1.45149512029947,
12.5663937883685));
#435533=CARTESIAN_POINT('Ctrl Pts',(-2.27772777658511,-1.44229334364049,
12.5540940315304));
#435534=CARTESIAN_POINT('Ctrl Pts',(-2.28901586886885,-1.43037508169057,
12.5508374392248));
#435535=CARTESIAN_POINT('Ctrl Pts',(-2.29885991602329,-1.47157040678728,
12.5434499600945));
#435536=CARTESIAN_POINT('Ctrl Pts',(-2.29219649274381,-1.46233871187557,
12.5311293540533));
#435537=CARTESIAN_POINT('Ctrl Pts',(-2.30353439464537,-1.45040540784716,
12.5278936106989));
#435538=CARTESIAN_POINT('Ctrl Pts',(-2.31333673822216,-1.49162700535937,
12.5204817579905));
#435539=CARTESIAN_POINT('Ctrl Pts',(-2.3066403355513,-1.48234961986679,
12.5081597038247));
#435540=CARTESIAN_POINT('Ctrl Pts',(-2.31803893211648,-1.47041831477309,
12.5049254088044));
#435541=CARTESIAN_POINT('Ctrl Pts',(-2.30292856860467,-1.47720723304881,
12.5369868989719));
#435542=CARTESIAN_POINT('Ctrl Pts',(-2.30347374562544,-1.4779625364228,
12.5342545179733));
#435543=CARTESIAN_POINT('Ctrl Pts',(-2.30409518707979,-1.47861035401455,
12.5314872231885));
#435544=CARTESIAN_POINT('Ctrl Pts',(-2.30479822681678,-1.47907549510966,
12.5287124745062));
#435545=CARTESIAN_POINT('Ctrl Pts',(-2.30543226294736,-1.47949498243676,
12.5262100684184));
#435546=CARTESIAN_POINT('Ctrl Pts',(-2.30613256864847,-1.47976464938453,
12.5237004536639));
#435547=CARTESIAN_POINT('Ctrl Pts',(-2.30693498999869,-1.47982726366503,
12.5212220730815));
#435548=CARTESIAN_POINT('Ctrl Pts',(-2.30754931295728,-1.47987520031331,
12.5193246583486));
#435549=CARTESIAN_POINT('Ctrl Pts',(-2.30823087961677,-1.47980171894315,
12.517417831369));
#435550=CARTESIAN_POINT('Ctrl Pts',(-2.30898854715649,-1.47950999201131,
12.5155812248348));
#435551=CARTESIAN_POINT('Ctrl Pts',(-2.30931131760089,-1.4793857147703,
12.5147988205793));
#435552=CARTESIAN_POINT('Ctrl Pts',(-2.30964832607415,-1.47922196256213,
12.5140295443047));
#435553=CARTESIAN_POINT('Ctrl Pts',(-2.31000200775598,-1.47901245833598,
12.5132817086137));
#435554=CARTESIAN_POINT('Ctrl Pts',(-2.31053725713645,-1.4786954020308,
12.5121499604604));
#435555=CARTESIAN_POINT('Ctrl Pts',(-2.31111860616464,-1.47826056134241,
12.5110494206568));
#435556=CARTESIAN_POINT('Ctrl Pts',(-2.31173453076288,-1.47767252307581,
12.5100666561695));
#435557=CARTESIAN_POINT('Ctrl Pts',(-2.31208819324883,-1.47733487285726,
12.5095023550641));
#435558=CARTESIAN_POINT('Ctrl Pts',(-2.31245689089972,-1.47694233957501,
12.5089719619137));
#435559=CARTESIAN_POINT('Ctrl Pts',(-2.3128290574779,-1.4764979081123,12.5085043804652));
#435560=CARTESIAN_POINT('Ctrl Pts',(-2.31337367478695,-1.4758475405579,
12.5078201359221));
#435561=CARTESIAN_POINT('Ctrl Pts',(-2.31394059035579,-1.47506639732494,
12.5072563000949));
#435562=CARTESIAN_POINT('Ctrl Pts',(-2.31448452395654,-1.47420245576189,
12.5068768744332));
#435563=CARTESIAN_POINT('Ctrl Pts',(-2.31487673752719,-1.47357949442099,
12.5066032824114));
#435564=CARTESIAN_POINT('Ctrl Pts',(-2.31526394327209,-1.47290257039882,
12.5064197834844));
#435565=CARTESIAN_POINT('Ctrl Pts',(-2.31562676234242,-1.47221076831766,
12.5063282718343));
#435566=CARTESIAN_POINT('Ctrl Pts',(-2.31615636585915,-1.47120095145569,
12.5061946931565));
#435567=CARTESIAN_POINT('Ctrl Pts',(-2.31664626910326,-1.47013834367698,
12.5062515701262));
#435568=CARTESIAN_POINT('Ctrl Pts',(-2.31708011165234,-1.4690953670419,
12.5064436508398));
#435569=CARTESIAN_POINT('',(-2.2744821880986,-1.41032585949838,12.5737548217797));
#435570=CARTESIAN_POINT('Origin',(-2.2877031887093,-1.41852373378699,12.5893111709658));
#435571=CARTESIAN_POINT('Ctrl Pts',(-2.31708011165234,-1.4690953670419,
12.5064436508398));
#435572=CARTESIAN_POINT('Ctrl Pts',(-2.31077490124847,-1.46039567109812,
12.5164271754438));
#435573=CARTESIAN_POINT('Ctrl Pts',(-2.30446702228504,-1.45169264920894,
12.5264061185523));
#435574=CARTESIAN_POINT('Ctrl Pts',(-2.29815638154398,-1.4429861836819,
12.536380305637));
#435575=CARTESIAN_POINT('Ctrl Pts',(-2.29026936055351,-1.43210486763459,
12.5488460165097));
#435576=CARTESIAN_POINT('Ctrl Pts',(-2.2823780233362,-1.42121816944895,
12.5613043021964));
#435577=CARTESIAN_POINT('Ctrl Pts',(-2.2744821880986,-1.41032585949838,
12.5737548217797));
#435578=CARTESIAN_POINT('Ctrl Pts',(-2.30307839592131,-1.37732355084815,
12.5893111709658));
#435579=CARTESIAN_POINT('Ctrl Pts',(-2.29188208210002,-1.37556253086672,
12.5770542771492));
#435580=CARTESIAN_POINT('Ctrl Pts',(-2.28637003248251,-1.39097100203906,
12.5737548217797));
#435581=CARTESIAN_POINT('Ctrl Pts',(-2.29263233250645,-1.37568053452202,
12.5928319619712));
#435582=CARTESIAN_POINT('Ctrl Pts',(-2.28460154450062,-1.37771519920616,
12.5821634970842));
#435583=CARTESIAN_POINT('Ctrl Pts',(-2.28256625099379,-1.39036316673619,
12.5773203894503));
#435584=CARTESIAN_POINT('Ctrl Pts',(-2.27650764618195,-1.38021689763316,
12.5969440695591));
#435585=CARTESIAN_POINT('Ctrl Pts',(-2.2743882779987,-1.38363257048866,
12.5878292599214));
#435586=CARTESIAN_POINT('Ctrl Pts',(-2.27681963783929,-1.3919819886381,
12.5813877129824));
#435587=CARTESIAN_POINT('Ctrl Pts',(-2.26044824178409,-1.40626052979013,
12.596957478804));
#435588=CARTESIAN_POINT('Ctrl Pts',(-2.26255201538024,-1.40287014193547,
12.5878468778671));
#435589=CARTESIAN_POINT('Ctrl Pts',(-2.27107683179591,-1.40130649650995,
12.5814011370086));
#435590=CARTESIAN_POINT('Ctrl Pts',(-2.26366679896377,-1.42281286789751,
12.5928371701607));
#435591=CARTESIAN_POINT('Ctrl Pts',(-2.26185749593652,-1.4147344096127,
12.5821692192952));
#435592=CARTESIAN_POINT('Ctrl Pts',(-2.27221263799302,-1.40719817348598,
12.5773318885715));
#435593=CARTESIAN_POINT('Ctrl Pts',(-2.26986465849436,-1.43139955763532,
12.5893111709658));
#435594=CARTESIAN_POINT('Ctrl Pts',(-2.2632312919443,-1.42220950416582,
12.5770542771492));
#435595=CARTESIAN_POINT('Ctrl Pts',(-2.27448218809855,-1.41032585949842,
12.5737548217797));
#435596=CARTESIAN_POINT('',(-2.28637003248251,-1.39097100203906,12.5737548217797));
#435597=CARTESIAN_POINT('Origin',(-2.29966013418298,-1.39905637134363,12.5893111709658));
#435598=CARTESIAN_POINT('Ctrl Pts',(-2.27448218809855,-1.41032585949842,
12.5737548217797));
#435599=CARTESIAN_POINT('Ctrl Pts',(-2.27386946955627,-1.40953283010492,
12.5746934679442));
#435600=CARTESIAN_POINT('Ctrl Pts',(-2.27333641347121,-1.40854329150111,
12.5756680099006));
#435601=CARTESIAN_POINT('Ctrl Pts',(-2.27294073479529,-1.40747140435528,
12.5765688348656));
#435602=CARTESIAN_POINT('Ctrl Pts',(-2.27283598324615,-1.4071876340996,
12.5768073183026));
#435603=CARTESIAN_POINT('Ctrl Pts',(-2.27274064777522,-1.40689823735086,
12.5770407398754));
#435604=CARTESIAN_POINT('Ctrl Pts',(-2.27265526938078,-1.40660552303166,
12.5772674179684));
#435605=CARTESIAN_POINT('Ctrl Pts',(-2.27230489953727,-1.40540430261896,
12.5781976435658));
#435606=CARTESIAN_POINT('Ctrl Pts',(-2.27211314135924,-1.40407582744646,
12.5790594849312));
#435607=CARTESIAN_POINT('Ctrl Pts',(-2.27214073651319,-1.40270289946905,
12.5797571720116));
#435608=CARTESIAN_POINT('Ctrl Pts',(-2.27215871574822,-1.40180838752568,
12.580211740231));
#435609=CARTESIAN_POINT('Ctrl Pts',(-2.2722893964261,-1.40085473164395,
12.5806009430798));
#435610=CARTESIAN_POINT('Ctrl Pts',(-2.27254113185966,-1.39991147031441,
12.5808812374708));
#435611=CARTESIAN_POINT('Ctrl Pts',(-2.27275745610945,-1.39910089590865,
12.5811221033394));
#435612=CARTESIAN_POINT('Ctrl Pts',(-2.27306771237705,-1.39828143218088,
12.581287365893));
#435613=CARTESIAN_POINT('Ctrl Pts',(-2.27346218710277,-1.3975022833028,
12.581359338449));
#435614=CARTESIAN_POINT('Ctrl Pts',(-2.27351701094406,-1.39739399769756,
12.5813693411482));
#435615=CARTESIAN_POINT('Ctrl Pts',(-2.27357342013422,-1.39728644747941,
12.5813775999465));
#435616=CARTESIAN_POINT('Ctrl Pts',(-2.27363134702667,-1.39717971962542,
12.5813841266931));
#435617=CARTESIAN_POINT('Ctrl Pts',(-2.27372962700582,-1.39699864291267,
12.5813952001081));
#435618=CARTESIAN_POINT('Ctrl Pts',(-2.27383346908963,-1.39681901107323,
12.5814007534795));
#435619=CARTESIAN_POINT('Ctrl Pts',(-2.27394299878601,-1.39664100104132,
12.5814005856065));
#435620=CARTESIAN_POINT('Ctrl Pts',(-2.27444438291267,-1.39582614071267,
12.5813998171494));
#435621=CARTESIAN_POINT('Ctrl Pts',(-2.27503001890481,-1.39510138828226,
12.58127954464));
#435622=CARTESIAN_POINT('Ctrl Pts',(-2.27567356714382,-1.3944522613523,
12.5810700125799));
#435623=CARTESIAN_POINT('Ctrl Pts',(-2.27645090014271,-1.39366818992993,
12.5808169217085));
#435624=CARTESIAN_POINT('Ctrl Pts',(-2.27732468184969,-1.39300616735629,
12.5804173076348));
#435625=CARTESIAN_POINT('Ctrl Pts',(-2.27820260862559,-1.39250345477061,
12.5799304713245));
#435626=CARTESIAN_POINT('Ctrl Pts',(-2.27929063647639,-1.39188043550615,
12.5793271277669));
#435627=CARTESIAN_POINT('Ctrl Pts',(-2.28043652230898,-1.39143551026852,
12.5785808224116));
#435628=CARTESIAN_POINT('Ctrl Pts',(-2.281580484799,-1.39115786718032,12.5777485681082));
#435629=CARTESIAN_POINT('Ctrl Pts',(-2.28328511423958,-1.39074414856083,
12.576508418016));
#435630=CARTESIAN_POINT('Ctrl Pts',(-2.28496949883696,-1.39069867286553,
12.5750928681475));
#435631=CARTESIAN_POINT('Ctrl Pts',(-2.28637003248251,-1.39097100203906,
12.5737548217797));
#435632=CARTESIAN_POINT('Ctrl Pts',(-2.28637003248251,-1.39097100203906,
12.5737548217797));
#435633=CARTESIAN_POINT('Ctrl Pts',(-2.29188208210002,-1.37556253086672,
12.5770542771492));
#435634=CARTESIAN_POINT('Ctrl Pts',(-2.30307839592131,-1.37732355084816,
12.5893111709658));
#435635=CARTESIAN_POINT('Ctrl Pts',(-2.3108205997239,-1.39486775911961,
12.5508408821982));
#435636=CARTESIAN_POINT('Ctrl Pts',(-2.31634670108406,-1.37941046542419,
12.55409748406));
#435637=CARTESIAN_POINT('Ctrl Pts',(-2.32755729853427,-1.3811737320161,
12.5663972313419));
#435638=CARTESIAN_POINT('Ctrl Pts',(-2.33524746748103,-1.39875954474662,
12.52790050457));
#435639=CARTESIAN_POINT('Ctrl Pts',(-2.34076446449977,-1.38325103027111,
12.5311362602938));
#435640=CARTESIAN_POINT('Ctrl Pts',(-2.35201150595693,-1.38502002898392,
12.5434568539655));
#435641=CARTESIAN_POINT('Ctrl Pts',(-2.35965247968752,-1.40264673159036,
12.5049357605811));
#435642=CARTESIAN_POINT('Ctrl Pts',(-2.36514025680051,-1.38708499366211,
12.5081700652078));
#435643=CARTESIAN_POINT('Ctrl Pts',(-2.37644295232159,-1.38886274596296,
12.5204921097672));
#435644=CARTESIAN_POINT('Ctrl Pts',(-2.35804995117097,-1.40239148209752,
12.5064436508395));
#435645=CARTESIAN_POINT('Ctrl Pts',(-2.3588429028393,-1.40146407957311,
12.5062361689309));
#435646=CARTESIAN_POINT('Ctrl Pts',(-2.35962796118144,-1.4004658436191,
12.5061871075061));
#435647=CARTESIAN_POINT('Ctrl Pts',(-2.36033233894485,-1.39945843674622,
12.5063648335164));
#435648=CARTESIAN_POINT('Ctrl Pts',(-2.36065231077281,-1.39900081040512,
12.5064455676329));
#435649=CARTESIAN_POINT('Ctrl Pts',(-2.36095991625174,-1.39853478243063,
12.506574497099));
#435650=CARTESIAN_POINT('Ctrl Pts',(-2.36124108907258,-1.39807975576188,
12.5067492519495));
#435651=CARTESIAN_POINT('Ctrl Pts',(-2.36180611677043,-1.39716536200812,
12.5071004286051));
#435652=CARTESIAN_POINT('Ctrl Pts',(-2.36228448942298,-1.39626135040563,
12.5076537929613));
#435653=CARTESIAN_POINT('Ctrl Pts',(-2.36264866276314,-1.39543999565603,
12.5083435010505));
#435654=CARTESIAN_POINT('Ctrl Pts',(-2.36267158965122,-1.39538828646611,
12.5083869222964));
#435655=CARTESIAN_POINT('Ctrl Pts',(-2.36269405550518,-1.39533689440635,
12.5084308732337));
#435656=CARTESIAN_POINT('Ctrl Pts',(-2.3627160503358,-1.39528583299742,
12.5084753333615));
#435657=CARTESIAN_POINT('Ctrl Pts',(-2.36289247790797,-1.39487625310285,
12.5088319622689));
#435658=CARTESIAN_POINT('Ctrl Pts',(-2.36304336570438,-1.39448014302746,
12.509227847131));
#435659=CARTESIAN_POINT('Ctrl Pts',(-2.36316684368446,-1.39411027792921,
12.5096423454524));
#435660=CARTESIAN_POINT('Ctrl Pts',(-2.36355376902495,-1.39295128440671,
12.5109411997424));
#435661=CARTESIAN_POINT('Ctrl Pts',(-2.36370452181833,-1.39198177128923,
12.5124831113042));
#435662=CARTESIAN_POINT('Ctrl Pts',(-2.36371057587997,-1.39117748164997,
12.5140723025008));
#435663=CARTESIAN_POINT('Ctrl Pts',(-2.36371114315218,-1.39110211882986,
12.5142212114565));
#435664=CARTESIAN_POINT('Ctrl Pts',(-2.36371046410849,-1.39102818948882,
12.5143705582413));
#435665=CARTESIAN_POINT('Ctrl Pts',(-2.36370862867909,-1.39095566512588,
12.5145201959299));
#435666=CARTESIAN_POINT('Ctrl Pts',(-2.36368504985568,-1.39002398170639,
12.5164425148273));
#435667=CARTESIAN_POINT('Ctrl Pts',(-2.36348055697308,-1.38929197047674,
12.5184635205941));
#435668=CARTESIAN_POINT('Ctrl Pts',(-2.3631576019843,-1.38869453357128,
12.5205025929158));
#435669=CARTESIAN_POINT('Ctrl Pts',(-2.36297027529006,-1.38834799648593,
12.5216853356836));
#435670=CARTESIAN_POINT('Ctrl Pts',(-2.3627438562664,-1.3880471324298,12.5228750347131));
#435671=CARTESIAN_POINT('Ctrl Pts',(-2.36249456233346,-1.38778357905086,
12.5240609649613));
#435672=CARTESIAN_POINT('Ctrl Pts',(-2.36188268374922,-1.3871367014214,
12.5269717671326));
#435673=CARTESIAN_POINT('Ctrl Pts',(-2.3611082265875,-1.38670353275584,
12.5299036066169));
#435674=CARTESIAN_POINT('Ctrl Pts',(-2.36022510272288,-1.38641622740281,
12.5328133004019));
#435675=CARTESIAN_POINT('Ctrl Pts',(-2.35980115184509,-1.38627830410407,
12.5342101228451));
#435676=CARTESIAN_POINT('Ctrl Pts',(-2.35935252492081,-1.38617466632391,
12.5356023438238));
#435677=CARTESIAN_POINT('Ctrl Pts',(-2.35888624416239,-1.38610132694861,
12.5369868989719));
#435678=CARTESIAN_POINT('Origin',(-14.9503750405813,-3.36120017670074,-1.24017999715448));
#435679=CARTESIAN_POINT('Ctrl Pts',(-2.30290407571476,-1.47717336773802,
12.5369868989719));
#435680=CARTESIAN_POINT('Ctrl Pts',(-2.3119050321431,-1.48959375771016,
12.5369868989719));
#435681=CARTESIAN_POINT('Ctrl Pts',(-2.30336319205093,-1.50233425501304,
12.5369868989719));
#435682=CARTESIAN_POINT('Ctrl Pts',(-2.30594669739915,-1.48137198416061,
12.5218025310015));
#435683=CARTESIAN_POINT('Ctrl Pts',(-2.30991710317046,-1.49250265088438,
12.5216901060417));
#435684=CARTESIAN_POINT('Ctrl Pts',(-2.30338924410837,-1.50229542693877,
12.5161920673678));
#435685=CARTESIAN_POINT('Ctrl Pts',(-2.31197458300952,-1.48134617209131,
12.5042015548895));
#435686=CARTESIAN_POINT('Ctrl Pts',(-2.31297237030655,-1.48770083695479,
12.4980677368514));
#435687=CARTESIAN_POINT('Ctrl Pts',(-2.30929066544941,-1.49341361465647,
12.4907278922777));
#435688=CARTESIAN_POINT('Ctrl Pts',(-2.31706321967367,-1.46908465702972,
12.506463626192));
#435689=CARTESIAN_POINT('Ctrl Pts',(-2.32258891308682,-1.4725881054224,
12.4999376786891));
#435690=CARTESIAN_POINT('Ctrl Pts',(-2.32252142477613,-1.47254531589429,
12.4906970594712));
#435691=CARTESIAN_POINT('Origin',(-2.28509003838978,-1.4900830568971,12.5369868989719));
#435692=CARTESIAN_POINT('Origin',(-2.28509003838978,-1.49008305689711,14.));
#435693=CARTESIAN_POINT('Origin',(-2.28509003838978,-1.49008305689711,13.7435492065112));
#435694=CARTESIAN_POINT('Ctrl Pts',(-2.28843733125914,-1.45713070971702,
13.793642941384));
#435695=CARTESIAN_POINT('Ctrl Pts',(-2.29478745209017,-1.46588183446972,
13.8071662555867));
#435696=CARTESIAN_POINT('Ctrl Pts',(-2.2826242822311,-1.47780142685429,
13.8103758687955));
#435697=CARTESIAN_POINT('Ctrl Pts',(-2.29816509014281,-1.47060781668864,
13.7804579775006));
#435698=CARTESIAN_POINT('Ctrl Pts',(-2.30599235766558,-1.48141186939382,
13.7901904343351));
#435699=CARTESIAN_POINT('Ctrl Pts',(-2.29667151463007,-1.49411532598138,
13.7927914348262));
#435700=CARTESIAN_POINT('Ctrl Pts',(-2.30389218786353,-1.47854229678566,
13.7597120340895));
#435701=CARTESIAN_POINT('Ctrl Pts',(-2.31294590014608,-1.49104899034863,
13.7635825532445));
#435702=CARTESIAN_POINT('Ctrl Pts',(-2.30493578061372,-1.50375229311687,
13.7651073818885));
#435703=CARTESIAN_POINT('Ctrl Pts',(-2.30277069099354,-1.47698854390422,
13.7381884353898));
#435704=CARTESIAN_POINT('Ctrl Pts',(-2.31161321235313,-1.4892019679381,
13.7368803041982));
#435705=CARTESIAN_POINT('Ctrl Pts',(-2.3033170165916,-1.50186541032181,
13.7363986145813));
#435706=CARTESIAN_POINT('Origin',(-2.27295924579953,-1.47327671404081,13.7902182540695));
#435707=CARTESIAN_POINT('Ctrl Pts',(-2.26986235416098,-1.43139636644336,
13.8235227101244));
#435708=CARTESIAN_POINT('Ctrl Pts',(-2.27659477970197,-1.44071608396346,
13.8358800583119));
#435709=CARTESIAN_POINT('Ctrl Pts',(-2.26512092677521,-1.45267337245507,
13.8390832900376));
#435710=CARTESIAN_POINT('Ctrl Pts',(-2.27684314555667,-1.44106775211369,
13.8124254819052));
#435711=CARTESIAN_POINT('Ctrl Pts',(-2.28358864514716,-1.45040556855599,
13.8247886449157));
#435712=CARTESIAN_POINT('Ctrl Pts',(-2.27208799635011,-1.46236616462598,
13.8279860620657));
#435713=CARTESIAN_POINT('Ctrl Pts',(-2.28382080838877,-1.45073480338359,
13.8013225099955));
#435714=CARTESIAN_POINT('Ctrl Pts',(-2.29057620086112,-1.46008631162437,
13.8136962257787));
#435715=CARTESIAN_POINT('Ctrl Pts',(-2.27905206061218,-1.47205431130703,
13.8168830918626));
#435716=CARTESIAN_POINT('Ctrl Pts',(-2.2907954643849,-1.46039768889795,
13.7902140179785));
#435717=CARTESIAN_POINT('Ctrl Pts',(-2.29755777648181,-1.46975876985307,
13.802602731458));
#435718=CARTESIAN_POINT('Ctrl Pts',(-2.28601323914175,-1.4817379939567,
13.8057746032558));
#435719=CARTESIAN_POINT('Origin',(-2.25202612827951,-1.44427538148359,13.8235269408515));
#435720=CARTESIAN_POINT('Ctrl Pts',(-2.30307839592131,-1.37732355084816,
13.8235269408515));
#435721=CARTESIAN_POINT('Ctrl Pts',(-2.31474248116712,-1.37915814458239,
13.8362179249168));
#435722=CARTESIAN_POINT('Ctrl Pts',(-2.32008978759712,-1.36293873281744,
13.8391868794938));
#435723=CARTESIAN_POINT('Ctrl Pts',(-2.2924062656288,-1.37564497743644,
13.8400110824519));
#435724=CARTESIAN_POINT('Ctrl Pts',(-2.3022895481309,-1.3737364204305,13.8494522556836));
#435725=CARTESIAN_POINT('Ctrl Pts',(-2.30250901645348,-1.36028726725673,
13.85569149686));
#435726=CARTESIAN_POINT('Ctrl Pts',(-2.27668711643539,-1.37992353732036,
13.8586819406588));
#435727=CARTESIAN_POINT('Ctrl Pts',(-2.27897762377551,-1.37622088695071,
13.868010383617));
#435728=CARTESIAN_POINT('Ctrl Pts',(-2.27645326077068,-1.36753063619411,
13.8744918421245));
#435729=CARTESIAN_POINT('Ctrl Pts',(-2.26026597218442,-1.40655843021363,
13.8587686893867));
#435730=CARTESIAN_POINT('Ctrl Pts',(-2.25799580245194,-1.41022809740638,
13.8680909899357));
#435731=CARTESIAN_POINT('Ctrl Pts',(-2.24911906805347,-1.4118712614045,
13.8745789365163));
#435732=CARTESIAN_POINT('Ctrl Pts',(-2.26353156092593,-1.42262550530934,
13.8400379222776));
#435733=CARTESIAN_POINT('Ctrl Pts',(-2.26629061465845,-1.43230320423053,
13.8494748685453));
#435734=CARTESIAN_POINT('Ctrl Pts',(-2.25440014789936,-1.43857838594228,
13.8557104837033));
#435735=CARTESIAN_POINT('Ctrl Pts',(-2.26986465848896,-1.43139955763904,
13.8235269408542));
#435736=CARTESIAN_POINT('Ctrl Pts',(-2.27677516083295,-1.44097356286906,
13.8362179249195));
#435737=CARTESIAN_POINT('Ctrl Pts',(-2.26472646953937,-1.45307695256651,
13.8391868794965));
#435738=CARTESIAN_POINT('Origin',(-2.30649665765963,-1.35559073035269,13.8235269408515));
#435739=CARTESIAN_POINT('Ctrl Pts',(-2.33840705068917,-1.38288024203628,
13.7902140241682));
#435740=CARTESIAN_POINT('Ctrl Pts',(-2.34981421122245,-1.38467893154836,
13.8026027327198));
#435741=CARTESIAN_POINT('Ctrl Pts',(-2.35527873261449,-1.36896534067199,
13.8057746032556));
#435742=CARTESIAN_POINT('Ctrl Pts',(-2.3266346818964,-1.38102861685037,
13.8013225161808));
#435743=CARTESIAN_POINT('Ctrl Pts',(-2.33803017537325,-1.38282546306104,
13.8136962270464));
#435744=CARTESIAN_POINT('Ctrl Pts',(-2.3434939083512,-1.3671351403346,13.8168830918628));
#435745=CARTESIAN_POINT('Ctrl Pts',(-2.31485723792953,-1.3791761934122,
13.8124254880875));
#435746=CARTESIAN_POINT('Ctrl Pts',(-2.32623604599283,-1.38097040691662,
13.8247886461868));
#435747=CARTESIAN_POINT('Ctrl Pts',(-2.33170379763449,-1.36530438463322,
13.8279860620656));
#435748=CARTESIAN_POINT('Ctrl Pts',(-2.3030745133256,-1.37732293940539,
13.8235227163065));
#435749=CARTESIAN_POINT('Ctrl Pts',(-2.31443126669601,-1.37911367560055,
13.8358800595847));
#435750=CARTESIAN_POINT('Ctrl Pts',(-2.31990818454371,-1.36347304896067,
13.8390832900376));
#435751=CARTESIAN_POINT('Origin',(-2.34182920731495,-1.36114803492019,13.7902182540695));
#435752=CARTESIAN_POINT('Ctrl Pts',(-2.35861966586612,-1.38605937007289,
13.7382347919292));
#435753=CARTESIAN_POINT('Ctrl Pts',(-2.3735229768461,-1.38842774305202,
13.7369371795942));
#435754=CARTESIAN_POINT('Ctrl Pts',(-2.38106522452574,-1.37528779339612,
13.7364597369711));
#435755=CARTESIAN_POINT('Ctrl Pts',(-2.36048825233909,-1.38635327239884,
13.7595490285574));
#435756=CARTESIAN_POINT('Ctrl Pts',(-2.37574730134179,-1.38877715976248,
13.7633824266926));
#435757=CARTESIAN_POINT('Ctrl Pts',(-2.38345047934689,-1.37587155210806,
13.7648920890506));
#435758=CARTESIAN_POINT('Ctrl Pts',(-2.35095856369513,-1.38485438664562,
13.780380659011));
#435759=CARTESIAN_POINT('Ctrl Pts',(-2.36415624800675,-1.38695629406881,
13.7901039518744));
#435760=CARTESIAN_POINT('Ctrl Pts',(-2.37128930719404,-1.37289909278063,
13.7926933640891));
#435761=CARTESIAN_POINT('Ctrl Pts',(-2.33439383754983,-1.38224898853699,
13.7936647693663));
#435762=CARTESIAN_POINT('Ctrl Pts',(-2.34507321223805,-1.38395904356925,
13.8072068914933));
#435763=CARTESIAN_POINT('Ctrl Pts',(-2.3502002794335,-1.36769997066146,
13.8104111085397));
#435764=CARTESIAN_POINT('Origin',(-2.36230450590072,-1.36436850645314,13.7435492065112));
#435765=CARTESIAN_POINT('Origin',(-2.36230450590072,-1.36436850645314,14.));
#435766=CARTESIAN_POINT('Origin',(-2.36230450590072,-1.36436850645314,12.5369868989719));
#435767=CARTESIAN_POINT('Ctrl Pts',(-2.35803415101985,-1.40238208536313,
12.506462012331));
#435768=CARTESIAN_POINT('Ctrl Pts',(-2.36365400976818,-1.40572435639323,
12.4999388158272));
#435769=CARTESIAN_POINT('Ctrl Pts',(-2.3635875194692,-1.40568481294382,
12.4907030323752));
#435770=CARTESIAN_POINT('Ctrl Pts',(-2.3666678544068,-1.3922980510028,12.5042014951932));
#435771=CARTESIAN_POINT('Ctrl Pts',(-2.37278456078797,-1.39031638499599,
12.4980716682127));
#435772=CARTESIAN_POINT('Ctrl Pts',(-2.3762141316028,-1.38445433678294,
12.4907355092744));
#435773=CARTESIAN_POINT('Ctrl Pts',(-2.36396772154394,-1.38690963901333,
12.5218047446509));
#435774=CARTESIAN_POINT('Ctrl Pts',(-2.37568491888256,-1.38541760769181,
12.5216906929434));
#435775=CARTESIAN_POINT('Ctrl Pts',(-2.38146799229632,-1.37517422855108,
12.5161988840775));
#435776=CARTESIAN_POINT('Ctrl Pts',(-2.35884829980673,-1.3860953248911,
12.5369868989719));
#435777=CARTESIAN_POINT('Ctrl Pts',(-2.37398783342561,-1.38850365487752,
12.5369868989719));
#435778=CARTESIAN_POINT('Ctrl Pts',(-2.38149002219928,-1.37513493410383,
12.5369868989719));
#435779=CARTESIAN_POINT('Origin',(-4.38993701924921E-31,-7.84818254312667E-31,
12.5));
#435780=CARTESIAN_POINT('Origin',(-2.18315043670734,-1.56046289035817,12.5));
#435781=CARTESIAN_POINT('',(-2.18315043670734,-1.56046289035817,12.5893111709658));
#435782=CARTESIAN_POINT('',(-2.18315043670734,-1.56046289035817,13.8235269408515));
#435783=CARTESIAN_POINT('',(-2.18315043670734,-1.56046289035817,12.5));
#435784=CARTESIAN_POINT('',(-2.21791244830466,-1.56888163426146,13.7902182540695));
#435785=CARTESIAN_POINT('',(-2.18315043670734,-1.56046289035817,13.8235269408515));
#435786=CARTESIAN_POINT('',(-2.23805711869615,-1.5737603168592,13.7435492065112));
#435787=CARTESIAN_POINT('Origin',(-2.17178134270818,-1.55770983220249,13.7445212918709));
#435788=CARTESIAN_POINT('',(-2.23805711869615,-1.5737603168592,12.5369868989719));
#435789=CARTESIAN_POINT('',(-2.23805711869615,-1.5737603168592,12.5));
#435790=CARTESIAN_POINT('Ctrl Pts',(-2.23805711869615,-1.5737603168592,
12.5369868989719));
#435791=CARTESIAN_POINT('Ctrl Pts',(-2.21976823989799,-1.5693310741369,
12.5544431401645));
#435792=CARTESIAN_POINT('Ctrl Pts',(-2.20146628040763,-1.56489866350248,
12.5718848856037));
#435793=CARTESIAN_POINT('Ctrl Pts',(-2.18315043670734,-1.56046289035817,
12.5893111709658));
#435794=CARTESIAN_POINT('Origin',(-2.2878767035474,-1.84701015017872,12.5));
#435795=CARTESIAN_POINT('',(-2.17485966055452,-1.66000200552889,13.7435492065112));
#435796=CARTESIAN_POINT('',(-2.16413910514116,-1.64226281217913,13.7902182540695));
#435797=CARTESIAN_POINT('Origin',(-2.13596733839878,-1.59564727800405,13.7418732680442));
#435798=CARTESIAN_POINT('',(-2.14563951868149,-1.61165173575209,13.8235269408515));
#435799=CARTESIAN_POINT('',(-2.16413910514116,-1.64226281217913,13.7902182540695));
#435800=CARTESIAN_POINT('',(-2.14563951868149,-1.61165173575209,12.5893111709658));
#435801=CARTESIAN_POINT('',(-2.14563951868149,-1.61165173575209,12.5));
#435802=CARTESIAN_POINT('',(-2.17485966055452,-1.66000200552889,12.5369868989719));
#435803=CARTESIAN_POINT('Ctrl Pts',(-2.14563951868149,-1.61165173575209,
12.5893111709658));
#435804=CARTESIAN_POINT('Ctrl Pts',(-2.15538681230881,-1.6277804827829,
12.5718848856037));
#435805=CARTESIAN_POINT('Ctrl Pts',(-2.1651267170616,-1.64389700351864,
12.5544431401645));
#435806=CARTESIAN_POINT('Ctrl Pts',(-2.17485966055452,-1.66000200552889,
12.5369868989719));
#435807=CARTESIAN_POINT('',(-2.17485966055452,-1.66000200552889,12.5));
#435808=CARTESIAN_POINT('Origin',(-2.17505932048481,-1.59387208764385,12.5));
#435809=CARTESIAN_POINT('',(-2.14800907319443,-1.57266184734094,13.8587068136939));
#435810=CARTESIAN_POINT('Ctrl Pts',(-2.14563951867576,-1.61165173575538,
13.8235269408542));
#435811=CARTESIAN_POINT('Ctrl Pts',(-2.14473318419907,-1.61015203337041,
13.8262006681044));
#435812=CARTESIAN_POINT('Ctrl Pts',(-2.14395437788002,-1.60852744457645,
13.8288634856214));
#435813=CARTESIAN_POINT('Ctrl Pts',(-2.14329465193769,-1.60678828640047,
13.8314912288862));
#435814=CARTESIAN_POINT('Ctrl Pts',(-2.14261454253872,-1.6049953937069,
13.8342001611531));
#435815=CARTESIAN_POINT('Ctrl Pts',(-2.1420597655961,-1.60307892736555,
13.836875030195));
#435816=CARTESIAN_POINT('Ctrl Pts',(-2.14165213356702,-1.60101735872816,
13.8394886372969));
#435817=CARTESIAN_POINT('Ctrl Pts',(-2.14162065115665,-1.60085813878165,
13.8396904925131));
#435818=CARTESIAN_POINT('Ctrl Pts',(-2.14159006710582,-1.60069804534658,
13.8398919674349));
#435819=CARTESIAN_POINT('Ctrl Pts',(-2.14156040246006,-1.60053706533774,
13.8400930404591));
#435820=CARTESIAN_POINT('Ctrl Pts',(-2.14109820732166,-1.59802888849779,
13.8432258934518));
#435821=CARTESIAN_POINT('Ctrl Pts',(-2.14086045607714,-1.59531849162118,
13.8462331177034));
#435822=CARTESIAN_POINT('Ctrl Pts',(-2.14095100018776,-1.59248584378433,
13.8489036603661));
#435823=CARTESIAN_POINT('Ctrl Pts',(-2.14098062727446,-1.59155896844693,
13.8497774930041));
#435824=CARTESIAN_POINT('Ctrl Pts',(-2.1410455342675,-1.59061921738479,
13.85061494757));
#435825=CARTESIAN_POINT('Ctrl Pts',(-2.14114972096597,-1.58967000778862,
13.8514076489583));
#435826=CARTESIAN_POINT('Ctrl Pts',(-2.14137009085921,-1.58766229259623,
13.8530843267192));
#435827=CARTESIAN_POINT('Ctrl Pts',(-2.14179077808467,-1.58541537373579,
13.8546805203176));
#435828=CARTESIAN_POINT('Ctrl Pts',(-2.14252148138838,-1.58308477177075,
13.8559412814273));
#435829=CARTESIAN_POINT('Ctrl Pts',(-2.14261927318769,-1.58277286164461,
13.8561100121513));
#435830=CARTESIAN_POINT('Ctrl Pts',(-2.14272254699551,-1.58245948265099,
13.8562727473908));
#435831=CARTESIAN_POINT('Ctrl Pts',(-2.14283149278315,-1.5821450282265,
13.8564289040185));
#435832=CARTESIAN_POINT('Ctrl Pts',(-2.1433255606872,-1.58071898099889,
13.8571370725437));
#435833=CARTESIAN_POINT('Ctrl Pts',(-2.14394711454076,-1.579246495635,13.8577210840554));
#435834=CARTESIAN_POINT('Ctrl Pts',(-2.14469903237326,-1.5777962209433,
13.8581177131616));
#435835=CARTESIAN_POINT('Ctrl Pts',(-2.14491079831511,-1.57738777367319,
13.8582294175695));
#435836=CARTESIAN_POINT('Ctrl Pts',(-2.14513273381987,-1.57698103883377,
13.8583265086086));
#435837=CARTESIAN_POINT('Ctrl Pts',(-2.14536448888114,-1.57657740300675,
13.8584082369006));
#435838=CARTESIAN_POINT('Ctrl Pts',(-2.14569745875663,-1.57599748656254,
13.8585256585398));
#435839=CARTESIAN_POINT('Ctrl Pts',(-2.14605511815475,-1.5754169183704,
13.8586122832068));
#435840=CARTESIAN_POINT('Ctrl Pts',(-2.14642884846448,-1.57485119410699,
13.8586682984299));
#435841=CARTESIAN_POINT('Ctrl Pts',(-2.14672779566557,-1.5743986707747,
13.8587131050557));
#435842=CARTESIAN_POINT('Ctrl Pts',(-2.14704013193033,-1.57395051783153,
13.8587357943552));
#435843=CARTESIAN_POINT('Ctrl Pts',(-2.14736630986575,-1.57350697159873,
13.8587355499465));
#435844=CARTESIAN_POINT('Ctrl Pts',(-2.14757712644181,-1.57322029709392,
13.8587353919793));
#435845=CARTESIAN_POINT('Ctrl Pts',(-2.14779141426411,-1.57293862411962,
13.8587257282814));
#435846=CARTESIAN_POINT('Ctrl Pts',(-2.14800907319443,-1.57266184734094,
13.8587068136939));
#435847=CARTESIAN_POINT('Ctrl Pts',(-2.14800907319443,-1.57266184734094,
13.8587068136939));
#435848=CARTESIAN_POINT('Ctrl Pts',(-2.14872494155066,-1.57175154360425,
13.8586446046466));
#435849=CARTESIAN_POINT('Ctrl Pts',(-2.14947723124705,-1.57089413691004,
13.858482427929));
#435850=CARTESIAN_POINT('Ctrl Pts',(-2.15026279169027,-1.5700864555523,
13.8582284286032));
#435851=CARTESIAN_POINT('Ctrl Pts',(-2.15106868532482,-1.56925786843266,
13.8579678548414));
#435852=CARTESIAN_POINT('Ctrl Pts',(-2.15191266088537,-1.56848065799959,
13.857615680862));
#435853=CARTESIAN_POINT('Ctrl Pts',(-2.15275488136508,-1.56777833743812,
13.8571944833187));
#435854=CARTESIAN_POINT('Ctrl Pts',(-2.15485672870745,-1.56602562464953,
13.8561433417727));
#435855=CARTESIAN_POINT('Ctrl Pts',(-2.15704289203238,-1.56465365893415,
13.8546163505475));
#435856=CARTESIAN_POINT('Ctrl Pts',(-2.15911542500467,-1.56360264802645,
13.8528973491086));
#435857=CARTESIAN_POINT('Ctrl Pts',(-2.15949404620135,-1.56341064383982,
13.8525833129073));
#435858=CARTESIAN_POINT('Ctrl Pts',(-2.15986887664421,-1.56322920984854,
13.8522628768812));
#435859=CARTESIAN_POINT('Ctrl Pts',(-2.16023873932082,-1.56305780519975,
13.851937733538));
#435860=CARTESIAN_POINT('Ctrl Pts',(-2.16249743937065,-1.56201106079091,
13.8499521282529));
#435861=CARTESIAN_POINT('Ctrl Pts',(-2.16479705984628,-1.56123802173827,
13.847639871647));
#435862=CARTESIAN_POINT('Ctrl Pts',(-2.16699114162711,-1.56070316305052,
13.8452109780794));
#435863=CARTESIAN_POINT('Ctrl Pts',(-2.16797830443553,-1.56046251905589,
13.8441181685877));
#435864=CARTESIAN_POINT('Ctrl Pts',(-2.16894418485651,-1.56026937647777,
13.8430021611332));
#435865=CARTESIAN_POINT('Ctrl Pts',(-2.16987681917792,-1.5601174904455,
13.8418824960098));
#435866=CARTESIAN_POINT('Ctrl Pts',(-2.17207459577202,-1.5597595671319,
13.8392439765549));
#435867=CARTESIAN_POINT('Ctrl Pts',(-2.17419220479122,-1.5596099068373,
13.8364981347964));
#435868=CARTESIAN_POINT('Ctrl Pts',(-2.17623283400634,-1.55963397838338,
13.8336931113419));
#435869=CARTESIAN_POINT('Ctrl Pts',(-2.17822027726992,-1.55965742254057,
13.8309611966328));
#435870=CARTESIAN_POINT('Ctrl Pts',(-2.18013668608987,-1.55984624831165,
13.8281701127185));
#435871=CARTESIAN_POINT('Ctrl Pts',(-2.18197027689338,-1.56020499048229,
13.825358068512));
#435872=CARTESIAN_POINT('Ctrl Pts',(-2.18236780135844,-1.56028276617205,
13.8247484142932));
#435873=CARTESIAN_POINT('Ctrl Pts',(-2.18276131079612,-1.5603686509502,
13.8241378483365));
#435874=CARTESIAN_POINT('Ctrl Pts',(-2.18315043670734,-1.56046289035817,
13.8235269408515));
#435875=CARTESIAN_POINT('',(-2.14726040899293,-1.57365294711932,12.5969504640361));
#435876=CARTESIAN_POINT('Origin',(-2.17508612331582,-1.59389148586697,12.584524458991));
#435877=CARTESIAN_POINT('Origin',(-2.17508612331582,-1.59389148586697,12.584524458991));
#435878=CARTESIAN_POINT('Ctrl Pts',(-2.14563951868149,-1.61165173575209,
12.5893111709658));
#435879=CARTESIAN_POINT('Ctrl Pts',(-2.13977729878546,-1.60195158047238,
12.5770542771492));
#435880=CARTESIAN_POINT('Ctrl Pts',(-2.15195938587367,-1.59102453013707,
12.5737548217797));
#435881=CARTESIAN_POINT('Ctrl Pts',(-2.15845822617462,-1.63286271987995,
12.5663937883685));
#435882=CARTESIAN_POINT('Ctrl Pts',(-2.15258852820297,-1.62315019070507,
12.5540940315304));
#435883=CARTESIAN_POINT('Ctrl Pts',(-2.16481050928352,-1.61219167010326,
12.5508374392248));
#435884=CARTESIAN_POINT('Ctrl Pts',(-2.17126399974902,-1.65405230238483,
12.5434499600945));
#435885=CARTESIAN_POINT('Ctrl Pts',(-2.1653752172991,-1.64430819431878,
12.5311293540533));
#435886=CARTESIAN_POINT('Ctrl Pts',(-2.17764806832898,-1.63333874163613,
12.5278936106989));
#435887=CARTESIAN_POINT('Ctrl Pts',(-2.18405785253628,-1.67522215968519,
12.5204817579905));
#435888=CARTESIAN_POINT('Ctrl Pts',(-2.17813992463758,-1.66542982494346,
12.5081597038247));
#435889=CARTESIAN_POINT('Ctrl Pts',(-2.19047310544298,-1.65446731172267,
12.5049254088044));
#435890=CARTESIAN_POINT('Ctrl Pts',(-2.17485966055452,-1.66000200552889,
12.5369868989719));
#435891=CARTESIAN_POINT('Ctrl Pts',(-2.17534145930686,-1.66079923268157,
12.5342545179733));
#435892=CARTESIAN_POINT('Ctrl Pts',(-2.17590802981826,-1.66149554796143,
12.5314872231885));
#435893=CARTESIAN_POINT('Ctrl Pts',(-2.1765708169311,-1.66201644560318,
12.5287124745063));
#435894=CARTESIAN_POINT('Ctrl Pts',(-2.17716855124728,-1.66248621695156,
12.5262100684184));
#435895=CARTESIAN_POINT('Ctrl Pts',(-2.17784454637923,-1.66281206802078,
12.5237004536639));
#435896=CARTESIAN_POINT('Ctrl Pts',(-2.17863919409348,-1.66293987874678,
12.5212220730815));
#435897=CARTESIAN_POINT('Ctrl Pts',(-2.17924756566123,-1.66303772891404,
12.5193246583486));
#435898=CARTESIAN_POINT('Ctrl Pts',(-2.17993285387773,-1.66302004605718,
12.517417831369));
#435899=CARTESIAN_POINT('Ctrl Pts',(-2.18071177879441,-1.66279104676097,
12.5155812248348));
#435900=CARTESIAN_POINT('Ctrl Pts',(-2.18104360499566,-1.66269349182991,
12.5147988205793));
#435901=CARTESIAN_POINT('Ctrl Pts',(-2.18139283942619,-1.6625577538129,
12.5140295443047));
#435902=CARTESIAN_POINT('Ctrl Pts',(-2.18176242080078,-1.66237777503528,
12.5132817086137));
#435903=CARTESIAN_POINT('Ctrl Pts',(-2.18232173221537,-1.66210540150232,
12.5121499604604));
#435904=CARTESIAN_POINT('Ctrl Pts',(-2.18293659040559,-1.66171939305322,
12.5110494206568));
#435905=CARTESIAN_POINT('Ctrl Pts',(-2.18359839614335,-1.66118351500816,
12.5100666561695));
#435906=CARTESIAN_POINT('Ctrl Pts',(-2.18397840347396,-1.66087581506871,
12.5095023550641));
#435907=CARTESIAN_POINT('Ctrl Pts',(-2.18437786942042,-1.66051464018997,
12.5089719619137));
#435908=CARTESIAN_POINT('Ctrl Pts',(-2.18478502293511,-1.66010202256744,
12.5085043804652));
#435909=CARTESIAN_POINT('Ctrl Pts',(-2.1853808390684,-1.6594982104241,12.5078201359221));
#435910=CARTESIAN_POINT('Ctrl Pts',(-2.18600953869774,-1.65876587526262,
12.5072563000949));
#435911=CARTESIAN_POINT('Ctrl Pts',(-2.18662208166213,-1.65794914403194,
12.5068768744332));
#435912=CARTESIAN_POINT('Ctrl Pts',(-2.18706376730705,-1.65736022459066,
12.5066032824114));
#435913=CARTESIAN_POINT('Ctrl Pts',(-2.18750486024884,-1.65671711384018,
12.5064197834844));
#435914=CARTESIAN_POINT('Ctrl Pts',(-2.18792286036064,-1.65605718679586,
12.5063282718343));
#435915=CARTESIAN_POINT('Ctrl Pts',(-2.18853301111429,-1.65509389761941,
12.5061946931565));
#435916=CARTESIAN_POINT('Ctrl Pts',(-2.18910789664451,-1.65407475724285,
12.5062515701262));
#435917=CARTESIAN_POINT('Ctrl Pts',(-2.18962530789657,-1.65307061322183,
12.5064436508398));
#435918=CARTESIAN_POINT('',(-2.15195938587367,-1.59102453013707,12.5737548217797));
#435919=CARTESIAN_POINT('Origin',(-2.16446819183562,-1.60027276096282,12.5893111709658));
#435920=CARTESIAN_POINT('Ctrl Pts',(-2.18962530789657,-1.65307061322183,
12.5064436508398));
#435921=CARTESIAN_POINT('Ctrl Pts',(-2.18405018354364,-1.643885931616,12.5164271754438));
#435922=CARTESIAN_POINT('Ctrl Pts',(-2.17847267060597,-1.6346977176192,
12.5264061185523));
#435923=CARTESIAN_POINT('Ctrl Pts',(-2.17289268576872,-1.62550584633245,
12.536380305637));
#435924=CARTESIAN_POINT('Ctrl Pts',(-2.16591883646502,-1.61401787153639,
12.5488460165097));
#435925=CARTESIAN_POINT('Ctrl Pts',(-2.15894112399064,-1.60252418069806,
12.5613043021964));
#435926=CARTESIAN_POINT('Ctrl Pts',(-2.15195938587367,-1.59102453013707,
12.5737548217797));
#435927=CARTESIAN_POINT('Ctrl Pts',(-2.18315043670734,-1.56046289035817,
12.5893111709658));
#435928=CARTESIAN_POINT('Ctrl Pts',(-2.17213491717367,-1.5577951265075,
12.5770542771492));
#435929=CARTESIAN_POINT('Ctrl Pts',(-2.16538527500074,-1.57270304404793,
12.5737548217797));
#435930=CARTESIAN_POINT('Ctrl Pts',(-2.17287305279036,-1.55797388988848,
12.5928319619712));
#435931=CARTESIAN_POINT('Ctrl Pts',(-2.16470314250846,-1.55934720061706,
12.5821634970842));
#435932=CARTESIAN_POINT('Ctrl Pts',(-2.16164369450117,-1.57178718776297,
12.5773203894503));
#435933=CARTESIAN_POINT('Ctrl Pts',(-2.15643226432231,-1.56118084699587,
12.5969440695591));
#435934=CARTESIAN_POINT('Ctrl Pts',(-2.15404153911457,-1.56441240629952,
12.5878292599214));
#435935=CARTESIAN_POINT('Ctrl Pts',(-2.15578425371447,-1.5729322208475,
12.5813877129824));
#435936=CARTESIAN_POINT('Ctrl Pts',(-2.1383034984697,-1.58582883056862,
12.596957478804));
#435937=CARTESIAN_POINT('Ctrl Pts',(-2.14067662001774,-1.58262120102843,
12.5878468778671));
#435938=CARTESIAN_POINT('Ctrl Pts',(-2.14930052242839,-1.58175761018249,
12.5814011370086));
#435939=CARTESIAN_POINT('Ctrl Pts',(-2.14016217694572,-1.60258843442619,
12.5928371701607));
#435940=CARTESIAN_POINT('Ctrl Pts',(-2.13901736357199,-1.59438938155143,
12.5821692192952));
#435941=CARTESIAN_POINT('Ctrl Pts',(-2.14995232295486,-1.58772226183877,
12.5773318885715));
#435942=CARTESIAN_POINT('Ctrl Pts',(-2.14563951868144,-1.61165173575211,
12.5893111709658));
#435943=CARTESIAN_POINT('Ctrl Pts',(-2.13977729878542,-1.60195158047241,
12.5770542771492));
#435944=CARTESIAN_POINT('Ctrl Pts',(-2.15195938587362,-1.5910245301371,
12.5737548217797));
#435945=CARTESIAN_POINT('',(-2.16538527500074,-1.57270304404793,12.5737548217797));
#435946=CARTESIAN_POINT('Origin',(-2.17797212232493,-1.581844776621,12.5893111709658));
#435947=CARTESIAN_POINT('Ctrl Pts',(-2.15195938587362,-1.5910245301371,
12.5737548217797));
#435948=CARTESIAN_POINT('Ctrl Pts',(-2.15141334535943,-1.59018419723408,
12.5746934679442));
#435949=CARTESIAN_POINT('Ctrl Pts',(-2.15096271955715,-1.58915450221877,
12.5756680099006));
#435950=CARTESIAN_POINT('Ctrl Pts',(-2.15065572622269,-1.58805393020359,
12.5765688348656));
#435951=CARTESIAN_POINT('Ctrl Pts',(-2.15057445313592,-1.58776256594631,
12.5768073183026));
#435952=CARTESIAN_POINT('Ctrl Pts',(-2.15050302340756,-1.58746636141546,
12.5770407398754));
#435953=CARTESIAN_POINT('Ctrl Pts',(-2.15044178803712,-1.58716766194725,
12.5772674179684));
#435954=CARTESIAN_POINT('Ctrl Pts',(-2.15019049463559,-1.58594188010145,
12.5781976435658));
#435955=CARTESIAN_POINT('Ctrl Pts',(-2.15010765757659,-1.5846021952488,
12.5790594849312));
#435956=CARTESIAN_POINT('Ctrl Pts',(-2.15024706728575,-1.5832360848372,
12.5797571720116));
#435957=CARTESIAN_POINT('Ctrl Pts',(-2.15033789772399,-1.58234601478309,
12.580211740231));
#435958=CARTESIAN_POINT('Ctrl Pts',(-2.15054587538036,-1.58140618380107,
12.5806009430798));
#435959=CARTESIAN_POINT('Ctrl Pts',(-2.1508736577402,-1.58048657987062,
12.5808812374708));
#435960=CARTESIAN_POINT('Ctrl Pts',(-2.15115533152798,-1.57969633501893,
12.5811221033394));
#435961=CARTESIAN_POINT('Ctrl Pts',(-2.15153134934478,-1.57890488675521,
12.581287365893));
#435962=CARTESIAN_POINT('Ctrl Pts',(-2.15198801935523,-1.57816048378301,
12.581359338449));
#435963=CARTESIAN_POINT('Ctrl Pts',(-2.1520514870568,-1.57805702714121,
12.5813693411482));
#435964=CARTESIAN_POINT('Ctrl Pts',(-2.15211647489126,-1.57795443266022,
12.5813775999465));
#435965=CARTESIAN_POINT('Ctrl Pts',(-2.15218290834766,-1.57785278151387,
12.5813841266931));
#435966=CARTESIAN_POINT('Ctrl Pts',(-2.15229562074141,-1.57768031804963,
12.5813952001081));
#435967=CARTESIAN_POINT('Ctrl Pts',(-2.1524137589618,-1.57750974801417,
12.5814007534795));
#435968=CARTESIAN_POINT('Ctrl Pts',(-2.15253743367731,-1.57734125798304,
12.5814005856065));
#435969=CARTESIAN_POINT('Ctrl Pts',(-2.15310356817123,-1.57656997649586,
12.5813998171494));
#435970=CARTESIAN_POINT('Ctrl Pts',(-2.15374632955927,-1.5758953703895,
12.58127954464));
#435971=CARTESIAN_POINT('Ctrl Pts',(-2.15444064631559,-1.57530085853175,
12.5810700125799));
#435972=CARTESIAN_POINT('Ctrl Pts',(-2.15527930190294,-1.57458275589817,
12.5808169217085));
#435973=CARTESIAN_POINT('Ctrl Pts',(-2.15620413715905,-1.57399415747095,
12.5804173076348));
#435974=CARTESIAN_POINT('Ctrl Pts',(-2.15712011844871,-1.57356467680243,
12.5799304713245));
#435975=CARTESIAN_POINT('Ctrl Pts',(-2.15825530783048,-1.57303241495377,
12.5793271277669));
#435976=CARTESIAN_POINT('Ctrl Pts',(-2.15943364635984,-1.57268237050142,
12.5785808224116));
#435977=CARTESIAN_POINT('Ctrl Pts',(-2.16059643289824,-1.57249889481065,
12.5777485681082));
#435978=CARTESIAN_POINT('Ctrl Pts',(-2.16232911223324,-1.57222549593015,
12.576508418016));
#435979=CARTESIAN_POINT('Ctrl Pts',(-2.16401159887118,-1.57231746453322,
12.5750928681475));
#435980=CARTESIAN_POINT('Ctrl Pts',(-2.16538527500074,-1.57270304404793,
12.5737548217797));
#435981=CARTESIAN_POINT('Ctrl Pts',(-2.16538527500074,-1.57270304404793,
12.5737548217797));
#435982=CARTESIAN_POINT('Ctrl Pts',(-2.17213491717367,-1.5577951265075,
12.5770542771492));
#435983=CARTESIAN_POINT('Ctrl Pts',(-2.18315043670734,-1.56046289035817,
12.5893111709658));
#435984=CARTESIAN_POINT('Ctrl Pts',(-2.18943686311886,-1.57857978320892,
12.5508408821982));
#435985=CARTESIAN_POINT('Ctrl Pts',(-2.19620448976733,-1.56362435094581,
12.55409748406));
#435986=CARTESIAN_POINT('Ctrl Pts',(-2.2072340622827,-1.5662955181799,12.5663972313419));
#435987=CARTESIAN_POINT('Ctrl Pts',(-2.21346523583044,-1.58444963573048,
12.52790050457));
#435988=CARTESIAN_POINT('Ctrl Pts',(-2.22022796340049,-1.56944241103187,
12.5311362602938));
#435989=CARTESIAN_POINT('Ctrl Pts',(-2.23129339143735,-1.57212226183859,
12.5434568539655));
#435990=CARTESIAN_POINT('Ctrl Pts',(-2.23747220055742,-1.59031312334059,
12.5049357605811));
#435991=CARTESIAN_POINT('Ctrl Pts',(-2.24421014365406,-1.57525047059229,
12.5081700652078));
#435992=CARTESIAN_POINT('Ctrl Pts',(-2.25533032707183,-1.57794358218308,
12.5204921097672));
#435993=CARTESIAN_POINT('Ctrl Pts',(-2.23589580952561,-1.58992810221813,
12.5064436508395));
#435994=CARTESIAN_POINT('Ctrl Pts',(-2.236761714628,-1.58906841847149,12.5062361689309));
#435995=CARTESIAN_POINT('Ctrl Pts',(-2.23762552625068,-1.58813749360828,
12.5061871075061));
#435996=CARTESIAN_POINT('Ctrl Pts',(-2.23840967326764,-1.5871908521255,
12.5063648335164));
#435997=CARTESIAN_POINT('Ctrl Pts',(-2.23876588121094,-1.58676082917275,
12.5064455676329));
#435998=CARTESIAN_POINT('Ctrl Pts',(-2.23911044876432,-1.58632142457011,
12.506574497099));
#435999=CARTESIAN_POINT('Ctrl Pts',(-2.23942777490356,-1.58589083016024,
12.5067492519495));
#436000=CARTESIAN_POINT('Ctrl Pts',(-2.24006545409804,-1.58502553397919,
12.5071004286051));
#436001=CARTESIAN_POINT('Ctrl Pts',(-2.24061592034305,-1.58416352221299,
12.5076537929612));
#436002=CARTESIAN_POINT('Ctrl Pts',(-2.24104582996362,-1.58337458396168,
12.5083435010503));
#436003=CARTESIAN_POINT('Ctrl Pts',(-2.24107289534344,-1.58332491558395,
12.5083869222963));
#436004=CARTESIAN_POINT('Ctrl Pts',(-2.24109947537414,-1.58327552570261,
12.5084308732336));
#436005=CARTESIAN_POINT('Ctrl Pts',(-2.24112555899769,-1.5832264269791,
12.5084753333615));
#436006=CARTESIAN_POINT('Ctrl Pts',(-2.24133478408543,-1.58283259041285,
12.508831962269));
#436007=CARTESIAN_POINT('Ctrl Pts',(-2.24151745646358,-1.58245009711726,
12.509227847131));
#436008=CARTESIAN_POINT('Ctrl Pts',(-2.24167067102003,-1.5820915273163,
12.5096423454524));
#436009=CARTESIAN_POINT('Ctrl Pts',(-2.24215077763003,-1.58096792825642,
12.5109411997424));
#436010=CARTESIAN_POINT('Ctrl Pts',(-2.24238005312552,-1.58001392886605,
12.5124831113042));
#436011=CARTESIAN_POINT('Ctrl Pts',(-2.24245164411503,-1.57921280889644,
12.5140723025008));
#436012=CARTESIAN_POINT('Ctrl Pts',(-2.24245835226916,-1.57913774307785,
12.5142212114565));
#436013=CARTESIAN_POINT('Ctrl Pts',(-2.24246370141256,-1.57906400438223,
12.5143705582413));
#436014=CARTESIAN_POINT('Ctrl Pts',(-2.24246778349925,-1.57899157173358,
12.5145201959299));
#436015=CARTESIAN_POINT('Ctrl Pts',(-2.24252022398046,-1.5780610665208,
12.5164425148273));
#436016=CARTESIAN_POINT('Ctrl Pts',(-2.24237607724193,-1.57731482292979,
12.5184635205941));
#436017=CARTESIAN_POINT('Ctrl Pts',(-2.24210289351335,-1.57669305011659,
12.5205025929158));
#436018=CARTESIAN_POINT('Ctrl Pts',(-2.24194443612279,-1.57633239724016,
12.5216853356836));
#436019=CARTESIAN_POINT('Ctrl Pts',(-2.24174329370341,-1.57601407903197,
12.5228750347131));
#436020=CARTESIAN_POINT('Ctrl Pts',(-2.24151631132257,-1.57573108283529,
12.5240609649613));
#436021=CARTESIAN_POINT('Ctrl Pts',(-2.24095919524596,-1.57503648385276,
12.5269717671326));
#436022=CARTESIAN_POINT('Ctrl Pts',(-2.24022262229414,-1.57454163107181,
12.5299036066169));
#436023=CARTESIAN_POINT('Ctrl Pts',(-2.23936585500481,-1.57418329891015,
12.5328133004019));
#436024=CARTESIAN_POINT('Ctrl Pts',(-2.23895455681786,-1.5740112786075,
12.5342101228451));
#436025=CARTESIAN_POINT('Ctrl Pts',(-2.23851587010387,-1.57387141841433,
12.5356023438238));
#436026=CARTESIAN_POINT('Ctrl Pts',(-2.23805711869614,-1.5737603168592,
12.5369868989719));
#436027=CARTESIAN_POINT('Origin',(-14.6270958531998,-4.56871522885748,-1.24066348164869));
#436028=CARTESIAN_POINT('Ctrl Pts',(-2.17483800949988,-1.65996625650419,
12.5369868989719));
#436029=CARTESIAN_POINT('Ctrl Pts',(-2.18279663890026,-1.67307898016302,
12.5369868989719));
#436030=CARTESIAN_POINT('Ctrl Pts',(-2.17324475226915,-1.68508084524608,
12.5369868989719));
#436031=CARTESIAN_POINT('Ctrl Pts',(-2.17752828089512,-1.66439890429058,
12.5218025310016));
#436032=CARTESIAN_POINT('Ctrl Pts',(-2.18057822279872,-1.67581615956887,
12.5216901060418));
#436033=CARTESIAN_POINT('Ctrl Pts',(-2.17327388248902,-1.68504426985358,
12.5161920673678));
#436034=CARTESIAN_POINT('Ctrl Pts',(-2.18353821313673,-1.66486450674627,
12.5042015548894));
#436035=CARTESIAN_POINT('Ctrl Pts',(-2.18401471619858,-1.67127935591431,
12.4980677368513));
#436036=CARTESIAN_POINT('Ctrl Pts',(-2.17987961749313,-1.67667303169434,
12.4907278922777));
#436037=CARTESIAN_POINT('Ctrl Pts',(-2.18960934508998,-1.65305856199325,
12.506463626192));
#436038=CARTESIAN_POINT('Ctrl Pts',(-2.19483108864571,-1.65700074826163,
12.4999376786891));
#436039=CARTESIAN_POINT('Ctrl Pts',(-2.19476731264059,-1.6569526001883,
12.4906970594712));
#436040=CARTESIAN_POINT('Origin',(-2.15603098740039,-1.67138098031816,12.5369868989719));
#436041=CARTESIAN_POINT('Origin',(-2.15603098740039,-1.67138098031816,14.));
#436042=CARTESIAN_POINT('Origin',(-2.15603098740039,-1.67138098031816,13.7435492065112));
#436043=CARTESIAN_POINT('Ctrl Pts',(-2.16205306463871,-1.63881111479855,
13.793642941384));
#436044=CARTESIAN_POINT('Ctrl Pts',(-2.1676687580577,-1.64805071470493,
13.8071662555867));
#436045=CARTESIAN_POINT('Ctrl Pts',(-2.15457450270751,-1.65893923436826,
13.8103758687955));
#436046=CARTESIAN_POINT('Ctrl Pts',(-2.17064994587363,-1.65303628046563,
13.7804579775006));
#436047=CARTESIAN_POINT('Ctrl Pts',(-2.177570538214,-1.66444237854459,13.7901904343351));
#436048=CARTESIAN_POINT('Ctrl Pts',(-2.16724525986977,-1.67634383019045,
13.7927914348262));
#436049=CARTESIAN_POINT('Ctrl Pts',(-2.17571125336112,-1.66141117086671,
13.7597120340895));
#436050=CARTESIAN_POINT('Ctrl Pts',(-2.18371542853105,-1.67461421104018,
13.7635825532445));
#436051=CARTESIAN_POINT('Ctrl Pts',(-2.17469652490333,-1.68662234551219,
13.7651073818884));
#436052=CARTESIAN_POINT('Ctrl Pts',(-2.17472013346362,-1.65977117556342,
13.7381884353898));
#436053=CARTESIAN_POINT('Ctrl Pts',(-2.18253772462018,-1.67266470801713,
13.7368803041982));
#436054=CARTESIAN_POINT('Ctrl Pts',(-2.17323694564973,-1.68460979686827,
13.7363986145813));
#436055=CARTESIAN_POINT('Origin',(-2.14531043198703,-1.65364178696841,13.7902182540695));
#436056=CARTESIAN_POINT('Ctrl Pts',(-2.1456374821273,-1.61164836735401,
13.8235227101244));
#436057=CARTESIAN_POINT('Ctrl Pts',(-2.15158786257978,-1.62148582946527,
13.8358800583119));
#436058=CARTESIAN_POINT('Ctrl Pts',(-2.13917755793398,-1.63246810553425,
13.8390832900376));
#436059=CARTESIAN_POINT('Ctrl Pts',(-2.1518067377986,-1.62185657159162,
13.8124254819052));
#436060=CARTESIAN_POINT('Ctrl Pts',(-2.15776867356756,-1.63171313805881,
13.8247886449157));
#436061=CARTESIAN_POINT('Ctrl Pts',(-2.1453313926142,-1.64269652658828,
13.8279860620657));
#436062=CARTESIAN_POINT('Ctrl Pts',(-2.15797322861023,-1.63206020084418,
13.8013225099955));
#436063=CARTESIAN_POINT('Ctrl Pts',(-2.1639439083346,-1.64193121991324,
13.8136962257787));
#436064=CARTESIAN_POINT('Ctrl Pts',(-2.15148261063204,-1.65292007264905,
13.8168830918626));
#436065=CARTESIAN_POINT('Ctrl Pts',(-2.16413706213862,-1.64225943311734,
13.7902140179785));
#436066=CARTESIAN_POINT('Ctrl Pts',(-2.17011385819802,-1.65214055706196,
13.802602731458));
#436067=CARTESIAN_POINT('Ctrl Pts',(-2.15763131637945,-1.66313893431814,
13.8057746032558));
#436068=CARTESIAN_POINT('Origin',(-2.12681084552735,-1.62303071054136,13.8235269408515));
#436069=CARTESIAN_POINT('Ctrl Pts',(-2.18315043670734,-1.56046289035817,
13.8235269408515));
#436070=CARTESIAN_POINT('Ctrl Pts',(-2.19462617425083,-1.56324211086471,
13.8362179249168));
#436071=CARTESIAN_POINT('Ctrl Pts',(-2.20127772059233,-1.54751252297043,
13.8391868794938));
#436072=CARTESIAN_POINT('Ctrl Pts',(-2.17265063636421,-1.55792002456695,
13.8400110824519));
#436073=CARTESIAN_POINT('Ctrl Pts',(-2.18265659817329,-1.55682339740282,
13.8494522556837));
#436074=CARTESIAN_POINT('Ctrl Pts',(-2.18397156707257,-1.54343688388251,
13.85569149686));
#436075=CARTESIAN_POINT('Ctrl Pts',(-2.15663504899221,-1.56090309130709,
13.8586819406588));
#436076=CARTESIAN_POINT('Ctrl Pts',(-2.15921973523695,-1.55739945881335,
13.868010383617));
#436077=CARTESIAN_POINT('Ctrl Pts',(-2.1574121079548,-1.54853236512931,
13.8744918421245));
#436078=CARTESIAN_POINT('Ctrl Pts',(-2.138097553707,-1.58611088308855,13.8587686893867));
#436079=CARTESIAN_POINT('Ctrl Pts',(-2.1355358258333,-1.58958329985802,
13.8680909899357));
#436080=CARTESIAN_POINT('Ctrl Pts',(-2.12655469491602,-1.59049746010243,
13.8745789365162));
#436081=CARTESIAN_POINT('Ctrl Pts',(-2.14004266069163,-1.60239067211602,
13.8400379222776));
#436082=CARTESIAN_POINT('Ctrl Pts',(-2.142003711595,-1.6122610577854,13.8494748685453));
#436083=CARTESIAN_POINT('Ctrl Pts',(-2.12964132381769,-1.61754617592111,
13.8557104837033));
#436084=CARTESIAN_POINT('Ctrl Pts',(-2.14563951867576,-1.61165173575538,
13.8235269408542));
#436085=CARTESIAN_POINT('Ctrl Pts',(-2.15174665658629,-1.6217571543678,
13.8362179249195));
#436086=CARTESIAN_POINT('Ctrl Pts',(-2.13875151769632,-1.63283819083947,
13.8391868794965));
#436087=CARTESIAN_POINT('Origin',(-2.18832875108976,-1.53908100409533,13.8235269408515));
#436088=CARTESIAN_POINT('Ctrl Pts',(-2.21790861637325,-1.56888070545357,
13.7902140241682));
#436089=CARTESIAN_POINT('Ctrl Pts',(-2.22913121062742,-1.57160319945704,
13.8026027327198));
#436090=CARTESIAN_POINT('Ctrl Pts',(-2.2358583528096,-1.55638730348163,
13.8057746032556));
#436091=CARTESIAN_POINT('Ctrl Pts',(-2.20632634380879,-1.56607568405177,
13.8013225161808));
#436092=CARTESIAN_POINT('Ctrl Pts',(-2.21753746007388,-1.56879538991384,
13.8136962270464));
#436093=CARTESIAN_POINT('Ctrl Pts',(-2.22426191989512,-1.55360262040246,
13.8168830918628));
#436094=CARTESIAN_POINT('Ctrl Pts',(-2.19473907802239,-1.56326945338002,
13.8124254880875));
#436095=CARTESIAN_POINT('Ctrl Pts',(-2.20593377898326,-1.56598517527985,
13.8247886461868));
#436096=CARTESIAN_POINT('Ctrl Pts',(-2.21266026338476,-1.55081695291219,
13.8279860620656));
#436097=CARTESIAN_POINT('Ctrl Pts',(-2.18314661686892,-1.56046196448233,
13.8235227163065));
#436098=CARTESIAN_POINT('Ctrl Pts',(-2.19431961995507,-1.56317242298117,
13.8358800595847));
#436099=CARTESIAN_POINT('Ctrl Pts',(-2.20105317008208,-1.54803025888599,
13.8390832900376));
#436100=CARTESIAN_POINT('Origin',(-2.22309076268708,-1.54749974799863,13.7902182540695));
#436101=CARTESIAN_POINT('Ctrl Pts',(-2.23779484729206,-1.57369677098558,
13.7382347919292));
#436102=CARTESIAN_POINT('Ctrl Pts',(-2.25245552434945,-1.57727202159944,
13.7369371795943));
#436103=CARTESIAN_POINT('Ctrl Pts',(-2.26104370370444,-1.56479055724679,
13.7364597369711));
#436104=CARTESIAN_POINT('Ctrl Pts',(-2.23963326042968,-1.57414200252046,
13.7595490285573));
#436105=CARTESIAN_POINT('Ctrl Pts',(-2.25464396688323,-1.57780157875066,
13.7633824266926));
#436106=CARTESIAN_POINT('Ctrl Pts',(-2.26337344003257,-1.5655667939613,
13.7648920890506));
#436107=CARTESIAN_POINT('Ctrl Pts',(-2.2302574541424,-1.57187134609213,
13.7803806590111));
#436108=CARTESIAN_POINT('Ctrl Pts',(-2.24323989928002,-1.57504199338444,
13.7901039518744));
#436109=CARTESIAN_POINT('Ctrl Pts',(-2.25149501620699,-1.56161297681778,
13.7926933640892));
#436110=CARTESIAN_POINT('Ctrl Pts',(-2.21396020989002,-1.56792443827051,
13.7936647693663));
#436111=CARTESIAN_POINT('Ctrl Pts',(-2.22446466447944,-1.57049927141529,
13.8072068914933));
#436112=CARTESIAN_POINT('Ctrl Pts',(-2.2308999371656,-1.55471220280514,
13.8104111085397));
#436113=CARTESIAN_POINT('Origin',(-2.24323543307856,-1.55237843059637,13.7435492065112));
#436114=CARTESIAN_POINT('Origin',(-2.24323543307856,-1.55237843059637,14.));
#436115=CARTESIAN_POINT('Origin',(-2.24323543307856,-1.55237843059637,12.5369868989719));
#436116=CARTESIAN_POINT('Ctrl Pts',(-2.23588082786927,-1.5899174488916,
12.506462012331));
#436117=CARTESIAN_POINT('Ctrl Pts',(-2.24120956088414,-1.59370666945078,
12.4999388158272));
#436118=CARTESIAN_POINT('Ctrl Pts',(-2.24114651498437,-1.5936618380023,
12.4907030323752));
#436119=CARTESIAN_POINT('Ctrl Pts',(-2.24530774573641,-1.58057069530115,
12.5042014951932));
#436120=CARTESIAN_POINT('Ctrl Pts',(-2.25156562345814,-1.57909419147928,
12.4980716682127));
#436121=CARTESIAN_POINT('Ctrl Pts',(-2.25546159400896,-1.57353119060809,
12.4907355092743));
#436122=CARTESIAN_POINT('Ctrl Pts',(-2.24305580294359,-1.57498012691293,
12.5218047446509));
#436123=CARTESIAN_POINT('Ctrl Pts',(-2.25485562667871,-1.57444812056282,
12.5216906929434));
#436124=CARTESIAN_POINT('Ctrl Pts',(-2.26145438788765,-1.56471019959181,
12.5161988840776));
#436125=CARTESIAN_POINT('Ctrl Pts',(-2.23801978982061,-1.57375124195579,
12.5369868989719));
#436126=CARTESIAN_POINT('Ctrl Pts',(-2.25291264663855,-1.57738557096137,
12.5369868989719));
#436127=CARTESIAN_POINT('Ctrl Pts',(-2.26147954735017,-1.56467283153519,
12.5369868989719));
#436128=CARTESIAN_POINT('Origin',(-4.15555475928479E-31,-8.1970313822065E-31,
12.5));
#436129=CARTESIAN_POINT('Origin',(-2.04869397153156,-1.7332176067911,12.5));
#436130=CARTESIAN_POINT('',(-2.04869397153156,-1.7332176067911,12.5893111709658));
#436131=CARTESIAN_POINT('',(-2.04869397153156,-1.7332176067911,13.8235269408515));
#436132=CARTESIAN_POINT('',(-2.04869397153156,-1.7332176067911,12.5));
#436133=CARTESIAN_POINT('',(-2.08265410961903,-1.74444176467851,13.7902182540695));
#436134=CARTESIAN_POINT('',(-2.04869397153156,-1.7332176067911,13.8235269408515));
#436135=CARTESIAN_POINT('',(-2.10233409235841,-1.75094619151327,13.7435492065112));
#436136=CARTESIAN_POINT('Origin',(-2.0375871070498,-1.72954702250194,13.74452129187));
#436137=CARTESIAN_POINT('',(-2.10233409235841,-1.75094619151327,12.5369868989719));
#436138=CARTESIAN_POINT('',(-2.10233409235841,-1.75094619151327,12.5));
#436139=CARTESIAN_POINT('Ctrl Pts',(-2.10233409235841,-1.75094619151327,
12.5369868989719));
#436140=CARTESIAN_POINT('Ctrl Pts',(-2.08446709269668,-1.74504097332302,
12.5544431401645));
#436141=CARTESIAN_POINT('Ctrl Pts',(-2.06658731408192,-1.73913153156377,
12.5718848856037));
#436142=CARTESIAN_POINT('Ctrl Pts',(-2.04869397153156,-1.7332176067911,
12.5893111709658));
#436143=CARTESIAN_POINT('Origin',(-2.12971550850767,-2.02734756722178,12.5));
#436144=CARTESIAN_POINT('',(-2.03231742028997,-1.83174973854323,13.7435492065112));
#436145=CARTESIAN_POINT('',(-2.02307844558101,-1.81319574610499,13.7902182540695));
#436146=CARTESIAN_POINT('Origin',(-1.99880001686223,-1.76443906075294,13.7418732680451));
#436147=CARTESIAN_POINT('',(-2.00713550187734,-1.78117863747128,13.8235269408515));
#436148=CARTESIAN_POINT('',(-2.02307844558101,-1.81319574610499,13.7902182540695));
#436149=CARTESIAN_POINT('',(-2.00713550187734,-1.78117863747128,12.5893111709658));
#436150=CARTESIAN_POINT('',(-2.00713550187734,-1.78117863747128,12.5));
#436151=CARTESIAN_POINT('',(-2.03231742028997,-1.83174973854323,12.5369868989719));
#436152=CARTESIAN_POINT('Ctrl Pts',(-2.00713550187734,-1.78117863747128,
12.5893111709658));
#436153=CARTESIAN_POINT('Ctrl Pts',(-2.01553571957422,-1.79804821234696,
12.5718848856037));
#436154=CARTESIAN_POINT('Ctrl Pts',(-2.02392956953899,-1.81490499934768,
12.5544431401645));
#436155=CARTESIAN_POINT('Ctrl Pts',(-2.03231742028997,-1.83174973854323,
12.5369868989719));
#436156=CARTESIAN_POINT('',(-2.03231742028997,-1.83174973854323,12.5));
#436157=CARTESIAN_POINT('Origin',(-2.03790661809615,-1.76585613664249,12.5));
#436158=CARTESIAN_POINT('',(-2.01267520976314,-1.74251162538801,13.8587068136939));
#436159=CARTESIAN_POINT('Ctrl Pts',(-2.00713550187136,-1.78117863747409,
13.8235269408542));
#436160=CARTESIAN_POINT('Ctrl Pts',(-2.00635442281481,-1.77961005055124,
13.8262006681044));
#436161=CARTESIAN_POINT('Ctrl Pts',(-2.0057106269782,-1.7779273874974,13.8288634856214));
#436162=CARTESIAN_POINT('Ctrl Pts',(-2.00519485375642,-1.7761402424379,
13.8314912288862));
#436163=CARTESIAN_POINT('Ctrl Pts',(-2.0046631447643,-1.77429788021702,
13.834200161153));
#436164=CARTESIAN_POINT('Ctrl Pts',(-2.00426642359461,-1.77234257128823,
13.8368750301949));
#436165=CARTESIAN_POINT('Ctrl Pts',(-2.0040281849101,-1.77025463655578,
13.8394886372968));
#436166=CARTESIAN_POINT('Ctrl Pts',(-2.00400978515861,-1.77009338029176,
13.839690492513));
#436167=CARTESIAN_POINT('Ctrl Pts',(-2.00399235197489,-1.76993132667031,
13.8398919674349));
#436168=CARTESIAN_POINT('Ctrl Pts',(-2.00397590740097,-1.76976846436512,
13.8400930404591));
#436169=CARTESIAN_POINT('Ctrl Pts',(-2.00371968987599,-1.7672309600821,
13.8432258934518));
#436170=CARTESIAN_POINT('Ctrl Pts',(-2.00370365223667,-1.76451020289391,
13.8462331177034));
#436171=CARTESIAN_POINT('Ctrl Pts',(-2.00402478216495,-1.76169436064464,
13.8489036603661));
#436172=CARTESIAN_POINT('Ctrl Pts',(-2.00412985961466,-1.76077298429107,
13.8497774930041));
#436173=CARTESIAN_POINT('Ctrl Pts',(-2.00427114907082,-1.75984165069557,
13.85061494757));
#436174=CARTESIAN_POINT('Ctrl Pts',(-2.00445235849077,-1.75890409169918,
13.8514076489583));
#436175=CARTESIAN_POINT('Ctrl Pts',(-2.00483564254826,-1.75692101920558,
13.8530843267192));
#436176=CARTESIAN_POINT('Ctrl Pts',(-2.00543807471819,-1.75471586669665,
13.8546805203176));
#436177=CARTESIAN_POINT('Ctrl Pts',(-2.00635631236334,-1.75245257872016,
13.8559412814273));
#436178=CARTESIAN_POINT('Ctrl Pts',(-2.00647920233942,-1.75214967738872,
13.8561100121513));
#436179=CARTESIAN_POINT('Ctrl Pts',(-2.00660767580941,-1.75184575891194,
13.8562727473908));
#436180=CARTESIAN_POINT('Ctrl Pts',(-2.00674189004378,-1.7515412309017,
13.8564289040185));
#436181=CARTESIAN_POINT('Ctrl Pts',(-2.00735055006546,-1.75016019984948,
13.8571370725437));
#436182=CARTESIAN_POINT('Ctrl Pts',(-2.00809005697689,-1.74874327646846,
13.8577210840554));
#436183=CARTESIAN_POINT('Ctrl Pts',(-2.00895768371589,-1.74735911572998,
13.8581177131616));
#436184=CARTESIAN_POINT('Ctrl Pts',(-2.00920203726839,-1.74696928842465,
13.8582294175695));
#436185=CARTESIAN_POINT('Ctrl Pts',(-2.00945638696643,-1.74658199676585,
13.8583265086086));
#436186=CARTESIAN_POINT('Ctrl Pts',(-2.00972027094894,-1.74619859419274,
13.8584082369006));
#436187=CARTESIAN_POINT('Ctrl Pts',(-2.01009940146851,-1.74564774750865,
13.8585256585398));
#436188=CARTESIAN_POINT('Ctrl Pts',(-2.01050319248188,-1.74509826367057,
13.8586122832068));
#436189=CARTESIAN_POINT('Ctrl Pts',(-2.01092179101424,-1.74456488429777,
13.8586682984299));
#436190=CARTESIAN_POINT('Ctrl Pts',(-2.01125662834578,-1.74413823367172,
13.8587131050557));
#436191=CARTESIAN_POINT('Ctrl Pts',(-2.0116044539627,-1.74371703022565,
13.8587357943552));
#436192=CARTESIAN_POINT('Ctrl Pts',(-2.01196569970361,-1.74330154638619,
13.8587355499465));
#436193=CARTESIAN_POINT('Ctrl Pts',(-2.01219918143841,-1.74303300927519,
13.8587353919793));
#436194=CARTESIAN_POINT('Ctrl Pts',(-2.01243571519801,-1.74276973999133,
13.8587257282814));
#436195=CARTESIAN_POINT('Ctrl Pts',(-2.01267520976314,-1.74251162538801,
13.8587068136939));
#436196=CARTESIAN_POINT('Ctrl Pts',(-2.01267520976314,-1.74251162538801,
13.8587068136939));
#436197=CARTESIAN_POINT('Ctrl Pts',(-2.01346289433184,-1.74166270052876,
13.8586446046466));
#436198=CARTESIAN_POINT('Ctrl Pts',(-2.01428256745166,-1.74086946537878,
13.858482427929));
#436199=CARTESIAN_POINT('Ctrl Pts',(-2.0151313475361,-1.74012850198304,
13.8582284286032));
#436200=CARTESIAN_POINT('Ctrl Pts',(-2.01600209716854,-1.73936835973146,
13.8579678548414));
#436201=CARTESIAN_POINT('Ctrl Pts',(-2.0169066143356,-1.73866252724527,
13.857615680862));
#436202=CARTESIAN_POINT('Ctrl Pts',(-2.01780327804193,-1.73803119238542,
13.8571944833187));
#436203=CARTESIAN_POINT('Ctrl Pts',(-2.02004099402433,-1.73645563167503,
13.8561433417727));
#436204=CARTESIAN_POINT('Ctrl Pts',(-2.02233171101368,-1.73526642366871,
13.8546163505474));
#436205=CARTESIAN_POINT('Ctrl Pts',(-2.02448301494958,-1.7343878405908,
13.8528973491086));
#436206=CARTESIAN_POINT('Ctrl Pts',(-2.02487602643913,-1.73422733642475,
13.8525833129072));
#436207=CARTESIAN_POINT('Ctrl Pts',(-2.02526439821924,-1.73407705830097,
13.8522628768812));
#436208=CARTESIAN_POINT('Ctrl Pts',(-2.0256470012784,-1.73393637122879,
13.851937733538));
#436209=CARTESIAN_POINT('Ctrl Pts',(-2.02798350507697,-1.73307721479843,
13.8499521282529));
#436210=CARTESIAN_POINT('Ctrl Pts',(-2.0303384836145,-1.73249418838686,
13.847639871647));
#436211=CARTESIAN_POINT('Ctrl Pts',(-2.03256886071764,-1.73213994743128,
13.8452109780794));
#436212=CARTESIAN_POINT('Ctrl Pts',(-2.03357235354285,-1.73198056709294,
13.8441181685877));
#436213=CARTESIAN_POINT('Ctrl Pts',(-2.03455076298957,-1.73186679540193,
13.8430021611332));
#436214=CARTESIAN_POINT('Ctrl Pts',(-2.03549267416889,-1.73179143311325,
13.8418824960098));
#436215=CARTESIAN_POINT('Ctrl Pts',(-2.03771231191553,-1.73161383995553,
13.8392439765549));
#436216=CARTESIAN_POINT('Ctrl Pts',(-2.03983507346879,-1.7316372824372,
13.8364981347964));
#436217=CARTESIAN_POINT('Ctrl Pts',(-2.04186695060406,-1.7318276041125,
13.8336931113419));
#436218=CARTESIAN_POINT('Ctrl Pts',(-2.04384586989768,-1.7320129653377,
13.8309611966328));
#436219=CARTESIAN_POINT('Ctrl Pts',(-2.04574051097205,-1.7323573679165,
13.8281701127185));
#436220=CARTESIAN_POINT('Ctrl Pts',(-2.04753875983612,-1.73286437107488,
13.8253580685121));
#436221=CARTESIAN_POINT('Ctrl Pts',(-2.04792862213057,-1.73297428990679,
13.8247484142932));
#436222=CARTESIAN_POINT('Ctrl Pts',(-2.04831382179132,-1.73309196358275,
13.8241378483365));
#436223=CARTESIAN_POINT('Ctrl Pts',(-2.04869397153156,-1.7332176067911,
13.8235269408515));
#436224=CARTESIAN_POINT('',(-2.01184825284715,-1.74343840428094,12.5969504640361));
#436225=CARTESIAN_POINT('Origin',(-2.03793175060768,-1.76587765499918,12.584524458991));
#436226=CARTESIAN_POINT('Origin',(-2.03793175060768,-1.76587765499918,12.584524458991));
#436227=CARTESIAN_POINT('Ctrl Pts',(-2.00713550187734,-1.78117863747128,
12.5893111709658));
#436228=CARTESIAN_POINT('Ctrl Pts',(-2.00208344074157,-1.77103293331434,
12.5770542771492));
#436229=CARTESIAN_POINT('Ctrl Pts',(-2.01511564898405,-1.76113519502827,
12.5737548217797));
#436230=CARTESIAN_POINT('Ctrl Pts',(-2.01818266405917,-1.803363887463,12.5663937883685));
#436231=CARTESIAN_POINT('Ctrl Pts',(-2.01312415831784,-1.79320524105137,
12.5540940315304));
#436232=CARTESIAN_POINT('Ctrl Pts',(-2.02619869292755,-1.78327938894427,
12.5508374392248));
#436233=CARTESIAN_POINT('Ctrl Pts',(-2.02921867978978,-1.82552675280944,
12.5434499600945));
#436234=CARTESIAN_POINT('Ctrl Pts',(-2.02414372704488,-1.81533507702074,
12.5311293540533));
#436235=CARTESIAN_POINT('Ctrl Pts',(-2.03726985340451,-1.80540247558145,
12.5278936106989));
#436236=CARTESIAN_POINT('Ctrl Pts',(-2.04024442218595,-1.84766898693051,
12.5204817579905));
#436237=CARTESIAN_POINT('Ctrl Pts',(-2.03514435189319,-1.83742686931171,
12.5081597038247));
#436238=CARTESIAN_POINT('Ctrl Pts',(-2.04833004165538,-1.82750610168062,
12.5049254088044));
#436239=CARTESIAN_POINT('Ctrl Pts',(-2.03231742028997,-1.83174973854323,
12.5369868989719));
#436240=CARTESIAN_POINT('Ctrl Pts',(-2.03273263448266,-1.83258358405944,
12.5342545179733));
#436241=CARTESIAN_POINT('Ctrl Pts',(-2.03324056361785,-1.83332376316411,
12.5314872231885));
#436242=CARTESIAN_POINT('Ctrl Pts',(-2.03385868736767,-1.83389695086464,
12.5287124745063));
#436243=CARTESIAN_POINT('Ctrl Pts',(-2.03441614204618,-1.83441387998348,
12.5262100684184));
#436244=CARTESIAN_POINT('Ctrl Pts',(-2.0350633279729,-1.83479374668903,
12.5237004536639));
#436245=CARTESIAN_POINT('Ctrl Pts',(-2.03584491380172,-1.83498590330125,
12.5212220730815));
#436246=CARTESIAN_POINT('Ctrl Pts',(-2.03644328536625,-1.83513301581077,
12.5193246583486));
#436247=CARTESIAN_POINT('Ctrl Pts',(-2.03712773465973,-1.83517124914371,
12.517417831369));
#436248=CARTESIAN_POINT('Ctrl Pts',(-2.03792273333658,-1.83500650143566,
12.5155812248347));
#436249=CARTESIAN_POINT('Ctrl Pts',(-2.03826140704605,-1.8349363180265,
12.5147988205793));
#436250=CARTESIAN_POINT('Ctrl Pts',(-2.03862054333634,-1.83482949751477,
12.5140295443047));
#436251=CARTESIAN_POINT('Ctrl Pts',(-2.03900356490061,-1.83468024191474,
12.5132817086137));
#436252=CARTESIAN_POINT('Ctrl Pts',(-2.03958321622414,-1.83445436375493,
12.5121499604604));
#436253=CARTESIAN_POINT('Ctrl Pts',(-2.04022749179658,-1.83411975636767,
12.5110494206568));
#436254=CARTESIAN_POINT('Ctrl Pts',(-2.04093077446586,-1.83363960472413,
12.5100666561695));
#436255=CARTESIAN_POINT('Ctrl Pts',(-2.04133459775504,-1.8333639027561,
12.5095023550641));
#436256=CARTESIAN_POINT('Ctrl Pts',(-2.04176217361714,-1.83303648984005,
12.5089719619137));
#436257=CARTESIAN_POINT('Ctrl Pts',(-2.04220160452889,-1.83265843195989,
12.5085043804652));
#436258=CARTESIAN_POINT('Ctrl Pts',(-2.04284465442835,-1.83210519349779,
12.5078201359221));
#436259=CARTESIAN_POINT('Ctrl Pts',(-2.04353095422585,-1.83142653997754,
12.5072563000949));
#436260=CARTESIAN_POINT('Ctrl Pts',(-2.04420803018151,-1.83066245429082,
12.5068768744332));
#436261=CARTESIAN_POINT('Ctrl Pts',(-2.04469624855562,-1.83011149591086,
12.5066032824114));
#436262=CARTESIAN_POINT('Ctrl Pts',(-2.04518829329354,-1.82950647822802,
12.5064197834844));
#436263=CARTESIAN_POINT('Ctrl Pts',(-2.04565869272502,-1.82888281792614,
12.5063282718343));
#436264=CARTESIAN_POINT('Ctrl Pts',(-2.046345330263,-1.82797246696574,12.5061946931565));
#436265=CARTESIAN_POINT('Ctrl Pts',(-2.04700137231097,-1.82700357620241,
12.5062515701262));
#436266=CARTESIAN_POINT('Ctrl Pts',(-2.0475989089795,-1.82604494720823,
12.5064436508398));
#436267=CARTESIAN_POINT('',(-2.01511564898405,-1.76113519502827,12.5737548217797));
#436268=CARTESIAN_POINT('Origin',(-2.02682901625738,-1.77137223694085,12.5893111709658));
#436269=CARTESIAN_POINT('Ctrl Pts',(-2.0475989089795,-1.82604494720823,
12.5064436508398));
#436270=CARTESIAN_POINT('Ctrl Pts',(-2.04279097221024,-1.81643640248107,
12.5164271754438));
#436271=CARTESIAN_POINT('Ctrl Pts',(-2.03798094272672,-1.80682414242484,
12.5264061185523));
#436272=CARTESIAN_POINT('Ctrl Pts',(-2.03316874767174,-1.79720803576523,
12.536380305637));
#436273=CARTESIAN_POINT('Ctrl Pts',(-2.02715447987134,-1.7851898527973,
12.5488460165097));
#436274=CARTESIAN_POINT('Ctrl Pts',(-2.02113682766512,-1.77316565792249,
12.5613043021964));
#436275=CARTESIAN_POINT('Ctrl Pts',(-2.01511564898405,-1.76113519502827,
12.5737548217797));
#436276=CARTESIAN_POINT('Ctrl Pts',(-2.04869397153156,-1.7332176067911,
12.5893111709658));
#436277=CARTESIAN_POINT('Ctrl Pts',(-2.03793255275056,-1.72966085259949,
12.5770542771492));
#436278=CARTESIAN_POINT('Ctrl Pts',(-2.02999023577725,-1.7439690067764,
12.5737548217797));
#436279=CARTESIAN_POINT('Ctrl Pts',(-2.03865366140676,-1.72989918606534,
12.5928319619712));
#436280=CARTESIAN_POINT('Ctrl Pts',(-2.03039899825379,-1.73060200368204,
12.5821634970843));
#436281=CARTESIAN_POINT('Ctrl Pts',(-2.02633575586776,-1.74275122438183,
12.5773203894503));
#436282=CARTESIAN_POINT('Ctrl Pts',(-2.02200618152989,-1.73175539539853,
12.5969440695591));
#436283=CARTESIAN_POINT('Ctrl Pts',(-2.01936000917948,-1.73478133565634,
12.5878292599214));
#436284=CARTESIAN_POINT('Ctrl Pts',(-2.02040248106055,-1.74341484864271,
12.5813877129824));
#436285=CARTESIAN_POINT('Ctrl Pts',(-2.00192869816824,-1.75484370212301,
12.596957478804));
#436286=CARTESIAN_POINT('Ctrl Pts',(-2.0045553749358,-1.75184017714266,
12.5878468778671));
#436287=CARTESIAN_POINT('Ctrl Pts',(-2.01322097269373,-1.75168238793089,
12.5814011370086));
#436288=CARTESIAN_POINT('Ctrl Pts',(-2.002415128742,-1.77169903933225,12.5928371701607));
#436289=CARTESIAN_POINT('Ctrl Pts',(-2.00194242356592,-1.76343395521167,
12.5821692192952));
#436290=CARTESIAN_POINT('Ctrl Pts',(-2.01338442992461,-1.75768032049477,
12.5773318885715));
#436291=CARTESIAN_POINT('Ctrl Pts',(-2.00713550187729,-1.7811786374713,
12.5893111709658));
#436292=CARTESIAN_POINT('Ctrl Pts',(-2.00208344074152,-1.77103293331436,
12.5770542771492));
#436293=CARTESIAN_POINT('Ctrl Pts',(-2.015115648984,-1.76113519502829,12.5737548217797));
#436294=CARTESIAN_POINT('',(-2.02999023577725,-1.7439690067764,12.5737548217797));
#436295=CARTESIAN_POINT('Origin',(-2.0417900653329,-1.75410626589599,12.5893111709658));
#436296=CARTESIAN_POINT('Ctrl Pts',(-2.015115648984,-1.76113519502829,12.5737548217797));
#436297=CARTESIAN_POINT('Ctrl Pts',(-2.01463992030744,-1.76025315089259,
12.5746934679442));
#436298=CARTESIAN_POINT('Ctrl Pts',(-2.01427472362832,-1.75919015191621,
12.5756680099006));
#436299=CARTESIAN_POINT('Ctrl Pts',(-2.01405845862531,-1.75806821915688,
12.5765688348656));
#436300=CARTESIAN_POINT('Ctrl Pts',(-2.01400120485989,-1.75777119987905,
12.5768073183026));
#436301=CARTESIAN_POINT('Ctrl Pts',(-2.01395415622715,-1.75747015875835,
12.5770407398754));
#436302=CARTESIAN_POINT('Ctrl Pts',(-2.013917471392,-1.75716746193681,12.5772674179684));
#436303=CARTESIAN_POINT('Ctrl Pts',(-2.01376692674856,-1.75592527603386,
12.5781976435658));
#436304=CARTESIAN_POINT('Ctrl Pts',(-2.01379356207557,-1.75458329688271,
12.5790594849312));
#436305=CARTESIAN_POINT('Ctrl Pts',(-2.01404385859131,-1.75323309527633,
12.5797571720116));
#436306=CARTESIAN_POINT('Ctrl Pts',(-2.01420693577118,-1.75235339038084,
12.580211740231));
#436307=CARTESIAN_POINT('Ctrl Pts',(-2.01449082634906,-1.75143363871864,
12.5806009430798));
#436308=CARTESIAN_POINT('Ctrl Pts',(-2.01489247429766,-1.75054381199972,
12.5808812374708));
#436309=CARTESIAN_POINT('Ctrl Pts',(-2.01523762313082,-1.74977915565123,
12.5811221033394));
#436310=CARTESIAN_POINT('Ctrl Pts',(-2.01567690016029,-1.74902098980917,
12.581287365893));
#436311=CARTESIAN_POINT('Ctrl Pts',(-2.01619272639188,-1.74831628662182,
12.581359338449));
#436312=CARTESIAN_POINT('Ctrl Pts',(-2.01626441558667,-1.74821834743035,
12.5813693411482));
#436313=CARTESIAN_POINT('Ctrl Pts',(-2.01633754958212,-1.74812139143585,
12.5813775999465));
#436314=CARTESIAN_POINT('Ctrl Pts',(-2.01641204749879,-1.74802549346873,
12.5813841266931));
#436315=CARTESIAN_POINT('Ctrl Pts',(-2.01653844222476,-1.7478627909689,
12.5813952001081));
#436316=CARTESIAN_POINT('Ctrl Pts',(-2.01667009039135,-1.74770241785286,
12.5814007534795));
#436317=CARTESIAN_POINT('Ctrl Pts',(-2.01680708709116,-1.74754456909587,
12.5814005856065));
#436318=CARTESIAN_POINT('Ctrl Pts',(-2.0174342044207,-1.7468219992012,12.5813998171494));
#436319=CARTESIAN_POINT('Ctrl Pts',(-2.01812981373364,-1.74620202881124,
12.58127954464));
#436320=CARTESIAN_POINT('Ctrl Pts',(-2.01887027844383,-1.74566608840401,
12.5810700125799));
#436321=CARTESIAN_POINT('Ctrl Pts',(-2.01976467550507,-1.74501873341378,
12.5808169217085));
#436322=CARTESIAN_POINT('Ctrl Pts',(-2.02073440968425,-1.74450747615839,
12.5804173076348));
#436323=CARTESIAN_POINT('Ctrl Pts',(-2.02168234978333,-1.74415408553003,
12.5799304713245));
#436324=CARTESIAN_POINT('Ctrl Pts',(-2.02285714619801,-1.74371612321196,
12.5793271277669));
#436325=CARTESIAN_POINT('Ctrl Pts',(-2.02406009577564,-1.74346328903295,
12.5785808224116));
#436326=CARTESIAN_POINT('Ctrl Pts',(-2.02523396820987,-1.74337520174007,
12.5777485681082));
#436327=CARTESIAN_POINT('Ctrl Pts',(-2.02698316674419,-1.74324394202301,
12.576508418016));
#436328=CARTESIAN_POINT('Ctrl Pts',(-2.02865255875168,-1.74347274288858,
12.5750928681475));
#436329=CARTESIAN_POINT('Ctrl Pts',(-2.02999023577725,-1.7439690067764,
12.5737548217797));
#436330=CARTESIAN_POINT('Ctrl Pts',(-2.02999023577725,-1.7439690067764,
12.5737548217797));
#436331=CARTESIAN_POINT('Ctrl Pts',(-2.03793255275056,-1.72966085259949,
12.5770542771492));
#436332=CARTESIAN_POINT('Ctrl Pts',(-2.04869397153156,-1.7332176067911,
12.5893111709658));
#436333=CARTESIAN_POINT('Ctrl Pts',(-2.05348278542143,-1.7517866192883,
12.5508408821982));
#436334=CARTESIAN_POINT('Ctrl Pts',(-2.06144689991941,-1.73743257439174,
12.55409748406));
#436335=CARTESIAN_POINT('Ctrl Pts',(-2.07222204751465,-1.74099386609078,
12.5663972313419));
#436336=CARTESIAN_POINT('Ctrl Pts',(-2.07695275823144,-1.75959547580437,
12.52790050457));
#436337=CARTESIAN_POINT('Ctrl Pts',(-2.08491621151662,-1.74518941148699,
12.5311362602938));
#436338=CARTESIAN_POINT('Ctrl Pts',(-2.09572638753523,-1.74876228042263,
12.5434568539655));
#436339=CARTESIAN_POINT('Ctrl Pts',(-2.10040191308955,-1.76739624363818,
12.5049357605811));
#436340=CARTESIAN_POINT('Ctrl Pts',(-2.10834518227021,-1.7529329155387,
12.5081700652078));
#436341=CARTESIAN_POINT('Ctrl Pts',(-2.11920885059873,-1.75652346420613,
12.5204921097672));
#436342=CARTESIAN_POINT('Ctrl Pts',(-2.09886215016469,-1.76688401313815,
12.5064436508395));
#436343=CARTESIAN_POINT('Ctrl Pts',(-2.09979524624555,-1.76609776922277,
12.5062361689309));
#436344=CARTESIAN_POINT('Ctrl Pts',(-2.10073206262496,-1.76524035060173,
12.5061871075061));
#436345=CARTESIAN_POINT('Ctrl Pts',(-2.10159076052644,-1.76436077425194,
12.5063648335164));
#436346=CARTESIAN_POINT('Ctrl Pts',(-2.10198083407998,-1.76396121641935,
12.5064455676329));
#436347=CARTESIAN_POINT('Ctrl Pts',(-2.1023600706676,-1.76355135935368,
12.506574497099));
#436348=CARTESIAN_POINT('Ctrl Pts',(-2.10271143837214,-1.76314806273744,
12.5067492519495));
#436349=CARTESIAN_POINT('Ctrl Pts',(-2.10341752541355,-1.76233762253225,
12.5071004286051));
#436350=CARTESIAN_POINT('Ctrl Pts',(-2.10403642198906,-1.76152334714826,
12.5076537929613));
#436351=CARTESIAN_POINT('Ctrl Pts',(-2.10452920691249,-1.760772075649,12.5083435010505));
#436352=CARTESIAN_POINT('Ctrl Pts',(-2.10456023066832,-1.7607247786185,
12.5083869222964));
#436353=CARTESIAN_POINT('Ctrl Pts',(-2.10459074798995,-1.76067771959725,
12.5084308732337));
#436354=CARTESIAN_POINT('Ctrl Pts',(-2.10462074682411,-1.76063091030325,
12.5084753333615));
#436355=CARTESIAN_POINT('Ctrl Pts',(-2.10486137706898,-1.76025543798268,
12.5088319622689));
#436356=CARTESIAN_POINT('Ctrl Pts',(-2.10507461837437,-1.75988910689663,
12.509227847131));
#436357=CARTESIAN_POINT('Ctrl Pts',(-2.1052565498896,-1.75954421861582,
12.5096423454524));
#436358=CARTESIAN_POINT('Ctrl Pts',(-2.10582664273882,-1.75846349138493,
12.5109411997424));
#436359=CARTESIAN_POINT('Ctrl Pts',(-2.10613291514583,-1.75753135443021,
12.5124831113042));
#436360=CARTESIAN_POINT('Ctrl Pts',(-2.10626956663698,-1.75673873545148,
12.5140723025008));
#436361=CARTESIAN_POINT('Ctrl Pts',(-2.10628237103138,-1.75666446618504,
12.5142212114565));
#436362=CARTESIAN_POINT('Ctrl Pts',(-2.10629371276419,-1.75659140885369,
12.5143705582413));
#436363=CARTESIAN_POINT('Ctrl Pts',(-2.10630368520137,-1.75651954994667,
12.5145201959299));
#436364=CARTESIAN_POINT('Ctrl Pts',(-2.10643179600443,-1.75559641529929,
12.5164425148273));
#436365=CARTESIAN_POINT('Ctrl Pts',(-2.10634895468274,-1.75484090547488,
12.518463520594));
#436366=CARTESIAN_POINT('Ctrl Pts',(-2.10612736020703,-1.75419893454944,
12.5205025929157));
#436367=CARTESIAN_POINT('Ctrl Pts',(-2.10599882662793,-1.75382656596732,
12.5216853356836));
#436368=CARTESIAN_POINT('Ctrl Pts',(-2.10582429938244,-1.75349291196221,
12.5228750347131));
#436369=CARTESIAN_POINT('Ctrl Pts',(-2.10562113908398,-1.75319235624078,
12.5240609649613));
#436370=CARTESIAN_POINT('Ctrl Pts',(-2.10512249303057,-1.75245465834681,
12.5269717671327));
#436371=CARTESIAN_POINT('Ctrl Pts',(-2.10442870606012,-1.75190141461407,
12.5299036066169));
#436372=CARTESIAN_POINT('Ctrl Pts',(-2.10360399699103,-1.7514744402852,
12.5328133004019));
#436373=CARTESIAN_POINT('Ctrl Pts',(-2.1032080886165,-1.75126946774538,
12.5342101228452));
#436374=CARTESIAN_POINT('Ctrl Pts',(-2.1027822615005,-1.7510943158857,12.5356023438238));
#436375=CARTESIAN_POINT('Ctrl Pts',(-2.10233409235841,-1.75094619151327,
12.5369868989719));
#436376=CARTESIAN_POINT('Origin',(-14.20522036749,-5.7454903392375,-1.23974147293322));
#436377=CARTESIAN_POINT('Ctrl Pts',(-2.03229875515483,-1.83171234370852,
12.5369868989719));
#436378=CARTESIAN_POINT('Ctrl Pts',(-2.03916209416162,-1.84543013804155,
12.5369868989719));
#436379=CARTESIAN_POINT('Ctrl Pts',(-2.02866372722115,-1.85661350047279,
12.5369868989719));
#436380=CARTESIAN_POINT('Ctrl Pts',(-2.03461877294864,-1.83634952431904,
12.5218025310016));
#436381=CARTESIAN_POINT('Ctrl Pts',(-2.03672795412435,-1.84797738820165,
12.5216901060418));
#436382=CARTESIAN_POINT('Ctrl Pts',(-2.02869574174667,-1.85657942116523,
12.5161920673677));
#436383=CARTESIAN_POINT('Ctrl Pts',(-2.0405707567139,-1.83730344279213,
12.5042015548895));
#436384=CARTESIAN_POINT('Ctrl Pts',(-2.04052280449143,-1.84373578650199,
12.4980677368513));
#436385=CARTESIAN_POINT('Ctrl Pts',(-2.03596183033724,-1.84877446633788,
12.4907278922778));
#436386=CARTESIAN_POINT('Ctrl Pts',(-2.04758398157485,-1.82603163496219,
12.506463626192));
#436387=CARTESIAN_POINT('Ctrl Pts',(-2.05246702543131,-1.83038632450706,
12.4999376786891));
#436388=CARTESIAN_POINT('Ctrl Pts',(-2.05240738615054,-1.83033313830599,
12.4906970594712));
#436389=CARTESIAN_POINT('Origin',(-2.01262390590993,-1.84155613907365,12.5369868989719));
#436390=CARTESIAN_POINT('Origin',(-2.01262390590993,-1.84155613907365,14.));
#436391=CARTESIAN_POINT('Origin',(-2.01262390590993,-1.84155613907365,13.7435492065112));
#436392=CARTESIAN_POINT('Ctrl Pts',(-2.02128069158676,-1.8095855022959,
13.793642941384));
#436393=CARTESIAN_POINT('Ctrl Pts',(-2.02612458608051,-1.819252089343,13.8071662555867));
#436394=CARTESIAN_POINT('Ctrl Pts',(-2.01218638534816,-1.82903707498322,
13.8103758687955));
#436395=CARTESIAN_POINT('Ctrl Pts',(-2.02868948434669,-1.82446406052789,
13.7804579775006));
#436396=CARTESIAN_POINT('Ctrl Pts',(-2.03465734610451,-1.83639629827982,
13.7901904343351));
#436397=CARTESIAN_POINT('Ctrl Pts',(-2.02339634547535,-1.84741654278687,
13.7927914348262));
#436398=CARTESIAN_POINT('Ctrl Pts',(-2.03305131943469,-1.8332236277192,
13.7597120340895));
#436399=CARTESIAN_POINT('Ctrl Pts',(-2.03995269102682,-1.84703515044914,
13.7635825532445));
#436400=CARTESIAN_POINT('Ctrl Pts',(-2.02998502261937,-1.85826820447123,
13.7651073818884));
#436401=CARTESIAN_POINT('Ctrl Pts',(-2.03219717224905,-1.8315083038922,
13.7381884353898));
#436402=CARTESIAN_POINT('Ctrl Pts',(-2.03893780842326,-1.84499614043455,
13.7368803041982));
#436403=CARTESIAN_POINT('Ctrl Pts',(-2.02869434139341,-1.85614338315763,
13.7363986145813));
#436404=CARTESIAN_POINT('Origin',(-2.00338493120097,-1.82300214663542,13.7902182540695));
#436405=CARTESIAN_POINT('Ctrl Pts',(-2.00713374665534,-1.7811751142832,
13.8235227101244));
#436406=CARTESIAN_POINT('Ctrl Pts',(-2.01226248321911,-1.79146485429833,
13.8358800583119));
#436407=CARTESIAN_POINT('Ctrl Pts',(-1.99899831538416,-1.80139903270938,
13.8390832900376));
#436408=CARTESIAN_POINT('Ctrl Pts',(-2.01245041122361,-1.79185220317311,
13.8124254819052));
#436409=CARTESIAN_POINT('Ctrl Pts',(-2.01758910747214,-1.80216192584157,
13.8247886449157));
#436410=CARTESIAN_POINT('Ctrl Pts',(-2.0042979624152,-1.81209501419199,
13.8279860620657));
#436411=CARTESIAN_POINT('Ctrl Pts',(-2.0177646930358,-1.80252450693912,
13.8013225099955));
#436412=CARTESIAN_POINT('Ctrl Pts',(-2.02291092612378,-1.81284934683313,
13.8136962257787));
#436413=CARTESIAN_POINT('Ctrl Pts',(-2.00959539884781,-1.82278592362019,
13.8168830918626));
#436414=CARTESIAN_POINT('Ctrl Pts',(-2.0230766848013,-1.81319221176308,
13.7902140179785));
#436415=CARTESIAN_POINT('Ctrl Pts',(-2.02822819023148,-1.82352762144762,
13.802602731458));
#436416=CARTESIAN_POINT('Ctrl Pts',(-2.01489071319075,-1.8334719594703,
13.8057746032558));
#436417=CARTESIAN_POINT('Origin',(-1.9874419874973,-1.7909850380017,13.8235269408515));
#436418=CARTESIAN_POINT('Ctrl Pts',(-2.04869397153156,-1.7332176067911,
13.8235269408515));
#436419=CARTESIAN_POINT('Ctrl Pts',(-2.05990499223275,-1.73692295881603,
13.8362179249168));
#436420=CARTESIAN_POINT('Ctrl Pts',(-2.06781651354226,-1.72178787260463,
13.8391868794938));
#436421=CARTESIAN_POINT('Ctrl Pts',(-2.03843637557668,-1.72982737097268,
13.8400110824519));
#436422=CARTESIAN_POINT('Ctrl Pts',(-2.04849842866773,-1.72954997152324,
13.8494522556837));
#436423=CARTESIAN_POINT('Ctrl Pts',(-2.05090014724273,-1.71631518269521,
13.85569149686));
#436424=CARTESIAN_POINT('Ctrl Pts',(-2.02223093111772,-1.73149509275204,
13.8586819406588));
#436425=CARTESIAN_POINT('Ctrl Pts',(-2.02509259560658,-1.7282137942304,
13.868010383617));
#436426=CARTESIAN_POINT('Ctrl Pts',(-2.02401373350842,-1.71922886666443,
13.8744918421245));
#436427=CARTESIAN_POINT('Ctrl Pts',(-2.00170044877093,-1.7551080297264,
13.8587686893867));
#436428=CARTESIAN_POINT('Ctrl Pts',(-1.99886421063234,-1.7583600877119,
13.8680909899357));
#436429=CARTESIAN_POINT('Ctrl Pts',(-1.98983845114073,-1.75853916061699,
13.8745789365163));
#436430=CARTESIAN_POINT('Ctrl Pts',(-2.00231212963259,-1.77149219337558,
13.8400379222776));
#436431=CARTESIAN_POINT('Ctrl Pts',(-2.00346212723657,-1.78148958000506,
13.8494748685453));
#436432=CARTESIAN_POINT('Ctrl Pts',(-1.99071008809211,-1.7857494629755,
13.8557104837033));
#436433=CARTESIAN_POINT('Ctrl Pts',(-2.00713550187136,-1.78117863747409,
13.8235269408542));
#436434=CARTESIAN_POINT('Ctrl Pts',(-2.01239863335326,-1.79174821957533,
13.8362179249195));
#436435=CARTESIAN_POINT('Ctrl Pts',(-1.99854352737215,-1.80173316035175,
13.8391868794965));
#436436=CARTESIAN_POINT('Origin',(-2.05559787773022,-1.71232894768622,13.8235269408515));
#436437=CARTESIAN_POINT('Ctrl Pts',(-2.08265036614452,-1.74444052662317,
13.7902140241682));
#436438=CARTESIAN_POINT('Ctrl Pts',(-2.09361370960642,-1.74806870736962,
13.8026027327198));
#436439=CARTESIAN_POINT('Ctrl Pts',(-2.10155870455742,-1.73345176557244,
13.8057746032556));
#436440=CARTESIAN_POINT('Ctrl Pts',(-2.07133526792135,-1.74070077596011,
13.8013225161808));
#436441=CARTESIAN_POINT('Ctrl Pts',(-2.08228739884563,-1.7443252422798,
13.8136962270464));
#436442=CARTESIAN_POINT('Ctrl Pts',(-2.09022783533951,-1.72973113135793,
13.8168830918628));
#436443=CARTESIAN_POINT('Ctrl Pts',(-2.06001529165748,-1.73695941305689,
13.8124254880875));
#436444=CARTESIAN_POINT('Ctrl Pts',(-2.07095138662803,-1.74057857067098,
13.8247886461868));
#436445=CARTESIAN_POINT('Ctrl Pts',(-2.07889184014546,-1.72600909023632,
13.8279860620656));
#436446=CARTESIAN_POINT('Ctrl Pts',(-2.04869023987082,-1.73321637264375,
13.8235227163065));
#436447=CARTESIAN_POINT('Ctrl Pts',(-2.05960513818058,-1.73682851579214,
13.8358800595847));
#436448=CARTESIAN_POINT('Ctrl Pts',(-2.06755050992176,-1.72228558284544,
13.8390832900376));
#436449=CARTESIAN_POINT('Origin',(-2.08955801581769,-1.72355310557363,13.7902182540695));
#436450=CARTESIAN_POINT('Ctrl Pts',(-2.1020778732194,-1.75086147952906,
13.7382347919292));
#436451=CARTESIAN_POINT('Ctrl Pts',(-2.11639835196728,-1.75561981507471,
13.7369371795943));
#436452=CARTESIAN_POINT('Ctrl Pts',(-2.12597531008095,-1.74387989811122,
13.7364597369711));
#436453=CARTESIAN_POINT('Ctrl Pts',(-2.10387387868557,-1.75145507733044,
13.7595490285574));
#436454=CARTESIAN_POINT('Ctrl Pts',(-2.11853634881506,-1.75632598855121,
13.7633824266926));
#436455=CARTESIAN_POINT('Ctrl Pts',(-2.12823402390517,-1.74484344710107,
13.7648920890506));
#436456=CARTESIAN_POINT('Ctrl Pts',(-2.09471434919886,-1.7484277610709,
13.7803806590111));
#436457=CARTESIAN_POINT('Ctrl Pts',(-2.10739515913211,-1.75264604809777,
13.7901039518744));
#436458=CARTESIAN_POINT('Ctrl Pts',(-2.11671739735761,-1.73993458414225,
13.7926933640892));
#436459=CARTESIAN_POINT('Ctrl Pts',(-2.07879304231111,-1.74316560955667,
13.7936647693663));
#436460=CARTESIAN_POINT('Ctrl Pts',(-2.08905267138956,-1.74658808572421,
13.8072068914933));
#436461=CARTESIAN_POINT('Ctrl Pts',(-2.09675332388845,-1.73137808174858,
13.8104111085397));
#436462=CARTESIAN_POINT('Origin',(-2.10923799855707,-1.73005753240838,13.7435492065112));
#436463=CARTESIAN_POINT('Origin',(-2.10923799855707,-1.73005753240838,14.));
#436464=CARTESIAN_POINT('Origin',(-2.10923799855707,-1.73005753240838,12.5369868989719));
#436465=CARTESIAN_POINT('Ctrl Pts',(-2.09884808670359,-1.76687217411561,
12.506462012331));
#436466=CARTESIAN_POINT('Ctrl Pts',(-2.10385023214597,-1.77108312756622,
12.4999388158272));
#436467=CARTESIAN_POINT('Ctrl Pts',(-2.10379105020547,-1.77103330646457,
12.4907030323752));
#436468=CARTESIAN_POINT('Ctrl Pts',(-2.10900548446784,-1.7583249023981,
12.5042014951932));
#436469=CARTESIAN_POINT('Ctrl Pts',(-2.11536288838638,-1.75736338665051,
12.4980716682127));
#436470=CARTESIAN_POINT('Ctrl Pts',(-2.11969933163196,-1.7521364539741,
12.4907355092744));
#436471=CARTESIAN_POINT('Ctrl Pts',(-2.10721671805287,-1.75256938192137,
12.5218047446509));
#436472=CARTESIAN_POINT('Ctrl Pts',(-2.11902064230432,-1.75300094095711,
12.5216906929434));
#436473=CARTESIAN_POINT('Ctrl Pts',(-2.12639117764129,-1.74383328241327,
12.5161988840775));
#436474=CARTESIAN_POINT('Ctrl Pts',(-2.10229762738049,-1.75093410415595,
12.5369868989719));
#436475=CARTESIAN_POINT('Ctrl Pts',(-2.11684469789254,-1.75577024632078,
12.5369868989719));
#436476=CARTESIAN_POINT('Ctrl Pts',(-2.12641929923131,-1.74379808942553,
12.5369868989719));
#436477=CARTESIAN_POINT('Origin',(-3.8935179680156E-31,-8.52561512546645E-31,
12.5));
#436478=CARTESIAN_POINT('Origin',(-1.90060378598595,-1.89443804601162,12.5));
#436479=CARTESIAN_POINT('',(-1.90060378598595,-1.89443804601162,12.5893111709658));
#436480=CARTESIAN_POINT('',(-1.90060378598595,-1.89443804601162,13.8235269408515));
#436481=CARTESIAN_POINT('',(-1.90060378598595,-1.89443804601162,12.5));
#436482=CARTESIAN_POINT('',(-1.93353605144762,-1.90839292296425,13.7902182540695));
#436483=CARTESIAN_POINT('',(-1.90060378598595,-1.89443804601162,13.8235269408515));
#436484=CARTESIAN_POINT('',(-1.95262037949673,-1.9164798081486,13.7435492065112));
#436485=CARTESIAN_POINT('Origin',(-1.88983306537385,-1.88987436272198,13.7445212918695));
#436486=CARTESIAN_POINT('',(-1.95262037949673,-1.9164798081486,12.5369868989719));
#436487=CARTESIAN_POINT('',(-1.95262037949673,-1.9164798081486,12.5));
#436488=CARTESIAN_POINT('Ctrl Pts',(-1.95262037949673,-1.9164798081486,
12.5369868989719));
#436489=CARTESIAN_POINT('Ctrl Pts',(-1.93529416090633,-1.90913791274317,
12.5544431401645));
#436490=CARTESIAN_POINT('Ctrl Pts',(-1.9179555501439,-1.90179076621901,
12.5718848856037));
#436491=CARTESIAN_POINT('Ctrl Pts',(-1.90060378598595,-1.89443804601162,
12.5893111709658));
#436492=CARTESIAN_POINT('Origin',(-1.95738140813714,-2.19419332069378,12.5));
#436493=CARTESIAN_POINT('',(-1.87625044290217,-1.99130747926499,13.7435492065112));
#436494=CARTESIAN_POINT('',(-1.86855453274996,-1.97206216149676,13.7902182540695));
#436495=CARTESIAN_POINT('Origin',(-1.84833101098961,-1.92148879265888,13.7418732680436));
#436496=CARTESIAN_POINT('',(-1.85527432946225,-1.93885208923188,13.8235269408515));
#436497=CARTESIAN_POINT('',(-1.86855453274996,-1.97206216149676,13.7902182540695));
#436498=CARTESIAN_POINT('',(-1.85527432946225,-1.93885208923188,12.5893111709658));
#436499=CARTESIAN_POINT('',(-1.85527432946225,-1.93885208923188,12.5));
#436500=CARTESIAN_POINT('',(-1.87625044290217,-1.99130747926499,12.5369868989719));
#436501=CARTESIAN_POINT('Ctrl Pts',(-1.85527432946225,-1.93885208923188,
12.5893111709658));
#436502=CARTESIAN_POINT('Ctrl Pts',(-1.86227156916585,-1.95635022771492,
12.5718848856037));
#436503=CARTESIAN_POINT('Ctrl Pts',(-1.86926350465598,-1.97383510184432,
12.5544431401645));
#436504=CARTESIAN_POINT('Ctrl Pts',(-1.87625044290217,-1.99130747926499,
12.5369868989719));
#436505=CARTESIAN_POINT('',(-1.87625044290217,-1.99130747926499,12.5));
#436506=CARTESIAN_POINT('Origin',(-1.88719198339499,-1.92608870439752,12.5));
#436507=CARTESIAN_POINT('',(-1.86394732487897,-1.90076527606225,13.8587068136939));
#436508=CARTESIAN_POINT('Ctrl Pts',(-1.85527432945606,-1.9388520892342,
13.8235269408542));
#436509=CARTESIAN_POINT('Ctrl Pts',(-1.8546237037719,-1.93722505646064,
13.8262006681044));
#436510=CARTESIAN_POINT('Ctrl Pts',(-1.85411920277279,-1.9354955169919,
13.8288634856214));
#436511=CARTESIAN_POINT('Ctrl Pts',(-1.85375081465725,-1.93367227820437,
13.8314912288862));
#436512=CARTESIAN_POINT('Ctrl Pts',(-1.8533710445076,-1.93179270707279,
13.8342001611531));
#436513=CARTESIAN_POINT('Ctrl Pts',(-1.85313501922478,-1.92981156781484,
13.8368750301949));
#436514=CARTESIAN_POINT('Ctrl Pts',(-1.85306775932398,-1.92771116184849,
13.8394886372969));
#436515=CARTESIAN_POINT('Ctrl Pts',(-1.85306256467869,-1.92754894240083,
13.8396904925131));
#436516=CARTESIAN_POINT('Ctrl Pts',(-1.85305839837702,-1.92738600703313,
13.8398919674349));
#436517=CARTESIAN_POINT('Ctrl Pts',(-1.85305528331088,-1.9272223462534,
13.8400930404591));
#436518=CARTESIAN_POINT('Ctrl Pts',(-1.85300674848469,-1.92467240119966,
13.8432258934518));
#436519=CARTESIAN_POINT('Ctrl Pts',(-1.8532125311784,-1.92195938989007,
13.8462331177034));
#436520=CARTESIAN_POINT('Ctrl Pts',(-1.85376210985766,-1.91917909219397,
13.8489036603661));
#436521=CARTESIAN_POINT('Ctrl Pts',(-1.85394193839728,-1.91826934643186,
13.8497774930041));
#436522=CARTESIAN_POINT('Ctrl Pts',(-1.85415867005854,-1.91735262817441,
13.85061494757));
#436523=CARTESIAN_POINT('Ctrl Pts',(-1.85441569628117,-1.91643295907823,
13.8514076489583));
#436524=CARTESIAN_POINT('Ctrl Pts',(-1.85495934381076,-1.91448772630367,
13.8530843267192));
#436525=CARTESIAN_POINT('Ctrl Pts',(-1.85573951183846,-1.91233901507234,
13.8546805203176));
#436526=CARTESIAN_POINT('Ctrl Pts',(-1.85683917310503,-1.91015810289246,
13.8559412814273));
#436527=CARTESIAN_POINT('Ctrl Pts',(-1.85698634344535,-1.90986622611413,
13.8561100121513));
#436528=CARTESIAN_POINT('Ctrl Pts',(-1.85713916160777,-1.90957379068151,
13.8562727473908));
#436529=CARTESIAN_POINT('Ctrl Pts',(-1.85729775111527,-1.9092812156692,
13.8564289040185));
#436530=CARTESIAN_POINT('Ctrl Pts',(-1.85801695272257,-1.90795439132617,
13.8571370725437));
#436531=CARTESIAN_POINT('Ctrl Pts',(-1.85886949139538,-1.90660245931935,
13.8577210840553));
#436532=CARTESIAN_POINT('Ctrl Pts',(-1.85984705312809,-1.90529362389541,
13.8581177131616));
#436533=CARTESIAN_POINT('Ctrl Pts',(-1.86012236815867,-1.90492501079129,
13.8582294175695));
#436534=CARTESIAN_POINT('Ctrl Pts',(-1.8604074393947,-1.90455973967519,
13.8583265086086));
#436535=CARTESIAN_POINT('Ctrl Pts',(-1.86070169619407,-1.90419912183687,
13.8584082369006));
#436536=CARTESIAN_POINT('Ctrl Pts',(-1.86112446430668,-1.9036810107067,
13.8585256585398));
#436537=CARTESIAN_POINT('Ctrl Pts',(-1.86157169977273,-1.90316626794696,
13.8586122832068));
#436538=CARTESIAN_POINT('Ctrl Pts',(-1.86203238082353,-1.90266878301648,
13.8586682984299));
#436539=CARTESIAN_POINT('Ctrl Pts',(-1.86240087999833,-1.9022708443862,
13.8587131050557));
#436540=CARTESIAN_POINT('Ctrl Pts',(-1.86278188024532,-1.90187939347669,
13.8587357943552));
#436541=CARTESIAN_POINT('Ctrl Pts',(-1.8631757897609,-1.90149473700695,
13.8587355499465));
#436542=CARTESIAN_POINT('Ctrl Pts',(-1.86343038287205,-1.90124612435993,
13.8587353919793));
#436543=CARTESIAN_POINT('Ctrl Pts',(-1.86368758847582,-1.90100301078014,
13.8587257282814));
#436544=CARTESIAN_POINT('Ctrl Pts',(-1.86394732487897,-1.90076527606225,
13.8587068136939));
#436545=CARTESIAN_POINT('Ctrl Pts',(-1.86394732487897,-1.90076527606225,
13.8587068136939));
#436546=CARTESIAN_POINT('Ctrl Pts',(-1.86480158374928,-1.89998337953533,
13.8586446046466));
#436547=CARTESIAN_POINT('Ctrl Pts',(-1.86568318550313,-1.89925959477865,
13.858482427929));
#436548=CARTESIAN_POINT('Ctrl Pts',(-1.86658953673735,-1.89859028033409,
13.8582284286032));
#436549=CARTESIAN_POINT('Ctrl Pts',(-1.86751934767254,-1.89790364157183,
13.8579678548414));
#436550=CARTESIAN_POINT('Ctrl Pts',(-1.86847838703359,-1.89727388423125,
13.857615680862));
#436551=CARTESIAN_POINT('Ctrl Pts',(-1.86942352681752,-1.89671773650235,
13.8571944833187));
#436552=CARTESIAN_POINT('Ctrl Pts',(-1.87178221980925,-1.89532981296677,
13.8561433417727));
#436553=CARTESIAN_POINT('Ctrl Pts',(-1.87416224611936,-1.89433127665259,
13.8546163505475));
#436554=CARTESIAN_POINT('Ctrl Pts',(-1.87637800444609,-1.89363096822991,
13.8528973491086));
#436555=CARTESIAN_POINT('Ctrl Pts',(-1.87678279080193,-1.89350303221316,
13.8525833129073));
#436556=CARTESIAN_POINT('Ctrl Pts',(-1.87718211936919,-1.89338491003298,
13.8522628768812));
#436557=CARTESIAN_POINT('Ctrl Pts',(-1.87757491665071,-1.89327587678666,
13.851937733538));
#436558=CARTESIAN_POINT('Ctrl Pts',(-1.87997367515072,-1.89261002587908,
13.8499521282529));
#436559=CARTESIAN_POINT('Ctrl Pts',(-1.88236833975653,-1.89222089205316,
13.847639871647));
#436560=CARTESIAN_POINT('Ctrl Pts',(-1.88462016939034,-1.89204962624485,
13.8452109780794));
#436561=CARTESIAN_POINT('Ctrl Pts',(-1.88563331415315,-1.89197257021266,
13.8441181685877));
#436562=CARTESIAN_POINT('Ctrl Pts',(-1.88661774147218,-1.89193892654058,
13.8430021611332));
#436563=CARTESIAN_POINT('Ctrl Pts',(-1.88756266124592,-1.89194058951909,
13.8418824960098));
#436564=CARTESIAN_POINT('Ctrl Pts',(-1.8897893888221,-1.89194450837042,
13.8392439765549));
#436565=CARTESIAN_POINT('Ctrl Pts',(-1.89190317628152,-1.89214089762252,
13.8364981347964));
#436566=CARTESIAN_POINT('Ctrl Pts',(-1.89391277952983,-1.89249620286769,
13.833693111342));
#436567=CARTESIAN_POINT('Ctrl Pts',(-1.89587000547208,-1.89284224761252,
13.8309611966328));
#436568=CARTESIAN_POINT('Ctrl Pts',(-1.89773027027713,-1.89333993505671,
13.8281701127186));
#436569=CARTESIAN_POINT('Ctrl Pts',(-1.89948121015224,-1.89399182518045,
13.8253580685121));
#436570=CARTESIAN_POINT('Ctrl Pts',(-1.89986081580685,-1.89413315566282,
13.8247484142933));
#436571=CARTESIAN_POINT('Ctrl Pts',(-1.9002351422505,-1.89428183513771,
13.8241378483365));
#436572=CARTESIAN_POINT('Ctrl Pts',(-1.90060378598595,-1.89443804601162,
13.8235269408515));
#436573=CARTESIAN_POINT('',(-1.86304757851021,-1.90162156650924,12.5969504640361));
#436574=CARTESIAN_POINT('Origin',(-1.88721527833432,-1.92611219968666,12.584524458991));
#436575=CARTESIAN_POINT('Origin',(-1.88721527833432,-1.92611219968666,12.584524458991));
#436576=CARTESIAN_POINT('Ctrl Pts',(-1.85527432946225,-1.93885208923188,
12.5893111709658));
#436577=CARTESIAN_POINT('Ctrl Pts',(-1.85106604772005,-1.92832835418495,
12.5770542771492));
#436578=CARTESIAN_POINT('Ctrl Pts',(-1.86486164992112,-1.9195257957634,
12.5737548217797));
#436579=CARTESIAN_POINT('Ctrl Pts',(-1.8644764292911,-1.96186396590907,
12.5663937883685));
#436580=CARTESIAN_POINT('Ctrl Pts',(-1.86026277930111,-1.95132680637659,
12.5540940315304));
#436581=CARTESIAN_POINT('Ctrl Pts',(-1.87410285856934,-1.94249967767227,
12.5508374392248));
#436582=CARTESIAN_POINT('Ctrl Pts',(-1.87366924431403,-1.98485262388478,
12.5434499600944));
#436583=CARTESIAN_POINT('Ctrl Pts',(-1.86944189424743,-1.97428120429418,
12.5311293540532));
#436584=CARTESIAN_POINT('Ctrl Pts',(-1.88333394373153,-1.9654515539222,
12.5278936106989));
#436585=CARTESIAN_POINT('Ctrl Pts',(-1.88285350182261,-2.00781988191172,
12.5204817579905));
#436586=CARTESIAN_POINT('Ctrl Pts',(-1.87860522926214,-1.99719614101879,
12.5081597038247));
#436587=CARTESIAN_POINT('Ctrl Pts',(-1.89255567939123,-1.98838314004918,
12.5049254088044));
#436588=CARTESIAN_POINT('Ctrl Pts',(-1.87625044290217,-1.99130747926499,
12.5369868989719));
#436589=CARTESIAN_POINT('Ctrl Pts',(-1.87659630935327,-1.99217239404041,
12.5342545179733));
#436590=CARTESIAN_POINT('Ctrl Pts',(-1.87704221692763,-1.99295151120007,
12.5314872231885));
#436591=CARTESIAN_POINT('Ctrl Pts',(-1.87761156380286,-1.9935731744898,
12.5287124745063));
#436592=CARTESIAN_POINT('Ctrl Pts',(-1.87812502907479,-1.99413382130109,
12.5262100684184));
#436593=CARTESIAN_POINT('Ctrl Pts',(-1.87873909888072,-1.99456517569273,
12.5237004536639));
#436594=CARTESIAN_POINT('Ctrl Pts',(-1.87950242149938,-1.9948203994206,
12.5212220730815));
#436595=CARTESIAN_POINT('Ctrl Pts',(-1.88008681099664,-1.99501579526291,
12.5193246583486));
#436596=CARTESIAN_POINT('Ctrl Pts',(-1.88076586646999,-1.99510969034912,
12.517417831369));
#436597=CARTESIAN_POINT('Ctrl Pts',(-1.88157164832197,-1.99501029059805,
12.5155812248347));
#436598=CARTESIAN_POINT('Ctrl Pts',(-1.88191491572201,-1.99496794576981,
12.5147988205793));
#436599=CARTESIAN_POINT('Ctrl Pts',(-1.8822815638793,-1.99489075363624,
12.5140295443047));
#436600=CARTESIAN_POINT('Ctrl Pts',(-1.88267547668793,-1.99477321448519,
12.5132817086137));
#436601=CARTESIAN_POINT('Ctrl Pts',(-1.88327161043647,-1.99459533488041,
12.5121499604604));
#436602=CARTESIAN_POINT('Ctrl Pts',(-1.8839410158435,-1.99431435531195,
12.5110494206568));
#436603=CARTESIAN_POINT('Ctrl Pts',(-1.88468109521418,-1.99389312539989,
12.5100666561695));
#436604=CARTESIAN_POINT('Ctrl Pts',(-1.88510604708456,-1.9936512561544,
12.5095023550641));
#436605=CARTESIAN_POINT('Ctrl Pts',(-1.88555888741544,-1.99335978408002,
12.5089719619137));
#436606=CARTESIAN_POINT('Ctrl Pts',(-1.88602767138404,-1.99301880185507,
12.5085043804652));
#436607=CARTESIAN_POINT('Ctrl Pts',(-1.88671367565868,-1.9925198187849,
12.5078201359221));
#436608=CARTESIAN_POINT('Ctrl Pts',(-1.88745300841245,-1.99189936323301,
12.5072563000949));
#436609=CARTESIAN_POINT('Ctrl Pts',(-1.88819011153062,-1.99119300795444,
12.5068768744332));
#436610=CARTESIAN_POINT('Ctrl Pts',(-1.88872161362118,-1.99068367717293,
12.5066032824114));
#436611=CARTESIAN_POINT('Ctrl Pts',(-1.88926133567869,-1.99012077885057,
12.5064197834844));
#436612=CARTESIAN_POINT('Ctrl Pts',(-1.88978100399925,-1.98953753564754,
12.5063282718343));
#436613=CARTESIAN_POINT('Ctrl Pts',(-1.89053955886202,-1.98868618113864,
12.5061946931565));
#436614=CARTESIAN_POINT('Ctrl Pts',(-1.89127239157615,-1.9877739877967,
12.5062515701262));
#436615=CARTESIAN_POINT('Ctrl Pts',(-1.89194607715322,-1.98686725334717,
12.5064436508398));
#436616=CARTESIAN_POINT('',(-1.86486164992112,-1.9195257957634,12.5737548217797));
#436617=CARTESIAN_POINT('Origin',(-1.8757016279792,-1.93068352293789,12.5893111709658));
#436618=CARTESIAN_POINT('Ctrl Pts',(-1.89194607715322,-1.98686725334717,
12.5064436508398));
#436619=CARTESIAN_POINT('Ctrl Pts',(-1.88793732399357,-1.97689878877853,
12.5164271754438));
#436620=CARTESIAN_POINT('Ctrl Pts',(-1.88392678791681,-1.96692645066764,
12.5264061185523));
#436621=CARTESIAN_POINT('Ctrl Pts',(-1.87991440700823,-1.95695010223845,
12.536380305637));
#436622=CARTESIAN_POINT('Ctrl Pts',(-1.87489974467104,-1.94448169012345,
12.5488460165097));
#436623=CARTESIAN_POINT('Ctrl Pts',(-1.8698821992156,-1.93200701024519,
12.5613043021964));
#436624=CARTESIAN_POINT('Ctrl Pts',(-1.86486164992112,-1.9195257957634,
12.5737548217797));
#436625=CARTESIAN_POINT('Ctrl Pts',(-1.90060378598595,-1.89443804601162,
12.5893111709658));
#436626=CARTESIAN_POINT('Ctrl Pts',(-1.8901680834241,-1.89001597109137,
12.5770542771492));
#436627=CARTESIAN_POINT('Ctrl Pts',(-1.88108594645948,-1.90362914349941,
12.5737548217797));
#436628=CARTESIAN_POINT('Ctrl Pts',(-1.89086736626069,-1.89031228857221,
12.5928319619712));
#436629=CARTESIAN_POINT('Ctrl Pts',(-1.882582883658,-1.89033993594174,12.5821634970842));
#436630=CARTESIAN_POINT('Ctrl Pts',(-1.87754288710091,-1.90211753913613,
12.5773203894503));
#436631=CARTESIAN_POINT('Ctrl Pts',(-1.87412398120692,-1.89080539736434,
12.5969440695591));
#436632=CARTESIAN_POINT('Ctrl Pts',(-1.87123997155424,-1.89360558144314,
12.5878292599214));
#436633=CARTESIAN_POINT('Ctrl Pts',(-1.87157526323811,-1.90229533826341,
12.5813877129824));
#436634=CARTESIAN_POINT('Ctrl Pts',(-1.85223139267545,-1.91218037836861,
12.596957478804));
#436635=CARTESIAN_POINT('Ctrl Pts',(-1.85509414456203,-1.90940094591129,
12.5878468778671));
#436636=CARTESIAN_POINT('Ctrl Pts',(-1.86374376954388,-1.90995000839486,
12.5814011370086));
#436637=CARTESIAN_POINT('Ctrl Pts',(-1.85134233823174,-1.92901927944131,
12.5928371701607));
#436638=CARTESIAN_POINT('Ctrl Pts',(-1.85154488702826,-1.92074316684609,
12.5821692192952));
#436639=CARTESIAN_POINT('Ctrl Pts',(-1.86341779569826,-1.91594130661471,
12.5773318885715));
#436640=CARTESIAN_POINT('Ctrl Pts',(-1.8552743294622,-1.9388520892319,12.5893111709658));
#436641=CARTESIAN_POINT('Ctrl Pts',(-1.85106604772,-1.92832835418497,12.5770542771492));
#436642=CARTESIAN_POINT('Ctrl Pts',(-1.86486164992107,-1.91952579576342,
12.5737548217797));
#436643=CARTESIAN_POINT('',(-1.88108594645948,-1.90362914349941,12.5737548217797));
#436644=CARTESIAN_POINT('Origin',(-1.89202023232773,-1.9146944673786,12.5893111709658));
#436645=CARTESIAN_POINT('Ctrl Pts',(-1.86486164992107,-1.91952579576342,
12.5737548217797));
#436646=CARTESIAN_POINT('Ctrl Pts',(-1.864459398978,-1.91860791025323,12.5746934679442));
#436647=CARTESIAN_POINT('Ctrl Pts',(-1.86418206174568,-1.91751868139859,
12.5756680099006));
#436648=CARTESIAN_POINT('Ctrl Pts',(-1.86405796428202,-1.91638285417251,
12.5765688348656));
#436649=CARTESIAN_POINT('Ctrl Pts',(-1.86402511085232,-1.91608215648843,
12.5768073183026));
#436650=CARTESIAN_POINT('Ctrl Pts',(-1.86400275641609,-1.91577828215687,
12.5770407398754));
#436651=CARTESIAN_POINT('Ctrl Pts',(-1.86399086624776,-1.9154736023794,
12.5772674179684));
#436652=CARTESIAN_POINT('Ctrl Pts',(-1.86394207221219,-1.91422327896154,
12.5781976435658));
#436653=CARTESIAN_POINT('Ctrl Pts',(-1.86407800267149,-1.91288793616173,
12.5790594849312));
#436654=CARTESIAN_POINT('Ctrl Pts',(-1.8644375203118,-1.91156262872948,
12.5797571720116));
#436655=CARTESIAN_POINT('Ctrl Pts',(-1.86467175898157,-1.91069914328356,
12.580211740231));
#436656=CARTESIAN_POINT('Ctrl Pts',(-1.86502967323599,-1.90980559173675,
12.5806009430798));
#436657=CARTESIAN_POINT('Ctrl Pts',(-1.86550251387252,-1.90895146387936,
12.5808812374708));
#436658=CARTESIAN_POINT('Ctrl Pts',(-1.86590884084254,-1.9082174846959,
12.5811221033394));
#436659=CARTESIAN_POINT('Ctrl Pts',(-1.86640845376854,-1.90749764674408,
12.581287365893));
#436660=CARTESIAN_POINT('Ctrl Pts',(-1.86698000348281,-1.90683733302502,
12.581359338449));
#436661=CARTESIAN_POINT('Ctrl Pts',(-1.86705943709104,-1.90674556305303,
12.5813693411482));
#436662=CARTESIAN_POINT('Ctrl Pts',(-1.8671402305528,-1.90665489077119,
12.5813775999465));
#436663=CARTESIAN_POINT('Ctrl Pts',(-1.86722229715839,-1.90656538416846,
12.5813841266931));
#436664=CARTESIAN_POINT('Ctrl Pts',(-1.86736153308052,-1.90641352539133,
12.5813952001081));
#436665=CARTESIAN_POINT('Ctrl Pts',(-1.86750581509648,-1.90626441645135,
12.5814007534795));
#436666=CARTESIAN_POINT('Ctrl Pts',(-1.86765522209018,-1.90611825942592,
12.5814005856065));
#436667=CARTESIAN_POINT('Ctrl Pts',(-1.86833914889296,-1.9054492097072,
12.5813998171494));
#436668=CARTESIAN_POINT('Ctrl Pts',(-1.8690829769656,-1.9048880008343,12.58127954464));
#436669=CARTESIAN_POINT('Ctrl Pts',(-1.86986466195916,-1.90441419847258,
12.5810700125799));
#436670=CARTESIAN_POINT('Ctrl Pts',(-1.87080884842942,-1.90384189916634,
12.5808169217085));
#436671=CARTESIAN_POINT('Ctrl Pts',(-1.87181702811071,-1.90341138541547,
12.5804173076348));
#436672=CARTESIAN_POINT('Ctrl Pts',(-1.87279061863424,-1.90313643658359,
12.5799304713245));
#436673=CARTESIAN_POINT('Ctrl Pts',(-1.87399720400554,-1.90279568836309,
12.5793271277669));
#436674=CARTESIAN_POINT('Ctrl Pts',(-1.87521675920047,-1.90264174702716,
12.5785808224116));
#436675=CARTESIAN_POINT('Ctrl Pts',(-1.87639390560314,-1.90264963433858,
12.5777485681082));
#436676=CARTESIAN_POINT('Ctrl Pts',(-1.87814798270914,-1.9026613872967,
12.576508418016));
#436677=CARTESIAN_POINT('Ctrl Pts',(-1.87979317055781,-1.90302549779276,
12.5750928681475));
#436678=CARTESIAN_POINT('Ctrl Pts',(-1.88108594645948,-1.90362914349941,
12.5737548217797));
#436679=CARTESIAN_POINT('Ctrl Pts',(-1.88108594645948,-1.90362914349941,
12.5737548217797));
#436680=CARTESIAN_POINT('Ctrl Pts',(-1.8901680834241,-1.89001597109137,
12.5770542771492));
#436681=CARTESIAN_POINT('Ctrl Pts',(-1.90060378598595,-1.89443804601162,
12.5893111709658));
#436682=CARTESIAN_POINT('Ctrl Pts',(-1.90386311858782,-1.91333560444078,
12.5508408821982));
#436683=CARTESIAN_POINT('Ctrl Pts',(-1.91297072106733,-1.89967847071131,
12.55409748406));
#436684=CARTESIAN_POINT('Ctrl Pts',(-1.92341973691294,-1.9041061870666,
12.5663972313419));
#436685=CARTESIAN_POINT('Ctrl Pts',(-1.92661850269949,-1.92303149829958,
12.52790050457));
#436686=CARTESIAN_POINT('Ctrl Pts',(-1.93572968623204,-1.90932246434462,
12.5311362602938));
#436687=CARTESIAN_POINT('Ctrl Pts',(-1.94621267029458,-1.91376457455593,
12.5434568539655));
#436688=CARTESIAN_POINT('Ctrl Pts',(-1.94935379743199,-1.93271763353421,
12.5049357605811));
#436689=CARTESIAN_POINT('Ctrl Pts',(-1.95844953155081,-1.91894988114578,
12.5081700652078));
#436690=CARTESIAN_POINT('Ctrl Pts',(-1.96898438886974,-1.92341397238087,
12.5204921097672));
#436691=CARTESIAN_POINT('Ctrl Pts',(-1.94786090948231,-1.93208160246608,
12.5064436508395));
#436692=CARTESIAN_POINT('Ctrl Pts',(-1.94885498694117,-1.9313740307055,
12.5062361689309));
#436693=CARTESIAN_POINT('Ctrl Pts',(-1.94985857371886,-1.93059582430609,
12.5061871075061));
#436694=CARTESIAN_POINT('Ctrl Pts',(-1.95078610801201,-1.92978916652478,
12.5063648335164));
#436695=CARTESIAN_POINT('Ctrl Pts',(-1.95120745130064,-1.92942273280379,
12.5064455676329));
#436696=CARTESIAN_POINT('Ctrl Pts',(-1.95161883316559,-1.92904515080624,
12.506574497099));
#436697=CARTESIAN_POINT('Ctrl Pts',(-1.95200190414132,-1.92867183585609,
12.5067492519495));
#436698=CARTESIAN_POINT('Ctrl Pts',(-1.95277170013684,-1.92792164497268,
12.5071004286051));
#436699=CARTESIAN_POINT('Ctrl Pts',(-1.9534549083882,-1.92716052483932,
12.5076537929613));
#436700=CARTESIAN_POINT('Ctrl Pts',(-1.95400728921211,-1.92645191968004,
12.5083435010505));
#436701=CARTESIAN_POINT('Ctrl Pts',(-1.95404206488602,-1.92640730875062,
12.5083869222964));
#436702=CARTESIAN_POINT('Ctrl Pts',(-1.95407631641088,-1.92636289375941,
12.5084308732337));
#436703=CARTESIAN_POINT('Ctrl Pts',(-1.95411003081841,-1.92631868540296,
12.5084753333615));
#436704=CARTESIAN_POINT('Ctrl Pts',(-1.95438046486583,-1.92596407603442,
12.5088319622689));
#436705=CARTESIAN_POINT('Ctrl Pts',(-1.95462285601273,-1.92561634503086,
12.509227847131));
#436706=CARTESIAN_POINT('Ctrl Pts',(-1.95483229376253,-1.92528743344482,
12.5096423454524));
#436707=CARTESIAN_POINT('Ctrl Pts',(-1.95548857897713,-1.92425677010434,
12.5109411997424));
#436708=CARTESIAN_POINT('Ctrl Pts',(-1.95586981010331,-1.92335269880289,
12.5124831113042));
#436709=CARTESIAN_POINT('Ctrl Pts',(-1.95607061270299,-1.92257385556357,
12.5140723025008));
#436710=CARTESIAN_POINT('Ctrl Pts',(-1.95608942812651,-1.922500877099,12.5142212114565));
#436711=CARTESIAN_POINT('Ctrl Pts',(-1.95610668697138,-1.92242898731641,
12.5143705582413));
#436712=CARTESIAN_POINT('Ctrl Pts',(-1.95612248339413,-1.92235818036019,
12.5145201959299));
#436713=CARTESIAN_POINT('Ctrl Pts',(-1.95632541196278,-1.92144855958696,
12.5164425148273));
#436714=CARTESIAN_POINT('Ctrl Pts',(-1.95630442735326,-1.92068881132239,
12.5184635205941));
#436715=CARTESIAN_POINT('Ctrl Pts',(-1.95613589680507,-1.92003091449528,
12.5205025929157));
#436716=CARTESIAN_POINT('Ctrl Pts',(-1.95603814240719,-1.91964930825897,
12.5216853356836));
#436717=CARTESIAN_POINT('Ctrl Pts',(-1.95589139178563,-1.91930253886929,
12.5228750347131));
#436718=CARTESIAN_POINT('Ctrl Pts',(-1.95571340556782,-1.91898642377186,
12.5240609649613));
#436719=CARTESIAN_POINT('Ctrl Pts',(-1.95527654794483,-1.91821053622422,
12.5269717671327));
#436720=CARTESIAN_POINT('Ctrl Pts',(-1.95463016399357,-1.91760258328547,
12.5299036066169));
#436721=CARTESIAN_POINT('Ctrl Pts',(-1.95384300144752,-1.9171098082331,
12.5328133004019));
#436722=CARTESIAN_POINT('Ctrl Pts',(-1.95346511759031,-1.91687324751453,
12.5342101228451));
#436723=CARTESIAN_POINT('Ctrl Pts',(-1.95305498388151,-1.91666396959508,
12.5356023438238));
#436724=CARTESIAN_POINT('Ctrl Pts',(-1.95262037949673,-1.9164798081486,
12.5369868989719));
#436725=CARTESIAN_POINT('Origin',(-13.6892547326121,-6.88406632582468,-1.23928728697254));
#436726=CARTESIAN_POINT('Ctrl Pts',(-1.87623488789991,-1.99126868747673,
12.5369868989719));
#436727=CARTESIAN_POINT('Ctrl Pts',(-1.8819572621244,-2.00550026282593,
12.5369868989719));
#436728=CARTESIAN_POINT('Ctrl Pts',(-1.87058227977446,-2.01579069917351,
12.5369868989719));
#436729=CARTESIAN_POINT('Ctrl Pts',(-1.87816921275666,-1.99607954123951,
12.5218025310015));
#436730=CARTESIAN_POINT('Ctrl Pts',(-1.87932359695175,-2.00784063221076,
12.5216901060418));
#436731=CARTESIAN_POINT('Ctrl Pts',(-1.87061696555422,-2.01575934274308,
12.5161920673677));
#436732=CARTESIAN_POINT('Ctrl Pts',(-1.88402363857561,-1.99751542755993,
12.5042015548895));
#436733=CARTESIAN_POINT('Ctrl Pts',(-1.88345155018289,-2.00392245962545,
12.4980677368512));
#436734=CARTESIAN_POINT('Ctrl Pts',(-1.87849505311052,-2.00857261193425,
12.4907278922778));
#436735=CARTESIAN_POINT('Ctrl Pts',(-1.89193228448991,-1.98685276867447,
12.506463626192));
#436736=CARTESIAN_POINT('Ctrl Pts',(-1.89644413279589,-1.99159098175539,
12.4999376786891));
#436737=CARTESIAN_POINT('Ctrl Pts',(-1.89638902712905,-1.99153311137196,
12.4906970594712));
#436738=CARTESIAN_POINT('Origin',(-1.85582314438521,-1.99947604555898,12.5369868989719));
#436739=CARTESIAN_POINT('Origin',(-1.85582314438521,-1.99947604555898,14.));
#436740=CARTESIAN_POINT('Origin',(-1.85582314438521,-1.99947604555898,13.7435492065112));
#436741=CARTESIAN_POINT('Ctrl Pts',(-1.86705702902013,-1.96831739683604,
13.793642941384));
#436742=CARTESIAN_POINT('Ctrl Pts',(-1.87109688927,-1.97834664148194,13.8071662555867));
#436743=CARTESIAN_POINT('Ctrl Pts',(-1.85640749958171,-1.98696297563403,
13.8103758687955));
#436744=CARTESIAN_POINT('Ctrl Pts',(-1.87322842901165,-1.98375033328277,
13.7804579775005));
#436745=CARTESIAN_POINT('Ctrl Pts',(-1.87820384505148,-1.99612930363412,
13.7901904343351));
#436746=CARTESIAN_POINT('Ctrl Pts',(-1.86608206223867,-2.00619500309334,
13.7927914348262));
#436747=CARTESIAN_POINT('Ctrl Pts',(-1.87686176440724,-1.99283628378975,
13.7597120340895));
#436748=CARTESIAN_POINT('Ctrl Pts',(-1.88261440493231,-2.00716437567116,
13.7635825532445));
#436749=CARTESIAN_POINT('Ctrl Pts',(-1.87176430493386,-2.01754759512214,
13.7651073818885));
#436750=CARTESIAN_POINT('Ctrl Pts',(-1.87615027414212,-1.9910570466362,
13.7381884353898));
#436751=CARTESIAN_POINT('Ctrl Pts',(-1.88176909751235,-2.00504942794033,
13.7368803041982));
#436752=CARTESIAN_POINT('Ctrl Pts',(-1.87065111100612,-2.01532464147419,
13.7363986145813));
#436753=CARTESIAN_POINT('Origin',(-1.84812723423301,-1.98023072779075,13.7902182540695));
#436754=CARTESIAN_POINT('Ctrl Pts',(-1.85527286725314,-1.93884843470003,
13.8235227101244));
#436755=CARTESIAN_POINT('Ctrl Pts',(-1.85954582903258,-1.94952197609691,
13.8358800583119));
#436756=CARTESIAN_POINT('Ctrl Pts',(-1.84551606885696,-1.95834194653175,
13.8390832900376));
#436757=CARTESIAN_POINT('Ctrl Pts',(-1.85970155919287,-1.94992335397727,
13.8124254819052));
#436758=CARTESIAN_POINT('Ctrl Pts',(-1.86398281874529,-1.96061762334364,
13.8247886449157));
#436759=CARTESIAN_POINT('Ctrl Pts',(-1.84992625996221,-1.96943430845088,
13.8279860620657));
#436760=CARTESIAN_POINT('Ctrl Pts',(-1.86412826633697,-1.96099330983601,
13.8013225099955));
#436761=CARTESIAN_POINT('Ctrl Pts',(-1.86841580545634,-1.97170326044898,
13.8136962257787));
#436762=CARTESIAN_POINT('Ctrl Pts',(-1.85433466124413,-1.98052143500817,
13.8168830918626));
#436763=CARTESIAN_POINT('Ctrl Pts',(-1.86855306591077,-1.97205849539518,
13.7902140179785));
#436764=CARTESIAN_POINT('Ctrl Pts',(-1.87284499829307,-1.98277941037341,
13.802602731458));
#436765=CARTESIAN_POINT('Ctrl Pts',(-1.85874134473934,-1.99160353123376,
13.8057746032558));
#436766=CARTESIAN_POINT('Origin',(-1.8348470309453,-1.94702065552588,13.8235269408515));
#436767=CARTESIAN_POINT('Ctrl Pts',(-1.90060378598595,-1.89443804601162,
13.8235269408515));
#436768=CARTESIAN_POINT('Ctrl Pts',(-1.91147548235175,-1.89904487104853,
13.8362179249168));
#436769=CARTESIAN_POINT('Ctrl Pts',(-1.92059432876028,-1.88460500802166,
13.8391868794938));
#436770=CARTESIAN_POINT('Ctrl Pts',(-1.89065665702799,-1.89022300162599,
13.8400110824519));
#436771=CARTESIAN_POINT('Ctrl Pts',(-1.90070784009783,-1.89076667593883,
13.8494522556837));
#436772=CARTESIAN_POINT('Ctrl Pts',(-1.9041803253077,-1.87777168713915,
13.85569149686));
#436773=CARTESIAN_POINT('Ctrl Pts',(-1.87436920004126,-1.89056428003132,
13.8586819406588));
#436774=CARTESIAN_POINT('Ctrl Pts',(-1.87748879886921,-1.88752715198205,
13.868010383617));
#436775=CARTESIAN_POINT('Ctrl Pts',(-1.87714588160431,-1.87848418374469,
13.8744918421245));
#436776=CARTESIAN_POINT('Ctrl Pts',(-1.85198235760561,-1.91242522199886,
13.8587686893867));
#436777=CARTESIAN_POINT('Ctrl Pts',(-1.848890483899,-1.91543527929105,13.8680909899357));
#436778=CARTESIAN_POINT('Ctrl Pts',(-1.83988016077333,-1.91487807315619,
13.8745789365163));
#436779=CARTESIAN_POINT('Ctrl Pts',(-1.8512565417091,-1.92880472636389,
13.8400379222776));
#436780=CARTESIAN_POINT('Ctrl Pts',(-1.85158783296944,-1.93886258299485,
13.8494748685453));
#436781=CARTESIAN_POINT('Ctrl Pts',(-1.83853100517432,-1.9420688819817,
13.8557104837033));
#436782=CARTESIAN_POINT('Ctrl Pts',(-1.85527432945606,-1.9388520892342,
13.8235269408542));
#436783=CARTESIAN_POINT('Ctrl Pts',(-1.85965842923767,-1.94981549599923,
13.8362179249195));
#436784=CARTESIAN_POINT('Ctrl Pts',(-1.8450355596098,-1.95863789294693,
13.8391868794965));
#436785=CARTESIAN_POINT('Origin',(-1.90918733964416,-1.87418162464464,13.8235269408515));
#436786=CARTESIAN_POINT('Ctrl Pts',(-1.93353242134223,-1.90839138390051,
13.7902140241683));
#436787=CARTESIAN_POINT('Ctrl Pts',(-1.94416355476995,-1.91290110644569,
13.8026027327198));
#436788=CARTESIAN_POINT('Ctrl Pts',(-1.95327352985919,-1.89898039216277,
13.8057746032556));
#436789=CARTESIAN_POINT('Ctrl Pts',(-1.92255979757213,-1.90374179139983,
13.8013225161808));
#436790=CARTESIAN_POINT('Ctrl Pts',(-1.9331800585313,-1.90824689795181,
13.8136962270464));
#436791=CARTESIAN_POINT('Ctrl Pts',(-1.94228362940304,-1.89434856701977,
13.8168830918628));
#436792=CARTESIAN_POINT('Ctrl Pts',(-1.91158244340521,-1.89909019441801,
13.8124254880875));
#436793=CARTESIAN_POINT('Ctrl Pts',(-1.92218715447773,-1.90358870284954,
13.8247886461868));
#436794=CARTESIAN_POINT('Ctrl Pts',(-1.931288734703,-1.88971492183638,13.8279860620656));
#436795=CARTESIAN_POINT('Ctrl Pts',(-1.90060016733647,-1.8944365118058,
13.8235227163065));
#436796=CARTESIAN_POINT('Ctrl Pts',(-1.91118432402242,-1.89892630138706,
13.8358800595847));
#436797=CARTESIAN_POINT('Ctrl Pts',(-1.92028864223974,-1.88507938040817,
13.8390832900376));
#436798=CARTESIAN_POINT('Origin',(-1.94211960510584,-1.88813650159727,13.7902182540695));
#436799=CARTESIAN_POINT('Ctrl Pts',(-1.95237191771892,-1.91637449379808,
13.7382347919292));
#436800=CARTESIAN_POINT('Ctrl Pts',(-1.96625689773392,-1.92228424833753,
13.7369371795942));
#436801=CARTESIAN_POINT('Ctrl Pts',(-1.97675890153011,-1.91136400597366,
13.7364597369712));
#436802=CARTESIAN_POINT('Ctrl Pts',(-1.95411356339353,-1.91711250757053,
13.7595490285574));
#436803=CARTESIAN_POINT('Ctrl Pts',(-1.96833022087941,-1.92316233867132,
13.7633824266926));
#436804=CARTESIAN_POINT('Ctrl Pts',(-1.97893156148258,-1.91250845497929,
13.7648920890506));
#436805=CARTESIAN_POINT('Ctrl Pts',(-1.94523126586499,-1.91334867777003,
13.780380659011));
#436806=CARTESIAN_POINT('Ctrl Pts',(-1.95752605189593,-1.91858653252729,
13.7901039518744));
#436807=CARTESIAN_POINT('Ctrl Pts',(-1.96785337346261,-1.90667721387824,
13.7926933640891));
#436808=CARTESIAN_POINT('Ctrl Pts',(-1.92979185001233,-1.90680630131331,
13.7936647693663));
#436809=CARTESIAN_POINT('Ctrl Pts',(-1.93973837744101,-1.91105364448938,
13.8072068914933));
#436810=CARTESIAN_POINT('Ctrl Pts',(-1.94865316318078,-1.89652192521527,
13.8104111085397));
#436811=CARTESIAN_POINT('Origin',(-1.96120393315495,-1.89622338678162,13.7435492065112));
#436812=CARTESIAN_POINT('Origin',(-1.96120393315495,-1.89622338678162,14.));
#436813=CARTESIAN_POINT('Origin',(-1.96120393315495,-1.89622338678162,12.5369868989719));
#436814=CARTESIAN_POINT('Ctrl Pts',(-1.94784785780646,-1.93206865653427,
12.506462012331));
#436815=CARTESIAN_POINT('Ctrl Pts',(-1.95249012722371,-1.93667331967586,
12.4999388158272));
#436816=CARTESIAN_POINT('Ctrl Pts',(-1.95243520308855,-1.93661884047225,
12.4907030323752));
#436817=CARTESIAN_POINT('Ctrl Pts',(-1.95866813966155,-1.92437774737275,
12.5042014951932));
#436818=CARTESIAN_POINT('Ctrl Pts',(-1.96508276230269,-1.92393761842813,
12.4980716682127));
#436819=CARTESIAN_POINT('Ctrl Pts',(-1.96983081992872,-1.9190815383211,
12.4907355092743));
#436820=CARTESIAN_POINT('Ctrl Pts',(-1.95735445356975,-1.9184955768467,
12.5218047446509));
#436821=CARTESIAN_POINT('Ctrl Pts',(-1.96908392516923,-1.91988782931414,
12.5216906929434));
#436822=CARTESIAN_POINT('Ctrl Pts',(-1.97717718493758,-1.91135144245249,
12.5161988840776));
#436823=CARTESIAN_POINT('Ctrl Pts',(-1.95258502108486,-1.91646478877674,
12.5369868989719));
#436824=CARTESIAN_POINT('Ctrl Pts',(-1.96668949693684,-1.92247056037261,
12.5369868989719));
#436825=CARTESIAN_POINT('Ctrl Pts',(-1.97720808151055,-1.91131865873717,
12.5369868989719));
#436826=CARTESIAN_POINT('Origin',(-3.60557045705452E-31,-8.83174710230764E-31,
12.5));
#436827=CARTESIAN_POINT('Origin',(-1.73986539582215,-2.04305131259621,12.5));
#436828=CARTESIAN_POINT('',(-1.73986539582215,-2.04305131259621,12.5893111709658));
#436829=CARTESIAN_POINT('',(-1.73986539582215,-2.04305131259621,13.8235269408515));
#436830=CARTESIAN_POINT('',(-1.73986539582215,-2.04305131259621,12.5));
#436831=CARTESIAN_POINT('',(-1.77155062986483,-2.05964404121034,13.7902182540695));
#436832=CARTESIAN_POINT('',(-1.73986539582215,-2.04305131259621,13.8235269408515));
#436833=CARTESIAN_POINT('',(-1.7899123001692,-2.06925956785762,13.7435492065112));
#436834=CARTESIAN_POINT('Origin',(-1.72950249645161,-2.03762490086689,13.7445212918703));
#436835=CARTESIAN_POINT('',(-1.7899123001692,-2.06925956785762,12.5369868989719));
#436836=CARTESIAN_POINT('',(-1.7899123001692,-2.06925956785762,12.5));
#436837=CARTESIAN_POINT('Ctrl Pts',(-1.7899123001692,-2.06925956785762,
12.5369868989719));
#436838=CARTESIAN_POINT('Ctrl Pts',(-1.77324216577622,-2.0605298543396,
12.5544431401645));
#436839=CARTESIAN_POINT('Ctrl Pts',(-1.75656010846005,-2.05179389709846,
12.5718848856037));
#436840=CARTESIAN_POINT('Ctrl Pts',(-1.73986539582215,-2.04305131259621,
12.5893111709658));
#436841=CARTESIAN_POINT('Origin',(-1.77202125744066,-2.34643707963298,12.5));
#436842=CARTESIAN_POINT('',(-1.70769732837638,-2.13761339725486,13.7435492065112));
#436843=CARTESIAN_POINT('',(-1.70159569779326,-2.11780482857113,13.7902182540695));
#436844=CARTESIAN_POINT('Origin',(-1.68556166719576,-2.06575133368299,13.7418732680461));
#436845=CARTESIAN_POINT('',(-1.6910666124833,-2.08362280022673,13.8235269408515));
#436846=CARTESIAN_POINT('',(-1.70159569779326,-2.11780482857113,13.7902182540695));
#436847=CARTESIAN_POINT('',(-1.6910666124833,-2.08362280022673,12.5893111709658));
#436848=CARTESIAN_POINT('',(-1.6910666124833,-2.08362280022673,12.5));
#436849=CARTESIAN_POINT('',(-1.70769732837638,-2.13761339725486,12.5369868989719));
#436850=CARTESIAN_POINT('Ctrl Pts',(-1.6910666124833,-2.08362280022673,
12.5893111709658));
#436851=CARTESIAN_POINT('Ctrl Pts',(-1.69661430871786,-2.10163305509251,
12.5718848856037));
#436852=CARTESIAN_POINT('Ctrl Pts',(-1.70215779955624,-2.11962965739805,
12.5544431401645));
#436853=CARTESIAN_POINT('Ctrl Pts',(-1.70769732837638,-2.13761339725486,
12.5369868989719));
#436854=CARTESIAN_POINT('',(-1.70769732837638,-2.13761339725486,12.5));
#436855=CARTESIAN_POINT('Origin',(-1.72391839740909,-2.07350346960706,12.5));
#436856=CARTESIAN_POINT('',(-1.70281517807711,-2.04636964742875,13.8587068136939));
#436857=CARTESIAN_POINT('Ctrl Pts',(-1.69106661247695,-2.08362280022854,
13.8235269408542));
#436858=CARTESIAN_POINT('Ctrl Pts',(-1.69055076997176,-2.08194814923894,
13.8262006681044));
#436859=CARTESIAN_POINT('Ctrl Pts',(-1.69018892118107,-2.08018324315511,
13.8288634856214));
#436860=CARTESIAN_POINT('Ctrl Pts',(-1.6899703697339,-2.07833604399288,
13.8314912288862));
#436861=CARTESIAN_POINT('Ctrl Pts',(-1.68974506573441,-2.07643177218637,
13.8342001611531));
#436862=CARTESIAN_POINT('Ctrl Pts',(-1.68967130704777,-2.07443798675416,
13.8368750301949));
#436863=CARTESIAN_POINT('Ctrl Pts',(-1.68977547353421,-2.07233908740906,
13.8394886372969));
#436864=CARTESIAN_POINT('Ctrl Pts',(-1.68978351856463,-2.07217698432142,
13.8396904925131));
#436865=CARTESIAN_POINT('Ctrl Pts',(-1.68979264687108,-2.07201425151545,
13.8398919674349));
#436866=CARTESIAN_POINT('Ctrl Pts',(-1.68980288204296,-2.07185088139667,
13.8400930404591));
#436867=CARTESIAN_POINT('Ctrl Pts',(-1.68996235290682,-2.06930546503583,
13.8432258934518));
#436868=CARTESIAN_POINT('Ctrl Pts',(-1.6903885864837,-2.06661825424749,
13.8462331177034));
#436869=CARTESIAN_POINT('Ctrl Pts',(-1.69116295655849,-2.06389200352702,
13.8489036603661));
#436870=CARTESIAN_POINT('Ctrl Pts',(-1.69141633945876,-2.06299994256431,
13.8497774930041));
#436871=CARTESIAN_POINT('Ctrl Pts',(-1.69170707101167,-2.06210394025367,
13.85061494757));
#436872=CARTESIAN_POINT('Ctrl Pts',(-1.69203820356988,-2.0612082813038,
13.8514076489583));
#436873=CARTESIAN_POINT('Ctrl Pts',(-1.69273859668696,-2.05931383345145,
13.8530843267192));
#436874=CARTESIAN_POINT('Ctrl Pts',(-1.69369130868293,-2.05723586281645,
13.8546805203176));
#436875=CARTESIAN_POINT('Ctrl Pts',(-1.69496507550662,-2.05515184004389,
13.8559412814274));
#436876=CARTESIAN_POINT('Ctrl Pts',(-1.69513554681686,-2.05487293021049,
13.8561100121513));
#436877=CARTESIAN_POINT('Ctrl Pts',(-1.69531169269203,-2.05459392393159,
13.8562727473908));
#436878=CARTESIAN_POINT('Ctrl Pts',(-1.69549360208566,-2.05431524895565,
13.8564289040185));
#436879=CARTESIAN_POINT('Ctrl Pts',(-1.69631855911052,-2.05305146111891,
13.8571370725437));
#436880=CARTESIAN_POINT('Ctrl Pts',(-1.69727845604051,-2.05177351737073,
13.8577210840554));
#436881=CARTESIAN_POINT('Ctrl Pts',(-1.69835944725488,-2.05054871734515,
13.8581177131616));
#436882=CARTESIAN_POINT('Ctrl Pts',(-1.69866389158743,-2.05020377150161,
13.8582294175695));
#436883=CARTESIAN_POINT('Ctrl Pts',(-1.69897778725942,-2.04986295174723,
13.8583265086086));
#436884=CARTESIAN_POINT('Ctrl Pts',(-1.69930045864519,-2.04952751849591,
13.8584082369006));
#436885=CARTESIAN_POINT('Ctrl Pts',(-1.6997640508988,-2.04904559086375,
13.8585256585398));
#436886=CARTESIAN_POINT('Ctrl Pts',(-1.70025175453929,-2.0485690147105,
13.8586122832068));
#436887=CARTESIAN_POINT('Ctrl Pts',(-1.70075145235216,-2.04811073490248,
13.8586682984299));
#436888=CARTESIAN_POINT('Ctrl Pts',(-1.70115116106901,-2.04774415648388,
13.8587131050557));
#436889=CARTESIAN_POINT('Ctrl Pts',(-1.70156280045229,-2.04738506315215,
13.8587357943552));
#436890=CARTESIAN_POINT('Ctrl Pts',(-1.70198675233971,-2.04703379387748,
13.8587355499465));
#436891=CARTESIAN_POINT('Ctrl Pts',(-1.70226076255196,-2.04680676017067,
13.8587353919793));
#436892=CARTESIAN_POINT('Ctrl Pts',(-1.70253692833895,-2.0465854201758,
13.8587257282814));
#436893=CARTESIAN_POINT('Ctrl Pts',(-1.70281517807711,-2.04636964742875,
13.8587068136939));
#436894=CARTESIAN_POINT('Ctrl Pts',(-1.70281517807711,-2.04636964742875,
13.8587068136939));
#436895=CARTESIAN_POINT('Ctrl Pts',(-1.70373032629727,-2.04565998262645,
13.8586446046466));
#436896=CARTESIAN_POINT('Ctrl Pts',(-1.70466798977104,-2.04501046493111,
13.858482427929));
#436897=CARTESIAN_POINT('Ctrl Pts',(-1.7056258805372,-2.04441725361486,
13.8582284286032));
#436898=CARTESIAN_POINT('Ctrl Pts',(-1.70660856503678,-2.0438086878096,
13.8579678548414));
#436899=CARTESIAN_POINT('Ctrl Pts',(-1.70761574434311,-2.04325919654583,
13.857615680862));
#436900=CARTESIAN_POINT('Ctrl Pts',(-1.7086030704553,-2.04278193701926,
13.8571944833187));
#436901=CARTESIAN_POINT('Ctrl Pts',(-1.71106704374375,-2.04159088706059,
13.8561433417727));
#436902=CARTESIAN_POINT('Ctrl Pts',(-1.71352054069227,-2.04078966753298,
13.8546163505474));
#436903=CARTESIAN_POINT('Ctrl Pts',(-1.71578600790379,-2.04027229420252,
13.8528973491085));
#436904=CARTESIAN_POINT('Ctrl Pts',(-1.71619987533943,-2.04017777772819,
13.8525833129072));
#436905=CARTESIAN_POINT('Ctrl Pts',(-1.71660750322806,-2.04009259757524,
13.8522628768811));
#436906=CARTESIAN_POINT('Ctrl Pts',(-1.71700788073077,-2.04001594375306,
13.851937733538));
#436907=CARTESIAN_POINT('Ctrl Pts',(-1.71945293059018,-2.03954782949618,
13.8499521282529));
#436908=CARTESIAN_POINT('Ctrl Pts',(-1.72187134516643,-2.03935517787733,
13.847639871647));
#436909=CARTESIAN_POINT('Ctrl Pts',(-1.72412964177623,-2.03936802696199,
13.8452109780794));
#436910=CARTESIAN_POINT('Ctrl Pts',(-1.72514569616539,-2.03937380803114,
13.8441181685877));
#436911=CARTESIAN_POINT('Ctrl Pts',(-1.72612959015532,-2.03942051627108,
13.8430021611332));
#436912=CARTESIAN_POINT('Ctrl Pts',(-1.72707123023827,-2.03949919344993,
13.8418824960098));
#436913=CARTESIAN_POINT('Ctrl Pts',(-1.72929022913938,-2.039684598231,13.8392439765549));
#436914=CARTESIAN_POINT('Ctrl Pts',(-1.73138097559818,-2.04005262731545,
13.8364981347964));
#436915=CARTESIAN_POINT('Ctrl Pts',(-1.7333549313815,-2.04057055163272,
13.8336931113419));
#436916=CARTESIAN_POINT('Ctrl Pts',(-1.73527743895667,-2.0410749770265,
13.8309611966327));
#436917=CARTESIAN_POINT('Ctrl Pts',(-1.73709094773704,-2.04172263730824,
13.8281701127185));
#436918=CARTESIAN_POINT('Ctrl Pts',(-1.73878292640722,-2.04251507617613,
13.825358068512));
#436919=CARTESIAN_POINT('Ctrl Pts',(-1.73914974920895,-2.04268687777791,
13.8247484142932));
#436920=CARTESIAN_POINT('Ctrl Pts',(-1.73951071135475,-2.04286557361434,
13.8241378483365));
#436921=CARTESIAN_POINT('Ctrl Pts',(-1.73986539582215,-2.04305131259621,
13.8235269408515));
#436922=CARTESIAN_POINT('',(-1.7018486299195,-2.04714975095789,12.5969504640361));
#436923=CARTESIAN_POINT('Origin',(-1.72393969975224,-2.07352878547137,12.584524458991));
#436924=CARTESIAN_POINT('Origin',(-1.72393969975224,-2.07352878547137,12.584524458991));
#436925=CARTESIAN_POINT('Ctrl Pts',(-1.6910666124833,-2.08362280022673,
12.5893111709658));
#436926=CARTESIAN_POINT('Ctrl Pts',(-1.68773011555536,-2.07279106801025,
12.5770542771492));
#436927=CARTESIAN_POINT('Ctrl Pts',(-1.70219730425849,-2.0651422690272,
12.5737548217797));
#436928=CARTESIAN_POINT('Ctrl Pts',(-1.69836241150306,-2.10730816334679,
12.5663937883685));
#436929=CARTESIAN_POINT('Ctrl Pts',(-1.69502165840993,-2.09646261375159,
12.5540940315304));
#436930=CARTESIAN_POINT('Ctrl Pts',(-1.70953517889259,-2.08879295153526,
12.5508374392248));
#436931=CARTESIAN_POINT('Ctrl Pts',(-1.70565084915105,-2.13096962822584,
12.5434499600945));
#436932=CARTESIAN_POINT('Ctrl Pts',(-1.70229923407987,-2.12008881588674,
12.5311293540533));
#436933=CARTESIAN_POINT('Ctrl Pts',(-1.71686475739119,-2.11242087644829,
12.5278936106989));
#436934=CARTESIAN_POINT('Ctrl Pts',(-1.7129325020536,-2.15460906684579,
12.5204817579905));
#436935=CARTESIAN_POINT('Ctrl Pts',(-1.70956429877839,-2.14367440192156,
12.5081597038247));
#436936=CARTESIAN_POINT('Ctrl Pts',(-1.72418667133044,-2.13602781668084,
12.5049254088044));
#436937=CARTESIAN_POINT('Ctrl Pts',(-1.70769732837638,-2.13761339725486,
12.5369868989719));
#436938=CARTESIAN_POINT('Ctrl Pts',(-1.70797154540172,-2.13850362542434,
12.5342545179733));
#436939=CARTESIAN_POINT('Ctrl Pts',(-1.70835246397393,-2.13931649574285,
12.5314872231885));
#436940=CARTESIAN_POINT('Ctrl Pts',(-1.70886924506505,-2.13998249755516,
12.5287124745063));
#436941=CARTESIAN_POINT('Ctrl Pts',(-1.70933530390373,-2.14058313104687,
12.5262100684184));
#436942=CARTESIAN_POINT('Ctrl Pts',(-1.70991217105562,-2.14106310253228,
12.5237004536639));
#436943=CARTESIAN_POINT('Ctrl Pts',(-1.71065215067803,-2.14137969490402,
12.5212220730815));
#436944=CARTESIAN_POINT('Ctrl Pts',(-1.7112186690923,-2.14162207375199,
12.5193246583487));
#436945=CARTESIAN_POINT('Ctrl Pts',(-1.71188781174333,-2.14177100573518,
12.5174178313692));
#436946=CARTESIAN_POINT('Ctrl Pts',(-1.7126990144251,-2.14173761543006,
12.515581224835));
#436947=CARTESIAN_POINT('Ctrl Pts',(-1.71304459112783,-2.1417233909806,
12.5147988205795));
#436948=CARTESIAN_POINT('Ctrl Pts',(-1.71341631116917,-2.1416763409261,
12.5140295443048));
#436949=CARTESIAN_POINT('Ctrl Pts',(-1.71381849379747,-2.14159130042768,
12.5132817086137));
#436950=CARTESIAN_POINT('Ctrl Pts',(-1.71442714279929,-2.14146260313735,
12.5121499604604));
#436951=CARTESIAN_POINT('Ctrl Pts',(-1.71511722325838,-2.14123712126033,
12.5110494206568));
#436952=CARTESIAN_POINT('Ctrl Pts',(-1.71588917422434,-2.14087761629533,
12.5100666561695));
#436953=CARTESIAN_POINT('Ctrl Pts',(-1.71633242669134,-2.1406711893723,
12.5095023550641));
#436954=CARTESIAN_POINT('Ctrl Pts',(-1.71680751791336,-2.14041759783811,
12.5089719619137));
#436955=CARTESIAN_POINT('Ctrl Pts',(-1.71730253525883,-2.1401159604488,
12.5085043804652));
#436956=CARTESIAN_POINT('Ctrl Pts',(-1.71802692866339,-2.13967455342057,
12.5078201359221));
#436957=CARTESIAN_POINT('Ctrl Pts',(-1.7188143742359,-2.13911642486643,
12.5072563000949));
#436958=CARTESIAN_POINT('Ctrl Pts',(-1.71960659921693,-2.13847250067384,
12.5068768744332));
#436959=CARTESIAN_POINT('Ctrl Pts',(-1.72017784796522,-2.1380081870031,
12.5066032824114));
#436960=CARTESIAN_POINT('Ctrl Pts',(-1.72076165558107,-2.1374911540367,
12.5064197834844));
#436961=CARTESIAN_POINT('Ctrl Pts',(-1.72132713448378,-2.1369522093198,
12.5063282718343));
#436962=CARTESIAN_POINT('Ctrl Pts',(-1.72215255861389,-2.13616551688619,
12.5061946931565));
#436963=CARTESIAN_POINT('Ctrl Pts',(-1.72295730511337,-2.13531609146183,
12.5062515701262));
#436964=CARTESIAN_POINT('Ctrl Pts',(-1.7237026563326,-2.1344672857251,12.5064436508398));
#436965=CARTESIAN_POINT('',(-1.70219730425849,-2.0651422690272,12.5737548217797));
#436966=CARTESIAN_POINT('Origin',(-1.7120917548358,-2.07714642863014,12.5893111709658));
#436967=CARTESIAN_POINT('Ctrl Pts',(-1.7237026563326,-2.13446728572511,
12.5064436508398));
#436968=CARTESIAN_POINT('Ctrl Pts',(-1.72051976437344,-2.12420523980202,
12.5164271754438));
#436969=CARTESIAN_POINT('Ctrl Pts',(-1.71733541115934,-2.11393918790128,
12.5264061185523));
#436970=CARTESIAN_POINT('Ctrl Pts',(-1.71414954613012,-2.10366898865532,
12.536380305637));
#436971=CARTESIAN_POINT('Ctrl Pts',(-1.71016786100664,-2.09083332261872,
12.5488460165097));
#436972=CARTESIAN_POINT('Ctrl Pts',(-1.70618381323914,-2.07799117467343,
12.5613043021964));
#436973=CARTESIAN_POINT('Ctrl Pts',(-1.70219730425849,-2.0651422690272,
12.5737548217797));
#436974=CARTESIAN_POINT('Ctrl Pts',(-1.73986539582215,-2.0430513125962,
12.5893111709658));
#436975=CARTESIAN_POINT('Ctrl Pts',(-1.72982485735823,-2.03779334512633,
12.5770542771492));
#436976=CARTESIAN_POINT('Ctrl Pts',(-1.71966334052536,-2.05062094234913,
12.5737548217797));
#436977=CARTESIAN_POINT('Ctrl Pts',(-1.7304976607633,-2.0381456746782,12.5928319619712));
#436978=CARTESIAN_POINT('Ctrl Pts',(-1.72223849057577,-2.03749796781189,
12.5821634970843));
#436979=CARTESIAN_POINT('Ctrl Pts',(-1.71625528019318,-2.04882557549479,
12.5773203894503));
#436980=CARTESIAN_POINT('Ctrl Pts',(-1.71376979499771,-2.03727240137162,
12.5969440695591));
#436981=CARTESIAN_POINT('Ctrl Pts',(-1.71066714065118,-2.03982819450837,
12.5878292599214));
#436982=CARTESIAN_POINT('Ctrl Pts',(-1.71029302082701,-2.0485163662646,
12.5813877129824));
#436983=CARTESIAN_POINT('Ctrl Pts',(-1.69020779286108,-2.05679180968373,
12.596957478804));
#436984=CARTESIAN_POINT('Ctrl Pts',(-1.69328756872517,-2.05425496641387,
12.5878468778671));
#436985=CARTESIAN_POINT('Ctrl Pts',(-1.70186365910379,-2.05550722667254,
12.5814011370086));
#436986=CARTESIAN_POINT('Ctrl Pts',(-1.68794916991053,-2.07350221451147,
12.5928371701607));
#436987=CARTESIAN_POINT('Ctrl Pts',(-1.68882562475084,-2.06527014960546,
12.5821692192951));
#436988=CARTESIAN_POINT('Ctrl Pts',(-1.70105042348384,-2.0614520194472,
12.5773318885715));
#436989=CARTESIAN_POINT('Ctrl Pts',(-1.69106661248325,-2.08362280022674,
12.5893111709658));
#436990=CARTESIAN_POINT('Ctrl Pts',(-1.68773011555531,-2.07279106801026,
12.5770542771492));
#436991=CARTESIAN_POINT('Ctrl Pts',(-1.70219730425843,-2.06514226902721,
12.5737548217797));
#436992=CARTESIAN_POINT('',(-1.71966334052536,-2.05062094234913,12.5737548217797));
#436993=CARTESIAN_POINT('Origin',(-1.72965931683779,-2.06254069308315,12.5893111709658));
#436994=CARTESIAN_POINT('Ctrl Pts',(-1.70219730425843,-2.06514226902721,
12.5737548217797));
#436995=CARTESIAN_POINT('Ctrl Pts',(-1.7018712079625,-2.06419465051916,
12.5746934679442));
#436996=CARTESIAN_POINT('Ctrl Pts',(-1.70168357581051,-2.06308644042457,
12.5756680099006));
#436997=CARTESIAN_POINT('Ctrl Pts',(-1.70165247173435,-2.06194427747454,
12.5765688348656));
#436998=CARTESIAN_POINT('Ctrl Pts',(-1.70164423727452,-2.06164190247768,
12.5768073183026));
#436999=CARTESIAN_POINT('Ctrl Pts',(-1.70164672579989,-2.06133721716881,
12.5770407398754));
#437000=CARTESIAN_POINT('Ctrl Pts',(-1.70165970942549,-2.06103258202906,
12.5772674179684));
#437001=CARTESIAN_POINT('Ctrl Pts',(-1.70171299071403,-2.05978244179235,
12.5781976435658));
#437002=CARTESIAN_POINT('Ctrl Pts',(-1.70195731171084,-2.0584626218299,
12.5790594849312));
#437003=CARTESIAN_POINT('Ctrl Pts',(-1.70242365794515,-2.05717102827408,
12.5797571720116));
#437004=CARTESIAN_POINT('Ctrl Pts',(-1.70272749928512,-2.0563295086309,
12.580211740231));
#437005=CARTESIAN_POINT('Ctrl Pts',(-1.70315705535578,-2.0554681036376,
12.5806009430798));
#437006=CARTESIAN_POINT('Ctrl Pts',(-1.70369794200381,-2.05465535872171,
12.5808812374708));
#437007=CARTESIAN_POINT('Ctrl Pts',(-1.70416274307174,-2.05395694121364,
12.5811221033394));
#437008=CARTESIAN_POINT('Ctrl Pts',(-1.70471936705266,-2.05328022155487,
12.581287365893));
#437009=CARTESIAN_POINT('Ctrl Pts',(-1.70534283668056,-2.05266869158297,
12.581359338449));
#437010=CARTESIAN_POINT('Ctrl Pts',(-1.70542948608469,-2.05258370154449,
12.5813693411482));
#437011=CARTESIAN_POINT('Ctrl Pts',(-1.70551740134559,-2.05249991638436,
12.5813775999465));
#437012=CARTESIAN_POINT('Ctrl Pts',(-1.70560649050039,-2.05241739679769,
12.5813841266931));
#437013=CARTESIAN_POINT('Ctrl Pts',(-1.7057576410266,-2.05227739233838,
12.5813952001081));
#437014=CARTESIAN_POINT('Ctrl Pts',(-1.70591359671892,-2.05214053986984,
12.5814007534795));
#437015=CARTESIAN_POINT('Ctrl Pts',(-1.7060744197276,-2.05200704722687,
12.5814005856065));
#437016=CARTESIAN_POINT('Ctrl Pts',(-1.70681060458359,-2.05139597009959,
12.5813998171494));
#437017=CARTESIAN_POINT('Ctrl Pts',(-1.70759770136284,-2.0508972574962,
12.58127954464));
#437018=CARTESIAN_POINT('Ctrl Pts',(-1.70841540465512,-2.05048874625654,
12.5810700125799));
#437019=CARTESIAN_POINT('Ctrl Pts',(-1.70940309712921,-2.04999531119176,
12.5808169217085));
#437020=CARTESIAN_POINT('Ctrl Pts',(-1.71044301304317,-2.04964840594338,
12.5804173076348));
#437021=CARTESIAN_POINT('Ctrl Pts',(-1.71143577490685,-2.04945372864711,
12.5799304713245));
#437022=CARTESIAN_POINT('Ctrl Pts',(-1.71266611960818,-2.04921246214735,
12.5793271277669));
#437023=CARTESIAN_POINT('Ctrl Pts',(-1.71389416448181,-2.0491584381087,
12.5785808224116));
#437024=CARTESIAN_POINT('Ctrl Pts',(-1.71506675113783,-2.04926224753565,
12.5777485681082));
#437025=CARTESIAN_POINT('Ctrl Pts',(-1.71681403372176,-2.04941693495497,
12.576508418016));
#437026=CARTESIAN_POINT('Ctrl Pts',(-1.71842406895792,-2.04991393198624,
12.5750928681475));
#437027=CARTESIAN_POINT('Ctrl Pts',(-1.71966334052536,-2.05062094234913,
12.5737548217797));
#437028=CARTESIAN_POINT('Ctrl Pts',(-1.71966334052536,-2.05062094234913,
12.5737548217797));
#437029=CARTESIAN_POINT('Ctrl Pts',(-1.72982485735823,-2.03779334512633,
12.5770542771492));
#437030=CARTESIAN_POINT('Ctrl Pts',(-1.73986539582215,-2.0430513125962,
12.5893111709658));
#437031=CARTESIAN_POINT('Ctrl Pts',(-1.74157355681532,-2.06215165682384,
12.5508408821982));
#437032=CARTESIAN_POINT('Ctrl Pts',(-1.75176403768451,-2.04928232023313,
12.55409748406));
#437033=CARTESIAN_POINT('Ctrl Pts',(-1.76181738530398,-2.05454699552289,
12.5663972313419));
#437034=CARTESIAN_POINT('Ctrl Pts',(-1.76346291890175,-2.07367006345149,
12.52790050457));
#437035=CARTESIAN_POINT('Ctrl Pts',(-1.77366119925847,-2.06074929121809,
12.5311362602938));
#437036=CARTESIAN_POINT('Ctrl Pts',(-1.78374722883563,-2.06603108119449,
12.5434568539655));
#437037=CARTESIAN_POINT('Ctrl Pts',(-1.78533305387325,-2.08517710645503,
12.5049357605811));
#437038=CARTESIAN_POINT('Ctrl Pts',(-1.79552072232037,-2.07219655189828,
12.5081700652078));
#437039=CARTESIAN_POINT('Ctrl Pts',(-1.80565666089238,-2.07750447791038,
12.5204921097672));
#437040=CARTESIAN_POINT('Ctrl Pts',(-1.78389697582175,-2.08442150750062,
12.5064436508395));
#437041=CARTESIAN_POINT('Ctrl Pts',(-1.78494541923713,-2.08379731666816,
12.5062361689309));
#437042=CARTESIAN_POINT('Ctrl Pts',(-1.78600909770868,-2.08310350132558,
12.5061871075061));
#437043=CARTESIAN_POINT('Ctrl Pts',(-1.7869992958058,-2.08237513028719,
12.5063648335164));
#437044=CARTESIAN_POINT('Ctrl Pts',(-1.78744910485947,-2.08204425923376,
12.5064455676329));
#437045=CARTESIAN_POINT('Ctrl Pts',(-1.78788989432329,-2.08170146505024,
12.506574497099));
#437046=CARTESIAN_POINT('Ctrl Pts',(-1.78830211929608,-2.08136061611557,
12.5067492519495));
#437047=CARTESIAN_POINT('Ctrl Pts',(-1.78913050138035,-2.08067566695052,
12.5071004286051));
#437048=CARTESIAN_POINT('Ctrl Pts',(-1.78987347466938,-2.0799727671967,
12.5076537929613));
#437049=CARTESIAN_POINT('Ctrl Pts',(-1.7904817753905,-2.07931154402785,
12.5083435010505));
#437050=CARTESIAN_POINT('Ctrl Pts',(-1.79052007155613,-2.07926991607787,
12.5083869222964));
#437051=CARTESIAN_POINT('Ctrl Pts',(-1.79055782934599,-2.07922844069112,
12.5084308732337));
#437052=CARTESIAN_POINT('Ctrl Pts',(-1.79059503496308,-2.07918712747152,
12.5084753333615));
#437053=CARTESIAN_POINT('Ctrl Pts',(-1.79089347311909,-2.07885574092186,
12.5088319622689));
#437054=CARTESIAN_POINT('Ctrl Pts',(-1.7911634010344,-2.07852892409326,
12.509227847131));
#437055=CARTESIAN_POINT('Ctrl Pts',(-1.79139895124509,-2.07821817805432,
12.5096423454524));
#437056=CARTESIAN_POINT('Ctrl Pts',(-1.79213706135524,-2.07724443749871,
12.5109411997424));
#437057=CARTESIAN_POINT('Ctrl Pts',(-1.79259071417036,-2.0763744482959,
12.5124831113042));
#437058=CARTESIAN_POINT('Ctrl Pts',(-1.79285433157038,-2.07561456386924,
12.5140723025008));
#437059=CARTESIAN_POINT('Ctrl Pts',(-1.7928790328095,-2.07554336186619,
12.5142212114565));
#437060=CARTESIAN_POINT('Ctrl Pts',(-1.79290209391165,-2.075473118047,12.5143705582413));
#437061=CARTESIAN_POINT('Ctrl Pts',(-1.79292360919738,-2.07540383425019,
12.5145201959299));
#437062=CARTESIAN_POINT('Ctrl Pts',(-1.79320000507549,-2.07451378072728,
12.5164425148273));
#437063=CARTESIAN_POINT('Ctrl Pts',(-1.79324101682725,-2.0737548500219,
12.518463520594));
#437064=CARTESIAN_POINT('Ctrl Pts',(-1.79312667174958,-2.07308540548798,
12.5205025929157));
#437065=CARTESIAN_POINT('Ctrl Pts',(-1.79306034707231,-2.072697101124,12.5216853356836));
#437066=CARTESIAN_POINT('Ctrl Pts',(-1.79294234967585,-2.07233952404283,
12.5228750347131));
#437067=CARTESIAN_POINT('Ctrl Pts',(-1.79279072200761,-2.07200995326322,
12.5240609649613));
#437068=CARTESIAN_POINT('Ctrl Pts',(-1.79241856003044,-2.07120103946552,
12.5269717671327));
#437069=CARTESIAN_POINT('Ctrl Pts',(-1.79182388067692,-2.07054242314726,
12.5299036066169));
#437070=CARTESIAN_POINT('Ctrl Pts',(-1.79107950309077,-2.06998712670806,
12.532813300402));
#437071=CARTESIAN_POINT('Ctrl Pts',(-1.79072215850561,-2.06972055208331,
12.5342101228452));
#437072=CARTESIAN_POINT('Ctrl Pts',(-1.79033044757617,-2.06947854081411,
12.5356023438239));
#437073=CARTESIAN_POINT('Ctrl Pts',(-1.7899123001692,-2.06925956785762,
12.5369868989719));
#437074=CARTESIAN_POINT('Origin',(-13.0832437096424,-7.97730267717418,-1.24008275899548));
#437075=CARTESIAN_POINT('Ctrl Pts',(-1.70768498702298,-2.13757346666599,
12.5369868989719));
#437076=CARTESIAN_POINT('Ctrl Pts',(-1.71222831500884,-2.15222411424545,
12.5369868989719));
#437077=CARTESIAN_POINT('Ctrl Pts',(-1.70005241588022,-2.16155314335328,
12.5369868989719));
#437078=CARTESIAN_POINT('Ctrl Pts',(-1.70922074632988,-2.14252597814296,
12.5218025310015));
#437079=CARTESIAN_POINT('Ctrl Pts',(-1.70941265130796,-2.15434202808292,
12.5216901060417));
#437080=CARTESIAN_POINT('Ctrl Pts',(-1.70008954208609,-2.16152471847184,
12.5161920673678));
#437081=CARTESIAN_POINT('Ctrl Pts',(-1.71493865396465,-2.14443427672418,
12.5042015548895));
#437082=CARTESIAN_POINT('Ctrl Pts',(-1.71384623655552,-2.15077335940398,
12.4980677368514));
#437083=CARTESIAN_POINT('Ctrl Pts',(-1.70852720123522,-2.15500403818936,
12.4907278922777));
#437084=CARTESIAN_POINT('Ctrl Pts',(-1.72369009019854,-2.13445172501886,
12.506463626192));
#437085=CARTESIAN_POINT('Ctrl Pts',(-1.72780071734796,-2.13954192960951,
12.4999376786891));
#437086=CARTESIAN_POINT('Ctrl Pts',(-1.72775051201418,-2.13947976016159,
12.4906970594712));
#437087=CARTESIAN_POINT('Origin',(-1.68667218602388,-2.14408976885145,12.5369868989719));
#437088=CARTESIAN_POINT('Origin',(-1.68667218602388,-2.14408976885145,14.));
#437089=CARTESIAN_POINT('Origin',(-1.68667218602388,-2.14408976885145,13.7435492065112));
#437090=CARTESIAN_POINT('Ctrl Pts',(-1.7004084099681,-2.11395046384977,
13.793642941384));
#437091=CARTESIAN_POINT('Ctrl Pts',(-1.70361735137066,-2.12427562312607,
13.8071662555867));
#437092=CARTESIAN_POINT('Ctrl Pts',(-1.68827452819122,-2.13166596550781,
13.8103758687955));
#437093=CARTESIAN_POINT('Ctrl Pts',(-1.70530134754244,-2.12983507486535,
13.7804579775006));
#437094=CARTESIAN_POINT('Ctrl Pts',(-1.70925120729145,-2.1425783978108,
13.7901904343351));
#437095=CARTESIAN_POINT('Ctrl Pts',(-1.69634931075966,-2.15162256665308,
13.7927914348263));
#437096=CARTESIAN_POINT('Ctrl Pts',(-1.70818200399808,-2.13918694318659,
13.7597120340895));
#437097=CARTESIAN_POINT('Ctrl Pts',(-1.71274763058253,-2.15393625313195,
13.7635825532445));
#437098=CARTESIAN_POINT('Ctrl Pts',(-1.70108730461836,-2.16340053939947,
13.7651073818884));
#437099=CARTESIAN_POINT('Ctrl Pts',(-1.70761790550376,-2.1373556332361,
13.7381884353898));
#437100=CARTESIAN_POINT('Ctrl Pts',(-1.71207752372754,-2.15175944231302,
13.7368803041982));
#437101=CARTESIAN_POINT('Ctrl Pts',(-1.7001590061108,-2.16109424680689,
13.7363986145813));
#437102=CARTESIAN_POINT('Origin',(-1.68057055544076,-2.12428120016772,13.7902182540695));
#437103=CARTESIAN_POINT('Ctrl Pts',(-1.69106545301784,-2.08361903867141,
13.8235227101244));
#437104=CARTESIAN_POINT('Ctrl Pts',(-1.69445420415729,-2.09460535079307,
13.8358800583119));
#437105=CARTESIAN_POINT('Ctrl Pts',(-1.67975221738023,-2.10225241780362,
13.8390832900376));
#437106=CARTESIAN_POINT('Ctrl Pts',(-1.69457670011487,-2.09501808657546,
13.8124254819053));
#437107=CARTESIAN_POINT('Ctrl Pts',(-1.69797203189519,-2.10602573404153,
13.8247886449158));
#437108=CARTESIAN_POINT('Ctrl Pts',(-1.6832436034655,-2.11366734232083,
13.8279860620657));
#437109=CARTESIAN_POINT('Ctrl Pts',(-1.69808637358516,-2.10641202579702,
13.8013225099955));
#437110=CARTESIAN_POINT('Ctrl Pts',(-1.70148668587057,-2.11743581417462,
13.8136962257787));
#437111=CARTESIAN_POINT('Ctrl Pts',(-1.68673363241358,-2.12507690300919,
13.8168830918626));
#437112=CARTESIAN_POINT('Ctrl Pts',(-1.70159453465617,-2.11780105510718,
13.7902140179785));
#437113=CARTESIAN_POINT('Ctrl Pts',(-1.70499833188868,-2.12883612945875,
13.802602731458));
#437114=CARTESIAN_POINT('Ctrl Pts',(-1.69022235930942,-2.13648131008831,
13.8057746032558));
#437115=CARTESIAN_POINT('Origin',(-1.6700414701308,-2.09009917182332,13.8235269408515));
#437116=CARTESIAN_POINT('Ctrl Pts',(-1.73986539582215,-2.04305131259621,
13.8235269408515));
#437117=CARTESIAN_POINT('Ctrl Pts',(-1.75032541850696,-2.04852895298456,
13.8362179249168));
#437118=CARTESIAN_POINT('Ctrl Pts',(-1.76059090559615,-2.03488040804824,
13.8391868794938));
#437119=CARTESIAN_POINT('Ctrl Pts',(-1.73029493036326,-2.03803951006836,
13.8400110824519));
#437120=CARTESIAN_POINT('Ctrl Pts',(-1.74026835444688,-2.03940064008055,
13.8494522556837));
#437121=CARTESIAN_POINT('Ctrl Pts',(-1.74478849747539,-2.0267319308157,
13.85569149686));
#437122=CARTESIAN_POINT('Ctrl Pts',(-1.71403385118767,-2.03705207394814,
13.8586819406588));
#437123=CARTESIAN_POINT('Ctrl Pts',(-1.71739062393921,-2.03427932795733,
13.868010383617));
#437124=CARTESIAN_POINT('Ctrl Pts',(-1.71778593356539,-2.02523849851021,
13.8744918421245));
#437125=CARTESIAN_POINT('Ctrl Pts',(-1.68993962940601,-2.05701553994687,
13.8587686893867));
#437126=CARTESIAN_POINT('Ctrl Pts',(-1.68661269604077,-2.05976356511108,
13.8680909899357));
#437127=CARTESIAN_POINT('Ctrl Pts',(-1.67767777149484,-2.05847378805118,
13.8745789365163));
#437128=CARTESIAN_POINT('Ctrl Pts',(-1.68788114693638,-2.07328138212866,
13.8400379222776));
#437129=CARTESIAN_POINT('Ctrl Pts',(-1.68739152716436,-2.08333277538466,
13.8494748685453));
#437130=CARTESIAN_POINT('Ctrl Pts',(-1.67411680175335,-2.08546415299714,
13.8557104837033));
#437131=CARTESIAN_POINT('Ctrl Pts',(-1.69106661247695,-2.08362280022854,
13.8235269408542));
#437132=CARTESIAN_POINT('Ctrl Pts',(-1.69454250509754,-2.09490707199417,
13.8362179249195));
#437133=CARTESIAN_POINT('Ctrl Pts',(-1.67924918460769,-2.10250821351705,
13.8391868794965));
#437134=CARTESIAN_POINT('Origin',(-1.75007147480651,-2.02356193210926,13.8235269408515));
#437135=CARTESIAN_POINT('Ctrl Pts',(-1.77154713728628,-2.05964221138041,
13.7902140241682));
#437136=CARTESIAN_POINT('Ctrl Pts',(-1.78177531224088,-2.06500346426484,
13.8026027327198));
#437137=CARTESIAN_POINT('Ctrl Pts',(-1.7919896420872,-2.05187161755297,
13.8057746032556));
#437138=CARTESIAN_POINT('Ctrl Pts',(-1.76099000897013,-2.05411371931309,
13.8013225161808));
#437139=CARTESIAN_POINT('Ctrl Pts',(-1.7712077238797,-2.05946948535651,
13.8136962270464));
#437140=CARTESIAN_POINT('Ctrl Pts',(-1.78141384636714,-2.0463594255136,
13.8168830918628));
#437141=CARTESIAN_POINT('Ctrl Pts',(-1.75042832938096,-2.0485828438631,
13.8124254880875));
#437142=CARTESIAN_POINT('Ctrl Pts',(-1.76063108395295,-2.05393076628067,
13.8247886461867));
#437143=CARTESIAN_POINT('Ctrl Pts',(-1.77083322137131,-2.04084501241263,
13.8279860620656));
#437144=CARTESIAN_POINT('Ctrl Pts',(-1.73986191426544,-2.0430494885418,
13.8235227163065));
#437145=CARTESIAN_POINT('Ctrl Pts',(-1.75004489351111,-2.04838704574704,
13.8358800595847));
#437146=CARTESIAN_POINT('Ctrl Pts',(-1.76024757046894,-2.03532828571048,
13.8390832900376));
#437147=CARTESIAN_POINT('Origin',(-1.78175670884918,-2.04015466072339,13.7902182540695));
#437148=CARTESIAN_POINT('Ctrl Pts',(-1.78967324922472,-2.06913435199042,
13.7382347919292));
#437149=CARTESIAN_POINT('Ctrl Pts',(-1.80303032825568,-2.07615619708222,
13.7369371795943));
#437150=CARTESIAN_POINT('Ctrl Pts',(-1.81438748863182,-2.06612830172923,
13.7364597369711));
#437151=CARTESIAN_POINT('Ctrl Pts',(-1.7913489447432,-2.07001187037406,
13.7595490285574));
#437152=CARTESIAN_POINT('Ctrl Pts',(-1.8050251800755,-2.07720036072702,
13.7633824266926));
#437153=CARTESIAN_POINT('Ctrl Pts',(-1.81645963601905,-2.0674460346313,
13.7648920890506));
#437154=CARTESIAN_POINT('Ctrl Pts',(-1.7828029893974,-2.06553657469893,
13.7803806590111));
#437155=CARTESIAN_POINT('Ctrl Pts',(-1.79462993175343,-2.07175914012728,
13.7901039518744));
#437156=CARTESIAN_POINT('Ctrl Pts',(-1.80589361004016,-2.06073122133546,
13.7926933640892));
#437157=CARTESIAN_POINT('Ctrl Pts',(-1.76794821134497,-2.05775751173561,
13.7936647693663));
#437158=CARTESIAN_POINT('Ctrl Pts',(-1.7775154446249,-2.06280145655211,
13.8072068914932));
#437159=CARTESIAN_POINT('Ctrl Pts',(-1.78758503717726,-2.04904472817376,
13.8104111085397));
#437160=CARTESIAN_POINT('Origin',(-1.80011837915356,-2.04977018737067,13.7435492065112));
#437161=CARTESIAN_POINT('Origin',(-1.80011837915356,-2.04977018737067,14.));
#437162=CARTESIAN_POINT('Origin',(-1.80011837915356,-2.04977018737067,12.5369868989719));
#437163=CARTESIAN_POINT('Ctrl Pts',(-1.7838850227879,-2.08440754081258,
12.506462012331));
#437164=CARTESIAN_POINT('Ctrl Pts',(-1.78813652264298,-2.08937527037166,
12.4999388158272));
#437165=CARTESIAN_POINT('Ctrl Pts',(-1.7880862218242,-2.0893164956162,12.4907030323752));
#437166=CARTESIAN_POINT('Ctrl Pts',(-1.79529618154332,-2.07762417593863,
12.5042014951932));
#437167=CARTESIAN_POINT('Ctrl Pts',(-1.80172533465173,-2.07770836278244,
12.4980716682127));
#437168=CARTESIAN_POINT('Ctrl Pts',(-1.80685340911806,-2.07325545165674,
12.4907355092743));
#437169=CARTESIAN_POINT('Ctrl Pts',(-1.79446631813886,-2.0716545002376,
12.5218047446509));
#437170=CARTESIAN_POINT('Ctrl Pts',(-1.80604327938808,-2.07399818092629,
12.5216906929434));
#437171=CARTESIAN_POINT('Ctrl Pts',(-1.8148054042794,-2.06614987399298,
12.5161988840776));
#437172=CARTESIAN_POINT('Ctrl Pts',(-1.78987828362776,-2.06924171642266,
12.5369868989719));
#437173=CARTESIAN_POINT('Ctrl Pts',(-1.80344630185995,-2.07637715003048,
12.5369868989719));
#437174=CARTESIAN_POINT('Ctrl Pts',(-1.8148388702237,-2.06611971772031,
12.5369868989719));
#437175=CARTESIAN_POINT('Origin',(-3.293628469579E-31,-9.1133900549324E-31,
12.5));
#437176=CARTESIAN_POINT('Origin',(-1.56754848850674,-2.1780684097752,12.5));
#437177=CARTESIAN_POINT('',(-1.56754848850674,-2.1780684097752,12.5893111709658));
#437178=CARTESIAN_POINT('',(-1.56754848850674,-2.1780684097752,13.8235269408515));
#437179=CARTESIAN_POINT('',(-1.56754848850674,-2.1780684097752,12.5));
#437180=CARTESIAN_POINT('',(-1.59777583112556,-2.19718856817951,13.7902182540695));
#437181=CARTESIAN_POINT('',(-1.56754848850674,-2.1780684097752,13.8235269408515));
#437182=CARTESIAN_POINT('',(-1.61529264979877,-2.20826874654634,13.7435492065112));
#437183=CARTESIAN_POINT('Origin',(-1.55766237376227,-2.17181538148075,13.7445212918706));
#437184=CARTESIAN_POINT('',(-1.61529264979877,-2.20826874654634,12.5369868989719));
#437185=CARTESIAN_POINT('',(-1.61529264979877,-2.20826874654634,12.5));
#437186=CARTESIAN_POINT('Ctrl Pts',(-1.61529264979877,-2.20826874654634,
12.5369868989719));
#437187=CARTESIAN_POINT('Ctrl Pts',(-1.59938953659722,-2.1982093097189,
12.5544431401645));
#437188=CARTESIAN_POINT('Ctrl Pts',(-1.58347504906643,-2.18814267811487,
12.5718848856037));
#437189=CARTESIAN_POINT('Ctrl Pts',(-1.56754848850674,-2.1780684097752,
12.5893111709658));
#437190=CARTESIAN_POINT('Origin',(-1.57486859763885,-2.48306568694209,12.5));
#437191=CARTESIAN_POINT('',(-1.52777976988047,-2.26969385076738,13.7435492065112));
#437192=CARTESIAN_POINT('',(-1.52331302421127,-2.24945385392455,13.7902182540695));
#437193=CARTESIAN_POINT('Origin',(-1.51157518860124,-2.19626664039524,13.7418732680442));
#437194=CARTESIAN_POINT('',(-1.51560512620464,-2.21452734525963,13.8235269408515));
#437195=CARTESIAN_POINT('',(-1.52331302421127,-2.24945385392455,13.7902182540695));
#437196=CARTESIAN_POINT('',(-1.51560512620464,-2.21452734525963,12.5893111709658));
#437197=CARTESIAN_POINT('',(-1.51560512620464,-2.21452734525963,12.5));
#437198=CARTESIAN_POINT('',(-1.52777976988047,-2.26969385076738,12.5369868989719));
#437199=CARTESIAN_POINT('Ctrl Pts',(-1.51560512620464,-2.21452734525963,
12.5893111709658));
#437200=CARTESIAN_POINT('Ctrl Pts',(-1.51966635996702,-2.2329298612335,
12.5718848856037));
#437201=CARTESIAN_POINT('Ctrl Pts',(-1.52372451513673,-2.25131842729607,
12.5544431401645));
#437202=CARTESIAN_POINT('Ctrl Pts',(-1.52777976988047,-2.26969385076738,
12.5369868989719));
#437203=CARTESIAN_POINT('',(-1.52777976988047,-2.26969385076738,12.5));
#437204=CARTESIAN_POINT('Origin',(-1.54917241891494,-2.20711941133036,12.5));
#437205=CARTESIAN_POINT('',(-1.53035107720997,-2.17835576641872,13.8587068136939));
#437206=CARTESIAN_POINT('Ctrl Pts',(-1.51560512619815,-2.21452734526091,
13.8235269408542));
#437207=CARTESIAN_POINT('Ctrl Pts',(-1.5152274997187,-2.21281622058131,
13.8262006681044));
#437208=CARTESIAN_POINT('Ctrl Pts',(-1.51501071118043,-2.2110276930412,
13.8288634856214));
#437209=CARTESIAN_POINT('Ctrl Pts',(-1.51494345082546,-2.20916882630991,
13.8314912288862));
#437210=CARTESIAN_POINT('Ctrl Pts',(-1.51487411233706,-2.20725252644317,
13.8342001611531));
#437211=CARTESIAN_POINT('Ctrl Pts',(-1.51496311109849,-2.2052593631498,
13.836875030195));
#437212=CARTESIAN_POINT('Ctrl Pts',(-1.5152380107614,-2.2031759382548,13.8394886372969));
#437213=CARTESIAN_POINT('Ctrl Pts',(-1.51525924192918,-2.20301503029649,
13.8396904925131));
#437214=CARTESIAN_POINT('Ctrl Pts',(-1.51528160409637,-2.20285358301223,
13.8398919674349));
#437215=CARTESIAN_POINT('Ctrl Pts',(-1.5153051213929,-2.20269159075557,
13.8400930404591));
#437216=CARTESIAN_POINT('Ctrl Pts',(-1.51567153669451,-2.20016764241355,
13.8432258934518));
#437217=CARTESIAN_POINT('Ctrl Pts',(-1.51631538464042,-2.19752411509091,
13.8462331177034));
#437218=CARTESIAN_POINT('Ctrl Pts',(-1.51730939280566,-2.19487005409481,
13.8489036603661));
#437219=CARTESIAN_POINT('Ctrl Pts',(-1.51763464384518,-2.19400161445002,
13.8497774930041));
#437220=CARTESIAN_POINT('Ctrl Pts',(-1.51799744051924,-2.19313229083374,
13.85061494757));
#437221=CARTESIAN_POINT('Ctrl Pts',(-1.51840047578048,-2.19226660249271,
13.8514076489583));
#437222=CARTESIAN_POINT('Ctrl Pts',(-1.51925295348439,-2.19043554680052,
13.8530843267192));
#437223=CARTESIAN_POINT('Ctrl Pts',(-1.52037186930745,-2.18844214531363,
13.8546805203176));
#437224=CARTESIAN_POINT('Ctrl Pts',(-1.52181126498018,-2.18646888077616,
13.8559412814273));
#437225=CARTESIAN_POINT('Ctrl Pts',(-1.52200390280191,-2.18620479398656,
13.8561100121513));
#437226=CARTESIAN_POINT('Ctrl Pts',(-1.52220220416813,-2.18594107360209,
13.8562727473908));
#437227=CARTESIAN_POINT('Ctrl Pts',(-1.52240622287091,-2.18567815319846,
13.8564289040185));
#437228=CARTESIAN_POINT('Ctrl Pts',(-1.52333144536046,-2.18448581216754,
13.8571370725437));
#437229=CARTESIAN_POINT('Ctrl Pts',(-1.52439231259193,-2.18329036118281,
13.8577210840553));
#437230=CARTESIAN_POINT('Ctrl Pts',(-1.52556953946978,-2.18215774739768,
13.8581177131616));
#437231=CARTESIAN_POINT('Ctrl Pts',(-1.5259010870775,-2.18183876437241,
13.8582294175695));
#437232=CARTESIAN_POINT('Ctrl Pts',(-1.52624171826153,-2.18152466407897,
13.8583265086086));
#437233=CARTESIAN_POINT('Ctrl Pts',(-1.52659065690888,-2.1812166476676,
13.8584082369006));
#437234=CARTESIAN_POINT('Ctrl Pts',(-1.52709198817353,-2.18077411068233,
13.8585256585398));
#437235=CARTESIAN_POINT('Ctrl Pts',(-1.52761691440119,-2.18033887267123,
13.8586122832068));
#437236=CARTESIAN_POINT('Ctrl Pts',(-1.52815230356963,-2.17992284776219,
13.8586682984299));
#437237=CARTESIAN_POINT('Ctrl Pts',(-1.52858056183296,-2.17959006907418,
13.8587131050557));
#437238=CARTESIAN_POINT('Ctrl Pts',(-1.52902010096034,-2.17926572302709,
13.8587357943552));
#437239=CARTESIAN_POINT('Ctrl Pts',(-1.52947127388974,-2.17895017858655,
13.8587355499465));
#437240=CARTESIAN_POINT('Ctrl Pts',(-1.52976287771037,-2.17874623469178,
13.8587353919793));
#437241=CARTESIAN_POINT('Ctrl Pts',(-1.53005616584286,-2.17854814126293,
13.8587257282814));
#437242=CARTESIAN_POINT('Ctrl Pts',(-1.53035107720997,-2.17835576641872,
13.8587068136939));
#437243=CARTESIAN_POINT('Ctrl Pts',(-1.53035107720997,-2.17835576641872,
13.8587068136939));
#437244=CARTESIAN_POINT('Ctrl Pts',(-1.53132102461955,-2.17772305604325,
13.8586446046466));
#437245=CARTESIAN_POINT('Ctrl Pts',(-1.53230850981748,-2.17715212784241,
13.858482427929));
#437246=CARTESIAN_POINT('Ctrl Pts',(-1.53331156551055,-2.17663896737792,
13.8582284286032));
#437247=CARTESIAN_POINT('Ctrl Pts',(-1.53434058397129,-2.17611252443469,
13.8579678548414));
#437248=CARTESIAN_POINT('Ctrl Pts',(-1.53538920061079,-2.17564695602143,
13.857615680862));
#437249=CARTESIAN_POINT('Ctrl Pts',(-1.53641214255887,-2.1752517607806,
13.8571944833187));
#437250=CARTESIAN_POINT('Ctrl Pts',(-1.53896499880822,-2.17426551063984,
13.8561433417727));
#437251=CARTESIAN_POINT('Ctrl Pts',(-1.54147563877766,-2.17366693988258,
13.8546163505474));
#437252=CARTESIAN_POINT('Ctrl Pts',(-1.54377573856338,-2.1733359446785,
13.8528973491086));
#437253=CARTESIAN_POINT('Ctrl Pts',(-1.54419593285942,-2.1732754767381,
13.8525833129072));
#437254=CARTESIAN_POINT('Ctrl Pts',(-1.54460914737315,-2.17322380547224,
13.8522628768812));
#437255=CARTESIAN_POINT('Ctrl Pts',(-1.54501444065091,-2.17318004119271,
13.851937733538));
#437256=CARTESIAN_POINT('Ctrl Pts',(-1.54748951046632,-2.17291277880968,
13.8499521282529));
#437257=CARTESIAN_POINT('Ctrl Pts',(-1.54991558086299,-2.17291789146262,
13.847639871647));
#437258=CARTESIAN_POINT('Ctrl Pts',(-1.55216531585744,-2.17311476993172,
13.8452109780794));
#437259=CARTESIAN_POINT('Ctrl Pts',(-1.55317751819863,-2.17320334963015,
13.8441181685877));
#437260=CARTESIAN_POINT('Ctrl Pts',(-1.55415433120731,-2.17333009894648,
13.8430021611332));
#437261=CARTESIAN_POINT('Ctrl Pts',(-1.55508642514008,-2.17348526674203,
13.8418824960098));
#437262=CARTESIAN_POINT('Ctrl Pts',(-1.55728292829453,-2.1738509236146,
13.8392439765549));
#437263=CARTESIAN_POINT('Ctrl Pts',(-1.55933672017995,-2.17438814335857,
13.8364981347964));
#437264=CARTESIAN_POINT('Ctrl Pts',(-1.5612618921482,-2.17506524004704,
13.8336931113419));
#437265=CARTESIAN_POINT('Ctrl Pts',(-1.56313688738556,-2.17572468922201,
13.8309611966328));
#437266=CARTESIAN_POINT('Ctrl Pts',(-1.56489157153951,-2.17651801226898,
13.8281701127186));
#437267=CARTESIAN_POINT('Ctrl Pts',(-1.56651332916587,-2.17744572633109,
13.8253580685121));
#437268=CARTESIAN_POINT('Ctrl Pts',(-1.56686492796953,-2.17764685574097,
13.8247484142933));
#437269=CARTESIAN_POINT('Ctrl Pts',(-1.56721012367397,-2.17785437874765,
13.8241378483365));
#437270=CARTESIAN_POINT('Ctrl Pts',(-1.56754848850674,-2.1780684097752,
13.8235269408515));
#437271=CARTESIAN_POINT('',(-1.52932415948195,-2.17905449156983,12.5969504640361));
#437272=CARTESIAN_POINT('Origin',(-1.54919158689835,-2.20714637929695,12.584524458991));
#437273=CARTESIAN_POINT('Origin',(-1.54919158689835,-2.20714637929695,12.584524458991));
#437274=CARTESIAN_POINT('Ctrl Pts',(-1.51560512620464,-2.21452734525963,
12.5893111709658));
#437275=CARTESIAN_POINT('Ctrl Pts',(-1.51316261792752,-2.20345969926439,
12.5770542771492));
#437276=CARTESIAN_POINT('Ctrl Pts',(-1.5282051163788,-2.1970155612151,12.5737548217797));
#437277=CARTESIAN_POINT('Ctrl Pts',(-1.52094607207655,-2.23872857263882,
12.5663937883685));
#437278=CARTESIAN_POINT('Ctrl Pts',(-1.51850044804093,-2.22764680832408,
12.5540940315304));
#437279=CARTESIAN_POINT('Ctrl Pts',(-1.53359082465374,-2.22118565293236,
12.5508374392248));
#437280=CARTESIAN_POINT('Ctrl Pts',(-1.52628162899956,-2.26290538127628,
12.5434499600945));
#437281=CARTESIAN_POINT('Ctrl Pts',(-1.52382805336934,-2.25178758619933,
12.5311293540532));
#437282=CARTESIAN_POINT('Ctrl Pts',(-1.53897011935321,-2.24533238656652,
12.5278936106989));
#437283=CARTESIAN_POINT('Ctrl Pts',(-1.5316122190974,-2.28705968392546,
12.5204817579905));
#437284=CARTESIAN_POINT('Ctrl Pts',(-1.52914649994453,-2.27588686336092,
12.5081597038247));
#437285=CARTESIAN_POINT('Ctrl Pts',(-1.54434348544273,-2.26945758061226,
12.5049254088044));
#437286=CARTESIAN_POINT('Ctrl Pts',(-1.52777976988047,-2.26969385076738,
12.5369868989719));
#437287=CARTESIAN_POINT('Ctrl Pts',(-1.527980512611,-2.27060346800934,12.5342545179733));
#437288=CARTESIAN_POINT('Ctrl Pts',(-1.52829390723081,-2.27144468196882,
12.5314872231885));
#437289=CARTESIAN_POINT('Ctrl Pts',(-1.52875468344491,-2.27215059017153,
12.5287124745063));
#437290=CARTESIAN_POINT('Ctrl Pts',(-1.52917023430568,-2.27278721322688,
12.5262100684184));
#437291=CARTESIAN_POINT('Ctrl Pts',(-1.52970605984781,-2.27331260767502,
12.5237004536639));
#437292=CARTESIAN_POINT('Ctrl Pts',(-1.53041777203167,-2.27368846182062,
12.5212220730815));
#437293=CARTESIAN_POINT('Ctrl Pts',(-1.53096264927644,-2.27397621068306,
12.5193246583486));
#437294=CARTESIAN_POINT('Ctrl Pts',(-1.53161742607129,-2.27417918844543,
12.517417831369));
#437295=CARTESIAN_POINT('Ctrl Pts',(-1.53242865116297,-2.27421202979317,
12.5155812248347));
#437296=CARTESIAN_POINT('Ctrl Pts',(-1.53277423741238,-2.27422602038384,
12.5147988205793));
#437297=CARTESIAN_POINT('Ctrl Pts',(-1.53314855560214,-2.27420942551876,
12.5140295443047));
#437298=CARTESIAN_POINT('Ctrl Pts',(-1.53355633159097,-2.27415744960347,
12.5132817086137));
#437299=CARTESIAN_POINT('Ctrl Pts',(-1.53417344538737,-2.27407879108683,
12.5121499604604));
#437300=CARTESIAN_POINT('Ctrl Pts',(-1.53487960852689,-2.27391030744599,
12.5110494206568));
#437301=CARTESIAN_POINT('Ctrl Pts',(-1.53567829388182,-2.27361491987427,
12.5100666561695));
#437302=CARTESIAN_POINT('Ctrl Pts',(-1.53613689717341,-2.27344530901081,
12.5095023550641));
#437303=CARTESIAN_POINT('Ctrl Pts',(-1.53663107763282,-2.27323128562668,
12.5089719619137));
#437304=CARTESIAN_POINT('Ctrl Pts',(-1.5371490340964,-2.27297100042007,
12.5085043804652));
#437305=CARTESIAN_POINT('Ctrl Pts',(-1.53790699591229,-2.27259010692472,
12.5078201359221));
#437306=CARTESIAN_POINT('Ctrl Pts',(-1.53873731398321,-2.27209801962174,
12.5072563000949));
#437307=CARTESIAN_POINT('Ctrl Pts',(-1.53957938870058,-2.27152081172439,
12.5068768744332));
#437308=CARTESIAN_POINT('Ctrl Pts',(-1.54018658254042,-2.27110460509528,
12.5066032824114));
#437309=CARTESIAN_POINT('Ctrl Pts',(-1.54081059057126,-2.27063687825392,
12.5064197834844));
#437310=CARTESIAN_POINT('Ctrl Pts',(-1.54141811688731,-2.27014581861132,
12.5063282718343));
#437311=CARTESIAN_POINT('Ctrl Pts',(-1.54230491722335,-2.26942902356136,
12.5061946931565));
#437312=CARTESIAN_POINT('Ctrl Pts',(-1.54317622205301,-2.26864801884064,
12.5062515701262));
#437313=CARTESIAN_POINT('Ctrl Pts',(-1.54398827872502,-2.26786279047885,
12.5064436508398));
#437314=CARTESIAN_POINT('',(-1.5282051163788,-2.19701556121511,12.5737548217797));
#437315=CARTESIAN_POINT('Origin',(-1.53708819353923,-2.20978626754489,12.5893111709658));
#437316=CARTESIAN_POINT('Ctrl Pts',(-1.54398827872502,-2.26786279047885,
12.5064436508398));
#437317=CARTESIAN_POINT('Ctrl Pts',(-1.54165242958721,-2.25737545542381,
12.5164271754438));
#437318=CARTESIAN_POINT('Ctrl Pts',(-1.53931545058102,-2.24688400861484,
12.5264061185523));
#437319=CARTESIAN_POINT('Ctrl Pts',(-1.53697730283729,-2.23638830503363,
12.536380305637));
#437320=CARTESIAN_POINT('Ctrl Pts',(-1.53405509238508,-2.22327080431518,
12.5488460165097));
#437321=CARTESIAN_POINT('Ctrl Pts',(-1.53113105548609,-2.21014665067863,
12.5613043021964));
#437322=CARTESIAN_POINT('Ctrl Pts',(-1.5282051163788,-2.19701556121511,
12.5737548217797));
#437323=CARTESIAN_POINT('Ctrl Pts',(-1.56754848850674,-2.1780684097752,
12.5893111709658));
#437324=CARTESIAN_POINT('Ctrl Pts',(-1.55796993226765,-2.17200954066172,
12.5770542771492));
#437325=CARTESIAN_POINT('Ctrl Pts',(-1.54679665878452,-2.18396619715615,
12.5737548217797));
#437326=CARTESIAN_POINT('Ctrl Pts',(-1.55861177884555,-2.17241553758958,
12.5928319619712));
#437327=CARTESIAN_POINT('Ctrl Pts',(-1.5504328844881,-2.17109678686975,
12.5821634970842));
#437328=CARTESIAN_POINT('Ctrl Pts',(-1.54354627755795,-2.18189901568095,
12.5773203894503));
#437329=CARTESIAN_POINT('Ctrl Pts',(-1.54201075355491,-2.17018169367406,
12.5969440695591));
#437330=CARTESIAN_POINT('Ctrl Pts',(-1.53871010216729,-2.1724760874871,
12.5878292599214));
#437331=CARTESIAN_POINT('Ctrl Pts',(-1.53762906054079,-2.18110485582971,
12.5813877129824));
#437332=CARTESIAN_POINT('Ctrl Pts',(-1.51693613904987,-2.18771563085215,
12.596957478804));
#437333=CARTESIAN_POINT('Ctrl Pts',(-1.52021244349124,-2.18543825904317,
12.5878468778671));
#437334=CARTESIAN_POINT('Ctrl Pts',(-1.5286579268001,-2.18738538349153,
12.5814011370086));
#437335=CARTESIAN_POINT('Ctrl Pts',(-1.51332297835558,-2.20418633444784,
12.5928371701607));
#437336=CARTESIAN_POINT('Ctrl Pts',(-1.51486750657731,-2.1960531002648,
12.5821692192951));
#437337=CARTESIAN_POINT('Ctrl Pts',(-1.52736284135469,-2.1932441092059,
12.5773318885715));
#437338=CARTESIAN_POINT('Ctrl Pts',(-1.51560512620458,-2.21452734525964,
12.5893111709658));
#437339=CARTESIAN_POINT('Ctrl Pts',(-1.51316261792746,-2.2034596992644,
12.5770542771492));
#437340=CARTESIAN_POINT('Ctrl Pts',(-1.52820511637874,-2.19701556121512,
12.5737548217797));
#437341=CARTESIAN_POINT('',(-1.54679665878452,-2.18396619715615,12.5737548217797));
#437342=CARTESIAN_POINT('Origin',(-1.55578780396799,-2.1966610507705,12.5893111709658));
#437343=CARTESIAN_POINT('Ctrl Pts',(-1.52820511637874,-2.19701556121512,
12.5737548217797));
#437344=CARTESIAN_POINT('Ctrl Pts',(-1.527957344847,-2.19604451595402,12.5746934679442));
#437345=CARTESIAN_POINT('Ctrl Pts',(-1.52786066643634,-2.19492469957481,
12.5756680099006));
#437346=CARTESIAN_POINT('Ctrl Pts',(-1.52792276274019,-2.1937838018068,
12.5765688348656));
#437347=CARTESIAN_POINT('Ctrl Pts',(-1.5279392020492,-2.19348176175288,
12.5768073183026));
#437348=CARTESIAN_POINT('Ctrl Pts',(-1.52796651697544,-2.19317829309718,
12.5770407398754));
#437349=CARTESIAN_POINT('Ctrl Pts',(-1.52800428799108,-2.19287572989175,
12.5772674179684));
#437350=CARTESIAN_POINT('Ctrl Pts',(-1.52815929002556,-2.19163409231321,
12.5781976435658));
#437351=CARTESIAN_POINT('Ctrl Pts',(-1.52851037564396,-2.19033857837221,
12.5790594849312));
#437352=CARTESIAN_POINT('Ctrl Pts',(-1.52908044701501,-2.18908929403484,
12.5797571720116));
#437353=CARTESIAN_POINT('Ctrl Pts',(-1.52945186901119,-2.18827534036879,
12.580211740231));
#437354=CARTESIAN_POINT('Ctrl Pts',(-1.52995020827331,-2.18745181443711,
12.5806009430798));
#437355=CARTESIAN_POINT('Ctrl Pts',(-1.53055554142144,-2.18668586114604,
12.5808812374708));
#437356=CARTESIAN_POINT('Ctrl Pts',(-1.53107572341285,-2.18602765316665,
12.5811221033394));
#437357=CARTESIAN_POINT('Ctrl Pts',(-1.53168565420794,-2.18539855525862,
12.581287365893));
#437358=CARTESIAN_POINT('Ctrl Pts',(-1.53235689466196,-2.18483987866494,
12.581359338449));
#437359=CARTESIAN_POINT('Ctrl Pts',(-1.53245018322449,-2.18476223415464,
12.5813693411482));
#437360=CARTESIAN_POINT('Ctrl Pts',(-1.532544635223,-2.18468589369265,12.5813775999465));
#437361=CARTESIAN_POINT('Ctrl Pts',(-1.53264015405337,-2.18461091027627,
12.5813841266931));
#437362=CARTESIAN_POINT('Ctrl Pts',(-1.53280221330185,-2.18448369184134,
12.5813952001081));
#437363=CARTESIAN_POINT('Ctrl Pts',(-1.53296880481113,-2.18436000657486,
12.5814007534795));
#437364=CARTESIAN_POINT('Ctrl Pts',(-1.5331399735842,-2.18424006668586,
12.5814005856065));
#437365=CARTESIAN_POINT('Ctrl Pts',(-1.53392351730465,-2.18369102876748,
12.5813998171494));
#437366=CARTESIAN_POINT('Ctrl Pts',(-1.5347486447913,-2.18325813128369,
12.58127954464));
#437367=CARTESIAN_POINT('Ctrl Pts',(-1.53559692470179,-2.18291762974099,
12.5810700125799));
#437368=CARTESIAN_POINT('Ctrl Pts',(-1.53662155024926,-2.18250634264661,
12.5808169217085));
#437369=CARTESIAN_POINT('Ctrl Pts',(-1.53768628192706,-2.18224535449793,
12.5804173076348));
#437370=CARTESIAN_POINT('Ctrl Pts',(-1.53869160846448,-2.18213224428254,
12.5799304713245));
#437371=CARTESIAN_POINT('Ctrl Pts',(-1.53993752475485,-2.18199206509227,
12.5793271277669));
#437372=CARTESIAN_POINT('Ctrl Pts',(-1.54116588687115,-2.18203831787197,
12.5785808224116));
#437373=CARTESIAN_POINT('Ctrl Pts',(-1.54232611040979,-2.18223735857984,
12.5777485681082));
#437374=CARTESIAN_POINT('Ctrl Pts',(-1.54405497059434,-2.18253395104111,
12.576508418016));
#437375=CARTESIAN_POINT('Ctrl Pts',(-1.54561913869913,-2.18316052717434,
12.5750928681475));
#437376=CARTESIAN_POINT('Ctrl Pts',(-1.54679665878452,-2.18396619715615,
12.5737548217797));
#437377=CARTESIAN_POINT('Ctrl Pts',(-1.54679665878452,-2.18396619715615,
12.5737548217797));
#437378=CARTESIAN_POINT('Ctrl Pts',(-1.55796993226765,-2.17200954066172,
12.5770542771492));
#437379=CARTESIAN_POINT('Ctrl Pts',(-1.56754848850674,-2.1780684097752,
12.5893111709658));
#437380=CARTESIAN_POINT('Ctrl Pts',(-1.56769411036162,-2.19724443016183,
12.5508408821982));
#437381=CARTESIAN_POINT('Ctrl Pts',(-1.57889965365159,-2.18524853402163,
12.55409748406));
#437382=CARTESIAN_POINT('Ctrl Pts',(-1.58849042967524,-2.19131513270037,
12.5663972313419));
#437383=CARTESIAN_POINT('Ctrl Pts',(-1.58857178032965,-2.21050869646258,
12.52790050457));
#437384=CARTESIAN_POINT('Ctrl Pts',(-1.59978928963743,-2.19846217155821,
12.5311362602938));
#437385=CARTESIAN_POINT('Ctrl Pts',(-1.60941124386633,-2.20454849185883,
12.5434568539655));
#437386=CARTESIAN_POINT('Ctrl Pts',(-1.60943121340021,-2.22376006976241,
12.5049357605811));
#437387=CARTESIAN_POINT('Ctrl Pts',(-1.62064301892296,-2.21165309648626,
12.5081700652078));
#437388=CARTESIAN_POINT('Ctrl Pts',(-1.63031258574915,-2.21776953390351,
12.5204921097672));
#437389=CARTESIAN_POINT('Ctrl Pts',(-1.60806150210938,-2.22288993130809,
12.5064436508395));
#437390=CARTESIAN_POINT('Ctrl Pts',(-1.60915733426334,-2.22235327529076,
12.5062361689309));
#437391=CARTESIAN_POINT('Ctrl Pts',(-1.610274025824,-2.22174846823163,12.5061871075061));
#437392=CARTESIAN_POINT('Ctrl Pts',(-1.61132029812014,-2.22110323112525,
12.5063648335164));
#437393=CARTESIAN_POINT('Ctrl Pts',(-1.6117955795338,-2.22081012463166,
12.5064455676329));
#437394=CARTESIAN_POINT('Ctrl Pts',(-1.61226284321535,-2.2205043995009,
12.506574497099));
#437395=CARTESIAN_POINT('Ctrl Pts',(-1.61270147889601,-2.22019828487513,
12.5067492519495));
#437396=CARTESIAN_POINT('Ctrl Pts',(-1.61358293432294,-2.21958313565211,
12.5071004286051));
#437397=CARTESIAN_POINT('Ctrl Pts',(-1.61438072828498,-2.21894313395972,
12.5076537929613));
#437398=CARTESIAN_POINT('Ctrl Pts',(-1.6150409007624,-2.21833369311237,
12.5083435010505));
#437399=CARTESIAN_POINT('Ctrl Pts',(-1.61508246256507,-2.21829532516899,
12.5083869222964));
#437400=CARTESIAN_POINT('Ctrl Pts',(-1.61512347534805,-2.21825706539857,
12.5084308732337));
#437401=CARTESIAN_POINT('Ctrl Pts',(-1.61516392457745,-2.2182189222485,
12.5084753333615));
#437402=CARTESIAN_POINT('Ctrl Pts',(-1.61548838078535,-2.21791296384052,
12.5088319622689));
#437403=CARTESIAN_POINT('Ctrl Pts',(-1.61578404914335,-2.21760923609894,
12.509227847131));
#437404=CARTESIAN_POINT('Ctrl Pts',(-1.61604414426715,-2.21731872357072,
12.5096423454524));
#437405=CARTESIAN_POINT('Ctrl Pts',(-1.61685916727184,-2.21640838588275,
12.5109411997424));
#437406=CARTESIAN_POINT('Ctrl Pts',(-1.61738222279126,-2.21557826841318,
12.5124831113042));
#437407=CARTESIAN_POINT('Ctrl Pts',(-1.61770690066132,-2.21484239970466,
12.5140723025008));
#437408=CARTESIAN_POINT('Ctrl Pts',(-1.61773732333336,-2.2147734480007,
12.5142212114565));
#437409=CARTESIAN_POINT('Ctrl Pts',(-1.61776603322498,-2.21470531760595,
12.5143705582413));
#437410=CARTESIAN_POINT('Ctrl Pts',(-1.61779312419301,-2.21463801804078,
12.5145201959299));
#437411=CARTESIAN_POINT('Ctrl Pts',(-1.6181411480116,-2.21377345492755,
12.5164425148273));
#437412=CARTESIAN_POINT('Ctrl Pts',(-1.61824388319819,-2.21302039233999,
12.518463520594));
#437413=CARTESIAN_POINT('Ctrl Pts',(-1.61818448453867,-2.21234385514217,
12.5205025929157));
#437414=CARTESIAN_POINT('Ctrl Pts',(-1.61815003096181,-2.211951436752,12.5216853356836));
#437415=CARTESIAN_POINT('Ctrl Pts',(-1.61806157204364,-2.21158543159583,
12.5228750347131));
#437416=CARTESIAN_POINT('Ctrl Pts',(-1.61793731198208,-2.21124459837319,
12.5240609649613));
#437417=CARTESIAN_POINT('Ctrl Pts',(-1.6176323223273,-2.2104080415133,12.5269717671327));
#437418=CARTESIAN_POINT('Ctrl Pts',(-1.6170933050645,-2.20970314479846,
12.5299036066169));
#437419=CARTESIAN_POINT('Ctrl Pts',(-1.61639666614827,-2.20908902237862,
12.532813300402));
#437420=CARTESIAN_POINT('Ctrl Pts',(-1.61606223890442,-2.20879420785782,
12.5342101228452));
#437421=CARTESIAN_POINT('Ctrl Pts',(-1.61569155752594,-2.20852107378394,
12.5356023438238));
#437422=CARTESIAN_POINT('Ctrl Pts',(-1.61529264979877,-2.20826874654634,
12.5369868989719));
#437423=CARTESIAN_POINT('Origin',(-12.389845183083,-9.01739099410739,-1.24054046559061));
#437424=CARTESIAN_POINT('Ctrl Pts',(-1.52777072430559,-2.26965304710934,
12.5369868989719));
#437425=CARTESIAN_POINT('Ctrl Pts',(-1.53110477095469,-2.28462526927665,
12.5369868989719));
#437426=CARTESIAN_POINT('Ctrl Pts',(-1.5182089836472,-2.29293080799521,
12.5369868989719));
#437427=CARTESIAN_POINT('Ctrl Pts',(-1.52889769783785,-2.27471425815371,
12.5218025310016));
#437428=CARTESIAN_POINT('Ctrl Pts',(-1.52812584650303,-2.28650663319956,
12.5216901060418));
#437429=CARTESIAN_POINT('Ctrl Pts',(-1.51824830321041,-2.29290550382566,
12.5161920673678));
#437430=CARTESIAN_POINT('Ctrl Pts',(-1.53444103555654,-2.27708226958361,
12.5042015548894));
#437431=CARTESIAN_POINT('Ctrl Pts',(-1.5328355589886,-2.28331121732834,
12.4980677368513));
#437432=CARTESIAN_POINT('Ctrl Pts',(-1.52718938272283,-2.28709426812096,
12.4907278922777));
#437433=CARTESIAN_POINT('Ctrl Pts',(-1.54397702274574,-2.26784625729298,
12.506463626192));
#437434=CARTESIAN_POINT('Ctrl Pts',(-1.54765907319314,-2.27325457892166,
12.4999376786891));
#437435=CARTESIAN_POINT('Ctrl Pts',(-1.54761410230062,-2.27318852413666,
12.4906970594712));
#437436=CARTESIAN_POINT('Origin',(-1.50629670254587,-2.27443492848211,12.5369868989719));
#437437=CARTESIAN_POINT('Origin',(-1.50629670254587,-2.27443492848211,14.));
#437438=CARTESIAN_POINT('Origin',(-1.50629670254587,-2.27443492848211,13.7435492065112));
#437439=CARTESIAN_POINT('Ctrl Pts',(-1.52244385349537,-2.24551553930385,
13.793642941384));
#437440=CARTESIAN_POINT('Ctrl Pts',(-1.52480052107501,-2.25606790097908,
13.8071662555867));
#437441=CARTESIAN_POINT('Ctrl Pts',(-1.50890636836131,-2.26218307008128,
13.8103758687955));
#437442=CARTESIAN_POINT('Ctrl Pts',(-1.52602576696028,-2.26174611542281,
13.7804579775006));
#437443=CARTESIAN_POINT('Ctrl Pts',(-1.52892378475354,-2.27476898625067,
13.7901904343352));
#437444=CARTESIAN_POINT('Ctrl Pts',(-1.5153276344955,-2.28273143702447,
13.7927914348263));
#437445=CARTESIAN_POINT('Ctrl Pts',(-1.5281345741825,-2.27130166641751,
13.7597120340895));
#437446=CARTESIAN_POINT('Ctrl Pts',(-1.53148280333467,-2.28637404020259,
13.7635825532445));
#437447=CARTESIAN_POINT('Ctrl Pts',(-1.51908984895029,-2.29485641002304,
13.7651073818884));
#437448=CARTESIAN_POINT('Ctrl Pts',(-1.5277216214414,-2.26943047073569,
13.7381884353898));
#437449=CARTESIAN_POINT('Ctrl Pts',(-1.53099235649522,-2.28414985261245,
13.7368803041982));
#437450=CARTESIAN_POINT('Ctrl Pts',(-1.5183526235363,-2.29248212648255,
13.7363986145813));
#437451=CARTESIAN_POINT('Origin',(-1.50182995687668,-2.25419493163929,13.7902182540695));
#437452=CARTESIAN_POINT('Ctrl Pts',(-1.51560427719888,-2.21452350171337,
13.8235227101244));
#437453=CARTESIAN_POINT('Ctrl Pts',(-1.51808626611861,-2.22574947246525,
13.8358800583119));
#437454=CARTESIAN_POINT('Ctrl Pts',(-1.50280989203645,-2.23217274608225,
13.8390832900376));
#437455=CARTESIAN_POINT('Ctrl Pts',(-1.51817471268307,-2.22617081946112,
13.8124254819053));
#437456=CARTESIAN_POINT('Ctrl Pts',(-1.5206615213185,-2.2374185909491,13.8247886449158));
#437457=CARTESIAN_POINT('Ctrl Pts',(-1.5053592385034,-2.2438342687582,13.8279860620657));
#437458=CARTESIAN_POINT('Ctrl Pts',(-1.52074399618169,-2.2378129172599,
13.8013225099955));
#437459=CARTESIAN_POINT('Ctrl Pts',(-1.52323445311582,-2.24907718190935,
13.8136962257787));
#437460=CARTESIAN_POINT('Ctrl Pts',(-1.50790766955075,-2.25549033483369,
13.8168830918626));
#437461=CARTESIAN_POINT('Ctrl Pts',(-1.52331217251677,-2.24944999821001,
13.7902140179785));
#437462=CARTESIAN_POINT('Ctrl Pts',(-1.5258051828905,-2.26072579533578,
13.802602731458));
#437463=CARTESIAN_POINT('Ctrl Pts',(-1.51045522294536,-2.26714115831884,
13.8057746032558));
#437464=CARTESIAN_POINT('Origin',(-1.49412205887004,-2.21926842297437,13.8235269408515));
#437465=CARTESIAN_POINT('Ctrl Pts',(-1.56754848850674,-2.1780684097752,
13.8235269408515));
#437466=CARTESIAN_POINT('Ctrl Pts',(-1.57752722778538,-2.18438041272197,
13.8362179249168));
#437467=CARTESIAN_POINT('Ctrl Pts',(-1.58887104043234,-2.1716140146909,
13.8391868794938));
#437468=CARTESIAN_POINT('Ctrl Pts',(-1.55841837641544,-2.17229320182404,
13.8400110824519));
#437469=CARTESIAN_POINT('Ctrl Pts',(-1.56824767002107,-2.17446272943999,
13.8494522556837));
#437470=CARTESIAN_POINT('Ctrl Pts',(-1.57378539006221,-2.1622046078799,
13.85569149686));
#437471=CARTESIAN_POINT('Ctrl Pts',(-1.54229188985012,-2.16998362240276,
13.8586819406588));
#437472=CARTESIAN_POINT('Ctrl Pts',(-1.5458634977564,-2.16749371063752,
13.868010383617));
#437473=CARTESIAN_POINT('Ctrl Pts',(-1.54699440355332,-2.15851518520896,
13.8744918421245));
#437474=CARTESIAN_POINT('Ctrl Pts',(-1.51665063179312,-2.1879167588602,
13.8587686893867));
#437475=CARTESIAN_POINT('Ctrl Pts',(-1.5131107789619,-2.19038446424236,
13.8680909899357));
#437476=CARTESIAN_POINT('Ctrl Pts',(-1.50431071344441,-2.18837069951095,
13.8745789365163));
#437477=CARTESIAN_POINT('Ctrl Pts',(-1.51327318161156,-2.20396069236267,
13.8400379222776));
#437478=CARTESIAN_POINT('Ctrl Pts',(-1.51196590914601,-2.21393873187997,
13.8494748685453));
#437479=CARTESIAN_POINT('Ctrl Pts',(-1.49856162722656,-2.21498100415174,
13.8557104837033));
#437480=CARTESIAN_POINT('Ctrl Pts',(-1.51560512619815,-2.21452734526091,
13.8235269408542));
#437481=CARTESIAN_POINT('Ctrl Pts',(-1.51814968016583,-2.22605738706032,
13.8362179249195));
#437482=CARTESIAN_POINT('Ctrl Pts',(-1.50228768333862,-2.23238668881565,
13.8391868794965));
#437483=CARTESIAN_POINT('Origin',(-1.57930917304549,-2.1594757687799,13.8235269408515));
#437484=CARTESIAN_POINT('Ctrl Pts',(-1.59777249931641,-2.19718645976062,
13.7902140241682));
#437485=CARTESIAN_POINT('Ctrl Pts',(-1.60752964898108,-2.20336356473089,
13.8026027327198));
#437486=CARTESIAN_POINT('Ctrl Pts',(-1.6187803589046,-2.19110797586335,
13.8057746032556));
#437487=CARTESIAN_POINT('Ctrl Pts',(-1.58770112240133,-2.19081585932922,
13.8013225161808));
#437488=CARTESIAN_POINT('Ctrl Pts',(-1.59744829405439,-2.19698664312471,
13.8136962270464));
#437489=CARTESIAN_POINT('Ctrl Pts',(-1.60868904809625,-2.18475209965617,
13.8168830918628));
#437490=CARTESIAN_POINT('Ctrl Pts',(-1.57762540362503,-2.18444251247466,
13.8124254880875));
#437491=CARTESIAN_POINT('Ctrl Pts',(-1.58735830404812,-2.19060425933693,
13.8247886461867));
#437492=CARTESIAN_POINT('Ctrl Pts',(-1.59859310511831,-2.178393616147,13.8279860620656));
#437493=CARTESIAN_POINT('Ctrl Pts',(-1.56754516721199,-2.17806630801099,
13.8235227163065));
#437494=CARTESIAN_POINT('Ctrl Pts',(-1.57725920297056,-2.18421611227764,
13.8358800595847));
#437495=CARTESIAN_POINT('Ctrl Pts',(-1.58849234153707,-2.17203241707693,
13.8390832900376));
#437496=CARTESIAN_POINT('Origin',(-1.60953651566431,-2.17859592718422,13.7902182540695));
#437497=CARTESIAN_POINT('Ctrl Pts',(-1.61506460053222,-2.20812446245339,
13.7382347919292));
#437498=CARTESIAN_POINT('Ctrl Pts',(-1.62780488942199,-2.21621166887702,
13.7369371795943));
#437499=CARTESIAN_POINT('Ctrl Pts',(-1.63994162634958,-2.20714285452394,
13.7364597369711));
#437500=CARTESIAN_POINT('Ctrl Pts',(-1.61666319441731,-2.20913564570813,
13.7595490285573));
#437501=CARTESIAN_POINT('Ctrl Pts',(-1.62970799450626,-2.21741495709601,
13.7633824266926));
#437502=CARTESIAN_POINT('Ctrl Pts',(-1.64189947137254,-2.20862510202744,
13.7648920890506));
#437503=CARTESIAN_POINT('Ctrl Pts',(-1.60851045317711,-2.20397866651274,
13.7803806590111));
#437504=CARTESIAN_POINT('Ctrl Pts',(-1.61979084550826,-2.21114453246598,
13.7901039518744));
#437505=CARTESIAN_POINT('Ctrl Pts',(-1.63191592259437,-2.20107140251142,
13.7926933640892));
#437506=CARTESIAN_POINT('Ctrl Pts',(-1.59433916902201,-2.19501468542339,
13.7936647693663));
#437507=CARTESIAN_POINT('Ctrl Pts',(-1.60346343979419,-2.20082166525979,
13.8072068914933));
#437508=CARTESIAN_POINT('Ctrl Pts',(-1.61462082768211,-2.18793147653482,
13.8104111085397));
#437509=CARTESIAN_POINT('Origin',(-1.62705333433752,-2.18967610555104,13.7435492065112));
#437510=CARTESIAN_POINT('Origin',(-1.62705333433752,-2.18967610555104,14.));
#437511=CARTESIAN_POINT('Origin',(-1.62705333433752,-2.18967610555104,12.5369868989719));
#437512=CARTESIAN_POINT('Ctrl Pts',(-1.608050727263,-2.22287503680982,12.506462012331));
#437513=CARTESIAN_POINT('Ctrl Pts',(-1.61188316452582,-2.22817277336579,
12.4999388158272));
#437514=CARTESIAN_POINT('Ctrl Pts',(-1.61183782176707,-2.22811009419478,
12.4907030323752));
#437515=CARTESIAN_POINT('Ctrl Pts',(-1.61997682353992,-2.2170443583975,
12.5042014951932));
#437516=CARTESIAN_POINT('Ctrl Pts',(-1.62637772216243,-2.21765230078023,
12.4980716682127));
#437517=CARTESIAN_POINT('Ctrl Pts',(-1.63185168697956,-2.21363219202466,
12.4907355092744));
#437518=CARTESIAN_POINT('Ctrl Pts',(-1.6196363054269,-2.21102690472837,
12.5218047446509));
#437519=CARTESIAN_POINT('Ctrl Pts',(-1.63098371355879,-2.21430641682998,
12.5216906929434));
#437520=CARTESIAN_POINT('Ctrl Pts',(-1.64035639307753,-2.2071984190128,
12.5161988840775));
#437521=CARTESIAN_POINT('Ctrl Pts',(-1.61526020150225,-2.20824818184664,
12.5369868989719));
#437522=CARTESIAN_POINT('Ctrl Pts',(-1.62820146919188,-2.21646579233303,
12.5369868989719));
#437523=CARTESIAN_POINT('Ctrl Pts',(-1.64039220568286,-2.20717109086776,
12.5369868989719));
#437524=CARTESIAN_POINT('Origin',(-2.95976792804887E-31,-9.36866969595883E-31,
12.5));
#437525=CARTESIAN_POINT('Origin',(-1.38479980462761,-2.29859082104314,12.5));
#437526=CARTESIAN_POINT('',(-1.38479980462761,-2.29859082104314,12.5893111709658));
#437527=CARTESIAN_POINT('',(-1.38479980462761,-2.29859082104314,13.8235269408515));
#437528=CARTESIAN_POINT('',(-1.38479980462761,-2.29859082104314,12.5));
#437529=CARTESIAN_POINT('',(-1.41336809784461,-2.32011116773805,13.7902182540695));
#437530=CARTESIAN_POINT('',(-1.38479980462761,-2.29859082104314,13.8235269408515));
#437531=CARTESIAN_POINT('',(-1.42992349334847,-2.33258226106549,13.7435492065112));
#437532=CARTESIAN_POINT('Origin',(-1.37545626496778,-2.29155278905242,13.7445212918694));
#437533=CARTESIAN_POINT('',(-1.42992349334847,-2.33258226106549,12.5369868989719));
#437534=CARTESIAN_POINT('',(-1.42992349334847,-2.33258226106549,12.5));
#437535=CARTESIAN_POINT('Ctrl Pts',(-1.42992349334847,-2.33258226106549,
12.5369868989719));
#437536=CARTESIAN_POINT('Ctrl Pts',(-1.41489323393287,-2.32126004482102,
12.5544431401645));
#437537=CARTESIAN_POINT('Ctrl Pts',(-1.39985222447626,-2.30992973062657,
12.5718848856037));
#437538=CARTESIAN_POINT('Ctrl Pts',(-1.38479980462761,-2.29859082104314,
12.5893111709658));
#437539=CARTESIAN_POINT('Origin',(-1.36723544715477,-2.6031699017816,12.5));
#437540=CARTESIAN_POINT('',(-1.33769508908193,-2.38666986617617,13.7435492065112));
#437541=CARTESIAN_POINT('',(-1.33489295378212,-2.36613313501387,13.7902182540695));
#437542=CARTESIAN_POINT('Origin',(-1.3275294265206,-2.31216615498027,13.7418732680447));
#437543=CARTESIAN_POINT('',(-1.33005753786832,-2.33069457618112,13.8235269408515));
#437544=CARTESIAN_POINT('',(-1.33489295378212,-2.36613313501387,13.7902182540695));
#437545=CARTESIAN_POINT('',(-1.33005753786832,-2.33069457618112,12.5893111709658));
#437546=CARTESIAN_POINT('',(-1.33005753786832,-2.33069457618112,12.5));
#437547=CARTESIAN_POINT('',(-1.33769508908193,-2.38666986617617,12.5369868989719));
#437548=CARTESIAN_POINT('Ctrl Pts',(-1.33005753786832,-2.33069457618112,
12.5893111709658));
#437549=CARTESIAN_POINT('Ctrl Pts',(-1.33260528231789,-2.34936688755548,
12.5718848856037));
#437550=CARTESIAN_POINT('Ctrl Pts',(-1.33515109546584,-2.36802504450183,
12.5544431401645));
#437551=CARTESIAN_POINT('Ctrl Pts',(-1.33769508908193,-2.38666986617617,
12.5369868989719));
#437552=CARTESIAN_POINT('',(-1.33769508908193,-2.38666986617617,12.5));
#437553=CARTESIAN_POINT('Origin',(-1.36411695356838,-2.32604733752032,12.5));
#437554=CARTESIAN_POINT('',(-1.34770274241472,-2.29584528718626,13.8587068136939));
#437555=CARTESIAN_POINT('Ctrl Pts',(-1.33005753786175,-2.33069457618187,
13.8235269408542));
#437556=CARTESIAN_POINT('Ctrl Pts',(-1.32982064044995,-2.3289583650647,
13.8262006681044));
#437557=CARTESIAN_POINT('Ctrl Pts',(-1.32975035485606,-2.327158118424,13.8288634856214));
#437558=CARTESIAN_POINT('Ctrl Pts',(-1.32983483319984,-2.32529995457508,
13.8314912288862));
#437559=CARTESIAN_POINT('Ctrl Pts',(-1.32992192165874,-2.32338437930756,
13.8342001611531));
#437560=CARTESIAN_POINT('Ctrl Pts',(-1.33017308559617,-2.32140510232591,
13.8368750301949));
#437561=CARTESIAN_POINT('Ctrl Pts',(-1.33061688902365,-2.31935101672995,
13.8394886372969));
#437562=CARTESIAN_POINT('Ctrl Pts',(-1.33065116503887,-2.31919237471686,
13.8396904925131));
#437563=CARTESIAN_POINT('Ctrl Pts',(-1.33068661225026,-2.31903328735934,
13.8398919674349));
#437564=CARTESIAN_POINT('Ctrl Pts',(-1.3307232551677,-2.31887375099653,
13.8400930404591));
#437565=CARTESIAN_POINT('Ctrl Pts',(-1.3312941764737,-2.31638806713311,
13.8432258934518));
#437566=CARTESIAN_POINT('Ctrl Pts',(-1.33215135408679,-2.31380581551435,
13.8462331177034));
#437567=CARTESIAN_POINT('Ctrl Pts',(-1.33335838538214,-2.31124160658065,
13.8489036603661));
#437568=CARTESIAN_POINT('Ctrl Pts',(-1.33375334006891,-2.31040256757635,
13.8497774930041));
#437569=CARTESIAN_POINT('Ctrl Pts',(-1.33418578751209,-2.30956570785966,
13.85061494757));
#437570=CARTESIAN_POINT('Ctrl Pts',(-1.3346580433432,-2.30873575114057,
13.8514076489583));
#437571=CARTESIAN_POINT('Ctrl Pts',(-1.33565693253548,-2.30698027298202,
13.8530843267192));
#437572=CARTESIAN_POINT('Ctrl Pts',(-1.33693460598547,-2.30508470640123,
13.8546805203176));
#437573=CARTESIAN_POINT('Ctrl Pts',(-1.33853005156653,-2.30323533184876,
13.8559412814273));
#437574=CARTESIAN_POINT('Ctrl Pts',(-1.33874357392681,-2.30298782555699,
13.8561100121513));
#437575=CARTESIAN_POINT('Ctrl Pts',(-1.33896271112119,-2.30274114608263,
13.8562727473908));
#437576=CARTESIAN_POINT('Ctrl Pts',(-1.3391874814223,-2.30249572994325,
13.8564289040185));
#437577=CARTESIAN_POINT('Ctrl Pts',(-1.34020681217352,-2.30138277055099,
13.8571370725437));
#437578=CARTESIAN_POINT('Ctrl Pts',(-1.34136158981007,-2.30027776785877,
13.8577210840553));
#437579=CARTESIAN_POINT('Ctrl Pts',(-1.34262721810076,-2.29924487767196,
13.8581177131616));
#437580=CARTESIAN_POINT('Ctrl Pts',(-1.34298366258902,-2.29895398024436,
13.8582294175695));
#437581=CARTESIAN_POINT('Ctrl Pts',(-1.34334876244077,-2.2986686896975,
13.8583265086086));
#437582=CARTESIAN_POINT('Ctrl Pts',(-1.34372164622057,-2.29839013992448,
13.8584082369006));
#437583=CARTESIAN_POINT('Ctrl Pts',(-1.3442573802194,-2.29798993859672,
13.8585256585398));
#437584=CARTESIAN_POINT('Ctrl Pts',(-1.3448160357368,-2.29759893516493,
13.8586122832068));
#437585=CARTESIAN_POINT('Ctrl Pts',(-1.34538355333422,-2.29722793373199,
13.8586682984299));
#437586=CARTESIAN_POINT('Ctrl Pts',(-1.34583751115595,-2.29693116936183,
13.8587131050557));
#437587=CARTESIAN_POINT('Ctrl Pts',(-1.34630202496706,-2.29664372906882,
13.8587357943552));
#437588=CARTESIAN_POINT('Ctrl Pts',(-1.34677741645704,-2.29636600935861,
13.8587355499465));
#437589=CARTESIAN_POINT('Ctrl Pts',(-1.34708467331092,-2.29618651248872,
13.8587353919793));
#437590=CARTESIAN_POINT('Ctrl Pts',(-1.34739313200497,-2.29601298390489,
13.8587257282814));
#437591=CARTESIAN_POINT('Ctrl Pts',(-1.34770274241472,-2.29584528718626,
13.8587068136939));
#437592=CARTESIAN_POINT('Ctrl Pts',(-1.34770274241472,-2.29584528718626,
13.8587068136939));
#437593=CARTESIAN_POINT('Ctrl Pts',(-1.34872103417355,-2.29529374182091,
13.8586446046466));
#437594=CARTESIAN_POINT('Ctrl Pts',(-1.34975176954439,-2.29480520254764,
13.858482427929));
#437595=CARTESIAN_POINT('Ctrl Pts',(-1.35079331499402,-2.29437550793324,
13.8582284286032));
#437596=CARTESIAN_POINT('Ctrl Pts',(-1.35186181946785,-2.29393469124296,
13.8579678548414));
#437597=CARTESIAN_POINT('Ctrl Pts',(-1.3529448950698,-2.29355614396119,
13.857615680862));
#437598=CARTESIAN_POINT('Ctrl Pts',(-1.35399664534387,-2.29324564296522,
13.8571944833187));
#437599=CARTESIAN_POINT('Ctrl Pts',(-1.356621395717,-2.29247075597434,13.8561433417727));
#437600=CARTESIAN_POINT('Ctrl Pts',(-1.35917247081262,-2.29207881737704,
13.8546163505475));
#437601=CARTESIAN_POINT('Ctrl Pts',(-1.36149189638798,-2.29193640301783,
13.8528973491086));
#437602=CARTESIAN_POINT('Ctrl Pts',(-1.36191562122068,-2.29191038601552,
13.8525833129073));
#437603=CARTESIAN_POINT('Ctrl Pts',(-1.36233167248507,-2.2918925675005,
13.8522628768812));
#437604=CARTESIAN_POINT('Ctrl Pts',(-1.36273918437797,-2.2918819840077,
13.851937733538));
#437605=CARTESIAN_POINT('Ctrl Pts',(-1.36522780296811,-2.29181735208559,
13.8499521282529));
#437606=CARTESIAN_POINT('Ctrl Pts',(-1.367645384087,-2.29202019498647,13.847639871647));
#437607=CARTESIAN_POINT('Ctrl Pts',(-1.36987158585087,-2.29239979264626,
13.8452109780794));
#437608=CARTESIAN_POINT('Ctrl Pts',(-1.37087320010452,-2.29257058149069,
13.8441181685877));
#437609=CARTESIAN_POINT('Ctrl Pts',(-1.37183643160253,-2.29277652838762,
13.8430021611332));
#437610=CARTESIAN_POINT('Ctrl Pts',(-1.37275277645379,-2.29300715418379,
13.8418824960098));
#437611=CARTESIAN_POINT('Ctrl Pts',(-1.37491216649548,-2.29355062976171,
13.8392439765549));
#437612=CARTESIAN_POINT('Ctrl Pts',(-1.37691533616139,-2.29425346505643,
13.8364981347964));
#437613=CARTESIAN_POINT('Ctrl Pts',(-1.37877891261276,-2.29508522814937,
13.8336931113419));
#437614=CARTESIAN_POINT('Ctrl Pts',(-1.38059391772835,-2.29589531258005,
13.8309611966328));
#437615=CARTESIAN_POINT('Ctrl Pts',(-1.38227810012235,-2.29682901895827,
13.8281701127186));
#437616=CARTESIAN_POINT('Ctrl Pts',(-1.38381884417546,-2.29788583443058,
13.8253580685121));
#437617=CARTESIAN_POINT('Ctrl Pts',(-1.384152879149,-2.29811495316553,13.8247484142933));
#437618=CARTESIAN_POINT('Ctrl Pts',(-1.38448001119162,-2.29834992231107,
13.8241378483365));
#437619=CARTESIAN_POINT('Ctrl Pts',(-1.38479980462761,-2.29859082104314,
13.8235269408515));
#437620=CARTESIAN_POINT('',(-1.34662228908371,-2.29645798405909,12.5969504640361));
#437621=CARTESIAN_POINT('Origin',(-1.36413385963227,-2.32607577812183,12.584524458991));
#437622=CARTESIAN_POINT('Origin',(-1.36413385963227,-2.32607577812183,12.584524458991));
#437623=CARTESIAN_POINT('Ctrl Pts',(-1.33005753786832,-2.33069457618112,
12.5893111709658));
#437624=CARTESIAN_POINT('Ctrl Pts',(-1.32852527273163,-2.31946466976519,
12.5770542771492));
#437625=CARTESIAN_POINT('Ctrl Pts',(-1.3440429755857,-2.31426807732518,
12.5737548217797));
#437626=CARTESIAN_POINT('Ctrl Pts',(-1.3334080874788,-2.35525061264415,
12.5663937883685));
#437627=CARTESIAN_POINT('Ctrl Pts',(-1.33187386772512,-2.344006380923,12.5540940315304));
#437628=CARTESIAN_POINT('Ctrl Pts',(-1.34744067650152,-2.33879673027902,
12.5508374392248));
#437629=CARTESIAN_POINT('Ctrl Pts',(-1.33675525642581,-2.37978187236747,
12.5434499600945));
#437630=CARTESIAN_POINT('Ctrl Pts',(-1.33521604837739,-2.3685010816448,
12.5311293540533));
#437631=CARTESIAN_POINT('Ctrl Pts',(-1.35083388908308,-2.36330158010592,
12.5278936106989));
#437632=CARTESIAN_POINT('Ctrl Pts',(-1.34009930952133,-2.4042902961469,
12.5204817579905));
#437633=CARTESIAN_POINT('Ctrl Pts',(-1.33855248344495,-2.39295367321952,
12.5081597038247));
#437634=CARTESIAN_POINT('Ctrl Pts',(-1.35422294845813,-2.38778447877886,
12.5049254088044));
#437635=CARTESIAN_POINT('Ctrl Pts',(-1.33769508908193,-2.38666986617616,
12.5369868989719));
#437636=CARTESIAN_POINT('Ctrl Pts',(-1.33782102160788,-2.38759281913793,
12.5342545179733));
#437637=CARTESIAN_POINT('Ctrl Pts',(-1.33806480668581,-2.38845677859828,
12.5314872231885));
#437638=CARTESIAN_POINT('Ctrl Pts',(-1.33846651163321,-2.38919789548877,
12.5287124745063));
#437639=CARTESIAN_POINT('Ctrl Pts',(-1.33882878909364,-2.38986627148637,
12.5262100684185));
#437640=CARTESIAN_POINT('Ctrl Pts',(-1.33932000719543,-2.39043359248387,
12.5237004536639));
#437641=CARTESIAN_POINT('Ctrl Pts',(-1.33999871561359,-2.39086620715601,
12.5212220730815));
#437642=CARTESIAN_POINT('Ctrl Pts',(-1.34051832562065,-2.39119741111168,
12.5193246583486));
#437643=CARTESIAN_POINT('Ctrl Pts',(-1.34115437912775,-2.39145308386972,
12.5174178313691));
#437644=CARTESIAN_POINT('Ctrl Pts',(-1.34196022806013,-2.39155193831661,
12.5155812248348));
#437645=CARTESIAN_POINT('Ctrl Pts',(-1.34230352403678,-2.39159405084233,
12.5147988205794));
#437646=CARTESIAN_POINT('Ctrl Pts',(-1.34267794934921,-2.39160802160276,
12.5140295443047));
#437647=CARTESIAN_POINT('Ctrl Pts',(-1.34308860501669,-2.39158945616174,
12.5132817086137));
#437648=CARTESIAN_POINT('Ctrl Pts',(-1.34371007681718,-2.39156135987824,
12.5121499604604));
#437649=CARTESIAN_POINT('Ctrl Pts',(-1.34442762323797,-2.39145099570438,
12.5110494206568));
#437650=CARTESIAN_POINT('Ctrl Pts',(-1.34524772786261,-2.3912216912815,
12.5100666561695));
#437651=CARTESIAN_POINT('Ctrl Pts',(-1.34571863004954,-2.39109002520993,
12.5095023550641));
#437652=CARTESIAN_POINT('Ctrl Pts',(-1.34622861105696,-2.39091699426612,
12.5089719619137));
#437653=CARTESIAN_POINT('Ctrl Pts',(-1.34676605972385,-2.39069979339732,
12.5085043804652));
#437654=CARTESIAN_POINT('Ctrl Pts',(-1.34755254584023,-2.39038194821823,
12.5078201359221));
#437655=CARTESIAN_POINT('Ctrl Pts',(-1.34842021077976,-2.38995917692624,
12.5072563000949));
#437656=CARTESIAN_POINT('Ctrl Pts',(-1.34930653136514,-2.38945252654746,
12.5068768744332));
#437657=CARTESIAN_POINT('Ctrl Pts',(-1.34994562952171,-2.38908719674643,
12.5066032824114));
#437658=CARTESIAN_POINT('Ctrl Pts',(-1.35060568529704,-2.38867188867508,
12.5064197834844));
#437659=CARTESIAN_POINT('Ctrl Pts',(-1.35125121603904,-2.38823198202769,
12.5063282718343));
#437660=CARTESIAN_POINT('Ctrl Pts',(-1.35219349107109,-2.38758985451416,
12.5061946931565));
#437661=CARTESIAN_POINT('Ctrl Pts',(-1.35312555584104,-2.38688246795464,
12.5062515701262));
#437662=CARTESIAN_POINT('Ctrl Pts',(-1.35399891386266,-2.38616604253298,
12.5064436508398));
#437663=CARTESIAN_POINT('',(-1.3440429755857,-2.31426807732518,12.5737548217797));
#437664=CARTESIAN_POINT('Origin',(-1.35185556391636,-2.32772034343821,12.5893111709658));
#437665=CARTESIAN_POINT('Ctrl Pts',(-1.35399891386266,-2.38616604253298,
12.5064436508398));
#437666=CARTESIAN_POINT('Ctrl Pts',(-1.3525256522368,-2.3755232098305,12.5164271754438));
#437667=CARTESIAN_POINT('Ctrl Pts',(-1.35105159964824,-2.36487618696084,
12.5264061185523));
#437668=CARTESIAN_POINT('Ctrl Pts',(-1.34957672917747,-2.35422482622005,
12.536380305637));
#437669=CARTESIAN_POINT('Ctrl Pts',(-1.34773344022497,-2.34091278562278,
12.5488460165097));
#437670=CARTESIAN_POINT('Ctrl Pts',(-1.34588887317763,-2.32759396537209,
12.5613043021964));
#437671=CARTESIAN_POINT('Ctrl Pts',(-1.3440429755857,-2.31426807732518,
12.5737548217797));
#437672=CARTESIAN_POINT('Ctrl Pts',(-1.38479980462761,-2.29859082104314,
12.5893111709658));
#437673=CARTESIAN_POINT('Ctrl Pts',(-1.37574697432478,-2.29177137106034,
12.5770542771492));
#437674=CARTESIAN_POINT('Ctrl Pts',(-1.36363630048295,-2.30277751725016,
12.5737548217797));
#437675=CARTESIAN_POINT('Ctrl Pts',(-1.37635359269243,-2.29222833352163,
12.5928319619712));
#437676=CARTESIAN_POINT('Ctrl Pts',(-1.3683094033576,-2.29024731501676,
12.5821634970842));
#437677=CARTESIAN_POINT('Ctrl Pts',(-1.36056522911279,-2.30045227790575,
12.5773203894503));
#437678=CARTESIAN_POINT('Ctrl Pts',(-1.35998988496106,-2.28864878485988,
12.5969440695591));
#437679=CARTESIAN_POINT('Ctrl Pts',(-1.35651320182277,-2.29066651053694,
12.5878292599214));
#437680=CARTESIAN_POINT('Ctrl Pts',(-1.35473243254761,-2.29917845243625,
12.5813877129824));
#437681=CARTESIAN_POINT('Ctrl Pts',(-1.33356952551014,-2.30408056544493,
12.596957478804));
#437682=CARTESIAN_POINT('Ctrl Pts',(-1.33702055526328,-2.30207782063047,
12.5878468778671));
#437683=CARTESIAN_POINT('Ctrl Pts',(-1.34527922820436,-2.30470685147657,
12.5814011370086));
#437684=CARTESIAN_POINT('Ctrl Pts',(-1.32862587206039,-2.32020195799361,
12.5928371701607));
#437685=CARTESIAN_POINT('Ctrl Pts',(-1.33082819508306,-2.31222167986515,
12.5821692192951));
#437686=CARTESIAN_POINT('Ctrl Pts',(-1.34351091151346,-2.31044052127765,
12.5773318885715));
#437687=CARTESIAN_POINT('Ctrl Pts',(-1.33005753786826,-2.33069457618113,
12.5893111709658));
#437688=CARTESIAN_POINT('Ctrl Pts',(-1.32852527273157,-2.31946466976519,
12.5770542771492));
#437689=CARTESIAN_POINT('Ctrl Pts',(-1.34404297558565,-2.31426807732519,
12.5737548217797));
#437690=CARTESIAN_POINT('',(-1.36363630048295,-2.30277751725016,12.5737548217797));
#437691=CARTESIAN_POINT('Origin',(-1.3715627799497,-2.31616299158853,12.5893111709658));
#437692=CARTESIAN_POINT('Ctrl Pts',(-1.34404297558565,-2.31426807732519,
12.5737548217797));
#437693=CARTESIAN_POINT('Ctrl Pts',(-1.34387517769676,-2.31328006745706,
12.5746934679442));
#437694=CARTESIAN_POINT('Ctrl Pts',(-1.34387009640631,-2.31215609698649,
12.5756680099006));
#437695=CARTESIAN_POINT('Ctrl Pts',(-1.3440249798495,-2.31102405688693,
12.5765688348656));
#437696=CARTESIAN_POINT('Ctrl Pts',(-1.34406598352647,-2.31072436180267,
12.5768073183026));
#437697=CARTESIAN_POINT('Ctrl Pts',(-1.34411794307724,-2.31042412933394,
12.5770407398754));
#437698=CARTESIAN_POINT('Ctrl Pts',(-1.34418025012305,-2.31012565157104,
12.5772674179684));
#437699=CARTESIAN_POINT('Ctrl Pts',(-1.3444359413905,-2.30890077954389,
12.5781976435658));
#437700=CARTESIAN_POINT('Ctrl Pts',(-1.34489145521362,-2.30763819305588,
12.5790594849312));
#437701=CARTESIAN_POINT('Ctrl Pts',(-1.3455614579905,-2.30643953171811,
12.5797571720116));
#437702=CARTESIAN_POINT('Ctrl Pts',(-1.34599798889079,-2.30565856075654,
12.580211740231));
#437703=CARTESIAN_POINT('Ctrl Pts',(-1.3465617949788,-2.30487839431568,
12.5806009430798));
#437704=CARTESIAN_POINT('Ctrl Pts',(-1.34722754623479,-2.30416432994221,
12.5808812374708));
#437705=CARTESIAN_POINT('Ctrl Pts',(-1.34779964742438,-2.30355071175701,
12.5811221033394));
#437706=CARTESIAN_POINT('Ctrl Pts',(-1.34845882604483,-2.30297342214248,
12.581287365893));
#437707=CARTESIAN_POINT('Ctrl Pts',(-1.34917337033051,-2.30247131682757,
12.581359338449));
#437708=CARTESIAN_POINT('Ctrl Pts',(-1.34927267723144,-2.30240153455688,
12.5813693411482));
#437709=CARTESIAN_POINT('Ctrl Pts',(-1.34937303740507,-2.30233314682621,
12.5813775999465));
#437710=CARTESIAN_POINT('Ctrl Pts',(-1.34947435024895,-2.3022661985824,
12.5813841266931));
#437711=CARTESIAN_POINT('Ctrl Pts',(-1.34964623974214,-2.30215261278955,
12.5813952001081));
#437712=CARTESIAN_POINT('Ctrl Pts',(-1.34982235842937,-2.30204291783015,
12.5814007534795));
#437713=CARTESIAN_POINT('Ctrl Pts',(-1.35000273386689,-2.3019373288753,
12.5814005856065));
#437714=CARTESIAN_POINT('Ctrl Pts',(-1.35082842209762,-2.30145398392258,
12.5813998171494));
#437715=CARTESIAN_POINT('Ctrl Pts',(-1.35168608920437,-2.30108978241973,
12.58127954464));
#437716=CARTESIAN_POINT('Ctrl Pts',(-1.35255930057023,-2.30081955655557,
12.5810700125799));
#437717=CARTESIAN_POINT('Ctrl Pts',(-1.35361404047712,-2.30049315447935,
12.5808169217085));
#437718=CARTESIAN_POINT('Ctrl Pts',(-1.35469650230511,-2.30031982026343,
12.5804173076348));
#437719=CARTESIAN_POINT('Ctrl Pts',(-1.35570770323402,-2.30028902985874,
12.5799304713245));
#437720=CARTESIAN_POINT('Ctrl Pts',(-1.35696089974608,-2.30025087084736,
12.5793271277669));
#437721=CARTESIAN_POINT('Ctrl Pts',(-1.35818140455784,-2.30039709264079,
12.5785808224116));
#437722=CARTESIAN_POINT('Ctrl Pts',(-1.35932154388287,-2.30069004004651,
12.5777485681082));
#437723=CARTESIAN_POINT('Ctrl Pts',(-1.36102047638875,-2.30112656377583,
12.576508418016));
#437724=CARTESIAN_POINT('Ctrl Pts',(-1.3625283680815,-2.30187854925022,
12.5750928681475));
#437725=CARTESIAN_POINT('Ctrl Pts',(-1.36363630048295,-2.30277751725016,
12.5737548217797));
#437726=CARTESIAN_POINT('Ctrl Pts',(-1.36363630048295,-2.30277751725016,
12.5737548217797));
#437727=CARTESIAN_POINT('Ctrl Pts',(-1.37574697432478,-2.29177137106034,
12.5770542771492));
#437728=CARTESIAN_POINT('Ctrl Pts',(-1.38479980462761,-2.29859082104314,
12.5893111709658));
#437729=CARTESIAN_POINT('Ctrl Pts',(-1.38338191825478,-2.31771490433691,
12.5508408821982));
#437730=CARTESIAN_POINT('Ctrl Pts',(-1.39552795292374,-2.30667227935687,
12.55409748406));
#437731=CARTESIAN_POINT('Ctrl Pts',(-1.40459233231949,-2.31350042921128,
12.5663972313419));
#437732=CARTESIAN_POINT('Ctrl Pts',(-1.40310895865535,-2.33263675880696,
12.52790050457));
#437733=CARTESIAN_POINT('Ctrl Pts',(-1.41527104624047,-2.3215446488673,
12.5311362602938));
#437734=CARTESIAN_POINT('Ctrl Pts',(-1.42436489260328,-2.32839499603476,
12.5434568539655));
#437735=CARTESIAN_POINT('Ctrl Pts',(-1.42281887373945,-2.3475442767001,
12.5049357605811));
#437736=CARTESIAN_POINT('Ctrl Pts',(-1.4349802036219,-2.3363914546142,12.5081700652078));
#437737=CARTESIAN_POINT('Ctrl Pts',(-1.44411904933042,-2.34327569955473,
12.5204921097672));
#437738=CARTESIAN_POINT('Ctrl Pts',(-1.42152464441194,-2.34656538937372,
12.5064436508395));
#437739=CARTESIAN_POINT('Ctrl Pts',(-1.42266057272229,-2.34611983952878,
12.5062361689309));
#437740=CARTESIAN_POINT('Ctrl Pts',(-1.42382284597399,-2.3456080656443,
12.5061871075061));
#437741=CARTESIAN_POINT('Ctrl Pts',(-1.42491822969963,-2.34505025641642,
12.5063648335164));
#437742=CARTESIAN_POINT('Ctrl Pts',(-1.42541582055389,-2.34479686505801,
12.5064455676329));
#437743=CARTESIAN_POINT('Ctrl Pts',(-1.42590644889045,-2.34453024353031,
12.506574497099));
#437744=CARTESIAN_POINT('Ctrl Pts',(-1.4263685762309,-2.34426090035578,
12.5067492519495));
#437745=CARTESIAN_POINT('Ctrl Pts',(-1.42729723905996,-2.34371964479143,
12.5071004286051));
#437746=CARTESIAN_POINT('Ctrl Pts',(-1.42814454450776,-2.3431468002662,
12.5076537929612));
#437747=CARTESIAN_POINT('Ctrl Pts',(-1.42885219540251,-2.3425931974687,
12.5083435010503));
#437748=CARTESIAN_POINT('Ctrl Pts',(-1.42889674625536,-2.34255834486418,
12.5083869222963));
#437749=CARTESIAN_POINT('Ctrl Pts',(-1.42894074109824,-2.3425235553225,
12.5084308732336));
#437750=CARTESIAN_POINT('Ctrl Pts',(-1.42898416475707,-2.34248883607826,
12.5084753333615));
#437751=CARTESIAN_POINT('Ctrl Pts',(-1.42933247981433,-2.34221034191469,
12.508831962269));
#437752=CARTESIAN_POINT('Ctrl Pts',(-1.42965192099085,-2.34193172451815,
12.509227847131));
#437753=CARTESIAN_POINT('Ctrl Pts',(-1.42993483013762,-2.3416633788136,
12.5096423454524));
#437754=CARTESIAN_POINT('Ctrl Pts',(-1.43082134219323,-2.34082250214037,
12.5109411997424));
#437755=CARTESIAN_POINT('Ctrl Pts',(-1.43141031956876,-2.34003778069885,
12.5124831113042));
#437756=CARTESIAN_POINT('Ctrl Pts',(-1.43179389723121,-2.33933082479333,
12.5140723025008));
#437757=CARTESIAN_POINT('Ctrl Pts',(-1.4318298388783,-2.33926458225068,
12.5142212114565));
#437758=CARTESIAN_POINT('Ctrl Pts',(-1.43186400649979,-2.33919901867689,
12.5143705582413));
#437759=CARTESIAN_POINT('Ctrl Pts',(-1.4318964928642,-2.33913415121086,
12.5145201959299));
#437760=CARTESIAN_POINT('Ctrl Pts',(-1.43231382858219,-2.33830083203218,
12.5164425148273));
#437761=CARTESIAN_POINT('Ctrl Pts',(-1.4324776035179,-2.3375586490697,12.5184635205941));
#437762=CARTESIAN_POINT('Ctrl Pts',(-1.43247354656481,-2.33687952145141,
12.5205025929157));
#437763=CARTESIAN_POINT('Ctrl Pts',(-1.43247119337121,-2.3364856005147,
12.5216853356836));
#437764=CARTESIAN_POINT('Ctrl Pts',(-1.43241286161085,-2.33611360298746,
12.5228750347131));
#437765=CARTESIAN_POINT('Ctrl Pts',(-1.43231679608618,-2.33576377551066,
12.5240609649613));
#437766=CARTESIAN_POINT('Ctrl Pts',(-1.43208100840961,-2.33490514273647,
12.5269717671326));
#437767=CARTESIAN_POINT('Ctrl Pts',(-1.4316012403085,-2.33415865659639,
12.5299036066169));
#437768=CARTESIAN_POINT('Ctrl Pts',(-1.43095697607925,-2.33348979507929,
12.5328133004019));
#437769=CARTESIAN_POINT('Ctrl Pts',(-1.43064769173483,-2.33316870260444,
12.5342101228451));
#437770=CARTESIAN_POINT('Ctrl Pts',(-1.43030050673073,-2.33286626338807,
12.5356023438238));
#437771=CARTESIAN_POINT('Ctrl Pts',(-1.42992349334847,-2.33258226106549,
12.5369868989719));
#437772=CARTESIAN_POINT('Origin',(-11.6129774570238,-9.99679300240355,-1.23967694121652));
#437773=CARTESIAN_POINT('Ctrl Pts',(-1.33768939948239,-2.38662846099065,
12.5369868989719));
#437774=CARTESIAN_POINT('Ctrl Pts',(-1.33979197726431,-2.40182262007747,
12.5369868989719));
#437775=CARTESIAN_POINT('Ctrl Pts',(-1.32626212111486,-2.40904939641688,
12.5369868989719));
#437776=CARTESIAN_POINT('Ctrl Pts',(-1.33840008741708,-2.39176469007801,
12.5218025310015));
#437777=CARTESIAN_POINT('Ctrl Pts',(-1.33666961631256,-2.40345491391935,
12.5216901060417));
#437778=CARTESIAN_POINT('Ctrl Pts',(-1.3263033723702,-2.40902738135429,
12.5161920673678));
#437779=CARTESIAN_POINT('Ctrl Pts',(-1.34373196522167,-2.39457665563101,
12.5042015548895));
#437780=CARTESIAN_POINT('Ctrl Pts',(-1.3416241136767,-2.40065401582123,
12.4980677368515));
#437781=CARTESIAN_POINT('Ctrl Pts',(-1.33568837083694,-2.4039642630422,
12.4907278922777));
#437782=CARTESIAN_POINT('Ctrl Pts',(-1.35398904294486,-2.38614864689313,
12.506463626192));
#437783=CARTESIAN_POINT('Ctrl Pts',(-1.35721801325199,-2.39183909407168,
12.4999376786891));
#437784=CARTESIAN_POINT('Ctrl Pts',(-1.35717857607461,-2.3917695935333,
12.4906970594712));
#437785=CARTESIAN_POINT('Origin',(-1.31589706303389,-2.38964409891908,12.5369868989719));
#437786=CARTESIAN_POINT('Origin',(-1.31589706303389,-2.38964409891908,14.));
#437787=CARTESIAN_POINT('Origin',(-1.31589706303389,-2.38964409891908,13.7435492065112));
#437788=CARTESIAN_POINT('Ctrl Pts',(-1.33434768436319,-2.36213707932785,
13.793642941384));
#437789=CARTESIAN_POINT('Ctrl Pts',(-1.33583639488598,-2.37284641917609,
13.8071662555867));
#437790=CARTESIAN_POINT('Ctrl Pts',(-1.31949668560198,-2.37764571955728,
13.8103758687955));
#437791=CARTESIAN_POINT('Ctrl Pts',(-1.33659473667552,-2.37860560874395,
13.7804579775006));
#437792=CARTESIAN_POINT('Ctrl Pts',(-1.33842162668272,-2.39182136239747,
13.7901904343352));
#437793=CARTESIAN_POINT('Ctrl Pts',(-1.32422170283523,-2.39864910630666,
13.7927914348262));
#437794=CARTESIAN_POINT('Ctrl Pts',(-1.3379176609002,-2.38830125179683,
13.7597120340895));
#437795=CARTESIAN_POINT('Ctrl Pts',(-1.34002621070749,-2.40359638526088,
13.7635825532444));
#437796=CARTESIAN_POINT('Ctrl Pts',(-1.32698310096964,-2.41104038986257,
13.7651073818884));
#437797=CARTESIAN_POINT('Ctrl Pts',(-1.33765860204468,-2.3864026228822,
13.7381884353898));
#437798=CARTESIAN_POINT('Ctrl Pts',(-1.33971868772639,-2.40133962250093,
13.7368803041982));
#437799=CARTESIAN_POINT('Ctrl Pts',(-1.32644185476272,-2.40861391583939,
13.7363986145813));
#437800=CARTESIAN_POINT('Origin',(-1.31309492773408,-2.36910736775679,13.7902182540695));
#437801=CARTESIAN_POINT('Ctrl Pts',(-1.33005700497226,-2.33069067622211,
13.8235227101244));
#437802=CARTESIAN_POINT('Ctrl Pts',(-1.33161571444549,-2.342081598621,13.8358800583119));
#437803=CARTESIAN_POINT('Ctrl Pts',(-1.31586661480734,-2.34723833301828,
13.8390832900376));
#437804=CARTESIAN_POINT('Ctrl Pts',(-1.33166952301955,-2.34250875283556,
13.8124254819052));
#437805=CARTESIAN_POINT('Ctrl Pts',(-1.33323125920889,-2.353921796282,13.8247886449158));
#437806=CARTESIAN_POINT('Ctrl Pts',(-1.31745695617586,-2.35906884834355,
13.8279860620657));
#437807=CARTESIAN_POINT('Ctrl Pts',(-1.33328131838873,-2.35432153297157,
13.8013225099955));
#437808=CARTESIAN_POINT('Ctrl Pts',(-1.33484534639161,-2.36575131207001,
13.8136962257787));
#437809=CARTESIAN_POINT('Ctrl Pts',(-1.31904682993433,-2.3708938506096,
13.8168830918626));
#437810=CARTESIAN_POINT('Ctrl Pts',(-1.33489241919809,-2.36612922270791,
13.7902140179785));
#437811=CARTESIAN_POINT('Ctrl Pts',(-1.3364580521403,-2.37757070403835,
13.802602731458));
#437812=CARTESIAN_POINT('Ctrl Pts',(-1.32063625628017,-2.38271355619271,
13.8057746032558));
#437813=CARTESIAN_POINT('Origin',(-1.30825951182028,-2.33366880892404,13.8235269408515));
#437814=CARTESIAN_POINT('Ctrl Pts',(-1.38479980462761,-2.29859082104314,
13.8235269408515));
#437815=CARTESIAN_POINT('Ctrl Pts',(-1.39423085363655,-2.30569518121011,
13.8362179249168));
#437816=CARTESIAN_POINT('Ctrl Pts',(-1.40657750063972,-2.29389588835687,
13.8391868794938));
#437817=CARTESIAN_POINT('Ctrl Pts',(-1.37617080529356,-2.29209064072475,
13.8400110824519));
#437818=CARTESIAN_POINT('Ctrl Pts',(-1.38579055609397,-2.29505412809609,
13.8494522556837));
#437819=CARTESIAN_POINT('Ctrl Pts',(-1.39230900053449,-2.2832881700173,
13.85569149686));
#437820=CARTESIAN_POINT('Ctrl Pts',(-1.36028623044585,-2.28847428787239,
13.8586819406588));
#437821=CARTESIAN_POINT('Ctrl Pts',(-1.36404890504555,-2.28628378028469,
13.868010383617));
#437822=CARTESIAN_POINT('Ctrl Pts',(-1.36590788102171,-2.27742730948009,
13.8744918421245));
#437823=CARTESIAN_POINT('Ctrl Pts',(-1.33326857445539,-2.30425775272418,
13.8587686893867));
#437824=CARTESIAN_POINT('Ctrl Pts',(-1.32953935929475,-2.30642871615213,
13.8680909899357));
#437825=CARTESIAN_POINT('Ctrl Pts',(-1.32093271578979,-2.30370436502123,
13.8745789365163));
#437826=CARTESIAN_POINT('Ctrl Pts',(-1.32859463293563,-2.31997300781692,
13.8400379222776));
#437827=CARTESIAN_POINT('Ctrl Pts',(-1.32647840745911,-2.3298112913888,
13.8494748685453));
#437828=CARTESIAN_POINT('Ctrl Pts',(-1.31303377231583,-2.32975752216985,
13.8557104837033));
#437829=CARTESIAN_POINT('Ctrl Pts',(-1.33005753786175,-2.33069457618187,
13.8235269408542));
#437830=CARTESIAN_POINT('Ctrl Pts',(-1.33165381958967,-2.34239365748921,
13.8362179249195));
#437831=CARTESIAN_POINT('Ctrl Pts',(-1.31532870539695,-2.34740899901807,
13.8391868794965));
#437832=CARTESIAN_POINT('Origin',(-1.39803682930552,-2.28101865049774,13.8235269408515));
#437833=CARTESIAN_POINT('Ctrl Pts',(-1.41336494897749,-2.32010879476138,
13.7902140241683));
#437834=CARTESIAN_POINT('Ctrl Pts',(-1.42258614113104,-2.32706064420306,
13.8026027327198));
#437835=CARTESIAN_POINT('Ctrl Pts',(-1.43479835951345,-2.31576287210172,
13.8057746032556));
#437836=CARTESIAN_POINT('Ctrl Pts',(-1.4038463468152,-2.3129384812607,13.8013225161808));
#437837=CARTESIAN_POINT('Ctrl Pts',(-1.41305810939257,-2.31988321726021,
13.8136962270464));
#437838=CARTESIAN_POINT('Ctrl Pts',(-1.42525868962529,-2.30860560903426,
13.8168830918628));
#437839=CARTESIAN_POINT('Ctrl Pts',(-1.39432364109784,-2.30576507657335,
13.8124254880875));
#437840=CARTESIAN_POINT('Ctrl Pts',(-1.40352191652556,-2.31269964247155,
13.8247886461867));
#437841=CARTESIAN_POINT('Ctrl Pts',(-1.41571461550004,-2.30144536977557,
13.8279860620656));
#437842=CARTESIAN_POINT('Ctrl Pts',(-1.3847966656975,-2.29858845555602,
13.8235227163066));
#437843=CARTESIAN_POINT('Ctrl Pts',(-1.39397711266371,-2.30550958095132,
13.8358800595847));
#437844=CARTESIAN_POINT('Ctrl Pts',(-1.40616595815507,-2.29428203106785,
13.8390832900376));
#437845=CARTESIAN_POINT('Origin',(-1.42660512252251,-2.30253899719266,13.7902182540695));
#437846=CARTESIAN_POINT('Ctrl Pts',(-1.42970796339007,-2.33241986893362,
13.7382347919292));
#437847=CARTESIAN_POINT('Ctrl Pts',(-1.44174667761807,-2.34151861766462,
13.7369371795942));
#437848=CARTESIAN_POINT('Ctrl Pts',(-1.45458222311529,-2.33346923577475,
13.7364597369711));
#437849=CARTESIAN_POINT('Ctrl Pts',(-1.43121881726327,-2.33355798780178,
13.7595490285574));
#437850=CARTESIAN_POINT('Ctrl Pts',(-1.44354537111657,-2.34287302277328,
13.7633824266926));
#437851=CARTESIAN_POINT('Ctrl Pts',(-1.45641273663841,-2.33510613376707,
13.7648920890506));
#437852=CARTESIAN_POINT('Ctrl Pts',(-1.42351354527644,-2.32775364393176,
13.780380659011));
#437853=CARTESIAN_POINT('Ctrl Pts',(-1.43417231843284,-2.3358151227542,
13.7901039518744));
#437854=CARTESIAN_POINT('Ctrl Pts',(-1.4470781039309,-2.32676381665488,
13.7926933640892));
#437855=CARTESIAN_POINT('Ctrl Pts',(-1.41012006257667,-2.31766439853161,
13.7936647693663));
#437856=CARTESIAN_POINT('Ctrl Pts',(-1.41874065032452,-2.3241957688952,
13.8072068914933));
#437857=CARTESIAN_POINT('Ctrl Pts',(-1.43091158297241,-2.31225790190283,
13.8104111085397));
#437858=CARTESIAN_POINT('Origin',(-1.44316051802638,-2.31501009052009,13.7435492065112));
#437859=CARTESIAN_POINT('Origin',(-1.44316051802638,-2.31501009052009,14.));
#437860=CARTESIAN_POINT('Origin',(-1.44316051802638,-2.31501009052009,12.5369868989719));
#437861=CARTESIAN_POINT('Ctrl Pts',(-1.42151511945786,-2.34654966618566,
12.506462012331));
#437862=CARTESIAN_POINT('Ctrl Pts',(-1.42490298989075,-2.3521421541758,
12.4999388158272));
#437863=CARTESIAN_POINT('Ctrl Pts',(-1.42486290694061,-2.35207598770878,
12.4907030323752));
#437864=CARTESIAN_POINT('Ctrl Pts',(-1.43387678705323,-2.34171047643781,
12.5042014951932));
#437865=CARTESIAN_POINT('Ctrl Pts',(-1.44020683426554,-2.3428381286032,
12.4980716682127));
#437866=CARTESIAN_POINT('Ctrl Pts',(-1.44599026110078,-2.33927757537827,
12.4907355092744));
#437867=CARTESIAN_POINT('Ctrl Pts',(-1.4340278803235,-2.33568528996193,
12.5218047446509));
#437868=CARTESIAN_POINT('Ctrl Pts',(-1.44507022020915,-2.3398788088645,
12.5216906929434));
#437869=CARTESIAN_POINT('Ctrl Pts',(-1.4549910807195,-2.33355842271618,
12.5161988840775));
#437870=CARTESIAN_POINT('Ctrl Pts',(-1.42989282923491,-2.33255911995573,
12.5369868989719));
#437871=CARTESIAN_POINT('Ctrl Pts',(-1.44212122438067,-2.3418042204787,
12.5369868989719));
#437872=CARTESIAN_POINT('Ctrl Pts',(-1.45502900165886,-2.3335341045631,
12.5369868989719));
#437873=CARTESIAN_POINT('Origin',(-2.60621061928491E-31,-9.59588718149408E-31,
12.5));
#437874=CARTESIAN_POINT('Origin',(-1.19283550652458,-2.40381648963782,12.5));
#437875=CARTESIAN_POINT('',(-1.19283550652458,-2.40381648963782,12.5893111709658));
#437876=CARTESIAN_POINT('',(-1.19283550652458,-2.40381648963782,13.8235269408515));
#437877=CARTESIAN_POINT('',(-1.19283550652458,-2.40381648963782,12.5));
#437878=CARTESIAN_POINT('',(-1.21955463306182,-2.42759381026669,13.7902182540695));
#437879=CARTESIAN_POINT('',(-1.19283550652458,-2.40381648963782,13.8235269408515));
#437880=CARTESIAN_POINT('',(-1.2350384319707,-2.44137282548623,13.7435492065112));
#437881=CARTESIAN_POINT('Origin',(-1.18409672167107,-2.39604029089782,13.7445212918711));
#437882=CARTESIAN_POINT('',(-1.2350384319707,-2.44137282548623,12.5369868989719));
#437883=CARTESIAN_POINT('',(-1.2350384319707,-2.44137282548623,12.5));
#437884=CARTESIAN_POINT('Ctrl Pts',(-1.2350384319707,-2.44137282548623,
12.5369868989719));
#437885=CARTESIAN_POINT('Ctrl Pts',(-1.22098105023765,-2.42886317730581,
12.5544431401645));
#437886=CARTESIAN_POINT('Ctrl Pts',(-1.20691361429157,-2.41634458189252,
12.5718848856037));
#437887=CARTESIAN_POINT('Ctrl Pts',(-1.19283550652458,-2.40381648963782,
12.5893111709658));
#437888=CARTESIAN_POINT('Origin',(-1.15050357034785,-2.70595045041756,12.5));
#437889=CARTESIAN_POINT('',(-1.1387082681697,-2.48776298739836,13.7435492065112));
#437890=CARTESIAN_POINT('',(-1.13758939098738,-2.46706619047416,13.7902182540695));
#437891=CARTESIAN_POINT('Origin',(-1.13464917513303,-2.41267858528178,13.7418732680441));
#437892=CARTESIAN_POINT('',(-1.13565863606154,-2.43135141923567,13.8235269408515));
#437893=CARTESIAN_POINT('',(-1.13758939098738,-2.46706619047416,13.7902182540695));
#437894=CARTESIAN_POINT('',(-1.13565863606154,-2.43135141923567,12.5893111709658));
#437895=CARTESIAN_POINT('',(-1.13565863606154,-2.43135141923567,12.5));
#437896=CARTESIAN_POINT('',(-1.1387082681697,-2.48776298739836,12.5369868989719));
#437897=CARTESIAN_POINT('Ctrl Pts',(-1.13565863606154,-2.43135141923567,
12.5893111709658));
#437898=CARTESIAN_POINT('Ctrl Pts',(-1.13667593637934,-2.45016926485903,
12.5718848856037));
#437899=CARTESIAN_POINT('Ctrl Pts',(-1.13769246553904,-2.46897284573306,
12.5544431401645));
#437900=CARTESIAN_POINT('Ctrl Pts',(-1.1387082681697,-2.48776298739836,
12.5369868989719));
#437901=CARTESIAN_POINT('',(-1.1387082681697,-2.48776298739836,12.5));
#437902=CARTESIAN_POINT('Origin',(-1.16998351495927,-2.42949580244988,12.5));
#437903=CARTESIAN_POINT('',(-1.15608566822344,-2.39805633635573,13.8587068136939));
#437904=CARTESIAN_POINT('Ctrl Pts',(-1.13565863605493,-2.43135141923588,
13.8235269408542));
#437905=CARTESIAN_POINT('Ctrl Pts',(-1.13556404422397,-2.42960167587965,
13.8262006681044));
#437906=CARTESIAN_POINT('Ctrl Pts',(-1.13564072931349,-2.42780169048275,
13.8288634856214));
#437907=CARTESIAN_POINT('Ctrl Pts',(-1.13587638416659,-2.42595659529002,
13.8314912288862));
#437908=CARTESIAN_POINT('Ctrl Pts',(-1.13611932001346,-2.42405449245906,
13.8342001611531));
#437909=CARTESIAN_POINT('Ctrl Pts',(-1.13653097767233,-2.42210227355088,
13.8368750301949));
#437910=CARTESIAN_POINT('Ctrl Pts',(-1.13714073142578,-2.4200911968547,
13.8394886372969));
#437911=CARTESIAN_POINT('Ctrl Pts',(-1.13718782418721,-2.41993587652327,
13.8396904925131));
#437912=CARTESIAN_POINT('Ctrl Pts',(-1.13723612054746,-2.41978020779261,
13.8398919674349));
#437913=CARTESIAN_POINT('Ctrl Pts',(-1.13728564523326,-2.41962418901184,
13.8400930404591));
#437914=CARTESIAN_POINT('Ctrl Pts',(-1.13805727315653,-2.41719331144304,
13.8432258934518));
#437915=CARTESIAN_POINT('Ctrl Pts',(-1.13912207606121,-2.41468951998664,
13.8462331177034));
#437916=CARTESIAN_POINT('Ctrl Pts',(-1.14053409789255,-2.41223222750274,
13.8489036603661));
#437917=CARTESIAN_POINT('Ctrl Pts',(-1.14099612786829,-2.41142817280506,
13.849777493004));
#437918=CARTESIAN_POINT('Ctrl Pts',(-1.14149534821422,-2.41062934615131,
13.85061494757));
#437919=CARTESIAN_POINT('Ctrl Pts',(-1.14203368183056,-2.40984064427917,
13.8514076489583));
#437920=CARTESIAN_POINT('Ctrl Pts',(-1.14317233506844,-2.40817242607178,
13.8530843267192));
#437921=CARTESIAN_POINT('Ctrl Pts',(-1.14460026343935,-2.40638730907992,
13.8546805203176));
#437922=CARTESIAN_POINT('Ctrl Pts',(-1.14634114150165,-2.40467413179495,
13.8559412814273));
#437923=CARTESIAN_POINT('Ctrl Pts',(-1.1465741274444,-2.40444485311456,
13.8561100121513));
#437924=CARTESIAN_POINT('Ctrl Pts',(-1.14681264214506,-2.40421685616153,
13.8562727473908));
#437925=CARTESIAN_POINT('Ctrl Pts',(-1.14705666823522,-2.40399057749032,
13.8564289040185));
#437926=CARTESIAN_POINT('Ctrl Pts',(-1.14816332377013,-2.40296440629786,
13.8571370725437));
#437927=CARTESIAN_POINT('Ctrl Pts',(-1.14940432695712,-2.40195720550874,
13.8577210840553));
#437928=CARTESIAN_POINT('Ctrl Pts',(-1.15074993411319,-2.40103091263404,
13.8581177131616));
#437929=CARTESIAN_POINT('Ctrl Pts',(-1.15112890340273,-2.40077003667849,
13.8582294175695));
#437930=CARTESIAN_POINT('Ctrl Pts',(-1.15151604224291,-2.40051545443973,
13.8583265086086));
#437931=CARTESIAN_POINT('Ctrl Pts',(-1.15191038967512,-2.40026822500784,
13.8584082369006));
#437932=CARTESIAN_POINT('Ctrl Pts',(-1.15247696118677,-2.3999130226114,
13.8585256585398));
#437933=CARTESIAN_POINT('Ctrl Pts',(-1.15306562823362,-2.39956885582225,
13.8586122832068));
#437934=CARTESIAN_POINT('Ctrl Pts',(-1.15366149752404,-2.39924534681874,
13.8586682984299));
#437935=CARTESIAN_POINT('Ctrl Pts',(-1.15413813388975,-2.39898657168434,
13.8587131050557));
#437936=CARTESIAN_POINT('Ctrl Pts',(-1.15462453112183,-2.39873795001314,
13.8587357943552));
#437937=CARTESIAN_POINT('Ctrl Pts',(-1.15512097752044,-2.39849990321211,
13.8587355499465));
#437938=CARTESIAN_POINT('Ctrl Pts',(-1.15544184266373,-2.39834604788929,
13.8587353919793));
#437939=CARTESIAN_POINT('Ctrl Pts',(-1.15576341917743,-2.39819823895467,
13.8587257282814));
#437940=CARTESIAN_POINT('Ctrl Pts',(-1.15608566822344,-2.39805633635573,
13.8587068136939));
#437941=CARTESIAN_POINT('Ctrl Pts',(-1.15608566822344,-2.39805633635573,
13.8587068136939));
#437942=CARTESIAN_POINT('Ctrl Pts',(-1.15714552776804,-2.39758962644377,
13.8586446046466));
#437943=CARTESIAN_POINT('Ctrl Pts',(-1.15821265393815,-2.39718672724622,
13.858482427929));
#437944=CARTESIAN_POINT('Ctrl Pts',(-1.15928575783141,-2.39684335802857,
13.8582284286032));
#437945=CARTESIAN_POINT('Ctrl Pts',(-1.16038663759735,-2.3964911011536,
13.8579678548414));
#437946=CARTESIAN_POINT('Ctrl Pts',(-1.16149696447231,-2.39620209417302,
13.857615680862));
#437947=CARTESIAN_POINT('Ctrl Pts',(-1.16257052384783,-2.39597835375481,
13.8571944833187));
#437948=CARTESIAN_POINT('Ctrl Pts',(-1.16524970106408,-2.39541998665887,
13.8561433417727));
#437949=CARTESIAN_POINT('Ctrl Pts',(-1.16782423430203,-2.39523728850824,
13.8546163505475));
#437950=CARTESIAN_POINT('Ctrl Pts',(-1.17014755027251,-2.39528440273794,
13.8528973491086));
#437951=CARTESIAN_POINT('Ctrl Pts',(-1.170571985823,-2.3952930098126,13.8525833129073));
#437952=CARTESIAN_POINT('Ctrl Pts',(-1.17098810508553,-2.3953091626277,
13.8522628768812));
#437953=CARTESIAN_POINT('Ctrl Pts',(-1.17139512366914,-2.39533183035303,
13.851937733538));
#437954=CARTESIAN_POINT('Ctrl Pts',(-1.17388072968787,-2.3954702590066,
13.8499521282529));
#437955=CARTESIAN_POINT('Ctrl Pts',(-1.1762737329255,-2.39586948226938,
13.847639871647));
#437956=CARTESIAN_POINT('Ctrl Pts',(-1.17846158645337,-2.39642927296008,
13.8452109780794));
#437957=CARTESIAN_POINT('Ctrl Pts',(-1.17944594704187,-2.39668113437892,
13.8441181685877));
#437958=CARTESIAN_POINT('Ctrl Pts',(-1.18038918688252,-2.39696490831384,
13.8430021611332));
#437959=CARTESIAN_POINT('Ctrl Pts',(-1.18128368452846,-2.39726945733401,
13.8418824960098));
#437960=CARTESIAN_POINT('Ctrl Pts',(-1.18339159107294,-2.39798713487697,
13.8392439765549));
#437961=CARTESIAN_POINT('Ctrl Pts',(-1.18533080775571,-2.39885090846952,
13.8364981347964));
#437962=CARTESIAN_POINT('Ctrl Pts',(-1.18712038689639,-2.39983180272077,
13.8336931113419));
#437963=CARTESIAN_POINT('Ctrl Pts',(-1.18886332333062,-2.40078713142894,
13.8309611966328));
#437964=CARTESIAN_POINT('Ctrl Pts',(-1.19046579600871,-2.40185500747651,
13.8281701127186));
#437965=CARTESIAN_POINT('Ctrl Pts',(-1.1919152730911,-2.40303389142641,
13.8253580685121));
#437966=CARTESIAN_POINT('Ctrl Pts',(-1.19222952128689,-2.40328947473904,
13.8247484142933));
#437967=CARTESIAN_POINT('Ctrl Pts',(-1.19253641265792,-2.40355032634256,
13.8241378483365));
#437968=CARTESIAN_POINT('Ctrl Pts',(-1.19283550652458,-2.40381648963782,
13.8235269408515));
#437969=CARTESIAN_POINT('',(-1.15495886952874,-2.39857892755329,12.5969504640361));
#437970=CARTESIAN_POINT('Origin',(-1.16999804659657,-2.42952552641878,12.584524458991));
#437971=CARTESIAN_POINT('Origin',(-1.16999804659657,-2.42952552641878,12.584524458991));
#437972=CARTESIAN_POINT('Ctrl Pts',(-1.13565863606154,-2.43135141923567,
12.5893111709658));
#437973=CARTESIAN_POINT('Ctrl Pts',(-1.13504681103694,-2.42003398557344,
12.5770542771492));
#437974=CARTESIAN_POINT('Ctrl Pts',(-1.15093645054157,-2.41611952120801,
12.5737548217797));
#437975=CARTESIAN_POINT('Ctrl Pts',(-1.13699649205574,-2.45609884841133,
12.5663937883685));
#437976=CARTESIAN_POINT('Ctrl Pts',(-1.13638388656337,-2.44476697779074,
12.5540940315304));
#437977=CARTESIAN_POINT('Ctrl Pts',(-1.15232353295924,-2.44084350125998,
12.5508374392248));
#437978=CARTESIAN_POINT('Ctrl Pts',(-1.13833299816964,-2.48082130773439,
12.5434499600945));
#437979=CARTESIAN_POINT('Ctrl Pts',(-1.13771840087868,-2.46945259316697,
12.5311293540533));
#437980=CARTESIAN_POINT('Ctrl Pts',(-1.15370808215303,-2.46554339154704,
12.5278936106989));
#437981=CARTESIAN_POINT('Ctrl Pts',(-1.13966826014122,-2.50552075312746,
12.5204817579905));
#437982=CARTESIAN_POINT('Ctrl Pts',(-1.13905062101366,-2.4940957711924,
12.5081597038247));
#437983=CARTESIAN_POINT('Ctrl Pts',(-1.1550902811826,-2.49022106519589,
12.5049254088044));
#437984=CARTESIAN_POINT('Ctrl Pts',(-1.1387082681697,-2.48776298739836,
12.5369868989719));
#437985=CARTESIAN_POINT('Ctrl Pts',(-1.1387585524309,-2.48869313398025,
12.5342545179733));
#437986=CARTESIAN_POINT('Ctrl Pts',(-1.13893110561746,-2.48957408943381,
12.5314872231885));
#437987=CARTESIAN_POINT('Ctrl Pts',(-1.13927106601802,-2.49034548300144,
12.5287124745063));
#437988=CARTESIAN_POINT('Ctrl Pts',(-1.13957765918138,-2.49104116400929,
12.5262100684184));
#437989=CARTESIAN_POINT('Ctrl Pts',(-1.14002100086742,-2.49164663612851,
12.5237004536639));
#437990=CARTESIAN_POINT('Ctrl Pts',(-1.14066218882733,-2.49213313234792,
12.5212220730815));
#437991=CARTESIAN_POINT('Ctrl Pts',(-1.14115307367782,-2.49250558728916,
12.5193246583486));
#437992=CARTESIAN_POINT('Ctrl Pts',(-1.14176617106602,-2.49281225358285,
12.517417831369));
#437993=CARTESIAN_POINT('Ctrl Pts',(-1.14256128104741,-2.49297646326884,
12.5155812248347));
#437994=CARTESIAN_POINT('Ctrl Pts',(-1.14290000217322,-2.49304641747771,
12.5147988205793));
#437995=CARTESIAN_POINT('Ctrl Pts',(-1.14327204286964,-2.49309086089055,
12.5140295443047));
#437996=CARTESIAN_POINT('Ctrl Pts',(-1.14368284537006,-2.49310582947374,
12.5132817086137));
#437997=CARTESIAN_POINT('Ctrl Pts',(-1.14430453938234,-2.4931284823995,
12.5121499604604));
#437998=CARTESIAN_POINT('Ctrl Pts',(-1.14502869393135,-2.493076972148,12.5110494206568));
#437999=CARTESIAN_POINT('Ctrl Pts',(-1.14586476016472,-2.49291527685706,
12.5100666561695));
#438000=CARTESIAN_POINT('Ctrl Pts',(-1.14634482747063,-2.49282243179336,
12.5095023550641));
#438001=CARTESIAN_POINT('Ctrl Pts',(-1.14686721518658,-2.49269154478228,
12.5089719619137));
#438002=CARTESIAN_POINT('Ctrl Pts',(-1.14742057942457,-2.49251887368723,
12.5085043804652));
#438003=CARTESIAN_POINT('Ctrl Pts',(-1.14823035590611,-2.49226619203162,
12.5078201359221));
#438004=CARTESIAN_POINT('Ctrl Pts',(-1.14912959354634,-2.49191555022426,
12.5072563000953));
#438005=CARTESIAN_POINT('Ctrl Pts',(-1.15005426168245,-2.4914828290387,
12.5068768744336));
#438006=CARTESIAN_POINT('Ctrl Pts',(-1.15072101106295,-2.49117080727528,
12.5066032824118));
#438007=CARTESIAN_POINT('Ctrl Pts',(-1.15141272202142,-2.49081068178022,
12.5064197834844));
#438008=CARTESIAN_POINT('Ctrl Pts',(-1.15209196128879,-2.4904248556342,
12.5063282718343));
#438009=CARTESIAN_POINT('Ctrl Pts',(-1.15308344033198,-2.48986166890977,
12.5061946931565));
#438010=CARTESIAN_POINT('Ctrl Pts',(-1.15407006230495,-2.48923260805229,
12.5062515701262));
#438011=CARTESIAN_POINT('Ctrl Pts',(-1.15499890962263,-2.48858975326374,
12.5064436508398));
#438012=CARTESIAN_POINT('',(-1.15093645054157,-2.41611952120801,12.5737548217797));
#438013=CARTESIAN_POINT('Origin',(-1.15762655855609,-2.43016382449276,12.5893111709658));
#438014=CARTESIAN_POINT('Ctrl Pts',(-1.15499890962263,-2.48858975326374,
12.5064436508398));
#438015=CARTESIAN_POINT('Ctrl Pts',(-1.15439803982179,-2.47786224920951,
12.5164271754438));
#438016=CARTESIAN_POINT('Ctrl Pts',(-1.15379672322763,-2.46713050445973,
12.5264061185523));
#438017=CARTESIAN_POINT('Ctrl Pts',(-1.15319494504947,-2.45639436960773,
12.536380305637));
#438018=CARTESIAN_POINT('Ctrl Pts',(-1.15244284438053,-2.44297637856549,
12.5488460165097));
#438019=CARTESIAN_POINT('Ctrl Pts',(-1.1516900224742,-2.42955152625198,
12.5613043021964));
#438020=CARTESIAN_POINT('Ctrl Pts',(-1.15093645054157,-2.41611952120801,
12.5737548217797));
#438021=CARTESIAN_POINT('Ctrl Pts',(-1.19283550652457,-2.40381648963782,
12.5893111709658));
#438022=CARTESIAN_POINT('Ctrl Pts',(-1.18436864725005,-2.39628184110022,
12.5770542771492));
#438023=CARTESIAN_POINT('Ctrl Pts',(-1.17140116758582,-2.40626423289842,
12.5737548217797));
#438024=CARTESIAN_POINT('Ctrl Pts',(-1.1849360004623,-2.39678672808515,
12.5928319619712));
#438025=CARTESIAN_POINT('Ctrl Pts',(-1.1770800489029,-2.39415662514653,
12.5821634970842));
#438026=CARTESIAN_POINT('Ctrl Pts',(-1.16852984354534,-2.40369640976901,
12.5773203894503));
#438027=CARTESIAN_POINT('Ctrl Pts',(-1.16891850806534,-2.39188529598292,
12.5969440695591));
#438028=CARTESIAN_POINT('Ctrl Pts',(-1.16528892992905,-2.39361292589252,
12.5878292599214));
#438029=CARTESIAN_POINT('Ctrl Pts',(-1.16282028373094,-2.40195139577956,
12.5813877129824));
#438030=CARTESIAN_POINT('Ctrl Pts',(-1.14132822680162,-2.40511222402121,
12.596957478804));
#438031=CARTESIAN_POINT('Ctrl Pts',(-1.14493101583289,-2.40339743413758,
12.5878468778671));
#438032=CARTESIAN_POINT('Ctrl Pts',(-1.15294791830037,-2.4066908756149,
12.5814011370086));
#438033=CARTESIAN_POINT('Ctrl Pts',(-1.13508697979447,-2.42077702031531,
12.5928371701607));
#438034=CARTESIAN_POINT('Ctrl Pts',(-1.13793244152173,-2.41300280567571,
12.5821692192951));
#438035=CARTESIAN_POINT('Ctrl Pts',(-1.1507181382198,-2.41226133287615,
12.5773318885715));
#438036=CARTESIAN_POINT('Ctrl Pts',(-1.13565863606148,-2.43135141923566,
12.5893111709658));
#438037=CARTESIAN_POINT('Ctrl Pts',(-1.13504681103689,-2.42003398557343,
12.5770542771492));
#438038=CARTESIAN_POINT('Ctrl Pts',(-1.15093645054151,-2.41611952120801,
12.5737548217797));
#438039=CARTESIAN_POINT('',(-1.17140116758582,-2.40626423289842,12.5737548217797));
#438040=CARTESIAN_POINT('Origin',(-1.17821023192278,-2.42025124983754,12.5893111709658));
#438041=CARTESIAN_POINT('Ctrl Pts',(-1.15093645054151,-2.41611952120801,
12.5737548217797));
#438042=CARTESIAN_POINT('Ctrl Pts',(-1.15084974296275,-2.41512112177552,
12.5746934679442));
#438043=CARTESIAN_POINT('Ctrl Pts',(-1.15093629260766,-2.41400047705163,
12.5756680099006));
#438044=CARTESIAN_POINT('Ctrl Pts',(-1.15118293246642,-2.4128848281606,
12.5765688348656));
#438045=CARTESIAN_POINT('Ctrl Pts',(-1.15124822763864,-2.41258947246734,
12.5768073183026));
#438046=CARTESIAN_POINT('Ctrl Pts',(-1.15132448603172,-2.41229447418314,
12.5770407398754));
#438047=CARTESIAN_POINT('Ctrl Pts',(-1.15141091446458,-2.41200206818303,
12.5772674179684));
#438048=CARTESIAN_POINT('Ctrl Pts',(-1.1517655933818,-2.41080211302853,
12.5781976435658));
#438049=CARTESIAN_POINT('Ctrl Pts',(-1.15232250404031,-2.40958085629827,
12.5790594849312));
#438050=CARTESIAN_POINT('Ctrl Pts',(-1.15308797946507,-2.40844079485354,
12.5797571720116));
#438051=CARTESIAN_POINT('Ctrl Pts',(-1.15358671422835,-2.40769800382934,
12.580211740231));
#438052=CARTESIAN_POINT('Ctrl Pts',(-1.15421223510576,-2.40696638875824,
12.5806009430798));
#438053=CARTESIAN_POINT('Ctrl Pts',(-1.15493397400486,-2.40630896528297,
12.5808812374708));
#438054=CARTESIAN_POINT('Ctrl Pts',(-1.15555418715358,-2.40574402041974,
12.5811221033394));
#438055=CARTESIAN_POINT('Ctrl Pts',(-1.15625822687442,-2.40522238086587,
12.581287365893));
#438056=CARTESIAN_POINT('Ctrl Pts',(-1.15701131981742,-2.40478018825776,
12.581359338449));
#438057=CARTESIAN_POINT('Ctrl Pts',(-1.15711598418572,-2.40471873261616,
12.5813693411482));
#438058=CARTESIAN_POINT('Ctrl Pts',(-1.15722158465408,-2.40465875272587,
12.5813775999465));
#438059=CARTESIAN_POINT('Ctrl Pts',(-1.15732801729123,-2.40460028518414,
12.5813841266931));
#438060=CARTESIAN_POINT('Ctrl Pts',(-1.1575085931329,-2.40450108792808,
12.5813952001081));
#438061=CARTESIAN_POINT('Ctrl Pts',(-1.15769306695728,-2.40440611327763,
12.5814007534795));
#438062=CARTESIAN_POINT('Ctrl Pts',(-1.15788144869047,-2.40431557793399,
12.5814005856065));
#438063=CARTESIAN_POINT('Ctrl Pts',(-1.15874378661253,-2.40390114252785,
12.5813998171494));
#438064=CARTESIAN_POINT('Ctrl Pts',(-1.1596282857063,-2.40360806070685,
12.58127954464));
#438065=CARTESIAN_POINT('Ctrl Pts',(-1.16052061744996,-2.40340990882978,
12.5810700125799));
#438066=CARTESIAN_POINT('Ctrl Pts',(-1.16159845259619,-2.40317056392368,
12.5808169217085));
#438067=CARTESIAN_POINT('Ctrl Pts',(-1.1626914409695,-2.40308603715113,
12.5804173076348));
#438068=CARTESIAN_POINT('Ctrl Pts',(-1.16370178691457,-2.40313777146221,
12.5799304713245));
#438069=CARTESIAN_POINT('Ctrl Pts',(-1.1649539238323,-2.40320188657163,
12.5793271277669));
#438070=CARTESIAN_POINT('Ctrl Pts',(-1.16615844908136,-2.40344710429688,
12.5785808224116));
#438071=CARTESIAN_POINT('Ctrl Pts',(-1.16727091675368,-2.40383200888381,
12.5777485681082));
#438072=CARTESIAN_POINT('Ctrl Pts',(-1.16892861546537,-2.40440555888777,
12.576508418016));
#438073=CARTESIAN_POINT('Ctrl Pts',(-1.17037019597565,-2.40527794936408,
12.5750928681475));
#438074=CARTESIAN_POINT('Ctrl Pts',(-1.17140116758582,-2.40626423289842,
12.5737548217797));
#438075=CARTESIAN_POINT('Ctrl Pts',(-1.17140116758582,-2.40626423289842,
12.5737548217797));
#438076=CARTESIAN_POINT('Ctrl Pts',(-1.18436864725005,-2.39628184110022,
12.5770542771492));
#438077=CARTESIAN_POINT('Ctrl Pts',(-1.19283550652458,-2.40381648963782,
12.5893111709658));
#438078=CARTESIAN_POINT('Ctrl Pts',(-1.1898635477239,-2.42276136821965,
12.5508408821982));
#438079=CARTESIAN_POINT('Ctrl Pts',(-1.20286924391508,-2.4127455012471,
12.55409748406));
#438080=CARTESIAN_POINT('Ctrl Pts',(-1.21134690473358,-2.42028976206649,
12.5663972313419));
#438081=CARTESIAN_POINT('Ctrl Pts',(-1.20830867835785,-2.43924150837951,
12.52790050457));
#438082=CARTESIAN_POINT('Ctrl Pts',(-1.22133440753403,-2.4291776295661,
12.5311362602938));
#438083=CARTESIAN_POINT('Ctrl Pts',(-1.22983962798362,-2.4367464156702,
12.5434568539655));
#438084=CARTESIAN_POINT('Ctrl Pts',(-1.22673790922254,-2.45570596379389,
12.5049357605811));
#438085=CARTESIAN_POINT('Ctrl Pts',(-1.23976783182079,-2.44558151308914,
12.5081700652078));
#438086=CARTESIAN_POINT('Ctrl Pts',(-1.24831513890126,-2.45318775203869,
12.5204921097672));
#438087=CARTESIAN_POINT('Ctrl Pts',(-1.225527774741,-2.45462484192911,12.5064436508395));
#438088=CARTESIAN_POINT('Ctrl Pts',(-1.22669623979225,-2.45427336331726,
12.5062361689309));
#438089=CARTESIAN_POINT('Ctrl Pts',(-1.22789635999824,-2.45385802837819,
12.5061871075061));
#438090=CARTESIAN_POINT('Ctrl Pts',(-1.22903356555542,-2.45339135915718,
12.5063648335164));
#438091=CARTESIAN_POINT('Ctrl Pts',(-1.22955015446524,-2.45317936921165,
12.5064455676329));
#438092=CARTESIAN_POINT('Ctrl Pts',(-1.2300608824062,-2.4529536256093,12.506574497099));
#438093=CARTESIAN_POINT('Ctrl Pts',(-1.23054342602523,-2.45272284632038,
12.5067492519495));
#438094=CARTESIAN_POINT('Ctrl Pts',(-1.23151311615859,-2.45225908638114,
12.5071004286051));
#438095=CARTESIAN_POINT('Ctrl Pts',(-1.23240429441423,-2.4517572112088,
12.5076537929612));
#438096=CARTESIAN_POINT('Ctrl Pts',(-1.2331547144264,-2.45126313059638,
12.5083435010503));
#438097=CARTESIAN_POINT('Ctrl Pts',(-1.23320195785079,-2.45123202526912,
12.5083869222963));
#438098=CARTESIAN_POINT('Ctrl Pts',(-1.23324864197509,-2.45120093747488,
12.5084308732336));
#438099=CARTESIAN_POINT('Ctrl Pts',(-1.233294751086,-2.45116987318738,12.5084753333615));
#438100=CARTESIAN_POINT('Ctrl Pts',(-1.23366460701339,-2.45092069660093,
12.508831962269));
#438101=CARTESIAN_POINT('Ctrl Pts',(-1.23400569518013,-2.45066904370223,
12.509227847131));
#438102=CARTESIAN_POINT('Ctrl Pts',(-1.23430953563616,-2.45042465061774,
12.5096423454524));
#438103=CARTESIAN_POINT('Ctrl Pts',(-1.23526163715123,-2.44965883085478,
12.5109411997424));
#438104=CARTESIAN_POINT('Ctrl Pts',(-1.23591261683561,-2.44892472763303,
12.5124831113042));
#438105=CARTESIAN_POINT('Ctrl Pts',(-1.23635254164439,-2.44825138920541,
12.5140723025008));
#438106=CARTESIAN_POINT('Ctrl Pts',(-1.23639376308081,-2.44818829665726,
12.5142212114565));
#438107=CARTESIAN_POINT('Ctrl Pts',(-1.23643316105228,-2.4481257362192,
12.5143705582413));
#438108=CARTESIAN_POINT('Ctrl Pts',(-1.23647082662168,-2.4480637325346,
12.5145201959299));
#438109=CARTESIAN_POINT('Ctrl Pts',(-1.23695469693871,-2.44726720289212,
12.5164425148273));
#438110=CARTESIAN_POINT('Ctrl Pts',(-1.23717842172837,-2.44654083865989,
12.5184635205941));
#438111=CARTESIAN_POINT('Ctrl Pts',(-1.23722973348005,-2.44586364010339,
12.5205025929158));
#438112=CARTESIAN_POINT('Ctrl Pts',(-1.23725949632984,-2.44547083809898,
12.5216853356836));
#438113=CARTESIAN_POINT('Ctrl Pts',(-1.23723167991553,-2.44509532378282,
12.5228750347131));
#438114=CARTESIAN_POINT('Ctrl Pts',(-1.23716444822797,-2.44473883009601,
12.5240609649613));
#438115=CARTESIAN_POINT('Ctrl Pts',(-1.23699943165769,-2.44386383546695,
12.5269717671326));
#438116=CARTESIAN_POINT('Ctrl Pts',(-1.23658210549582,-2.44308072764374,
12.5299036066169));
#438117=CARTESIAN_POINT('Ctrl Pts',(-1.2359945034257,-2.44236157819242,
12.5328133004019));
#438118=CARTESIAN_POINT('Ctrl Pts',(-1.23571242021699,-2.44201634458096,
12.5342101228451));
#438119=CARTESIAN_POINT('Ctrl Pts',(-1.2353910420462,-2.44168661290519,
12.5356023438238));
#438120=CARTESIAN_POINT('Ctrl Pts',(-1.2350384319707,-2.44137282548623,
12.5369868989719));
#438121=CARTESIAN_POINT('Origin',(-10.7595719109441,-10.9101544928126,-1.23977369531144));
#438122=CARTESIAN_POINT('Ctrl Pts',(-1.13870597240883,-2.48772125622983,
12.5369868989719));
#438123=CARTESIAN_POINT('Ctrl Pts',(-1.1395630890155,-2.50303623761445,
12.5369868989719));
#438124=CARTESIAN_POINT('Ctrl Pts',(-1.12548920298435,-2.50913615857057,
12.5369868989719));
#438125=CARTESIAN_POINT('Ctrl Pts',(-1.13899564523504,-2.49289832260301,
12.5218025310015));
#438126=CARTESIAN_POINT('Ctrl Pts',(-1.13631807036062,-2.50440859872906,
12.5216901060418));
#438127=CARTESIAN_POINT('Ctrl Pts',(-1.12553211141151,-2.50911757912156,
12.5161920673677));
#438128=CARTESIAN_POINT('Ctrl Pts',(-1.14408058035852,-2.49613552911253,
12.5042015548896));
#438129=CARTESIAN_POINT('Ctrl Pts',(-1.14148438124073,-2.50202085791889,
12.4980677368514));
#438130=CARTESIAN_POINT('Ctrl Pts',(-1.13529857321621,-2.50483627241908,
12.4907278922778));
#438131=CARTESIAN_POINT('Ctrl Pts',(-1.15499048945561,-2.48857161093493,
12.5064636261921));
#438132=CARTESIAN_POINT('Ctrl Pts',(-1.15774489135786,-2.49450631467633,
12.4999376786892));
#438133=CARTESIAN_POINT('Ctrl Pts',(-1.15771125034352,-2.49443383089918,
12.4906970594712));
#438134=CARTESIAN_POINT('Origin',(-1.11674034567515,-2.48895058214127,12.5369868989719));
#438135=CARTESIAN_POINT('Origin',(-1.11674034567515,-2.48895058214127,14.));
#438136=CARTESIAN_POINT('Origin',(-1.11674034567515,-2.48895058214127,13.7435492065112));
#438137=CARTESIAN_POINT('Ctrl Pts',(-1.13737165154344,-2.46303898681411,
13.793642941384));
#438138=CARTESIAN_POINT('Ctrl Pts',(-1.1379824978865,-2.47383403594557,
13.8071662555867));
#438139=CARTESIAN_POINT('Ctrl Pts',(-1.1213059701016,-2.47728552905356,
13.8103758687955));
#438140=CARTESIAN_POINT('Ctrl Pts',(-1.13826888894079,-2.4796358741812,
13.7804579775006));
#438141=CARTESIAN_POINT('Ctrl Pts',(-1.13901249351036,-2.4929565620003,
13.7901904343351));
#438142=CARTESIAN_POINT('Ctrl Pts',(-1.12430329422377,-2.49860416153562,
13.7927914348263));
#438143=CARTESIAN_POINT('Ctrl Pts',(-1.13879712632548,-2.48940708638739,
13.7597120340895));
#438144=CARTESIAN_POINT('Ctrl Pts',(-1.13965196473683,-2.50482319294067,
13.7635825532445));
#438145=CARTESIAN_POINT('Ctrl Pts',(-1.12604549938884,-2.51117929370123,
13.7651073818884));
#438146=CARTESIAN_POINT('Ctrl Pts',(-1.13869368534948,-2.48749365930215,
13.7381884353898));
#438147=CARTESIAN_POINT('Ctrl Pts',(-1.13952941212877,-2.50254887339484,
13.7368803041982));
#438148=CARTESIAN_POINT('Ctrl Pts',(-1.12570383429319,-2.50871677697964,
13.7363986145813));
#438149=CARTESIAN_POINT('Origin',(-1.11562146849283,-2.46825378521706,13.7902182540695));
#438150=CARTESIAN_POINT('Ctrl Pts',(-1.13565842282151,-2.43134748881746,
13.8235227101244));
#438151=CARTESIAN_POINT('Ctrl Pts',(-1.13628347989388,-2.44282755815418,
13.8358800583119));
#438152=CARTESIAN_POINT('Ctrl Pts',(-1.1201664623594,-2.44668343611514,
13.8390832900376));
#438153=CARTESIAN_POINT('Ctrl Pts',(-1.13630229239036,-2.44325767694664,
13.8124254819053));
#438154=CARTESIAN_POINT('Ctrl Pts',(-1.13692856303695,-2.45476004043042,
13.8247886449157));
#438155=CARTESIAN_POINT('Ctrl Pts',(-1.12078721517006,-2.45860421396217,
13.8279860620657));
#438156=CARTESIAN_POINT('Ctrl Pts',(-1.13694587339782,-2.45516252731703,
13.8013225099955));
#438157=CARTESIAN_POINT('Ctrl Pts',(-1.1375730641211,-2.46668175757036,
13.8136962257787));
#438158=CARTESIAN_POINT('Ctrl Pts',(-1.1214079512921,-2.47051945897964,
13.8168830918626));
#438159=CARTESIAN_POINT('Ctrl Pts',(-1.13758917707139,-2.46706224761251,
13.7902140179785));
#438160=CARTESIAN_POINT('Ctrl Pts',(-1.13821701355319,-2.4785932719771,
13.802602731458));
#438161=CARTESIAN_POINT('Ctrl Pts',(-1.12202867321908,-2.48242938847018,
13.8057746032558));
#438162=CARTESIAN_POINT('Origin',(-1.11369071356699,-2.43253901397857,13.8235269408515));
#438163=CARTESIAN_POINT('Ctrl Pts',(-1.19283550652458,-2.40381648963782,
13.8235269408515));
#438164=CARTESIAN_POINT('Ctrl Pts',(-1.20165610318867,-2.41166592868022,
13.8362179249168));
#438165=CARTESIAN_POINT('Ctrl Pts',(-1.2149234196493,-2.40091226335202,
13.8391868794938));
#438166=CARTESIAN_POINT('Ctrl Pts',(-1.18476504451463,-2.39663459457976,
13.8400110824519));
#438167=CARTESIAN_POINT('Ctrl Pts',(-1.19411123465536,-2.40037232018696,
13.8494522556836));
#438168=CARTESIAN_POINT('Ctrl Pts',(-1.20156702432301,-2.38917682609929,
13.85569149686));
#438169=CARTESIAN_POINT('Ctrl Pts',(-1.16922809060941,-2.39173553452791,
13.8586819406588));
#438170=CARTESIAN_POINT('Ctrl Pts',(-1.17315679192385,-2.38985900858434,
13.868010383617));
#438171=CARTESIAN_POINT('Ctrl Pts',(-1.17573146690084,-2.3811835307557,
13.8744918421245));
#438172=CARTESIAN_POINT('Ctrl Pts',(-1.14101383472849,-2.40526429141955,
13.8587686893867));
#438173=CARTESIAN_POINT('Ctrl Pts',(-1.13712007455004,-2.40712406548985,
13.8680909899357));
#438174=CARTESIAN_POINT('Ctrl Pts',(-1.12876412885016,-2.40370725806675,
13.8745789365163));
#438175=CARTESIAN_POINT('Ctrl Pts',(-1.13507450618019,-2.42054628567277,
13.8400379222776));
#438176=CARTESIAN_POINT('Ctrl Pts',(-1.1321634108241,-2.43017934114523,
13.8494748685453));
#438177=CARTESIAN_POINT('Ctrl Pts',(-1.11876789428566,-2.42902988826086,
13.8557104837033));
#438178=CARTESIAN_POINT('Ctrl Pts',(-1.13565863605493,-2.43135141923588,
13.8235269408542));
#438179=CARTESIAN_POINT('Ctrl Pts',(-1.13629602255157,-2.44314168459525,
13.8362179249195));
#438180=CARTESIAN_POINT('Ctrl Pts',(-1.11961643193484,-2.44680968962724,
13.8391868794965));
#438181=CARTESIAN_POINT('Origin',(-1.20746078112637,-2.38738172943811,13.8235269408515));
#438182=CARTESIAN_POINT('Ctrl Pts',(-1.21955168809193,-2.427591188524,13.7902140241682));
#438183=CARTESIAN_POINT('Ctrl Pts',(-1.22817555722196,-2.43527151902604,
13.8026027327198));
#438184=CARTESIAN_POINT('Ctrl Pts',(-1.2412680137648,-2.42500674850023,
13.8057746032556));
#438185=CARTESIAN_POINT('Ctrl Pts',(-1.21064920540935,-2.41966887920736,
13.8013225161808));
#438186=CARTESIAN_POINT('Ctrl Pts',(-1.21926425615093,-2.42734135133865,
13.8136962270464));
#438187=CARTESIAN_POINT('Ctrl Pts',(-1.23234346972602,-2.41709572897734,
13.8168830918628));
#438188=CARTESIAN_POINT('Ctrl Pts',(-1.20174288478636,-2.4117431545119,
13.8124254880875));
#438189=CARTESIAN_POINT('Ctrl Pts',(-1.21034532221329,-2.41940439105412,
13.8247886461868));
#438190=CARTESIAN_POINT('Ctrl Pts',(-1.22341477869207,-2.40918138418004,
13.8279860620656));
#438191=CARTESIAN_POINT('Ctrl Pts',(-1.19283257084815,-2.40381387616973,
13.8235227163065));
#438192=CARTESIAN_POINT('Ctrl Pts',(-1.2014183346621,-2.41146026374608,
13.8358800595848));
#438193=CARTESIAN_POINT('Ctrl Pts',(-1.21448177232259,-2.40126357667191,
13.8390832900376));
#438194=CARTESIAN_POINT('Origin',(-1.23417990766361,-2.41115905006698,13.7902182540695));
#438195=CARTESIAN_POINT('Ctrl Pts',(-1.23483685563678,-2.44119340600829,
13.7382347919292));
#438196=CARTESIAN_POINT('Ctrl Pts',(-1.24609387954608,-2.45124314637504,
13.7369371795942));
#438197=CARTESIAN_POINT('Ctrl Pts',(-1.25954281517536,-2.44426676425679,
13.7364597369711));
#438198=CARTESIAN_POINT('Ctrl Pts',(-1.23624991501483,-2.44245088649656,
13.7595490285574));
#438199=CARTESIAN_POINT('Ctrl Pts',(-1.2477761914503,-2.4527396550308,13.7633824266926));
#438200=CARTESIAN_POINT('Ctrl Pts',(-1.26123381543314,-2.44604741945186,
13.7648920890506));
#438201=CARTESIAN_POINT('Ctrl Pts',(-1.22904338959518,-2.43603780490276,
13.780380659011));
#438202=CARTESIAN_POINT('Ctrl Pts',(-1.23900961120005,-2.44494124878293,
13.7901039518743));
#438203=CARTESIAN_POINT('Ctrl Pts',(-1.25261021923682,-2.43697200148753,
13.7926933640892));
#438204=CARTESIAN_POINT('Ctrl Pts',(-1.21651683976832,-2.42489043745532,
13.7936647693663));
#438205=CARTESIAN_POINT('Ctrl Pts',(-1.22457637590267,-2.4321027331539,
13.8072068914933));
#438206=CARTESIAN_POINT('Ctrl Pts',(-1.23767985776185,-2.42119663242936,
13.8104111085397));
#438207=CARTESIAN_POINT('Origin',(-1.24966370657249,-2.42493806528651,13.7435492065112));
#438208=CARTESIAN_POINT('Origin',(-1.24966370657249,-2.42493806528651,14.));
#438209=CARTESIAN_POINT('Origin',(-1.24966370657249,-2.42493806528651,12.5369868989719));
#438210=CARTESIAN_POINT('Ctrl Pts',(-1.22551956306621,-2.45460839468648,
12.506462012331));
#438211=CARTESIAN_POINT('Ctrl Pts',(-1.22844032095039,-2.46045841702592,
12.4999388158272));
#438212=CARTESIAN_POINT('Ctrl Pts',(-1.22840576455428,-2.46038920358981,
12.4907030323752));
#438213=CARTESIAN_POINT('Ctrl Pts',(-1.23823453712172,-2.45079289761245,
12.5042014951932));
#438214=CARTESIAN_POINT('Ctrl Pts',(-1.24445160750402,-2.45243275522135,
12.4980716682127));
#438215=CARTESIAN_POINT('Ctrl Pts',(-1.25050600860596,-2.44935545242138,
12.4907355092743));
#438216=CARTESIAN_POINT('Ctrl Pts',(-1.23887623627451,-2.44480007495175,
12.5218047446509));
#438217=CARTESIAN_POINT('Ctrl Pts',(-1.24954002296379,-2.44987969347884,
12.5216906929434));
#438218=CARTESIAN_POINT('Ctrl Pts',(-1.25994304277591,-2.44438898012643,
12.5161988840776));
#438219=CARTESIAN_POINT('Ctrl Pts',(-1.23500975610474,-2.44134726196669,
12.5369868989719));
#438220=CARTESIAN_POINT('Ctrl Pts',(-1.24644390075447,-2.45155832790758,
12.5369868989719));
#438221=CARTESIAN_POINT('Ctrl Pts',(-1.25998281969171,-2.44436783379859,
12.5369868989719));
#438222=CARTESIAN_POINT('Origin',(-2.2353094088441E-31,-9.79353041666015E-31,
12.5));
#438223=CARTESIAN_POINT('Origin',(-0.992933084929622,-2.49304515609577,
12.5));
#438224=CARTESIAN_POINT('',(-0.992933084929622,-2.49304515609577,12.5893111709658));
#438225=CARTESIAN_POINT('',(-0.992933084929622,-2.49304515609577,13.8235269408515));
#438226=CARTESIAN_POINT('',(-0.992933084929622,-2.49304515609577,12.5));
#438227=CARTESIAN_POINT('',(-1.01762523340836,-2.51892121651279,13.7902182540695));
#438228=CARTESIAN_POINT('',(-0.992933084929622,-2.49304515609577,13.8235269408515));
#438229=CARTESIAN_POINT('',(-1.03193439359516,-2.53391645655153,13.7435492065112));
#438230=CARTESIAN_POINT('Origin',(-0.984857210047735,-2.48458253992091,
13.7445212918699));
#438231=CARTESIAN_POINT('',(-1.03193439359516,-2.53391645655153,12.5369868989719));
#438232=CARTESIAN_POINT('',(-1.03193439359516,-2.53391645655153,12.5));
#438233=CARTESIAN_POINT('Ctrl Pts',(-1.03193439359516,-2.53391645655153,
12.5369868989719));
#438234=CARTESIAN_POINT('Ctrl Pts',(-1.01894343910079,-2.52030262607984,
12.5544431401645));
#438235=CARTESIAN_POINT('Ctrl Pts',(-1.00594319313049,-2.50667905863477,
12.5718848856037));
#438236=CARTESIAN_POINT('Ctrl Pts',(-0.992933084929622,-2.49304515609577,
12.5893111709658));
#438237=CARTESIAN_POINT('Origin',(-0.926115282099995,-2.79072334525639,
12.5));
#438238=CARTESIAN_POINT('',(-0.932143531606444,-2.57230045639142,13.7435492065112));
#438239=CARTESIAN_POINT('',(-0.932715358484657,-2.55158132747411,13.7902182540695));
#438240=CARTESIAN_POINT('Origin',(-0.934218020689041,-2.4971350376651,13.7418732680449));
#438241=CARTESIAN_POINT('',(-0.93370211340225,-2.51582801973994,13.8235269408515));
#438242=CARTESIAN_POINT('',(-0.932715358484657,-2.55158132747411,13.7902182540695));
#438243=CARTESIAN_POINT('',(-0.93370211340225,-2.51582801973994,12.5893111709658));
#438244=CARTESIAN_POINT('',(-0.93370211340225,-2.51582801973994,12.5));
#438245=CARTESIAN_POINT('',(-0.932143531606444,-2.57230045639142,12.5369868989719));
#438246=CARTESIAN_POINT('Ctrl Pts',(-0.93370211340225,-2.51582801973994,
12.5893111709658));
#438247=CARTESIAN_POINT('Ctrl Pts',(-0.933182199622504,-2.53466616995441,
12.5718848856037));
#438248=CARTESIAN_POINT('Ctrl Pts',(-0.932662679960124,-2.55349004002779,
12.5544431401645));
#438249=CARTESIAN_POINT('Ctrl Pts',(-0.932143531606444,-2.57230045639142,
12.5369868989719));
#438250=CARTESIAN_POINT('',(-0.932143531606444,-2.57230045639142,12.5));
#438251=CARTESIAN_POINT('Origin',(-0.968064029091806,-2.51677637365273,
12.5));
#438252=CARTESIAN_POINT('',(-0.956775034650937,-2.48430871625815,13.8587068136939));
#438253=CARTESIAN_POINT('Ctrl Pts',(-0.933702113395648,-2.51582801973962,
13.8235269408542));
#438254=CARTESIAN_POINT('Ctrl Pts',(-0.93375045663856,-2.5140763883977,
13.8262006681044));
#438255=CARTESIAN_POINT('Ctrl Pts',(-0.933973602084865,-2.51228864285042,
13.8288634856214));
#438256=CARTESIAN_POINT('Ctrl Pts',(-0.934358865203114,-2.51046889511799,
13.8314912288862));
#438257=CARTESIAN_POINT('Ctrl Pts',(-0.934756031739981,-2.50859292290412,
13.834200161153));
#438258=CARTESIAN_POINT('Ctrl Pts',(-0.935325443606471,-2.50668075376416,
13.8368750301949));
#438259=CARTESIAN_POINT('Ctrl Pts',(-0.93609708987527,-2.50472606935137,
13.8394886372968));
#438260=CARTESIAN_POINT('Ctrl Pts',(-0.936156685988365,-2.50457510433276,
13.839690492513));
#438261=CARTESIAN_POINT('Ctrl Pts',(-0.936217510093172,-2.50442389017867,
13.8398919674349));
#438262=CARTESIAN_POINT('Ctrl Pts',(-0.936279586968705,-2.50427242725917,
13.8400930404591));
#438263=CARTESIAN_POINT('Ctrl Pts',(-0.937246786452742,-2.50191253307414,
13.8432258934518));
#438264=CARTESIAN_POINT('Ctrl Pts',(-0.938512128561357,-2.49950386409913,
13.8462331177034));
#438265=CARTESIAN_POINT('Ctrl Pts',(-0.940119744156371,-2.49716984094109,
13.8489036603661));
#438266=CARTESIAN_POINT('Ctrl Pts',(-0.940645774687823,-2.49640612140139,
13.8497774930041));
#438267=CARTESIAN_POINT('Ctrl Pts',(-0.941208445707454,-2.49565064387015,
13.85061494757));
#438268=CARTESIAN_POINT('Ctrl Pts',(-0.941809274587624,-2.49490844552581,
13.8514076489583));
#438269=CARTESIAN_POINT('Ctrl Pts',(-0.94308011432168,-2.49333858898651,
13.8530843267192));
#438270=CARTESIAN_POINT('Ctrl Pts',(-0.944648794985787,-2.49167580124265,
13.8546805203176));
#438271=CARTESIAN_POINT('Ctrl Pts',(-0.946523520273043,-2.49011022213736,
13.8559412814273));
#438272=CARTESIAN_POINT('Ctrl Pts',(-0.946774419315257,-2.48990069688014,
13.8561100121513));
#438273=CARTESIAN_POINT('Ctrl Pts',(-0.947030724246209,-2.48969289973054,
13.8562727473908));
#438274=CARTESIAN_POINT('Ctrl Pts',(-0.94729238217205,-2.48948726437471,
13.8564289040185));
#438275=CARTESIAN_POINT('Ctrl Pts',(-0.948478997880653,-2.48855471038203,
13.8571370725437));
#438276=CARTESIAN_POINT('Ctrl Pts',(-0.94979796794662,-2.48765201425111,
13.8577210840554));
#438277=CARTESIAN_POINT('Ctrl Pts',(-0.951214599174453,-2.48683848301476,
13.8581177131616));
#438278=CARTESIAN_POINT('Ctrl Pts',(-0.951613571287177,-2.48660936461771,
13.8582294175695));
#438279=CARTESIAN_POINT('Ctrl Pts',(-0.952020172770695,-2.48638718488984,
13.8583265086086));
#438280=CARTESIAN_POINT('Ctrl Pts',(-0.952433359538227,-2.48617292107015,
13.8584082369006));
#438281=CARTESIAN_POINT('Ctrl Pts',(-0.953026998122757,-2.48586508141838,
13.8585256585398));
#438282=CARTESIAN_POINT('Ctrl Pts',(-0.953641759216969,-2.48557004164507,
13.8586122832068));
#438283=CARTESIAN_POINT('Ctrl Pts',(-0.954262014788582,-2.48529617797002,
13.8586682984299));
#438284=CARTESIAN_POINT('Ctrl Pts',(-0.954758157761914,-2.48507711417722,
13.8587131050557));
#438285=CARTESIAN_POINT('Ctrl Pts',(-0.95526320152162,-2.48486896566403,
13.8587357943552));
#438286=CARTESIAN_POINT('Ctrl Pts',(-0.955777399059998,-2.48467217593436,
13.8587355499465));
#438287=CARTESIAN_POINT('Ctrl Pts',(-0.956109737188121,-2.48454498604038,
13.8587353919793));
#438288=CARTESIAN_POINT('Ctrl Pts',(-0.956442291482867,-2.48442388039903,
13.8587257282814));
#438289=CARTESIAN_POINT('Ctrl Pts',(-0.956775034650937,-2.48430871625814,
13.8587068136939));
#438290=CARTESIAN_POINT('Ctrl Pts',(-0.956775034650937,-2.48430871625814,
13.8587068136939));
#438291=CARTESIAN_POINT('Ctrl Pts',(-0.957869408790883,-2.48392994767706,
13.8586446046466));
#438292=CARTESIAN_POINT('Ctrl Pts',(-0.958965824211619,-2.48361536978293,
13.858482427929));
#438293=CARTESIAN_POINT('Ctrl Pts',(-0.960063345219124,-2.48336061102754,
13.8582284286032));
#438294=CARTESIAN_POINT('Ctrl Pts',(-0.961189274103965,-2.48309925817926,
13.8579678548414));
#438295=CARTESIAN_POINT('Ctrl Pts',(-0.962319463209768,-2.48290171479365,
13.857615680862));
#438296=CARTESIAN_POINT('Ctrl Pts',(-0.96340768732622,-2.48276622390876,
13.8571944833187));
#438297=CARTESIAN_POINT('Ctrl Pts',(-0.966123461903261,-2.48242809254866,
13.8561433417727));
#438298=CARTESIAN_POINT('Ctrl Pts',(-0.96870432018962,-2.48245585067075,
13.8546163505474));
#438299=CARTESIAN_POINT('Ctrl Pts',(-0.971016065270771,-2.48269217995195,
13.8528973491086));
#438300=CARTESIAN_POINT('Ctrl Pts',(-0.971438386990478,-2.48273535382492,
13.8525833129072));
#438301=CARTESIAN_POINT('Ctrl Pts',(-0.971851805046089,-2.48278537047581,
13.8522628768812));
#438302=CARTESIAN_POINT('Ctrl Pts',(-0.972255621678871,-2.48284113856929,
13.851937733538));
#438303=CARTESIAN_POINT('Ctrl Pts',(-0.974721673828254,-2.48318170657871,
13.8499521282529));
#438304=CARTESIAN_POINT('Ctrl Pts',(-0.977074174142894,-2.48377465343844,
13.847639871647));
#438305=CARTESIAN_POINT('Ctrl Pts',(-0.979209119630498,-2.48451091184536,
13.8452109780794));
#438306=CARTESIAN_POINT('Ctrl Pts',(-0.980169675796545,-2.48484216974243,
13.8441181685877));
#438307=CARTESIAN_POINT('Ctrl Pts',(-0.981086646874305,-2.48520188224661,
13.8430021611332));
#438308=CARTESIAN_POINT('Ctrl Pts',(-0.981953344580685,-2.48557832776729,
13.8418824960098));
#438309=CARTESIAN_POINT('Ctrl Pts',(-0.983995739857683,-2.48646543124966,
13.8392439765549));
#438310=CARTESIAN_POINT('Ctrl Pts',(-0.985858098390244,-2.48748439486929,
13.8364981347964));
#438311=CARTESIAN_POINT('Ctrl Pts',(-0.987561770866305,-2.48860789258945,
13.8336931113419));
#438312=CARTESIAN_POINT('Ctrl Pts',(-0.989221039664782,-2.48970210802017,
13.8309611966328));
#438313=CARTESIAN_POINT('Ctrl Pts',(-0.990731138435674,-2.49089704719818,
13.8281701127186));
#438314=CARTESIAN_POINT('Ctrl Pts',(-0.9920797025165,-2.49219015434749,
13.8253580685121));
#438315=CARTESIAN_POINT('Ctrl Pts',(-0.992372072664643,-2.49247050137303,
13.8247484142933));
#438316=CARTESIAN_POINT('Ctrl Pts',(-0.992656681052636,-2.49275549951013,
13.8241378483365));
#438317=CARTESIAN_POINT('Ctrl Pts',(-0.992933084929622,-2.49304515609577,
13.8235269408515));
#438318=CARTESIAN_POINT('',(-0.955609389251859,-2.4847377240223,12.5969504640361));
#438319=CARTESIAN_POINT('Origin',(-0.968076089596869,-2.51680718318092,
12.584524458991));
#438320=CARTESIAN_POINT('Origin',(-0.968076089596869,-2.51680718318092,
12.584524458991));
#438321=CARTESIAN_POINT('Ctrl Pts',(-0.93370211340225,-2.51582801973994,
12.5893111709658));
#438322=CARTESIAN_POINT('Ctrl Pts',(-0.934014800084356,-2.50449837448519,
12.5770542771492));
#438323=CARTESIAN_POINT('Ctrl Pts',(-0.950170633310224,-2.50189208830887,
12.5737548217797));
#438324=CARTESIAN_POINT('Ctrl Pts',(-0.933018372569254,-2.54060215157013,
12.5663937883685));
#438325=CARTESIAN_POINT('Ctrl Pts',(-0.933331458126653,-2.52925805377942,
12.5540940315304));
#438326=CARTESIAN_POINT('Ctrl Pts',(-0.949537866425113,-2.52664686145088,
12.5508374392248));
#438327=CARTESIAN_POINT('Ctrl Pts',(-0.932335321622376,-2.565351286605,
12.5434499600945));
#438328=CARTESIAN_POINT('Ctrl Pts',(-0.932649425132359,-2.55397030511269,
12.5311293540533));
#438329=CARTESIAN_POINT('Ctrl Pts',(-0.948904538284701,-2.55137741850342,
12.5278936106989));
#438330=CARTESIAN_POINT('Ctrl Pts',(-0.931652906521892,-2.59007738287778,
12.5204817579905));
#438331=CARTESIAN_POINT('Ctrl Pts',(-0.931968564629642,-2.57864007330484,
12.5081597038247));
#438332=CARTESIAN_POINT('Ctrl Pts',(-0.948270678662287,-2.5760856412816,
12.5049254088044));
#438333=CARTESIAN_POINT('Ctrl Pts',(-0.932143531606444,-2.57230045639142,
12.5369868989719));
#438334=CARTESIAN_POINT('Ctrl Pts',(-0.932117832969429,-2.5732316066214,
12.5342545179733));
#438335=CARTESIAN_POINT('Ctrl Pts',(-0.932218005951635,-2.57412369545498,
12.5314872231885));
#438336=CARTESIAN_POINT('Ctrl Pts',(-0.932493959424984,-2.57492023220284,
12.5287124745063));
#438337=CARTESIAN_POINT('Ctrl Pts',(-0.932742827964356,-2.5756385885786,
12.5262100684184));
#438338=CARTESIAN_POINT('Ctrl Pts',(-0.933135342868856,-2.57627818250249,
12.5237004536639));
#438339=CARTESIAN_POINT('Ctrl Pts',(-0.933734743370431,-2.57681532271708,
12.5212220730815));
#438340=CARTESIAN_POINT('Ctrl Pts',(-0.934193636306667,-2.5772265500177,
12.5193246583486));
#438341=CARTESIAN_POINT('Ctrl Pts',(-0.934779697513991,-2.57758216903345,
12.517417831369));
#438342=CARTESIAN_POINT('Ctrl Pts',(-0.935558777218661,-2.57781064117019,
12.5155812248348));
#438343=CARTESIAN_POINT('Ctrl Pts',(-0.935890669360424,-2.57790797152848,
12.5147988205793));
#438344=CARTESIAN_POINT('Ctrl Pts',(-0.93625784957137,-2.57798259183014,
12.5140295443047));
#438345=CARTESIAN_POINT('Ctrl Pts',(-0.936666065081868,-2.5780309948241,
12.5132817086137));
#438346=CARTESIAN_POINT('Ctrl Pts',(-0.937283844034861,-2.57810424620765,
12.5121499604604));
#438347=CARTESIAN_POINT('Ctrl Pts',(-0.938009787583041,-2.57811193267073,
12.5110494206568));
#438348=CARTESIAN_POINT('Ctrl Pts',(-0.938856251542312,-2.57801892256721,
12.5100666561695));
#438349=CARTESIAN_POINT('Ctrl Pts',(-0.939342289198491,-2.57796551637995,
12.5095023550641));
#438350=CARTESIAN_POINT('Ctrl Pts',(-0.939873607218879,-2.57787764433308,
12.5089719619137));
#438351=CARTESIAN_POINT('Ctrl Pts',(-0.940439204480263,-2.57775065210944,
12.5085043804652));
#438352=CARTESIAN_POINT('Ctrl Pts',(-0.941266882398073,-2.57756481553203,
12.5078201359221));
#438353=CARTESIAN_POINT('Ctrl Pts',(-0.9421917084627,-2.57728863667177,
12.5072563000949));
#438354=CARTESIAN_POINT('Ctrl Pts',(-0.943148570635696,-2.57693272436758,
12.5068768744332));
#438355=CARTESIAN_POINT('Ctrl Pts',(-0.943838534133043,-2.57667608709517,
12.5066032824114));
#438356=CARTESIAN_POINT('Ctrl Pts',(-0.944557297050483,-2.57637354075296,
12.5064197834844));
#438357=CARTESIAN_POINT('Ctrl Pts',(-0.945265724617955,-2.57604436271765,
12.5063282718343));
#438358=CARTESIAN_POINT('Ctrl Pts',(-0.946299809542831,-2.57556386469705,
12.5061946931565));
#438359=CARTESIAN_POINT('Ctrl Pts',(-0.947334422912381,-2.57501731583782,
12.5062515701262));
#438360=CARTESIAN_POINT('Ctrl Pts',(-0.948312578200474,-2.57445230977494,
12.5064436508398));
#438361=CARTESIAN_POINT('',(-0.950170633310224,-2.50189208830887,12.5737548217797));
#438362=CARTESIAN_POINT('Origin',(-0.955693739443566,-2.51643496624412,
12.5893111709658));
#438363=CARTESIAN_POINT('Ctrl Pts',(-0.948312578200474,-2.57445230977494,
12.5064436508398));
#438364=CARTESIAN_POINT('Ctrl Pts',(-0.948588098914043,-2.56371152413852,
12.5164271754438));
#438365=CARTESIAN_POINT('Ctrl Pts',(-0.948863519977009,-2.55296647549931,
12.5264061185523));
#438366=CARTESIAN_POINT('Ctrl Pts',(-0.949138838825944,-2.5422170137422,
12.536380305637));
#438367=CARTESIAN_POINT('Ctrl Pts',(-0.949482931546433,-2.52878236677158,
12.5488460165097));
#438368=CARTESIAN_POINT('Ctrl Pts',(-0.949826864686682,-2.51534082257244,
12.5613043021964));
#438369=CARTESIAN_POINT('Ctrl Pts',(-0.950170633310223,-2.50189208830887,
12.5737548217797));
#438370=CARTESIAN_POINT('Ctrl Pts',(-0.992933084929621,-2.49304515609577,
12.5893111709658));
#438371=CARTESIAN_POINT('Ctrl Pts',(-0.985108542234949,-2.48484545084625,
12.5770542771492));
#438372=CARTESIAN_POINT('Ctrl Pts',(-0.971370553186003,-2.49373765708239,
12.5737548217797));
#438373=CARTESIAN_POINT('Ctrl Pts',(-0.985632854649774,-2.48539490241525,
12.5928319619712));
#438374=CARTESIAN_POINT('Ctrl Pts',(-0.978017420927295,-2.482133217944,
12.5821634970843));
#438375=CARTESIAN_POINT('Ctrl Pts',(-0.96871808466295,-2.49094433860724,
12.5773203894503));
#438376=CARTESIAN_POINT('Ctrl Pts',(-0.970068171356415,-2.47920420509449,
12.5969440695591));
#438377=CARTESIAN_POINT('Ctrl Pts',(-0.966309852465797,-2.48063024214462,
12.5878292599214));
#438378=CARTESIAN_POINT('Ctrl Pts',(-0.963169757777886,-2.48873974887805,
12.5813877129824));
#438379=CARTESIAN_POINT('Ctrl Pts',(-0.941491577049632,-2.49013825756221,
12.596957478804));
#438380=CARTESIAN_POINT('Ctrl Pts',(-0.945222149392466,-2.48872283425317,
12.5878468778671));
#438381=CARTESIAN_POINT('Ctrl Pts',(-0.952943930223114,-2.49265876905205,
12.5814011370086));
#438382=CARTESIAN_POINT('Ctrl Pts',(-0.933994270954195,-2.50524221096691,
12.5928371701607));
#438383=CARTESIAN_POINT('Ctrl Pts',(-0.937463935307683,-2.49772579593194,
12.5821692192952));
#438384=CARTESIAN_POINT('Ctrl Pts',(-0.950267525571416,-2.49802894329946,
12.5773318885715));
#438385=CARTESIAN_POINT('Ctrl Pts',(-0.933702113402194,-2.51582801973994,
12.5893111709658));
#438386=CARTESIAN_POINT('Ctrl Pts',(-0.934014800084301,-2.50449837448519,
12.5770542771492));
#438387=CARTESIAN_POINT('Ctrl Pts',(-0.950170633310168,-2.50189208830886,
12.5737548217797));
#438388=CARTESIAN_POINT('',(-0.971370553186003,-2.49373765708239,12.5737548217797));
#438389=CARTESIAN_POINT('Origin',(-0.977016889193419,-2.50823313533222,
12.5893111709658));
#438390=CARTESIAN_POINT('Ctrl Pts',(-0.950170633310168,-2.50189208830886,
12.5737548217797));
#438391=CARTESIAN_POINT('Ctrl Pts',(-0.950165593066157,-2.50088994349549,
12.5746934679442));
#438392=CARTESIAN_POINT('Ctrl Pts',(-0.950343197672823,-2.49978008222401,
12.5756680099006));
#438393=CARTESIAN_POINT('Ctrl Pts',(-0.950679952599606,-2.49868824900081,
12.5765688348656));
#438394=CARTESIAN_POINT('Ctrl Pts',(-0.95076910473847,-2.49839919824197,
12.5768073183026));
#438395=CARTESIAN_POINT('Ctrl Pts',(-0.95086915448683,-2.49811139730721,
12.5770407398754));
#438396=CARTESIAN_POINT('Ctrl Pts',(-0.95097912913978,-2.4978270089836,
12.5772674179684));
#438397=CARTESIAN_POINT('Ctrl Pts',(-0.951430435377096,-2.49665995620531,
12.5781976435658));
#438398=CARTESIAN_POINT('Ctrl Pts',(-0.95208503672244,-2.49548815649485,
12.5790594849312));
#438399=CARTESIAN_POINT('Ctrl Pts',(-0.952940890682436,-2.49441428186397,
12.5797571720116));
#438400=CARTESIAN_POINT('Ctrl Pts',(-0.953498510311139,-2.49371461392887,
12.580211740231));
#438401=CARTESIAN_POINT('Ctrl Pts',(-0.954181583239703,-2.49303641900513,
12.5806009430798));
#438402=CARTESIAN_POINT('Ctrl Pts',(-0.954954506728614,-2.49244001147281,
12.5808812374708));
#438403=CARTESIAN_POINT('Ctrl Pts',(-0.955618704420289,-2.4919274995464,
12.5811221033394));
#438404=CARTESIAN_POINT('Ctrl Pts',(-0.956362919973353,-2.49146498147834,
12.581287365893));
#438405=CARTESIAN_POINT('Ctrl Pts',(-0.957149549864385,-2.49108564429589,
12.581359338449));
#438406=CARTESIAN_POINT('Ctrl Pts',(-0.95725887517595,-2.49103292426054,
12.5813693411482));
#438407=CARTESIAN_POINT('Ctrl Pts',(-0.957369013185351,-2.49098175136691,
12.5813775999465));
#438408=CARTESIAN_POINT('Ctrl Pts',(-0.957479857324108,-2.4909321536191,
12.5813841266931));
#438409=CARTESIAN_POINT('Ctrl Pts',(-0.957667917811834,-2.49084800504121,
12.5813952001081));
#438410=CARTESIAN_POINT('Ctrl Pts',(-0.957859519130497,-2.49076838274033,
12.5814007534795));
#438411=CARTESIAN_POINT('Ctrl Pts',(-0.958054653510005,-2.49069350350569,
12.5814005856065));
#438412=CARTESIAN_POINT('Ctrl Pts',(-0.958947902406796,-2.49035073564537,
12.5813998171494));
#438413=CARTESIAN_POINT('Ctrl Pts',(-0.95985334729205,-2.49013072391739,
12.58127954464));
#438414=CARTESIAN_POINT('Ctrl Pts',(-0.960758861092978,-2.49000596469546,
12.5810700125799));
#438415=CARTESIAN_POINT('Ctrl Pts',(-0.961852618663497,-2.48985526976033,
12.5808169217085));
#438416=CARTESIAN_POINT('Ctrl Pts',(-0.962948859924826,-2.48986011294288,
12.5804173076348));
#438417=CARTESIAN_POINT('Ctrl Pts',(-0.963951627200476,-2.48999402768643,
12.5799304713245));
#438418=CARTESIAN_POINT('Ctrl Pts',(-0.965194371759275,-2.49015999024118,
12.5793271277669));
#438419=CARTESIAN_POINT('Ctrl Pts',(-0.966374901528837,-2.49050257201474,
12.5785808224116));
#438420=CARTESIAN_POINT('Ctrl Pts',(-0.967452294259638,-2.49097687230634,
12.5777485681082));
#438421=CARTESIAN_POINT('Ctrl Pts',(-0.969057727465717,-2.49168363170431,
12.576508418016));
#438422=CARTESIAN_POINT('Ctrl Pts',(-0.970423403313072,-2.49267062156785,
12.5750928681475));
#438423=CARTESIAN_POINT('Ctrl Pts',(-0.971370553186003,-2.49373765708239,
12.5737548217797));
#438424=CARTESIAN_POINT('Ctrl Pts',(-0.971370553186003,-2.49373765708239,
12.5737548217797));
#438425=CARTESIAN_POINT('Ctrl Pts',(-0.985108542234949,-2.48484545084625,
12.5770542771492));
#438426=CARTESIAN_POINT('Ctrl Pts',(-0.992933084929622,-2.49304515609577,
12.5893111709658));
#438427=CARTESIAN_POINT('Ctrl Pts',(-0.988426831596606,-2.51168475492439,
12.5508408821982));
#438428=CARTESIAN_POINT('Ctrl Pts',(-1.00220563854764,-2.50276229990149,
12.55409748406));
#438429=CARTESIAN_POINT('Ctrl Pts',(-1.01004016335483,-2.51097246587486,
12.5663972313419));
#438430=CARTESIAN_POINT('Ctrl Pts',(-1.0054673031628,-2.52961350816027,
12.52790050457));
#438431=CARTESIAN_POINT('Ctrl Pts',(-1.01926998985148,-2.52064483392629,
12.5311362602938));
#438432=CARTESIAN_POINT('Ctrl Pts',(-1.02712998354897,-2.52888168994422,
12.5434568539655));
#438433=CARTESIAN_POINT('Ctrl Pts',(-1.02249320631727,-2.5475253328616,
12.5049357605811));
#438434=CARTESIAN_POINT('Ctrl Pts',(-1.03630500964622,-2.53849663008702,
12.5081700652078));
#438435=CARTESIAN_POINT('Ctrl Pts',(-1.04420389718021,-2.54677424478032,
12.5204921097672));
#438436=CARTESIAN_POINT('Ctrl Pts',(-1.02137521992701,-2.54634917114605,
12.5064436508395));
#438437=CARTESIAN_POINT('Ctrl Pts',(-1.02256844577703,-2.54609410279946,
12.5062361689309));
#438438=CARTESIAN_POINT('Ctrl Pts',(-1.02379842633536,-2.5457779707913,
12.5061871075061));
#438439=CARTESIAN_POINT('Ctrl Pts',(-1.02496988580871,-2.54540554718385,
12.5063648335164));
#438440=CARTESIAN_POINT('Ctrl Pts',(-1.02550203496013,-2.5452363694093,
12.5064455676329));
#438441=CARTESIAN_POINT('Ctrl Pts',(-1.02602946369528,-2.54505300601871,
12.506574497099));
#438442=CARTESIAN_POINT('Ctrl Pts',(-1.02652921234473,-2.54486232641351,
12.5067492519495));
#438443=CARTESIAN_POINT('Ctrl Pts',(-1.02753347665467,-2.54447914834519,
12.5071004286051));
#438444=CARTESIAN_POINT('Ctrl Pts',(-1.028462597074,-2.54405158242217,12.5076537929613));
#438445=CARTESIAN_POINT('Ctrl Pts',(-1.02925079228227,-2.54362031201972,
12.5083435010505));
#438446=CARTESIAN_POINT('Ctrl Pts',(-1.02930041388091,-2.5435931609706,
12.5083869222964));
#438447=CARTESIAN_POINT('Ctrl Pts',(-1.02934947661137,-2.54356598180801,
12.5084308732337));
#438448=CARTESIAN_POINT('Ctrl Pts',(-1.02939796432575,-2.54353877920501,
12.5084753333615));
#438449=CARTESIAN_POINT('Ctrl Pts',(-1.02978689979309,-2.54332057842475,
12.5088319622689));
#438450=CARTESIAN_POINT('Ctrl Pts',(-1.03014736506458,-2.5430975647324,
12.509227847131));
#438451=CARTESIAN_POINT('Ctrl Pts',(-1.03047011482179,-2.54287875066362,
12.5096423454524));
#438452=CARTESIAN_POINT('Ctrl Pts',(-1.03148146971781,-2.54219308421511,
12.5109411997424));
#438453=CARTESIAN_POINT('Ctrl Pts',(-1.03219011954864,-2.54151448454895,
12.5124831113042));
#438454=CARTESIAN_POINT('Ctrl Pts',(-1.03268346387674,-2.54087924455539,
12.5140723025008));
#438455=CARTESIAN_POINT('Ctrl Pts',(-1.03272969078062,-2.54081972187223,
12.5142212114565));
#438456=CARTESIAN_POINT('Ctrl Pts',(-1.03277405691508,-2.54076058089929,
12.5143705582413));
#438457=CARTESIAN_POINT('Ctrl Pts',(-1.03281665103131,-2.54070185362042,
12.5145201959299));
#438458=CARTESIAN_POINT('Ctrl Pts',(-1.03336383587027,-2.53994741428748,
12.5164425148273));
#438459=CARTESIAN_POINT('Ctrl Pts',(-1.0336460216623,-2.53924170261964,
12.518463520594));
#438460=CARTESIAN_POINT('Ctrl Pts',(-1.03375236064752,-2.53857093976959,
12.5205025929157));
#438461=CARTESIAN_POINT('Ctrl Pts',(-1.03381404147384,-2.53818187073,12.5216853356836));
#438462=CARTESIAN_POINT('Ctrl Pts',(-1.03381692551923,-2.53780533861075,
12.5228750347131));
#438463=CARTESIAN_POINT('Ctrl Pts',(-1.03377897508456,-2.53744455112058,
12.5240609649613));
#438464=CARTESIAN_POINT('Ctrl Pts',(-1.03368582777863,-2.53655901758155,
12.5269717671327));
#438465=CARTESIAN_POINT('Ctrl Pts',(-1.03333372079274,-2.53574449952855,
12.5299036066169));
#438466=CARTESIAN_POINT('Ctrl Pts',(-1.03280669127657,-2.53497984796395,
12.532813300402));
#438467=CARTESIAN_POINT('Ctrl Pts',(-1.0325536864208,-2.53461277068862,
12.5342101228452));
#438468=CARTESIAN_POINT('Ctrl Pts',(-1.03226025380202,-2.53425794086336,
12.5356023438238));
#438469=CARTESIAN_POINT('Ctrl Pts',(-1.03193439359517,-2.53391645655153,
12.5369868989719));
#438470=CARTESIAN_POINT('Origin',(-9.8341648617864,-11.7505157552943,-1.23926451155288));
#438471=CARTESIAN_POINT('Ctrl Pts',(-0.932144644962174,-2.57225867695425,
12.5369868989719));
#438472=CARTESIAN_POINT('Ctrl Pts',(-0.931750596423733,-2.58759256196211,
12.5369868989719));
#438473=CARTESIAN_POINT('Ctrl Pts',(-0.917226339900628,-2.5925250335673,
12.5369868989719));
#438474=CARTESIAN_POINT('Ctrl Pts',(-0.93201137495496,-2.57744212809063,
12.5218025310015));
#438475=CARTESIAN_POINT('Ctrl Pts',(-0.928404515129539,-2.58869585751265,
12.5216901060417));
#438476=CARTESIAN_POINT('Ctrl Pts',(-0.917270619951127,-2.59251001337502,
12.5161920673678));
#438477=CARTESIAN_POINT('Ctrl Pts',(-0.936815527993009,-2.58108303248129,
12.5042015548895));
#438478=CARTESIAN_POINT('Ctrl Pts',(-0.93374825857915,-2.58673716401142,
12.4980677368514));
#438479=CARTESIAN_POINT('Ctrl Pts',(-0.927353550901787,-2.58903900967191,
12.4907278922777));
#438480=CARTESIAN_POINT('Ctrl Pts',(-0.948305664819111,-2.57443354149153,
12.506463626192));
#438481=CARTESIAN_POINT('Ctrl Pts',(-0.950567168226204,-2.58057300732139,
12.4999376786891));
#438482=CARTESIAN_POINT('Ctrl Pts',(-0.95053954725031,-2.58049802267305,
12.4906970594712));
#438483=CARTESIAN_POINT('Origin',(-0.910151905565128,-2.57169350988724,
12.5369868989719));
#438484=CARTESIAN_POINT('Origin',(-0.910151905565129,-2.57169350988724,
14.));
#438485=CARTESIAN_POINT('Origin',(-0.910151905565129,-2.57169350988724,
13.7435492065112));
#438486=CARTESIAN_POINT('Ctrl Pts',(-0.932826598035787,-2.54754977621595,
13.793642941384));
#438487=CARTESIAN_POINT('Ctrl Pts',(-0.932555515117465,-2.55835869535974,
13.8071662555867));
#438488=CARTESIAN_POINT('Ctrl Pts',(-0.915653148372656,-2.56043941207733,
13.8103758687955));
#438489=CARTESIAN_POINT('Ctrl Pts',(-0.932368049551305,-2.56416457198688,
13.7804579775006));
#438490=CARTESIAN_POINT('Ctrl Pts',(-0.93202342011753,-2.57750154699185,
13.7901904343352));
#438491=CARTESIAN_POINT('Ctrl Pts',(-0.916902832686253,-2.58193141831023,
13.7927914348263));
#438492=CARTESIAN_POINT('Ctrl Pts',(-0.932098084763358,-2.57394632754132,
13.7597120340895));
#438493=CARTESIAN_POINT('Ctrl Pts',(-0.931693522970168,-2.58938081553827,
13.7635825532445));
#438494=CARTESIAN_POINT('Ctrl Pts',(-0.917614250794026,-2.59460671365573,
13.7651073818884));
#438495=CARTESIAN_POINT('Ctrl Pts',(-0.932150950049518,-2.572030835827,
13.7381884353898));
#438496=CARTESIAN_POINT('Ctrl Pts',(-0.931756756302547,-2.58710407442778,
13.7368803041982));
#438497=CARTESIAN_POINT('Ctrl Pts',(-0.917474440534505,-2.59212454187823,
13.7363986145813));
#438498=CARTESIAN_POINT('Origin',(-0.910723732443341,-2.55097438096993,
13.7902182540695));
#438499=CARTESIAN_POINT('Ctrl Pts',(-0.933702221237335,-2.51582408501885,
13.8235227101244));
#438500=CARTESIAN_POINT('Ctrl Pts',(-0.93338946625715,-2.52731690332603,
13.8358800583119));
#438501=CARTESIAN_POINT('Ctrl Pts',(-0.917011786918914,-2.52984626461901,
13.8390832900376));
#438502=CARTESIAN_POINT('Ctrl Pts',(-0.933373157481985,-2.52774712432683,
13.8124254819052));
#438503=CARTESIAN_POINT('Ctrl Pts',(-0.933059794858003,-2.53926226151667,
13.8247886449157));
#438504=CARTESIAN_POINT('Ctrl Pts',(-0.916658820164166,-2.541777974178,
13.8279860620657));
#438505=CARTESIAN_POINT('Ctrl Pts',(-0.933044241202318,-2.53966482011645,
13.8013225099955));
#438506=CARTESIAN_POINT('Ctrl Pts',(-0.932730420795263,-2.5511968429479,
13.8136962257787));
#438507=CARTESIAN_POINT('Ctrl Pts',(-0.916306287753314,-2.5537041679572,
13.8168830918626));
#438508=CARTESIAN_POINT('Ctrl Pts',(-0.932715466660279,-2.55157738029588,
13.7902140179785));
#438509=CARTESIAN_POINT('Ctrl Pts',(-0.932401328533452,-2.56312121062995,
13.802602731458));
#438510=CARTESIAN_POINT('Ctrl Pts',(-0.915954174459412,-2.5656250627394,
13.8057746032558));
#438511=CARTESIAN_POINT('Origin',(-0.911710487360935,-2.51522107323576,
13.8235269408515));
#438512=CARTESIAN_POINT('Ctrl Pts',(-0.992933084929622,-2.49304515609577,
13.8235269408515));
#438513=CARTESIAN_POINT('Ctrl Pts',(-1.00108452963338,-2.50158743729183,
13.8362179249168));
#438514=CARTESIAN_POINT('Ctrl Pts',(-1.01518422374936,-2.4919509633572,
13.8391868794938));
#438515=CARTESIAN_POINT('Ctrl Pts',(-0.985474867836949,-2.48522934062473,
13.8400110824519));
#438516=CARTESIAN_POINT('Ctrl Pts',(-0.99448529996465,-2.48971643052063,
13.8494522556837));
#438517=CARTESIAN_POINT('Ctrl Pts',(-1.00282881780928,-2.47916590459,13.85569149686));
#438518=CARTESIAN_POINT('Ctrl Pts',(-0.970388930739011,-2.47908017580974,
13.8586819406588));
#438519=CARTESIAN_POINT('Ctrl Pts',(-0.974457513909136,-2.47753011948085,
13.868010383617));
#438520=CARTESIAN_POINT('Ctrl Pts',(-0.977730753849783,-2.46909336850175,
13.8744918421245));
#438521=CARTESIAN_POINT('Ctrl Pts',(-0.941165836185502,-2.4902641930962,
13.8587686893867));
#438522=CARTESIAN_POINT('Ctrl Pts',(-0.937133443320806,-2.49180040131925,
13.8680909899357));
#438523=CARTESIAN_POINT('Ctrl Pts',(-0.929083802866002,-2.48771387589363,
13.8745789365163));
#438524=CARTESIAN_POINT('Ctrl Pts',(-0.934000645860243,-2.50501122735948,
13.8400379222776));
#438525=CARTESIAN_POINT('Ctrl Pts',(-0.93031405348387,-2.51437494833773,
13.8494748685453));
#438526=CARTESIAN_POINT('Ctrl Pts',(-0.917056800502737,-2.51213746120722,
13.8557104837033));
#438527=CARTESIAN_POINT('Ctrl Pts',(-0.933702113395648,-2.51582801973962,
13.8235269408542));
#438528=CARTESIAN_POINT('Ctrl Pts',(-0.933376362959024,-2.52763100688032,
13.8362179249195));
#438529=CARTESIAN_POINT('Ctrl Pts',(-0.916453295841902,-2.52992726544712,
13.8391868794965));
#438530=CARTESIAN_POINT('Origin',(-1.00884928066582,-2.47785717685932,13.8235269408515));
#438531=CARTESIAN_POINT('Ctrl Pts',(-1.01762251193398,-2.51891836345134,
13.7902140241682));
#438532=CARTESIAN_POINT('Ctrl Pts',(-1.02559166761428,-2.52727606368141,
13.8026027327198));
#438533=CARTESIAN_POINT('Ctrl Pts',(-1.03947723417935,-2.51811260508543,
13.8057746032556));
#438534=CARTESIAN_POINT('Ctrl Pts',(-1.00939539328456,-2.51029677998016,
13.8013225161808));
#438535=CARTESIAN_POINT('Ctrl Pts',(-1.01735640044902,-2.51864592920702,
13.8136962270464));
#438536=CARTESIAN_POINT('Ctrl Pts',(-1.0312272073581,-2.50950047563681,
13.8168830918628));
#438537=CARTESIAN_POINT('Ctrl Pts',(-1.00116472785025,-2.50167147966678,
13.8124254880875));
#438538=CARTESIAN_POINT('Ctrl Pts',(-1.00911407947467,-2.51000840258784,
13.8247886461867));
#438539=CARTESIAN_POINT('Ctrl Pts',(-1.02297331838114,-2.50088469395972,
13.8279860620656));
#438540=CARTESIAN_POINT('Ctrl Pts',(-0.99293037204333,-2.49304231203889,
13.8235227163065));
#438541=CARTESIAN_POINT('Ctrl Pts',(-1.00086431586339,-2.50136307634855,
13.8358800595848));
#438542=CARTESIAN_POINT('Ctrl Pts',(-1.01471541067069,-2.49226510935382,
13.8390832900376));
#438543=CARTESIAN_POINT('Origin',(-1.03354142914456,-2.50373323727634,13.7902182540695));
#438544=CARTESIAN_POINT('Ctrl Pts',(-1.03174811234297,-2.53372120373454,
13.7382347919292));
#438545=CARTESIAN_POINT('Ctrl Pts',(-1.04214853229672,-2.54465505637297,
13.7369371795943));
#438546=CARTESIAN_POINT('Ctrl Pts',(-1.05612135761036,-2.53879810069833,
13.7364597369711));
#438547=CARTESIAN_POINT('Ctrl Pts',(-1.03305397354885,-2.53508967751775,
13.7595490285573));
#438548=CARTESIAN_POINT('Ctrl Pts',(-1.04370326709854,-2.54628370955771,
13.7633824266925));
#438549=CARTESIAN_POINT('Ctrl Pts',(-1.05766159127508,-2.54071066312963,
13.7648920890506));
#438550=CARTESIAN_POINT('Ctrl Pts',(-1.02639415293407,-2.52811053620009,
13.7803806590111));
#438551=CARTESIAN_POINT('Ctrl Pts',(-1.03560149942692,-2.53779669418791,
13.7901039518745));
#438552=CARTESIAN_POINT('Ctrl Pts',(-1.04980642019989,-2.53096253972233,
13.7926933640892));
#438553=CARTESIAN_POINT('Ctrl Pts',(-1.01481789810246,-2.51597923059652,
13.7936647693663));
#438554=CARTESIAN_POINT('Ctrl Pts',(-1.02226274774007,-2.52382445499216,
13.8072068914932));
#438555=CARTESIAN_POINT('Ctrl Pts',(-1.03621157730066,-2.51402269883642,
13.8104111085397));
#438556=CARTESIAN_POINT('Origin',(-1.04785058933137,-2.51872847731507,13.7435492065112));
#438557=CARTESIAN_POINT('Origin',(-1.04785058933137,-2.51872847731508,14.));
#438558=CARTESIAN_POINT('Origin',(-1.04785058933137,-2.51872847731508,12.5369868989719));
#438559=CARTESIAN_POINT('Ctrl Pts',(-1.02136837617885,-2.54633210930254,
12.506462012331));
#438560=CARTESIAN_POINT('Ctrl Pts',(-1.0238025843525,-2.55240073505779,
12.4999388158272));
#438561=CARTESIAN_POINT('Ctrl Pts',(-1.02377378447754,-2.55232893525659,
12.4907030323752));
#438562=CARTESIAN_POINT('Ctrl Pts',(-1.03435204063999,-2.54356569640584,
12.5042014951932));
#438563=CARTESIAN_POINT('Ctrl Pts',(-1.04041476061465,-2.54570684647648,
12.4980716682127));
#438564=CARTESIAN_POINT('Ctrl Pts',(-1.04669984494285,-2.54313327304381,
12.4907355092743));
#438565=CARTESIAN_POINT('Ctrl Pts',(-1.03548007527325,-2.53764511880636,
12.5218047446509));
#438566=CARTESIAN_POINT('Ctrl Pts',(-1.04569434302523,-2.54357703293483,
12.5216906929434));
#438567=CARTESIAN_POINT('Ctrl Pts',(-1.05651029175862,-2.53895253216972,
12.5161988840776));
#438568=CARTESIAN_POINT('Ctrl Pts',(-1.03190789680994,-2.53388864074319,
12.5369868989719));
#438569=CARTESIAN_POINT('Ctrl Pts',(-1.04247169861751,-2.5449977191429,
12.5369868989719));
#438570=CARTESIAN_POINT('Ctrl Pts',(-1.05655165994204,-2.53893469839246,
12.5369868989719));
#438571=CARTESIAN_POINT('Origin',(-1.84953258308752E-31,-9.96028411833586E-31,
12.5));
#438572=CARTESIAN_POINT('Origin',(-0.786422857476889,-2.5656830183634,12.5));
#438573=CARTESIAN_POINT('',(-0.786422857476889,-2.5656830183634,12.5893111709658));
#438574=CARTESIAN_POINT('',(-0.786422857476889,-2.5656830183634,13.8235269408515));
#438575=CARTESIAN_POINT('',(-0.786422857476889,-2.5656830183634,12.5));
#438576=CARTESIAN_POINT('',(-0.808923705722909,-2.59348561765575,13.7902182540695));
#438577=CARTESIAN_POINT('',(-0.786422857476889,-2.5656830183634,13.8235269408515));
#438578=CARTESIAN_POINT('',(-0.821963002087443,-2.60959729166526,13.7435492065112));
#438579=CARTESIAN_POINT('Origin',(-0.779063636183257,-2.55659030206942,
13.7445212918697));
#438580=CARTESIAN_POINT('',(-0.821963002087443,-2.60959729166526,12.5369868989719));
#438581=CARTESIAN_POINT('',(-0.821963002087443,-2.60959729166526,12.5));
#438582=CARTESIAN_POINT('Ctrl Pts',(-0.821963002087443,-2.60959729166526,
12.5369868989719));
#438583=CARTESIAN_POINT('Ctrl Pts',(-0.810124927490551,-2.59496987669798,
12.5544431401645));
#438584=CARTESIAN_POINT('Ctrl Pts',(-0.79827838598807,-2.58033199981474,
12.5718848856037));
#438585=CARTESIAN_POINT('Ctrl Pts',(-0.786422857476889,-2.5656830183634,
12.5893111709658));
#438586=CARTESIAN_POINT('Origin',(-0.695563849448027,-2.85692443666948,
12.5));
#438587=CARTESIAN_POINT('',(-0.719375533633202,-2.6397196902469,13.7435492065112));
#438588=CARTESIAN_POINT('',(-0.72163425915842,-2.61911611172101,13.7902182540695));
#438589=CARTESIAN_POINT('Origin',(-0.727569799452577,-2.56497346836795,
13.7418732680442));
#438590=CARTESIAN_POINT('',(-0.725531957228276,-2.58356219985526,13.8235269408515));
#438591=CARTESIAN_POINT('',(-0.72163425915842,-2.61911611172101,13.7902182540695));
#438592=CARTESIAN_POINT('',(-0.725531957228276,-2.58356219985526,12.5893111709658));
#438593=CARTESIAN_POINT('',(-0.725531957228276,-2.58356219985526,12.5));
#438594=CARTESIAN_POINT('',(-0.719375533633202,-2.6397196902469,12.5369868989719));
#438595=CARTESIAN_POINT('Ctrl Pts',(-0.725531957228276,-2.58356219985526,
12.5893111709658));
#438596=CARTESIAN_POINT('Ctrl Pts',(-0.723478289291409,-2.60229528987923,
12.5718848856037));
#438597=CARTESIAN_POINT('Ctrl Pts',(-0.721426178124584,-2.62101417940233,
12.5544431401645));
#438598=CARTESIAN_POINT('Ctrl Pts',(-0.719375533633202,-2.6397196902469,
12.5369868989719));
#438599=CARTESIAN_POINT('',(-0.719375533633202,-2.6397196902469,12.5));
#438600=CARTESIAN_POINT('Origin',(-0.759702236830053,-2.58730821332779,
12.5));
#438601=CARTESIAN_POINT('',(-0.75109722107967,-2.55402843153593,13.8587068136939));
#438602=CARTESIAN_POINT('Ctrl Pts',(-0.725531957221722,-2.5835621998544,
13.8235269408542));
#438603=CARTESIAN_POINT('Ctrl Pts',(-0.7257229138222,-2.58182033734436,
13.8262006681044));
#438604=CARTESIAN_POINT('Ctrl Pts',(-0.726091034629165,-2.58005672879837,
13.8288634856214));
#438605=CARTESIAN_POINT('Ctrl Pts',(-0.726623342150079,-2.57827443864714,
13.8314912288862));
#438606=CARTESIAN_POINT('Ctrl Pts',(-0.727172096299167,-2.57643708133592,
13.8342001611531));
#438607=CARTESIAN_POINT('Ctrl Pts',(-0.727895473031266,-2.57457768713431,
13.8368750301949));
#438608=CARTESIAN_POINT('Ctrl Pts',(-0.728823876636812,-2.57269240310717,
13.8394886372969));
#438609=CARTESIAN_POINT('Ctrl Pts',(-0.728895579499261,-2.57254679804869,
13.8396904925131));
#438610=CARTESIAN_POINT('Ctrl Pts',(-0.728968526574237,-2.57240104477644,
13.8398919674349));
#438611=CARTESIAN_POINT('Ctrl Pts',(-0.729042742528137,-2.57225514567896,
13.8400930404591));
#438612=CARTESIAN_POINT('Ctrl Pts',(-0.730199077019948,-2.56998193958415,
13.8432258934518));
#438613=CARTESIAN_POINT('Ctrl Pts',(-0.731656537689533,-2.56768442238517,
13.8462331177034));
#438614=CARTESIAN_POINT('Ctrl Pts',(-0.733449048631665,-2.56548920109201,
13.8489036603661));
#438615=CARTESIAN_POINT('Ctrl Pts',(-0.734035579072432,-2.56477089913782,
13.849777493004));
#438616=CARTESIAN_POINT('Ctrl Pts',(-0.734657956282971,-2.56406379830743,
13.85061494757));
#438617=CARTESIAN_POINT('Ctrl Pts',(-0.735317282009905,-2.56337304269841,
13.8514076489583));
#438618=CARTESIAN_POINT('Ctrl Pts',(-0.736711851011371,-2.56191199496346,
13.8530843267192));
#438619=CARTESIAN_POINT('Ctrl Pts',(-0.738410844657664,-2.56038260204569,
13.8546805203176));
#438620=CARTESIAN_POINT('Ctrl Pts',(-0.740406941182383,-2.55897503979074,
13.8559412814273));
#438621=CARTESIAN_POINT('Ctrl Pts',(-0.740674083632336,-2.55878666231271,
13.8561100121513));
#438622=CARTESIAN_POINT('Ctrl Pts',(-0.740946473126565,-2.55860044782226,
13.8562727473908));
#438623=CARTESIAN_POINT('Ctrl Pts',(-0.741224021597772,-2.55841682425119,
13.8564289040185));
#438624=CARTESIAN_POINT('Ctrl Pts',(-0.742482700748308,-2.55758409345124,
13.8571370725437));
#438625=CARTESIAN_POINT('Ctrl Pts',(-0.743870860165083,-2.55679190927231,
13.8577210840554));
#438626=CARTESIAN_POINT('Ctrl Pts',(-0.74534908801759,-2.55609655359047,
13.8581177131616));
#438627=CARTESIAN_POINT('Ctrl Pts',(-0.74576540785991,-2.55590071749705,
13.8582294175695));
#438628=CARTESIAN_POINT('Ctrl Pts',(-0.746188766120969,-2.55571241884951,
13.8583265086086));
#438629=CARTESIAN_POINT('Ctrl Pts',(-0.746618042534046,-2.55553254653241,
13.8584082369006));
#438630=CARTESIAN_POINT('Ctrl Pts',(-0.747234797624621,-2.55527411824739,
13.8585256585398));
#438631=CARTESIAN_POINT('Ctrl Pts',(-0.747871561632547,-2.55503016893092,
13.8586122832068));
#438632=CARTESIAN_POINT('Ctrl Pts',(-0.748512075786855,-2.55480777310193,
13.8586682984299));
#438633=CARTESIAN_POINT('Ctrl Pts',(-0.749024423618175,-2.55462987848412,
13.8587131050557));
#438634=CARTESIAN_POINT('Ctrl Pts',(-0.749544752922616,-2.55446358832294,
13.8587357943552));
#438635=CARTESIAN_POINT('Ctrl Pts',(-0.750073279700978,-2.55430936526782,
13.8587355499465));
#438636=CARTESIAN_POINT('Ctrl Pts',(-0.750414879158553,-2.55420968723043,
13.8587353919793));
#438637=CARTESIAN_POINT('Ctrl Pts',(-0.750756198140403,-2.55411609082041,
13.8587257282814));
#438638=CARTESIAN_POINT('Ctrl Pts',(-0.75109722107967,-2.55402843153593,
13.8587068136939));
#438639=CARTESIAN_POINT('Ctrl Pts',(-0.75109722107967,-2.55402843153593,
13.8587068136939));
#438640=CARTESIAN_POINT('Ctrl Pts',(-0.752218826935593,-2.55374012492815,
13.8586446046466));
#438641=CARTESIAN_POINT('Ctrl Pts',(-0.753337235143209,-2.55351596180143,
13.858482427929));
#438642=CARTESIAN_POINT('Ctrl Pts',(-0.754451869443705,-2.55335150888579,
13.8582284286032));
#438643=CARTESIAN_POINT('Ctrl Pts',(-0.755595354576482,-2.55318279932427,
13.8579678548414));
#438644=CARTESIAN_POINT('Ctrl Pts',(-0.756737884691099,-2.55307803415227,
13.857615680862));
#438645=CARTESIAN_POINT('Ctrl Pts',(-0.75783353159653,-2.5530316944702,
13.8571944833187));
#438646=CARTESIAN_POINT('Ctrl Pts',(-0.760567830502609,-2.55291604905436,
13.8561433417727));
#438647=CARTESIAN_POINT('Ctrl Pts',(-0.763137838651283,-2.55315407872345,
13.8546163505474));
#438648=CARTESIAN_POINT('Ctrl Pts',(-0.76542262856099,-2.55357805032377,
13.8528973491086));
#438649=CARTESIAN_POINT('Ctrl Pts',(-0.765840025968559,-2.55365550368003,
13.8525833129072));
#438650=CARTESIAN_POINT('Ctrl Pts',(-0.766247991588314,-2.55373905131416,
13.8522628768812));
#438651=CARTESIAN_POINT('Ctrl Pts',(-0.766645918937218,-2.55382754864833,
13.851937733538));
#438652=CARTESIAN_POINT('Ctrl Pts',(-0.769076006047064,-2.55436798958969,
13.8499521282529));
#438653=CARTESIAN_POINT('Ctrl Pts',(-0.771372347937259,-2.55515071408284,
13.847639871647));
#438654=CARTESIAN_POINT('Ctrl Pts',(-0.773440177674622,-2.55605854052776,
13.8452109780794));
#438655=CARTESIAN_POINT('Ctrl Pts',(-0.774370537075405,-2.5564669904364,
13.8441181685877));
#438656=CARTESIAN_POINT('Ctrl Pts',(-0.775255137099046,-2.55690024768248,
13.8430021611332));
#438657=CARTESIAN_POINT('Ctrl Pts',(-0.776088267135618,-2.55734608452085,
13.8418824960098));
#438658=CARTESIAN_POINT('Ctrl Pts',(-0.778051559341545,-2.5583967104153,
13.8392439765549));
#438659=CARTESIAN_POINT('Ctrl Pts',(-0.779824666035133,-2.55956408302726,
13.8364981347964));
#438660=CARTESIAN_POINT('Ctrl Pts',(-0.781431094187344,-2.56082270752436,
13.8336931113419));
#438661=CARTESIAN_POINT('Ctrl Pts',(-0.782995653189977,-2.56204852785448,
13.8309611966328));
#438662=CARTESIAN_POINT('Ctrl Pts',(-0.784403328595506,-2.56336257803986,
13.8281701127185));
#438663=CARTESIAN_POINT('Ctrl Pts',(-0.785642005203312,-2.56476130297386,
13.825358068512));
#438664=CARTESIAN_POINT('Ctrl Pts',(-0.785910551628698,-2.56506454804909,
13.8247484142932));
#438665=CARTESIAN_POINT('Ctrl Pts',(-0.786170983011782,-2.56537179610419,
13.8241378483365));
#438666=CARTESIAN_POINT('Ctrl Pts',(-0.786422857476889,-2.5656830183634,
13.8235269408515));
#438667=CARTESIAN_POINT('',(-0.749900486153921,-2.55436100089082,12.5969504640361));
#438668=CARTESIAN_POINT('Origin',(-0.759711745942211,-2.58733990338295,
12.584524458991));
#438669=CARTESIAN_POINT('Origin',(-0.759711745942211,-2.58733990338295,
12.584524458991));
#438670=CARTESIAN_POINT('Ctrl Pts',(-0.725531957228276,-2.58356219985526,
12.5893111709658));
#438671=CARTESIAN_POINT('Ctrl Pts',(-0.726767074738799,-2.57229573992789,
12.5770542771492));
#438672=CARTESIAN_POINT('Ctrl Pts',(-0.743081587281321,-2.57101497634516,
12.5737548217797));
#438673=CARTESIAN_POINT('Ctrl Pts',(-0.722831169750517,-2.60819816658008,
12.5663937883685));
#438674=CARTESIAN_POINT('Ctrl Pts',(-0.724067862824956,-2.59691733471841,
12.5540940315304));
#438675=CARTESIAN_POINT('Ctrl Pts',(-0.740433182052644,-2.59563580364621,
12.5508374392248));
#438676=CARTESIAN_POINT('Ctrl Pts',(-0.720133107334208,-2.63280927591654,
12.5434499600945));
#438677=CARTESIAN_POINT('Ctrl Pts',(-0.72137382133825,-2.62149176605326,
12.5311293540533));
#438678=CARTESIAN_POINT('Ctrl Pts',(-0.737786191272279,-2.62023244968732,
12.5278936106989));
#438679=CARTESIAN_POINT('Ctrl Pts',(-0.717437556521574,-2.65739747497773,
12.5204817579905));
#438680=CARTESIAN_POINT('Ctrl Pts',(-0.718684411212006,-2.6460239511751,
12.5081597038247));
#438681=CARTESIAN_POINT('Ctrl Pts',(-0.735140491229121,-2.64480679244879,
12.5049254088044));
#438682=CARTESIAN_POINT('Ctrl Pts',(-0.719375533633203,-2.6397196902469,
12.5369868989719));
#438683=CARTESIAN_POINT('Ctrl Pts',(-0.719274023118167,-2.64064564747381,
12.5342545179733));
#438684=CARTESIAN_POINT('Ctrl Pts',(-0.719301149261355,-2.64154293298339,
12.5314872231885));
#438685=CARTESIAN_POINT('Ctrl Pts',(-0.719511259382647,-2.64235931209083,
12.5287124745063));
#438686=CARTESIAN_POINT('Ctrl Pts',(-0.719700747118965,-2.64309556329136,
12.5262100684184));
#438687=CARTESIAN_POINT('Ctrl Pts',(-0.720039823120004,-2.64376502262788,
12.5237004536639));
#438688=CARTESIAN_POINT('Ctrl Pts',(-0.720593447251803,-2.64434923225817,
12.5212220730815));
#438689=CARTESIAN_POINT('Ctrl Pts',(-0.721017294417001,-2.64479649526832,
12.5193246583486));
#438690=CARTESIAN_POINT('Ctrl Pts',(-0.721572419302811,-2.64519870042026,
12.517417831369));
#438691=CARTESIAN_POINT('Ctrl Pts',(-0.722330284083855,-2.64548991456336,
12.5155812248348));
#438692=CARTESIAN_POINT('Ctrl Pts',(-0.722653138554123,-2.64561397335361,
12.5147988205793));
#438693=CARTESIAN_POINT('Ctrl Pts',(-0.723013014755882,-2.6457182739583,
12.5140295443047));
#438694=CARTESIAN_POINT('Ctrl Pts',(-0.723415926669586,-2.64579978924908,
12.5132817086137));
#438695=CARTESIAN_POINT('Ctrl Pts',(-0.724025679346283,-2.64592315161454,
12.5121499604604));
#438696=CARTESIAN_POINT('Ctrl Pts',(-0.724748580859092,-2.64598998364006,
12.5110494206568));
#438697=CARTESIAN_POINT('Ctrl Pts',(-0.725599809466267,-2.64596627769085,
12.5100666561695));
#438698=CARTESIAN_POINT('Ctrl Pts',(-0.726088582972301,-2.64595266578941,
12.5095023550641));
#438699=CARTESIAN_POINT('Ctrl Pts',(-0.726625295463391,-2.64590839348071,
12.5089719619137));
#438700=CARTESIAN_POINT('Ctrl Pts',(-0.727199361791711,-2.64582792524076,
12.5085043804652));
#438701=CARTESIAN_POINT('Ctrl Pts',(-0.72803943308581,-2.64571017045333,
12.5078201359221));
#438702=CARTESIAN_POINT('Ctrl Pts',(-0.728983693009031,-2.64551029246537,
12.5072563000949));
#438703=CARTESIAN_POINT('Ctrl Pts',(-0.729966381459002,-2.64523355758019,
12.5068768744332));
#438704=CARTESIAN_POINT('Ctrl Pts',(-0.730674967479934,-2.64503401267748,
12.5066032824114));
#438705=CARTESIAN_POINT('Ctrl Pts',(-0.731415999108655,-2.64479105888369,
12.5064197834844));
#438706=CARTESIAN_POINT('Ctrl Pts',(-0.732148900507654,-2.64452071958462,
12.5063282718343));
#438707=CARTESIAN_POINT('Ctrl Pts',(-0.733218709649654,-2.64412610790289,
12.5061946931565));
#438708=CARTESIAN_POINT('Ctrl Pts',(-0.734294429234505,-2.64366570823441,
12.5062515701262));
#438709=CARTESIAN_POINT('Ctrl Pts',(-0.735315383030953,-2.64318231091932,
12.5064436508398));
#438710=CARTESIAN_POINT('',(-0.743081587281321,-2.57101497634516,12.5737548217797));
#438711=CARTESIAN_POINT('Origin',(-0.747400936173413,-2.58595964847768,
12.5893111709658));
#438712=CARTESIAN_POINT('Ctrl Pts',(-0.735315383030953,-2.64318231091932,
12.5064436508398));
#438713=CARTESIAN_POINT('Ctrl Pts',(-0.736465460714024,-2.63249972185702,
12.5164271754438));
#438714=CARTESIAN_POINT('Ctrl Pts',(-0.737615786552383,-2.62181287585427,
12.5264061185523));
#438715=CARTESIAN_POINT('Ctrl Pts',(-0.7387663702269,-2.61112162308651,
12.536380305637));
#438716=CARTESIAN_POINT('Ctrl Pts',(-0.740204366456533,-2.59775972554652,
12.5488460165097));
#438717=CARTESIAN_POINT('Ctrl Pts',(-0.741642765825077,-2.58439094072071,
12.5613043021964));
#438718=CARTESIAN_POINT('Ctrl Pts',(-0.743081587281321,-2.57101497634516,
12.5737548217797));
#438719=CARTESIAN_POINT('Ctrl Pts',(-0.786422857476888,-2.5656830183634,
12.5893111709658));
#438720=CARTESIAN_POINT('Ctrl Pts',(-0.779292702402738,-2.55687282408755,
12.5770542771492));
#438721=CARTESIAN_POINT('Ctrl Pts',(-0.764875628019588,-2.56461566859623,
12.5737548217797));
#438722=CARTESIAN_POINT('Ctrl Pts',(-0.779770484807521,-2.55746318373105,
12.5928319619712));
#438723=CARTESIAN_POINT('Ctrl Pts',(-0.77244624837694,-2.55359162369919,
12.5821634970842));
#438724=CARTESIAN_POINT('Ctrl Pts',(-0.762459666754359,-2.56161544384893,
12.5773203894503));
#438725=CARTESIAN_POINT('Ctrl Pts',(-0.764762191017099,-2.55002441926106,
12.5969440695591));
#438726=CARTESIAN_POINT('Ctrl Pts',(-0.760900142364282,-2.55113937341043,
12.5878292599214));
#438727=CARTESIAN_POINT('Ctrl Pts',(-0.757109495998643,-2.55896594956091,
12.5813877129824));
#438728=CARTESIAN_POINT('Ctrl Pts',(-0.735389456187558,-2.55859283184303,
12.596957478804));
#438729=CARTESIAN_POINT('Ctrl Pts',(-0.739222985498508,-2.55748619451717,
12.5878468778671));
#438730=CARTESIAN_POINT('Ctrl Pts',(-0.746598257514899,-2.56203842964092,
12.5814011370086));
#438731=CARTESIAN_POINT('Ctrl Pts',(-0.726685984338924,-2.57303542804039,
12.5928371701607));
#438732=CARTESIAN_POINT('Ctrl Pts',(-0.730756761274845,-2.565826833112,
12.5821692192952));
#438733=CARTESIAN_POINT('Ctrl Pts',(-0.743493039323462,-2.56717258325088,
12.5773318885715));
#438734=CARTESIAN_POINT('Ctrl Pts',(-0.725531957228221,-2.58356219985525,
12.5893111709658));
#438735=CARTESIAN_POINT('Ctrl Pts',(-0.726767074738745,-2.57229573992789,
12.5770542771492));
#438736=CARTESIAN_POINT('Ctrl Pts',(-0.743081587281266,-2.57101497634516,
12.5737548217797));
#438737=CARTESIAN_POINT('',(-0.764875628019588,-2.56461566859623,12.5737548217797));
#438738=CARTESIAN_POINT('Origin',(-0.769321660262914,-2.57952314314061,
12.5893111709658));
#438739=CARTESIAN_POINT('Ctrl Pts',(-0.743081587281266,-2.57101497634516,
12.5737548217797));
#438740=CARTESIAN_POINT('Ctrl Pts',(-0.743158247913999,-2.5700157552593,
12.5746934679442));
#438741=CARTESIAN_POINT('Ctrl Pts',(-0.743425725553061,-2.56892406338389,
12.5756680099006));
#438742=CARTESIAN_POINT('Ctrl Pts',(-0.743850354499381,-2.56786331179849,
12.5765688348656));
#438743=CARTESIAN_POINT('Ctrl Pts',(-0.74396277031212,-2.56758248955916,
12.5768073183026));
#438744=CARTESIAN_POINT('Ctrl Pts',(-0.744085945601193,-2.56730380124158,
12.5770407398754));
#438745=CARTESIAN_POINT('Ctrl Pts',(-0.744218734611065,-2.56702932315182,
12.5772674179684));
#438746=CARTESIAN_POINT('Ctrl Pts',(-0.744763664799926,-2.56590293929345,
12.5781976435658));
#438747=CARTESIAN_POINT('Ctrl Pts',(-0.745511600568155,-2.56478839473652,
12.5790594849312));
#438748=CARTESIAN_POINT('Ctrl Pts',(-0.746452137496484,-2.56378785337799,
12.5797571720116));
#438749=CARTESIAN_POINT('Ctrl Pts',(-0.747064931123984,-2.56313596470665,
12.580211740231));
#438750=CARTESIAN_POINT('Ctrl Pts',(-0.747801010366068,-2.56251570320559,
12.5806009430798));
#438751=CARTESIAN_POINT('Ctrl Pts',(-0.748619974766494,-2.56198428060995,
12.5808812374708));
#438752=CARTESIAN_POINT('Ctrl Pts',(-0.749323736875072,-2.56152761230268,
12.5811221033394));
#438753=CARTESIAN_POINT('Ctrl Pts',(-0.750103175628632,-2.56112729370187,
12.581287365893));
#438754=CARTESIAN_POINT('Ctrl Pts',(-0.750918107575558,-2.56081333637143,
12.581359338449));
#438755=CARTESIAN_POINT('Ctrl Pts',(-0.751031366288477,-2.56076970278548,
12.5813693411482));
#438756=CARTESIAN_POINT('Ctrl Pts',(-0.751145308888634,-2.56072767743566,
12.5813775999465));
#438757=CARTESIAN_POINT('Ctrl Pts',(-0.751259826879553,-2.5606872795466,
12.5813841266931));
#438758=CARTESIAN_POINT('Ctrl Pts',(-0.751454120501815,-2.56061873964178,
12.5813952001081));
#438759=CARTESIAN_POINT('Ctrl Pts',(-0.751651574239596,-2.56055499956375,
12.5814007534795));
#438760=CARTESIAN_POINT('Ctrl Pts',(-0.751852162678322,-2.56049627474705,
12.5814005856065));
#438761=CARTESIAN_POINT('Ctrl Pts',(-0.752770378125813,-2.56022745549613,
12.5813998171494));
#438762=CARTESIAN_POINT('Ctrl Pts',(-0.753690743216226,-2.56008197800291,
12.58127954464));
#438763=CARTESIAN_POINT('Ctrl Pts',(-0.754603413029476,-2.56003144168815,
12.5810700125799));
#438764=CARTESIAN_POINT('Ctrl Pts',(-0.755705814248104,-2.55997039957394,
12.5808169217085));
#438765=CARTESIAN_POINT('Ctrl Pts',(-0.756798013092731,-2.560064580481,
12.5804173076348));
#438766=CARTESIAN_POINT('Ctrl Pts',(-0.75778652844819,-2.56027978447649,
12.5799304713245));
#438767=CARTESIAN_POINT('Ctrl Pts',(-0.759011610388055,-2.56054649002315,
12.5793271277669));
#438768=CARTESIAN_POINT('Ctrl Pts',(-0.760160288447277,-2.56098415601984,
12.5785808224116));
#438769=CARTESIAN_POINT('Ctrl Pts',(-0.761195436365689,-2.56154469562594,
12.5777485681082));
#438770=CARTESIAN_POINT('Ctrl Pts',(-0.762737920173045,-2.56237996105073,
12.576508418016));
#438771=CARTESIAN_POINT('Ctrl Pts',(-0.764018603010034,-2.56347498204679,
12.5750928681475));
#438772=CARTESIAN_POINT('Ctrl Pts',(-0.764875628019588,-2.56461566859623,
12.5737548217797));
#438773=CARTESIAN_POINT('Ctrl Pts',(-0.764875628019588,-2.56461566859623,
12.5737548217797));
#438774=CARTESIAN_POINT('Ctrl Pts',(-0.779292702402738,-2.55687282408755,
12.5770542771492));
#438775=CARTESIAN_POINT('Ctrl Pts',(-0.786422857476888,-2.5656830183634,
12.5893111709658));
#438776=CARTESIAN_POINT('Ctrl Pts',(-0.780412297983975,-2.58389329398392,
12.5508408821982));
#438777=CARTESIAN_POINT('Ctrl Pts',(-0.794872520007951,-2.57612362837677,
12.55409748406));
#438778=CARTESIAN_POINT('Ctrl Pts',(-0.802011771333854,-2.58494506220412,
12.5663972313419));
#438779=CARTESIAN_POINT('Ctrl Pts',(-0.795934708955605,-2.60315134740109,
12.52790050457));
#438780=CARTESIAN_POINT('Ctrl Pts',(-0.810422498554156,-2.59533756279374,
12.5311362602938));
#438781=CARTESIAN_POINT('Ctrl Pts',(-0.817584958538338,-2.60418767380778,
12.5434568539655));
#438782=CARTESIAN_POINT('Ctrl Pts',(-0.811443979823457,-2.62239134115121,
12.5049357605811));
#438783=CARTESIAN_POINT('Ctrl Pts',(-0.825945748610739,-2.61451847083413,
12.5081700652078));
#438784=CARTESIAN_POINT('Ctrl Pts',(-0.833143650804941,-2.62341237511111,
12.5204921097672));
#438785=CARTESIAN_POINT('Ctrl Pts',(-0.810425581539454,-2.62112796674706,
12.5064436508395));
#438786=CARTESIAN_POINT('Ctrl Pts',(-0.811635627467077,-2.6209710061035,
12.5062361689309));
#438787=CARTESIAN_POINT('Ctrl Pts',(-0.812887283060052,-2.6207561808326,
12.5061871075061));
#438788=CARTESIAN_POINT('Ctrl Pts',(-0.814085200580072,-2.62048048125635,
12.5063648335164));
#438789=CARTESIAN_POINT('Ctrl Pts',(-0.814629368608283,-2.62035524150297,
12.5064455676329));
#438790=CARTESIAN_POINT('Ctrl Pts',(-0.815169988186426,-2.62021547857725,
12.506574497099));
#438791=CARTESIAN_POINT('Ctrl Pts',(-0.815683616121469,-2.62006616759708,
12.5067492519495));
#438792=CARTESIAN_POINT('Ctrl Pts',(-0.81671577139458,-2.61976612138657,
12.5071004286051));
#438793=CARTESIAN_POINT('Ctrl Pts',(-0.817676650834413,-2.6194157100936,
12.5076537929613));
#438794=CARTESIAN_POINT('Ctrl Pts',(-0.818497375929666,-2.61905011993456,
12.5083435010505));
#438795=CARTESIAN_POINT('Ctrl Pts',(-0.818549045479092,-2.61902710384927,
12.5083869222964));
#438796=CARTESIAN_POINT('Ctrl Pts',(-0.818600160311445,-2.61900401419111,
12.5084308732337));
#438797=CARTESIAN_POINT('Ctrl Pts',(-0.81865070395164,-2.61898085430138,
12.5084753333615));
#438798=CARTESIAN_POINT('Ctrl Pts',(-0.819056130657566,-2.61879508141751,
12.5088319622689));
#438799=CARTESIAN_POINT('Ctrl Pts',(-0.819433574196886,-2.61860219105085,
12.509227847131));
#438800=CARTESIAN_POINT('Ctrl Pts',(-0.819773085408875,-2.61841041216931,
12.5096423454524));
#438801=CARTESIAN_POINT('Ctrl Pts',(-0.820836963285881,-2.61780946203232,
12.5109411997424));
#438802=CARTESIAN_POINT('Ctrl Pts',(-0.821598567315469,-2.61719088189056,
12.5124831113042));
#438803=CARTESIAN_POINT('Ctrl Pts',(-0.822142048037762,-2.6165979677484,
12.5140723025008));
#438804=CARTESIAN_POINT('Ctrl Pts',(-0.822192972776699,-2.61654241104388,
12.5142212114565));
#438805=CARTESIAN_POINT('Ctrl Pts',(-0.822242011824836,-2.61648708310949,
12.5143705582413));
#438806=CARTESIAN_POINT('Ctrl Pts',(-0.822289251031082,-2.61643202305668,
12.5145201959299));
#438807=CARTESIAN_POINT('Ctrl Pts',(-0.822896108967137,-2.61572469470258,
12.5164425148273));
#438808=CARTESIAN_POINT('Ctrl Pts',(-0.823234877861664,-2.61504433199383,
12.5184635205941));
#438809=CARTESIAN_POINT('Ctrl Pts',(-0.823395536412026,-2.61438446866632,
12.5205025929158));
#438810=CARTESIAN_POINT('Ctrl Pts',(-0.823488724739145,-2.61400172178183,
12.5216853356836));
#438811=CARTESIAN_POINT('Ctrl Pts',(-0.823522290051381,-2.61362667761862,
12.5228750347131));
#438812=CARTESIAN_POINT('Ctrl Pts',(-0.823513873423488,-2.61326399730633,
12.5240609649613));
#438813=CARTESIAN_POINT('Ctrl Pts',(-0.823493215261862,-2.61237381793693,
12.5269717671326));
#438814=CARTESIAN_POINT('Ctrl Pts',(-0.823208670665855,-2.61153331013741,
12.5299036066169));
#438815=CARTESIAN_POINT('Ctrl Pts',(-0.822745720998118,-2.61072824508954,
12.5328133004019));
#438816=CARTESIAN_POINT('Ctrl Pts',(-0.822523478200853,-2.61034176698903,
12.5342101228451));
#438817=CARTESIAN_POINT('Ctrl Pts',(-0.822259943879739,-2.60996420034821,
12.5356023438238));
#438818=CARTESIAN_POINT('Ctrl Pts',(-0.821963002087443,-2.60959729166526,
12.5369868989719));
#438819=CARTESIAN_POINT('Origin',(-8.84453359361121,-12.5140605108539,-1.24074782725411));
#438820=CARTESIAN_POINT('Ctrl Pts',(-0.719380048696327,-2.63967814057616,
12.5369868989719));
#438821=CARTESIAN_POINT('Ctrl Pts',(-0.717737457340924,-2.65492888473259,
12.5369868989719));
#438822=CARTESIAN_POINT('Ctrl Pts',(-0.70285948685656,-2.65866108220216,
12.5369868989719));
#438823=CARTESIAN_POINT('Ctrl Pts',(-0.718824722745646,-2.6448334814637,
12.5218025310016));
#438824=CARTESIAN_POINT('Ctrl Pts',(-0.714312581026351,-2.65575577246924,
12.5216901060418));
#438825=CARTESIAN_POINT('Ctrl Pts',(-0.702904843853943,-2.65864972122353,
12.5161920673678));
#438826=CARTESIAN_POINT('Ctrl Pts',(-0.723316122852456,-2.64885385411758,
12.5042015548894));
#438827=CARTESIAN_POINT('Ctrl Pts',(-0.719798195314405,-2.65423916105906,
12.4980677368513));
#438828=CARTESIAN_POINT('Ctrl Pts',(-0.713237143708695,-2.65601211947674,
12.4907278922777));
#438829=CARTESIAN_POINT('Ctrl Pts',(-0.735310022442628,-2.64316304158105,
12.506463626192));
#438830=CARTESIAN_POINT('Ctrl Pts',(-0.737063577422545,-2.64946641236729,
12.4999376786891));
#438831=CARTESIAN_POINT('Ctrl Pts',(-0.737042160298133,-2.64938942585823,
12.4906970594712));
#438832=CARTESIAN_POINT('Origin',(-0.697506554688065,-2.63732224162448,
12.5369868989719));
#438833=CARTESIAN_POINT('Origin',(-0.697506554688065,-2.63732224162448,
14.));
#438834=CARTESIAN_POINT('Origin',(-0.697506554688065,-2.63732224162448,
13.7435492065112));
#438835=CARTESIAN_POINT('Ctrl Pts',(-0.722073737423757,-2.61510704217319,
13.793642941384));
#438836=CARTESIAN_POINT('Ctrl Pts',(-0.720922529256145,-2.62585789975576,
13.8071662555867));
#438837=CARTESIAN_POINT('Ctrl Pts',(-0.703906806013424,-2.62655399325649,
13.8103758687955));
#438838=CARTESIAN_POINT('Ctrl Pts',(-0.720262454621957,-2.6316291776234,
13.7804579775006));
#438839=CARTESIAN_POINT('Ctrl Pts',(-0.718831884636872,-2.64489368444598,
13.7901904343351));
#438840=CARTESIAN_POINT('Ctrl Pts',(-0.703400534075535,-2.64807634748468,
13.7927914348263));
#438841=CARTESIAN_POINT('Ctrl Pts',(-0.7191960842325,-2.6413563805567,13.7597120340895));
#438842=CARTESIAN_POINT('Ctrl Pts',(-0.717534814526755,-2.65670653602619,
13.7635825532445));
#438843=CARTESIAN_POINT('Ctrl Pts',(-0.703076430755867,-2.66076745401083,
13.7651073818884));
#438844=CARTESIAN_POINT('Ctrl Pts',(-0.719404903971055,-2.63945157149465,
13.7381884353898));
#438845=CARTESIAN_POINT('Ctrl Pts',(-0.717783412992171,-2.65444252468754,
13.7368803041982));
#438846=CARTESIAN_POINT('Ctrl Pts',(-0.703139405746687,-2.65828214562106,
13.7363986145813));
#438847=CARTESIAN_POINT('Origin',(-0.699765280213282,-2.61671866309859,
13.7902182540695));
#438848=CARTESIAN_POINT('Ctrl Pts',(-0.725532385420848,-2.58355828701616,
13.8235227101244));
#438849=CARTESIAN_POINT('Ctrl Pts',(-0.724283899720923,-2.59498737148417,
13.8358800583119));
#438850=CARTESIAN_POINT('Ctrl Pts',(-0.707754549332778,-2.59617338362709,
13.8390832900376));
#438851=CARTESIAN_POINT('Ctrl Pts',(-0.724232578206299,-2.5954148316435,
13.8124254819053));
#438852=CARTESIAN_POINT('Ctrl Pts',(-0.722981667688322,-2.60686611120135,
13.8247886449158));
#438853=CARTESIAN_POINT('Ctrl Pts',(-0.706430211948133,-2.60803662133952,
13.8279860620657));
#438854=CARTESIAN_POINT('Ctrl Pts',(-0.722933353523072,-2.60726606255325,
13.8013225099955));
#438855=CARTESIAN_POINT('Ctrl Pts',(-0.721680610408695,-2.61873413425349,
13.8136962257787));
#438856=CARTESIAN_POINT('Ctrl Pts',(-0.705106757049417,-2.61989439702853,
13.8168830918626));
#438857=CARTESIAN_POINT('Ctrl Pts',(-0.721634688705769,-2.61911218649399,
13.7902140179785));
#438858=CARTESIAN_POINT('Ctrl Pts',(-0.720380666507743,-2.63059200051128,
13.802602731458));
#438859=CARTESIAN_POINT('Ctrl Pts',(-0.703784151790519,-2.63174692551444,
13.8057746032558));
#438860=CARTESIAN_POINT('Origin',(-0.703662978283139,-2.58116475123284,
13.8235269408515));
#438861=CARTESIAN_POINT('Ctrl Pts',(-0.786422857476889,-2.5656830183634,
13.8235269408515));
#438862=CARTESIAN_POINT('Ctrl Pts',(-0.793850903700689,-2.57486129424115,
13.8362179249168));
#438863=CARTESIAN_POINT('Ctrl Pts',(-0.808689144333974,-2.56640614084421,
13.8391868794938));
#438864=CARTESIAN_POINT('Ctrl Pts',(-0.779626518505738,-2.55728529544185,
13.8400110824519));
#438865=CARTESIAN_POINT('Ctrl Pts',(-0.788241229681228,-2.56249188878345,
13.8494522556837));
#438866=CARTESIAN_POINT('Ctrl Pts',(-0.79741695096815,-2.55265654301925,
13.85569149686));
#438867=CARTESIAN_POINT('Ctrl Pts',(-0.765091992637448,-2.54992694754099,
13.8586819406588));
#438868=CARTESIAN_POINT('Ctrl Pts',(-0.769273381913537,-2.54871367619591,
13.868010383617));
#438869=CARTESIAN_POINT('Ctrl Pts',(-0.773223403946076,-2.54057179725215,
13.8744918421245));
#438870=CARTESIAN_POINT('Ctrl Pts',(-0.735054534284133,-2.55869179743246,
13.8587686893867));
#438871=CARTESIAN_POINT('Ctrl Pts',(-0.730910343642403,-2.55989421659599,
13.8680909899357));
#438872=CARTESIAN_POINT('Ctrl Pts',(-0.723220577461804,-2.55516516832033,
13.8745789365163));
#438873=CARTESIAN_POINT('Ctrl Pts',(-0.726711165341349,-2.57280573262591,
13.8400379222776));
#438874=CARTESIAN_POINT('Ctrl Pts',(-0.722273609608704,-2.5818378050917,
13.8494748685453));
#438875=CARTESIAN_POINT('Ctrl Pts',(-0.709242845016182,-2.57852717382274,
13.8557104837033));
#438876=CARTESIAN_POINT('Ctrl Pts',(-0.725531957221722,-2.5835621998544,
13.8235269408542));
#438877=CARTESIAN_POINT('Ctrl Pts',(-0.72424523766725,-2.59529936184436,
13.8362179249195));
#438878=CARTESIAN_POINT('Ctrl Pts',(-0.707191314269287,-2.59620859272407,
13.8391868794965));
#438879=CARTESIAN_POINT('Origin',(-0.803524054690863,-2.55184289358619,
13.8235269408515));
#438880=CARTESIAN_POINT('Ctrl Pts',(-0.808921225855,-2.59348255226219,13.7902140241682));
#438881=CARTESIAN_POINT('Ctrl Pts',(-0.816182634669319,-2.6024620031042,
13.8026027327198));
#438882=CARTESIAN_POINT('Ctrl Pts',(-0.830768905102112,-2.59446083774312,
13.8057746032556));
#438883=CARTESIAN_POINT('Ctrl Pts',(-0.801424221355978,-2.58421906985202,
13.8013225161807));
#438884=CARTESIAN_POINT('Ctrl Pts',(-0.80867820575412,-2.59318933396389,
13.8136962270464));
#438885=CARTESIAN_POINT('Ctrl Pts',(-0.823248298065677,-2.58520491066934,
13.8168830918628));
#438886=CARTESIAN_POINT('Ctrl Pts',(-0.793923984830844,-2.57495159387123,
13.8124254880875));
#438887=CARTESIAN_POINT('Ctrl Pts',(-0.801167349029216,-2.58390872232463,
13.8247886461868));
#438888=CARTESIAN_POINT('Ctrl Pts',(-0.815724139415132,-2.57594502871805,
13.8279860620656));
#438889=CARTESIAN_POINT('Ctrl Pts',(-0.78642038543453,-2.56567996264446,
13.8235227163065));
#438890=CARTESIAN_POINT('Ctrl Pts',(-0.793649710173589,-2.57461973037378,
13.8358800595847));
#438891=CARTESIAN_POINT('Ctrl Pts',(-0.808196285377042,-2.56668102892777,
13.8390832900376));
#438892=CARTESIAN_POINT('Origin',(-0.826024902936883,-2.57964549287854,
13.7902182540695));
#438893=CARTESIAN_POINT('Ctrl Pts',(-0.821793255587976,-2.60938750488452,
13.7382347919292));
#438894=CARTESIAN_POINT('Ctrl Pts',(-0.831267858507332,-2.62113270680929,
13.7369371795943));
#438895=CARTESIAN_POINT('Ctrl Pts',(-0.845671586658218,-2.61643415465193,
13.7364597369711));
#438896=CARTESIAN_POINT('Ctrl Pts',(-0.822983228330782,-2.61085786499539,
13.7595490285573));
#438897=CARTESIAN_POINT('Ctrl Pts',(-0.832684669703119,-2.62288266610469,
13.7633824266925));
#438898=CARTESIAN_POINT('Ctrl Pts',(-0.84705080372898,-2.61846589653202,
13.7648920890506));
#438899=CARTESIAN_POINT('Ctrl Pts',(-0.816914432528308,-2.60335910898789,
13.7803806590111));
#438900=CARTESIAN_POINT('Ctrl Pts',(-0.825301630537322,-2.61376352130003,
13.7901039518745));
#438901=CARTESIAN_POINT('Ctrl Pts',(-0.84001633264238,-2.60810993983472,
13.7926933640891));
#438902=CARTESIAN_POINT('Ctrl Pts',(-0.806365510757895,-2.59032459706546,
13.7936647693663));
#438903=CARTESIAN_POINT('Ctrl Pts',(-0.813146129652744,-2.59875054148418,
13.8072068914933));
#438904=CARTESIAN_POINT('Ctrl Pts',(-0.827847479755415,-2.59011835896727,
13.8104111085397));
#438905=CARTESIAN_POINT('Origin',(-0.839064199301418,-2.59575716688805,
13.7435492065112));
#438906=CARTESIAN_POINT('Origin',(-0.839064199301418,-2.59575716688805,
14.));
#438907=CARTESIAN_POINT('Origin',(-0.839064199301418,-2.59575716688805,
12.5369868989719));
#438908=CARTESIAN_POINT('Ctrl Pts',(-0.810420151261945,-2.62111040384641,
12.506462012331));
#438909=CARTESIAN_POINT('Ctrl Pts',(-0.812351610471273,-2.62735724731432,
12.4999388158272));
#438910=CARTESIAN_POINT('Ctrl Pts',(-0.812328758775875,-2.62728333896387,
12.4907030323752));
#438911=CARTESIAN_POINT('Ctrl Pts',(-0.823586101983871,-2.61941148514846,
12.5042014951932));
#438912=CARTESIAN_POINT('Ctrl Pts',(-0.829454125149732,-2.62203967868035,
12.4980716682127));
#438913=CARTESIAN_POINT('Ctrl Pts',(-0.83592806650496,-2.6199869613216,
12.4907355092743));
#438914=CARTESIAN_POINT('Ctrl Pts',(-0.825192965213259,-2.61360255307729,
12.5218047446509));
#438915=CARTESIAN_POINT('Ctrl Pts',(-0.834889739761238,-2.62034728689729,
12.5216906929434));
#438916=CARTESIAN_POINT('Ctrl Pts',(-0.846046639061602,-2.61661977400911,
12.5161988840776));
#438917=CARTESIAN_POINT('Ctrl Pts',(-0.821938860714689,-2.60956740867775,
12.5369868989719));
#438918=CARTESIAN_POINT('Ctrl Pts',(-0.831562019321965,-2.62150057045239,
12.5369868989719));
#438919=CARTESIAN_POINT('Ctrl Pts',(-0.846089323214206,-2.61660537146327,
12.5369868989719));
#438920=CARTESIAN_POINT('Origin',(-1.45144742314189E-31,-1.0095038568149E-30,
12.5));
#438921=CARTESIAN_POINT('Origin',(-0.574679115658286,-2.62124668345172,
12.5));
#438922=CARTESIAN_POINT('',(-0.574679115658286,-2.62124668345172,12.5893111709658));
#438923=CARTESIAN_POINT('',(-0.574679115658286,-2.62124668345172,13.8235269408515));
#438924=CARTESIAN_POINT('',(-0.574679115658286,-2.62124668345172,12.5));
#438925=CARTESIAN_POINT('',(-0.594838924238891,-2.65079079990822,13.7902182540695));
#438926=CARTESIAN_POINT('',(-0.574679115658286,-2.62124668345172,13.8235269408515));
#438927=CARTESIAN_POINT('',(-0.60652158241518,-2.66791168735621,13.7435492065112));
#438928=CARTESIAN_POINT('Origin',(-0.568085522355904,-2.61158437756436,
13.744521291869));
#438929=CARTESIAN_POINT('',(-0.60652158241518,-2.66791168735621,12.5369868989719));
#438930=CARTESIAN_POINT('',(-0.60652158241518,-2.66791168735621,12.5));
#438931=CARTESIAN_POINT('Ctrl Pts',(-0.60652158241518,-2.66791168735621,
12.5369868989719));
#438932=CARTESIAN_POINT('Ctrl Pts',(-0.595915168149065,-2.65236803092659,
12.5544431401645));
#438933=CARTESIAN_POINT('Ctrl Pts',(-0.585301167893566,-2.63681325726076,
12.5718848856037));
#438934=CARTESIAN_POINT('Ctrl Pts',(-0.574679115658286,-2.62124668345172,
12.5893111709658));
#438935=CARTESIAN_POINT('Origin',(-0.460383554137941,-2.90411316731588,
12.5));
#438936=CARTESIAN_POINT('',(-0.501820210172241,-2.68957202508688,13.7435492065112));
#438937=CARTESIAN_POINT('',(-0.505750802898757,-2.66922111036815,13.7902182540695));
#438938=CARTESIAN_POINT('Origin',(-0.516079721241096,-2.61574242383222,
13.7418732680445));
#438939=CARTESIAN_POINT('',(-0.512533505583296,-2.6341031997883,13.8235269408515));
#438940=CARTESIAN_POINT('',(-0.505750802898757,-2.66922111036815,13.7902182540695));
#438941=CARTESIAN_POINT('',(-0.512533505583296,-2.6341031997883,12.5893111709658));
#438942=CARTESIAN_POINT('',(-0.512533505583296,-2.6341031997883,12.5));
#438943=CARTESIAN_POINT('',(-0.501820210172241,-2.68957202508688,12.5369868989719));
#438944=CARTESIAN_POINT('Ctrl Pts',(-0.512533505583296,-2.6341031997883,
12.5893111709658));
#438945=CARTESIAN_POINT('Ctrl Pts',(-0.508959750310596,-2.65260656399841,
12.5718848856037));
#438946=CARTESIAN_POINT('Ctrl Pts',(-0.505388704100567,-2.67109590184985,
12.5544431401645));
#438947=CARTESIAN_POINT('Ctrl Pts',(-0.501820210172241,-2.68957202508688,
12.5369868989719));
#438948=CARTESIAN_POINT('',(-0.501820210172241,-2.68957202508688,12.5));
#438949=CARTESIAN_POINT('Origin',(-0.546284751524244,-2.64062194371897,
12.5));
#438950=CARTESIAN_POINT('',(-0.54042097942408,-2.60675150898696,13.8587068136939));
#438951=CARTESIAN_POINT('Ctrl Pts',(-0.512533505576834,-2.6341031997869,
13.8235269408542));
#438952=CARTESIAN_POINT('Ctrl Pts',(-0.512865804750207,-2.63238269791637,
13.8262006681044));
#438953=CARTESIAN_POINT('Ctrl Pts',(-0.513376451134595,-2.63065496289556,
13.8288634856214));
#438954=CARTESIAN_POINT('Ctrl Pts',(-0.514052260639445,-2.62892199117244,
13.8314912288862));
#438955=CARTESIAN_POINT('Ctrl Pts',(-0.514748950532427,-2.62713547607364,
13.834200161153));
#438956=CARTESIAN_POINT('Ctrl Pts',(-0.515621478177327,-2.62534123077201,
13.8368750301949));
#438957=CARTESIAN_POINT('Ctrl Pts',(-0.516700460746796,-2.62353789338469,
13.8394886372968));
#438958=CARTESIAN_POINT('Ctrl Pts',(-0.516783793187885,-2.62339861726397,
13.839690492513));
#438959=CARTESIAN_POINT('Ctrl Pts',(-0.516868377782284,-2.62325929483752,
13.8398919674349));
#438960=CARTESIAN_POINT('Ctrl Pts',(-0.516954238919628,-2.62311993049648,
13.8400930404591));
#438961=CARTESIAN_POINT('Ctrl Pts',(-0.518292013203951,-2.62094854030339,
13.8432258934518));
#438962=CARTESIAN_POINT('Ctrl Pts',(-0.519931893274218,-2.61877746447833,
13.8462331177034));
#438963=CARTESIAN_POINT('Ctrl Pts',(-0.521897370698895,-2.61673565388558,
13.8489036603661));
#438964=CARTESIAN_POINT('Ctrl Pts',(-0.522540497785662,-2.61606754969789,
13.849777493004));
#438965=CARTESIAN_POINT('Ctrl Pts',(-0.523218439369455,-2.61541353120771,
13.85061494757));
#438966=CARTESIAN_POINT('Ctrl Pts',(-0.52393187423922,-2.61477881519862,
13.8514076489583));
#438967=CARTESIAN_POINT('Ctrl Pts',(-0.525440891881487,-2.61343629929965,
13.8530843267192));
#438968=CARTESIAN_POINT('Ctrl Pts',(-0.527258891987578,-2.6120504790655,
13.8546805203176));
#438969=CARTESIAN_POINT('Ctrl Pts',(-0.529363076056738,-2.61081030075545,
13.8559412814274));
#438970=CARTESIAN_POINT('Ctrl Pts',(-0.529644684125489,-2.61064432467764,
13.8561100121513));
#438971=CARTESIAN_POINT('Ctrl Pts',(-0.52993134547584,-2.61048093207307,
13.8562727473908));
#438972=CARTESIAN_POINT('Ctrl Pts',(-0.530222937453116,-2.61032054227133,
13.8564289040185));
#438973=CARTESIAN_POINT('Ctrl Pts',(-0.531545303743502,-2.6095931763502,
13.8571370725437));
#438974=CARTESIAN_POINT('Ctrl Pts',(-0.532993414539191,-2.60891677597829,
13.8577210840553));
#438975=CARTESIAN_POINT('Ctrl Pts',(-0.534523401653899,-2.6083442233283,
13.8581177131616));
#438976=CARTESIAN_POINT('Ctrl Pts',(-0.534954298685957,-2.6081829727954,
13.8582294175695));
#438977=CARTESIAN_POINT('Ctrl Pts',(-0.535391596345183,-2.60802980832461,
13.8583265086086));
#438978=CARTESIAN_POINT('Ctrl Pts',(-0.535834105640109,-2.60788552453068,
13.8584082369006));
#438979=CARTESIAN_POINT('Ctrl Pts',(-0.536469872833358,-2.60767822741002,
13.8585256585398));
#438980=CARTESIAN_POINT('Ctrl Pts',(-0.537124402195584,-2.60748699199285,
13.8586122832068));
#438981=CARTESIAN_POINT('Ctrl Pts',(-0.537780912416568,-2.60731754401745,
13.8586682984299));
#438982=CARTESIAN_POINT('Ctrl Pts',(-0.538306055515589,-2.60718200243396,
13.8587131050557));
#438983=CARTESIAN_POINT('Ctrl Pts',(-0.538838207659092,-2.6070586772584,
13.8587357943552));
#438984=CARTESIAN_POINT('Ctrl Pts',(-0.53937754641893,-2.60694804720681,
13.8587355499465));
#438985=CARTESIAN_POINT('Ctrl Pts',(-0.539726133917808,-2.60687654436693,
13.8587353919793));
#438986=CARTESIAN_POINT('Ctrl Pts',(-0.540073946165131,-2.60681108005693,
13.8587257282814));
#438987=CARTESIAN_POINT('Ctrl Pts',(-0.54042097942408,-2.60675150898696,
13.8587068136939));
#438988=CARTESIAN_POINT('Ctrl Pts',(-0.54042097942408,-2.60675150898696,
13.8587068136939));
#438989=CARTESIAN_POINT('Ctrl Pts',(-0.541562352894183,-2.60655558298533,
13.8586446046466));
#438990=CARTESIAN_POINT('Ctrl Pts',(-0.542695311066701,-2.60642332639463,
13.858482427929));
#438991=CARTESIAN_POINT('Ctrl Pts',(-0.543819640952938,-2.60635027372574,
13.8582284286032));
#438992=CARTESIAN_POINT('Ctrl Pts',(-0.544973072628753,-2.60627533018529,
13.8579678548414));
#438993=CARTESIAN_POINT('Ctrl Pts',(-0.546120340402775,-2.60626404042183,
13.857615680862));
#438994=CARTESIAN_POINT('Ctrl Pts',(-0.547216118747798,-2.60630716032551,
13.8571944833187));
#438995=CARTESIAN_POINT('Ctrl Pts',(-0.549950745674822,-2.60641477045508,
13.8561433417727));
#438996=CARTESIAN_POINT('Ctrl Pts',(-0.552492800705602,-2.606861487623,
13.8546163505474));
#438997=CARTESIAN_POINT('Ctrl Pts',(-0.554735430543981,-2.60747028008139,
13.8528973491086));
#438998=CARTESIAN_POINT('Ctrl Pts',(-0.555145125928532,-2.60758149748164,
13.8525833129072));
#438999=CARTESIAN_POINT('Ctrl Pts',(-0.555544924168542,-2.60769802010329,
13.8522628768812));
#439000=CARTESIAN_POINT('Ctrl Pts',(-0.555934314092714,-2.607818657743,
13.851937733538));
#439001=CARTESIAN_POINT('Ctrl Pts',(-0.55831226433424,-2.60855537507098,
13.8499521282529));
#439002=CARTESIAN_POINT('Ctrl Pts',(-0.560537166023577,-2.6095226682952,
13.847639871647));
#439003=CARTESIAN_POINT('Ctrl Pts',(-0.562524118944962,-2.6105960213429,
13.8452109780794));
#439004=CARTESIAN_POINT('Ctrl Pts',(-0.563418090192172,-2.61107894509637,
13.8441181685877));
#439005=CARTESIAN_POINT('Ctrl Pts',(-0.564264432294491,-2.61158286382886,
13.8430021611332));
#439006=CARTESIAN_POINT('Ctrl Pts',(-0.565058450318323,-2.6120951250143,
13.8418824960098));
#439007=CARTESIAN_POINT('Ctrl Pts',(-0.566929574067454,-2.61330228157887,
13.8392439765549));
#439008=CARTESIAN_POINT('Ctrl Pts',(-0.568601629189551,-2.61461029451099,
13.8364981347964));
#439009=CARTESIAN_POINT('Ctrl Pts',(-0.570100122503587,-2.61599566984666,
13.8336931113419));
#439010=CARTESIAN_POINT('Ctrl Pts',(-0.571559559828334,-2.61734493744413,
13.8309611966328));
#439011=CARTESIAN_POINT('Ctrl Pts',(-0.572855444020918,-2.61876935384968,
13.8281701127186));
#439012=CARTESIAN_POINT('Ctrl Pts',(-0.573975989967246,-2.62026438828469,
13.8253580685121));
#439013=CARTESIAN_POINT('Ctrl Pts',(-0.574218925537742,-2.6205885133637,
13.8247484142933));
#439014=CARTESIAN_POINT('Ctrl Pts',(-0.574453446788048,-2.6209159666517,
13.8241378483365));
#439015=CARTESIAN_POINT('Ctrl Pts',(-0.574679115658286,-2.62124668345172,
13.8235269408515));
#439016=CARTESIAN_POINT('',(-0.539201119045522,-2.6069854267383,12.5969504640361));
#439017=CARTESIAN_POINT('Origin',(-0.546291645961924,-2.64065430340899,
12.584524458991));
#439018=CARTESIAN_POINT('Origin',(-0.546291645961924,-2.64065430340899,
12.584524458991));
#439019=CARTESIAN_POINT('Ctrl Pts',(-0.512533505583295,-2.6341031997883,
12.5893111709658));
#439020=CARTESIAN_POINT('Ctrl Pts',(-0.514682834418984,-2.6229749016203,
12.5770542771492));
#439021=CARTESIAN_POINT('Ctrl Pts',(-0.531047455888894,-2.6230281839015,
12.5737548217797));
#439022=CARTESIAN_POINT('Ctrl Pts',(-0.507833644755842,-2.65843705311383,
12.5663937883685));
#439023=CARTESIAN_POINT('Ctrl Pts',(-0.50998571535895,-2.64729455925604,
12.5540940315304));
#439024=CARTESIAN_POINT('Ctrl Pts',(-0.526401037016491,-2.64735121781805,
12.5508374392248));
#439025=CARTESIAN_POINT('Ctrl Pts',(-0.503138526030348,-2.68274635387966,
12.5434499600944));
#439026=CARTESIAN_POINT('Ctrl Pts',(-0.505297593781433,-2.67156763180639,
12.5311293540532));
#439027=CARTESIAN_POINT('Ctrl Pts',(-0.521757998883145,-2.67165026622646,
12.5278936106989));
#439028=CARTESIAN_POINT('Ctrl Pts',(-0.498447777951471,-2.70703302532143,
12.5204817579905));
#439029=CARTESIAN_POINT('Ctrl Pts',(-0.500617531612337,-2.69579897621351,
12.5081597038247));
#439030=CARTESIAN_POINT('Ctrl Pts',(-0.517118065116471,-2.69592719077464,
12.5049254088044));
#439031=CARTESIAN_POINT('Ctrl Pts',(-0.501820210172241,-2.68957202508688,
12.5369868989719));
#439032=CARTESIAN_POINT('Ctrl Pts',(-0.501643563314908,-2.69048662721815,
12.5342545179733));
#439033=CARTESIAN_POINT('Ctrl Pts',(-0.501597462099068,-2.69138313811672,
12.5314872231885));
#439034=CARTESIAN_POINT('Ctrl Pts',(-0.501740330620115,-2.69221392671548,
12.5287124745063));
#439035=CARTESIAN_POINT('Ctrl Pts',(-0.501869176543756,-2.69296317311051,
12.5262100684184));
#439036=CARTESIAN_POINT('Ctrl Pts',(-0.502152557146489,-2.69365804271822,
12.5237004536639));
#439037=CARTESIAN_POINT('Ctrl Pts',(-0.502656720631253,-2.69428543394549,
12.5212220730815));
#439038=CARTESIAN_POINT('Ctrl Pts',(-0.50304270139246,-2.69476575620364,
12.5193246583486));
#439039=CARTESIAN_POINT('Ctrl Pts',(-0.503563195692237,-2.69521187088284,
12.517417831369));
#439040=CARTESIAN_POINT('Ctrl Pts',(-0.504294802084582,-2.69556388905023,
12.5155812248347));
#439041=CARTESIAN_POINT('Ctrl Pts',(-0.504606470340122,-2.69571385068165,
12.5147988205793));
#439042=CARTESIAN_POINT('Ctrl Pts',(-0.504956647615943,-2.69584713748605,
12.5140295443047));
#439043=CARTESIAN_POINT('Ctrl Pts',(-0.50535157462054,-2.69596122260285,
12.5132817086137));
#439044=CARTESIAN_POINT('Ctrl Pts',(-0.505949243217482,-2.69613387499403,
12.5121499604604));
#439045=CARTESIAN_POINT('Ctrl Pts',(-0.506664291904626,-2.69625940782588,
12.5110494206568));
#439046=CARTESIAN_POINT('Ctrl Pts',(-0.507514620373767,-2.69630516379017,
12.5100666561695));
#439047=CARTESIAN_POINT('Ctrl Pts',(-0.508002877022615,-2.6963314367595,
12.5095023550641));
#439048=CARTESIAN_POINT('Ctrl Pts',(-0.508541412251363,-2.69633105881386,
12.5089719619137));
#439049=CARTESIAN_POINT('Ctrl Pts',(-0.509120127329921,-2.69629765006048,
12.5085043804652));
#439050=CARTESIAN_POINT('Ctrl Pts',(-0.509967001464448,-2.6962487607017,
12.5078201359221));
#439051=CARTESIAN_POINT('Ctrl Pts',(-0.510924411352231,-2.69612651374109,
12.5072563000949));
#439052=CARTESIAN_POINT('Ctrl Pts',(-0.511926386449674,-2.69593079789991,
12.5068768744332));
#439053=CARTESIAN_POINT('Ctrl Pts',(-0.512648879471132,-2.6957896733053,
12.5066032824114));
#439054=CARTESIAN_POINT('Ctrl Pts',(-0.513407248367904,-2.69560792887737,
12.5064197834844));
#439055=CARTESIAN_POINT('Ctrl Pts',(-0.514159746260541,-2.69539822737795,
12.5063282718343));
#439056=CARTESIAN_POINT('Ctrl Pts',(-0.515258160216331,-2.69509212811074,
12.5061946931565));
#439057=CARTESIAN_POINT('Ctrl Pts',(-0.516367827280128,-2.69472094151683,
12.5062515701262));
#439058=CARTESIAN_POINT('Ctrl Pts',(-0.517424785305864,-2.69432236987892,
12.5064436508398));
#439059=CARTESIAN_POINT('',(-0.531047455888895,-2.6230281839015,12.5737548217797));
#439060=CARTESIAN_POINT('Origin',(-0.534134302985502,-2.63827519590392,
12.5893111709658));
#439061=CARTESIAN_POINT('Ctrl Pts',(-0.517424785305864,-2.69432236987892,
12.5064436508398));
#439062=CARTESIAN_POINT('Ctrl Pts',(-0.519441766381226,-2.68376906825844,
12.5164271754438));
#439063=CARTESIAN_POINT('Ctrl Pts',(-0.521459341766315,-2.67321154408909,
12.5264061185523));
#439064=CARTESIAN_POINT('Ctrl Pts',(-0.52347753332189,-2.66264964883392,
12.536380305637));
#439065=CARTESIAN_POINT('Ctrl Pts',(-0.525999863433005,-2.64944942194814,
12.5488460165097));
#439066=CARTESIAN_POINT('Ctrl Pts',(-0.52852315671935,-2.63624236355297,
12.5613043021964));
#439067=CARTESIAN_POINT('Ctrl Pts',(-0.531047455888894,-2.6230281839015,
12.5737548217797));
#439068=CARTESIAN_POINT('Ctrl Pts',(-0.574679115658286,-2.62124668345172,
12.5893111709658));
#439069=CARTESIAN_POINT('Ctrl Pts',(-0.568290798210283,-2.61188463053886,
12.5770542771492));
#439070=CARTESIAN_POINT('Ctrl Pts',(-0.553290581744299,-2.61842658596736,
12.5737548217797));
#439071=CARTESIAN_POINT('Ctrl Pts',(-0.56871887104195,-2.61251196951086,
12.5928319619712));
#439072=CARTESIAN_POINT('Ctrl Pts',(-0.561734573488288,-2.60805629851163,
12.5821634970843));
#439073=CARTESIAN_POINT('Ctrl Pts',(-0.551127205560511,-2.6152394209486,
12.5773203894503));
#439074=CARTESIAN_POINT('Ctrl Pts',(-0.554366844473443,-2.60387464164186,
12.5969440695591));
#439075=CARTESIAN_POINT('Ctrl Pts',(-0.550426767355019,-2.60467109305456,
12.5878292599214));
#439076=CARTESIAN_POINT('Ctrl Pts',(-0.546010795437804,-2.61216265404911,
12.5813877129824));
#439077=CARTESIAN_POINT('Ctrl Pts',(-0.524393439825277,-2.61002039296604,
12.596957478804));
#439078=CARTESIAN_POINT('Ctrl Pts',(-0.528304414599265,-2.60922990611218,
12.5878468778671));
#439079=CARTESIAN_POINT('Ctrl Pts',(-0.535284096582965,-2.6143681471871,
12.5814011370086));
#439080=CARTESIAN_POINT('Ctrl Pts',(-0.514541722392628,-2.62370551886122,
12.5928371701607));
#439081=CARTESIAN_POINT('Ctrl Pts',(-0.51918652156212,-2.61685271604931,
12.5821692192951));
#439082=CARTESIAN_POINT('Ctrl Pts',(-0.531770729566533,-2.61923211321443,
12.5773318885715));
#439083=CARTESIAN_POINT('Ctrl Pts',(-0.512533505583241,-2.63410319978828,
12.5893111709658));
#439084=CARTESIAN_POINT('Ctrl Pts',(-0.514682834418931,-2.62297490162029,
12.5770542771492));
#439085=CARTESIAN_POINT('Ctrl Pts',(-0.53104745588884,-2.62302818390148,
12.5737548217797));
#439086=CARTESIAN_POINT('',(-0.553290581744299,-2.61842658596736,12.5737548217797));
#439087=CARTESIAN_POINT('Origin',(-0.556506722612499,-2.63364685002276,
12.5893111709658));
#439088=CARTESIAN_POINT('Ctrl Pts',(-0.53104745588884,-2.62302818390148,
12.5737548217797));
#439089=CARTESIAN_POINT('Ctrl Pts',(-0.531205307234454,-2.62203853619462,
12.5746934679442));
#439090=CARTESIAN_POINT('Ctrl Pts',(-0.531560877886354,-2.6209722787446,
12.5756680099006));
#439091=CARTESIAN_POINT('Ctrl Pts',(-0.532070555016628,-2.61994966792378,
12.5765688348656));
#439092=CARTESIAN_POINT('Ctrl Pts',(-0.532205486394558,-2.61967894302964,
12.5768073183026));
#439093=CARTESIAN_POINT('Ctrl Pts',(-0.532350967513118,-2.619411221954,
12.5770407398754));
#439094=CARTESIAN_POINT('Ctrl Pts',(-0.532505687190963,-2.6191484807045,
12.5772674179684));
#439095=CARTESIAN_POINT('Ctrl Pts',(-0.533140614910869,-2.61807026166477,
12.5781976435658));
#439096=CARTESIAN_POINT('Ctrl Pts',(-0.533976907712846,-2.61702038937152,
12.5790594849312));
#439097=CARTESIAN_POINT('Ctrl Pts',(-0.534995868491428,-2.616099839723,
12.5797571720115));
#439098=CARTESIAN_POINT('Ctrl Pts',(-0.535659758077238,-2.61550006852697,
12.580211740231));
#439099=CARTESIAN_POINT('Ctrl Pts',(-0.53644394514693,-2.61494186818654,
12.5806009430798));
#439100=CARTESIAN_POINT('Ctrl Pts',(-0.537303500385903,-2.61447896705728,
12.5808812374708));
#439101=CARTESIAN_POINT('Ctrl Pts',(-0.538042143490665,-2.61408118142139,
12.5811221033394));
#439102=CARTESIAN_POINT('Ctrl Pts',(-0.538851618408412,-2.61374572634208,
12.581287365893));
#439103=CARTESIAN_POINT('Ctrl Pts',(-0.539689429173579,-2.61349923819789,
12.581359338449));
#439104=CARTESIAN_POINT('Ctrl Pts',(-0.539805867569806,-2.61346498143563,
12.5813693411482));
#439105=CARTESIAN_POINT('Ctrl Pts',(-0.539922856491515,-2.61343238330141,
12.5813775999465));
#439106=CARTESIAN_POINT('Ctrl Pts',(-0.540040286236262,-2.61340145411238,
12.5813841266931));
#439107=CARTESIAN_POINT('Ctrl Pts',(-0.540239520001061,-2.61334897900239,
12.5813952001081));
#439108=CARTESIAN_POINT('Ctrl Pts',(-0.540441512135912,-2.61330154532691,
12.5814007534795));
#439109=CARTESIAN_POINT('Ctrl Pts',(-0.540646219750891,-2.61325936573213,
12.5814005856065));
#439110=CARTESIAN_POINT('Ctrl Pts',(-0.541583291176775,-2.61306628403835,
12.5813998171494));
#439111=CARTESIAN_POINT('Ctrl Pts',(-0.542512451594518,-2.61299630890861,
12.58127954464));
#439112=CARTESIAN_POINT('Ctrl Pts',(-0.543426203753064,-2.61302033181186,
12.5810700125799));
#439113=CARTESIAN_POINT('Ctrl Pts',(-0.544529912321574,-2.61304934874376,
12.5808169217085));
#439114=CARTESIAN_POINT('Ctrl Pts',(-0.545610800346387,-2.61323224061694,
12.5804173076348));
#439115=CARTESIAN_POINT('Ctrl Pts',(-0.546578485375059,-2.61352730171729,
12.5799304713245));
#439116=CARTESIAN_POINT('Ctrl Pts',(-0.547777751977805,-2.61389297537445,
12.5793271277669));
#439117=CARTESIAN_POINT('Ctrl Pts',(-0.548886934063721,-2.61442281299927,
12.5785808224116));
#439118=CARTESIAN_POINT('Ctrl Pts',(-0.549872948431136,-2.61506586162127,
12.5777485681082));
#439119=CARTESIAN_POINT('Ctrl Pts',(-0.551342217864523,-2.61602407451928,
12.576508418016));
#439120=CARTESIAN_POINT('Ctrl Pts',(-0.552529384958163,-2.6172198394638,
12.5750928681475));
#439121=CARTESIAN_POINT('Ctrl Pts',(-0.553290581744299,-2.61842658596736,
12.5737548217797));
#439122=CARTESIAN_POINT('Ctrl Pts',(-0.553290581744299,-2.61842658596736,
12.5737548217797));
#439123=CARTESIAN_POINT('Ctrl Pts',(-0.568290798210284,-2.61188463053886,
12.5770542771492));
#439124=CARTESIAN_POINT('Ctrl Pts',(-0.574679115658286,-2.62124668345172,
12.5893111709658));
#439125=CARTESIAN_POINT('Ctrl Pts',(-0.567204249287228,-2.63890644948437,
12.5508408821982));
#439126=CARTESIAN_POINT('Ctrl Pts',(-0.582249655992346,-2.63234127913569,
12.55409748406));
#439127=CARTESIAN_POINT('Ctrl Pts',(-0.588646123297284,-2.64171527563033,
12.5663972313419));
#439128=CARTESIAN_POINT('Ctrl Pts',(-0.581105300580312,-2.6593656439147,
12.52790050457));
#439129=CARTESIAN_POINT('Ctrl Pts',(-0.596181779239276,-2.65275874838143,
12.5311362602938));
#439130=CARTESIAN_POINT('Ctrl Pts',(-0.602599040520637,-2.66216321836284,
12.5434568539655));
#439131=CARTESIAN_POINT('Ctrl Pts',(-0.594994727522753,-2.67980576772958,
12.5049357605811));
#439132=CARTESIAN_POINT('Ctrl Pts',(-0.610089954889711,-2.67314112252303,
12.5081700652078));
#439133=CARTESIAN_POINT('Ctrl Pts',(-0.616538970892595,-2.68259212891811,
12.5204921097672));
#439134=CARTESIAN_POINT('Ctrl Pts',(-0.594082694617563,-2.67846358818504,
12.5064436508395));
#439135=CARTESIAN_POINT('Ctrl Pts',(-0.595301507966785,-2.67840577979169,
12.5062361689309));
#439136=CARTESIAN_POINT('Ctrl Pts',(-0.596566509032947,-2.67829369088479,
12.5061871075061));
#439137=CARTESIAN_POINT('Ctrl Pts',(-0.597782912656175,-2.67811655007494,
12.5063648335164));
#439138=CARTESIAN_POINT('Ctrl Pts',(-0.598335478212733,-2.67803608179261,
12.5064455676329));
#439139=CARTESIAN_POINT('Ctrl Pts',(-0.598885690899769,-2.67794084943099,
12.506574497099));
#439140=CARTESIAN_POINT('Ctrl Pts',(-0.599409780011249,-2.67783390071578,
12.5067492519495));
#439141=CARTESIAN_POINT('Ctrl Pts',(-0.600462957424485,-2.67761898312111,
12.5071004286051));
#439142=CARTESIAN_POINT('Ctrl Pts',(-0.601449201390686,-2.67734805838752,
12.5076537929613));
#439143=CARTESIAN_POINT('Ctrl Pts',(-0.602296994582825,-2.67705058141408,
12.5083435010505));
#439144=CARTESIAN_POINT('Ctrl Pts',(-0.60235036823071,-2.67703185346087,
12.5083869222964));
#439145=CARTESIAN_POINT('Ctrl Pts',(-0.602403195004169,-2.67701300696501,
12.5084308732337));
#439146=CARTESIAN_POINT('Ctrl Pts',(-0.60245545821059,-2.6769940439138,
12.5084753333615));
#439147=CARTESIAN_POINT('Ctrl Pts',(-0.602874678107263,-2.67684193521421,
12.5088319622689));
#439148=CARTESIAN_POINT('Ctrl Pts',(-0.603266588089933,-2.6766804518268,
12.509227847131));
#439149=CARTESIAN_POINT('Ctrl Pts',(-0.603620601365606,-2.67651698438931,
12.5096423454524));
#439150=CARTESIAN_POINT('Ctrl Pts',(-0.604729922291853,-2.67600474978787,
12.5109411997424));
#439151=CARTESIAN_POINT('Ctrl Pts',(-0.605539412171032,-2.6754503057193,
12.5124831113042));
#439152=CARTESIAN_POINT('Ctrl Pts',(-0.606129412512988,-2.67490366317433,
12.5140723025008));
#439153=CARTESIAN_POINT('Ctrl Pts',(-0.606184696191238,-2.67485244216915,
12.5142212114565));
#439154=CARTESIAN_POINT('Ctrl Pts',(-0.60623808180628,-2.67480129547157,
12.5143705582413));
#439155=CARTESIAN_POINT('Ctrl Pts',(-0.606289651733421,-2.67475026906041,
12.5145201959299));
#439156=CARTESIAN_POINT('Ctrl Pts',(-0.606952144227129,-2.67409475883863,
12.5164425148273));
#439157=CARTESIAN_POINT('Ctrl Pts',(-0.607345241773047,-2.67344427279055,
12.518463520594));
#439158=CARTESIAN_POINT('Ctrl Pts',(-0.6075591507324,-2.67279970026717,
12.5205025929157));
#439159=CARTESIAN_POINT('Ctrl Pts',(-0.607683226407384,-2.67242582265514,
12.5216853356836));
#439160=CARTESIAN_POINT('Ctrl Pts',(-0.607747249614855,-2.672054762305,
12.5228750347131));
#439161=CARTESIAN_POINT('Ctrl Pts',(-0.607768422805009,-2.67169260274821,
12.5240609649613));
#439162=CARTESIAN_POINT('Ctrl Pts',(-0.607820391264341,-2.67080370154528,
12.5269717671327));
#439163=CARTESIAN_POINT('Ctrl Pts',(-0.607605302655558,-2.66994279743996,
12.5299036066169));
#439164=CARTESIAN_POINT('Ctrl Pts',(-0.607209513689908,-2.66910267648389,
12.5328133004019));
#439165=CARTESIAN_POINT('Ctrl Pts',(-0.607019511940296,-2.6686993695062,
12.5342101228452));
#439166=CARTESIAN_POINT('Ctrl Pts',(-0.606787629694283,-2.66830157869353,
12.5356023438238));
#439167=CARTESIAN_POINT('Ctrl Pts',(-0.60652158241518,-2.66791168735621,
12.5369868989719));
#439168=CARTESIAN_POINT('Origin',(-7.79562337705996,-13.1941084893106,-1.24176179718076));
#439169=CARTESIAN_POINT('Ctrl Pts',(-0.50182809689576,-2.6895309816888,
12.5369868989719));
#439170=CARTESIAN_POINT('Ctrl Pts',(-0.49894789389784,-2.7045970938076,
12.5369868989719));
#439171=CARTESIAN_POINT('Ctrl Pts',(-0.483815219891114,-2.70710417998317,
12.5369868989719));
#439172=CARTESIAN_POINT('Ctrl Pts',(-0.500854410604185,-2.69462390438445,
12.5218025310016));
#439173=CARTESIAN_POINT('Ctrl Pts',(-0.495467014549673,-2.70514207092888,
12.5216901060418));
#439174=CARTESIAN_POINT('Ctrl Pts',(-0.483861351992054,-2.70709655382362,
12.5161920673678));
#439175=CARTESIAN_POINT('Ctrl Pts',(-0.505003168253044,-2.69899699038481,
12.5042015548894));
#439176=CARTESIAN_POINT('Ctrl Pts',(-0.501057993818192,-2.70407763440851,
12.4980677368513));
#439177=CARTESIAN_POINT('Ctrl Pts',(-0.494374261000064,-2.70530990683761,
12.4907278922777));
#439178=CARTESIAN_POINT('Ctrl Pts',(-0.51742101318441,-2.69430272772006,
12.506463626192));
#439179=CARTESIAN_POINT('Ctrl Pts',(-0.518654950118071,-2.70072805557008,
12.4999376786891));
#439180=CARTESIAN_POINT('Ctrl Pts',(-0.51863987937257,-2.70064957953281,
12.4906970594712));
#439181=CARTESIAN_POINT('Origin',(-0.480219412770034,-2.68540002897125,
12.5369868989719));
#439182=CARTESIAN_POINT('Origin',(-0.480219412770034,-2.68540002897125,
14.));
#439183=CARTESIAN_POINT('Origin',(-0.480219412770035,-2.68540002897125,
13.7435492065112));
#439184=CARTESIAN_POINT('Ctrl Pts',(-0.506515595222954,-2.66526120222706,
13.793642941384));
#439185=CARTESIAN_POINT('Ctrl Pts',(-0.504491922906485,-2.67588245306495,
13.8071662555867));
#439186=CARTESIAN_POINT('Ctrl Pts',(-0.487476079996624,-2.67518929096144,
13.8103758687955));
#439187=CARTESIAN_POINT('Ctrl Pts',(-0.50336363189204,-2.68158072527108,
13.7804579775006));
#439188=CARTESIAN_POINT('Ctrl Pts',(-0.500856641562832,-2.69468449080693,
13.7901904343351));
#439189=CARTESIAN_POINT('Ctrl Pts',(-0.485217220963456,-2.69659876546848,
13.7927914348262));
#439190=CARTESIAN_POINT('Ctrl Pts',(-0.50150795242008,-2.69118864265259,
13.7597120340895));
#439191=CARTESIAN_POINT('Ctrl Pts',(-0.498601030277574,-2.70635231284253,
13.7635825532445));
#439192=CARTESIAN_POINT('Ctrl Pts',(-0.4838597530705,-2.7092212259552,13.7651073818885));
#439193=CARTESIAN_POINT('Ctrl Pts',(-0.501871336950118,-2.68930719243286,
13.7381884353898));
#439194=CARTESIAN_POINT('Ctrl Pts',(-0.499033339494265,-2.70411609789771,
13.7368803041982));
#439195=CARTESIAN_POINT('Ctrl Pts',(-0.484125094223456,-2.70674932027047,
13.7363986145813));
#439196=CARTESIAN_POINT('Origin',(-0.48415000549655,-2.66504911425252,13.7902182540695));
#439197=CARTESIAN_POINT('Ctrl Pts',(-0.512534251283801,-2.63409933487053,
13.8235227101244));
#439198=CARTESIAN_POINT('Ctrl Pts',(-0.510358343330453,-2.64538862682787,
13.8358800583119));
#439199=CARTESIAN_POINT('Ctrl Pts',(-0.493787321992115,-2.64522339710559,
13.8390832900376));
#439200=CARTESIAN_POINT('Ctrl Pts',(-0.510272350612621,-2.64581048146887,
13.8124254819053));
#439201=CARTESIAN_POINT('Ctrl Pts',(-0.508092216803741,-2.65712169701854,
13.8247886449158));
#439202=CARTESIAN_POINT('Ctrl Pts',(-0.49150042722439,-2.65693921508178,
13.8279860620657));
#439203=CARTESIAN_POINT('Ctrl Pts',(-0.508011463651739,-2.65751637951236,
13.8013225099955));
#439204=CARTESIAN_POINT('Ctrl Pts',(-0.505828134628754,-2.66884418195635,
13.8136962257787));
#439205=CARTESIAN_POINT('Ctrl Pts',(-0.48921485721179,-2.66864966113977,
13.8168830918626));
#439206=CARTESIAN_POINT('Ctrl Pts',(-0.505751550959262,-2.6692172332141,
13.7902140179785));
#439207=CARTESIAN_POINT('Ctrl Pts',(-0.503565990000837,-2.68055663464635,
13.802602731458));
#439208=CARTESIAN_POINT('Ctrl Pts',(-0.486930561707674,-2.68035494670785,
13.8057746032558));
#439209=CARTESIAN_POINT('Origin',(-0.490932708181089,-2.62993120367267,
13.8235269408515));
#439210=CARTESIAN_POINT('Ctrl Pts',(-0.574679115658286,-2.62124668345172,
13.8235269408515));
#439211=CARTESIAN_POINT('Ctrl Pts',(-0.581334330980055,-2.6309998740995,
13.8362179249168));
#439212=CARTESIAN_POINT('Ctrl Pts',(-0.596812372087366,-2.6237823088911,
13.8391868794938));
#439213=CARTESIAN_POINT('Ctrl Pts',(-0.568589883323139,-2.61232293854011,
13.8400110824519));
#439214=CARTESIAN_POINT('Ctrl Pts',(-0.57675154406485,-2.61821438630772,
13.8494522556836));
#439215=CARTESIAN_POINT('Ctrl Pts',(-0.586698405882847,-2.6091596733134,
13.85569149686));
#439216=CARTESIAN_POINT('Ctrl Pts',(-0.554703493556176,-2.60380437614469,
13.8586819406588));
#439217=CARTESIAN_POINT('Ctrl Pts',(-0.558969862482477,-2.60293596390406,
13.868010383617));
#439218=CARTESIAN_POINT('Ctrl Pts',(-0.563570379861988,-2.59514313985668,
13.8744918421245));
#439219=CARTESIAN_POINT('Ctrl Pts',(-0.524051565732569,-2.61009173001124,
13.8587686893867));
#439220=CARTESIAN_POINT('Ctrl Pts',(-0.519823156218783,-2.6109523582141,
13.8680909899357));
#439221=CARTESIAN_POINT('Ctrl Pts',(-0.512544438437598,-2.60561225812444,
13.8745789365163));
#439222=CARTESIAN_POINT('Ctrl Pts',(-0.514585541916014,-2.62347864022474,
13.8400379222776));
#439223=CARTESIAN_POINT('Ctrl Pts',(-0.509426554028352,-2.63211895722606,
13.8494748685453));
#439224=CARTESIAN_POINT('Ctrl Pts',(-0.496708995412886,-2.62775721352352,
13.8557104837033));
#439225=CARTESIAN_POINT('Ctrl Pts',(-0.512533505576834,-2.6341031997869,
13.8235269408542));
#439226=CARTESIAN_POINT('Ctrl Pts',(-0.510294379810855,-2.64569642774958,
13.8362179249195));
#439227=CARTESIAN_POINT('Ctrl Pts',(-0.493223091178564,-2.64521258016071,
13.8391868794964));
#439228=CARTESIAN_POINT('Origin',(-0.592851508704073,-2.60884651688069,
13.8235269408515));
#439229=CARTESIAN_POINT('Ctrl Pts',(-0.594836702480581,-2.65078754258225,
13.7902140241683));
#439230=CARTESIAN_POINT('Ctrl Pts',(-0.601342040951324,-2.66032898727232,
13.8026027327198));
#439231=CARTESIAN_POINT('Ctrl Pts',(-0.61653194602864,-2.65354336158153,
13.8057746032556));
#439232=CARTESIAN_POINT('Ctrl Pts',(-0.588119703459966,-2.64094380818014,
13.8013225161808));
#439233=CARTESIAN_POINT('Ctrl Pts',(-0.594618391022464,-2.65047549154932,
13.8136962270464));
#439234=CARTESIAN_POINT('Ctrl Pts',(-0.609790807176059,-2.64370523355015,
13.8168830918628));
#439235=CARTESIAN_POINT('Ctrl Pts',(-0.581399808680621,-2.63109583005556,
13.8124254880875));
#439236=CARTESIAN_POINT('Ctrl Pts',(-0.587888982059299,-2.64061355582919,
13.8247886461868));
#439237=CARTESIAN_POINT('Ctrl Pts',(-0.603046450886306,-2.63386287431128,
13.8279860620656));
#439238=CARTESIAN_POINT('Ctrl Pts',(-0.574676900910916,-2.62124343640604,
13.8235227163066));
#439239=CARTESIAN_POINT('Ctrl Pts',(-0.581153496605596,-2.63074271487572,
13.8358800595847));
#439240=CARTESIAN_POINT('Ctrl Pts',(-0.596298747147209,-2.62401610972678,
13.8390832900376));
#439241=CARTESIAN_POINT('Origin',(-0.613011317284678,-2.63839063333718,
13.7902182540695));
#439242=CARTESIAN_POINT('Ctrl Pts',(-0.606369500303375,-2.66768876270811,
13.7382347919292));
#439243=CARTESIAN_POINT('Ctrl Pts',(-0.614855234269111,-2.68016715153825,
13.7369371795943));
#439244=CARTESIAN_POINT('Ctrl Pts',(-0.629594010822871,-2.67665827098757,
13.7364597369711));
#439245=CARTESIAN_POINT('Ctrl Pts',(-0.607435665510839,-2.66925122414269,
13.7595490285574));
#439246=CARTESIAN_POINT('Ctrl Pts',(-0.616124693214113,-2.68202677125392,
13.7633824266926));
#439247=CARTESIAN_POINT('Ctrl Pts',(-0.6308030328376,-2.67879567140946,
13.7648920890506));
#439248=CARTESIAN_POINT('Ctrl Pts',(-0.601998281355425,-2.66128275642936,
13.7803806590111));
#439249=CARTESIAN_POINT('Ctrl Pts',(-0.609509515461666,-2.67233618341856,
13.7901039518744));
#439250=CARTESIAN_POINT('Ctrl Pts',(-0.624636074984075,-2.66790079860536,
13.7926933640892));
#439251=CARTESIAN_POINT('Ctrl Pts',(-0.592546893980175,-2.64743178071439,
13.7936647693663));
#439252=CARTESIAN_POINT('Ctrl Pts',(-0.598618158232228,-2.65638237188629,
13.8072068914933));
#439253=CARTESIAN_POINT('Ctrl Pts',(-0.613974193817631,-2.64897720875863,
13.8104111085397));
#439254=CARTESIAN_POINT('Origin',(-0.624693975460967,-2.65551152078517,
13.7435492065112));
#439255=CARTESIAN_POINT('Origin',(-0.624693975460967,-2.65551152078517,
14.));
#439256=CARTESIAN_POINT('Origin',(-0.624693975460967,-2.65551152078517,
12.5369868989719));
#439257=CARTESIAN_POINT('Ctrl Pts',(-0.594078713948304,-2.67844564110547,
12.506462012331));
#439258=CARTESIAN_POINT('Ctrl Pts',(-0.595494570650946,-2.68482913057342,
12.4999388158272));
#439259=CARTESIAN_POINT('Ctrl Pts',(-0.595477819209372,-2.68475360552158,
12.4907030323752));
#439260=CARTESIAN_POINT('Ctrl Pts',(-0.607339333701184,-2.67782552262988,
12.5042014951932));
#439261=CARTESIAN_POINT('Ctrl Pts',(-0.612973609332226,-2.68092326942868,
12.4980716682127));
#439262=CARTESIAN_POINT('Ctrl Pts',(-0.619593324702907,-2.67940506863922,
12.4907355092743));
#439263=CARTESIAN_POINT('Ctrl Pts',(-0.609414332117057,-2.6721668935716,
12.5218047446509));
#439264=CARTESIAN_POINT('Ctrl Pts',(-0.618529083026261,-2.67967956199229,
12.5216906929434));
#439265=CARTESIAN_POINT('Ctrl Pts',(-0.629952685569496,-2.67687384296435,
12.5161988840776));
#439266=CARTESIAN_POINT('Ctrl Pts',(-0.606499957111761,-2.66787993605588,
12.5369868989719));
#439267=CARTESIAN_POINT('Ctrl Pts',(-0.615118431985925,-2.68055776798267,
12.5369868989719));
#439268=CARTESIAN_POINT('Ctrl Pts',(-0.629996401635299,-2.67686296749648,
12.5369868989719));
#439269=CARTESIAN_POINT('Origin',(-1.04370312006722E-31,-1.01968969974689E-30,
12.5));
#439270=CARTESIAN_POINT('Origin',(-0.359110979140358,-2.65936638433693,
12.5));
#439271=CARTESIAN_POINT('',(-0.359110979140358,-2.65936638433693,12.5893111709658));
#439272=CARTESIAN_POINT('',(-0.359110979140358,-2.65936638433693,13.8235269408515));
#439273=CARTESIAN_POINT('',(-0.359110979140358,-2.65936638433693,12.5));
#439274=CARTESIAN_POINT('',(-0.376795587855578,-2.69045540673699,13.7902182540695));
#439275=CARTESIAN_POINT('',(-0.359110979140358,-2.65936638433693,13.8235269408515));
#439276=CARTESIAN_POINT('',(-0.38704386168096,-2.70847157094225,13.7435492065112));
#439277=CARTESIAN_POINT('Origin',(-0.353326893110259,-2.64919878991666,
13.744521291872));
#439278=CARTESIAN_POINT('',(-0.38704386168096,-2.70847157094225,12.5369868989719));
#439279=CARTESIAN_POINT('',(-0.38704386168096,-2.70847157094225,12.5));
#439280=CARTESIAN_POINT('Ctrl Pts',(-0.38704386168096,-2.70847157094225,
12.5369868989719));
#439281=CARTESIAN_POINT('Ctrl Pts',(-0.377739691682629,-2.6921151135193,
12.5544431401645));
#439282=CARTESIAN_POINT('Ctrl Pts',(-0.368428867094625,-2.67574695752327,
12.5718848856037));
#439283=CARTESIAN_POINT('Ctrl Pts',(-0.359110979140358,-2.65936638433693,
12.5893111709658));
#439284=CARTESIAN_POINT('Origin',(-0.222139482233007,-2.93197550397874,
12.5));
#439285=CARTESIAN_POINT('',(-0.280925356007091,-2.72152570184806,13.7435492065112));
#439286=CARTESIAN_POINT('',(-0.286501658488811,-2.70156288291627,13.7902182540695));
#439287=CARTESIAN_POINT('Origin',(-0.301155217631046,-2.6491040450355,13.7418732680457));
#439288=CARTESIAN_POINT('',(-0.296124228020734,-2.66711467752318,13.8235269408515));
#439289=CARTESIAN_POINT('',(-0.286501658488811,-2.70156288291627,13.7902182540695));
#439290=CARTESIAN_POINT('',(-0.296124228020734,-2.66711467752318,12.5893111709658));
#439291=CARTESIAN_POINT('',(-0.296124228020734,-2.66711467752318,12.5));
#439292=CARTESIAN_POINT('',(-0.280925356007091,-2.72152570184806,12.5369868989719));
#439293=CARTESIAN_POINT('Ctrl Pts',(-0.296124228020734,-2.66711467752318,
12.5893111709658));
#439294=CARTESIAN_POINT('Ctrl Pts',(-0.291054168163914,-2.68526517908345,
12.5718848856037));
#439295=CARTESIAN_POINT('Ctrl Pts',(-0.285987951634028,-2.70340192177036,
12.5544431401645));
#439296=CARTESIAN_POINT('Ctrl Pts',(-0.280925356007091,-2.72152570184806,
12.5369868989719));
#439297=CARTESIAN_POINT('',(-0.280925356007091,-2.72152570184806,12.5));
#439298=CARTESIAN_POINT('Origin',(-0.32923183132768,-2.67636277074664,12.5));
#439299=CARTESIAN_POINT('',(-0.326148325313847,-2.64212708522933,13.8587068136939));
#439300=CARTESIAN_POINT('Ctrl Pts',(-0.296124228014408,-2.66711467752126,
13.8235269408542));
#439301=CARTESIAN_POINT('Ctrl Pts',(-0.296595658364503,-2.66542698594632,
13.8262006681044));
#439302=CARTESIAN_POINT('Ctrl Pts',(-0.297245432058879,-2.6637466222422,
13.8288634856214));
#439303=CARTESIAN_POINT('Ctrl Pts',(-0.298060246146911,-2.66207450158807,
13.8314912288862));
#439304=CARTESIAN_POINT('Ctrl Pts',(-0.298900235427497,-2.66035071766492,
13.8342001611531));
#439305=CARTESIAN_POINT('Ctrl Pts',(-0.299916107457681,-2.65863356166973,
13.8368750301949));
#439306=CARTESIAN_POINT('Ctrl Pts',(-0.301138488540095,-2.65692417183499,
13.8394886372968));
#439307=CARTESIAN_POINT('Ctrl Pts',(-0.301232895996174,-2.65679215151165,
13.8396904925131));
#439308=CARTESIAN_POINT('Ctrl Pts',(-0.301328555213474,-2.65666018709877,
13.8398919674349));
#439309=CARTESIAN_POINT('Ctrl Pts',(-0.301425490142556,-2.65652828496087,
13.8400930404591));
#439310=CARTESIAN_POINT('Ctrl Pts',(-0.302935801552247,-2.65447316091299,
13.8432258934518));
#439311=CARTESIAN_POINT('Ctrl Pts',(-0.304747187891887,-2.65244297461327,
13.8462331177034));
#439312=CARTESIAN_POINT('Ctrl Pts',(-0.306872551871129,-2.65056816263354,
13.8489036603661));
#439313=CARTESIAN_POINT('Ctrl Pts',(-0.307567995699242,-2.64995470233548,
13.8497774930041));
#439314=CARTESIAN_POINT('Ctrl Pts',(-0.308296990066901,-2.64935811857066,
13.85061494757));
#439315=CARTESIAN_POINT('Ctrl Pts',(-0.309059786288148,-2.64878366609183,
13.8514076489583));
#439316=CARTESIAN_POINT('Ctrl Pts',(-0.31067321030777,-2.64756861625064,
13.8530843267192));
#439317=CARTESIAN_POINT('Ctrl Pts',(-0.312598118382892,-2.64633559110513,
13.8546805203176));
#439318=CARTESIAN_POINT('Ctrl Pts',(-0.314796386998666,-2.64527104992204,
13.8559412814274));
#439319=CARTESIAN_POINT('Ctrl Pts',(-0.315090586630988,-2.64512857978785,
13.8561100121513));
#439320=CARTESIAN_POINT('Ctrl Pts',(-0.315389612153481,-2.64498909641999,
13.8562727473908));
#439321=CARTESIAN_POINT('Ctrl Pts',(-0.315693307140336,-2.64485300775523,
13.8564289040185));
#439322=CARTESIAN_POINT('Ctrl Pts',(-0.317070560441086,-2.64423584721311,
13.8571370725437));
#439323=CARTESIAN_POINT('Ctrl Pts',(-0.318568985677268,-2.6436797319811,
13.8577210840553));
#439324=CARTESIAN_POINT('Ctrl Pts',(-0.320140550242359,-2.64323379260637,
13.8581177131616));
#439325=CARTESIAN_POINT('Ctrl Pts',(-0.320583156915499,-2.64310820072968,
13.8582294175695));
#439326=CARTESIAN_POINT('Ctrl Pts',(-0.321031483829118,-2.64299118971994,
13.8583265086086));
#439327=CARTESIAN_POINT('Ctrl Pts',(-0.321484281179541,-2.64288345463402,
13.8584082369006));
#439328=CARTESIAN_POINT('Ctrl Pts',(-0.322134829549688,-2.64272866820585,
13.8585256585398));
#439329=CARTESIAN_POINT('Ctrl Pts',(-0.322802768481298,-2.64259141932814,
13.8586122832068));
#439330=CARTESIAN_POINT('Ctrl Pts',(-0.323470905801753,-2.64247604685465,
13.8586682984299));
#439331=CARTESIAN_POINT('Ctrl Pts',(-0.324005349427795,-2.64238376031236,
13.8587131050557));
#439332=CARTESIAN_POINT('Ctrl Pts',(-0.324545783025643,-2.6423042208311,
13.8587357943552));
#439333=CARTESIAN_POINT('Ctrl Pts',(-0.325092344556493,-2.64223792000778,
13.8587355499465));
#439334=CARTESIAN_POINT('Ctrl Pts',(-0.325445600304463,-2.64219506820499,
13.8587353919793));
#439335=CARTESIAN_POINT('Ctrl Pts',(-0.325797591184218,-2.64215817164918,
13.8587257282814));
#439336=CARTESIAN_POINT('Ctrl Pts',(-0.326148325313847,-2.64212708522933,
13.8587068136939));
#439337=CARTESIAN_POINT('Ctrl Pts',(-0.326148325313847,-2.64212708522933,
13.8587068136939));
#439338=CARTESIAN_POINT('Ctrl Pts',(-0.327301870745918,-2.64202484368912,
13.8586446046466));
#439339=CARTESIAN_POINT('Ctrl Pts',(-0.328441839233545,-2.64198537378024,
13.858482427929));
#439340=CARTESIAN_POINT('Ctrl Pts',(-0.329568382475551,-2.64200420751158,
13.8582284286032));
#439341=CARTESIAN_POINT('Ctrl Pts',(-0.330724084796904,-2.64202352872909,
13.8579678548414));
#439342=CARTESIAN_POINT('Ctrl Pts',(-0.331868455352584,-2.64210578950569,
13.857615680862));
#439343=CARTESIAN_POINT('Ctrl Pts',(-0.332957072913103,-2.64223808203927,
13.8571944833187));
#439344=CARTESIAN_POINT('Ctrl Pts',(-0.335673829370046,-2.64256823158661,
13.8561433417727));
#439345=CARTESIAN_POINT('Ctrl Pts',(-0.338171014326103,-2.64322066342429,
13.8546163505474));
#439346=CARTESIAN_POINT('Ctrl Pts',(-0.34035655976158,-2.64401022532738,
13.8528973491086));
#439347=CARTESIAN_POINT('Ctrl Pts',(-0.340755826667932,-2.64415446663818,
13.8525833129072));
#439348=CARTESIAN_POINT('Ctrl Pts',(-0.341144796936879,-2.64430318880852,
13.8522628768812));
#439349=CARTESIAN_POINT('Ctrl Pts',(-0.341523058110627,-2.64445516393018,
13.851937733538));
#439350=CARTESIAN_POINT('Ctrl Pts',(-0.34383304661731,-2.64538325491252,
13.8499521282529));
#439351=CARTESIAN_POINT('Ctrl Pts',(-0.34597170175213,-2.646528679691,13.847639871647));
#439352=CARTESIAN_POINT('Ctrl Pts',(-0.347864555013669,-2.64776041635405,
13.8452109780794));
#439353=CARTESIAN_POINT('Ctrl Pts',(-0.348716188876148,-2.64831460017443,
13.8441181685877));
#439354=CARTESIAN_POINT('Ctrl Pts',(-0.34951864079009,-2.6488858268973,
13.8430021611332));
#439355=CARTESIAN_POINT('Ctrl Pts',(-0.350268262742234,-2.64946110341616,
13.8418824960098));
#439356=CARTESIAN_POINT('Ctrl Pts',(-0.352034766014743,-2.65081675722306,
13.8392439765549));
#439357=CARTESIAN_POINT('Ctrl Pts',(-0.35359464231439,-2.65225670586511,
13.8364981347964));
#439358=CARTESIAN_POINT('Ctrl Pts',(-0.354975228564488,-2.65375961259506,
13.8336931113419));
#439359=CARTESIAN_POINT('Ctrl Pts',(-0.35631983189675,-2.65522334830663,
13.8309611966328));
#439360=CARTESIAN_POINT('Ctrl Pts',(-0.357495300980898,-2.6567486516762,
13.8281701127186));
#439361=CARTESIAN_POINT('Ctrl Pts',(-0.358490259217353,-2.65833004640473,
13.8253580685121));
#439362=CARTESIAN_POINT('Ctrl Pts',(-0.358705967236808,-2.65867289448857,
13.8247484142933));
#439363=CARTESIAN_POINT('Ctrl Pts',(-0.358913017654098,-2.65901837386185,
13.8241378483365));
#439364=CARTESIAN_POINT('Ctrl Pts',(-0.359110979140358,-2.65936638433693,
13.8235269408515));
#439365=CARTESIAN_POINT('',(-0.324913457451728,-2.64226079469317,12.5969504640361));
#439366=CARTESIAN_POINT('Origin',(-0.329236065209537,-2.67639558472314,
12.584524458991));
#439367=CARTESIAN_POINT('Origin',(-0.329236065209537,-2.67639558472314,
12.584524458991));
#439368=CARTESIAN_POINT('Ctrl Pts',(-0.296124228020734,-2.66711467752318,
12.5893111709658));
#439369=CARTESIAN_POINT('Ctrl Pts',(-0.2991734647528,-2.65619859810282,
12.5770542771492));
#439370=CARTESIAN_POINT('Ctrl Pts',(-0.31547929129419,-2.65758557166315,
12.5737548217797));
#439371=CARTESIAN_POINT('Ctrl Pts',(-0.289456570641965,-2.69098447967037,
12.5663937883685));
#439372=CARTESIAN_POINT('Ctrl Pts',(-0.292509697098965,-2.68005447527472,
12.5540940315304));
#439373=CARTESIAN_POINT('Ctrl Pts',(-0.308865779929059,-2.6814489464175,
12.5508374392248));
#439374=CARTESIAN_POINT('Ctrl Pts',(-0.282795640847762,-2.71483019747978,
12.5434499600945));
#439375=CARTESIAN_POINT('Ctrl Pts',(-0.285858694106043,-2.70386465574756,
12.5311293540533));
#439376=CARTESIAN_POINT('Ctrl Pts',(-0.302257593095427,-2.70528869103514,
12.5278936106989));
#439377=CARTESIAN_POINT('Ctrl Pts',(-0.276140911657195,-2.73865371751063,
12.5204817579905));
#439378=CARTESIAN_POINT('Ctrl Pts',(-0.279219124935868,-2.72763390384074,
12.5081597038247));
#439379=CARTESIAN_POINT('Ctrl Pts',(-0.295654303598946,-2.72910663844256,
12.5049254088044));
#439380=CARTESIAN_POINT('Ctrl Pts',(-0.280925356007091,-2.72152570184806,
12.5369868989719));
#439381=CARTESIAN_POINT('Ctrl Pts',(-0.280674748363148,-2.7224228623574,
12.5342545179733));
#439382=CARTESIAN_POINT('Ctrl Pts',(-0.280555726584263,-2.72331263251285,
12.5314872231885));
#439383=CARTESIAN_POINT('Ctrl Pts',(-0.28063040273863,-2.72415230184187,
12.5287124745062));
#439384=CARTESIAN_POINT('Ctrl Pts',(-0.280697749401231,-2.72490955732024,
12.5262100684184));
#439385=CARTESIAN_POINT('Ctrl Pts',(-0.280923548754504,-2.72562521295656,
12.5237004536639));
#439386=CARTESIAN_POINT('Ctrl Pts',(-0.281374896467423,-2.72629161059571,
12.5212220730815));
#439387=CARTESIAN_POINT('Ctrl Pts',(-0.281720442186355,-2.72680179563647,
12.5193246583486));
#439388=CARTESIAN_POINT('Ctrl Pts',(-0.282202842096404,-2.72728885102334,
12.517417831369));
#439389=CARTESIAN_POINT('Ctrl Pts',(-0.282903321380209,-2.7276993305922,
12.5155812248348));
#439390=CARTESIAN_POINT('Ctrl Pts',(-0.283201729320206,-2.72787419709488,
12.5147988205793));
#439391=CARTESIAN_POINT('Ctrl Pts',(-0.283539877298099,-2.7280355830973,
12.5140295443047));
#439392=CARTESIAN_POINT('Ctrl Pts',(-0.283924191219537,-2.72818147882248,
12.5132817086137));
#439393=CARTESIAN_POINT('Ctrl Pts',(-0.284505798350819,-2.72840227226621,
12.5121499604604));
#439394=CARTESIAN_POINT('Ctrl Pts',(-0.285208235681259,-2.72858567050411,
12.5110494206568));
#439395=CARTESIAN_POINT('Ctrl Pts',(-0.286052005216699,-2.7287005838835,
12.5100666561695));
#439396=CARTESIAN_POINT('Ctrl Pts',(-0.286536495740919,-2.72876656688133,
12.509502355064));
#439397=CARTESIAN_POINT('Ctrl Pts',(-0.287073269844165,-2.72881008581394,
12.5089719619137));
#439398=CARTESIAN_POINT('Ctrl Pts',(-0.287652782419591,-2.72882395887686,
12.5085043804652));
#439399=CARTESIAN_POINT('Ctrl Pts',(-0.288500823586905,-2.72884426029734,
12.5078201359221));
#439400=CARTESIAN_POINT('Ctrl Pts',(-0.289465012034477,-2.72880045789742,
12.5072563000949));
#439401=CARTESIAN_POINT('Ctrl Pts',(-0.290479605800433,-2.72868706355689,
12.5068768744332));
#439402=CARTESIAN_POINT('Ctrl Pts',(-0.291211197750561,-2.72860529843127,
12.5066032824114));
#439403=CARTESIAN_POINT('Ctrl Pts',(-0.2919818570955,-2.72848597284837,
12.5064197834844));
#439404=CARTESIAN_POINT('Ctrl Pts',(-0.292748943732452,-2.72833830467749,
12.5063282718343));
#439405=CARTESIAN_POINT('Ctrl Pts',(-0.293868652738381,-2.72812275486491,
12.5061946931565));
#439406=CARTESIAN_POINT('Ctrl Pts',(-0.295004882629896,-2.72784325153112,
12.5062515701262));
#439407=CARTESIAN_POINT('Ctrl Pts',(-0.296090811003642,-2.72753215799887,
12.5064436508398));
#439408=CARTESIAN_POINT('',(-0.31547929129419,-2.65758557166315,12.5737548217797));
#439409=CARTESIAN_POINT('Origin',(-0.31731309413718,-2.6730334571862,12.5893111709658));
#439410=CARTESIAN_POINT('Ctrl Pts',(-0.296090811003642,-2.72753215799887,
12.5064436508398));
#439411=CARTESIAN_POINT('Ctrl Pts',(-0.298961272795007,-2.71717837430133,
12.5164271754438));
#439412=CARTESIAN_POINT('Ctrl Pts',(-0.301832671095516,-2.70682043054686,
12.5264061185523));
#439413=CARTESIAN_POINT('Ctrl Pts',(-0.304705039800327,-2.69645818047462,
12.536380305637));
#439414=CARTESIAN_POINT('Ctrl Pts',(-0.308294918102195,-2.68350746957508,
12.5488460165097));
#439415=CARTESIAN_POINT('Ctrl Pts',(-0.311886313205838,-2.67055002840516,
12.5613043021964));
#439416=CARTESIAN_POINT('Ctrl Pts',(-0.31547929129419,-2.65758557166315,
12.5737548217797));
#439417=CARTESIAN_POINT('Ctrl Pts',(-0.359110979140358,-2.65936638433693,
12.5893111709658));
#439418=CARTESIAN_POINT('Ctrl Pts',(-0.353507012517122,-2.64951477570456,
12.5770542771492));
#439419=CARTESIAN_POINT('Ctrl Pts',(-0.338023477934023,-2.65481230641886,
12.5737548217797));
#439420=CARTESIAN_POINT('Ctrl Pts',(-0.353882527021608,-2.6501749191677,
12.5928319619712));
#439421=CARTESIAN_POINT('Ctrl Pts',(-0.347284647692764,-2.64516478895648,
12.5821634970842));
#439422=CARTESIAN_POINT('Ctrl Pts',(-0.336127083743247,-2.651459411186,
12.5773203894503));
#439423=CARTESIAN_POINT('Ctrl Pts',(-0.34028227804391,-2.64039650789161,
12.5969440695591));
#439424=CARTESIAN_POINT('Ctrl Pts',(-0.336290393023035,-2.6408691563149,
12.5878292599214));
#439425=CARTESIAN_POINT('Ctrl Pts',(-0.331278483118768,-2.64797584705111,
12.5813877129824));
#439426=CARTESIAN_POINT('Ctrl Pts',(-0.309907671639785,-2.64407869899691,
12.596957478804));
#439427=CARTESIAN_POINT('Ctrl Pts',(-0.313870064984958,-2.64360962317464,
12.5878468778671));
#439428=CARTESIAN_POINT('Ctrl Pts',(-0.320407708303931,-2.64929967605414,
12.5814011370086));
#439429=CARTESIAN_POINT('Ctrl Pts',(-0.298973270177215,-2.65691528233498,
12.5928371701607));
#439430=CARTESIAN_POINT('Ctrl Pts',(-0.304161181208116,-2.65046387591163,
12.5821692192952));
#439431=CARTESIAN_POINT('Ctrl Pts',(-0.316509573340324,-2.65386108560742,
12.5773318885715));
#439432=CARTESIAN_POINT('Ctrl Pts',(-0.296124228020682,-2.66711467752316,
12.5893111709658));
#439433=CARTESIAN_POINT('Ctrl Pts',(-0.299173464752748,-2.6561985981028,
12.5770542771492));
#439434=CARTESIAN_POINT('Ctrl Pts',(-0.315479291294137,-2.65758557166314,
12.5737548217797));
#439435=CARTESIAN_POINT('',(-0.338023477934023,-2.65481230641886,12.5737548217797));
#439436=CARTESIAN_POINT('Origin',(-0.339988324540244,-2.67024407163915,
12.5893111709658));
#439437=CARTESIAN_POINT('Ctrl Pts',(-0.315479291294137,-2.65758557166314,
12.5737548217797));
#439438=CARTESIAN_POINT('Ctrl Pts',(-0.315717282877971,-2.65661208327746,
12.5746934679442));
#439439=CARTESIAN_POINT('Ctrl Pts',(-0.316158580278691,-2.65557835602022,
12.5756680099006));
#439440=CARTESIAN_POINT('Ctrl Pts',(-0.316749913775715,-2.65460069127028,
12.5765688348656));
#439441=CARTESIAN_POINT('Ctrl Pts',(-0.316906462772773,-2.65434186535084,
12.5768073183026));
#439442=CARTESIAN_POINT('Ctrl Pts',(-0.317073281567976,-2.65408689315674,
12.5770407398754));
#439443=CARTESIAN_POINT('Ctrl Pts',(-0.317248902279859,-2.65383763724717,
12.5772674179684));
#439444=CARTESIAN_POINT('Ctrl Pts',(-0.31796960219159,-2.6528147583959,
12.5781976435658));
#439445=CARTESIAN_POINT('Ctrl Pts',(-0.318888686636697,-2.65183654509322,
12.5790594849312));
#439446=CARTESIAN_POINT('Ctrl Pts',(-0.319979290249667,-2.65100211326074,
12.5797571720116));
#439447=CARTESIAN_POINT('Ctrl Pts',(-0.320689857718127,-2.65045845091839,
12.580211740231));
#439448=CARTESIAN_POINT('Ctrl Pts',(-0.32151693397986,-2.64996602646976,
12.5806009430798));
#439449=CARTESIAN_POINT('Ctrl Pts',(-0.322411359859084,-2.64957472733751,
12.5808812374708));
#439450=CARTESIAN_POINT('Ctrl Pts',(-0.323179968412034,-2.64923847157078,
12.5811221033394));
#439451=CARTESIAN_POINT('Ctrl Pts',(-0.324014092571948,-2.64897011241116,
12.581287365893));
#439452=CARTESIAN_POINT('Ctrl Pts',(-0.324869206662944,-2.64879273379116,
12.581359338449));
#439453=CARTESIAN_POINT('Ctrl Pts',(-0.32498804986416,-2.64876808182571,
12.5813693411482));
#439454=CARTESIAN_POINT('Ctrl Pts',(-0.325107306565449,-2.64874512784228,
12.5813775999465));
#439455=CARTESIAN_POINT('Ctrl Pts',(-0.325226866588446,-2.64872387318194,
12.5813841266931));
#439456=CARTESIAN_POINT('Ctrl Pts',(-0.325429714627947,-2.64868781207998,
12.5813952001081));
#439457=CARTESIAN_POINT('Ctrl Pts',(-0.325634900935537,-2.64865700047033,
12.5814007534795));
#439458=CARTESIAN_POINT('Ctrl Pts',(-0.325842365431365,-2.6486316467957,
12.5814005856065));
#439459=CARTESIAN_POINT('Ctrl Pts',(-0.326792056779908,-2.64851558758589,
12.5813998171494));
#439460=CARTESIAN_POINT('Ctrl Pts',(-0.327723829115703,-2.64852158049257,
12.58127954464));
#439461=CARTESIAN_POINT('Ctrl Pts',(-0.328632582749688,-2.64862000274537,
12.5810700125799));
#439462=CARTESIAN_POINT('Ctrl Pts',(-0.329730253669656,-2.64873888562049,
12.5808169217085));
#439463=CARTESIAN_POINT('Ctrl Pts',(-0.330792637743183,-2.64900927134455,
12.5804173076348));
#439464=CARTESIAN_POINT('Ctrl Pts',(-0.331733052660859,-2.64938222596681,
12.5799304713245));
#439465=CARTESIAN_POINT('Ctrl Pts',(-0.33289852300511,-2.64984443423661,
12.5793271277669));
#439466=CARTESIAN_POINT('Ctrl Pts',(-0.33396082769394,-2.65046291750759,
12.5785808224116));
#439467=CARTESIAN_POINT('Ctrl Pts',(-0.334891146747424,-2.651184195763,
12.5777485681082));
#439468=CARTESIAN_POINT('Ctrl Pts',(-0.336277424061175,-2.6522589793855,
12.576508418016));
#439469=CARTESIAN_POINT('Ctrl Pts',(-0.337363175010326,-2.65354753066006,
12.5750928681475));
#439470=CARTESIAN_POINT('Ctrl Pts',(-0.338023477934023,-2.65481230641886,
12.5737548217797));
#439471=CARTESIAN_POINT('Ctrl Pts',(-0.338023477934023,-2.65481230641886,
12.5737548217797));
#439472=CARTESIAN_POINT('Ctrl Pts',(-0.353507012517122,-2.64951477570456,
12.5770542771492));
#439473=CARTESIAN_POINT('Ctrl Pts',(-0.359110979140358,-2.65936638433693,
12.5893111709658));
#439474=CARTESIAN_POINT('Ctrl Pts',(-0.350221549893586,-2.67635811795242,
12.5508408821982));
#439475=CARTESIAN_POINT('Ctrl Pts',(-0.365752016580534,-2.67104113298767,
12.55409748406));
#439476=CARTESIAN_POINT('Ctrl Pts',(-0.371363132429934,-2.68090530974955,
12.5663972313419));
#439477=CARTESIAN_POINT('Ctrl Pts',(-0.362408732305296,-2.69788230083249,
12.52790050457));
#439478=CARTESIAN_POINT('Ctrl Pts',(-0.377973568546624,-2.69252626217299,
12.5311362602938));
#439479=CARTESIAN_POINT('Ctrl Pts',(-0.383602925310125,-2.70242250592573,
12.5434568539655));
#439480=CARTESIAN_POINT('Ctrl Pts',(-0.374585883477606,-2.71938652906053,
12.5049357605811));
#439481=CARTESIAN_POINT('Ctrl Pts',(-0.39017411317665,-2.71397446107877,
12.5081700652078));
#439482=CARTESIAN_POINT('Ctrl Pts',(-0.395831325850728,-2.72391967470371,
12.5204921097672));
#439483=CARTESIAN_POINT('Ctrl Pts',(-0.373786285379738,-2.71797447635903,
12.5064436508395));
#439484=CARTESIAN_POINT('Ctrl Pts',(-0.37500575514881,-2.71801620492121,
12.5062361689309));
#439485=CARTESIAN_POINT('Ctrl Pts',(-0.376275683314774,-2.7180075983115,
12.5061871075061));
#439486=CARTESIAN_POINT('Ctrl Pts',(-0.37750247807579,-2.71793019511092,
12.5063648335164));
#439487=CARTESIAN_POINT('Ctrl Pts',(-0.378059763928082,-2.71789503380278,
12.5064455676329));
#439488=CARTESIAN_POINT('Ctrl Pts',(-0.378615908149357,-2.71784496576091,
12.506574497099));
#439489=CARTESIAN_POINT('Ctrl Pts',(-0.379146970710706,-2.71778109103672,
12.5067492519495));
#439490=CARTESIAN_POINT('Ctrl Pts',(-0.380214161542032,-2.71765273229903,
12.5071004286051));
#439491=CARTESIAN_POINT('Ctrl Pts',(-0.381219206743642,-2.71746309708426,
12.5076537929612));
#439492=CARTESIAN_POINT('Ctrl Pts',(-0.382088426108788,-2.71723571295662,
12.5083435010503));
#439493=CARTESIAN_POINT('Ctrl Pts',(-0.382143148662405,-2.71722139776691,
12.5083869222963));
#439494=CARTESIAN_POINT('Ctrl Pts',(-0.3821973358236,-2.71720691985364,
12.5084308732336));
#439495=CARTESIAN_POINT('Ctrl Pts',(-0.38225097079332,-2.71719227983691,
12.5084753333615));
#439496=CARTESIAN_POINT('Ctrl Pts',(-0.382681194041496,-2.71707484757989,
12.508831962269));
#439497=CARTESIAN_POINT('Ctrl Pts',(-0.383084962371223,-2.71694584581703,
12.509227847131));
#439498=CARTESIAN_POINT('Ctrl Pts',(-0.383451121810638,-2.71681177767242,
12.5096423454524));
#439499=CARTESIAN_POINT('Ctrl Pts',(-0.384598503438387,-2.71639166744329,
12.5109411997424));
#439500=CARTESIAN_POINT('Ctrl Pts',(-0.385450492145566,-2.71590504918171,
12.5124831113042));
#439501=CARTESIAN_POINT('Ctrl Pts',(-0.386083085752253,-2.71540831604987,
12.5140723025008));
#439502=CARTESIAN_POINT('Ctrl Pts',(-0.38614236046606,-2.71536177161137,
12.5142212114565));
#439503=CARTESIAN_POINT('Ctrl Pts',(-0.386199737375547,-2.71531514652344,
12.5143705582413));
#439504=CARTESIAN_POINT('Ctrl Pts',(-0.386255294834225,-2.71526849332626,
12.5145201959299));
#439505=CARTESIAN_POINT('Ctrl Pts',(-0.386969013107346,-2.7146691635492,
12.5164425148273));
#439506=CARTESIAN_POINT('Ctrl Pts',(-0.387413823305344,-2.71405288303911,
12.518463520594));
#439507=CARTESIAN_POINT('Ctrl Pts',(-0.387679559144856,-2.71342789084365,
12.5205025929157));
#439508=CARTESIAN_POINT('Ctrl Pts',(-0.387833696464559,-2.71306537059791,
12.5216853356836));
#439509=CARTESIAN_POINT('Ctrl Pts',(-0.387927751503383,-2.71270076340624,
12.5228750347131));
#439510=CARTESIAN_POINT('Ctrl Pts',(-0.387978373607497,-2.71234153471706,
12.5240609649613));
#439511=CARTESIAN_POINT('Ctrl Pts',(-0.388102622846261,-2.71145982717144,
12.5269717671326));
#439512=CARTESIAN_POINT('Ctrl Pts',(-0.38795842160391,-2.71058425593512,
12.5299036066169));
#439513=CARTESIAN_POINT('Ctrl Pts',(-0.387632427250619,-2.7097146699372,
12.5328133004019));
#439514=CARTESIAN_POINT('Ctrl Pts',(-0.387475930978956,-2.70929721802372,
12.5342101228451));
#439515=CARTESIAN_POINT('Ctrl Pts',(-0.387277243946127,-2.70888185027142,
12.5356023438238));
#439516=CARTESIAN_POINT('Ctrl Pts',(-0.38704386168096,-2.70847157094225,
12.5369868989719));
#439517=CARTESIAN_POINT('Origin',(-6.69284171101566,-13.7831702063622,-1.23871760707945));
#439518=CARTESIAN_POINT('Ctrl Pts',(-0.28093656190616,-2.72148543785968,
12.5369868989719));
#439519=CARTESIAN_POINT('Ctrl Pts',(-0.276837914541471,-2.73626665545045,
12.5369868989719));
#439520=CARTESIAN_POINT('Ctrl Pts',(-0.261551242461182,-2.73753194608714,
12.5369868989719));
#439521=CARTESIAN_POINT('Ctrl Pts',(-0.279550994995317,-2.72648204980315,
12.5218025310016));
#439522=CARTESIAN_POINT('Ctrl Pts',(-0.273324196837474,-2.73652609522353,
12.5216901060418));
#439523=CARTESIAN_POINT('Ctrl Pts',(-0.261597842664173,-2.7375281054975,
12.5161920673678));
#439524=CARTESIAN_POINT('Ctrl Pts',(-0.283329500888561,-2.73117874698419,
12.5042015548894));
#439525=CARTESIAN_POINT('Ctrl Pts',(-0.278983334041869,-2.7359209172424,
12.4980677368513));
#439526=CARTESIAN_POINT('Ctrl Pts',(-0.272221399150479,-2.73660430311319,
12.4907278922777));
#439527=CARTESIAN_POINT('Ctrl Pts',(-0.296088652451907,-2.72751227373476,
12.506463626192));
#439528=CARTESIAN_POINT('Ctrl Pts',(-0.296794759692605,-2.73401679915181,
12.4999376786891));
#439529=CARTESIAN_POINT('Ctrl Pts',(-0.296786135619339,-2.73393735583142,
12.4906970594712));
#439530=CARTESIAN_POINT('Origin',(-0.259736489890645,-2.71560692218504,
12.5369868989719));
#439531=CARTESIAN_POINT('Origin',(-0.259736489890645,-2.71560692218504,
14.));
#439532=CARTESIAN_POINT('Origin',(-0.259736489890645,-2.71560692218504,
13.7435492065112));
#439533=CARTESIAN_POINT('Ctrl Pts',(-0.287586675305132,-2.69767848871726,
13.793642941384));
#439534=CARTESIAN_POINT('Ctrl Pts',(-0.284704006045186,-2.70809945013853,
13.8071662555867));
#439535=CARTESIAN_POINT('Ctrl Pts',(-0.267801281095337,-2.70602164531021,
13.8103758687955));
#439536=CARTESIAN_POINT('Ctrl Pts',(-0.283115007241042,-2.71368679562173,
13.7804579775006));
#439537=CARTESIAN_POINT('Ctrl Pts',(-0.279548280174751,-2.72654261647316,
13.7901904343351));
#439538=CARTESIAN_POINT('Ctrl Pts',(-0.263804867301074,-2.72717576357554,
13.7927914348263));
#439539=CARTESIAN_POINT('Ctrl Pts',(-0.280482367927284,-2.72311148834653,
13.7597120340895));
#439540=CARTESIAN_POINT('Ctrl Pts',(-0.276349138435289,-2.73798776153368,
13.7635825532445));
#439541=CARTESIAN_POINT('Ctrl Pts',(-0.261423068559663,-2.7396455776309,
13.7651073818884));
#439542=CARTESIAN_POINT('Ctrl Pts',(-0.280997898984724,-2.72126591770987,
13.7381884353898));
#439543=CARTESIAN_POINT('Ctrl Pts',(-0.276962281456728,-2.7357942246241,
13.7368803041982));
#439544=CARTESIAN_POINT('Ctrl Pts',(-0.261889010073193,-2.73720352477568,
13.7363986145813));
#439545=CARTESIAN_POINT('Origin',(-0.265312792372365,-2.69564410325325,
13.7902182540695));
#439546=CARTESIAN_POINT('Ctrl Pts',(-0.296125286266661,-2.66711088624712,
13.8235227101244));
#439547=CARTESIAN_POINT('Ctrl Pts',(-0.293036436368329,-2.67818525731844,
13.8358800583119));
#439548=CARTESIAN_POINT('Ctrl Pts',(-0.276534021492768,-2.67666988530749,
13.8390832900376));
#439549=CARTESIAN_POINT('Ctrl Pts',(-0.29291634471462,-2.67859869906812,
13.8124254819052));
#439550=CARTESIAN_POINT('Ctrl Pts',(-0.289821496045629,-2.68969457633634,
13.8247886449158));
#439551=CARTESIAN_POINT('Ctrl Pts',(-0.273299788249322,-2.68816031671179,
13.8279860620657));
#439552=CARTESIAN_POINT('Ctrl Pts',(-0.2897088413058,-2.69008136342514,
13.8013225099955));
#439553=CARTESIAN_POINT('Ctrl Pts',(-0.286609456068655,-2.70119351195657,
13.8136962257787));
#439554=CARTESIAN_POINT('Ctrl Pts',(-0.270067313214188,-2.69964550205236,
13.8168830918626));
#439555=CARTESIAN_POINT('Ctrl Pts',(-0.286502720084255,-2.70155907963701,
13.7902140179785));
#439556=CARTESIAN_POINT('Ctrl Pts',(-0.283400164913025,-2.71268260663856,
13.802602731458));
#439557=CARTESIAN_POINT('Ctrl Pts',(-0.266836529074552,-2.71112564795836,
13.8057746032558));
#439558=CARTESIAN_POINT('Origin',(-0.274935361904289,-2.66119589786016,
13.8235269408515));
#439559=CARTESIAN_POINT('Ctrl Pts',(-0.359110979140358,-2.65936638433693,
13.8235269408515));
#439560=CARTESIAN_POINT('Ctrl Pts',(-0.364949074200162,-2.66962958388014,
13.8362179249168));
#439561=CARTESIAN_POINT('Ctrl Pts',(-0.38096391197163,-2.66369763856593,
13.8391868794938));
#439562=CARTESIAN_POINT('Ctrl Pts',(-0.353769376277788,-2.64997600348538,
13.8400110824519));
#439563=CARTESIAN_POINT('Ctrl Pts',(-0.361423672080065,-2.65651309906617,
13.8494522556836));
#439564=CARTESIAN_POINT('Ctrl Pts',(-0.372075479704802,-2.64829927646268,
13.85569149686));
#439565=CARTESIAN_POINT('Ctrl Pts',(-0.340623534244925,-2.64035391622262,
13.8586819406588));
#439566=CARTESIAN_POINT('Ctrl Pts',(-0.344946490840129,-2.63983614222662,
13.868010383617));
#439567=CARTESIAN_POINT('Ctrl Pts',(-0.350166887882488,-2.63244423303395,
13.8744918421245));
#439568=CARTESIAN_POINT('Ctrl Pts',(-0.309561120473473,-2.64412193276161,
13.8587686893867));
#439569=CARTESIAN_POINT('Ctrl Pts',(-0.305276631455309,-2.64463504266512,
13.8680909899357));
#439570=CARTESIAN_POINT('Ctrl Pts',(-0.298457400739466,-2.63871942824649,
13.8745789365163));
#439571=CARTESIAN_POINT('Ctrl Pts',(-0.299035436609865,-2.6566927303164,
13.8400379222776));
#439572=CARTESIAN_POINT('Ctrl Pts',(-0.293189348780438,-2.66488379196912,
13.8494748685453));
#439573=CARTESIAN_POINT('Ctrl Pts',(-0.280869629396328,-2.65949996251772,
13.8557104837033));
#439574=CARTESIAN_POINT('Ctrl Pts',(-0.296124228014408,-2.66711467752126,
13.8235269408542));
#439575=CARTESIAN_POINT('Ctrl Pts',(-0.292947597049464,-2.67848682043731,
13.8362179249195));
#439576=CARTESIAN_POINT('Ctrl Pts',(-0.275972549792128,-2.67661311430574,
13.8391868794965));
#439577=CARTESIAN_POINT('Origin',(-0.378233633740471,-2.64848869703472,
13.8235269408515));
#439578=CARTESIAN_POINT('Ctrl Pts',(-0.376793638992285,-2.69045197915557,
13.7902140241682));
#439579=CARTESIAN_POINT('Ctrl Pts',(-0.38249961516522,-2.70049192095354,
13.8026027327198));
#439580=CARTESIAN_POINT('Ctrl Pts',(-0.398192068574959,-2.69496699215246,
13.8057746032556));
#439581=CARTESIAN_POINT('Ctrl Pts',(-0.370901345970342,-2.68009350118988,
13.8013225161807));
#439582=CARTESIAN_POINT('Ctrl Pts',(-0.376601489003658,-2.69012317203617,
13.8136962270464));
#439583=CARTESIAN_POINT('Ctrl Pts',(-0.392275259073093,-2.68461213428235,
13.8168830918628));
#439584=CARTESIAN_POINT('Ctrl Pts',(-0.365006512727856,-2.66973055759115,
13.8124254880875));
#439585=CARTESIAN_POINT('Ctrl Pts',(-0.370698310908615,-2.67974554179035,
13.8247886461868));
#439586=CARTESIAN_POINT('Ctrl Pts',(-0.386355587722492,-2.67425279703273,
13.8279860620656));
#439587=CARTESIAN_POINT('Ctrl Pts',(-0.359109036426738,-2.65936296757305,
13.8235227163065));
#439588=CARTESIAN_POINT('Ctrl Pts',(-0.364789802401239,-2.66935854065216,
13.8358800595847));
#439589=CARTESIAN_POINT('Ctrl Pts',(-0.380432939137479,-2.66388879624773,
13.8390832900376));
#439590=CARTESIAN_POINT('Origin',(-0.395918242455691,-2.67957771943477,
13.7902182540695));
#439591=CARTESIAN_POINT('Ctrl Pts',(-0.386910456038192,-2.70823699195356,
13.7382347919292));
#439592=CARTESIAN_POINT('Ctrl Pts',(-0.394350849890824,-2.72136552607016,
13.7369371795943));
#439593=CARTESIAN_POINT('Ctrl Pts',(-0.409326590721183,-2.71906966814732,
13.7364597369711));
#439594=CARTESIAN_POINT('Ctrl Pts',(-0.387845718556795,-2.70988115678884,
13.7595490285573));
#439595=CARTESIAN_POINT('Ctrl Pts',(-0.395464508545196,-2.72332243074375,
13.7633824266926));
#439596=CARTESIAN_POINT('Ctrl Pts',(-0.410357371837858,-2.72129850306384,
13.7648920890506));
#439597=CARTESIAN_POINT('Ctrl Pts',(-0.383075930942875,-2.70149600620757,
13.7803806590111));
#439598=CARTESIAN_POINT('Ctrl Pts',(-0.389661215122637,-2.71312488914086,
13.7901039518744));
#439599=CARTESIAN_POINT('Ctrl Pts',(-0.405098967304464,-2.70993721773393,
13.7926933640892));
#439600=CARTESIAN_POINT('Ctrl Pts',(-0.374784975386382,-2.68692074265818,
13.7936647693663));
#439601=CARTESIAN_POINT('Ctrl Pts',(-0.380106481733742,-2.69633641587572,
13.8072068914933));
#439602=CARTESIAN_POINT('Ctrl Pts',(-0.396015010918582,-2.69020755227619,
13.8104111085397));
#439603=CARTESIAN_POINT('Origin',(-0.406166516281074,-2.69759388364003,
13.7435492065112));
#439604=CARTESIAN_POINT('Origin',(-0.406166516281074,-2.69759388364003,
14.));
#439605=CARTESIAN_POINT('Origin',(-0.406166516281074,-2.69759388364003,
12.5369868989719));
#439606=CARTESIAN_POINT('Ctrl Pts',(-0.373783780809424,-2.71795626453539,
12.506462012331));
#439607=CARTESIAN_POINT('Ctrl Pts',(-0.374674612712626,-2.72443391893418,
12.4999388158272));
#439608=CARTESIAN_POINT('Ctrl Pts',(-0.374664073002957,-2.72435727978771,
12.4907030323752));
#439609=CARTESIAN_POINT('Ctrl Pts',(-0.38705082235667,-2.71841907306833,
12.5042014951932));
#439610=CARTESIAN_POINT('Ctrl Pts',(-0.392413855278163,-2.72196575814019,
12.4980716682127));
#439611=CARTESIAN_POINT('Ctrl Pts',(-0.399135291550663,-2.72099217729576,
12.4907355092744));
#439612=CARTESIAN_POINT('Ctrl Pts',(-0.389580147186854,-2.71294840426563,
12.5218047446509));
#439613=CARTESIAN_POINT('Ctrl Pts',(-0.398052217293834,-2.72117901171824,
12.5216906929434));
#439614=CARTESIAN_POINT('Ctrl Pts',(-0.409666500889807,-2.71931375814775,
12.5161988840775));
#439615=CARTESIAN_POINT('Ctrl Pts',(-0.387024896359692,-2.70843816262876,
12.5369868989719));
#439616=CARTESIAN_POINT('Ctrl Pts',(-0.394581332972405,-2.72177629582793,
12.5369868989719));
#439617=CARTESIAN_POINT('Ctrl Pts',(-0.409710957945607,-2.71930648213231,
12.5369868989719));
#439618=CARTESIAN_POINT('Origin',(-6.29013144927391E-32,-1.0265181555254E-30,
12.5));
#439619=CARTESIAN_POINT('Origin',(-0.141153018305391,-2.67978844069895,
12.5));
#439620=CARTESIAN_POINT('',(-0.141153018305391,-2.67978844069895,12.5893111709658));
#439621=CARTESIAN_POINT('',(-0.141153018305391,-2.67978844069895,13.8235269408515));
#439622=CARTESIAN_POINT('',(-0.141153018305391,-2.67978844069895,12.5));
#439623=CARTESIAN_POINT('',(-0.156244739001983,-2.71221547672782,13.7902182540695));
#439624=CARTESIAN_POINT('',(-0.141153018305391,-2.67978844069895,13.8235269408515));
#439625=CARTESIAN_POINT('',(-0.164990427904997,-2.73100702309002,13.7435492065112));
#439626=CARTESIAN_POINT('Origin',(-0.136216931677467,-2.66918322139446,
13.7445212918691));
#439627=CARTESIAN_POINT('',(-0.164990427904997,-2.73100702309002,12.5369868989719));
#439628=CARTESIAN_POINT('',(-0.164990427904997,-2.73100702309002,12.5));
#439629=CARTESIAN_POINT('Ctrl Pts',(-0.164990427904997,-2.73100702309002,
12.5369868989719));
#439630=CARTESIAN_POINT('Ctrl Pts',(-0.157050419890708,-2.71394661419927,
12.5544431401645));
#439631=CARTESIAN_POINT('Ctrl Pts',(-0.149104732971654,-2.69687400325064,
12.5718848856037));
#439632=CARTESIAN_POINT('Ctrl Pts',(-0.141153018305391,-2.67978844069895,
12.5893111709658));
#439633=CARTESIAN_POINT('Origin',(0.017582891275753,-2.94032602740454,12.5));
#439634=CARTESIAN_POINT('',(-0.0581609899471342,-2.73536807408357,13.7435492065112));
#439635=CARTESIAN_POINT('',(-0.0653458928110684,-2.71592620020509,13.7902182540695));
#439636=CARTESIAN_POINT('Origin',(-0.0842265757358376,-2.66483631588591,
13.7418732680455));
#439637=CARTESIAN_POINT('',(-0.0777442925777539,-2.68237694712209,13.8235269408515));
#439638=CARTESIAN_POINT('',(-0.0653458928110684,-2.71592620020509,13.7902182540695));
#439639=CARTESIAN_POINT('',(-0.0777442925777539,-2.68237694712209,12.5893111709658));
#439640=CARTESIAN_POINT('',(-0.0777442925777539,-2.68237694712209,12.5));
#439641=CARTESIAN_POINT('',(-0.0581609899471342,-2.73536807408357,12.5369868989719));
#439642=CARTESIAN_POINT('Ctrl Pts',(-0.0777442925777539,-2.68237694712209,
12.5893111709658));
#439643=CARTESIAN_POINT('Ctrl Pts',(-0.0712116685486591,-2.70005379743926,
12.5718848856037));
#439644=CARTESIAN_POINT('Ctrl Pts',(-0.0646839965340555,-2.71771724793141,
12.5544431401645));
#439645=CARTESIAN_POINT('Ctrl Pts',(-0.0581609899471342,-2.73536807408357,
12.5369868989719));
#439646=CARTESIAN_POINT('',(-0.0581609899471342,-2.73536807408357,12.5));
#439647=CARTESIAN_POINT('Origin',(-0.10998792761306,-2.69429284510378,12.5));
#439648=CARTESIAN_POINT('',(-0.109705207909741,-2.65991974163977,13.8587068136939));
#439649=CARTESIAN_POINT('Ctrl Pts',(-0.0777442925716052,-2.68237694711966,
13.8235269408542));
#439650=CARTESIAN_POINT('Ctrl Pts',(-0.0783517168072231,-2.68073329714929,
13.8262006681044));
#439651=CARTESIAN_POINT('Ctrl Pts',(-0.0791362936748559,-2.67911148730507,
13.8288634856214));
#439652=CARTESIAN_POINT('Ctrl Pts',(-0.0800846898927516,-2.67751134540702,
13.8314912288862));
#439653=CARTESIAN_POINT('Ctrl Pts',(-0.0810623885708681,-2.67586176415711,
13.8342001611531));
#439654=CARTESIAN_POINT('Ctrl Pts',(-0.0822148445255834,-2.6742331248582,
13.8368750301949));
#439655=CARTESIAN_POINT('Ctrl Pts',(-0.0835724893765199,-2.67262905828337,
13.8394886372969));
#439656=CARTESIAN_POINT('Ctrl Pts',(-0.0836773435815423,-2.67250517233087,
13.8396904925131));
#439657=CARTESIAN_POINT('Ctrl Pts',(-0.0837834408254324,-2.67238144413296,
13.8398919674349));
#439658=CARTESIAN_POINT('Ctrl Pts',(-0.0838908044602892,-2.67225788198516,
13.8400930404591));
#439659=CARTESIAN_POINT('Ctrl Pts',(-0.0855636021221009,-2.67033270059394,
13.8432258934518));
#439660=CARTESIAN_POINT('Ctrl Pts',(-0.0875344402538826,-2.66845691437443,
13.8462331177034));
#439661=CARTESIAN_POINT('Ctrl Pts',(-0.0898055468410686,-2.66676157757213,
13.8489036603661));
#439662=CARTESIAN_POINT('Ctrl Pts',(-0.0905486793465914,-2.66620684364079,
13.8497774930041));
#439663=CARTESIAN_POINT('Ctrl Pts',(-0.0913238751608761,-2.66567166476784,
13.85061494757));
#439664=CARTESIAN_POINT('Ctrl Pts',(-0.0921309564506031,-2.66516129870573,
13.8514076489583));
#439665=CARTESIAN_POINT('Ctrl Pts',(-0.0938380497769036,-2.66408180087857,
13.8530843267192));
#439666=CARTESIAN_POINT('Ctrl Pts',(-0.0958570558753725,-2.66300977640063,
13.8546805203176));
#439667=CARTESIAN_POINT('Ctrl Pts',(-0.0981347799227737,-2.66212795669042,
13.8559412814273));
#439668=CARTESIAN_POINT('Ctrl Pts',(-0.0984396132686843,-2.6620099406151,
13.8561100121513));
#439669=CARTESIAN_POINT('Ctrl Pts',(-0.0987490129978316,-2.66189529472272,
13.8562727473908));
#439670=CARTESIAN_POINT('Ctrl Pts',(-0.0990627899542671,-2.66178441284256,
13.8564289040185));
#439671=CARTESIAN_POINT('Ctrl Pts',(-0.100485764871901,-2.66128156478103,
13.8571370725437));
#439672=CARTESIAN_POINT('Ctrl Pts',(-0.102024532775858,-2.66084943554403,
13.8577210840554));
#439673=CARTESIAN_POINT('Ctrl Pts',(-0.10362721628845,-2.66053307709753,
13.8581177131616));
#439674=CARTESIAN_POINT('Ctrl Pts',(-0.10407858712828,-2.66044397967027,
13.8582294175695));
#439675=CARTESIAN_POINT('Ctrl Pts',(-0.104534959754643,-2.66036390081054,
13.8583265086086));
#439676=CARTESIAN_POINT('Ctrl Pts',(-0.104995031868896,-2.66029343139185,
13.8584082369006));
#439677=CARTESIAN_POINT('Ctrl Pts',(-0.105656032123871,-2.66019218573432,
13.8585256585398));
#439678=CARTESIAN_POINT('Ctrl Pts',(-0.106332935601478,-2.66010983676469,
13.8586122832068));
#439679=CARTESIAN_POINT('Ctrl Pts',(-0.107008253677771,-2.66004930757789,
13.8586682984299));
#439680=CARTESIAN_POINT('Ctrl Pts',(-0.107548441196678,-2.66000089022851,
13.8587131050557));
#439681=CARTESIAN_POINT('Ctrl Pts',(-0.108093559752444,-2.65996566576368,
13.8587357943552));
#439682=CARTESIAN_POINT('Ctrl Pts',(-0.108643706777496,-2.65994413538968,
13.8587355499465));
#439683=CARTESIAN_POINT('Ctrl Pts',(-0.108999279915972,-2.65993021979565,
13.8587353919793));
#439684=CARTESIAN_POINT('Ctrl Pts',(-0.109353106987064,-2.6599221365345,
13.8587257282814));
#439685=CARTESIAN_POINT('Ctrl Pts',(-0.109705207909741,-2.65991974163977,
13.8587068136939));
#439686=CARTESIAN_POINT('Ctrl Pts',(-0.109705207909741,-2.65991974163977,
13.8587068136939));
#439687=CARTESIAN_POINT('Ctrl Pts',(-0.110863248649113,-2.65991186496157,
13.8586446046466));
#439688=CARTESIAN_POINT('Ctrl Pts',(-0.11200264114951,-2.65996544440026,
13.858482427929));
#439689=CARTESIAN_POINT('Ctrl Pts',(-0.113123900787746,-2.66007603919643,
13.8582284286032));
#439690=CARTESIAN_POINT('Ctrl Pts',(-0.114274182746367,-2.6601894965924,
13.8579678548414));
#439691=CARTESIAN_POINT('Ctrl Pts',(-0.115408040486462,-2.66036476047715,
13.857615680862));
#439692=CARTESIAN_POINT('Ctrl Pts',(-0.116482252692222,-2.66058534525566,
13.8571944833187));
#439693=CARTESIAN_POINT('Ctrl Pts',(-0.119163059113111,-2.66113583712999,
13.8561433417727));
#439694=CARTESIAN_POINT('Ctrl Pts',(-0.121598755640584,-2.66198964181121,
13.8546163505474));
#439695=CARTESIAN_POINT('Ctrl Pts',(-0.123712672228886,-2.66295471875481,
13.8528973491086));
#439696=CARTESIAN_POINT('Ctrl Pts',(-0.124098853601637,-2.66313102407402,
13.8525833129072));
#439697=CARTESIAN_POINT('Ctrl Pts',(-0.124474407366545,-2.66331095607156,
13.8522628768812));
#439698=CARTESIAN_POINT('Ctrl Pts',(-0.124839022524153,-2.6634932573058,
13.851937733538));
#439699=CARTESIAN_POINT('Ctrl Pts',(-0.127065676703604,-2.66460654565014,
13.8499521282529));
#439700=CARTESIAN_POINT('Ctrl Pts',(-0.12910385288684,-2.66592247936995,
13.847639871647));
#439701=CARTESIAN_POINT('Ctrl Pts',(-0.130890009862378,-2.66730440264407,
13.8452109780794));
#439702=CARTESIAN_POINT('Ctrl Pts',(-0.131693638857281,-2.66792615852948,
13.8441181685877));
#439703=CARTESIAN_POINT('Ctrl Pts',(-0.132446860397751,-2.66856089182315,
13.8430021611332));
#439704=CARTESIAN_POINT('Ctrl Pts',(-0.133147097667796,-2.66919535530509,
13.8418824960098));
#439705=CARTESIAN_POINT('Ctrl Pts',(-0.134797224675853,-2.67069048470191,
13.8392439765549));
#439706=CARTESIAN_POINT('Ctrl Pts',(-0.136234541433634,-2.67225278643325,
13.8364981347964));
#439707=CARTESIAN_POINT('Ctrl Pts',(-0.137488033046078,-2.67386322296115,
13.8336931113419));
#439708=CARTESIAN_POINT('Ctrl Pts',(-0.138708854272521,-2.67543168586716,
13.8309611966328));
#439709=CARTESIAN_POINT('Ctrl Pts',(-0.139756085695415,-2.67704772555847,
13.8281701127186));
#439710=CARTESIAN_POINT('Ctrl Pts',(-0.140618834939088,-2.67870495665951,
13.8253580685121));
#439711=CARTESIAN_POINT('Ctrl Pts',(-0.140805879906225,-2.67906424615075,
13.8247484142933));
#439712=CARTESIAN_POINT('Ctrl Pts',(-0.140984081604137,-2.6794254525011,
13.8241378483365));
#439713=CARTESIAN_POINT('Ctrl Pts',(-0.141153018305391,-2.67978844069895,
13.8235269408515));
#439714=CARTESIAN_POINT('',(-0.108463550405648,-2.65995235300169,12.5969504640361));
#439715=CARTESIAN_POINT('Origin',(-0.10998947276331,-2.69432589499518,12.584524458991));
#439716=CARTESIAN_POINT('Origin',(-0.10998947276331,-2.69432589499518,12.584524458991));
#439717=CARTESIAN_POINT('Ctrl Pts',(-0.0777442925777539,-2.68237694712209,
12.5893111709658));
#439718=CARTESIAN_POINT('Ctrl Pts',(-0.0816731450388344,-2.67174573115689,
12.5770542771492));
#439719=CARTESIAN_POINT('Ctrl Pts',(-0.0978116640663424,-2.67445716591615,
12.5737548217797));
#439720=CARTESIAN_POINT('Ctrl Pts',(-0.0691532108074482,-2.70562384849586,
12.5663937883685));
#439721=CARTESIAN_POINT('Ctrl Pts',(-0.0730870750654656,-2.69497907093825,
12.5540940315304));
#439722=CARTESIAN_POINT('Ctrl Pts',(-0.0892750720354502,-2.69770207468649,
12.5508374392248));
#439723=CARTESIAN_POINT('Ctrl Pts',(-0.0605707973333296,-2.72884729403113,
12.5434499600944));
#439724=CARTESIAN_POINT('Ctrl Pts',(-0.0645174519850021,-2.71816790651098,
12.5311293540532));
#439725=CARTESIAN_POINT('Ctrl Pts',(-0.08074571289465,-2.72092386594619,
12.5278936106989));
#439726=CARTESIAN_POINT('Ctrl Pts',(-0.0519963731558851,-2.75204912105586,
12.5204817579905));
#439727=CARTESIAN_POINT('Ctrl Pts',(-0.0559625610508614,-2.74131687786583,
12.5081597038247));
#439728=CARTESIAN_POINT('Ctrl Pts',(-0.0722230114704962,-2.74412433170255,
12.5049254088044));
#439729=CARTESIAN_POINT('Ctrl Pts',(-0.0581609899471349,-2.73536807408356,
12.5369868989719));
#439730=CARTESIAN_POINT('Ctrl Pts',(-0.0578380892691153,-2.73624182251581,
12.5342545179733));
#439731=CARTESIAN_POINT('Ctrl Pts',(-0.0576469389974919,-2.73711893065454,
12.5314872231885));
#439732=CARTESIAN_POINT('Ctrl Pts',(-0.0576529258276875,-2.73796189285297,
12.5287124745063));
#439733=CARTESIAN_POINT('Ctrl Pts',(-0.0576583250483176,-2.73872211800443,
12.5262100684184));
#439734=CARTESIAN_POINT('Ctrl Pts',(-0.0578250404946854,-2.73945379709917,
12.5237004536639));
#439735=CARTESIAN_POINT('Ctrl Pts',(-0.0582205687912007,-2.74015476638387,
12.5212220730815));
#439736=CARTESIAN_POINT('Ctrl Pts',(-0.0585233799181101,-2.74069141900998,
12.5193246583486));
#439737=CARTESIAN_POINT('Ctrl Pts',(-0.0589644751466254,-2.74121617383129,
12.517417831369));
#439738=CARTESIAN_POINT('Ctrl Pts',(-0.0596291657478373,-2.74168238312781,
12.5155812248347));
#439739=CARTESIAN_POINT('Ctrl Pts',(-0.0599123275166779,-2.74188099079401,
12.5147988205793));
#439740=CARTESIAN_POINT('Ctrl Pts',(-0.0602361958776334,-2.74206940199723,
12.5140295443047));
#439741=CARTESIAN_POINT('Ctrl Pts',(-0.060607339170164,-2.74224613741881,
12.5132817086137));
#439742=CARTESIAN_POINT('Ctrl Pts',(-0.0611690143362852,-2.74251360257115,
12.5121499604604));
#439743=CARTESIAN_POINT('Ctrl Pts',(-0.0618541657054794,-2.74275364573008,
12.5110494206568));
#439744=CARTESIAN_POINT('Ctrl Pts',(-0.0626857611601713,-2.742936951795,
12.5100666561695));
#439745=CARTESIAN_POINT('Ctrl Pts',(-0.0631632613552607,-2.74304220571536,
12.5095023550641));
#439746=CARTESIAN_POINT('Ctrl Pts',(-0.0636947021899745,-2.74312933191489,
12.5089719619137));
#439747=CARTESIAN_POINT('Ctrl Pts',(-0.0642711557016938,-2.74319039447116,
12.5085043804652));
#439748=CARTESIAN_POINT('Ctrl Pts',(-0.0651147203277434,-2.74327975156831,
12.5078201359221));
#439749=CARTESIAN_POINT('Ctrl Pts',(-0.0660792708199977,-2.74331468522683,
12.5072563000949));
#439750=CARTESIAN_POINT('Ctrl Pts',(-0.0670997313003516,-2.74328436700756,
12.5068768744332));
#439751=CARTESIAN_POINT('Ctrl Pts',(-0.0678355535554259,-2.74326250548436,
12.5066032824114));
#439752=CARTESIAN_POINT('Ctrl Pts',(-0.0686133747377393,-2.74320639283856,
12.5064197834844));
#439753=CARTESIAN_POINT('Ctrl Pts',(-0.0693899452839983,-2.74312174070353,
12.5063282718343));
#439754=CARTESIAN_POINT('Ctrl Pts',(-0.0705234978613715,-2.74299817479403,
12.5061946931565));
#439755=CARTESIAN_POINT('Ctrl Pts',(-0.0716787291581415,-2.74281221476893,
12.5062515701262));
#439756=CARTESIAN_POINT('Ctrl Pts',(-0.072786401205737,-2.74259066961847,
12.5064436508398));
#439757=CARTESIAN_POINT('',(-0.0978116640663425,-2.67445716591615,12.5737548217797));
#439758=CARTESIAN_POINT('Origin',(-0.0983802190003496,-2.69000312183037,
12.5893111709658));
#439759=CARTESIAN_POINT('Ctrl Pts',(-0.0727864012057365,-2.74259066961847,
12.5064436508398));
#439760=CARTESIAN_POINT('Ctrl Pts',(-0.0764912412634739,-2.73250530656612,
12.5164271754438));
#439761=CARTESIAN_POINT('Ctrl Pts',(-0.0801973537974575,-2.72241587363327,
12.5264061185523));
#439762=CARTESIAN_POINT('Ctrl Pts',(-0.0839047845116802,-2.71232222780853,
12.536380305637));
#439763=CARTESIAN_POINT('Ctrl Pts',(-0.0885383209564884,-2.69970721773956,
12.5488460165097));
#439764=CARTESIAN_POINT('Ctrl Pts',(-0.0931739177355619,-2.68708562342805,
12.5613043021964));
#439765=CARTESIAN_POINT('Ctrl Pts',(-0.0978116640663423,-2.67445716591615,
12.5737548217797));
#439766=CARTESIAN_POINT('Ctrl Pts',(-0.141153018305391,-2.67978844069895,
12.5893111709658));
#439767=CARTESIAN_POINT('Ctrl Pts',(-0.136370695980209,-2.66951283717712,
12.5770542771492));
#439768=CARTESIAN_POINT('Ctrl Pts',(-0.120506883648043,-2.67353068898434,
12.5737548217797));
#439769=CARTESIAN_POINT('Ctrl Pts',(-0.136691153170441,-2.67020139198557,
12.5928319619712));
#439770=CARTESIAN_POINT('Ctrl Pts',(-0.130523599864772,-2.6646701441523,
12.5821634970842));
#439771=CARTESIAN_POINT('Ctrl Pts',(-0.118890091640733,-2.67003437650195,
12.5773203894503));
#439772=CARTESIAN_POINT('Ctrl Pts',(-0.123933189196619,-2.65934697101611,
12.5969440695591));
#439773=CARTESIAN_POINT('Ctrl Pts',(-0.119916061609491,-2.6594926710527,
12.5878292599214));
#439774=CARTESIAN_POINT('Ctrl Pts',(-0.114341567151678,-2.66616719767624,
12.5813877129824));
#439775=CARTESIAN_POINT('Ctrl Pts',(-0.0933595190306978,-2.66054109752823,
12.596957478804));
#439776=CARTESIAN_POINT('Ctrl Pts',(-0.0973469618730906,-2.66039655435977,
12.5878468778671));
#439777=CARTESIAN_POINT('Ctrl Pts',(-0.103399059589684,-2.66660055268072,
12.5814011370086));
#439778=CARTESIAN_POINT('Ctrl Pts',(-0.0814152001758918,-2.67244371296496,
12.5928371701607));
#439779=CARTESIAN_POINT('Ctrl Pts',(-0.0871116983762444,-2.66643663597552,
12.5821692192952));
#439780=CARTESIAN_POINT('Ctrl Pts',(-0.099142098123944,-2.67082905033195,
12.5773318885715));
#439781=CARTESIAN_POINT('Ctrl Pts',(-0.0777442925777029,-2.68237694712207,
12.5893111709658));
#439782=CARTESIAN_POINT('Ctrl Pts',(-0.0816731450387836,-2.67174573115687,
12.5770542771492));
#439783=CARTESIAN_POINT('Ctrl Pts',(-0.0978116640662907,-2.67445716591612,
12.5737548217797));
#439784=CARTESIAN_POINT('',(-0.120506883648043,-2.67353068898434,12.5737548217797));
#439785=CARTESIAN_POINT('Origin',(-0.121207360262299,-2.68907125951804,
12.5893111709658));
#439786=CARTESIAN_POINT('Ctrl Pts',(-0.0978116640662907,-2.67445716591612,
12.5737548217797));
#439787=CARTESIAN_POINT('Ctrl Pts',(-0.09812821209362,-2.67350631525623,
12.5746934679442));
#439788=CARTESIAN_POINT('Ctrl Pts',(-0.0986522994817637,-2.67251199747613,
12.5756680099006));
#439789=CARTESIAN_POINT('Ctrl Pts',(-0.0993213541186758,-2.67158578499467,
12.5765688348656));
#439790=CARTESIAN_POINT('Ctrl Pts',(-0.0994984789271169,-2.67134058049372,
12.5768073183026));
#439791=CARTESIAN_POINT('Ctrl Pts',(-0.0996855252474055,-2.67110005397904,
12.5770407398754));
#439792=CARTESIAN_POINT('Ctrl Pts',(-0.0998808782664673,-2.67086594216634,
12.5772674179684));
#439793=CARTESIAN_POINT('Ctrl Pts',(-0.100682554231018,-2.66990521059353,
12.5781976435658));
#439794=CARTESIAN_POINT('Ctrl Pts',(-0.10167831396391,-2.66900516612956,
12.5790594849312));
#439795=CARTESIAN_POINT('Ctrl Pts',(-0.10283330262416,-2.66826240511929,
12.5797571720116));
#439796=CARTESIAN_POINT('Ctrl Pts',(-0.103585819266005,-2.6677784696138,
12.580211740231));
#439797=CARTESIAN_POINT('Ctrl Pts',(-0.104450280663714,-2.66735509806044,
12.5806009430798));
#439798=CARTESIAN_POINT('Ctrl Pts',(-0.105373624926531,-2.66703800495638,
12.5808812374708));
#439799=CARTESIAN_POINT('Ctrl Pts',(-0.106167083964563,-2.66676551678545,
12.5811221033394));
#439800=CARTESIAN_POINT('Ctrl Pts',(-0.107020306407977,-2.66656603943146,
12.581287365893));
#439801=CARTESIAN_POINT('Ctrl Pts',(-0.10788703318161,-2.66645895076109,
12.581359338449));
#439802=CARTESIAN_POINT('Ctrl Pts',(-0.108007490305921,-2.6664440676472,
12.5813693411482));
#439803=CARTESIAN_POINT('Ctrl Pts',(-0.108128221153119,-2.66643091056954,
12.5813775999465));
#439804=CARTESIAN_POINT('Ctrl Pts',(-0.108249115802138,-2.66641947188415,
12.5813841266931));
#439805=CARTESIAN_POINT('Ctrl Pts',(-0.108454228196106,-2.66640006477089,
12.5813952001081));
#439806=CARTESIAN_POINT('Ctrl Pts',(-0.108661243195412,-2.66638608027326,
12.5814007534795));
#439807=CARTESIAN_POINT('Ctrl Pts',(-0.1088700839301,-2.66637772124331,
12.5814005856065));
#439808=CARTESIAN_POINT('Ctrl Pts',(-0.109826075162065,-2.66633945687235,
12.5813998171494));
#439809=CARTESIAN_POINT('Ctrl Pts',(-0.110754258624749,-2.66642137793365,
12.58127954464));
#439810=CARTESIAN_POINT('Ctrl Pts',(-0.111651966128673,-2.66659354455215,
12.5810700125799));
#439811=CARTESIAN_POINT('Ctrl Pts',(-0.112736294581228,-2.66680150222457,
12.5808169217085));
#439812=CARTESIAN_POINT('Ctrl Pts',(-0.113773104712742,-2.66715758242712,
12.5804173076348));
#439813=CARTESIAN_POINT('Ctrl Pts',(-0.114679991213303,-2.66760594861982,
12.5799304713245));
#439814=CARTESIAN_POINT('Ctrl Pts',(-0.115803909286207,-2.66816161558249,
12.5793271277669));
#439815=CARTESIAN_POINT('Ctrl Pts',(-0.116812267115515,-2.6688646285955,
12.5785808224116));
#439816=CARTESIAN_POINT('Ctrl Pts',(-0.117680699735257,-2.66965933649654,
12.5777485681082));
#439817=CARTESIAN_POINT('Ctrl Pts',(-0.118974759482569,-2.67084353833583,
12.576508418016));
#439818=CARTESIAN_POINT('Ctrl Pts',(-0.119951868793801,-2.67221630084431,
12.5750928681475));
#439819=CARTESIAN_POINT('Ctrl Pts',(-0.120506883648043,-2.67353068898434,
12.5737548217797));
#439820=CARTESIAN_POINT('Ctrl Pts',(-0.120506883648043,-2.67353068898434,
12.5737548217797));
#439821=CARTESIAN_POINT('Ctrl Pts',(-0.13637069598021,-2.66951283717712,
12.5770542771492));
#439822=CARTESIAN_POINT('Ctrl Pts',(-0.141153018305391,-2.67978844069895,
12.5893111709658));
#439823=CARTESIAN_POINT('Ctrl Pts',(-0.13090818386789,-2.69599906471351,
12.5508408821982));
#439824=CARTESIAN_POINT('Ctrl Pts',(-0.146820357843191,-2.69196564879042,
12.55409748406));
#439825=CARTESIAN_POINT('Ctrl Pts',(-0.151608781186871,-2.70225436135064,
12.5663972313419));
#439826=CARTESIAN_POINT('Ctrl Pts',(-0.141300393710007,-2.7184449961575,
12.52790050457));
#439827=CARTESIAN_POINT('Ctrl Pts',(-0.157250006116537,-2.71437545792533,
12.5311362602938));
#439828=CARTESIAN_POINT('Ctrl Pts',(-0.162053995921704,-2.72469761758001,
12.5434568539655));
#439829=CARTESIAN_POINT('Ctrl Pts',(-0.151684232180235,-2.74087022170778,
12.5049357605811));
#439830=CARTESIAN_POINT('Ctrl Pts',(-0.167661727114596,-2.7367467473703,
12.5081700652078));
#439831=CARTESIAN_POINT('Ctrl Pts',(-0.172489488642897,-2.74711998446926,
12.5204921097672));
#439832=CARTESIAN_POINT('Ctrl Pts',(-0.151002390083106,-2.73939769282708,
12.5064436508395));
#439833=CARTESIAN_POINT('Ctrl Pts',(-0.152214400901913,-2.7395386806481,
12.5062361689309));
#439834=CARTESIAN_POINT('Ctrl Pts',(-0.153480805005259,-2.73963361361113,
12.5061871075061));
#439835=CARTESIAN_POINT('Ctrl Pts',(-0.154709826787334,-2.73965646312534,
12.5063648335164));
#439836=CARTESIAN_POINT('Ctrl Pts',(-0.15526812428996,-2.73966684278411,
12.5064455676329));
#439837=CARTESIAN_POINT('Ctrl Pts',(-0.15582649899744,-2.73966227225654,
12.506574497099));
#439838=CARTESIAN_POINT('Ctrl Pts',(-0.156361000874931,-2.73964189659912,
12.5067492519495));
#439839=CARTESIAN_POINT('Ctrl Pts',(-0.157435103145554,-2.73960095092461,
12.5071004286051));
#439840=CARTESIAN_POINT('Ctrl Pts',(-0.158452261172662,-2.73949386721969,
12.5076537929612));
#439841=CARTESIAN_POINT('Ctrl Pts',(-0.159337122199412,-2.73933808914168,
12.5083435010503));
#439842=CARTESIAN_POINT('Ctrl Pts',(-0.159392829489099,-2.73932828198072,
12.5083869222963));
#439843=CARTESIAN_POINT('Ctrl Pts',(-0.15944801643132,-2.73931826899819,
12.5084308732336));
#439844=CARTESIAN_POINT('Ctrl Pts',(-0.159502666232373,-2.73930804944287,
12.5084753333615));
#439845=CARTESIAN_POINT('Ctrl Pts',(-0.159941029767316,-2.73922607512072,
12.508831962269));
#439846=CARTESIAN_POINT('Ctrl Pts',(-0.160353969432502,-2.73913041346787,
12.509227847131));
#439847=CARTESIAN_POINT('Ctrl Pts',(-0.160729838305002,-2.73902663681752,
12.5096423454524));
#439848=CARTESIAN_POINT('Ctrl Pts',(-0.161907644998823,-2.73870144672494,
12.5109411997424));
#439849=CARTESIAN_POINT('Ctrl Pts',(-0.162796462689724,-2.7382858926346,
12.5124831113042));
#439850=CARTESIAN_POINT('Ctrl Pts',(-0.163467439755059,-2.73784237459294,
12.5140723025007));
#439851=CARTESIAN_POINT('Ctrl Pts',(-0.163530311040982,-2.73780081646667,
12.5142212114565));
#439852=CARTESIAN_POINT('Ctrl Pts',(-0.16359129741105,-2.73775902327066,
12.5143705582413));
#439853=CARTESIAN_POINT('Ctrl Pts',(-0.163650472675545,-2.7377170537568,
12.5145201959299));
#439854=CARTESIAN_POINT('Ctrl Pts',(-0.16441066705073,-2.73717789286522,
12.5164425148273));
#439855=CARTESIAN_POINT('Ctrl Pts',(-0.164904229762332,-2.73659991913824,
12.5184635205941));
#439856=CARTESIAN_POINT('Ctrl Pts',(-0.165220024053834,-2.73599866649064,
12.5205025929158));
#439857=CARTESIAN_POINT('Ctrl Pts',(-0.165403197259821,-2.73564991612361,
12.5216853356836));
#439858=CARTESIAN_POINT('Ctrl Pts',(-0.16552665820923,-2.73529418849112,
12.5228750347131));
#439859=CARTESIAN_POINT('Ctrl Pts',(-0.165606392345552,-2.73494028127722,
12.5240609649613));
#439860=CARTESIAN_POINT('Ctrl Pts',(-0.165802095505566,-2.73407163500715,
12.5269717671326));
#439861=CARTESIAN_POINT('Ctrl Pts',(-0.165729741265119,-2.73318722342193,
12.5299036066169));
#439862=CARTESIAN_POINT('Ctrl Pts',(-0.165475710962818,-2.73229395933351,
12.5328133004019));
#439863=CARTESIAN_POINT('Ctrl Pts',(-0.165353761625971,-2.73186514055786,
12.5342101228451));
#439864=CARTESIAN_POINT('Ctrl Pts',(-0.165189592035753,-2.73143496006979,
12.5356023438238));
#439865=CARTESIAN_POINT('Ctrl Pts',(-0.164990427904997,-2.73100702309002,
12.5369868989719));
#439866=CARTESIAN_POINT('Origin',(-5.54802939368013,-14.2847916318076,-1.24104469436926));
#439867=CARTESIAN_POINT('Ctrl Pts',(-0.0581754404483332,-2.73532885745512,
12.5369868989719));
#439868=CARTESIAN_POINT('Ctrl Pts',(-0.0528856245388476,-2.74972681395348,
12.5369868989719));
#439869=CARTESIAN_POINT('Ctrl Pts',(-0.0375466846655909,-2.74974188875088,
12.5369868989719));
#439870=CARTESIAN_POINT('Ctrl Pts',(-0.0563872136373922,-2.74019590701836,
12.5218025310015));
#439871=CARTESIAN_POINT('Ctrl Pts',(-0.049362451690614,-2.74969898984949,
12.5216901060417));
#439872=CARTESIAN_POINT('Ctrl Pts',(-0.0375934428539549,-2.74974185928964,
12.5161920673678));
#439873=CARTESIAN_POINT('Ctrl Pts',(-0.0597703224417318,-2.74518495963511,
12.5042015548895));
#439874=CARTESIAN_POINT('Ctrl Pts',(-0.0550520862064945,-2.74955709776713,
12.4980677368514));
#439875=CARTESIAN_POINT('Ctrl Pts',(-0.0482569488029278,-2.74968704925948,
12.4907278922777));
#439876=CARTESIAN_POINT('Ctrl Pts',(-0.0727858705885265,-2.74257067557562,
12.506463626192));
#439877=CARTESIAN_POINT('Ctrl Pts',(-0.0729594491090722,-2.74911111201621,
12.4999376786891));
#439878=CARTESIAN_POINT('Ctrl Pts',(-0.0729573290998271,-2.74903123009488,
12.4906970594712));
#439879=CARTESIAN_POINT('Origin',(-0.0375250635245384,-2.72774189937528,
12.5369868989719));
#439880=CARTESIAN_POINT('Origin',(-0.0375250635245384,-2.72774189937529,
14.));
#439881=CARTESIAN_POINT('Origin',(-0.0375250635245385,-2.72774189937529,
13.7435492065112));
#439882=CARTESIAN_POINT('Ctrl Pts',(-0.0667439135116158,-2.71214316995067,
13.793642941384));
#439883=CARTESIAN_POINT('Ctrl Pts',(-0.0630214309965092,-2.7222944921764,
13.8071662555867));
#439884=CARTESIAN_POINT('Ctrl Pts',(-0.0463443088524619,-2.71884587207157,
13.8103758687955));
#439885=CARTESIAN_POINT('Ctrl Pts',(-0.0609822989275359,-2.72773372807434,
13.7804579775006));
#439886=CARTESIAN_POINT('Ctrl Pts',(-0.056379571104308,-2.74025605087462,
13.7901904343351));
#439887=CARTESIAN_POINT('Ctrl Pts',(-0.0406369357715464,-2.73960385692835,
13.7927914348262));
#439888=CARTESIAN_POINT('Ctrl Pts',(-0.0575902195522705,-2.73691247636728,
13.7597120340895));
#439889=CARTESIAN_POINT('Ctrl Pts',(-0.0522581886711211,-2.75140235340799,
13.7635825532445));
#439890=CARTESIAN_POINT('Ctrl Pts',(-0.0372466566593459,-2.75183803999715,
13.7651073818885));
#439891=CARTESIAN_POINT('Ctrl Pts',(-0.0582544663629731,-2.7351150672818,
13.7381884353898));
#439892=CARTESIAN_POINT('Ctrl Pts',(-0.0530480851316511,-2.74926609215989,
13.7368803041982));
#439893=CARTESIAN_POINT('Ctrl Pts',(-0.0379100977695342,-2.7494420914303,
13.7363986145813));
#439894=CARTESIAN_POINT('Origin',(-0.0447099663884728,-2.70830002549681,
13.7902182540695));
#439895=CARTESIAN_POINT('Ctrl Pts',(-0.0777456563266526,-2.68237325471805,
13.8235227101244));
#439896=CARTESIAN_POINT('Ctrl Pts',(-0.0737644202697953,-2.69315900679101,
13.8358800583119));
#439897=CARTESIAN_POINT('Ctrl Pts',(-0.0574404327052881,-2.69030357704212,
13.8390832900376));
#439898=CARTESIAN_POINT('Ctrl Pts',(-0.0736110288703346,-2.69356128426274,
13.8124254819053));
#439899=CARTESIAN_POINT('Ctrl Pts',(-0.0696220610485445,-2.70436798201703,
13.8247886449158));
#439900=CARTESIAN_POINT('Ctrl Pts',(-0.0532803842747365,-2.70149215494931,
13.8279860620657));
#439901=CARTESIAN_POINT('Ctrl Pts',(-0.0694782544195676,-2.7047442996965,
13.8013225099954));
#439902=CARTESIAN_POINT('Ctrl Pts',(-0.0654834388656869,-2.71556684480029,
13.8136962257787));
#439903=CARTESIAN_POINT('Ctrl Pts',(-0.0491225158051164,-2.71267564755892,
13.8168830918626));
#439904=CARTESIAN_POINT('Ctrl Pts',(-0.0653472608767126,-2.7159224961108,
13.7902140179785));
#439905=CARTESIAN_POINT('Ctrl Pts',(-0.0613483584854679,-2.72675612344471,
13.802602731458));
#439906=CARTESIAN_POINT('Ctrl Pts',(-0.0449667433653669,-2.72385425532595,
13.8057746032558));
#439907=CARTESIAN_POINT('Origin',(-0.0571083661551582,-2.67475077241381,
13.8235269408515));
#439908=CARTESIAN_POINT('Ctrl Pts',(-0.141153018305391,-2.67978844069895,
13.8235269408515));
#439909=CARTESIAN_POINT('Ctrl Pts',(-0.146135141543826,-2.69049334923794,
13.8362179249168));
#439910=CARTESIAN_POINT('Ctrl Pts',(-0.162580199876342,-2.68588649993529,
13.8391868794938));
#439911=CARTESIAN_POINT('Ctrl Pts',(-0.136594592401137,-2.6699939153427,
13.8400110824519));
#439912=CARTESIAN_POINT('Ctrl Pts',(-0.143690585188303,-2.67713315544417,
13.8494522556837));
#439913=CARTESIAN_POINT('Ctrl Pts',(-0.154976452597479,-2.66981488486574,
13.85569149686));
#439914=CARTESIAN_POINT('Ctrl Pts',(-0.1242767815122,-2.65933233661583,
13.8586819406588));
#439915=CARTESIAN_POINT('Ctrl Pts',(-0.128627557213407,-2.65916864656495,
13.868010383617));
#439916=CARTESIAN_POINT('Ctrl Pts',(-0.134433093037599,-2.65222684416309,
13.8744918421245));
#439917=CARTESIAN_POINT('Ctrl Pts',(-0.0930105970316168,-2.66055594029887,
13.8587686893867));
#439918=CARTESIAN_POINT('Ctrl Pts',(-0.0886985410766003,-2.66071811724128,
13.8680909899357));
#439919=CARTESIAN_POINT('Ctrl Pts',(-0.0823841782814193,-2.65426635593163,
13.8745789365163));
#439920=CARTESIAN_POINT('Ctrl Pts',(-0.0814952998104526,-2.67222696861125,
13.8400379222776));
#439921=CARTESIAN_POINT('Ctrl Pts',(-0.0750010167891939,-2.6799142647515,
13.8494748685453));
#439922=CARTESIAN_POINT('Ctrl Pts',(-0.0631611223363676,-2.67354417804797,
13.8557104837033));
#439923=CARTESIAN_POINT('Ctrl Pts',(-0.0777442925716052,-2.68237694711966,
13.8235269408542));
#439924=CARTESIAN_POINT('Ctrl Pts',(-0.0736512963626614,-2.69345232525425,
13.8362179249195));
#439925=CARTESIAN_POINT('Ctrl Pts',(-0.0568854566190928,-2.69020122978514,
13.8391868794965));
#439926=CARTESIAN_POINT('Origin',(-0.161098676348483,-2.67050562187986,
13.8235269408515));
#439927=CARTESIAN_POINT('Ctrl Pts',(-0.156243076003075,-2.71221190170094,
13.7902140241682));
#439928=CARTESIAN_POINT('Ctrl Pts',(-0.161111717548197,-2.72268352645062,
13.8026027327198));
#439929=CARTESIAN_POINT('Ctrl Pts',(-0.177202288601978,-2.71845606202887,
13.8057746032556));
#439930=CARTESIAN_POINT('Ctrl Pts',(-0.151214701217703,-2.7014076141335,
13.8013225161808));
#439931=CARTESIAN_POINT('Ctrl Pts',(-0.156078366210402,-2.71186852665221,
13.8136962270464));
#439932=CARTESIAN_POINT('Ctrl Pts',(-0.172149183841851,-2.70765338419072,
13.8168830918628));
#439933=CARTESIAN_POINT('Ctrl Pts',(-0.146184158654719,-2.6905986687405,
13.8124254880875));
#439934=CARTESIAN_POINT('Ctrl Pts',(-0.15104070365975,-2.70104426329777,
13.8247886461868));
#439935=CARTESIAN_POINT('Ctrl Pts',(-0.167093591866573,-2.6968460086106,
13.8279860620656));
#439936=CARTESIAN_POINT('Ctrl Pts',(-0.141151360553966,-2.67978487695487,
13.8235227163065));
#439937=CARTESIAN_POINT('Ctrl Pts',(-0.145998492247995,-2.69021022575372,
13.8358800595847));
#439938=CARTESIAN_POINT('Ctrl Pts',(-0.162035412684806,-2.68603374234038,
13.8390832900376));
#439939=CARTESIAN_POINT('Origin',(-0.176190397045074,-2.70293265790873,
13.7902182540695));
#439940=CARTESIAN_POINT('Ctrl Pts',(-0.164876586523801,-2.73076235084519,
13.7382347919292));
#439941=CARTESIAN_POINT('Ctrl Pts',(-0.1712221256698,-2.7444536620198,13.7369371795942));
#439942=CARTESIAN_POINT('Ctrl Pts',(-0.186335169692392,-2.74338610528046,
13.7364597369711));
#439943=CARTESIAN_POINT('Ctrl Pts',(-0.165674722335759,-2.73247727743542,
13.7595490285574));
#439944=CARTESIAN_POINT('Ctrl Pts',(-0.172172572818978,-2.74649482877354,
13.7633824266926));
#439945=CARTESIAN_POINT('Ctrl Pts',(-0.187180850232742,-2.74569154216298,
13.7648920890506));
#439946=CARTESIAN_POINT('Ctrl Pts',(-0.161604273412965,-2.72373124577991,
13.780380659011));
#439947=CARTESIAN_POINT('Ctrl Pts',(-0.167219783686543,-2.73585819635999,
13.7901039518744));
#439948=CARTESIAN_POINT('Ctrl Pts',(-0.182865992834047,-2.73393945178664,
13.7926933640892));
#439949=CARTESIAN_POINT('Ctrl Pts',(-0.154528924616555,-2.70852869037029,
13.7936647693663));
#439950=CARTESIAN_POINT('Ctrl Pts',(-0.159065259312451,-2.71834678588172,
13.8072068914933));
#439951=CARTESIAN_POINT('Ctrl Pts',(-0.175420413459769,-2.71353500838634,
13.8104111085397));
#439952=CARTESIAN_POINT('Origin',(-0.184936085948089,-2.72172420427093,
13.7435492065112));
#439953=CARTESIAN_POINT('Origin',(-0.184936085948089,-2.72172420427093,
14.));
#439954=CARTESIAN_POINT('Origin',(-0.184936085948089,-2.72172420427093,
12.5369868989719));
#439955=CARTESIAN_POINT('Ctrl Pts',(-0.15100137827924,-2.73937933745604,
12.506462012331));
#439956=CARTESIAN_POINT('Ctrl Pts',(-0.151361257043662,-2.74590804906438,
12.4999388158272));
#439957=CARTESIAN_POINT('Ctrl Pts',(-0.151356999205927,-2.74583080584417,
12.4907030323752));
#439958=CARTESIAN_POINT('Ctrl Pts',(-0.164186551648245,-2.74092199308309,
12.5042014951932));
#439959=CARTESIAN_POINT('Ctrl Pts',(-0.169242651760944,-2.74489401382405,
12.4980716682127));
#439960=CARTESIAN_POINT('Ctrl Pts',(-0.176021078885824,-2.7444715319445,
12.4907355092743));
#439961=CARTESIAN_POINT('Ctrl Pts',(-0.167153370653351,-2.73567569093429,
12.5218047446509));
#439962=CARTESIAN_POINT('Ctrl Pts',(-0.174926379729319,-2.74456946408416,
12.5216906929434));
#439963=CARTESIAN_POINT('Ctrl Pts',(-0.186654053236909,-2.74365708892587,
12.5161988840776));
#439964=CARTESIAN_POINT('Ctrl Pts',(-0.164974248776966,-2.73097218009018,
12.5369868989719));
#439965=CARTESIAN_POINT('Ctrl Pts',(-0.171418360289289,-2.74488185148592,
12.5369868989719));
#439966=CARTESIAN_POINT('Ctrl Pts',(-0.186698955428321,-2.74365346078353,
12.5369868989719));
#439967=CARTESIAN_POINT('Origin',(-2.10137191087939E-32,-1.02994378190383E-30,
12.5));
#439968=CARTESIAN_POINT('Origin',(0.0777442925777901,-2.68237694712209,
12.5));
#439969=CARTESIAN_POINT('',(0.0777442925777901,-2.68237694712209,12.5893111709658));
#439970=CARTESIAN_POINT('',(0.0777442925777901,-2.68237694712209,13.8235269408515));
#439971=CARTESIAN_POINT('',(0.0777442925777901,-2.68237694712209,12.5));
#439972=CARTESIAN_POINT('',(0.0653458928111052,-2.71592620020509,13.7902182540695));
#439973=CARTESIAN_POINT('',(0.0777442925777901,-2.68237694712209,13.8235269408515));
#439974=CARTESIAN_POINT('',(0.0581609899471712,-2.73536807408357,13.7435492065112));
#439975=CARTESIAN_POINT('Origin',(0.081799530956857,-2.67140467892656,13.7445212918695));
#439976=CARTESIAN_POINT('',(0.0581609899471712,-2.73536807408357,12.5369868989719));
#439977=CARTESIAN_POINT('',(0.0581609899471712,-2.73536807408357,12.5));
#439978=CARTESIAN_POINT('Ctrl Pts',(0.0581609899471712,-2.73536807408357,
12.5369868989719));
#439979=CARTESIAN_POINT('Ctrl Pts',(0.0646839965340922,-2.71771724793141,
12.5544431401645));
#439980=CARTESIAN_POINT('Ctrl Pts',(0.0712116685486955,-2.70005379743926,
12.5718848856037));
#439981=CARTESIAN_POINT('Ctrl Pts',(0.0777442925777901,-2.68237694712209,
12.5893111709658));
#439982=CARTESIAN_POINT('Origin',(0.257188253544047,-2.9291091662376,12.5));
#439983=CARTESIAN_POINT('',(0.164990427905034,-2.73100702309001,13.7435492065112));
#439984=CARTESIAN_POINT('',(0.156244739002019,-2.71221547672782,13.7902182540695));
#439985=CARTESIAN_POINT('Origin',(0.133262580124126,-2.66283454072077,13.7418732680448));
#439986=CARTESIAN_POINT('',(0.141153018305427,-2.67978844069895,13.8235269408515));
#439987=CARTESIAN_POINT('',(0.156244739002019,-2.71221547672782,13.7902182540695));
#439988=CARTESIAN_POINT('',(0.141153018305427,-2.67978844069895,12.5893111709658));
#439989=CARTESIAN_POINT('',(0.141153018305427,-2.67978844069895,12.5));
#439990=CARTESIAN_POINT('',(0.164990427905034,-2.73100702309001,12.5369868989719));
#439991=CARTESIAN_POINT('Ctrl Pts',(0.141153018305427,-2.67978844069895,
12.5893111709658));
#439992=CARTESIAN_POINT('Ctrl Pts',(0.14910473297169,-2.69687400325064,
12.5718848856037));
#439993=CARTESIAN_POINT('Ctrl Pts',(0.157050419890744,-2.71394661419926,
12.5544431401645));
#439994=CARTESIAN_POINT('Ctrl Pts',(0.164990427905034,-2.73100702309001,
12.5369868989719));
#439995=CARTESIAN_POINT('',(0.164990427905034,-2.73100702309001,12.5));
#439996=CARTESIAN_POINT('Origin',(0.109987927613096,-2.69429284510378,12.5));
#439997=CARTESIAN_POINT('',(0.107467979553556,-2.66001107102548,13.8587068136939));
#439998=CARTESIAN_POINT('Ctrl Pts',(0.141153018311358,-2.67978844069603,
13.8235269408542));
#439999=CARTESIAN_POINT('Ctrl Pts',(0.140413642498288,-2.67819977054959,
13.8262006681044));
#440000=CARTESIAN_POINT('Ctrl Pts',(0.139499483687007,-2.67664730744221,
13.8288634856214));
#440001=CARTESIAN_POINT('Ctrl Pts',(0.138423816759605,-2.67512979298056,
13.8314912288862));
#440002=CARTESIAN_POINT('Ctrl Pts',(0.137314915107352,-2.67356539209496,
13.8342001611531));
#440003=CARTESIAN_POINT('Ctrl Pts',(0.136033544632342,-2.67203610781815,
13.8368750301949));
#440004=CARTESIAN_POINT('Ctrl Pts',(0.134549670915372,-2.67054803930163,
13.8394886372969));
#440005=CARTESIAN_POINT('Ctrl Pts',(0.134435067748838,-2.67043311216055,
13.8396904925131));
#440006=CARTESIAN_POINT('Ctrl Pts',(0.13431923853801,-2.67031844356835,
13.8398919674349));
#440007=CARTESIAN_POINT('Ctrl Pts',(0.134202160684652,-2.67020404369636,
13.8400930404591));
#440008=CARTESIAN_POINT('Ctrl Pts',(0.132378008963169,-2.66842161672634,
13.8432258934518));
#440009=CARTESIAN_POINT('Ctrl Pts',(0.13026083464185,-2.66671271363484,
13.8462331177034));
#440010=CARTESIAN_POINT('Ctrl Pts',(0.127859099286356,-2.66520813419667,
13.8489036603661));
#440011=CARTESIAN_POINT('Ctrl Pts',(0.127073223527637,-2.66471581829483,
13.849777493004));
#440012=CARTESIAN_POINT('Ctrl Pts',(0.12625698506697,-2.66424560584087,
13.85061494757));
#440013=CARTESIAN_POINT('Ctrl Pts',(0.125410989701583,-2.66380272259741,
13.8514076489583));
#440014=CARTESIAN_POINT('Ctrl Pts',(0.123621587492998,-2.66286596066418,
13.8530843267192));
#440015=CARTESIAN_POINT('Ctrl Pts',(0.121521919523597,-2.66196207099981,
13.8546805203176));
#440016=CARTESIAN_POINT('Ctrl Pts',(0.119179897922236,-2.66126884112717,
13.8559412814273));
#440017=CARTESIAN_POINT('Ctrl Pts',(0.118866459478416,-2.66117606448823,
13.8561100121513));
#440018=CARTESIAN_POINT('Ctrl Pts',(0.11854874454682,-2.66108701902086,
13.8562727473908));
#440019=CARTESIAN_POINT('Ctrl Pts',(0.118226973754739,-2.66100208182593,
13.8564289040185));
#440020=CARTESIAN_POINT('Ctrl Pts',(0.116767746883536,-2.66061689261589,
13.8571370725437));
#440021=CARTESIAN_POINT('Ctrl Pts',(0.115198876558341,-2.66031162512267,
13.8577210840553));
#440022=CARTESIAN_POINT('Ctrl Pts',(0.113575739692616,-2.66012695291767,
13.8581177131616));
#440023=CARTESIAN_POINT('Ctrl Pts',(0.11311860848455,-2.66007494286852,
13.8582294175695));
#440024=CARTESIAN_POINT('Ctrl Pts',(0.112657227229961,-2.66003232907039,
13.8583265086086));
#440025=CARTESIAN_POINT('Ctrl Pts',(0.112192942055877,-2.65999959428129,
13.8584082369006));
#440026=CARTESIAN_POINT('Ctrl Pts',(0.111525888763714,-2.65995256316754,
13.8585256585398));
#440027=CARTESIAN_POINT('Ctrl Pts',(0.110844525421073,-2.6599256621248,
13.8586122832068));
#440028=CARTESIAN_POINT('Ctrl Pts',(0.110166520719318,-2.65992037903644,
13.8586682984299));
#440029=CARTESIAN_POINT('Ctrl Pts',(0.10962418416636,-2.65991615308945,
13.8587131050557));
#440030=CARTESIAN_POINT('Ctrl Pts',(0.109078008326726,-2.65992547805404,
13.8587357943552));
#440031=CARTESIAN_POINT('Ctrl Pts',(0.108527936945158,-2.65994886141044,
13.8587355499465));
#440032=CARTESIAN_POINT('Ctrl Pts',(0.108172412696959,-2.65996397463117,
13.8587353919793));
#440033=CARTESIAN_POINT('Ctrl Pts',(0.107819104095523,-2.65998475845746,
13.8587257282814));
#440034=CARTESIAN_POINT('Ctrl Pts',(0.107467979553556,-2.66001107102548,
13.8587068136939));
#440035=CARTESIAN_POINT('Ctrl Pts',(0.107467979553556,-2.66001107102548,
13.8587068136939));
#440036=CARTESIAN_POINT('Ctrl Pts',(0.106313150076722,-2.66009761162726,
13.8586446046466));
#440037=CARTESIAN_POINT('Ctrl Pts',(0.105181916032446,-2.66024388385118,
13.858482427929));
#440038=CARTESIAN_POINT('Ctrl Pts',(0.104073401795672,-2.66044550372209,
13.8582284286032));
#440039=CARTESIAN_POINT('Ctrl Pts',(0.102936195136436,-2.66065234225626,
13.8579678548414));
#440040=CARTESIAN_POINT('Ctrl Pts',(0.101820395848112,-2.66091944289693,
13.857615680862));
#440041=CARTESIAN_POINT('Ctrl Pts',(0.100767737702107,-2.66122685196505,
13.8571944833187));
#440042=CARTESIAN_POINT('Ctrl Pts',(0.0981407216417111,-2.66199402273378,
13.8561433417727));
#440043=CARTESIAN_POINT('Ctrl Pts',(0.0957827227013604,-2.66304351832924,
13.8546163505474));
#440044=CARTESIAN_POINT('Ctrl Pts',(0.093754502726362,-2.66417768788552,
13.8528973491086));
#440045=CARTESIAN_POINT('Ctrl Pts',(0.0933839768605227,-2.66438488393034,
13.8525833129072));
#440046=CARTESIAN_POINT('Ctrl Pts',(0.0930243388479905,-2.66459482833731,
13.8522628768812));
#440047=CARTESIAN_POINT('Ctrl Pts',(0.0926757961602304,-2.6648062424995,
13.851937733538));
#440048=CARTESIAN_POINT('Ctrl Pts',(0.0905472943242078,-2.66609731945559,
13.8499521282529));
#440049=CARTESIAN_POINT('Ctrl Pts',(0.088623160818785,-2.66757500479494,
13.847639871647));
#440050=CARTESIAN_POINT('Ctrl Pts',(0.0869555867092282,-2.66909791820874,
13.8452109780794));
#440051=CARTESIAN_POINT('Ctrl Pts',(0.086205310600268,-2.66978310847635,
13.8441181685877));
#440052=CARTESIAN_POINT('Ctrl Pts',(0.0855063319983435,-2.67047712429546,
13.8430021611332));
#440053=CARTESIAN_POINT('Ctrl Pts',(0.0848601393738974,-2.67116655249071,
13.8418824960098));
#440054=CARTESIAN_POINT('Ctrl Pts',(0.0833373699532803,-2.67279120763798,
13.8392439765549));
#440055=CARTESIAN_POINT('Ctrl Pts',(0.0820321778432484,-2.67446546559834,
13.8364981347964));
#440056=CARTESIAN_POINT('Ctrl Pts',(0.0809141226483275,-2.67617271473482,
13.8336931113419));
#440057=CARTESIAN_POINT('Ctrl Pts',(0.079825207891543,-2.6778354669734,
13.8309611966328));
#440058=CARTESIAN_POINT('Ctrl Pts',(0.0789131832822403,-2.67953148850894,
13.8281701127186));
#440059=CARTESIAN_POINT('Ctrl Pts',(0.0781883844852199,-2.68125352738293,
13.8253580685121));
#440060=CARTESIAN_POINT('Ctrl Pts',(0.0780312473237982,-2.6816268672693,
13.8247484142933));
#440061=CARTESIAN_POINT('Ctrl Pts',(0.0778830802481646,-2.68200139682803,
13.8241378483365));
#440062=CARTESIAN_POINT('Ctrl Pts',(0.0777442925777901,-2.68237694712209,
13.8235269408515));
#440063=CARTESIAN_POINT('',(0.108708163673209,-2.65994236726223,12.5969504640361));
#440064=CARTESIAN_POINT('Origin',(0.109989081477175,-2.69432591096847,12.584524458991));
#440065=CARTESIAN_POINT('Origin',(0.109989081477175,-2.69432591096847,12.584524458991));
#440066=CARTESIAN_POINT('Ctrl Pts',(0.141153018305427,-2.67978844069895,
12.5893111709658));
#440067=CARTESIAN_POINT('Ctrl Pts',(0.136370695980246,-2.66951283717712,
12.5770542771492));
#440068=CARTESIAN_POINT('Ctrl Pts',(0.12050688364808,-2.67353068898434,
12.5737548217797));
#440069=CARTESIAN_POINT('Ctrl Pts',(0.151610352235496,-2.70225773700608,
12.5663937883685));
#440070=CARTESIAN_POINT('Ctrl Pts',(0.146821929394034,-2.69196902552492,
12.5540940315303));
#440071=CARTESIAN_POINT('Ctrl Pts',(0.130909746733166,-2.69600244073795,
12.5508374392248));
#440072=CARTESIAN_POINT('Ctrl Pts',(0.162057134843887,-2.72470436206883,
12.5434499600945));
#440073=CARTESIAN_POINT('Ctrl Pts',(0.157253143134597,-2.71438219832273,
12.5311293540533));
#440074=CARTESIAN_POINT('Ctrl Pts',(0.141303516703331,-2.71845174145023,
12.5278936106989));
#440075=CARTESIAN_POINT('Ctrl Pts',(0.172494192629982,-2.7471300917566,
12.5204817579905));
#440076=CARTESIAN_POINT('Ctrl Pts',(0.167666424444766,-2.73675684035417,
12.5081597038247));
#440077=CARTESIAN_POINT('Ctrl Pts',(0.151688912883333,-2.74088033028371,
12.5049254088044));
#440078=CARTESIAN_POINT('Ctrl Pts',(0.164990427905034,-2.73100702309001,
12.5369868989719));
#440079=CARTESIAN_POINT('Ctrl Pts',(0.165383472766402,-2.73185154479352,
12.5342545179733));
#440080=CARTESIAN_POINT('Ctrl Pts',(0.165645479457248,-2.73271015390558,
12.5314872231885));
#440081=CARTESIAN_POINT('Ctrl Pts',(0.165708221792586,-2.73355079919908,
12.5287124745063));
#440082=CARTESIAN_POINT('Ctrl Pts',(0.165764805944844,-2.73430893485067,
12.5262100684184));
#440083=CARTESIAN_POINT('Ctrl Pts',(0.165658283869168,-2.73505176820016,
12.5237004536639));
#440084=CARTESIAN_POINT('Ctrl Pts',(0.165321207164616,-2.73578264429546,
12.5212220730815));
#440085=CARTESIAN_POINT('Ctrl Pts',(0.16506314578782,-2.73634219317223,
12.5193246583486));
#440086=CARTESIAN_POINT('Ctrl Pts',(0.164666290656814,-2.73690115527121,
12.517417831369));
#440087=CARTESIAN_POINT('Ctrl Pts',(0.164041812144491,-2.73741999174944,
12.5155812248347));
#440088=CARTESIAN_POINT('Ctrl Pts',(0.163775780941654,-2.73764101887792,
12.5147988205793));
#440089=CARTESIAN_POINT('Ctrl Pts',(0.163468347488137,-2.73785520143648,
12.5140295443047));
#440090=CARTESIAN_POINT('Ctrl Pts',(0.163112844721882,-2.73806160040939,
12.5132817086137));
#440091=CARTESIAN_POINT('Ctrl Pts',(0.162574839376482,-2.73837395733388,
12.5121499604604));
#440092=CARTESIAN_POINT('Ctrl Pts',(0.161911533537851,-2.73866904796622,
12.5110494206568));
#440093=CARTESIAN_POINT('Ctrl Pts',(0.161097646294455,-2.73891952684504,
12.5100666561695));
#440094=CARTESIAN_POINT('Ctrl Pts',(0.160630314113512,-2.73906335124046,
12.5095023550641));
#440095=CARTESIAN_POINT('Ctrl Pts',(0.160107743198438,-2.73919350489643,
12.5089719619137));
#440096=CARTESIAN_POINT('Ctrl Pts',(0.159538184953438,-2.73930135058482,
12.5085043804652));
#440097=CARTESIAN_POINT('Ctrl Pts',(0.158704710652061,-2.7394591687019,
12.5078201359221));
#440098=CARTESIAN_POINT('Ctrl Pts',(0.157746217039477,-2.73957260594112,
12.5072563000949));
#440099=CARTESIAN_POINT('Ctrl Pts',(0.156726680840859,-2.73962556560587,
12.5068768744332));
#440100=CARTESIAN_POINT('Ctrl Pts',(0.155991525056544,-2.73966375316991,
12.5066032824114));
#440101=CARTESIAN_POINT('Ctrl Pts',(0.155211718308491,-2.73967122688161,
12.5064197834844));
#440102=CARTESIAN_POINT('Ctrl Pts',(0.154430831801786,-2.73965015412842,
12.5063282718343));
#440103=CARTESIAN_POINT('Ctrl Pts',(0.153290979258348,-2.73961939443274,
12.5061946931565));
#440104=CARTESIAN_POINT('Ctrl Pts',(0.152124434430004,-2.73952821524961,
12.5062515701262));
#440105=CARTESIAN_POINT('Ctrl Pts',(0.151002390083283,-2.73939769282737,
12.5064436508398));
#440106=CARTESIAN_POINT('',(0.120506883648079,-2.67353068898434,12.5737548217797));
#440107=CARTESIAN_POINT('Origin',(0.121207360262335,-2.68907125951804,12.5893111709658));
#440108=CARTESIAN_POINT('Ctrl Pts',(0.151002390083283,-2.73939769282737,
12.5064436508398));
#440109=CARTESIAN_POINT('Ctrl Pts',(0.146487826858497,-2.72964786684735,
12.5164271754438));
#440110=CARTESIAN_POINT('Ctrl Pts',(0.141971663658479,-2.71989408824766,
12.5264061185523));
#440111=CARTESIAN_POINT('Ctrl Pts',(0.137453843274561,-2.71013621821805,
12.536380305637));
#440112=CARTESIAN_POINT('Ctrl Pts',(0.131807484107369,-2.69794085979033,
12.5488460165097));
#440113=CARTESIAN_POINT('Ctrl Pts',(0.126158534784632,-2.68573910696496,
12.5613043021964));
#440114=CARTESIAN_POINT('Ctrl Pts',(0.12050688364808,-2.67353068898434,
12.5737548217797));
#440115=CARTESIAN_POINT('Ctrl Pts',(0.0777442925777903,-2.68237694712209,
12.5893111709658));
#440116=CARTESIAN_POINT('Ctrl Pts',(0.0816731450388711,-2.67174573115689,
12.5770542771492));
#440117=CARTESIAN_POINT('Ctrl Pts',(0.0978116640663786,-2.67445716591614,
12.5737548217797));
#440118=CARTESIAN_POINT('Ctrl Pts',(0.0814098777526247,-2.67245811509199,
12.5928319619712));
#440119=CARTESIAN_POINT('Ctrl Pts',(0.0871060609854467,-2.6664425591784,
12.5821634970842));
#440120=CARTESIAN_POINT('Ctrl Pts',(0.099138094406165,-2.67084070356696,
12.5773203894503));
#440121=CARTESIAN_POINT('Ctrl Pts',(0.0932406545772418,-2.66059991880985,
12.5969440695591));
#440122=CARTESIAN_POINT('Ctrl Pts',(0.0972562914093082,-2.66041770085005,
12.5878292599214));
#440123=CARTESIAN_POINT('Ctrl Pts',(0.103356273079777,-2.66661564548747,
12.5813877129824));
#440124=CARTESIAN_POINT('Ctrl Pts',(0.123809925774304,-2.65929803401389,
12.596957478804));
#440125=CARTESIAN_POINT('Ctrl Pts',(0.119823969208925,-2.65947898541016,
12.5878468778671));
#440126=CARTESIAN_POINT('Ctrl Pts',(0.114297692806488,-2.66615564258733,
12.5814011370086));
#440127=CARTESIAN_POINT('Ctrl Pts',(0.136684674550041,-2.67018747160734,
12.5928371701607));
#440128=CARTESIAN_POINT('Ctrl Pts',(0.130517498435897,-2.66466470015807,
12.5821692192952));
#440129=CARTESIAN_POINT('Ctrl Pts',(0.118885151398158,-2.67002308838229,
12.5773318885715));
#440130=CARTESIAN_POINT('Ctrl Pts',(0.141153018305476,-2.67978844069892,
12.5893111709658));
#440131=CARTESIAN_POINT('Ctrl Pts',(0.136370695980294,-2.6695128371771,
12.5770542771492));
#440132=CARTESIAN_POINT('Ctrl Pts',(0.120506883648129,-2.67353068898432,
12.5737548217797));
#440133=CARTESIAN_POINT('',(0.0978116640663786,-2.67445716591615,12.5737548217797));
#440134=CARTESIAN_POINT('Origin',(0.0983802190003859,-2.69000312183037,
12.5893111709658));
#440135=CARTESIAN_POINT('Ctrl Pts',(0.120506883648129,-2.67353068898432,
12.5737548217797));
#440136=CARTESIAN_POINT('Ctrl Pts',(0.120113885752202,-2.67260880380448,
12.5746934679442));
#440137=CARTESIAN_POINT('Ctrl Pts',(0.119510496091739,-2.67166051252229,
12.5756680099006));
#440138=CARTESIAN_POINT('Ctrl Pts',(0.118768172763169,-2.67079191610057,
12.5765688348656));
#440139=CARTESIAN_POINT('Ctrl Pts',(0.118571650879716,-2.67056196481359,
12.5768073183026));
#440140=CARTESIAN_POINT('Ctrl Pts',(0.118365621796738,-2.6703374846426,
12.5770407398754));
#440141=CARTESIAN_POINT('Ctrl Pts',(0.118151836512603,-2.67012007490227,
12.5772674179684));
#440142=CARTESIAN_POINT('Ctrl Pts',(0.117274519516509,-2.66922788411801,
12.5781976435658));
#440143=CARTESIAN_POINT('Ctrl Pts',(0.116208711112566,-2.66841199814016,
12.5790594849312));
#440144=CARTESIAN_POINT('Ctrl Pts',(0.114997023664009,-2.66776585090409,
12.5797571720116));
#440145=CARTESIAN_POINT('Ctrl Pts',(0.114207565722877,-2.6673448627464,
12.580211740231));
#440146=CARTESIAN_POINT('Ctrl Pts',(0.113311472037167,-2.66699336155614,
12.5806009430798));
#440147=CARTESIAN_POINT('Ctrl Pts',(0.112365354094484,-2.66675258468255,
12.5808812374708));
#440148=CARTESIAN_POINT('Ctrl Pts',(0.111552324910359,-2.66654567747125,
12.5811221033394));
#440149=CARTESIAN_POINT('Ctrl Pts',(0.110685682238033,-2.66641640941177,
12.581287365893));
#440150=CARTESIAN_POINT('Ctrl Pts',(0.109813110705442,-2.66638032334846,
12.581359338449));
#440151=CARTESIAN_POINT('Ctrl Pts',(0.109691841280325,-2.66637530813081,
12.5813693411482));
#440152=CARTESIAN_POINT('Ctrl Pts',(0.109570439731087,-2.6663720355171,
12.5813775999465));
#440153=CARTESIAN_POINT('Ctrl Pts',(0.109449014989987,-2.66637048892921,
12.5813841266931));
#440154=CARTESIAN_POINT('Ctrl Pts',(0.109243003230692,-2.66636786495581,
12.5813952001081));
#440155=CARTESIAN_POINT('Ctrl Pts',(0.109035537190336,-2.66637080063471,
12.5814007534795));
#440156=CARTESIAN_POINT('Ctrl Pts',(0.108826710017423,-2.6663794918774,
12.5814005856065));
#440157=CARTESIAN_POINT('Ctrl Pts',(0.107870780865955,-2.66641927698838,
12.5813998171494));
#440158=CARTESIAN_POINT('Ctrl Pts',(0.106952363184188,-2.66657658103314,
12.58127954464));
#440159=CARTESIAN_POINT('Ctrl Pts',(0.106071675905653,-2.66682134627691,
12.5810700125799));
#440160=CARTESIAN_POINT('Ctrl Pts',(0.105007905947459,-2.66711699482262,
12.5808169217085));
#440161=CARTESIAN_POINT('Ctrl Pts',(0.104003569558322,-2.66755639984867,
12.5804173076348));
#440162=CARTESIAN_POINT('Ctrl Pts',(0.103136246654913,-2.66807719380877,
12.5799304713245));
#440163=CARTESIAN_POINT('Ctrl Pts',(0.102061360342698,-2.66872262159235,
12.5793271277669));
#440164=CARTESIAN_POINT('Ctrl Pts',(0.101113659827898,-2.66950548591178,
12.5785808224116));
#440165=CARTESIAN_POINT('Ctrl Pts',(0.1003128929177,-2.67036833480848,12.5777485681082));
#440166=CARTESIAN_POINT('Ctrl Pts',(0.0991196624909412,-2.67165407419672,
12.576508418016));
#440167=CARTESIAN_POINT('Ctrl Pts',(0.0982576973188824,-2.67310191243109,
12.5750928681475));
#440168=CARTESIAN_POINT('Ctrl Pts',(0.0978116640663786,-2.67445716591614,
12.5737548217797));
#440169=CARTESIAN_POINT('Ctrl Pts',(0.0978116640663786,-2.67445716591614,
12.5737548217797));
#440170=CARTESIAN_POINT('Ctrl Pts',(0.0816731450388708,-2.67174573115689,
12.5770542771492));
#440171=CARTESIAN_POINT('Ctrl Pts',(0.0777442925777901,-2.68237694712209,
12.5893111709658));
#440172=CARTESIAN_POINT('Ctrl Pts',(0.0892763545231182,-2.69769858250746,
12.5508408821982));
#440173=CARTESIAN_POINT('Ctrl Pts',(0.0730883661518879,-2.69497557734355,
12.55409748406));
#440174=CARTESIAN_POINT('Ctrl Pts',(0.0691545014812997,-2.70562035601753,
12.5663972313419));
#440175=CARTESIAN_POINT('Ctrl Pts',(0.080748275692504,-2.72091688854494,
12.52790050457));
#440176=CARTESIAN_POINT('Ctrl Pts',(0.0645200291598312,-2.71816093284563,
12.5311362602938));
#440177=CARTESIAN_POINT('Ctrl Pts',(0.0605733760725459,-2.72884031613277,
12.5434568539655));
#440178=CARTESIAN_POINT('Ctrl Pts',(0.0722268526561591,-2.74411387524132,
12.5049357605811));
#440179=CARTESIAN_POINT('Ctrl Pts',(0.0559664200791695,-2.74130643558952,
12.5081700652078));
#440180=CARTESIAN_POINT('Ctrl Pts',(0.0520002376530914,-2.75203866398107,
12.5204921097672));
#440181=CARTESIAN_POINT('Ctrl Pts',(0.0727864012058899,-2.74259066961817,
12.5064436508395));
#440182=CARTESIAN_POINT('Ctrl Pts',(0.0715899150693781,-2.74282997844734,
12.5062361689309));
#440183=CARTESIAN_POINT('Ctrl Pts',(0.0703354627390177,-2.74302781921991,
12.5061871075061));
#440184=CARTESIAN_POINT('Ctrl Pts',(0.0691123928730676,-2.74315076938917,
12.5063648335164));
#440185=CARTESIAN_POINT('Ctrl Pts',(0.0685567990978748,-2.74320662093993,
12.5064455676329));
#440186=CARTESIAN_POINT('Ctrl Pts',(0.0679999097957444,-2.74324757834277,
12.506574497099));
#440187=CARTESIAN_POINT('Ctrl Pts',(0.0674655256239186,-2.74327083734875,
12.5067492519495));
#440188=CARTESIAN_POINT('Ctrl Pts',(0.0663916598874039,-2.74331757722413,
12.5071004286051));
#440189=CARTESIAN_POINT('Ctrl Pts',(0.0653691580536572,-2.74329375765344,
12.5076537929612));
#440190=CARTESIAN_POINT('Ctrl Pts',(0.0644745439694499,-2.74321062230247,
12.5083435010503));
#440191=CARTESIAN_POINT('Ctrl Pts',(0.0644182226665065,-2.7432053884353,
12.5083869222963));
#440192=CARTESIAN_POINT('Ctrl Pts',(0.0643624032032485,-2.74319990701827,
12.5084308732336));
#440193=CARTESIAN_POINT('Ctrl Pts',(0.064307102256264,-2.7431941759338,
12.5084753333615));
#440194=CARTESIAN_POINT('Ctrl Pts',(0.0638635156715535,-2.74314820507212,
12.508831962269));
#440195=CARTESIAN_POINT('Ctrl Pts',(0.0634441527162526,-2.74308652014177,
12.509227847131));
#440196=CARTESIAN_POINT('Ctrl Pts',(0.0630610757559996,-2.74301372560217,
12.5096423454524));
#440197=CARTESIAN_POINT('Ctrl Pts',(0.0618606821053256,-2.74278561973258,
12.5109411997424));
#440198=CARTESIAN_POINT('Ctrl Pts',(0.0609409503657873,-2.74244389525738,
12.5124831113042));
#440199=CARTESIAN_POINT('Ctrl Pts',(0.0602360550834692,-2.74205654384529,
12.5140723025008));
#440200=CARTESIAN_POINT('Ctrl Pts',(0.0601700056234664,-2.74202024859372,
12.5142212114565));
#440201=CARTESIAN_POINT('Ctrl Pts',(0.0601058156470521,-2.74198356541646,
12.5143705582413));
#440202=CARTESIAN_POINT('Ctrl Pts',(0.0600434163783638,-2.74194655888611,
12.5145201959299));
#440203=CARTESIAN_POINT('Ctrl Pts',(0.0592418048692627,-2.74147115490679,
12.5164425148273));
#440204=CARTESIAN_POINT('Ctrl Pts',(0.0587027742224739,-2.74093533428272,
12.5184635205941));
#440205=CARTESIAN_POINT('Ctrl Pts',(0.0583390230378892,-2.74036182242016,
12.5205025929157));
#440206=CARTESIAN_POINT('Ctrl Pts',(0.0581280329330801,-2.74002916280799,
12.5216853356836));
#440207=CARTESIAN_POINT('Ctrl Pts',(0.0579759876853332,-2.73968468204338,
12.5228750347131));
#440208=CARTESIAN_POINT('Ctrl Pts',(0.0578676721343238,-2.73933845149886,
12.5240609649613));
#440209=CARTESIAN_POINT('Ctrl Pts',(0.0576018174252999,-2.73848864720195,
12.5269717671327));
#440210=CARTESIAN_POINT('Ctrl Pts',(0.0576018431583101,-2.73760128088103,
12.5299036066169));
#440211=CARTESIAN_POINT('Ctrl Pts',(0.0577822188798732,-2.73669028322723,
12.5328133004019));
#440212=CARTESIAN_POINT('Ctrl Pts',(0.0578688097291865,-2.7362529513076,
12.5342101228452));
#440213=CARTESIAN_POINT('Ctrl Pts',(0.0579973693552569,-2.73581082086395,
12.5356023438238));
#440214=CARTESIAN_POINT('Ctrl Pts',(0.0581609899471714,-2.73536807408357,
12.5369868989719));
#440215=CARTESIAN_POINT('Origin',(-4.36479134863697,-14.6883069150384,-1.23969978058422));
#440216=CARTESIAN_POINT('Ctrl Pts',(0.164972828967398,-2.73096911480167,
12.5369868989719));
#440217=CARTESIAN_POINT('Ctrl Pts',(0.171418610569547,-2.74488799418265,
12.5369868989719));
#440218=CARTESIAN_POINT('Ctrl Pts',(0.186707740121687,-2.74365275282046,
12.5369868989719));
#440219=CARTESIAN_POINT('Ctrl Pts',(0.167151815324024,-2.73567421257279,
12.5218025310015));
#440220=CARTESIAN_POINT('Ctrl Pts',(0.174927792427972,-2.74457309136637,
12.5216901060418));
#440221=CARTESIAN_POINT('Ctrl Pts',(0.186661135115968,-2.74365653468369,
12.5161920673677));
#440222=CARTESIAN_POINT('Ctrl Pts',(0.164186617639527,-2.74092241930334,
12.5042015548895));
#440223=CARTESIAN_POINT('Ctrl Pts',(0.169245524179631,-2.74489542945129,
12.4980677368513));
#440224=CARTESIAN_POINT('Ctrl Pts',(0.17602864357708,-2.74447108175938,
12.4907278922778));
#440225=CARTESIAN_POINT('Ctrl Pts',(0.1510012892348,-2.73937772206282,12.506463626192));
#440226=CARTESIAN_POINT('Ctrl Pts',(0.15136139457082,-2.74591054400155,
12.4999376786891));
#440227=CARTESIAN_POINT('Ctrl Pts',(0.151356996407733,-2.74583075508029,
12.4906970594712));
#440228=CARTESIAN_POINT('Origin',(0.184936085948126,-2.72172420427093,12.5369868989719));
#440229=CARTESIAN_POINT('Origin',(0.184936085948126,-2.72172420427093,14.));
#440230=CARTESIAN_POINT('Origin',(0.184936085948126,-2.72172420427093,13.7435492065112));
#440231=CARTESIAN_POINT('Ctrl Pts',(0.154543018014346,-2.70855898586017,
13.793642941384));
#440232=CARTESIAN_POINT('Ctrl Pts',(0.159080541277636,-2.7183731135158,
13.8071662555867));
#440233=CARTESIAN_POINT('Ctrl Pts',(0.175421077119549,-2.71357662813231,
13.8103758687955));
#440234=CARTESIAN_POINT('Ctrl Pts',(0.16155623652397,-2.72362804261103,
13.7804579775005));
#440235=CARTESIAN_POINT('Ctrl Pts',(0.167164334709864,-2.73573353336799,
13.7901904343351));
#440236=CARTESIAN_POINT('Ctrl Pts',(0.182801427860942,-2.73380033861611,
13.7927914348263));
#440237=CARTESIAN_POINT('Ctrl Pts',(0.165685182232128,-2.73249976341654,
13.7597120340895));
#440238=CARTESIAN_POINT('Ctrl Pts',(0.172180530716661,-2.74650681656974,
13.7635825532445));
#440239=CARTESIAN_POINT('Ctrl Pts',(0.187177625595774,-2.74571747422855,
13.7651073818884));
#440240=CARTESIAN_POINT('Ctrl Pts',(0.164876640121115,-2.7307624773432,
13.7381884353898));
#440241=CARTESIAN_POINT('Ctrl Pts',(0.171219137447652,-2.74444204744936,
13.7368803041982));
#440242=CARTESIAN_POINT('Ctrl Pts',(0.186321099980056,-2.74338357459246,
13.7363986145813));
#440243=CARTESIAN_POINT('Origin',(0.176190397045111,-2.70293265790873,13.7902182540695));
#440244=CARTESIAN_POINT('Ctrl Pts',(0.141151358129088,-2.67978487173929,
13.8235227101244));
#440245=CARTESIAN_POINT('Ctrl Pts',(0.145998485875386,-2.69021022741335,
13.8358800583119));
#440246=CARTESIAN_POINT('Ctrl Pts',(0.162035412684842,-2.68603374234037,
13.8390832900376));
#440247=CARTESIAN_POINT('Ctrl Pts',(0.146184156226102,-2.69059866351688,
13.8124254819053));
#440248=CARTESIAN_POINT('Ctrl Pts',(0.151040697278011,-2.7010442649666,
13.8247886449157));
#440249=CARTESIAN_POINT('Ctrl Pts',(0.167093591866549,-2.69684600861049,
13.8279860620657));
#440250=CARTESIAN_POINT('Ctrl Pts',(0.151214698786735,-2.70140760890482,
13.8013225099955));
#440251=CARTESIAN_POINT('Ctrl Pts',(0.156078359818992,-2.71186852832885,
13.8136962257787));
#440252=CARTESIAN_POINT('Ctrl Pts',(0.172149183841997,-2.70765338419096,
13.8168830918626));
#440253=CARTESIAN_POINT('Ctrl Pts',(0.156243073570434,-2.71221189646866,
13.7902140179785));
#440254=CARTESIAN_POINT('Ctrl Pts',(0.16111171114607,-2.72268352813243,
13.802602731458));
#440255=CARTESIAN_POINT('Ctrl Pts',(0.177202288601925,-2.71845606202867,
13.8057746032558));
#440256=CARTESIAN_POINT('Origin',(0.161098676348519,-2.67050562187986,13.8235269408515));
#440257=CARTESIAN_POINT('Ctrl Pts',(0.0777442925777901,-2.68237694712209,
13.8235269408515));
#440258=CARTESIAN_POINT('Ctrl Pts',(0.0736512963688843,-2.69345232525672,
13.8362179249168));
#440259=CARTESIAN_POINT('Ctrl Pts',(0.0568854566252772,-2.69020122978765,
13.8391868794938));
#440260=CARTESIAN_POINT('Ctrl Pts',(0.0814892059514253,-2.6722434582114,
13.8400110824519));
#440261=CARTESIAN_POINT('Ctrl Pts',(0.0749987388406147,-2.67993733236846,
13.8494522556836));
#440262=CARTESIAN_POINT('Ctrl Pts',(0.0631539172325783,-2.67356331569846,
13.85569149686));
#440263=CARTESIAN_POINT('Ctrl Pts',(0.0928970126972653,-2.66061333906781,
13.8586819406588));
#440264=CARTESIAN_POINT('Ctrl Pts',(0.0885473715845184,-2.66080482229236,
13.868010383617));
#440265=CARTESIAN_POINT('Ctrl Pts',(0.0821953318615578,-2.65435932323096,
13.8744918421245));
#440266=CARTESIAN_POINT('Ctrl Pts',(0.124158896587816,-2.65928438701428,
13.8587686893867));
#440267=CARTESIAN_POINT('Ctrl Pts',(0.128469823458744,-2.65909455173477,
13.8680909899357));
#440268=CARTESIAN_POINT('Ctrl Pts',(0.134237297290658,-2.65214957894116,
13.8745789365163));
#440269=CARTESIAN_POINT('Ctrl Pts',(0.136587174763426,-2.66997797731641,
13.8400379222776));
#440270=CARTESIAN_POINT('Ctrl Pts',(0.143686434594472,-2.67711035025669,
13.8494748685453));
#440271=CARTESIAN_POINT('Ctrl Pts',(0.1549677115719,-2.66979639817705,13.8557104837033));
#440272=CARTESIAN_POINT('Ctrl Pts',(0.141153018311358,-2.67978844069603,
13.8235269408542));
#440273=CARTESIAN_POINT('Ctrl Pts',(0.146135141549828,-2.69049334923498,
13.8362179249195));
#440274=CARTESIAN_POINT('Ctrl Pts',(0.162580199882306,-2.68588649993228,
13.8391868794965));
#440275=CARTESIAN_POINT('Origin',(0.0571083661551944,-2.67475077241381,
13.8235269408515));
#440276=CARTESIAN_POINT('Ctrl Pts',(0.0653472588786357,-2.71592250152398,
13.7902140241683));
#440277=CARTESIAN_POINT('Ctrl Pts',(0.061348351967527,-2.72675612229032,
13.8026027327198));
#440278=CARTESIAN_POINT('Ctrl Pts',(0.0449667433653299,-2.72385425532615,
13.8057746032556));
#440279=CARTESIAN_POINT('Ctrl Pts',(0.0694782524228607,-2.70474430510597,
13.8013225161808));
#440280=CARTESIAN_POINT('Ctrl Pts',(0.0654834323588351,-2.71556684365019,
13.8136962270464));
#440281=CARTESIAN_POINT('Ctrl Pts',(0.0491225158052474,-2.71267564755867,
13.8168830918628));
#440282=CARTESIAN_POINT('Ctrl Pts',(0.0736110268755906,-2.69356128966689,
13.8124254880875));
#440283=CARTESIAN_POINT('Ctrl Pts',(0.0696220545519912,-2.70436798087383,
13.8247886461867));
#440284=CARTESIAN_POINT('Ctrl Pts',(0.0532803842747332,-2.70149215494944,
13.8279860620656));
#440285=CARTESIAN_POINT('Ctrl Pts',(0.0777456543349514,-2.68237326011396,
13.8235227163066));
#440286=CARTESIAN_POINT('Ctrl Pts',(0.0737644137830837,-2.69315900565633,
13.8358800595847));
#440287=CARTESIAN_POINT('Ctrl Pts',(0.0574404327053244,-2.69030357704212,
13.8390832900376));
#440288=CARTESIAN_POINT('Origin',(0.0447099663885099,-2.7083000254968,13.7902182540695));
#440289=CARTESIAN_POINT('Ctrl Pts',(0.0582545094711805,-2.73511493683604,
13.7382347919292));
#440290=CARTESIAN_POINT('Ctrl Pts',(0.0530460535478754,-2.74927791165169,
13.7369371795942));
#440291=CARTESIAN_POINT('Ctrl Pts',(0.0378962811475617,-2.74944576050981,
13.7364597369711));
#440292=CARTESIAN_POINT('Ctrl Pts',(0.0575988118280146,-2.73688921262768,
13.7595490285574));
#440293=CARTESIAN_POINT('Ctrl Pts',(0.0522651429729168,-2.75138975685757,
13.7633824266926));
#440294=CARTESIAN_POINT('Ctrl Pts',(0.0372413290480186,-2.75181245705624,
13.7648920890506));
#440295=CARTESIAN_POINT('Ctrl Pts',(0.0609428338936695,-2.72784050329564,
13.780380659011));
#440296=CARTESIAN_POINT('Ctrl Pts',(0.0563344678206781,-2.74038481866723,
13.7901039518743));
#440297=CARTESIAN_POINT('Ctrl Pts',(0.0405839246479046,-2.73974776985598,
13.7926933640892));
#440298=CARTESIAN_POINT('Ctrl Pts',(0.0667554906511187,-2.71211182652376,
13.7936647693663));
#440299=CARTESIAN_POINT('Ctrl Pts',(0.0630345161656322,-2.7222670065233,
13.8072068914933));
#440300=CARTESIAN_POINT('Ctrl Pts',(0.0463415779082944,-2.71880433671745,
13.8104111085397));
#440301=CARTESIAN_POINT('Origin',(0.0375250635245752,-2.72774189937528,
13.7435492065112));
#440302=CARTESIAN_POINT('Origin',(0.0375250635245752,-2.72774189937529,
14.));
#440303=CARTESIAN_POINT('Origin',(0.0375250635245754,-2.72774189937529,
12.5369868989719));
#440304=CARTESIAN_POINT('Ctrl Pts',(0.0727859135099193,-2.74257229285171,
12.506462012331));
#440305=CARTESIAN_POINT('Ctrl Pts',(0.0729593828180789,-2.749108614171,
12.4999388158272));
#440306=CARTESIAN_POINT('Ctrl Pts',(0.0729573304486722,-2.74903128091793,
12.4907030323752));
#440307=CARTESIAN_POINT('Ctrl Pts',(0.0597703534725135,-2.74518452945416,
12.5042014951932));
#440308=CARTESIAN_POINT('Ctrl Pts',(0.0550548336806712,-2.74955545272149,
12.4980716682127));
#440309=CARTESIAN_POINT('Ctrl Pts',(0.0482645250175523,-2.74968688135409,
12.4907355092743));
#440310=CARTESIAN_POINT('Ctrl Pts',(0.0563857839834866,-2.7401975072345,
12.5218047446509));
#440311=CARTESIAN_POINT('Ctrl Pts',(0.0493635640314674,-2.74969525948866,
12.5216906929434));
#440312=CARTESIAN_POINT('Ctrl Pts',(0.0376005463445374,-2.74974183444874,
12.5161988840776));
#440313=CARTESIAN_POINT('Ctrl Pts',(0.0581742752125333,-2.73533202827181,
12.5369868989719));
#440314=CARTESIAN_POINT('Ctrl Pts',(0.0528853732995049,-2.74972067129591,
12.5369868989719));
#440315=CARTESIAN_POINT('Ctrl Pts',(0.0375554978341709,-2.7497418783242,
12.5369868989719));
#440316=CARTESIAN_POINT('Origin',(2.10137191088009E-32,-1.02994378190383E-30,
12.5));
#440317=CARTESIAN_POINT('Origin',(0.29612422802077,-2.66711467752317,12.5));
#440318=CARTESIAN_POINT('',(0.29612422802077,-2.66711467752317,12.5893111709658));
#440319=CARTESIAN_POINT('',(0.29612422802077,-2.66711467752317,13.8235269408515));
#440320=CARTESIAN_POINT('',(0.29612422802077,-2.66711467752317,12.5));
#440321=CARTESIAN_POINT('',(0.286501658488847,-2.70156288291627,13.7902182540695));
#440322=CARTESIAN_POINT('',(0.29612422802077,-2.66711467752317,13.8235269408515));
#440323=CARTESIAN_POINT('',(0.280925356007127,-2.72152570184805,13.7435492065112));
#440324=CARTESIAN_POINT('Origin',(0.299271631209852,-2.65584837906756,13.7445212918687));
#440325=CARTESIAN_POINT('',(0.280925356007127,-2.72152570184805,12.5369868989719));
#440326=CARTESIAN_POINT('',(0.280925356007127,-2.72152570184805,12.5));
#440327=CARTESIAN_POINT('Ctrl Pts',(0.280925356007127,-2.72152570184805,
12.5369868989719));
#440328=CARTESIAN_POINT('Ctrl Pts',(0.285987951634065,-2.70340192177036,
12.5544431401645));
#440329=CARTESIAN_POINT('Ctrl Pts',(0.29105416816395,-2.68526517908345,
12.5718848856037));
#440330=CARTESIAN_POINT('Ctrl Pts',(0.29612422802077,-2.66711467752317,
12.5893111709658));
#440331=CARTESIAN_POINT('Origin',(0.495082070418079,-2.89839956683834,12.5));
#440332=CARTESIAN_POINT('',(0.387043861680997,-2.70847157094224,13.7435492065112));
#440333=CARTESIAN_POINT('',(0.376795587855615,-2.69045540673698,13.7902182540695));
#440334=CARTESIAN_POINT('Origin',(0.349864895500878,-2.64311204102572,13.7418732680451));
#440335=CARTESIAN_POINT('',(0.359110979140394,-2.65936638433693,13.8235269408515));
#440336=CARTESIAN_POINT('',(0.376795587855615,-2.69045540673698,13.7902182540695));
#440337=CARTESIAN_POINT('',(0.359110979140394,-2.65936638433693,12.5893111709658));
#440338=CARTESIAN_POINT('',(0.359110979140394,-2.65936638433693,12.5));
#440339=CARTESIAN_POINT('',(0.387043861680997,-2.70847157094224,12.5369868989719));
#440340=CARTESIAN_POINT('Ctrl Pts',(0.359110979140394,-2.65936638433693,
12.5893111709658));
#440341=CARTESIAN_POINT('Ctrl Pts',(0.368428867094661,-2.67574695752327,
12.5718848856037));
#440342=CARTESIAN_POINT('Ctrl Pts',(0.377739691682666,-2.69211511351929,
12.5544431401645));
#440343=CARTESIAN_POINT('Ctrl Pts',(0.387043861680997,-2.70847157094224,
12.5369868989719));
#440344=CARTESIAN_POINT('',(0.387043861680997,-2.70847157094224,12.5));
#440345=CARTESIAN_POINT('Origin',(0.329231831327716,-2.67636277074664,12.5));
#440346=CARTESIAN_POINT('',(0.32392598534368,-2.64240046560444,13.8587068136939));
#440347=CARTESIAN_POINT('Ctrl Pts',(0.359110979146066,-2.65936638433354,
13.8235269408542));
#440348=CARTESIAN_POINT('Ctrl Pts',(0.358244572179592,-2.65784326634875,
13.8262006681044));
#440349=CARTESIAN_POINT('Ctrl Pts',(0.35720691500073,-2.65637048136405,
13.8288634856214));
#440350=CARTESIAN_POINT('Ctrl Pts',(0.356011135749757,-2.65494569314718,
13.8314912288862));
#440351=CARTESIAN_POINT('Ctrl Pts',(0.354778410680912,-2.65347688345567,
13.834200161153));
#440352=CARTESIAN_POINT('Ctrl Pts',(0.353376652994714,-2.65205713133551,
13.8368750301949));
#440353=CARTESIAN_POINT('Ctrl Pts',(0.35177642534648,-2.65069496372777,
13.8394886372968));
#440354=CARTESIAN_POINT('Ctrl Pts',(0.351652835883593,-2.65058976021926,
13.8396904925131));
#440355=CARTESIAN_POINT('Ctrl Pts',(0.351528045530105,-2.65048491433332,
13.8398919674349));
#440356=CARTESIAN_POINT('Ctrl Pts',(0.351402032592036,-2.65038043804941,
13.8400930404591));
#440357=CARTESIAN_POINT('Ctrl Pts',(0.349438666239621,-2.64875262725799,
13.8432258934518));
#440358=CARTESIAN_POINT('Ctrl Pts',(0.34718924517456,-2.64722197976263,
13.8462331177034));
#440359=CARTESIAN_POINT('Ctrl Pts',(0.344672864203285,-2.64591817041652,
13.8489036603661));
#440360=CARTESIAN_POINT('Ctrl Pts',(0.343849475064886,-2.64549154882528,
13.8497774930041));
#440361=CARTESIAN_POINT('Ctrl Pts',(0.342997625890127,-2.6450894319766,
13.85061494757));
#440362=CARTESIAN_POINT('Ctrl Pts',(0.342118346408661,-2.64471697886672,
13.8514076489583));
#440363=CARTESIAN_POINT('Ctrl Pts',(0.340258543494292,-2.64392918682355,
13.8530843267192));
#440364=CARTESIAN_POINT('Ctrl Pts',(0.338092186597919,-2.64319944720935,
13.8546805203176));
#440365=CARTESIAN_POINT('Ctrl Pts',(0.335701453210003,-2.6426994205047,
13.8559412814273));
#440366=CARTESIAN_POINT('Ctrl Pts',(0.33538149554936,-2.64263250071536,
13.8561100121513));
#440367=CARTESIAN_POINT('Ctrl Pts',(0.335057579755724,-2.64256964825588,
13.8562727473908));
#440368=CARTESIAN_POINT('Ctrl Pts',(0.334729956459484,-2.64251122098918,
13.8564289040185));
#440369=CARTESIAN_POINT('Ctrl Pts',(0.333244188548769,-2.64224625400127,
13.8571370725437));
#440370=CARTESIAN_POINT('Ctrl Pts',(0.331655656375487,-2.64206987975664,
13.8577210840554));
#440371=CARTESIAN_POINT('Ctrl Pts',(0.330022867864652,-2.64201812275619,
13.8581177131616));
#440372=CARTESIAN_POINT('Ctrl Pts',(0.329563018421135,-2.64200354620344,
13.8582294175695));
#440373=CARTESIAN_POINT('Ctrl Pts',(0.329099698954464,-2.64199868105471,
13.8583265086086));
#440374=CARTESIAN_POINT('Ctrl Pts',(0.328634290461799,-2.64200389873983,
13.8584082369006));
#440375=CARTESIAN_POINT('Ctrl Pts',(0.327965623262051,-2.64201139515416,
13.8585256585398));
#440376=CARTESIAN_POINT('Ctrl Pts',(0.327284334415004,-2.64204012106032,
13.8586122832068));
#440377=CARTESIAN_POINT('Ctrl Pts',(0.326608155097216,-2.64209011922848,
13.8586682984299));
#440378=CARTESIAN_POINT('Ctrl Pts',(0.326067278670486,-2.64213011280685,
13.8587131050557));
#440379=CARTESIAN_POINT('Ctrl Pts',(0.325523680257086,-2.64218392514477,
13.8587357943552));
#440380=CARTESIAN_POINT('Ctrl Pts',(0.324977345153289,-2.6422520666192,
13.8587355499465));
#440381=CARTESIAN_POINT('Ctrl Pts',(0.324624235750512,-2.64229610807868,
13.8587353919793));
#440382=CARTESIAN_POINT('Ctrl Pts',(0.324273796829112,-2.64234562067947,
13.8587257282814));
#440383=CARTESIAN_POINT('Ctrl Pts',(0.32392598534368,-2.64240046560444,
13.8587068136939));
#440384=CARTESIAN_POINT('Ctrl Pts',(0.32392598534368,-2.64240046560444,
13.8587068136939));
#440385=CARTESIAN_POINT('Ctrl Pts',(0.322782052329091,-2.64258084757279,
13.8586446046466));
#440386=CARTESIAN_POINT('Ctrl Pts',(0.321666504916931,-2.64281883916442,
13.858482427929));
#440387=CARTESIAN_POINT('Ctrl Pts',(0.320578113061042,-2.64311014236309,
13.8582284286032));
#440388=CARTESIAN_POINT('Ctrl Pts',(0.319461549623881,-2.64340898555914,
13.8579678548414));
#440389=CARTESIAN_POINT('Ctrl Pts',(0.318371234247498,-2.64376614544504,
13.857615680862));
#440390=CARTESIAN_POINT('Ctrl Pts',(0.317347135427535,-2.64415833304615,
13.8571944833187));
#440391=CARTESIAN_POINT('Ctrl Pts',(0.314791392086088,-2.64513707731437,
13.8561433417727));
#440392=CARTESIAN_POINT('Ctrl Pts',(0.312526782826766,-2.64637527960405,
13.8546163505474));
#440393=CARTESIAN_POINT('Ctrl Pts',(0.310597756934373,-2.64767099406172,
13.8528973491086));
#440394=CARTESIAN_POINT('Ctrl Pts',(0.31024535236395,-2.64790770197666,
13.8525833129072));
#440395=CARTESIAN_POINT('Ctrl Pts',(0.30990402343543,-2.64814626164768,
13.8522628768812));
#440396=CARTESIAN_POINT('Ctrl Pts',(0.3095738727116,-2.64838538181145,13.851937733538));
#440397=CARTESIAN_POINT('Ctrl Pts',(0.307557688047539,-2.64984565547516,
13.8499521282529));
#440398=CARTESIAN_POINT('Ctrl Pts',(0.305760402010941,-2.65147525868192,
13.847639871647));
#440399=CARTESIAN_POINT('Ctrl Pts',(0.304222508197929,-2.65312902749791,
13.8452109780794));
#440400=CARTESIAN_POINT('Ctrl Pts',(0.303530577938638,-2.65387309231953,
13.8441181685877));
#440401=CARTESIAN_POINT('Ctrl Pts',(0.302890493862539,-2.6546217721033,
13.8430021611332));
#440402=CARTESIAN_POINT('Ctrl Pts',(0.302302646188998,-2.65536157698095,
13.8418824960098));
#440403=CARTESIAN_POINT('Ctrl Pts',(0.300917368135071,-2.65710494606673,
13.8392439765549));
#440404=CARTESIAN_POINT('Ctrl Pts',(0.299752986510935,-2.65888001834563,
13.8364981347964));
#440405=CARTESIAN_POINT('Ctrl Pts',(0.298777808206391,-2.66067271862935,
13.8336931113419));
#440406=CARTESIAN_POINT('Ctrl Pts',(0.297828046467313,-2.66241869485869,
13.8309611966328));
#440407=CARTESIAN_POINT('Ctrl Pts',(0.297057298044904,-2.66418341149497,
13.8281701127186));
#440408=CARTESIAN_POINT('Ctrl Pts',(0.296475273110949,-2.66595879825733,
13.8253580685121));
#440409=CARTESIAN_POINT('Ctrl Pts',(0.296349089477127,-2.66634370402347,
13.8247484142932));
#440410=CARTESIAN_POINT('Ctrl Pts',(0.296231943051216,-2.66672906435817,
13.8241378483365));
#440411=CARTESIAN_POINT('Ctrl Pts',(0.29612422802077,-2.66711467752317,
13.8235269408515));
#440412=CARTESIAN_POINT('',(0.325156442858397,-2.64223090392825,12.5969504640361));
#440413=CARTESIAN_POINT('Origin',(0.329235676527349,-2.67639563253677,12.584524458991));
#440414=CARTESIAN_POINT('Origin',(0.329235676527349,-2.67639563253677,12.584524458991));
#440415=CARTESIAN_POINT('Ctrl Pts',(0.359110979140394,-2.65936638433693,
12.5893111709658));
#440416=CARTESIAN_POINT('Ctrl Pts',(0.353507012517157,-2.64951477570456,
12.5770542771492));
#440417=CARTESIAN_POINT('Ctrl Pts',(0.338023477934059,-2.65481230641886,
12.5737548217797));
#440418=CARTESIAN_POINT('Ctrl Pts',(0.371364973398318,-2.6809085461178,
12.5663937883685));
#440419=CARTESIAN_POINT('Ctrl Pts',(0.365753858137378,-2.67104437039046,
12.5540940315304));
#440420=CARTESIAN_POINT('Ctrl Pts',(0.3502233827359,-2.6763613553554,12.5508374392248));
#440421=CARTESIAN_POINT('Ctrl Pts',(0.383606603526242,-2.70242897212149,
12.5434499600945));
#440422=CARTESIAN_POINT('Ctrl Pts',(0.377977244531486,-2.69253272444612,
12.5311293540533));
#440423=CARTESIAN_POINT('Ctrl Pts',(0.362412394711088,-2.69788876912786,
12.5278936106989));
#440424=CARTESIAN_POINT('Ctrl Pts',(0.395836838023433,-2.72392936494126,
12.5204817579905));
#440425=CARTESIAN_POINT('Ctrl Pts',(0.390179617548724,-2.71398413760305,
12.5081597038247));
#440426=CARTESIAN_POINT('Ctrl Pts',(0.374591372548831,-2.71939622248025,
12.5049254088044));
#440427=CARTESIAN_POINT('Ctrl Pts',(0.387043861680996,-2.70847157094224,
12.5369868989719));
#440428=CARTESIAN_POINT('Ctrl Pts',(0.387504435077004,-2.70928124576439,
12.5342545179733));
#440429=CARTESIAN_POINT('Ctrl Pts',(0.387835554575771,-2.7101156419478,
12.5314872231885));
#440430=CARTESIAN_POINT('Ctrl Pts',(0.387966608536756,-2.71094837598063,
12.5287124745063));
#440431=CARTESIAN_POINT('Ctrl Pts',(0.38808479950371,-2.71169937686467,
12.5262100684184));
#440432=CARTESIAN_POINT('Ctrl Pts',(0.388039179685566,-2.71244842103555,
12.5237004536639));
#440433=CARTESIAN_POINT('Ctrl Pts',(0.387762797762829,-2.71320434008162,
12.5212220730815));
#440434=CARTESIAN_POINT('Ctrl Pts',(0.387551203492031,-2.7137830615036,
12.5193246583486));
#440435=CARTESIAN_POINT('Ctrl Pts',(0.387201229463953,-2.7143725110797,
12.517417831369));
#440436=CARTESIAN_POINT('Ctrl Pts',(0.386621118841982,-2.71494052196848,
12.5155812248348));
#440437=CARTESIAN_POINT('Ctrl Pts',(0.386373988598914,-2.71518249766018,
12.5147988205793));
#440438=CARTESIAN_POINT('Ctrl Pts',(0.386085035971748,-2.71542102622447,
12.5140295443047));
#440439=CARTESIAN_POINT('Ctrl Pts',(0.385747539544028,-2.7156557151976,
12.5132817086137));
#440440=CARTESIAN_POINT('Ctrl Pts',(0.385236784356158,-2.71601088521044,
12.5121499604604));
#440441=CARTESIAN_POINT('Ctrl Pts',(0.384599738239009,-2.71635905953673,
12.5110494206568));
#440442=CARTESIAN_POINT('Ctrl Pts',(0.38380897549223,-2.71667504433384,
12.5100666561695));
#440443=CARTESIAN_POINT('Ctrl Pts',(0.383354921343995,-2.7168564820767,
12.5095023550641));
#440444=CARTESIAN_POINT('Ctrl Pts',(0.382844697971814,-2.717028797038,12.5089719619137));
#440445=CARTESIAN_POINT('Ctrl Pts',(0.382285825309685,-2.71718270816325,
12.5085043804652));
#440446=CARTESIAN_POINT('Ctrl Pts',(0.381467987966943,-2.71740793704672,
12.5078201359221));
#440447=CARTESIAN_POINT('Ctrl Pts',(0.380521929851842,-2.71759912296043,
12.5072563000953));
#440448=CARTESIAN_POINT('Ctrl Pts',(0.379510102780157,-2.71773500807132,
12.5068768744336));
#440449=CARTESIAN_POINT('Ctrl Pts',(0.378780505807059,-2.71783299059064,
12.5066032824118));
#440450=CARTESIAN_POINT('Ctrl Pts',(0.378003902977509,-2.71790400092369,
12.5064197834844));
#440451=CARTESIAN_POINT('Ctrl Pts',(0.377223897181221,-2.71794664778805,
12.5063282718343));
#440452=CARTESIAN_POINT('Ctrl Pts',(0.376085330202333,-2.71800889900688,
12.5061946931565));
#440453=CARTESIAN_POINT('Ctrl Pts',(0.374915235005781,-2.71801310744814,
12.5062515701262));
#440454=CARTESIAN_POINT('Ctrl Pts',(0.373786285379937,-2.7179744763593,
12.5064436508398));
#440455=CARTESIAN_POINT('',(0.338023477934059,-2.65481230641886,12.5737548217797));
#440456=CARTESIAN_POINT('Origin',(0.33998832454028,-2.67024407163914,12.5893111709658));
#440457=CARTESIAN_POINT('Ctrl Pts',(0.373786285379937,-2.7179744763593,
12.5064436508398));
#440458=CARTESIAN_POINT('Ctrl Pts',(0.368492042661514,-2.70862507093491,
12.5164271754438));
#440459=CARTESIAN_POINT('Ctrl Pts',(0.363195883116453,-2.6992718564557,
12.5264061185523));
#440460=CARTESIAN_POINT('Ctrl Pts',(0.357897738412111,-2.68991469923633,
12.536380305637));
#440461=CARTESIAN_POINT('Ctrl Pts',(0.351276132111214,-2.6782201505481,
12.5488460165097));
#440462=CARTESIAN_POINT('Ctrl Pts',(0.344651423070526,-2.66651943986077,
12.5613043021964));
#440463=CARTESIAN_POINT('Ctrl Pts',(0.338023477934059,-2.65481230641886,
12.5737548217797));
#440464=CARTESIAN_POINT('Ctrl Pts',(0.296124228020771,-2.66711467752317,
12.5893111709658));
#440465=CARTESIAN_POINT('Ctrl Pts',(0.299173464752837,-2.65619859810282,
12.5770542771492));
#440466=CARTESIAN_POINT('Ctrl Pts',(0.315479291294226,-2.65758557166315,
12.5737548217797));
#440467=CARTESIAN_POINT('Ctrl Pts',(0.298969139370926,-2.65693007036703,
12.5928319619712));
#440468=CARTESIAN_POINT('Ctrl Pts',(0.3041560453713,-2.65047023890524,12.5821634970842));
#440469=CARTESIAN_POINT('Ctrl Pts',(0.316506532791419,-2.65387302640742,
12.5773203894503));
#440470=CARTESIAN_POINT('Ctrl Pts',(0.309793997178513,-2.64414701311201,
12.5969440695591));
#440471=CARTESIAN_POINT('Ctrl Pts',(0.313781419854935,-2.64363808978626,
12.5878292599214));
#440472=CARTESIAN_POINT('Ctrl Pts',(0.32036629436647,-2.64931820613859,
12.5813877129824));
#440473=CARTESIAN_POINT('Ctrl Pts',(0.340155435950474,-2.64035778083647,
12.596957478804));
#440474=CARTESIAN_POINT('Ctrl Pts',(0.336197491545416,-2.6408630225958,
12.5878468778671));
#440475=CARTESIAN_POINT('Ctrl Pts',(0.331233812914824,-2.64796790657724,
12.5814011370086));
#440476=CARTESIAN_POINT('Ctrl Pts',(0.353874935318227,-2.65016157317609,
12.5928371701607));
#440477=CARTESIAN_POINT('Ctrl Pts',(0.347278122829823,-2.64515986039979,
12.5821692192952));
#440478=CARTESIAN_POINT('Ctrl Pts',(0.336121239852369,-2.65144856330225,
12.5773318885715));
#440479=CARTESIAN_POINT('Ctrl Pts',(0.35911097914044,-2.6593663843369,12.5893111709658));
#440480=CARTESIAN_POINT('Ctrl Pts',(0.353507012517204,-2.64951477570453,
12.5770542771492));
#440481=CARTESIAN_POINT('Ctrl Pts',(0.338023477934106,-2.65481230641883,
12.5737548217797));
#440482=CARTESIAN_POINT('',(0.315479291294226,-2.65758557166315,12.5737548217797));
#440483=CARTESIAN_POINT('Origin',(0.317313094137216,-2.67303345718619,12.5893111709658));
#440484=CARTESIAN_POINT('Ctrl Pts',(0.338023477934106,-2.65481230641883,
12.5737548217797));
#440485=CARTESIAN_POINT('Ctrl Pts',(0.337556645505732,-2.6539255217128,
12.5746934679442));
#440486=CARTESIAN_POINT('Ctrl Pts',(0.336877969031576,-2.65302956765055,
12.5756680099006));
#440487=CARTESIAN_POINT('Ctrl Pts',(0.336067317050609,-2.65222436765443,
12.5765688348656));
#440488=CARTESIAN_POINT('Ctrl Pts',(0.335852705912866,-2.65201119986932,
12.5768073183026));
#440489=CARTESIAN_POINT('Ctrl Pts',(0.335629065156764,-2.65180425992053,
12.5770407398754));
#440490=CARTESIAN_POINT('Ctrl Pts',(0.335398270313362,-2.65160499907852,
12.5772674179684));
#440491=CARTESIAN_POINT('Ctrl Pts',(0.334451150685588,-2.6507872864653,
12.5781976435658));
#440492=CARTESIAN_POINT('Ctrl Pts',(0.333322386389675,-2.65006098856013,
12.5790594849312));
#440493=CARTESIAN_POINT('Ctrl Pts',(0.332062063732868,-2.6495157551015,
12.5797571720116));
#440494=CARTESIAN_POINT('Ctrl Pts',(0.331240918204794,-2.64916051589835,
12.580211740231));
#440495=CARTESIAN_POINT('Ctrl Pts',(0.330319155586716,-2.64888322425361,
12.5806009430798));
#440496=CARTESIAN_POINT('Ctrl Pts',(0.329356560222978,-2.64872036594087,
12.5808812374708));
#440497=CARTESIAN_POINT('Ctrl Pts',(0.328529371467841,-2.64858041662254,
12.5811221033394));
#440498=CARTESIAN_POINT('Ctrl Pts',(0.327655075930601,-2.64852221811518,
12.581287365893));
#440499=CARTESIAN_POINT('Ctrl Pts',(0.326782466458639,-2.64855737480574,
12.581359338449));
#440500=CARTESIAN_POINT('Ctrl Pts',(0.326661191760731,-2.64856226085977,
12.5813693411482));
#440501=CARTESIAN_POINT('Ctrl Pts',(0.326539927416732,-2.6485688944887,
12.5813775999465));
#440502=CARTESIAN_POINT('Ctrl Pts',(0.326418780645168,-2.64857725029061,
12.5813841266931));
#440503=CARTESIAN_POINT('Ctrl Pts',(0.326213240494816,-2.64859142691917,
12.5813952001081));
#440504=CARTESIAN_POINT('Ctrl Pts',(0.326006704065679,-2.64861126323816,
12.5814007534795));
#440505=CARTESIAN_POINT('Ctrl Pts',(0.32579928016492,-2.6486369469147,12.5814005856065));
#440506=CARTESIAN_POINT('Ctrl Pts',(0.324849774644737,-2.64875451674426,
12.5813998171494));
#440507=CARTESIAN_POINT('Ctrl Pts',(0.32394723466203,-2.64898615694003,
12.58127954464));
#440508=CARTESIAN_POINT('Ctrl Pts',(0.323089428437419,-2.64930189193674,
12.5810700125799));
#440509=CARTESIAN_POINT('Ctrl Pts',(0.322053296187149,-2.64968326386346,
12.5808169217085));
#440510=CARTESIAN_POINT('Ctrl Pts',(0.321088117233356,-2.65020306954505,
12.5804173076348));
#440511=CARTESIAN_POINT('Ctrl Pts',(0.320266129817922,-2.65079282547467,
12.5799304713245));
#440512=CARTESIAN_POINT('Ctrl Pts',(0.31924742845746,-2.65152371886375,
12.5793271277669));
#440513=CARTESIAN_POINT('Ctrl Pts',(0.318366692047735,-2.65238122465672,
12.5785808224116));
#440514=CARTESIAN_POINT('Ctrl Pts',(0.317638919818751,-2.65330647243203,
12.5777485681082));
#440515=CARTESIAN_POINT('Ctrl Pts',(0.316554459464165,-2.65468519298571,
12.576508418016));
#440516=CARTESIAN_POINT('Ctrl Pts',(0.315813374667285,-2.65619847182142,
12.5750928681475));
#440517=CARTESIAN_POINT('Ctrl Pts',(0.315479291294226,-2.65758557166315,
12.5737548217797));
#440518=CARTESIAN_POINT('Ctrl Pts',(0.315479291294226,-2.65758557166315,
12.5737548217797));
#440519=CARTESIAN_POINT('Ctrl Pts',(0.299173464752836,-2.65619859810282,
12.5770542771492));
#440520=CARTESIAN_POINT('Ctrl Pts',(0.29612422802077,-2.66711467752317,
12.5893111709658));
#440521=CARTESIAN_POINT('Ctrl Pts',(0.308866773504334,-2.68144536132376,
12.5508408821982));
#440522=CARTESIAN_POINT('Ctrl Pts',(0.292510699128997,-2.6800508880691,
12.55409748406));
#440523=CARTESIAN_POINT('Ctrl Pts',(0.289457572351812,-2.69098089361103,
12.5663972313419));
#440524=CARTESIAN_POINT('Ctrl Pts',(0.302259578642799,-2.70528152795879,
12.52790050457));
#440525=CARTESIAN_POINT('Ctrl Pts',(0.285860694287199,-2.70385749522283,
12.5311362602938));
#440526=CARTESIAN_POINT('Ctrl Pts',(0.282797642242939,-2.71482303260862,
12.5434568539655));
#440527=CARTESIAN_POINT('Ctrl Pts',(0.295657279704717,-2.72909590368206,
12.5049357605811));
#440528=CARTESIAN_POINT('Ctrl Pts',(0.279222119981116,-2.72762318176361,
12.5081700652078));
#440529=CARTESIAN_POINT('Ctrl Pts',(0.276143910946933,-2.7386429802385,
12.5204921097672));
#440530=CARTESIAN_POINT('Ctrl Pts',(0.29609081100377,-2.72753215799855,
12.5064436508395));
#440531=CARTESIAN_POINT('Ctrl Pts',(0.294917811967386,-2.7278681952751,
12.5062361689309));
#440532=CARTESIAN_POINT('Ctrl Pts',(0.293683659583299,-2.72816762725951,
12.5061871075061));
#440533=CARTESIAN_POINT('Ctrl Pts',(0.29247468096164,-2.72838985987073,
12.5063648335164));
#440534=CARTESIAN_POINT('Ctrl Pts',(0.291925488298788,-2.72849081163062,
12.5064455676329));
#440535=CARTESIAN_POINT('Ctrl Pts',(0.291373790408432,-2.72857702439911,
12.506574497099));
#440536=CARTESIAN_POINT('Ctrl Pts',(0.290843080180768,-2.72864376328366,
12.5067492519495));
#440537=CARTESIAN_POINT('Ctrl Pts',(0.289776597377541,-2.72877787766278,
12.5071004286051));
#440538=CARTESIAN_POINT('Ctrl Pts',(0.288755556318065,-2.72883748074164,
12.5076537929613));
#440539=CARTESIAN_POINT('Ctrl Pts',(0.287857142685456,-2.72882754136973,
12.5083435010505));
#440540=CARTESIAN_POINT('Ctrl Pts',(0.28780058217834,-2.72882691562687,
12.5083869222964));
#440541=CARTESIAN_POINT('Ctrl Pts',(0.287744501663466,-2.72882600225326,
12.5084308732337));
#440542=CARTESIAN_POINT('Ctrl Pts',(0.287688917589329,-2.72882479777907,
12.5084753333615));
#440543=CARTESIAN_POINT('Ctrl Pts',(0.287243059950386,-2.72881513630635,
12.5088319622689));
#440544=CARTESIAN_POINT('Ctrl Pts',(0.286820064496226,-2.72878783860156,
12.509227847131));
#440545=CARTESIAN_POINT('Ctrl Pts',(0.286432328762188,-2.72874651060836,
12.5096423454524));
#440546=CARTESIAN_POINT('Ctrl Pts',(0.285217336576357,-2.72861700696867,
12.5109411997424));
#440547=CARTESIAN_POINT('Ctrl Pts',(0.284272811451165,-2.72835138622861,
12.5124831113042));
#440548=CARTESIAN_POINT('Ctrl Pts',(0.283538688913669,-2.72802277920583,
12.5140723025008));
#440549=CARTESIAN_POINT('Ctrl Pts',(0.283469900827844,-2.72799198836788,
12.5142212114565));
#440550=CARTESIAN_POINT('Ctrl Pts',(0.283402934418785,-2.72796065932985,
12.5143705582413));
#440551=CARTESIAN_POINT('Ctrl Pts',(0.28333772640274,-2.72792886205536,
12.5145201959299));
#440552=CARTESIAN_POINT('Ctrl Pts',(0.28250003235206,-2.72752037872336,
12.5164425148273));
#440553=CARTESIAN_POINT('Ctrl Pts',(0.281919120930104,-2.72703027700005,
12.518463520594));
#440554=CARTESIAN_POINT('Ctrl Pts',(0.281509833556556,-2.72648832254934,
12.5205025929157));
#440555=CARTESIAN_POINT('Ctrl Pts',(0.281272430657261,-2.72617396748687,
12.5216853356836));
#440556=CARTESIAN_POINT('Ctrl Pts',(0.281092812947214,-2.7258430260528,
12.5228750347131));
#440557=CARTESIAN_POINT('Ctrl Pts',(0.280956636803638,-2.72550677628481,
12.5240609649613));
#440558=CARTESIAN_POINT('Ctrl Pts',(0.280622399764832,-2.72468146926846,
12.5269717671326));
#440559=CARTESIAN_POINT('Ctrl Pts',(0.280550096819154,-2.72379705348828,
12.5299036066169));
#440560=CARTESIAN_POINT('Ctrl Pts',(0.280655617589308,-2.72287438480819,
12.5328133004019));
#440561=CARTESIAN_POINT('Ctrl Pts',(0.280706273703273,-2.72243145011636,
12.5342101228451));
#440562=CARTESIAN_POINT('Ctrl Pts',(0.280798367822096,-2.72198031202227,
12.5356023438238));
#440563=CARTESIAN_POINT('Ctrl Pts',(0.280925356007128,-2.72152570184805,
12.5369868989719));
#440564=CARTESIAN_POINT('Origin',(-3.15300310277255,-14.9950921493851,-1.23957475124779));
#440565=CARTESIAN_POINT('Ctrl Pts',(0.387023231424868,-2.70843522326725,
12.5369868989719));
#440566=CARTESIAN_POINT('Ctrl Pts',(0.394582083106558,-2.72178239768519,
12.5369868989719));
#440567=CARTESIAN_POINT('Ctrl Pts',(0.409719655703063,-2.71930506049086,
12.5369868989719));
#440568=CARTESIAN_POINT('Ctrl Pts',(0.389578476532465,-2.71294705759693,
12.5218025310015));
#440569=CARTESIAN_POINT('Ctrl Pts',(0.398053920948921,-2.72118251178293,
12.5216901060418));
#440570=CARTESIAN_POINT('Ctrl Pts',(0.409673514028607,-2.71931262851088,
12.5161920673677));
#440571=CARTESIAN_POINT('Ctrl Pts',(0.387050922869208,-2.71841949249145,
12.5042015548895));
#440572=CARTESIAN_POINT('Ctrl Pts',(0.392416833525845,-2.72196693492833,
12.4980677368514));
#440573=CARTESIAN_POINT('Ctrl Pts',(0.399142794376768,-2.72099111201602,
12.4907278922778));
#440574=CARTESIAN_POINT('Ctrl Pts',(0.373783560391716,-2.71795466177511,
12.5064636261921));
#440575=CARTESIAN_POINT('Ctrl Pts',(0.374674953142716,-2.72443639435991,
12.4999376786892));
#440576=CARTESIAN_POINT('Ctrl Pts',(0.374664066076346,-2.72435722942082,
12.4906970594712));
#440577=CARTESIAN_POINT('Origin',(0.40616651628111,-2.69759388364003,12.5369868989719));
#440578=CARTESIAN_POINT('Origin',(0.406166516281111,-2.69759388364003,14.));
#440579=CARTESIAN_POINT('Origin',(0.40616651628111,-2.69759388364003,13.7435492065112));
#440580=CARTESIAN_POINT('Ctrl Pts',(0.374801491253232,-2.68694978859957,
13.793642941384));
#440581=CARTESIAN_POINT('Ctrl Pts',(0.380123858796038,-2.69636141028476,
13.8071662555867));
#440582=CARTESIAN_POINT('Ctrl Pts',(0.396019064765778,-2.69024897944144,
13.8103758687955));
#440583=CARTESIAN_POINT('Ctrl Pts',(0.383019641876292,-2.70139706189109,
13.7804579775006));
#440584=CARTESIAN_POINT('Ctrl Pts',(0.389595789456672,-2.71300516056098,
13.7901904343351));
#440585=CARTESIAN_POINT('Ctrl Pts',(0.405023278151095,-2.7098038300957,
13.7927914348262));
#440586=CARTESIAN_POINT('Ctrl Pts',(0.387857976464934,-2.70990271537105,
13.7597120340895));
#440587=CARTESIAN_POINT('Ctrl Pts',(0.395473417080355,-2.72333373000905,
13.7635825532445));
#440588=CARTESIAN_POINT('Ctrl Pts',(0.4103562716347,-2.72132461168045,13.7651073818884));
#440589=CARTESIAN_POINT('Ctrl Pts',(0.386910519767921,-2.70823711366196,
13.7381884353898));
#440590=CARTESIAN_POINT('Ctrl Pts',(0.394346924916404,-2.72135419371408,
13.7368803041981));
#440591=CARTESIAN_POINT('Ctrl Pts',(0.409312361550093,-2.71906829269215,
13.7363986145813));
#440592=CARTESIAN_POINT('Origin',(0.395918242455728,-2.67957771943477,13.7902182540695));
#440593=CARTESIAN_POINT('Ctrl Pts',(0.359109033584807,-2.65936296257247,
13.8235227101244));
#440594=CARTESIAN_POINT('Ctrl Pts',(0.364789796185102,-2.66935854282569,
13.8358800583119));
#440595=CARTESIAN_POINT('Ctrl Pts',(0.380432939137515,-2.66388879624773,
13.8390832900376));
#440596=CARTESIAN_POINT('Ctrl Pts',(0.365006509881553,-2.66973055258288,
13.8124254819052));
#440597=CARTESIAN_POINT('Ctrl Pts',(0.370698304684128,-2.67974554397383,
13.8247886449158));
#440598=CARTESIAN_POINT('Ctrl Pts',(0.386355587722459,-2.67425279703263,
13.8279860620657));
#440599=CARTESIAN_POINT('Ctrl Pts',(0.370901343121275,-2.68009349617674,
13.8013225099955));
#440600=CARTESIAN_POINT('Ctrl Pts',(0.376601482770181,-2.6901231742282,
13.8136962257787));
#440601=CARTESIAN_POINT('Ctrl Pts',(0.392275259073256,-2.68461213428257,
13.8168830918626));
#440602=CARTESIAN_POINT('Ctrl Pts',(0.376793636141255,-2.69045197413897,
13.7902140179785));
#440603=CARTESIAN_POINT('Ctrl Pts',(0.382499608921472,-2.7004919231516,
13.802602731458));
#440604=CARTESIAN_POINT('Ctrl Pts',(0.39819206857489,-2.69496699215227,
13.8057746032558));
#440605=CARTESIAN_POINT('Origin',(0.378233633740507,-2.64848869703471,13.8235269408515));
#440606=CARTESIAN_POINT('Ctrl Pts',(0.29612422802077,-2.66711467752317,
13.8235269408515));
#440607=CARTESIAN_POINT('Ctrl Pts',(0.292947597055868,-2.67848682043926,
13.8362179249168));
#440608=CARTESIAN_POINT('Ctrl Pts',(0.275972549798502,-2.67661311430774,
13.8391868794938));
#440609=CARTESIAN_POINT('Ctrl Pts',(0.299030707083143,-2.65670966175486,
13.8400110824519));
#440610=CARTESIAN_POINT('Ctrl Pts',(0.293188958636471,-2.6649069685045,
13.8494522556837));
#440611=CARTESIAN_POINT('Ctrl Pts',(0.280864008163117,-2.6595196237721,
13.85569149686));
#440612=CARTESIAN_POINT('Ctrl Pts',(0.309452592614156,-2.6441883987186,
13.8586819406588));
#440613=CARTESIAN_POINT('Ctrl Pts',(0.305133032233838,-2.6447337809293,
13.868010383617));
#440614=CARTESIAN_POINT('Ctrl Pts',(0.298276760388452,-2.6388274789412,
13.8744918421245));
#440615=CARTESIAN_POINT('Ctrl Pts',(0.340502133235233,-2.64031573488514,
13.8587686893867));
#440616=CARTESIAN_POINT('Ctrl Pts',(0.344783242515,-2.63977515070619,13.8680909899357));
#440617=CARTESIAN_POINT('Ctrl Pts',(0.349965445796858,-2.63238318407672,
13.8745789365163));
#440618=CARTESIAN_POINT('Ctrl Pts',(0.353760684224538,-2.64996072309787,
13.8400379222776));
#440619=CARTESIAN_POINT('Ctrl Pts',(0.361417676462514,-2.65649070807303,
13.8494748685453));
#440620=CARTESIAN_POINT('Ctrl Pts',(0.372065260927524,-2.64828156376166,
13.8557104837033));
#440621=CARTESIAN_POINT('Ctrl Pts',(0.359110979146066,-2.65936638433354,
13.8235269408542));
#440622=CARTESIAN_POINT('Ctrl Pts',(0.364949074205902,-2.6696295838767,
13.8362179249195));
#440623=CARTESIAN_POINT('Ctrl Pts',(0.380963911977324,-2.66369763856245,
13.8391868794965));
#440624=CARTESIAN_POINT('Origin',(0.274935361904325,-2.66119589786016,13.8235269408515));
#440625=CARTESIAN_POINT('Ctrl Pts',(0.286502718534059,-2.70155908519502,
13.7902140241682));
#440626=CARTESIAN_POINT('Ctrl Pts',(0.28340015832271,-2.71268260601928,
13.8026027327198));
#440627=CARTESIAN_POINT('Ctrl Pts',(0.266836529074531,-2.71112564795856,
13.8057746032556));
#440628=CARTESIAN_POINT('Ctrl Pts',(0.289708839756668,-2.69008136897932,
13.8013225161808));
#440629=CARTESIAN_POINT('Ctrl Pts',(0.286609449489767,-2.70119351134068,
13.8136962270464));
#440630=CARTESIAN_POINT('Ctrl Pts',(0.270067313214294,-2.6996455020521,
13.8168830918628));
#440631=CARTESIAN_POINT('Ctrl Pts',(0.292916343166988,-2.67859870461692,
13.8124254880875));
#440632=CARTESIAN_POINT('Ctrl Pts',(0.289821489477539,-2.68969457572655,
13.8247886461868));
#440633=CARTESIAN_POINT('Ctrl Pts',(0.273299788249313,-2.6881603167119,
13.8279860620656));
#440634=CARTESIAN_POINT('Ctrl Pts',(0.29612528472141,-2.66711089178739,
13.8235227163065));
#440635=CARTESIAN_POINT('Ctrl Pts',(0.293036429810745,-2.67818525671626,
13.8358800595847));
#440636=CARTESIAN_POINT('Ctrl Pts',(0.276534021492804,-2.67666988530749,
13.8390832900376));
#440637=CARTESIAN_POINT('Origin',(0.265312792372402,-2.69564410325325,13.7902182540695));
#440638=CARTESIAN_POINT('Ctrl Pts',(0.280997931316952,-2.72126578418443,
13.7382347919292));
#440639=CARTESIAN_POINT('Ctrl Pts',(0.276961220031182,-2.73580617038043,
13.7369371795942));
#440640=CARTESIAN_POINT('Ctrl Pts',(0.261875538488943,-2.73720830782959,
13.7364597369712));
#440641=CARTESIAN_POINT('Ctrl Pts',(0.280489035402188,-2.72308760166488,
13.7595490285574));
#440642=CARTESIAN_POINT('Ctrl Pts',(0.276355042861444,-2.7379746400571,
13.7633824266926));
#440643=CARTESIAN_POINT('Ctrl Pts',(0.261415673428344,-2.73962051406489,
13.7648920890506));
#440644=CARTESIAN_POINT('Ctrl Pts',(0.283084376695607,-2.71379643232392,
13.780380659011));
#440645=CARTESIAN_POINT('Ctrl Pts',(0.27951382273908,-2.72667463213789,
13.7901039518744));
#440646=CARTESIAN_POINT('Ctrl Pts',(0.263763762807191,-2.72732351854348,
13.7926933640892));
#440647=CARTESIAN_POINT('Ctrl Pts',(0.287595659142386,-2.69764630593868,
13.7936647693663));
#440648=CARTESIAN_POINT('Ctrl Pts',(0.284714807338599,-2.70807098937891,
13.8072068914933));
#440649=CARTESIAN_POINT('Ctrl Pts',(0.267795173721219,-2.70598047075885,
13.8104111085397));
#440650=CARTESIAN_POINT('Origin',(0.259736489890682,-2.71560692218503,13.7435492065112));
#440651=CARTESIAN_POINT('Origin',(0.259736489890682,-2.71560692218504,14.));
#440652=CARTESIAN_POINT('Origin',(0.259736489890682,-2.71560692218504,12.5369868989719));
#440653=CARTESIAN_POINT('Ctrl Pts',(0.296088827053501,-2.72751388213103,
12.506462012331));
#440654=CARTESIAN_POINT('Ctrl Pts',(0.296794490024615,-2.7340143150213,
12.4999388158272));
#440655=CARTESIAN_POINT('Ctrl Pts',(0.296786141106247,-2.73393740637542,
12.4907030323752));
#440656=CARTESIAN_POINT('Ctrl Pts',(0.283329496752321,-2.73117831570525,
12.5042014951932));
#440657=CARTESIAN_POINT('Ctrl Pts',(0.278985938287572,-2.73591905372581,
12.4980716682127));
#440658=CARTESIAN_POINT('Ctrl Pts',(0.272228936470035,-2.73660351823466,
12.4907355092744));
#440659=CARTESIAN_POINT('Ctrl Pts',(0.279549700530896,-2.72648376122487,
12.5218047446509));
#440660=CARTESIAN_POINT('Ctrl Pts',(0.273325001417991,-2.7365222866091,
12.5216906929433));
#440661=CARTESIAN_POINT('Ctrl Pts',(0.2616049204937,-2.73752750173883,12.5161988840775));
#440662=CARTESIAN_POINT('Ctrl Pts',(0.280935658998568,-2.72148869310332,
12.5369868989719));
#440663=CARTESIAN_POINT('Ctrl Pts',(0.27683716345445,-2.7362605537104,12.5369868989719));
#440664=CARTESIAN_POINT('Ctrl Pts',(0.2615600254548,-2.7375312173401,12.5369868989719));
#440665=CARTESIAN_POINT('Origin',(6.2901314492746E-32,-1.0265181555254E-30,
12.5));
#440666=CARTESIAN_POINT('Origin',(0.512533505583331,-2.63410319978829,12.5));
#440667=CARTESIAN_POINT('',(0.512533505583331,-2.63410319978829,12.5893111709658));
#440668=CARTESIAN_POINT('',(0.512533505583331,-2.63410319978829,13.8235269408515));
#440669=CARTESIAN_POINT('',(0.512533505583331,-2.63410319978829,12.5));
#440670=CARTESIAN_POINT('',(0.505750802898792,-2.66922111036814,13.7902182540695));
#440671=CARTESIAN_POINT('',(0.512533505583331,-2.63410319978829,13.8235269408515));
#440672=CARTESIAN_POINT('',(0.501820210172278,-2.68957202508688,13.7435492065112));
#440673=CARTESIAN_POINT('Origin',(0.514752128131608,-2.62261784643754,13.7445212918704));
#440674=CARTESIAN_POINT('',(0.501820210172278,-2.68957202508688,12.5369868989719));
#440675=CARTESIAN_POINT('',(0.501820210172278,-2.68957202508688,12.5));
#440676=CARTESIAN_POINT('Ctrl Pts',(0.501820210172278,-2.68957202508688,
12.5369868989719));
#440677=CARTESIAN_POINT('Ctrl Pts',(0.505388704100603,-2.67109590184984,
12.5544431401645));
#440678=CARTESIAN_POINT('Ctrl Pts',(0.508959750310632,-2.6526065639984,
12.5718848856037));
#440679=CARTESIAN_POINT('Ctrl Pts',(0.512533505583331,-2.63410319978829,
12.5893111709658));
#440680=CARTESIAN_POINT('Origin',(0.729681197796271,-2.84840159652405,12.5));
#440681=CARTESIAN_POINT('',(0.606521582415215,-2.6679116873562,13.7435492065112));
#440682=CARTESIAN_POINT('',(0.594838924238927,-2.65079079990821,13.7902182540695));
#440683=CARTESIAN_POINT('Origin',(0.564138917721049,-2.60580006677933,13.7418732680446));
#440684=CARTESIAN_POINT('',(0.574679115658322,-2.62124668345171,13.8235269408515));
#440685=CARTESIAN_POINT('',(0.594838924238927,-2.65079079990821,13.7902182540695));
#440686=CARTESIAN_POINT('',(0.574679115658322,-2.62124668345171,12.5893111709658));
#440687=CARTESIAN_POINT('',(0.574679115658322,-2.62124668345171,12.5));
#440688=CARTESIAN_POINT('',(0.606521582415215,-2.6679116873562,12.5369868989719));
#440689=CARTESIAN_POINT('Ctrl Pts',(0.574679115658322,-2.62124668345171,
12.5893111709658));
#440690=CARTESIAN_POINT('Ctrl Pts',(0.585301167893602,-2.63681325726075,
12.5718848856037));
#440691=CARTESIAN_POINT('Ctrl Pts',(0.595915168149101,-2.65236803092658,
12.5544431401645));
#440692=CARTESIAN_POINT('Ctrl Pts',(0.606521582415215,-2.6679116873562,
12.5369868989719));
#440693=CARTESIAN_POINT('',(0.606521582415216,-2.6679116873562,12.5));
#440694=CARTESIAN_POINT('Origin',(0.546284751524279,-2.64062194371896,12.5));
#440695=CARTESIAN_POINT('',(0.538228317145139,-2.60720512105024,13.8587068136939));
#440696=CARTESIAN_POINT('Ctrl Pts',(0.574679115663699,-2.62124668344787,
13.8235269408542));
#440697=CARTESIAN_POINT('Ctrl Pts',(0.573691443339235,-2.61979925372363,
13.8262006681044));
#440698=CARTESIAN_POINT('Ctrl Pts',(0.572537193230111,-2.61841594800268,
13.8288634856214));
#440699=CARTESIAN_POINT('Ctrl Pts',(0.571229259369184,-2.61709336776109,
13.8314912288862));
#440700=CARTESIAN_POINT('Ctrl Pts',(0.569880914465689,-2.61572992394984,
13.8342001611531));
#440701=CARTESIAN_POINT('Ctrl Pts',(0.568368098034423,-2.61442915220244,
13.8368750301949));
#440702=CARTESIAN_POINT('Ctrl Pts',(0.566662165705898,-2.61320195050416,
13.8394886372969));
#440703=CARTESIAN_POINT('Ctrl Pts',(0.566530412414152,-2.61310717074023,
13.8396904925131));
#440704=CARTESIAN_POINT('Ctrl Pts',(0.56639749137723,-2.61301284529263,
13.8398919674349));
#440705=CARTESIAN_POINT('Ctrl Pts',(0.566263381949771,-2.61291898786924,
13.8400930404591));
#440706=CARTESIAN_POINT('Ctrl Pts',(0.56417386684557,-2.61145662606867,
13.8432258934518));
#440707=CARTESIAN_POINT('Ctrl Pts',(0.561807168562829,-2.61011442037599,
13.8462331177034));
#440708=CARTESIAN_POINT('Ctrl Pts',(0.559192888075967,-2.60902005775802,
13.8489036603661));
#440709=CARTESIAN_POINT('Ctrl Pts',(0.558337465076753,-2.60866196957368,
13.8497774930041));
#440710=CARTESIAN_POINT('Ctrl Pts',(0.557455674103611,-2.60833062435157,
13.85061494757));
#440711=CARTESIAN_POINT('Ctrl Pts',(0.556548961965943,-2.60803107998926,
13.8514076489583));
#440712=CARTESIAN_POINT('Ctrl Pts',(0.554631135027298,-2.60739750046221,
13.8530843267192));
#440713=CARTESIAN_POINT('Ctrl Pts',(0.552412505951619,-2.6068467671949,
13.8546805203176));
#440714=CARTESIAN_POINT('Ctrl Pts',(0.549988970713338,-2.60654327125346,
13.8559412814274));
#440715=CARTESIAN_POINT('Ctrl Pts',(0.549664623101367,-2.60650265365389,
13.8561100121513));
#440716=CARTESIAN_POINT('Ctrl Pts',(0.549336662051907,-2.60646641247506,
13.8562727473908));
#440717=CARTESIAN_POINT('Ctrl Pts',(0.549005366530546,-2.60643488396042,
13.8564289040185));
#440718=CARTESIAN_POINT('Ctrl Pts',(0.547502945120647,-2.60629190250622,
13.8571370725437));
#440719=CARTESIAN_POINT('Ctrl Pts',(0.545905322518818,-2.60624559525167,
13.8577210840553));
#440720=CARTESIAN_POINT('Ctrl Pts',(0.544273748301041,-2.60632709789007,
13.8581177131616));
#440721=CARTESIAN_POINT('Ctrl Pts',(0.543814240844234,-2.60635005183828,
13.8582294175695));
#440722=CARTESIAN_POINT('Ctrl Pts',(0.543352066480071,-2.60638296771572,
13.8583265086086));
#440723=CARTESIAN_POINT('Ctrl Pts',(0.542888631885539,-2.60642610315221,
13.8584082369006));
#440724=CARTESIAN_POINT('Ctrl Pts',(0.542222800648099,-2.60648807720723,
13.8585256585398));
#440725=CARTESIAN_POINT('Ctrl Pts',(0.541546120161518,-2.60657223889611,
13.8586122832068));
#440726=CARTESIAN_POINT('Ctrl Pts',(0.540876266089495,-2.60667718559124,
13.8586682984299));
#440727=CARTESIAN_POINT('Ctrl Pts',(0.540340449232375,-2.60676113254431,
13.8587131050557));
#440728=CARTESIAN_POINT('Ctrl Pts',(0.539803045802962,-2.60685907414333,
13.8587357943552));
#440729=CARTESIAN_POINT('Ctrl Pts',(0.539264082746913,-2.6069715202655,
13.8587355499465));
#440730=CARTESIAN_POINT('Ctrl Pts',(0.538915738074296,-2.6070441968751,
13.8587353919793));
#440731=CARTESIAN_POINT('Ctrl Pts',(0.53857050094606,-2.60712210875223,
13.8587257282814));
#440732=CARTESIAN_POINT('Ctrl Pts',(0.538228317145139,-2.60720512105024,
13.8587068136939));
#440733=CARTESIAN_POINT('Ctrl Pts',(0.538228317145139,-2.60720512105024,
13.8587068136939));
#440734=CARTESIAN_POINT('Ctrl Pts',(0.537102893278351,-2.6074781439729,
13.8586446046466));
#440735=CARTESIAN_POINT('Ctrl Pts',(0.536010456282359,-2.60780627113746,
13.858482427929));
#440736=CARTESIAN_POINT('Ctrl Pts',(0.534949429875656,-2.60818531908914,
13.8582284286032));
#440737=CARTESIAN_POINT('Ctrl Pts',(0.533860940206025,-2.6085741781949,
13.8579678548414));
#440738=CARTESIAN_POINT('Ctrl Pts',(0.532803364610523,-2.60901902048591,
13.857615680862));
#440739=CARTESIAN_POINT('Ctrl Pts',(0.531814640325284,-2.60949337667623,
13.8571944833187));
#440740=CARTESIAN_POINT('Ctrl Pts',(0.529347177753043,-2.61067718106234,
13.8561433417727));
#440741=CARTESIAN_POINT('Ctrl Pts',(0.527191028775726,-2.61209585001429,
13.8546163505474));
#440742=CARTESIAN_POINT('Ctrl Pts',(0.525374034314981,-2.61354448660743,
13.8528973491086));
#440743=CARTESIAN_POINT('Ctrl Pts',(0.525042096234256,-2.61380913114036,
13.8525833129072));
#440744=CARTESIAN_POINT('Ctrl Pts',(0.524721347877461,-2.61407471850016,
13.8522628768812));
#440745=CARTESIAN_POINT('Ctrl Pts',(0.524411786216164,-2.61433995336027,
13.851937733538));
#440746=CARTESIAN_POINT('Ctrl Pts',(0.522521336100362,-2.6159597058513,
13.8499521282529));
#440747=CARTESIAN_POINT('Ctrl Pts',(0.520862858174635,-2.617730382185,13.847639871647));
#440748=CARTESIAN_POINT('Ctrl Pts',(0.519464879087762,-2.61950400084454,
13.8452109780794));
#440749=CARTESIAN_POINT('Ctrl Pts',(0.518835899359852,-2.62030198859155,
13.8441181685877));
#440750=CARTESIAN_POINT('Ctrl Pts',(0.518258969463494,-2.62110034999956,
13.8430021611332));
#440751=CARTESIAN_POINT('Ctrl Pts',(0.517733378770134,-2.62188560828021,
13.8418824960098));
#440752=CARTESIAN_POINT('Ctrl Pts',(0.516494810879796,-2.62373608947086,
13.8392439765549));
#440753=CARTESIAN_POINT('Ctrl Pts',(0.515478988509157,-2.62560016325515,
13.8364981347964));
#440754=CARTESIAN_POINT('Ctrl Pts',(0.514653176745716,-2.62746638456149,
13.8336931113419));
#440755=CARTESIAN_POINT('Ctrl Pts',(0.51384888853202,-2.62928396559786,
13.8309611966328));
#440756=CARTESIAN_POINT('Ctrl Pts',(0.51322454550009,-2.63110563343681,
13.8281701127186));
#440757=CARTESIAN_POINT('Ctrl Pts',(0.512789167709108,-2.63292255318155,
13.8253580685121));
#440758=CARTESIAN_POINT('Ctrl Pts',(0.512694777334148,-2.63331646334309,
13.8247484142933));
#440759=CARTESIAN_POINT('Ctrl Pts',(0.512609431148093,-2.63371008994432,
13.8241378483365));
#440760=CARTESIAN_POINT('Ctrl Pts',(0.512533505583331,-2.63410319978829,
13.8235269408515));
#440761=CARTESIAN_POINT('',(0.539440859563399,-2.60693582986604,12.5969504640361));
#440762=CARTESIAN_POINT('Origin',(0.546291262470293,-2.6406543827447,12.584524458991));
#440763=CARTESIAN_POINT('Origin',(0.546291262470293,-2.6406543827447,12.584524458991));
#440764=CARTESIAN_POINT('Ctrl Pts',(0.574679115658322,-2.62124668345171,
12.5893111709658));
#440765=CARTESIAN_POINT('Ctrl Pts',(0.568290798210319,-2.61188463053885,
12.5770542771492));
#440766=CARTESIAN_POINT('Ctrl Pts',(0.553290581744335,-2.61842658596736,
12.5737548217797));
#440767=CARTESIAN_POINT('Ctrl Pts',(0.588648221934046,-2.64171835117381,
12.5663937883685));
#440768=CARTESIAN_POINT('Ctrl Pts',(0.58225175529996,-2.63234435566225,
12.5540940315304));
#440769=CARTESIAN_POINT('Ctrl Pts',(0.567206339909307,-2.63890952672148,
12.5508374392248));
#440770=CARTESIAN_POINT('Ctrl Pts',(0.602603233552784,-2.66216936323413,
12.5434499600945));
#440771=CARTESIAN_POINT('Ctrl Pts',(0.596185969727734,-2.65276488952507,
12.5311293540533));
#440772=CARTESIAN_POINT('Ctrl Pts',(0.581109478025895,-2.65937179216727,
12.5278936106989));
#440773=CARTESIAN_POINT('Ctrl Pts',(0.616545254568319,-2.68260133761895,
12.5204817579905));
#440774=CARTESIAN_POINT('Ctrl Pts',(0.610096229673003,-2.67315031819204,
12.5081597038247));
#440775=CARTESIAN_POINT('Ctrl Pts',(0.595000988433243,-2.67981498148497,
12.5049254088044));
#440776=CARTESIAN_POINT('Ctrl Pts',(0.606521582415215,-2.6679116873562,
12.5369868989719));
#440777=CARTESIAN_POINT('Ctrl Pts',(0.607046619305898,-2.66868112704464,
12.5342545179733));
#440778=CARTESIAN_POINT('Ctrl Pts',(0.60744464806695,-2.66948575753048,
12.5314872231885));
#440779=CARTESIAN_POINT('Ctrl Pts',(0.60764314151109,-2.67030503859505,
12.5287124745063));
#440780=CARTESIAN_POINT('Ctrl Pts',(0.607822152751352,-2.67104390692456,
12.5262100684184));
#440781=CARTESIAN_POINT('Ctrl Pts',(0.607837738783102,-2.67179417715144,
12.5237004536639));
#440782=CARTESIAN_POINT('Ctrl Pts',(0.60762389091828,-2.67257010863176,
12.5212220730815));
#440783=CARTESIAN_POINT('Ctrl Pts',(0.607460171878443,-2.67316415130336,
12.5193246583486));
#440784=CARTESIAN_POINT('Ctrl Pts',(0.60715940797271,-2.67378016566691,
12.517417831369));
#440785=CARTESIAN_POINT('Ctrl Pts',(0.606627525781574,-2.67439357094749,
12.5155812248348));
#440786=CARTESIAN_POINT('Ctrl Pts',(0.606400941109268,-2.67465488489409,
12.5147988205793));
#440787=CARTESIAN_POINT('Ctrl Pts',(0.606132392240512,-2.67491617209588,
12.5140295443047));
#440788=CARTESIAN_POINT('Ctrl Pts',(0.605815148134369,-2.67517758925284,
12.5132817086137));
#440789=CARTESIAN_POINT('Ctrl Pts',(0.605335042095536,-2.67557320875619,
12.5121499604604));
#440790=CARTESIAN_POINT('Ctrl Pts',(0.604728495136676,-2.67597214973372,
12.5110494206568));
#440791=CARTESIAN_POINT('Ctrl Pts',(0.603966119282129,-2.67635153762243,
12.5100666561695));
#440792=CARTESIAN_POINT('Ctrl Pts',(0.603528364822044,-2.67656938127448,
12.5095023550641));
#440793=CARTESIAN_POINT('Ctrl Pts',(0.603033884445084,-2.67678271081349,
12.5089719619137));
#440794=CARTESIAN_POINT('Ctrl Pts',(0.602489416571183,-2.67698166312245,
12.5085043804652));
#440795=CARTESIAN_POINT('Ctrl Pts',(0.601692658759658,-2.67727280391125,
12.5078201359221));
#440796=CARTESIAN_POINT('Ctrl Pts',(0.600765332000758,-2.67754046618894,
12.5072563000949));
#440797=CARTESIAN_POINT('Ctrl Pts',(0.599767947598214,-2.67775837245307,
12.5068768744332));
#440798=CARTESIAN_POINT('Ctrl Pts',(0.599048764783803,-2.67791549787022,
12.5066032824114));
#440799=CARTESIAN_POINT('Ctrl Pts',(0.598280534038465,-2.67804957226223,
12.5064197834844));
#440800=CARTESIAN_POINT('Ctrl Pts',(0.597506599762478,-2.67815565493628,
12.5063282718343));
#440801=CARTESIAN_POINT('Ctrl Pts',(0.596376895323534,-2.67831050279803,
12.5061946931565));
#440802=CARTESIAN_POINT('Ctrl Pts',(0.595211036549254,-2.67841007085721,
12.5062515701262));
#440803=CARTESIAN_POINT('Ctrl Pts',(0.594082694617785,-2.67846358818529,
12.5064436508398));
#440804=CARTESIAN_POINT('',(0.553290581744335,-2.61842658596736,12.5737548217797));
#440805=CARTESIAN_POINT('Origin',(0.556506722612535,-2.63364685002275,12.5893111709658));
#440806=CARTESIAN_POINT('Ctrl Pts',(0.594082694617785,-2.67846358818529,
12.5064436508398));
#440807=CARTESIAN_POINT('Ctrl Pts',(0.588044004717534,-2.66957682206708,
12.5164271754438));
#440808=CARTESIAN_POINT('Ctrl Pts',(0.582003093895394,-2.66068641580753,
12.5264061185523));
#440809=CARTESIAN_POINT('Ctrl Pts',(0.575959883149501,-2.65179224173588,
12.536380305637));
#440810=CARTESIAN_POINT('Ctrl Pts',(0.568407095412342,-2.64067632807919,
12.5488460165097));
#440811=CARTESIAN_POINT('Ctrl Pts',(0.560850712999367,-2.62955452582905,
12.5613043021964));
#440812=CARTESIAN_POINT('Ctrl Pts',(0.553290581744335,-2.61842658596736,
12.5737548217797));
#440813=CARTESIAN_POINT('Ctrl Pts',(0.512533505583331,-2.63410319978829,
12.5893111709658));
#440814=CARTESIAN_POINT('Ctrl Pts',(0.514682834419019,-2.6229749016203,
12.5770542771492));
#440815=CARTESIAN_POINT('Ctrl Pts',(0.53104745588893,-2.62302818390149,
12.5737548217797));
#440816=CARTESIAN_POINT('Ctrl Pts',(0.514538810693153,-2.62372059438638,
12.5928319619712));
#440817=CARTESIAN_POINT('Ctrl Pts',(0.5191819214574,-2.61685947648896,12.5821634970842));
#440818=CARTESIAN_POINT('Ctrl Pts',(0.531768672420854,-2.61924426211537,
12.5773203894503));
#440819=CARTESIAN_POINT('Ctrl Pts',(0.524285711840975,-2.61009774529545,
12.5969440695591));
#440820=CARTESIAN_POINT('Ctrl Pts',(0.528218384721718,-2.60926550340454,
12.5878292599214));
#440821=CARTESIAN_POINT('Ctrl Pts',(0.535244330820872,-2.61438999123459,
12.5813877129824));
#440822=CARTESIAN_POINT('Ctrl Pts',(0.554237267822093,-2.60384638225596,
12.596957478804));
#440823=CARTESIAN_POINT('Ctrl Pts',(0.550333675044355,-2.60467255207779,
12.5878468778671));
#440824=CARTESIAN_POINT('Ctrl Pts',(0.545965626647944,-2.61215838103284,
12.5814011370086));
#440825=CARTESIAN_POINT('Ctrl Pts',(0.568710216777123,-2.61249928672123,
12.5928371701607));
#440826=CARTESIAN_POINT('Ctrl Pts',(0.561727668613172,-2.60805191819121,
12.5821692192952));
#440827=CARTESIAN_POINT('Ctrl Pts',(0.551120496911469,-2.61522908549165,
12.5773318885715));
#440828=CARTESIAN_POINT('Ctrl Pts',(0.574679115658365,-2.62124668345168,
12.5893111709658));
#440829=CARTESIAN_POINT('Ctrl Pts',(0.568290798210363,-2.61188463053882,
12.5770542771492));
#440830=CARTESIAN_POINT('Ctrl Pts',(0.55329058174438,-2.61842658596732,
12.5737548217797));
#440831=CARTESIAN_POINT('',(0.53104745588893,-2.62302818390149,12.5737548217797));
#440832=CARTESIAN_POINT('Origin',(0.534134302985538,-2.63827519590392,12.5893111709658));
#440833=CARTESIAN_POINT('Ctrl Pts',(0.55329058174438,-2.61842658596732,
12.5737548217797));
#440834=CARTESIAN_POINT('Ctrl Pts',(0.552753021476352,-2.61758080314103,
12.5746934679442));
#440835=CARTESIAN_POINT('Ctrl Pts',(0.552003574668472,-2.61674314872517,
12.5756680099006));
#440836=CARTESIAN_POINT('Ctrl Pts',(0.551129988790303,-2.61600670362779,
12.5765688348656));
#440837=CARTESIAN_POINT('Ctrl Pts',(0.550898716599976,-2.61581173794098,
12.5768073183026));
#440838=CARTESIAN_POINT('Ctrl Pts',(0.550658952463078,-2.6156237153656,
12.5770407398754));
#440839=CARTESIAN_POINT('Ctrl Pts',(0.550412683962006,-2.61544392946994,
12.5772674179684));
#440840=CARTESIAN_POINT('Ctrl Pts',(0.549402064627409,-2.61470613677027,
12.5781976435658));
#440841=CARTESIAN_POINT('Ctrl Pts',(0.548217856179683,-2.61407426033052,
12.5790594849312));
#440842=CARTESIAN_POINT('Ctrl Pts',(0.546917285553968,-2.61363356908804,
12.5797571720116));
#440843=CARTESIAN_POINT('Ctrl Pts',(0.546069917026963,-2.61334644289771,
12.580211740231));
#440844=CARTESIAN_POINT('Ctrl Pts',(0.54512861965466,-2.61314520612865,
12.5806009430798));
#440845=CARTESIAN_POINT('Ctrl Pts',(0.544155952783195,-2.61306135017195,
12.5808812374708));
#440846=CARTESIAN_POINT('Ctrl Pts',(0.543320109261729,-2.61298929008622,
12.5811221033394));
#440847=CARTESIAN_POINT('Ctrl Pts',(0.542443979152123,-2.61300254843245,
12.581287365893));
#440848=CARTESIAN_POINT('Ctrl Pts',(0.54157713881285,-2.61310871391489,
12.581359338449));
#440849=CARTESIAN_POINT('Ctrl Pts',(0.541456665905261,-2.61312346872472,
12.5813693411482));
#440850=CARTESIAN_POINT('Ctrl Pts',(0.541336345760709,-2.6131399644506,
12.5813775999465));
#440851=CARTESIAN_POINT('Ctrl Pts',(0.541216283170465,-2.61315816703582,
12.5813841266931));
#440852=CARTESIAN_POINT('Ctrl Pts',(0.541012582464843,-2.61318904992321,
12.5813952001081));
#440853=CARTESIAN_POINT('Ctrl Pts',(0.540808350112785,-2.61322565487485,
12.5814007534795));
#440854=CARTESIAN_POINT('Ctrl Pts',(0.540603709856019,-2.61326816006462,
12.5814005856065));
#440855=CARTESIAN_POINT('Ctrl Pts',(0.5396669467697,-2.61346273220494,12.5813998171494));
#440856=CARTESIAN_POINT('Ctrl Pts',(0.538786290740728,-2.61376716702444,
12.58127954464));
#440857=CARTESIAN_POINT('Ctrl Pts',(0.537957074128939,-2.61415177060978,
12.5810700125799));
#440858=CARTESIAN_POINT('Ctrl Pts',(0.536955474875768,-2.61461632795025,
12.5808169217085));
#440859=CARTESIAN_POINT('Ctrl Pts',(0.536035876464012,-2.61521307506634,
12.5804173076348));
#440860=CARTESIAN_POINT('Ctrl Pts',(0.535264694727185,-2.61586786823707,
12.5799304713245));
#440861=CARTESIAN_POINT('Ctrl Pts',(0.534308957607955,-2.61667936325673,
12.5793271277669));
#440862=CARTESIAN_POINT('Ctrl Pts',(0.533501046458801,-2.61760580396366,
12.5785808224116));
#440863=CARTESIAN_POINT('Ctrl Pts',(0.532851112115142,-2.6185872932463,
12.5777485681082));
#440864=CARTESIAN_POINT('Ctrl Pts',(0.531882638737466,-2.62004981980761,
12.576508418016));
#440865=CARTESIAN_POINT('Ctrl Pts',(0.531267366112818,-2.62161846862367,
12.5750928681475));
#440866=CARTESIAN_POINT('Ctrl Pts',(0.53104745588893,-2.62302818390149,
12.5737548217797));
#440867=CARTESIAN_POINT('Ctrl Pts',(0.53104745588893,-2.62302818390149,
12.5737548217797));
#440868=CARTESIAN_POINT('Ctrl Pts',(0.514682834419019,-2.62297490162029,
12.5770542771492));
#440869=CARTESIAN_POINT('Ctrl Pts',(0.512533505583331,-2.63410319978829,
12.5893111709658));
#440870=CARTESIAN_POINT('Ctrl Pts',(0.526401735067308,-2.64734756366781,
12.5508408821982));
#440871=CARTESIAN_POINT('Ctrl Pts',(0.509986421664261,-2.64729090231181,
12.55409748406));
#440872=CARTESIAN_POINT('Ctrl Pts',(0.50783435083545,-2.65843339733818,
12.5663972313419));
#440873=CARTESIAN_POINT('Ctrl Pts',(0.521759393966551,-2.67164296514411,
12.52790050457));
#440874=CARTESIAN_POINT('Ctrl Pts',(0.505299003657782,-2.67156033207436,
12.5311362602938));
#440875=CARTESIAN_POINT('Ctrl Pts',(0.503139936762534,-2.68273904971673,
12.5434568539655));
#440876=CARTESIAN_POINT('Ctrl Pts',(0.517120156336858,-2.69591624915291,
12.5049357605811));
#440877=CARTESIAN_POINT('Ctrl Pts',(0.500619642742995,-2.69578804568921,
12.5081700652078));
#440878=CARTESIAN_POINT('Ctrl Pts',(0.49844989207396,-2.70702207930673,
12.5204921097672));
#440879=CARTESIAN_POINT('Ctrl Pts',(0.517424785305965,-2.69432236987859,
12.5064436508395));
#440880=CARTESIAN_POINT('Ctrl Pts',(0.516283079484765,-2.69475289932988,
12.5062361689309));
#440881=CARTESIAN_POINT('Ctrl Pts',(0.515077440127446,-2.69515192985568,
12.5061871075061));
#440882=CARTESIAN_POINT('Ctrl Pts',(0.513890598303338,-2.69547196598749,
12.5063648335164));
#440883=CARTESIAN_POINT('Ctrl Pts',(0.513351461539388,-2.6956173461392,
12.5064455676329));
#440884=CARTESIAN_POINT('Ctrl Pts',(0.512808626519243,-2.6957482405416,
12.506574497099));
#440885=CARTESIAN_POINT('Ctrl Pts',(0.512285122024746,-2.69585801516844,
12.5067492519495));
#440886=CARTESIAN_POINT('Ctrl Pts',(0.511233119422025,-2.69607861154224,
12.5071004286051));
#440887=CARTESIAN_POINT('Ctrl Pts',(0.5102203339967,-2.696221240622,12.5076537929613));
#440888=CARTESIAN_POINT('Ctrl Pts',(0.509324099610258,-2.69628456337405,
12.5083435010505));
#440889=CARTESIAN_POINT('Ctrl Pts',(0.509267676299709,-2.69628854991971,
12.5083869222964));
#440890=CARTESIAN_POINT('Ctrl Pts',(0.509211707939692,-2.69629221066786,
12.5084308732337));
#440891=CARTESIAN_POINT('Ctrl Pts',(0.509156210641147,-2.69629554081953,
12.5084753333615));
#440892=CARTESIAN_POINT('Ctrl Pts',(0.508711049056997,-2.69632225303127,
12.5088319622689));
#440893=CARTESIAN_POINT('Ctrl Pts',(0.508287236068956,-2.69632952421375,
12.509227847131));
#440894=CARTESIAN_POINT('Ctrl Pts',(0.507897421878471,-2.69631993779793,
12.5096423454524));
#440895=CARTESIAN_POINT('Ctrl Pts',(0.506675916730021,-2.6962898982135,
12.5109411997424));
#440896=CARTESIAN_POINT('Ctrl Pts',(0.505712883878049,-2.69610214887079,
12.5124831113042));
#440897=CARTESIAN_POINT('Ctrl Pts',(0.50495441954974,-2.69583447306283,
12.5140723025008));
#440898=CARTESIAN_POINT('Ctrl Pts',(0.504883350611455,-2.69580939154645,
12.5142212114565));
#440899=CARTESIAN_POINT('Ctrl Pts',(0.504814053420152,-2.69578362513724,
12.5143705582413));
#440900=CARTESIAN_POINT('Ctrl Pts',(0.504746470605339,-2.69575724872422,
12.5145201959299));
#440901=CARTESIAN_POINT('Ctrl Pts',(0.503878268728772,-2.69541840442872,
12.5164425148273));
#440902=CARTESIAN_POINT('Ctrl Pts',(0.503259342401318,-2.69497728315226,
12.5184635205941));
#440903=CARTESIAN_POINT('Ctrl Pts',(0.502807242578748,-2.69447049273086,
12.5205025929158));
#440904=CARTESIAN_POINT('Ctrl Pts',(0.502545006762095,-2.69417653419916,
12.5216853356836));
#440905=CARTESIAN_POINT('Ctrl Pts',(0.502339011915975,-2.69386133445627,
12.5228750347131));
#440906=CARTESIAN_POINT('Ctrl Pts',(0.502175881409603,-2.69353730315154,
12.5240609649613));
#440907=CARTESIAN_POINT('Ctrl Pts',(0.501775486333361,-2.69274198569777,
12.5269717671326));
#440908=CARTESIAN_POINT('Ctrl Pts',(0.501631335873172,-2.69186640609945,
12.5299036066169));
#440909=CARTESIAN_POINT('Ctrl Pts',(0.501661299468604,-2.6909382066009,
12.5328133004019));
#440910=CARTESIAN_POINT('Ctrl Pts',(0.50167568373914,-2.69049261679416,
12.5342101228451));
#440911=CARTESIAN_POINT('Ctrl Pts',(0.50173069947955,-2.69003547329922,
12.5356023438238));
#440912=CARTESIAN_POINT('Ctrl Pts',(0.501820210172278,-2.68957202508688,
12.5369868989719));
#440913=CARTESIAN_POINT('Origin',(-1.92036686075476,-15.2026802942216,-1.24010651594408));
#440914=CARTESIAN_POINT('Ctrl Pts',(0.606498058131685,-2.6678771421826,
12.5369868989719));
#440915=CARTESIAN_POINT('Ctrl Pts',(0.615119676982169,-2.68056378839359,
12.5369868989719));
#440916=CARTESIAN_POINT('Ctrl Pts',(0.63000495457471,-2.67686084163745,
12.5369868989719));
#440917=CARTESIAN_POINT('Ctrl Pts',(0.609412557255683,-2.6721656875577,
12.5218025310016));
#440918=CARTESIAN_POINT('Ctrl Pts',(0.618531066300393,-2.67968291154709,
12.5216901060418));
#440919=CARTESIAN_POINT('Ctrl Pts',(0.629959583296767,-2.67687214545033,
12.5161920673678));
#440920=CARTESIAN_POINT('Ctrl Pts',(0.607339468066221,-2.6778259324648,
12.5042015548894));
#440921=CARTESIAN_POINT('Ctrl Pts',(0.612976673589232,-2.6809241995463,
12.4980677368514));
#440922=CARTESIAN_POINT('Ctrl Pts',(0.619600715733787,-2.67940339535413,
12.4907278922777));
#440923=CARTESIAN_POINT('Ctrl Pts',(0.594078363624189,-2.6784440616444,
12.506463626192));
#440924=CARTESIAN_POINT('Ctrl Pts',(0.595495111718461,-2.68483157001417,
12.4999376786891));
#440925=CARTESIAN_POINT('Ctrl Pts',(0.59547780820044,-2.68475355588686,
12.4906970594712));
#440926=CARTESIAN_POINT('Origin',(0.624693975461002,-2.65551152078516,12.5369868989719));
#440927=CARTESIAN_POINT('Origin',(0.624693975461003,-2.65551152078516,14.));
#440928=CARTESIAN_POINT('Origin',(0.624693975461002,-2.65551152078516,13.7435492065112));
#440929=CARTESIAN_POINT('Ctrl Pts',(0.592565722405718,-2.64745938381134,
13.793642941384));
#440930=CARTESIAN_POINT('Ctrl Pts',(0.598637514750161,-2.65640586673658,
13.8071662555867));
#440931=CARTESIAN_POINT('Ctrl Pts',(0.613981610874529,-2.64901816765223,
13.8103758687955));
#440932=CARTESIAN_POINT('Ctrl Pts',(0.601934114705725,-2.66118872942342,
13.7804579775006));
#440933=CARTESIAN_POINT('Ctrl Pts',(0.609434548503473,-2.67222218602483,
13.7901904343351));
#440934=CARTESIAN_POINT('Ctrl Pts',(0.624549765349318,-2.66777402417215,
13.7927914348263));
#440935=CARTESIAN_POINT('Ctrl Pts',(0.60744963985642,-2.66927171185723,
13.7597120340895));
#440936=CARTESIAN_POINT('Ctrl Pts',(0.616134493101865,-2.68203730679351,
13.7635825532445));
#440937=CARTESIAN_POINT('Ctrl Pts',(0.630804064389904,-2.67882178282857,
13.7651073818884));
#440938=CARTESIAN_POINT('Ctrl Pts',(0.606369573741418,-2.66768887881698,
13.7381884353898));
#440939=CARTESIAN_POINT('Ctrl Pts',(0.614850398662509,-2.6801561768115,
13.7368803041982));
#440940=CARTESIAN_POINT('Ctrl Pts',(0.629579716885802,-2.67665805991866,
13.7363986145813));
#440941=CARTESIAN_POINT('Origin',(0.613011317284714,-2.63839063333717,13.7902182540695));
#440942=CARTESIAN_POINT('Ctrl Pts',(0.574676897670838,-2.62124343165373,
13.8235227101244));
#440943=CARTESIAN_POINT('Ctrl Pts',(0.581153490587285,-2.6307427175487,
13.8358800583119));
#440944=CARTESIAN_POINT('Ctrl Pts',(0.596298747147244,-2.62401610972677,
13.8390832900376));
#440945=CARTESIAN_POINT('Ctrl Pts',(0.581399805435583,-2.63109582529598,
13.8124254819053));
#440946=CARTESIAN_POINT('Ctrl Pts',(0.587888976033493,-2.6406135585128,
13.8247886449158));
#440947=CARTESIAN_POINT('Ctrl Pts',(0.603046450886266,-2.63386287431115,
13.8279860620657));
#440948=CARTESIAN_POINT('Ctrl Pts',(0.588119700211747,-2.64094380341589,
13.8013225099955));
#440949=CARTESIAN_POINT('Ctrl Pts',(0.594618384988356,-2.65047549424216,
13.8136962257787));
#440950=CARTESIAN_POINT('Ctrl Pts',(0.609790807176251,-2.64370523355036,
13.8168830918626));
#440951=CARTESIAN_POINT('Ctrl Pts',(0.594836699230128,-2.65078753781472,
13.7902140179785));
#440952=CARTESIAN_POINT('Ctrl Pts',(0.601342034907494,-2.66032898997199,
13.802602731458));
#440953=CARTESIAN_POINT('Ctrl Pts',(0.616531946028556,-2.65354336158135,
13.8057746032558));
#440954=CARTESIAN_POINT('Origin',(0.592851508704108,-2.60884651688068,13.8235269408515));
#440955=CARTESIAN_POINT('Ctrl Pts',(0.512533505583331,-2.63410319978829,
13.8235269408515));
#440956=CARTESIAN_POINT('Ctrl Pts',(0.510294379817396,-2.645696427751,13.8362179249168));
#440957=CARTESIAN_POINT('Ctrl Pts',(0.493223091185079,-2.64521258016219,
13.8391868794938));
#440958=CARTESIAN_POINT('Ctrl Pts',(0.51458220819582,-2.62349590082558,
13.8400110824519));
#440959=CARTESIAN_POINT('Ctrl Pts',(0.509428054285371,-2.63214208844374,
13.8494522556836));
#440960=CARTESIAN_POINT('Ctrl Pts',(0.496704995458622,-2.6277772675394,
13.85569149686));
#440961=CARTESIAN_POINT('Ctrl Pts',(0.523948816583283,-2.61016682083629,
13.8586819406588));
#440962=CARTESIAN_POINT('Ctrl Pts',(0.519688082897046,-2.61106247260452,
13.868010383617));
#440963=CARTESIAN_POINT('Ctrl Pts',(0.512373206287159,-2.60573467315496,
13.8744918421245));
#440964=CARTESIAN_POINT('Ctrl Pts',(0.554579384364869,-2.60377621716178,
13.8587686893867));
#440965=CARTESIAN_POINT('Ctrl Pts',(0.55880218597755,-2.6028884815819,13.8680909899357));
#440966=CARTESIAN_POINT('Ctrl Pts',(0.563364632001517,-2.5950987134349,
13.8745789365163));
#440967=CARTESIAN_POINT('Ctrl Pts',(0.568579974698556,-2.61230841747989,
13.8400379222776));
#440968=CARTESIAN_POINT('Ctrl Pts',(0.576743743323402,-2.61819255851727,
13.8494748685453));
#440969=CARTESIAN_POINT('Ctrl Pts',(0.586686777358123,-2.60914285247514,
13.8557104837033));
#440970=CARTESIAN_POINT('Ctrl Pts',(0.574679115663699,-2.62124668344787,
13.8235269408542));
#440971=CARTESIAN_POINT('Ctrl Pts',(0.581334330985496,-2.6309998740956,
13.8362179249195));
#440972=CARTESIAN_POINT('Ctrl Pts',(0.596812372092759,-2.62378230888716,
13.8391868794965));
#440973=CARTESIAN_POINT('Origin',(0.490932708181124,-2.62993120367266,13.8235269408515));
#440974=CARTESIAN_POINT('Ctrl Pts',(0.50575154986725,-2.66921723887999,
13.7902140241682));
#440975=CARTESIAN_POINT('Ctrl Pts',(0.503565983381956,-2.6805566345663,
13.8026027327198));
#440976=CARTESIAN_POINT('Ctrl Pts',(0.48693056170767,-2.68035494670805,
13.8057746032556));
#440977=CARTESIAN_POINT('Ctrl Pts',(0.508011462560479,-2.65751638517433,
13.8013225161808));
#440978=CARTESIAN_POINT('Ctrl Pts',(0.505828128021538,-2.66884418187874,
13.8136962270464));
#440979=CARTESIAN_POINT('Ctrl Pts',(0.489214857211879,-2.66864966113952,
13.8168830918628));
#440980=CARTESIAN_POINT('Ctrl Pts',(0.510272349522419,-2.64581048712535,
13.8124254880875));
#440981=CARTESIAN_POINT('Ctrl Pts',(0.50809221020777,-2.65712169694612,
13.8247886461867));
#440982=CARTESIAN_POINT('Ctrl Pts',(0.491500427224399,-2.6569392150819,
13.8279860620656));
#440983=CARTESIAN_POINT('Ctrl Pts',(0.512534250195273,-2.63409934051833,
13.8235227163065));
#440984=CARTESIAN_POINT('Ctrl Pts',(0.510358336745589,-2.64538862676221,
13.8358800595847));
#440985=CARTESIAN_POINT('Ctrl Pts',(0.493787321992151,-2.64522339710558,
13.8390832900376));
#440986=CARTESIAN_POINT('Origin',(0.484150005496586,-2.66504911425251,13.7902182540695));
#440987=CARTESIAN_POINT('Ctrl Pts',(0.501871358291202,-2.68930705671633,
13.7382347919292));
#440988=CARTESIAN_POINT('Ctrl Pts',(0.499033255290564,-2.70412809042155,
13.7369371795943));
#440989=CARTESIAN_POINT('Ctrl Pts',(0.484112057328093,-2.70675518546834,
13.7364597369712));
#440990=CARTESIAN_POINT('Ctrl Pts',(0.501512650723195,-2.69116429199084,
13.7595490285573));
#440991=CARTESIAN_POINT('Ctrl Pts',(0.498605845535065,-2.70633875376109,
13.7633824266926));
#440992=CARTESIAN_POINT('Ctrl Pts',(0.483850339632552,-2.70919684855801,
13.7648920890506));
#440993=CARTESIAN_POINT('Ctrl Pts',(0.503342039676267,-2.68169249383999,
13.7803806590111));
#440994=CARTESIAN_POINT('Ctrl Pts',(0.500833059283693,-2.69481887580129,
13.7901039518744));
#440995=CARTESIAN_POINT('Ctrl Pts',(0.485188296642965,-2.69674937919179,
13.7926933640892));
#440996=CARTESIAN_POINT('Ctrl Pts',(0.506521925972004,-2.66522839426788,
13.7936647693663));
#440997=CARTESIAN_POINT('Ctrl Pts',(0.504500368443352,-2.67585320660048,
13.8072068914933));
#440998=CARTESIAN_POINT('Ctrl Pts',(0.487466636836108,-2.6751487512227,
13.8104111085397));
#440999=CARTESIAN_POINT('Origin',(0.480219412770071,-2.68540002897125,13.7435492065112));
#441000=CARTESIAN_POINT('Origin',(0.480219412770071,-2.68540002897125,14.));
#441001=CARTESIAN_POINT('Origin',(0.480219412770071,-2.68540002897125,12.5369868989719));
#441002=CARTESIAN_POINT('Ctrl Pts',(0.517421318304256,-2.69430431653286,
12.506462012331));
#441003=CARTESIAN_POINT('Ctrl Pts',(0.518654478867682,-2.70072560168575,
12.4999388158272));
#441004=CARTESIAN_POINT('Ctrl Pts',(0.518639888961025,-2.7006496294614,
12.4907030323752));
#441005=CARTESIAN_POINT('Ctrl Pts',(0.505003128977343,-2.69899656087809,
12.5042014951932));
#441006=CARTESIAN_POINT('Ctrl Pts',(0.501060437504569,-2.70407556482246,
12.4980716682127));
#441007=CARTESIAN_POINT('Ctrl Pts',(0.494381709264913,-2.70530851020918,
12.4907355092743));
#441008=CARTESIAN_POINT('Ctrl Pts',(0.50085325994376,-2.69462571562236,
12.5218047446509));
#441009=CARTESIAN_POINT('Ctrl Pts',(0.495467506015631,-2.70513820940652,
12.5216906929434));
#441010=CARTESIAN_POINT('Ctrl Pts',(0.483868357058764,-2.70709537516508,
12.5161988840776));
#441011=CARTESIAN_POINT('Ctrl Pts',(0.5018274623251,-2.68953429969622,12.5369868989719));
#441012=CARTESIAN_POINT('Ctrl Pts',(0.498946647961556,-2.70459107359116,
12.5369868989719));
#441013=CARTESIAN_POINT('Ctrl Pts',(0.483823914260394,-2.70710273776546,
12.5369868989719));
#441014=CARTESIAN_POINT('Origin',(1.04370312006728E-31,-1.01968969974689E-30,
12.5));
#441015=CARTESIAN_POINT('Origin',(0.725531957228311,-2.58356219985525,12.5));
#441016=CARTESIAN_POINT('',(0.725531957228311,-2.58356219985525,12.5893111709658));
#441017=CARTESIAN_POINT('',(0.725531957228311,-2.58356219985525,13.8235269408515));
#441018=CARTESIAN_POINT('',(0.725531957228311,-2.58356219985525,12.5));
#441019=CARTESIAN_POINT('',(0.721634259158455,-2.619116111721,13.7902182540695));
#441020=CARTESIAN_POINT('',(0.725531957228311,-2.58356219985525,13.8235269408515));
#441021=CARTESIAN_POINT('',(0.719375533633238,-2.6397196902469,13.7435492065112));
#441022=CARTESIAN_POINT('Origin',(0.726807034570083,-2.57193422473676,13.7445212918707));
#441023=CARTESIAN_POINT('',(0.719375533633238,-2.6397196902469,12.5369868989719));
#441024=CARTESIAN_POINT('',(0.719375533633238,-2.6397196902469,12.5));
#441025=CARTESIAN_POINT('Ctrl Pts',(0.719375533633238,-2.6397196902469,
12.5369868989719));
#441026=CARTESIAN_POINT('Ctrl Pts',(0.72142617812462,-2.62101417940232,
12.5544431401645));
#441027=CARTESIAN_POINT('Ctrl Pts',(0.723478289291444,-2.60229528987922,
12.5718848856037));
#441028=CARTESIAN_POINT('Ctrl Pts',(0.725531957228311,-2.58356219985525,
12.5893111709658));
#441029=CARTESIAN_POINT('Origin',(0.959424417192052,-2.77944798353807,12.5));
#441030=CARTESIAN_POINT('',(0.821963002087478,-2.60959729166525,13.7435492065112));
#441031=CARTESIAN_POINT('',(0.808923705722944,-2.59348561765574,13.7902182540695));
#441032=CARTESIAN_POINT('Origin',(0.774658688519583,-2.55114692301479,13.741873268044));
#441033=CARTESIAN_POINT('',(0.786422857476923,-2.56568301836339,13.8235269408515));
#441034=CARTESIAN_POINT('',(0.808923705722944,-2.59348561765574,13.7902182540695));
#441035=CARTESIAN_POINT('',(0.786422857476923,-2.56568301836339,12.5893111709658));
#441036=CARTESIAN_POINT('',(0.786422857476923,-2.56568301836339,12.5));
#441037=CARTESIAN_POINT('',(0.821963002087478,-2.60959729166525,12.5369868989719));
#441038=CARTESIAN_POINT('Ctrl Pts',(0.786422857476923,-2.56568301836339,
12.5893111709658));
#441039=CARTESIAN_POINT('Ctrl Pts',(0.798278385988105,-2.58033199981473,
12.5718848856037));
#441040=CARTESIAN_POINT('Ctrl Pts',(0.810124927490586,-2.59496987669797,
12.5544431401645));
#441041=CARTESIAN_POINT('Ctrl Pts',(0.821963002087478,-2.60959729166525,
12.5369868989719));
#441042=CARTESIAN_POINT('',(0.821963002087478,-2.60959729166525,12.5));
#441043=CARTESIAN_POINT('Origin',(0.759702236830088,-2.58730821332778,12.5));
#441044=CARTESIAN_POINT('',(0.7489488282979,-2.55465925657388,13.8587068136939));
#441045=CARTESIAN_POINT('Ctrl Pts',(0.786422857481969,-2.56568301835912,
13.8235269408542));
#441046=CARTESIAN_POINT('Ctrl Pts',(0.78532049259588,-2.56432090930143,
13.8262006681044));
#441047=CARTESIAN_POINT('Ctrl Pts',(0.784057330900536,-2.56303628851558,
13.8288634856214));
#441048=CARTESIAN_POINT('Ctrl Pts',(0.782645946513711,-2.56182471780257,
13.8314912288862));
#441049=CARTESIAN_POINT('Ctrl Pts',(0.781190954788442,-2.56057571336518,
13.834200161153));
#441050=CARTESIAN_POINT('Ctrl Pts',(0.779577147155867,-2.55940257841192,
13.8368750301949));
#441051=CARTESIAN_POINT('Ctrl Pts',(0.777776862845244,-2.55831850944794,
13.8394886372968));
#441052=CARTESIAN_POINT('Ctrl Pts',(0.777637822521051,-2.55823478417226,
13.8396904925131));
#441053=CARTESIAN_POINT('Ctrl Pts',(0.777497655368256,-2.5581516068833,
13.8398919674349));
#441054=CARTESIAN_POINT('Ctrl Pts',(0.777356341927515,-2.55806899292609,
13.8400930404591));
#441055=CARTESIAN_POINT('Ctrl Pts',(0.775154583449799,-2.55678181189288,
13.8432258934518));
#441056=CARTESIAN_POINT('Ctrl Pts',(0.772686357935972,-2.55563698016031,
13.8462331177034));
#441057=CARTESIAN_POINT('Ctrl Pts',(0.769991575538835,-2.55475934707315,
13.8489036603661));
#441058=CARTESIAN_POINT('Ctrl Pts',(0.769109811377731,-2.5544721753135,
13.8497774930041));
#441059=CARTESIAN_POINT('Ctrl Pts',(0.768203946779649,-2.55421380676574,
13.85061494757));
#441060=CARTESIAN_POINT('Ctrl Pts',(0.767275836005458,-2.55398916456931,
13.8514076489583));
#441061=CARTESIAN_POINT('Ctrl Pts',(0.765312747864439,-2.5535140139256,
13.8530843267192));
#441062=CARTESIAN_POINT('Ctrl Pts',(0.763056611219965,-2.55314595204423,
13.8546805203176));
#441063=CARTESIAN_POINT('Ctrl Pts',(0.76061640235854,-2.55304100658142,
13.8559412814273));
#441064=CARTESIAN_POINT('Ctrl Pts',(0.760289823275029,-2.55302696147503,
13.8561100121513));
#441065=CARTESIAN_POINT('Ctrl Pts',(0.759959999496362,-2.5530175727559,
13.8562727473908));
#441066=CARTESIAN_POINT('Ctrl Pts',(0.759627236466857,-2.55301315281039,
13.8564289040185));
#441067=CARTESIAN_POINT('Ctrl Pts',(0.758118159924363,-2.55299310840789,
13.8571370725437));
#441068=CARTESIAN_POINT('Ctrl Pts',(0.756522078808802,-2.55307717631056,
13.8577210840554));
#441069=CARTESIAN_POINT('Ctrl Pts',(0.7549025767413,-2.5532913962012,13.8581177131616));
#441070=CARTESIAN_POINT('Ctrl Pts',(0.754446469217524,-2.55335172789563,
13.8582294175695));
#441071=CARTESIAN_POINT('Ctrl Pts',(0.753988515650023,-2.5534222057495,
13.8583265086086));
#441072=CARTESIAN_POINT('Ctrl Pts',(0.7535301390344,-2.55350297187816,13.8584082369006));
#441073=CARTESIAN_POINT('Ctrl Pts',(0.752871574756299,-2.55361901114674,
13.8585256585398));
#441074=CARTESIAN_POINT('Ctrl Pts',(0.752204005827178,-2.5537580485362,
13.8586122832068));
#441075=CARTESIAN_POINT('Ctrl Pts',(0.751544934769251,-2.55391724535535,
13.8586682984299));
#441076=CARTESIAN_POINT('Ctrl Pts',(0.751017743254522,-2.55404458702999,
13.8587131050557));
#441077=CARTESIAN_POINT('Ctrl Pts',(0.750490111140253,-2.55418600610493,
13.8587357943552));
#441078=CARTESIAN_POINT('Ctrl Pts',(0.749962106842168,-2.55434200856446,
13.8587355499465));
#441079=CARTESIAN_POINT('Ctrl Pts',(0.749620845076198,-2.55444283667331,
13.8587353919793));
#441080=CARTESIAN_POINT('Ctrl Pts',(0.749283107237414,-2.55454862933603,
13.8587257282814));
#441081=CARTESIAN_POINT('Ctrl Pts',(0.7489488282979,-2.55465925657388,13.8587068136939));
#441082=CARTESIAN_POINT('Ctrl Pts',(0.7489488282979,-2.55465925657388,13.8587068136939));
#441083=CARTESIAN_POINT('Ctrl Pts',(0.747849403088895,-2.55502310352839,
13.8586446046466));
#441084=CARTESIAN_POINT('Ctrl Pts',(0.74678734649688,-2.55543918263377,
13.858482427929));
#441085=CARTESIAN_POINT('Ctrl Pts',(0.745760746494891,-2.55590345283694,
13.8582284286032));
#441086=CARTESIAN_POINT('Ctrl Pts',(0.744707574311953,-2.55637974005923,
13.8579678548414));
#441087=CARTESIAN_POINT('Ctrl Pts',(0.743689776488433,-2.5569093044033,
13.857615680862));
#441088=CARTESIAN_POINT('Ctrl Pts',(0.742743006534908,-2.55746267242064,
13.8571944833187));
#441089=CARTESIAN_POINT('Ctrl Pts',(0.740380245288189,-2.55884365890176,
13.8561433417727));
#441090=CARTESIAN_POINT('Ctrl Pts',(0.738346905408584,-2.56043335350817,
13.8546163505474));
#441091=CARTESIAN_POINT('Ctrl Pts',(0.73665403417784,-2.56202527179926,
13.8528973491086));
#441092=CARTESIAN_POINT('Ctrl Pts',(0.736344771579975,-2.56231609178447,
13.8525833129072));
#441093=CARTESIAN_POINT('Ctrl Pts',(0.736046738322298,-2.562606939393,13.8522628768812));
#441094=CARTESIAN_POINT('Ctrl Pts',(0.735759825805316,-2.56289652385522,
13.851937733538));
#441095=CARTESIAN_POINT('Ctrl Pts',(0.734007690871391,-2.56466497598797,
13.8499521282529));
#441096=CARTESIAN_POINT('Ctrl Pts',(0.732499057953502,-2.56656494188974,
13.847639871647));
#441097=CARTESIAN_POINT('Ctrl Pts',(0.731250296912941,-2.56844660725329,
13.8452109780794));
#441098=CARTESIAN_POINT('Ctrl Pts',(0.730688453472725,-2.56929320744889,
13.8441181685877));
#441099=CARTESIAN_POINT('Ctrl Pts',(0.730178517129381,-2.57013593751768,
13.8430021611332));
#441100=CARTESIAN_POINT('Ctrl Pts',(0.72971868113555,-2.57096142343704,
13.8418824960098));
#441101=CARTESIAN_POINT('Ctrl Pts',(0.728635065873759,-2.57290670208555,
13.8392439765549));
#441102=CARTESIAN_POINT('Ctrl Pts',(0.727774562886895,-2.57484737227174,
13.8364981347964));
#441103=CARTESIAN_POINT('Ctrl Pts',(0.727103613305592,-2.57677469520582,
13.8336931113419));
#441104=CARTESIAN_POINT('Ctrl Pts',(0.72645015102264,-2.57865178534729,
13.8309611966328));
#441105=CARTESIAN_POINT('Ctrl Pts',(0.725976368281059,-2.58051828149001,
13.8281701127186));
#441106=CARTESIAN_POINT('Ctrl Pts',(0.725690535000416,-2.582364642916,13.8253580685121));
#441107=CARTESIAN_POINT('Ctrl Pts',(0.725628566036692,-2.58276493606581,
13.8247484142933));
#441108=CARTESIAN_POINT('Ctrl Pts',(0.725575588055282,-2.58316420941347,
13.8241378483365));
#441109=CARTESIAN_POINT('Ctrl Pts',(0.725531957228311,-2.58356219985525,
13.8235269408515));
#441110=CARTESIAN_POINT('',(0.75013538634949,-2.5542920279702,12.5969504640361));
#441111=CARTESIAN_POINT('Origin',(0.759711370193215,-2.5873400137128,12.584524458991));
#441112=CARTESIAN_POINT('Origin',(0.759711370193215,-2.5873400137128,12.584524458991));
#441113=CARTESIAN_POINT('Ctrl Pts',(0.786422857476923,-2.56568301836339,
12.5893111709658));
#441114=CARTESIAN_POINT('Ctrl Pts',(0.779292702402773,-2.55687282408754,
12.5770542771492));
#441115=CARTESIAN_POINT('Ctrl Pts',(0.764875628019623,-2.56461566859622,
12.5737548217797));
#441116=CARTESIAN_POINT('Ctrl Pts',(0.802014113672929,-2.5849479564556,
12.5663937883685));
#441117=CARTESIAN_POINT('Ctrl Pts',(0.794874863095769,-2.57612652355341,
12.5540940315304));
#441118=CARTESIAN_POINT('Ctrl Pts',(0.780414632473082,-2.58389619057666,
12.5508374392248));
#441119=CARTESIAN_POINT('Ctrl Pts',(0.817589638482575,-2.60419345646147,
12.5434499600945));
#441120=CARTESIAN_POINT('Ctrl Pts',(0.810427175659408,-2.5953433419395,
12.5311293540533));
#441121=CARTESIAN_POINT('Ctrl Pts',(0.795939373640742,-2.60315713469527,
12.5278936106989));
#441122=CARTESIAN_POINT('Ctrl Pts',(0.833150664166861,-2.62342104099285,
12.5204817579905));
#441123=CARTESIAN_POINT('Ctrl Pts',(0.825952752047599,-2.61452712445222,
12.5081597038247));
#441124=CARTESIAN_POINT('Ctrl Pts',(0.811450970907885,-2.62240001392627,
12.5049254088044));
#441125=CARTESIAN_POINT('Ctrl Pts',(0.821963002087479,-2.60959729166525,
12.5369868989719));
#441126=CARTESIAN_POINT('Ctrl Pts',(0.822549008438961,-2.61032137572581,
12.5342545179733));
#441127=CARTESIAN_POINT('Ctrl Pts',(0.823011297646569,-2.61109088583094,
12.5314872231885));
#441128=CARTESIAN_POINT('Ctrl Pts',(0.823275909632745,-2.61189126174693,
12.5287124745063));
#441129=CARTESIAN_POINT('Ctrl Pts',(0.823514549856045,-2.61261308047509,
12.5262100684184));
#441130=CARTESIAN_POINT('Ctrl Pts',(0.823591238015218,-2.6133595838334,
12.5237004536639));
#441131=CARTESIAN_POINT('Ctrl Pts',(0.823441347330567,-2.61415036405197,
12.5212220730815));
#441132=CARTESIAN_POINT('Ctrl Pts',(0.823326593044888,-2.61475577471723,
12.5193246583486));
#441133=CARTESIAN_POINT('Ctrl Pts',(0.823077040795667,-2.61539425439427,
12.517417831369));
#441134=CARTESIAN_POINT('Ctrl Pts',(0.822596926623588,-2.61604897195571,
12.5155812248348));
#441135=CARTESIAN_POINT('Ctrl Pts',(0.822392395405655,-2.61632788515601,
12.5147988205793));
#441136=CARTESIAN_POINT('Ctrl Pts',(0.822146037443724,-2.61661019217209,
12.5140295443047));
#441137=CARTESIAN_POINT('Ctrl Pts',(0.821851156866344,-2.61689659782483,
12.5132817086137));
#441138=CARTESIAN_POINT('Ctrl Pts',(0.821404895003024,-2.61733003403616,
12.5121499604604));
#441139=CARTESIAN_POINT('Ctrl Pts',(0.820832883672389,-2.61777708677856,
12.5110494206568));
#441140=CARTESIAN_POINT('Ctrl Pts',(0.820103968195602,-2.61821735299507,
12.5100666561695));
#441141=CARTESIAN_POINT('Ctrl Pts',(0.819685426607374,-2.61847015284274,
12.5095023550641));
#441142=CARTESIAN_POINT('Ctrl Pts',(0.819209979910961,-2.61872307728656,
12.5089719619137));
#441143=CARTESIAN_POINT('Ctrl Pts',(0.818683540169158,-2.61896574678444,
12.5085043804652));
#441144=CARTESIAN_POINT('Ctrl Pts',(0.817913164180629,-2.61932086198467,
12.5078201359221));
#441145=CARTESIAN_POINT('Ctrl Pts',(0.817010739985508,-2.61966321937794,
12.5072563000949));
#441146=CARTESIAN_POINT('Ctrl Pts',(0.816034435680754,-2.61996169666502,
12.5068768744332));
#441147=CARTESIAN_POINT('Ctrl Pts',(0.815330453068009,-2.62017691933625,
12.5066032824114));
#441148=CARTESIAN_POINT('Ctrl Pts',(0.814575706854735,-2.62037316554443,
12.5064197834844));
#441149=CARTESIAN_POINT('Ctrl Pts',(0.813812994503966,-2.62054197806549,
12.5063282718343));
#441150=CARTESIAN_POINT('Ctrl Pts',(0.812699670601618,-2.62078839208319,
12.5061946931565));
#441151=CARTESIAN_POINT('Ctrl Pts',(0.811545806847401,-2.62098265715127,
12.5062515701262));
#441152=CARTESIAN_POINT('Ctrl Pts',(0.810425581539696,-2.6211279667473,
12.5064436508398));
#441153=CARTESIAN_POINT('',(0.764875628019623,-2.56461566859622,12.5737548217797));
#441154=CARTESIAN_POINT('Origin',(0.769321660262949,-2.5795231431406,12.5893111709658));
#441155=CARTESIAN_POINT('Ctrl Pts',(0.810425581539697,-2.6211279667473,
12.5064436508398));
#441156=CARTESIAN_POINT('Ctrl Pts',(0.803682630942583,-2.61276297989757,
12.5164271754438));
#441157=CARTESIAN_POINT('Ctrl Pts',(0.796937170108206,-2.60439454604452,
12.5264061185523));
#441158=CARTESIAN_POINT('Ctrl Pts',(0.790189109891219,-2.5960225443816,
12.536380305637));
#441159=CARTESIAN_POINT('Ctrl Pts',(0.781755403274068,-2.58555924032784,
12.5488460165097));
#441160=CARTESIAN_POINT('Ctrl Pts',(0.773317633967052,-2.57509036027389,
12.5613043021964));
#441161=CARTESIAN_POINT('Ctrl Pts',(0.764875628019623,-2.56461566859622,
12.5737548217797));
#441162=CARTESIAN_POINT('Ctrl Pts',(0.725531957228311,-2.58356219985525,
12.5893111709658));
#441163=CARTESIAN_POINT('Ctrl Pts',(0.726767074738834,-2.57229573992789,
12.5770542771492));
#441164=CARTESIAN_POINT('Ctrl Pts',(0.743081587281356,-2.57101497634515,
12.5737548217797));
#441165=CARTESIAN_POINT('Ctrl Pts',(0.726684311123145,-2.57305069073351,
12.5928319619712));
#441166=CARTESIAN_POINT('Ctrl Pts',(0.730752727515209,-2.56583394600807,
12.5821634970842));
#441167=CARTESIAN_POINT('Ctrl Pts',(0.743491979270983,-2.56718485940383,
12.5773203894503));
#441168=CARTESIAN_POINT('Ctrl Pts',(0.735288391592189,-2.55867870761977,
12.5969440695591));
#441169=CARTESIAN_POINT('Ctrl Pts',(0.739140143388078,-2.55752868559616,
12.5878292599214));
#441170=CARTESIAN_POINT('Ctrl Pts',(0.746560404562759,-2.56206344228292,
12.5813877129824));
#441171=CARTESIAN_POINT('Ctrl Pts',(0.764630742119066,-2.55000681560595,
12.596957478804));
#441172=CARTESIAN_POINT('Ctrl Pts',(0.760807478734539,-2.55114841546642,
12.5878468778671));
#441173=CARTESIAN_POINT('Ctrl Pts',(0.757064129213709,-2.55896537243845,
12.5814011370086));
#441174=CARTESIAN_POINT('Ctrl Pts',(0.779760825573947,-2.55745124854529,
12.5928371701607));
#441175=CARTESIAN_POINT('Ctrl Pts',(0.772439009440422,-2.55358782076535,
12.5821692192951));
#441176=CARTESIAN_POINT('Ctrl Pts',(0.7624521379921,-2.56160568959954,12.5773318885715));
#441177=CARTESIAN_POINT('Ctrl Pts',(0.786422857476964,-2.56568301836335,
12.5893111709658));
#441178=CARTESIAN_POINT('Ctrl Pts',(0.779292702402813,-2.5568728240875,
12.5770542771492));
#441179=CARTESIAN_POINT('Ctrl Pts',(0.764875628019665,-2.56461566859618,
12.5737548217797));
#441180=CARTESIAN_POINT('',(0.743081587281356,-2.57101497634515,12.5737548217797));
#441181=CARTESIAN_POINT('Origin',(0.747400936173448,-2.58595964847767,12.5893111709658));
#441182=CARTESIAN_POINT('Ctrl Pts',(0.764875628019665,-2.56461566859618,
12.5737548217797));
#441183=CARTESIAN_POINT('Ctrl Pts',(0.764270917286879,-2.56381651619478,
12.5746934679442));
#441184=CARTESIAN_POINT('Ctrl Pts',(0.763455687590138,-2.56304273587727,
12.5756680099006));
#441185=CARTESIAN_POINT('Ctrl Pts',(0.762524981384661,-2.56237994659924,
12.5765688348656));
#441186=CARTESIAN_POINT('Ctrl Pts',(0.762278587220015,-2.56220448047521,
12.5768073183026));
#441187=CARTESIAN_POINT('Ctrl Pts',(0.762024295293087,-2.56203662653245,
12.5770407398754));
#441188=CARTESIAN_POINT('Ctrl Pts',(0.761764192010584,-2.5618775120286,
12.5772674179684));
#441189=CARTESIAN_POINT('Ctrl Pts',(0.760696798474097,-2.56122454913118,
12.5781976435658));
#441190=CARTESIAN_POINT('Ctrl Pts',(0.759465026586396,-2.56069129919031,
12.5790594849312));
#441191=CARTESIAN_POINT('Ctrl Pts',(0.758132863074708,-2.56035808289148,
12.5797571720116));
#441192=CARTESIAN_POINT('Ctrl Pts',(0.757264910646512,-2.5601409804914,
12.580211740231));
#441193=CARTESIAN_POINT('Ctrl Pts',(0.756310342698694,-2.56001713779551,
12.5806009430798));
#441194=CARTESIAN_POINT('Ctrl Pts',(0.755334077257052,-2.56001284224241,
12.5808812374708));
#441195=CARTESIAN_POINT('Ctrl Pts',(0.754495141369994,-2.56000915093727,
12.5811221033394));
#441196=CARTESIAN_POINT('Ctrl Pts',(0.753623007189356,-2.56009377790496,
12.581287365893));
#441197=CARTESIAN_POINT('Ctrl Pts',(0.752767704662216,-2.56027024566553,
12.581359338449));
#441198=CARTESIAN_POINT('Ctrl Pts',(0.752648835272265,-2.56029477104033,
12.5813693411482));
#441199=CARTESIAN_POINT('Ctrl Pts',(0.752530260037864,-2.56032101908682,
12.5813775999465));
#441200=CARTESIAN_POINT('Ctrl Pts',(0.752412080625663,-2.56034894732016,
12.5813841266931));
#441201=CARTESIAN_POINT('Ctrl Pts',(0.752211574959359,-2.56039633094586,
12.5813952001081));
#441202=CARTESIAN_POINT('Ctrl Pts',(0.752011005816987,-2.56044946093023,
12.5814007534795));
#441203=CARTESIAN_POINT('Ctrl Pts',(0.751810511051359,-2.5605085047682,
12.5814005856065));
#441204=CARTESIAN_POINT('Ctrl Pts',(0.750892724402688,-2.5607787843738,
12.5813998171494));
#441205=CARTESIAN_POINT('Ctrl Pts',(0.750039812948028,-2.56115398785352,
12.58127954464));
#441206=CARTESIAN_POINT('Ctrl Pts',(0.7492447042488,-2.56160490055409,12.5810700125799));
#441207=CARTESIAN_POINT('Ctrl Pts',(0.748284303470506,-2.56214955175587,
12.5808169217085));
#441208=CARTESIAN_POINT('Ctrl Pts',(0.747416405376494,-2.56281926905284,
12.5804173076348));
#441209=CARTESIAN_POINT('Ctrl Pts',(0.746701161405496,-2.56353474192417,
12.5799304713245));
#441210=CARTESIAN_POINT('Ctrl Pts',(0.745814748800342,-2.56442143820894,
12.5793271277669));
#441211=CARTESIAN_POINT('Ctrl Pts',(0.74508503942716,-2.56541064851979,
12.5785808224116));
#441212=CARTESIAN_POINT('Ctrl Pts',(0.744517268174651,-2.56644184766051,
12.5777485681082));
#441213=CARTESIAN_POINT('Ctrl Pts',(0.743671226804427,-2.56797844735649,
12.576508418016));
#441214=CARTESIAN_POINT('Ctrl Pts',(0.743185860889815,-2.56959202705384,
12.5750928681475));
#441215=CARTESIAN_POINT('Ctrl Pts',(0.743081587281356,-2.57101497634515,
12.5737548217797));
#441216=CARTESIAN_POINT('Ctrl Pts',(0.743081587281356,-2.57101497634515,
12.5737548217797));
#441217=CARTESIAN_POINT('Ctrl Pts',(0.726767074738834,-2.57229573992789,
12.5770542771492));
#441218=CARTESIAN_POINT('Ctrl Pts',(0.725531957228311,-2.58356219985525,
12.5893111709658));
#441219=CARTESIAN_POINT('Ctrl Pts',(0.740433579933582,-2.59563210475723,
12.5508408821982));
#441220=CARTESIAN_POINT('Ctrl Pts',(0.72406826870519,-2.59691363237191,
12.55409748406));
#441221=CARTESIAN_POINT('Ctrl Pts',(0.72283157550105,-2.60819446541667,
12.5663972313419));
#441222=CARTESIAN_POINT('Ctrl Pts',(0.737786986607698,-2.62022505918647,
12.52790050457));
#441223=CARTESIAN_POINT('Ctrl Pts',(0.721374631527474,-2.62148437569243,
12.5311362602938));
#441224=CARTESIAN_POINT('Ctrl Pts',(0.720133918015219,-2.63280188106977,
12.5434568539655));
#441225=CARTESIAN_POINT('Ctrl Pts',(0.735141683647397,-2.64479571678053,
12.5049357605811));
#441226=CARTESIAN_POINT('Ctrl Pts',(0.718685624378847,-2.64601288494447,
12.5081700652078));
#441227=CARTESIAN_POINT('Ctrl Pts',(0.717438771407679,-2.65738639306438,
12.5204921097672));
#441228=CARTESIAN_POINT('Ctrl Pts',(0.73531538303103,-2.64318231091899,
12.5064436508395));
#441229=CARTESIAN_POINT('Ctrl Pts',(0.734212568288885,-2.64370446744255,
12.5062361689309));
#441230=CARTESIAN_POINT('Ctrl Pts',(0.733043465289341,-2.64420044102743,
12.5061871075061));
#441231=CARTESIAN_POINT('Ctrl Pts',(0.731886658499308,-2.64461615089218,
12.5063648335164));
#441232=CARTESIAN_POINT('Ctrl Pts',(0.731361165500473,-2.64480499195479,
12.5064455676329));
#441233=CARTESIAN_POINT('Ctrl Pts',(0.730830805828037,-2.64497969691044,
12.506574497099));
#441234=CARTESIAN_POINT('Ctrl Pts',(0.730317990902744,-2.64513177674755,
12.5067492519495));
#441235=CARTESIAN_POINT('Ctrl Pts',(0.729287469404289,-2.64543738708354,
12.5071004286051));
#441236=CARTESIAN_POINT('Ctrl Pts',(0.72828967953303,-2.64566209299121,
12.5076537929613));
#441237=CARTESIAN_POINT('Ctrl Pts',(0.727401588684731,-2.64579825646475,
12.5083435010505));
#441238=CARTESIAN_POINT('Ctrl Pts',(0.727345678058567,-2.64580682876913,
12.5083869222964));
#441239=CARTESIAN_POINT('Ctrl Pts',(0.727290194313603,-2.64581503927738,
12.5084308732337));
#441240=CARTESIAN_POINT('Ctrl Pts',(0.727235153116011,-2.64582288189328,
12.5084753333615));
#441241=CARTESIAN_POINT('Ctrl Pts',(0.72679365006355,-2.64588579002413,
12.5088319622689));
#441242=CARTESIAN_POINT('Ctrl Pts',(0.726371839947139,-2.64592758170536,
12.509227847131));
#441243=CARTESIAN_POINT('Ctrl Pts',(0.725982541449329,-2.64594980066293,
12.5096423454524));
#441244=CARTESIAN_POINT('Ctrl Pts',(0.72476265225349,-2.64601942504223,
12.5109411997424));
#441245=CARTESIAN_POINT('Ctrl Pts',(0.72378752049948,-2.64591079653777,
12.5124831113042));
#441246=CARTESIAN_POINT('Ctrl Pts',(0.723009761835327,-2.64570583328299,
12.5140723025007));
#441247=CARTESIAN_POINT('Ctrl Pts',(0.722936884996639,-2.64568662800152,
12.5142212114565));
#441248=CARTESIAN_POINT('Ctrl Pts',(0.722865718184468,-2.64566659569232,
12.5143705582413));
#441249=CARTESIAN_POINT('Ctrl Pts',(0.722796210323367,-2.64564581567146,
12.5145201959299));
#441250=CARTESIAN_POINT('Ctrl Pts',(0.721903278361162,-2.64537886536533,
12.5164425148273));
#441251=CARTESIAN_POINT('Ctrl Pts',(0.721250455980803,-2.64498966012505,
12.5184635205941));
#441252=CARTESIAN_POINT('Ctrl Pts',(0.720758552358941,-2.6445214063396,
12.5205025929158));
#441253=CARTESIAN_POINT('Ctrl Pts',(0.720473228761024,-2.6442498005842,
12.5216853356836));
#441254=CARTESIAN_POINT('Ctrl Pts',(0.720242227640543,-2.64395244013477,
12.5228750347131));
#441255=CARTESIAN_POINT('Ctrl Pts',(0.720053228377979,-2.64364278366818,
12.5240609649613));
#441256=CARTESIAN_POINT('Ctrl Pts',(0.719589339827475,-2.64288274848343,
12.5269717671326));
#441257=CARTESIAN_POINT('Ctrl Pts',(0.719374301150302,-2.64202183190473,
12.5299036066169));
#441258=CARTESIAN_POINT('Ctrl Pts',(0.719328508168226,-2.64109427860225,
12.5328133004019));
#441259=CARTESIAN_POINT('Ctrl Pts',(0.719306524870384,-2.64064899900724,
12.5342101228451));
#441260=CARTESIAN_POINT('Ctrl Pts',(0.719324096111705,-2.64018889232598,
12.5356023438238));
#441261=CARTESIAN_POINT('Ctrl Pts',(0.719375533633238,-2.6397196902469,
12.5369868989719));
#441262=CARTESIAN_POINT('Origin',(-0.674793679548759,-15.3084091091921,
-1.23987515702209));
#441263=CARTESIAN_POINT('Ctrl Pts',(0.821936740326726,-2.60956477888538,
12.5369868989719));
#441264=CARTESIAN_POINT('Ctrl Pts',(0.831563750894994,-2.62150646935213,
12.5369868989719));
#441265=CARTESIAN_POINT('Ctrl Pts',(0.846097674417172,-2.61660255553389,
12.5369868989719));
#441266=CARTESIAN_POINT('Ctrl Pts',(0.825191097956303,-2.61360149574402,
12.5218025310016));
#441267=CARTESIAN_POINT('Ctrl Pts',(0.834891989456039,-2.62035046365142,
12.5216901060417));
#441268=CARTESIAN_POINT('Ctrl Pts',(0.846053375474105,-2.61661751991462,
12.5161920673677));
#441269=CARTESIAN_POINT('Ctrl Pts',(0.823586269307168,-2.61941188266763,
12.5042015548895));
#441270=CARTESIAN_POINT('Ctrl Pts',(0.829457255023867,-2.62204035593764,
12.4980677368514));
#441271=CARTESIAN_POINT('Ctrl Pts',(0.835935296554527,-2.61998469116661,
12.4907278922778));
#441272=CARTESIAN_POINT('Ctrl Pts',(0.81041967336277,-2.62110885819555,
12.506463626192));
#441273=CARTESIAN_POINT('Ctrl Pts',(0.812352348575499,-2.62735963453601,
12.4999376786891));
#441274=CARTESIAN_POINT('Ctrl Pts',(0.812328743757883,-2.62728329039163,
12.4906970594712));
#441275=CARTESIAN_POINT('Origin',(0.839064199301453,-2.59575716688804,12.5369868989719));
#441276=CARTESIAN_POINT('Origin',(0.839064199301453,-2.59575716688804,14.));
#441277=CARTESIAN_POINT('Origin',(0.839064199301453,-2.59575716688804,13.7435492065112));
#441278=CARTESIAN_POINT('Ctrl Pts',(0.806386526442056,-2.59035057362389,
13.793642941384));
#441279=CARTESIAN_POINT('Ctrl Pts',(0.813167336811863,-2.5987723804214,
13.8071662555867));
#441280=CARTESIAN_POINT('Ctrl Pts',(0.827858210662747,-2.59015857701453,
13.8103758687955));
#441281=CARTESIAN_POINT('Ctrl Pts',(0.816842815313936,-2.60327062502669,
13.7804579775006));
#441282=CARTESIAN_POINT('Ctrl Pts',(0.82521762117959,-2.61365601372629,
13.7901904343352));
#441283=CARTESIAN_POINT('Ctrl Pts',(0.839919976902593,-2.60799062226948,
13.7927914348262));
#441284=CARTESIAN_POINT('Ctrl Pts',(0.822998826116797,-2.61087714549983,
13.7597120340895));
#441285=CARTESIAN_POINT('Ctrl Pts',(0.832695295726823,-2.62289236780633,
13.7635825532445));
#441286=CARTESIAN_POINT('Ctrl Pts',(0.847053960171936,-2.61849183698646,
13.7651073818885));
#441287=CARTESIAN_POINT('Ctrl Pts',(0.821793338245602,-2.60938761462116,
13.7381884353898));
#441288=CARTESIAN_POINT('Ctrl Pts',(0.83126214444869,-2.62112216274687,
13.7368803041982));
#441289=CARTESIAN_POINT('Ctrl Pts',(0.845657323078979,-2.6164351093739,
13.7363986145813));
#441290=CARTESIAN_POINT('Origin',(0.826024902936919,-2.57964549287853,13.7902182540695));
#441291=CARTESIAN_POINT('Ctrl Pts',(0.786420381817885,-2.56567995817206,
13.8235227101244));
#441292=CARTESIAN_POINT('Ctrl Pts',(0.793649704393192,-2.5746197335284,
13.8358800583119));
#441293=CARTESIAN_POINT('Ctrl Pts',(0.808196285377077,-2.56668102892776,
13.8390832900376));
#441294=CARTESIAN_POINT('Ctrl Pts',(0.793923981208646,-2.57495158939197,
13.8124254819053));
#441295=CARTESIAN_POINT('Ctrl Pts',(0.801167343242206,-2.58390872549045,
13.8247886449158));
#441296=CARTESIAN_POINT('Ctrl Pts',(0.81572413941509,-2.57594502871794,
13.8279860620657));
#441297=CARTESIAN_POINT('Ctrl Pts',(0.801424217730241,-2.58421906536838,
13.8013225099954));
#441298=CARTESIAN_POINT('Ctrl Pts',(0.808678199959595,-2.59318933713958,
13.8136962257787));
#441299=CARTESIAN_POINT('Ctrl Pts',(0.823248298065882,-2.58520491066953,
13.8168830918626));
#441300=CARTESIAN_POINT('Ctrl Pts',(0.808921222226775,-2.59348254777547,
13.7902140179785));
#441301=CARTESIAN_POINT('Ctrl Pts',(0.816182628865665,-2.60246200628751,
13.802602731458));
#441302=CARTESIAN_POINT('Ctrl Pts',(0.830768905102013,-2.59446083774294,
13.8057746032558));
#441303=CARTESIAN_POINT('Origin',(0.803524054690898,-2.55184289358618,13.8235269408515));
#441304=CARTESIAN_POINT('Ctrl Pts',(0.725531957228311,-2.58356219985525,
13.8235269408515));
#441305=CARTESIAN_POINT('Ctrl Pts',(0.724245237673885,-2.59529936184524,
13.8362179249168));
#441306=CARTESIAN_POINT('Ctrl Pts',(0.707191314275894,-2.59620859272501,
13.8391868794938));
#441307=CARTESIAN_POINT('Ctrl Pts',(0.726709249613043,-2.57282320752265,
13.8400110824519));
#441308=CARTESIAN_POINT('Ctrl Pts',(0.722276990282717,-2.58186073705733,
13.8494522556837));
#441309=CARTESIAN_POINT('Ctrl Pts',(0.709240492959898,-2.57854748714394,
13.85569149686));
#441310=CARTESIAN_POINT('Ctrl Pts',(0.73495824762352,-2.55877501340853,
13.8586819406588));
#441311=CARTESIAN_POINT('Ctrl Pts',(0.730784695111075,-2.56001497431954,
13.868010383617));
#441312=CARTESIAN_POINT('Ctrl Pts',(0.723059893033655,-2.55530113303484,
13.8744918421245));
#441313=CARTESIAN_POINT('Ctrl Pts',(0.764966001190711,-2.54990899830604,
13.8587686893867));
#441314=CARTESIAN_POINT('Ctrl Pts',(0.769102393088287,-2.54868001905906,
13.8680909899357));
#441315=CARTESIAN_POINT('Ctrl Pts',(0.773014719528825,-2.54054428901632,
13.8745789365163));
#441316=CARTESIAN_POINT('Ctrl Pts',(0.779615459250033,-2.5572716303441,
13.8400379222776));
#441317=CARTESIAN_POINT('Ctrl Pts',(0.788231675728506,-2.56247076945594,
13.8494748685453));
#441318=CARTESIAN_POINT('Ctrl Pts',(0.797403990081898,-2.55264072598367,
13.8557104837033));
#441319=CARTESIAN_POINT('Ctrl Pts',(0.786422857481969,-2.56568301835912,
13.8235269408542));
#441320=CARTESIAN_POINT('Ctrl Pts',(0.793850903705796,-2.57486129423682,
13.8362179249195));
#441321=CARTESIAN_POINT('Ctrl Pts',(0.808689144339033,-2.56640614083984,
13.8391868794965));
#441322=CARTESIAN_POINT('Origin',(0.703662978283174,-2.58116475123283,13.8235269408515));
#441323=CARTESIAN_POINT('Ctrl Pts',(0.721634688079212,-2.61911219223003,
13.7902140241682));
#441324=CARTESIAN_POINT('Ctrl Pts',(0.72038065990436,-2.63059200097101,
13.8026027327198));
#441325=CARTESIAN_POINT('Ctrl Pts',(0.703784151790531,-2.63174692551464,
13.8057746032556));
#441326=CARTESIAN_POINT('Ctrl Pts',(0.722933352896948,-2.60726606828531,
13.8013225161808));
#441327=CARTESIAN_POINT('Ctrl Pts',(0.721680603817138,-2.61873413471468,
13.8136962270464));
#441328=CARTESIAN_POINT('Ctrl Pts',(0.705106757049487,-2.61989439702825,
13.8168830918628));
#441329=CARTESIAN_POINT('Ctrl Pts',(0.72423257758078,-2.59541483737002,
13.8124254880875));
#441330=CARTESIAN_POINT('Ctrl Pts',(0.722981661108411,-2.60686611166678,
13.8247886461868));
#441331=CARTESIAN_POINT('Ctrl Pts',(0.706430211948158,-2.60803662133964,
13.8279860620656));
#441332=CARTESIAN_POINT('Ctrl Pts',(0.725532384796289,-2.58355829273389,
13.8235227163065));
#441333=CARTESIAN_POINT('Ctrl Pts',(0.724283893152617,-2.59498737195546,
13.8358800595847));
#441334=CARTESIAN_POINT('Ctrl Pts',(0.707754549332814,-2.59617338362708,
13.8390832900376));
#441335=CARTESIAN_POINT('Origin',(0.699765280213318,-2.61671866309858,13.7902182540695));
#441336=CARTESIAN_POINT('Ctrl Pts',(0.719404914178971,-2.63945143449022,
13.7382347919292));
#441337=CARTESIAN_POINT('Ctrl Pts',(0.717784306570684,-2.65445448417065,
13.7369371795943));
#441338=CARTESIAN_POINT('Ctrl Pts',(0.703126890298583,-2.65828905393098,
13.7364597369711));
#441339=CARTESIAN_POINT('Ctrl Pts',(0.719198782097412,-2.6413317279644,
13.7595490285574));
#441340=CARTESIAN_POINT('Ctrl Pts',(0.71753850857087,-2.65669262957323,
13.7633824266926));
#441341=CARTESIAN_POINT('Ctrl Pts',(0.703065061656196,-2.66074392500999,
13.7648920890506));
#441342=CARTESIAN_POINT('Ctrl Pts',(0.720250044428475,-2.63174233425766,
13.780380659011));
#441343=CARTESIAN_POINT('Ctrl Pts',(0.718819334450415,-2.64502954446009,
13.7901039518744));
#441344=CARTESIAN_POINT('Ctrl Pts',(0.703383982415013,-2.64822881765391,
13.7926933640892));
#441345=CARTESIAN_POINT('Ctrl Pts',(0.722077372954516,-2.61507382736496,
13.7936647693663));
#441346=CARTESIAN_POINT('Ctrl Pts',(0.720928562832835,-2.62582806221682,
13.8072068914933));
#441347=CARTESIAN_POINT('Ctrl Pts',(0.70389408990918,-2.62651435811564,
13.8104111085397));
#441348=CARTESIAN_POINT('Origin',(0.6975065546881,-2.63732224162447,13.7435492065112));
#441349=CARTESIAN_POINT('Origin',(0.697506554688101,-2.63732224162448,14.));
#441350=CARTESIAN_POINT('Origin',(0.697506554688101,-2.63732224162448,12.5369868989719));
#441351=CARTESIAN_POINT('Ctrl Pts',(0.735310456050207,-2.6431646002371,
12.506462012331));
#441352=CARTESIAN_POINT('Ctrl Pts',(0.737062907725849,-2.64946400505934,
12.4999388158272));
#441353=CARTESIAN_POINT('Ctrl Pts',(0.737042173924327,-2.64938947483913,
12.4907030323752));
#441354=CARTESIAN_POINT('Ctrl Pts',(0.723316048698657,-2.64885342924135,
12.5042014951932));
#441355=CARTESIAN_POINT('Ctrl Pts',(0.719800462179154,-2.65423689917626,
12.4980716682127));
#441356=CARTESIAN_POINT('Ctrl Pts',(0.713244453351888,-2.65601012039275,
12.4907355092743));
#441357=CARTESIAN_POINT('Ctrl Pts',(0.718823723546654,-2.64483538046438,
12.5218047446509));
#441358=CARTESIAN_POINT('Ctrl Pts',(0.714312756107054,-2.65575188373671,
12.5216906929434));
#441359=CARTESIAN_POINT('Ctrl Pts',(0.702911729540246,-2.65864797550892,
12.5161988840776));
#441360=CARTESIAN_POINT('Ctrl Pts',(0.719379686685556,-2.63968149926658,
12.5369868989719));
#441361=CARTESIAN_POINT('Ctrl Pts',(0.717735724846863,-2.65492298610329,
12.5369868989719));
#441362=CARTESIAN_POINT('Ctrl Pts',(0.702868034741916,-2.6586589361115,
12.5369868989719));
#441363=CARTESIAN_POINT('Origin',(1.45144742314195E-31,-1.0095038568149E-30,
12.5));
#441364=CARTESIAN_POINT('Origin',(0.933702113402283,-2.51582801973993,12.5));
#441365=CARTESIAN_POINT('',(0.933702113402283,-2.51582801973993,12.5893111709658));
#441366=CARTESIAN_POINT('',(0.933702113402283,-2.51582801973993,13.8235269408515));
#441367=CARTESIAN_POINT('',(0.933702113402283,-2.51582801973993,12.5));
#441368=CARTESIAN_POINT('',(0.93271535848469,-2.5515813274741,13.7902182540695));
#441369=CARTESIAN_POINT('',(0.933702113402283,-2.51582801973993,13.8235269408515));
#441370=CARTESIAN_POINT('',(0.932143531606478,-2.57230045639141,13.7435492065112));
#441371=CARTESIAN_POINT('Origin',(0.934025160108408,-2.50413480510781,13.7445212918703));
#441372=CARTESIAN_POINT('',(0.932143531606478,-2.57230045639141,12.5369868989719));
#441373=CARTESIAN_POINT('',(0.932143531606478,-2.57230045639141,12.5));
#441374=CARTESIAN_POINT('Ctrl Pts',(0.932143531606478,-2.57230045639141,
12.5369868989719));
#441375=CARTESIAN_POINT('Ctrl Pts',(0.932662679960157,-2.55349004002777,
12.5544431401645));
#441376=CARTESIAN_POINT('Ctrl Pts',(0.933182199622538,-2.5346661699544,
12.5718848856037));
#441377=CARTESIAN_POINT('Ctrl Pts',(0.933702113402283,-2.51582801973993,
12.5893111709658));
#441378=CARTESIAN_POINT('Origin',(1.18278282538531,-2.69199760279828,12.5));
#441379=CARTESIAN_POINT('',(1.0319343935952,-2.53391645655151,13.7435492065112));
#441380=CARTESIAN_POINT('',(1.01762523340839,-2.51892121651278,13.7902182540695));
#441381=CARTESIAN_POINT('Origin',(0.980023233558798,-2.47951631739082,13.7418732680453));
#441382=CARTESIAN_POINT('',(0.992933084929655,-2.49304515609576,13.8235269408515));
#441383=CARTESIAN_POINT('',(1.01762523340839,-2.51892121651278,13.7902182540695));
#441384=CARTESIAN_POINT('',(0.992933084929655,-2.49304515609576,12.5893111709658));
#441385=CARTESIAN_POINT('',(0.992933084929655,-2.49304515609576,12.5));
#441386=CARTESIAN_POINT('',(1.0319343935952,-2.53391645655151,12.5369868989719));
#441387=CARTESIAN_POINT('Ctrl Pts',(0.992933084929655,-2.49304515609576,
12.5893111709658));
#441388=CARTESIAN_POINT('Ctrl Pts',(1.00594319313052,-2.50667905863476,
12.5718848856037));
#441389=CARTESIAN_POINT('Ctrl Pts',(1.01894343910083,-2.52030262607983,
12.5544431401645));
#441390=CARTESIAN_POINT('Ctrl Pts',(1.0319343935952,-2.53391645655151,12.5369868989719));
#441391=CARTESIAN_POINT('',(1.0319343935952,-2.53391645655151,12.5));
#441392=CARTESIAN_POINT('Origin',(0.968064029091839,-2.51677637365271,12.5));
#441393=CARTESIAN_POINT('',(0.954685208566533,-2.48511255623394,13.8587068136939));
#441394=CARTESIAN_POINT('Ctrl Pts',(0.992933084934336,-2.49304515609109,
13.8235269408542));
#441395=CARTESIAN_POINT('Ctrl Pts',(0.991723363543063,-2.491777432311,13.8262006681044));
#441396=CARTESIAN_POINT('Ctrl Pts',(0.990359696394175,-2.49060004539963,
13.8288634856214));
#441397=CARTESIAN_POINT('Ctrl Pts',(0.988854254011685,-2.48950754701841,
13.8314912288862));
#441398=CARTESIAN_POINT('Ctrl Pts',(0.987302298194516,-2.48838129387334,
13.834200161153));
#441399=CARTESIAN_POINT('Ctrl Pts',(0.985598238984165,-2.48734360273377,
13.8368750301949));
#441400=CARTESIAN_POINT('Ctrl Pts',(0.983715583286505,-2.48640988080418,
13.8394886372968));
#441401=CARTESIAN_POINT('Ctrl Pts',(0.983570181220282,-2.48633776719466,
13.839690492513));
#441402=CARTESIAN_POINT('Ctrl Pts',(0.983423700740891,-2.48626629159546,
13.8398919674349));
#441403=CARTESIAN_POINT('Ctrl Pts',(0.983276123704499,-2.48619547088669,
13.8400930404591));
#441404=CARTESIAN_POINT('Ctrl Pts',(0.980976774192673,-2.48509203659824,
13.8432258934518));
#441405=CARTESIAN_POINT('Ctrl Pts',(0.978423447081325,-2.48415219749209,
13.8462331177034));
#441406=CARTESIAN_POINT('Ctrl Pts',(0.975666096106158,-2.48349713443913,
13.8489036603661));
#441407=CARTESIAN_POINT('Ctrl Pts',(0.974763858778177,-2.48328279018485,
13.8497774930041));
#441408=CARTESIAN_POINT('Ctrl Pts',(0.973839948934597,-2.4830991177115,
13.85061494757));
#441409=CARTESIAN_POINT('Ctrl Pts',(0.972896615947958,-2.4829508726377,
13.8514076489583));
#441410=CARTESIAN_POINT('Ctrl Pts',(0.970901330632243,-2.48263731292648,
13.8530843267192));
#441411=CARTESIAN_POINT('Ctrl Pts',(0.968622700636087,-2.48245437182213,
13.8546805203176));
#441412=CARTESIAN_POINT('Ctrl Pts',(0.966182057338866,-2.48254867523269,
13.8559412814273));
#441413=CARTESIAN_POINT('Ctrl Pts',(0.965855420113751,-2.48256129608735,
13.8561100121513));
#441414=CARTESIAN_POINT('Ctrl Pts',(0.965525928528726,-2.48257882230831,
13.8562727473908));
#441415=CARTESIAN_POINT('Ctrl Pts',(0.965193912474154,-2.48260154034592,
13.8564289040185));
#441416=CARTESIAN_POINT('Ctrl Pts',(0.963688223454477,-2.48270456638732,
13.8571370725437));
#441417=CARTESIAN_POINT('Ctrl Pts',(0.962104305481676,-2.48291844998919,
13.8577210840554));
#441418=CARTESIAN_POINT('Ctrl Pts',(0.96050765308351,-2.48326396153404,
13.8581177131616));
#441419=CARTESIAN_POINT('Ctrl Pts',(0.960057980813083,-2.48336126947722,
13.8582294175695));
#441420=CARTESIAN_POINT('Ctrl Pts',(0.959607295647674,-2.48346884028903,
13.8583265086086));
#441421=CARTESIAN_POINT('Ctrl Pts',(0.95915702743171,-2.48358669962459,
13.8584082369006));
#441422=CARTESIAN_POINT('Ctrl Pts',(0.958510112749561,-2.48375603188456,
13.8585256585398));
#441423=CARTESIAN_POINT('Ctrl Pts',(0.957856097938983,-2.4839490197037,
13.8586122832068));
#441424=CARTESIAN_POINT('Ctrl Pts',(0.957212195904303,-2.48416140721831,
13.8586682984299));
#441425=CARTESIAN_POINT('Ctrl Pts',(0.956697138104515,-2.48433129617669,
13.8587131050557));
#441426=CARTESIAN_POINT('Ctrl Pts',(0.956182788610058,-2.48451525160693,
13.8587357943552));
#441427=CARTESIAN_POINT('Ctrl Pts',(0.955669256851426,-2.4847137722332,
13.8587355499465));
#441428=CARTESIAN_POINT('Ctrl Pts',(0.955337349032966,-2.48484208084679,
13.8587353919793));
#441429=CARTESIAN_POINT('Ctrl Pts',(0.955009358073341,-2.48497505026233,
13.8587257282814));
#441430=CARTESIAN_POINT('Ctrl Pts',(0.954685208566533,-2.48511255623394,
13.8587068136939));
#441431=CARTESIAN_POINT('Ctrl Pts',(0.954685208566533,-2.48511255623394,
13.8587068136939));
#441432=CARTESIAN_POINT('Ctrl Pts',(0.953619098508562,-2.48556480587889,
13.8586446046467));
#441433=CARTESIAN_POINT('Ctrl Pts',(0.952594490131804,-2.48606606798737,
13.8584824279291));
#441434=CARTESIAN_POINT('Ctrl Pts',(0.951609148388065,-2.4866124708005,
13.8582284286032));
#441435=CARTESIAN_POINT('Ctrl Pts',(0.950598302378936,-2.48717301652643,
13.8579678548414));
#441436=CARTESIAN_POINT('Ctrl Pts',(0.949627055603989,-2.48778377876022,
13.857615680862));
#441437=CARTESIAN_POINT('Ctrl Pts',(0.948728540580012,-2.48841247603173,
13.8571944833187));
#441438=CARTESIAN_POINT('Ctrl Pts',(0.94648620444509,-2.48998145437067,
13.8561433417727));
#441439=CARTESIAN_POINT('Ctrl Pts',(0.944589205204621,-2.49173159547621,
13.8546163505474));
#441440=CARTESIAN_POINT('Ctrl Pts',(0.943031722982616,-2.49345620151167,
13.8528973491086));
#441441=CARTESIAN_POINT('Ctrl Pts',(0.942747193959171,-2.49377126159015,
13.8525833129072));
#441442=CARTESIAN_POINT('Ctrl Pts',(0.942473859162767,-2.49408543390456,
13.8522628768812));
#441443=CARTESIAN_POINT('Ctrl Pts',(0.94221150514556,-2.49439744083207,
13.851937733538));
#441444=CARTESIAN_POINT('Ctrl Pts',(0.940609345562412,-2.49630282384938,
13.8499521282529));
#441445=CARTESIAN_POINT('Ctrl Pts',(0.939260597355519,-2.49831943535962,
13.847639871647));
#441446=CARTESIAN_POINT('Ctrl Pts',(0.938169364659963,-2.50029662525464,
13.8452109780794));
#441447=CARTESIAN_POINT('Ctrl Pts',(0.937678396482841,-2.5011862039142,
13.8441181685877));
#441448=CARTESIAN_POINT('Ctrl Pts',(0.937238847234745,-2.50206769441421,
13.8430021611332));
#441449=CARTESIAN_POINT('Ctrl Pts',(0.936847826073116,-2.50292791449968,
13.8418824960098));
#441450=CARTESIAN_POINT('Ctrl Pts',(0.935926374720656,-2.50495504509759,
13.8392439765549));
#441451=CARTESIAN_POINT('Ctrl Pts',(0.935226917622972,-2.50695939684577,
13.8364981347964));
#441452=CARTESIAN_POINT('Ctrl Pts',(0.934715295282572,-2.50893499539145,
13.8336931113419));
#441453=CARTESIAN_POINT('Ctrl Pts',(0.934217007614046,-2.51085910291283,
13.8309611966328));
#441454=CARTESIAN_POINT('Ctrl Pts',(0.933896938108789,-2.51275800613543,
13.8281701127186));
#441455=CARTESIAN_POINT('Ctrl Pts',(0.933762551511809,-2.51462152201201,
13.8253580685121));
#441456=CARTESIAN_POINT('Ctrl Pts',(0.933733416352549,-2.51502553426522,
13.8247484142933));
#441457=CARTESIAN_POINT('Ctrl Pts',(0.933713159135509,-2.51542779726107,
13.8241378483365));
#441458=CARTESIAN_POINT('Ctrl Pts',(0.933702113402283,-2.51582801973993,
13.8235269408515));
#441459=CARTESIAN_POINT('',(0.955837885903104,-2.48464983405672,12.5969504640361));
#441460=CARTESIAN_POINT('Origin',(0.968075724091053,-2.5168073237707,12.584524458991));
#441461=CARTESIAN_POINT('Origin',(0.968075724091053,-2.5168073237707,12.584524458991));
#441462=CARTESIAN_POINT('Ctrl Pts',(0.992933084929655,-2.49304515609576,
12.5893111709658));
#441463=CARTESIAN_POINT('Ctrl Pts',(0.985108542234981,-2.48484545084624,
12.5770542771492));
#441464=CARTESIAN_POINT('Ctrl Pts',(0.971370553186036,-2.49373765708238,
12.5737548217797));
#441465=CARTESIAN_POINT('Ctrl Pts',(1.01004273380832,-2.51097515957357,
12.5663937883685));
#441466=CARTESIAN_POINT('Ctrl Pts',(1.00220820982281,-2.50276499446125,
12.5540940315304));
#441467=CARTESIAN_POINT('Ctrl Pts',(0.988429394417114,-2.51168745159643,
12.5508374392248));
#441468=CARTESIAN_POINT('Ctrl Pts',(1.02713511926105,-2.52888707189772,
12.5434499600945));
#441469=CARTESIAN_POINT('Ctrl Pts',(1.01927512244805,-2.52065021261488,
12.5311293540533));
#441470=CARTESIAN_POINT('Ctrl Pts',(1.0054724240448,-2.52961889598253,12.5278936106989));
#441471=CARTESIAN_POINT('Ctrl Pts',(1.04421159355556,-2.54678231017295,
12.5204817579905));
#441472=CARTESIAN_POINT('Ctrl Pts',(1.03631269512993,-2.53850468406579,
12.5081597038247));
#441473=CARTESIAN_POINT('Ctrl Pts',(1.02250088105112,-2.54753340694043,
12.5049254088044));
#441474=CARTESIAN_POINT('Ctrl Pts',(1.0319343935952,-2.53391645655151,12.5369868989719));
#441475=CARTESIAN_POINT('Ctrl Pts',(1.03257746963189,-2.53459036632423,
12.5342545179733));
#441476=CARTESIAN_POINT('Ctrl Pts',(1.03310094282764,-2.53531963508585,
12.5314872231885));
#441477=CARTESIAN_POINT('Ctrl Pts',(1.03342991240674,-2.5360957794836,12.5287124745063));
#441478=CARTESIAN_POINT('Ctrl Pts',(1.03372659350178,-2.53679574502586,
12.5262100684184));
#441479=CARTESIAN_POINT('Ctrl Pts',(1.03386387344133,-2.53753351365892,
12.5237004536639));
#441480=CARTESIAN_POINT('Ctrl Pts',(1.03377893743462,-2.53833388010387,
12.5212220730815));
#441481=CARTESIAN_POINT('Ctrl Pts',(1.03371391157394,-2.53894662985469,
12.5193246583486));
#441482=CARTESIAN_POINT('Ctrl Pts',(1.03351723171028,-2.53960332586833,
12.517417831369));
#441483=CARTESIAN_POINT('Ctrl Pts',(1.03309208063785,-2.54029499867328,
12.5155812248347));
#441484=CARTESIAN_POINT('Ctrl Pts',(1.03291096399581,-2.54058965500595,
12.5147988205793));
#441485=CARTESIAN_POINT('Ctrl Pts',(1.03268843641229,-2.54089110312969,
12.5140295443047));
#441486=CARTESIAN_POINT('Ctrl Pts',(1.03241788174527,-2.54120059129584,
12.5132817086137));
#441487=CARTESIAN_POINT('Ctrl Pts',(1.03200843385653,-2.54166895976869,
12.5121499604604));
#441488=CARTESIAN_POINT('Ctrl Pts',(1.03147476479515,-2.54216114921371,
12.5110494206568));
#441489=CARTESIAN_POINT('Ctrl Pts',(1.03078416050836,-2.54265936385898,
12.5100666561695));
#441490=CARTESIAN_POINT('Ctrl Pts',(1.03038761711721,-2.54294543756101,
12.5095023550641));
#441491=CARTESIAN_POINT('Ctrl Pts',(1.02993436812066,-2.54323627373919,
12.5089719619137));
#441492=CARTESIAN_POINT('Ctrl Pts',(1.02942945988058,-2.54352104550052,
12.5085043804652));
#441493=CARTESIAN_POINT('Ctrl Pts',(1.02869059244015,-2.5439377718791,12.5078201359221));
#441494=CARTESIAN_POINT('Ctrl Pts',(1.02781907629294,-2.544352546056,12.5072563000949));
#441495=CARTESIAN_POINT('Ctrl Pts',(1.02687034923004,-2.54472960804893,
12.5068768744332));
#441496=CARTESIAN_POINT('Ctrl Pts',(1.0261862517071,-2.54500149570287,12.5066032824114));
#441497=CARTESIAN_POINT('Ctrl Pts',(1.02545001273742,-2.54525860774108,
12.5064197834844));
#441498=CARTESIAN_POINT('Ctrl Pts',(1.02470359803672,-2.54548902668966,
12.5063282718343));
#441499=CARTESIAN_POINT('Ctrl Pts',(1.02361406365786,-2.54582536701869,
12.5061946931565));
#441500=CARTESIAN_POINT('Ctrl Pts',(1.02247987369661,-2.5461130362937,12.5062515701262));
#441501=CARTESIAN_POINT('Ctrl Pts',(1.02137521992727,-2.54634917114627,
12.5064436508398));
#441502=CARTESIAN_POINT('',(0.971370553186036,-2.49373765708238,12.5737548217797));
#441503=CARTESIAN_POINT('Origin',(0.977016889193453,-2.50823313533221,12.5893111709658));
#441504=CARTESIAN_POINT('Ctrl Pts',(1.02137521992727,-2.54634917114627,
12.5064436508398));
#441505=CARTESIAN_POINT('Ctrl Pts',(1.01397288185703,-2.53856163117237,
12.5164271754438));
#441506=CARTESIAN_POINT('Ctrl Pts',(1.00656776093935,-2.53077086027243,
12.5264061185523));
#441507=CARTESIAN_POINT('Ctrl Pts',(0.999159758478661,-2.52297674530802,
12.536380305637));
#441508=CARTESIAN_POINT('Ctrl Pts',(0.989901257907586,-2.51323568241935,
12.5488460165097));
#441509=CARTESIAN_POINT('Ctrl Pts',(0.980638253669115,-2.50348939323112,
12.5613043021964));
#441510=CARTESIAN_POINT('Ctrl Pts',(0.971370553186036,-2.49373765708238,
12.5737548217797));
#441511=CARTESIAN_POINT('Ctrl Pts',(0.933702113402283,-2.51582801973993,
12.5893111709658));
#441512=CARTESIAN_POINT('Ctrl Pts',(0.93401480008439,-2.50449837448518,
12.5770542771492));
#441513=CARTESIAN_POINT('Ctrl Pts',(0.950170633310257,-2.50189208830885,
12.5737548217797));
#441514=CARTESIAN_POINT('Ctrl Pts',(0.933993847357083,-2.5052575592573,
12.5928319619712));
#441515=CARTESIAN_POINT('Ctrl Pts',(0.93746049473711,-2.49773321394931,
12.5821634970842));
#441516=CARTESIAN_POINT('Ctrl Pts',(0.950267469666604,-2.49804126500864,
12.5773203894503));
#441517=CARTESIAN_POINT('Ctrl Pts',(0.941397848411402,-2.49023208529715,
12.5969440695591));
#441518=CARTESIAN_POINT('Ctrl Pts',(0.94514304634973,-2.48877193634766,
12.5878292599214));
#441519=CARTESIAN_POINT('Ctrl Pts',(0.952908241986078,-2.49268678383356,
12.5813877129824));
#441520=CARTESIAN_POINT('Ctrl Pts',(0.969935724982431,-2.4791973743196,
12.596957478804));
#441521=CARTESIAN_POINT('Ctrl Pts',(0.966218234178142,-2.48064680705999,
12.5878468778671));
#441522=CARTESIAN_POINT('Ctrl Pts',(0.963124494906348,-2.48874287149005,
12.5814011370086));
#441523=CARTESIAN_POINT('Ctrl Pts',(0.985622254728059,-2.48538379426003,
12.5928371701607));
#441524=CARTESIAN_POINT('Ctrl Pts',(0.97800989610333,-2.48213001770463,
12.5821692192951));
#441525=CARTESIAN_POINT('Ctrl Pts',(0.968709785890143,-2.49093523047833,
12.5773318885715));
#441526=CARTESIAN_POINT('Ctrl Pts',(0.992933084929691,-2.49304515609571,
12.5893111709658));
#441527=CARTESIAN_POINT('Ctrl Pts',(0.985108542235019,-2.4848454508462,
12.5770542771492));
#441528=CARTESIAN_POINT('Ctrl Pts',(0.971370553186075,-2.49373765708234,
12.5737548217797));
#441529=CARTESIAN_POINT('',(0.950170633310257,-2.50189208830885,12.5737548217797));
#441530=CARTESIAN_POINT('Origin',(0.955693739443599,-2.51643496624411,12.5893111709658));
#441531=CARTESIAN_POINT('Ctrl Pts',(0.971370553186075,-2.49373765708234,
12.5737548217797));
#441532=CARTESIAN_POINT('Ctrl Pts',(0.970702716238683,-2.49299045333321,
12.5746934679442));
#441533=CARTESIAN_POINT('Ctrl Pts',(0.9698271288722,-2.49228569649437,12.5756680099006));
#441534=CARTESIAN_POINT('Ctrl Pts',(0.968845496035647,-2.491700973789,12.5765688348656));
#441535=CARTESIAN_POINT('Ctrl Pts',(0.968585619609202,-2.49154617492584,
12.5768073183026));
#441536=CARTESIAN_POINT('Ctrl Pts',(0.968318492163072,-2.49139960665602,
12.5770407398754));
#441537=CARTESIAN_POINT('Ctrl Pts',(0.968046285043574,-2.49126222242476,
12.5772674179684));
#441538=CARTESIAN_POINT('Ctrl Pts',(0.966929220633075,-2.49069843468993,
12.5781976435658));
#441539=CARTESIAN_POINT('Ctrl Pts',(0.965658082544084,-2.49026735993831,
12.5790594849312));
#441540=CARTESIAN_POINT('Ctrl Pts',(0.964303191474802,-2.49004383608263,
12.5797571720116));
#441541=CARTESIAN_POINT('Ctrl Pts',(0.963420431225624,-2.48989820225346,
12.580211740231));
#441542=CARTESIAN_POINT('Ctrl Pts',(0.962458945194491,-2.48985257778344,
12.5806009430798));
#441543=CARTESIAN_POINT('Ctrl Pts',(0.961485578068116,-2.48992787122014,
12.5808812374708));
#441544=CARTESIAN_POINT('Ctrl Pts',(0.960649132795379,-2.48999257326061,
12.5811221033394));
#441545=CARTESIAN_POINT('Ctrl Pts',(0.959786798452788,-2.49014800567127,
12.581287365893));
#441546=CARTESIAN_POINT('Ctrl Pts',(0.958948725634985,-2.49039360134612,
12.581359338449));
#441547=CARTESIAN_POINT('Ctrl Pts',(0.958832250818849,-2.49042773407357,
12.5813693411482));
#441548=CARTESIAN_POINT('Ctrl Pts',(0.958716209593221,-2.49046355976426,
12.5813775999465));
#441549=CARTESIAN_POINT('Ctrl Pts',(0.958600699823552,-2.49050102778792,
12.5813841266931));
#441550=CARTESIAN_POINT('Ctrl Pts',(0.958404723528695,-2.49056459682172,
12.5813952001081));
#441551=CARTESIAN_POINT('Ctrl Pts',(0.95820915235056,-2.49063389826755,
12.5814007534795));
#441552=CARTESIAN_POINT('Ctrl Pts',(0.958014137335656,-2.49070908782672,
12.5814005856065));
#441553=CARTESIAN_POINT('Ctrl Pts',(0.957121434843356,-2.49105327623141,
12.5813998171494));
#441554=CARTESIAN_POINT('Ctrl Pts',(0.956301943948017,-2.4914967514541,
12.58127954464));
#441555=CARTESIAN_POINT('Ctrl Pts',(0.955546234478559,-2.49201097252028,
12.5810700125799));
#441556=CARTESIAN_POINT('Ctrl Pts',(0.954633423483868,-2.49263209301946,
12.5808169217085));
#441557=CARTESIAN_POINT('Ctrl Pts',(0.953823001426223,-2.49337032363922,
12.5804173076348));
#441558=CARTESIAN_POINT('Ctrl Pts',(0.953168455051674,-2.49414171485722,
12.5799304713245));
#441559=CARTESIAN_POINT('Ctrl Pts',(0.952357265890236,-2.49509771158963,
12.5793271277669));
#441560=CARTESIAN_POINT('Ctrl Pts',(0.95171061438851,-2.49614310847298,
12.5785808224116));
#441561=CARTESIAN_POINT('Ctrl Pts',(0.95122878465116,-2.49721715501164,
12.5777485681082));
#441562=CARTESIAN_POINT('Ctrl Pts',(0.95051080555412,-2.49881760202482,
12.576508418016));
#441563=CARTESIAN_POINT('Ctrl Pts',(0.950158576379626,-2.5004653744968,
12.5750928681475));
#441564=CARTESIAN_POINT('Ctrl Pts',(0.950170633310256,-2.50189208830885,
12.5737548217797));
#441565=CARTESIAN_POINT('Ctrl Pts',(0.950170633310257,-2.50189208830885,
12.5737548217797));
#441566=CARTESIAN_POINT('Ctrl Pts',(0.934014800084389,-2.50449837448518,
12.5770542771492));
#441567=CARTESIAN_POINT('Ctrl Pts',(0.933702113402283,-2.51582801973993,
12.5893111709658));
#441568=CARTESIAN_POINT('Ctrl Pts',(0.949537961488343,-2.52664314243865,
12.5508408821982));
#441569=CARTESIAN_POINT('Ctrl Pts',(0.933331560880742,-2.52925433066919,
12.55409748406));
#441570=CARTESIAN_POINT('Ctrl Pts',(0.933018475290506,-2.54059842964961,
12.5663972313419));
#441571=CARTESIAN_POINT('Ctrl Pts',(0.948904728579262,-2.55136998776663,
12.52790050457));
#441572=CARTESIAN_POINT('Ctrl Pts',(0.932649630242801,-2.55396287330473,
12.5311362602938));
#441573=CARTESIAN_POINT('Ctrl Pts',(0.932335526857248,-2.565343850286,12.5434568539655));
#441574=CARTESIAN_POINT('Ctrl Pts',(0.948270964343104,-2.57607450527355,
12.5049357605811));
#441575=CARTESIAN_POINT('Ctrl Pts',(0.931968871759239,-2.57862894501183,
12.5081700652078));
#441576=CARTESIAN_POINT('Ctrl Pts',(0.931653214086745,-2.59006623881408,
12.5204921097672));
#441577=CARTESIAN_POINT('Ctrl Pts',(0.948312578200522,-2.57445230977461,
12.5064436508395));
#441578=CARTESIAN_POINT('Ctrl Pts',(0.947255993587591,-2.57506261850493,
12.5062361689309));
#441579=CARTESIAN_POINT('Ctrl Pts',(0.946131207133394,-2.5756522345265,
12.5061871075061));
#441580=CARTESIAN_POINT('Ctrl Pts',(0.945012133735765,-2.57616085164362,
12.5063648335164));
#441581=CARTESIAN_POINT('Ctrl Pts',(0.944503781571251,-2.57639189691103,
12.5064455676329));
#441582=CARTESIAN_POINT('Ctrl Pts',(0.94398942670264,-2.57660924978727,
12.506574497099));
#441583=CARTESIAN_POINT('Ctrl Pts',(0.943490714045272,-2.57680262276842,
12.5067492519495));
#441584=CARTESIAN_POINT('Ctrl Pts',(0.942488531601621,-2.57719121328025,
12.5071004286051));
#441585=CARTESIAN_POINT('Ctrl Pts',(0.941512377411389,-2.57749650063508,
12.5076537929613));
#441586=CARTESIAN_POINT('Ctrl Pts',(0.940638340199299,-2.57770459868467,
12.5083435010505));
#441587=CARTESIAN_POINT('Ctrl Pts',(0.94058331433352,-2.57771769970049,
12.5083869222964));
#441588=CARTESIAN_POINT('Ctrl Pts',(0.940528684438786,-2.57773040532925,
12.5084308732337));
#441589=CARTESIAN_POINT('Ctrl Pts',(0.940474465632242,-2.57774270821808,
12.5084753333615));
#441590=CARTESIAN_POINT('Ctrl Pts',(0.940039559241441,-2.5778413936248,
12.5088319622689));
#441591=CARTESIAN_POINT('Ctrl Pts',(0.939622559073392,-2.57791742768805,
12.509227847131));
#441592=CARTESIAN_POINT('Ctrl Pts',(0.939236366985531,-2.57797130415551,
12.5096423454524));
#441593=CARTESIAN_POINT('Ctrl Pts',(0.938026211903631,-2.57814012915979,
12.5109411997424));
#441594=CARTESIAN_POINT('Ctrl Pts',(0.937045470588517,-2.57811134439835,
12.5124831113042));
#441595=CARTESIAN_POINT('Ctrl Pts',(0.936253593444106,-2.57797045769338,
12.5140723025008));
#441596=CARTESIAN_POINT('Ctrl Pts',(0.936179393688356,-2.57795725645481,
12.5142212114565));
#441597=CARTESIAN_POINT('Ctrl Pts',(0.936106830858711,-2.57794309155734,
12.5143705582413));
#441598=CARTESIAN_POINT('Ctrl Pts',(0.936035860514673,-2.57792804621625,
12.5145201959299));
#441599=CARTESIAN_POINT('Ctrl Pts',(0.935124140781716,-2.57773476640973,
12.5164425148273));
#441600=CARTESIAN_POINT('Ctrl Pts',(0.934441766773685,-2.57740006730229,
12.5184635205941));
#441601=CARTESIAN_POINT('Ctrl Pts',(0.933913332889976,-2.57697346630447,
12.5205025929158));
#441602=CARTESIAN_POINT('Ctrl Pts',(0.933606820292262,-2.57672602081686,
12.5216853356836));
#441603=CARTESIAN_POINT('Ctrl Pts',(0.933352350171766,-2.57644847854563,
12.5228750347131));
#441604=CARTESIAN_POINT('Ctrl Pts',(0.933138739911918,-2.57615525762987,
12.5240609649613));
#441605=CARTESIAN_POINT('Ctrl Pts',(0.93261444498892,-2.5754355626229,12.5269717671326));
#441606=CARTESIAN_POINT('Ctrl Pts',(0.932329949141683,-2.5745950383216,
12.5299036066169));
#441607=CARTESIAN_POINT('Ctrl Pts',(0.932208704326839,-2.57367430392938,
12.5328133004019));
#441608=CARTESIAN_POINT('Ctrl Pts',(0.93215049975584,-2.57323229780835,
12.5342101228451));
#441609=CARTESIAN_POINT('Ctrl Pts',(0.932130509564359,-2.57277228987482,
12.5356023438238));
#441610=CARTESIAN_POINT('Ctrl Pts',(0.932143531606478,-2.57230045639141,
12.5369868989719));
#441611=CARTESIAN_POINT('Origin',(0.575248376757179,-15.3118151806691,-1.23916491245692));
#441612=CARTESIAN_POINT('Ctrl Pts',(1.0319055691249,-2.53388619253255,12.5369868989719));
#441613=CARTESIAN_POINT('Ctrl Pts',(1.04247390524396,-2.54500345727526,
12.5369868989719));
#441614=CARTESIAN_POINT('Ctrl Pts',(1.05655975383268,-2.53893121113229,
12.5369868989719));
#441615=CARTESIAN_POINT('Ctrl Pts',(1.03547812804696,-2.53764421719005,
12.5218025310015));
#441616=CARTESIAN_POINT('Ctrl Pts',(1.04569684416929,-2.54358001574756,
12.5216901060418));
#441617=CARTESIAN_POINT('Ctrl Pts',(1.05651682202664,-2.53894973649539,
12.5161920673677));
#441618=CARTESIAN_POINT('Ctrl Pts',(1.03435223980804,-2.54356607896389,
12.5042015548895));
#441619=CARTESIAN_POINT('Ctrl Pts',(1.04041793527717,-2.54570726636648,
12.4980677368513));
#441620=CARTESIAN_POINT('Ctrl Pts',(1.04670686589631,-2.54313042112641,
12.4907278922778));
#441621=CARTESIAN_POINT('Ctrl Pts',(1.02136777388495,-2.54633060774792,
12.506463626192));
#441622=CARTESIAN_POINT('Ctrl Pts',(1.02380351458147,-2.55240305417384,
12.4999376786891));
#441623=CARTESIAN_POINT('Ctrl Pts',(1.02377376555043,-2.55232888807008,
12.4906970594712));
#441624=CARTESIAN_POINT('Origin',(1.0478505893314,-2.51872847731506,12.5369868989719));
#441625=CARTESIAN_POINT('Origin',(1.0478505893314,-2.51872847731506,14.));
#441626=CARTESIAN_POINT('Origin',(1.0478505893314,-2.51872847731506,13.7435492065112));
#441627=CARTESIAN_POINT('Ctrl Pts',(1.01484096118934,-2.51600340774675,
13.793642941384));
#441628=CARTESIAN_POINT('Ctrl Pts',(1.02228566441025,-2.52384449268177,
13.8071662555867));
#441629=CARTESIAN_POINT('Ctrl Pts',(1.036225550646,-2.51406190839289,13.8103758687955));
#441630=CARTESIAN_POINT('Ctrl Pts',(1.02631556175581,-2.52802818412982,
13.7804579775006));
#441631=CARTESIAN_POINT('Ctrl Pts',(1.03550900673808,-2.53769639187931,
13.7901904343352));
#441632=CARTESIAN_POINT('Ctrl Pts',(1.04970065958661,-2.53085147306375,
13.7927914348263));
#441633=CARTESIAN_POINT('Ctrl Pts',(1.03307109097461,-2.53510762250353,
13.7597120340895));
#441634=CARTESIAN_POINT('Ctrl Pts',(1.04371464854379,-2.54629251285811,
13.7635825532445));
#441635=CARTESIAN_POINT('Ctrl Pts',(1.05766685160311,-2.54073625998993,
13.7651073818884));
#441636=CARTESIAN_POINT('Ctrl Pts',(1.03174820367012,-2.53372130636869,
13.7381884353898));
#441637=CARTESIAN_POINT('Ctrl Pts',(1.04214197781216,-2.54464501314388,
13.7368803041982));
#441638=CARTESIAN_POINT('Ctrl Pts',(1.0561072193107,-2.53880021485767,13.7363986145813));
#441639=CARTESIAN_POINT('Origin',(1.03354142914459,-2.50373323727633,13.7902182540695));
#441640=CARTESIAN_POINT('Ctrl Pts',(0.992930368074177,-2.49304230787617,
13.8235227101244));
#441641=CARTESIAN_POINT('Ctrl Pts',(1.00086431035936,-2.50136307996383,
13.8358800583119));
#441642=CARTESIAN_POINT('Ctrl Pts',(1.01471541067073,-2.4922651093538,13.8390832900376));
#441643=CARTESIAN_POINT('Ctrl Pts',(1.001164723875,-2.50167147549767,13.8124254819053));
#441644=CARTESIAN_POINT('Ctrl Pts',(1.00911407396496,-2.51000840621482,
13.8247886449158));
#441645=CARTESIAN_POINT('Ctrl Pts',(1.0229733183811,-2.50088469395962,13.8279860620657));
#441646=CARTESIAN_POINT('Ctrl Pts',(1.00939538930543,-2.51029677580698,
13.8013225099955));
#441647=CARTESIAN_POINT('Ctrl Pts',(1.01735639493263,-2.51864593284445,
13.8136962257787));
#441648=CARTESIAN_POINT('Ctrl Pts',(1.0312272073583,-2.50950047563698,13.8168830918626));
#441649=CARTESIAN_POINT('Ctrl Pts',(1.01762250795212,-2.51891835927529,
13.7902140179785));
#441650=CARTESIAN_POINT('Ctrl Pts',(1.02559166208941,-2.52727606732718,
13.802602731458));
#441651=CARTESIAN_POINT('Ctrl Pts',(1.03947723417924,-2.51811260508526,
13.8057746032558));
#441652=CARTESIAN_POINT('Origin',(1.00884928066586,-2.47785717685931,13.8235269408515));
#441653=CARTESIAN_POINT('Ctrl Pts',(0.933702113402283,-2.51582801973993,
13.8235269408515));
#441654=CARTESIAN_POINT('Ctrl Pts',(0.933376362965707,-2.52763100688066,
13.8362179249168));
#441655=CARTESIAN_POINT('Ctrl Pts',(0.916453295848555,-2.52992726544752,
13.8391868794938));
#441656=CARTESIAN_POINT('Ctrl Pts',(0.934000160872677,-2.50502880025961,
13.8400110824519));
#441657=CARTESIAN_POINT('Ctrl Pts',(0.930319292077029,-2.51439752844278,
13.8494522556836));
#441658=CARTESIAN_POINT('Ctrl Pts',(0.917056111996971,-2.51215789865194,
13.85569149686));
#441659=CARTESIAN_POINT('Ctrl Pts',(0.941076652785396,-2.49035498043469,
13.8586819406588));
#441660=CARTESIAN_POINT('Ctrl Pts',(0.937018055750126,-2.49193099875321,
13.868010383617));
#441661=CARTESIAN_POINT('Ctrl Pts',(0.928934735488491,-2.48786248546938,
13.8744918421245));
#441662=CARTESIAN_POINT('Ctrl Pts',(0.970261895489138,-2.47907255577194,
13.8587686893867));
#441663=CARTESIAN_POINT('Ctrl Pts',(0.974284350665984,-2.47751051151197,
13.8680909899357));
#441664=CARTESIAN_POINT('Ctrl Pts',(0.977520521636126,-2.46908296151464,
13.8745789365163));
#441665=CARTESIAN_POINT('Ctrl Pts',(0.985462731547706,-2.48521662242851,
13.8400379222776));
#441666=CARTESIAN_POINT('Ctrl Pts',(0.994474056380701,-2.48969616020182,
13.8494748685452));
#441667=CARTESIAN_POINT('Ctrl Pts',(1.00281461081408,-2.47915119661686,
13.8557104837033));
#441668=CARTESIAN_POINT('Ctrl Pts',(0.992933084934336,-2.49304515609109,
13.8235269408542));
#441669=CARTESIAN_POINT('Ctrl Pts',(1.00108452963812,-2.50158743728711,
13.8362179249195));
#441670=CARTESIAN_POINT('Ctrl Pts',(1.01518422375405,-2.49195096335243,
13.8391868794965));
#441671=CARTESIAN_POINT('Origin',(0.911710487360968,-2.51522107323575,13.8235269408515));
#441672=CARTESIAN_POINT('Ctrl Pts',(0.932715466503348,-2.5515773860639,
13.7902140241683));
#441673=CARTESIAN_POINT('Ctrl Pts',(0.932401321989514,-2.56312121162638,
13.8026027327198));
#441674=CARTESIAN_POINT('Ctrl Pts',(0.915954174459439,-2.5656250627396,
13.8057746032556));
#441675=CARTESIAN_POINT('Ctrl Pts',(0.933044241045491,-2.53966482588052,
13.8013225161808));
#441676=CARTESIAN_POINT('Ctrl Pts',(0.932730414263208,-2.55119684394483,
13.8136962270464));
#441677=CARTESIAN_POINT('Ctrl Pts',(0.916306287753358,-2.55370416795692,
13.8168830918628));
#441678=CARTESIAN_POINT('Ctrl Pts',(0.933373157325311,-2.52774713008525,
13.8124254880875));
#441679=CARTESIAN_POINT('Ctrl Pts',(0.933059788337923,-2.53926226251689,
13.8247886461867));
#441680=CARTESIAN_POINT('Ctrl Pts',(0.916658820164197,-2.54177797417812,
13.8279860620656));
#441681=CARTESIAN_POINT('Ctrl Pts',(0.933702221080902,-2.51582409076846,
13.8235227163066));
#441682=CARTESIAN_POINT('Ctrl Pts',(0.933389459749114,-2.52731690433112,
13.8358800595847));
#441683=CARTESIAN_POINT('Ctrl Pts',(0.917011786918948,-2.529846264619,13.8390832900376));
#441684=CARTESIAN_POINT('Origin',(0.910723732443375,-2.55097438096992,13.7902182540695));
#441685=CARTESIAN_POINT('Ctrl Pts',(0.932150949056334,-2.57203069844641,
13.7382347919292));
#441686=CARTESIAN_POINT('Ctrl Pts',(0.931758621716637,-2.58711592128174,
13.7369371795942));
#441687=CARTESIAN_POINT('Ctrl Pts',(0.917462529821921,-2.59213244732652,
13.7364597369711));
#441688=CARTESIAN_POINT('Ctrl Pts',(0.932098764236209,-2.57392153707748,
13.7595490285574));
#441689=CARTESIAN_POINT('Ctrl Pts',(0.931696071217628,-2.58936665425904,
13.7633824266926));
#441690=CARTESIAN_POINT('Ctrl Pts',(0.917601001692082,-2.59458418963287,
13.7648920890506));
#441691=CARTESIAN_POINT('Ctrl Pts',(0.932364903967904,-2.56427836364779,
13.7803806590111));
#441692=CARTESIAN_POINT('Ctrl Pts',(0.932021985543206,-2.57763797789961,
13.7901039518744));
#441693=CARTESIAN_POINT('Ctrl Pts',(0.916898763834281,-2.58208473026154,
13.7926933640892));
#441694=CARTESIAN_POINT('Ctrl Pts',(0.932827514154394,-2.54751637559775,
13.7936647693663));
#441695=CARTESIAN_POINT('Ctrl Pts',(0.932559096581482,-2.55832846531025,
13.8072068914933));
#441696=CARTESIAN_POINT('Ctrl Pts',(0.915637243948269,-2.56040094529968,
13.8104111085397));
#441697=CARTESIAN_POINT('Origin',(0.910151905565162,-2.57169350988723,13.7435492065112));
#441698=CARTESIAN_POINT('Origin',(0.910151905565162,-2.57169350988723,14.));
#441699=CARTESIAN_POINT('Origin',(0.910151905565162,-2.57169350988723,12.5369868989719));
#441700=CARTESIAN_POINT('Ctrl Pts',(0.948306224028831,-2.57443505961824,
12.506462012331));
#441701=CARTESIAN_POINT('Ctrl Pts',(0.950566304539922,-2.58057066261006,
12.4999388158272));
#441702=CARTESIAN_POINT('Ctrl Pts',(0.950539564823561,-2.58049807038031,
12.4907030323752));
#441703=CARTESIAN_POINT('Ctrl Pts',(0.936815419454617,-2.58108261506304,
12.5042014951932));
#441704=CARTESIAN_POINT('Ctrl Pts',(0.933750333536626,-2.58673472488428,
12.4980716682127));
#441705=CARTESIAN_POINT('Ctrl Pts',(0.927360673278842,-2.58903642143593,
12.4907355092744));
#441706=CARTESIAN_POINT('Ctrl Pts',(0.932010533866908,-2.57744410221653,
12.5218047446509));
#441707=CARTESIAN_POINT('Ctrl Pts',(0.928404372659909,-2.5886919674489,
12.5216906929434));
#441708=CARTESIAN_POINT('Ctrl Pts',(0.917277340433921,-2.59250771222178,
12.5161988840775));
#441709=CARTESIAN_POINT('Ctrl Pts',(0.932144557920413,-2.57226205397613,
12.5369868989719));
#441710=CARTESIAN_POINT('Ctrl Pts',(0.931748388901365,-2.58758682417437,
12.5369868989719));
#441711=CARTESIAN_POINT('Ctrl Pts',(0.917234684417284,-2.59252219788557,
12.5369868989719));
#441712=CARTESIAN_POINT('Origin',(1.84953258308758E-31,-9.96028411833584E-31,
12.5));
#441713=CARTESIAN_POINT('Origin',(1.13565863606157,-2.43135141923565,12.5));
#441714=CARTESIAN_POINT('',(1.13565863606157,-2.43135141923565,12.5893111709658));
#441715=CARTESIAN_POINT('',(1.13565863606157,-2.43135141923565,13.8235269408515));
#441716=CARTESIAN_POINT('',(1.13565863606157,-2.43135141923565,12.5));
#441717=CARTESIAN_POINT('',(1.13758939098741,-2.46706619047414,13.7902182540695));
#441718=CARTESIAN_POINT('',(1.13565863606157,-2.43135141923565,13.8235269408515));
#441719=CARTESIAN_POINT('',(1.13870826816973,-2.48776298739835,13.7435492065112));
#441720=CARTESIAN_POINT('Origin',(1.13502750230952,-2.41967078150723,13.7445212918712));
#441721=CARTESIAN_POINT('',(1.13870826816973,-2.48776298739835,12.5369868989719));
#441722=CARTESIAN_POINT('',(1.13870826816973,-2.48776298739835,12.5));
#441723=CARTESIAN_POINT('Ctrl Pts',(1.13870826816973,-2.48776298739835,
12.5369868989719));
#441724=CARTESIAN_POINT('Ctrl Pts',(1.13769246553907,-2.46897284573305,
12.5544431401645));
#441725=CARTESIAN_POINT('Ctrl Pts',(1.13667593637937,-2.45016926485901,
12.5718848856037));
#441726=CARTESIAN_POINT('Ctrl Pts',(1.13565863606157,-2.43135141923565,
12.5893111709658));
#441727=CARTESIAN_POINT('Origin',(1.39827000902105,-2.58663242216022,12.5));
#441728=CARTESIAN_POINT('',(1.23503843197073,-2.44137282548621,13.7435492065112));
#441729=CARTESIAN_POINT('',(1.21955463306185,-2.42759381026668,13.7902182540695));
#441730=CARTESIAN_POINT('Origin',(1.17886588566605,-2.39138493976081,13.7418732680438));
#441731=CARTESIAN_POINT('',(1.19283550652461,-2.40381648963781,13.8235269408515));
#441732=CARTESIAN_POINT('',(1.21955463306185,-2.42759381026668,13.7902182540695));
#441733=CARTESIAN_POINT('',(1.19283550652461,-2.40381648963781,12.5893111709658));
#441734=CARTESIAN_POINT('',(1.19283550652461,-2.40381648963781,12.5));
#441735=CARTESIAN_POINT('',(1.23503843197073,-2.44137282548621,12.5369868989719));
#441736=CARTESIAN_POINT('Ctrl Pts',(1.19283550652461,-2.40381648963781,
12.5893111709658));
#441737=CARTESIAN_POINT('Ctrl Pts',(1.2069136142916,-2.4163445818925,12.5718848856037));
#441738=CARTESIAN_POINT('Ctrl Pts',(1.22098105023769,-2.42886317730579,
12.5544431401645));
#441739=CARTESIAN_POINT('Ctrl Pts',(1.23503843197073,-2.44137282548621,
12.5369868989719));
#441740=CARTESIAN_POINT('',(1.23503843197073,-2.44137282548621,12.5));
#441741=CARTESIAN_POINT('Origin',(1.16998351495931,-2.42949580244986,12.5));
#441742=CARTESIAN_POINT('',(1.15406831628268,-2.39902784184759,13.8587068136939));
#441743=CARTESIAN_POINT('Ctrl Pts',(1.19283550652889,-2.40381648963277,
13.8235269408542));
#441744=CARTESIAN_POINT('Ctrl Pts',(1.1915264791287,-2.40265158762287,13.8262006681044));
#441745=CARTESIAN_POINT('Ctrl Pts',(1.19007138150615,-2.40158926990163,
13.8288634856214));
#441746=CARTESIAN_POINT('Ctrl Pts',(1.18848189959866,-2.40062311424865,
13.8314912288862));
#441747=CARTESIAN_POINT('Ctrl Pts',(1.18684330769949,-2.39962710742477,
13.8342001611531));
#441748=CARTESIAN_POINT('Ctrl Pts',(1.18506033714425,-2.39873176576222,
13.8368750301949));
#441749=CARTESIAN_POINT('Ctrl Pts',(1.1831078388226,-2.3979546046324,13.8394886372969));
#441750=CARTESIAN_POINT('Ctrl Pts',(1.18295704264112,-2.39789458259322,
13.8396904925131));
#441751=CARTESIAN_POINT('Ctrl Pts',(1.18280522363857,-2.39783528434211,
13.8398919674349));
#441752=CARTESIAN_POINT('Ctrl Pts',(1.18265236510737,-2.39777672818192,
13.8400930404591));
#441753=CARTESIAN_POINT('Ctrl Pts',(1.18027072635307,-2.39686438381137,
13.8432258934518));
#441754=CARTESIAN_POINT('Ctrl Pts',(1.17764928961486,-2.39613579180582,
13.8462331177034));
#441755=CARTESIAN_POINT('Ctrl Pts',(1.17484771977747,-2.3957076581236,13.8489036603661));
#441756=CARTESIAN_POINT('Ctrl Pts',(1.17393101352317,-2.39556756780034,
13.8497774930041));
#441757=CARTESIAN_POINT('Ctrl Pts',(1.17299520690167,-2.39545981371141,
13.85061494757));
#441758=CARTESIAN_POINT('Ctrl Pts',(1.17204292942797,-2.39538895230675,
13.8514076489583));
#441759=CARTESIAN_POINT('Ctrl Pts',(1.17002872523211,-2.39523907021616,
13.8530843267192));
#441760=CARTESIAN_POINT('Ctrl Pts',(1.16774276579092,-2.39524246733169,
13.8546805203176));
#441761=CARTESIAN_POINT('Ctrl Pts',(1.16531793013634,-2.39553539204199,
13.8559412814274));
#441762=CARTESIAN_POINT('Ctrl Pts',(1.16499340848649,-2.395574594868,13.8561100121513));
#441763=CARTESIAN_POINT('Ctrl Pts',(1.16466644180727,-2.39561891939493,
13.8562727473908));
#441764=CARTESIAN_POINT('Ctrl Pts',(1.16433738223972,-2.39566862423088,
13.8564289040185));
#441765=CARTESIAN_POINT('Ctrl Pts',(1.16284510085487,-2.39589403509486,
13.8571370725437));
#441766=CARTESIAN_POINT('Ctrl Pts',(1.16128388673762,-2.39623631103585,
13.8577210840553));
#441767=CARTESIAN_POINT('Ctrl Pts',(1.15972070946708,-2.39671081491259,
13.8581177131616));
#441768=CARTESIAN_POINT('Ctrl Pts',(1.15928046494476,-2.3968444515362,13.8582294175695));
#441769=CARTESIAN_POINT('Ctrl Pts',(1.15884004741686,-2.39698839943994,
13.8583265086086));
#441770=CARTESIAN_POINT('Ctrl Pts',(1.15840088406123,-2.39714256764798,
13.8584082369006));
#441771=CARTESIAN_POINT('Ctrl Pts',(1.15776992408551,-2.39736406602108,
13.8585256585398));
#441772=CARTESIAN_POINT('Ctrl Pts',(1.15713381575414,-2.39760971996782,
13.8586122832068));
#441773=CARTESIAN_POINT('Ctrl Pts',(1.15650936780451,-2.39787388477401,
13.8586682984299));
#441774=CARTESIAN_POINT('Ctrl Pts',(1.15600987134434,-2.39808519043314,
13.8587131050557));
#441775=CARTESIAN_POINT('Ctrl Pts',(1.15551222738072,-2.39831045802565,
13.8587357943552));
#441776=CARTESIAN_POINT('Ctrl Pts',(1.15501658563067,-2.39855017569664,
13.8587355499465));
#441777=CARTESIAN_POINT('Ctrl Pts',(1.15469624055099,-2.39870511094251,
13.8587353919793));
#441778=CARTESIAN_POINT('Ctrl Pts',(1.15438017919576,-2.39886437222156,
13.8587257282814));
#441779=CARTESIAN_POINT('Ctrl Pts',(1.15406831628268,-2.39902784184759,
13.8587068136939));
#441780=CARTESIAN_POINT('Ctrl Pts',(1.15406831628268,-2.39902784184759,
13.8587068136939));
#441781=CARTESIAN_POINT('Ctrl Pts',(1.1530426161628,-2.39956548453605,13.8586446046466));
#441782=CARTESIAN_POINT('Ctrl Pts',(1.15206227460148,-2.40014859383079,
13.858482427929));
#441783=CARTESIAN_POINT('Ctrl Pts',(1.15112474840317,-2.40077349303306,
13.8582284286032));
#441784=CARTESIAN_POINT('Ctrl Pts',(1.15016295558127,-2.4014145669233,13.8579678548414));
#441785=CARTESIAN_POINT('Ctrl Pts',(1.14924472334194,-2.40210246252492,
13.857615680862));
#441786=CARTESIAN_POINT('Ctrl Pts',(1.14840044271675,-2.40280230517398,
13.8571944833187));
#441787=CARTESIAN_POINT('Ctrl Pts',(1.14629345407065,-2.40454883407875,
13.8561433417727));
#441788=CARTESIAN_POINT('Ctrl Pts',(1.14454541968629,-2.40644777478311,
13.8546163505474));
#441789=CARTESIAN_POINT('Ctrl Pts',(1.14313369126025,-2.40829359159431,
13.8528973491086));
#441790=CARTESIAN_POINT('Ctrl Pts',(1.14287578930493,-2.40863079509322,
13.8525833129072));
#441791=CARTESIAN_POINT('Ctrl Pts',(1.14262897196776,-2.40896620134861,
13.8522628768812));
#441792=CARTESIAN_POINT('Ctrl Pts',(1.14239292237302,-2.40929855438679,
13.851937733538));
#441793=CARTESIAN_POINT('Ctrl Pts',(1.14095140024834,-2.41132818827904,
13.8499521282529));
#441794=CARTESIAN_POINT('Ctrl Pts',(1.13977151244923,-2.41344802518087,
13.847639871647));
#441795=CARTESIAN_POINT('Ctrl Pts',(1.13884507007223,-2.41550758173481,
13.8452109780794));
#441796=CARTESIAN_POINT('Ctrl Pts',(1.13842824447041,-2.41643421885913,
13.8441181685877));
#441797=CARTESIAN_POINT('Ctrl Pts',(1.13806200744529,-2.41734860361652,
13.8430021611332));
#441798=CARTESIAN_POINT('Ctrl Pts',(1.13774240329718,-2.41823783324536,
13.8418824960098));
#441799=CARTESIAN_POINT('Ctrl Pts',(1.13698924796077,-2.42033332557299,
13.8392439765549));
#441800=CARTESIAN_POINT('Ctrl Pts',(1.13645549152385,-2.42238802025298,
13.8364981347964));
#441801=CARTESIAN_POINT('Ctrl Pts',(1.13610660118662,-2.42439874712789,
13.8336931113419));
#441802=CARTESIAN_POINT('Ctrl Pts',(1.13576680415474,-2.42635706741108,
13.8309611966328));
#441803=CARTESIAN_POINT('Ctrl Pts',(1.13560257789555,-2.42827574082591,
13.8281701127186));
#441804=CARTESIAN_POINT('Ctrl Pts',(1.13562053230287,-2.43014400976238,
13.8253580685121));
#441805=CARTESIAN_POINT('Ctrl Pts',(1.13562442483775,-2.43054905248411,
13.8247484142933));
#441806=CARTESIAN_POINT('Ctrl Pts',(1.13563702319352,-2.43095162813426,
13.8241378483365));
#441807=CARTESIAN_POINT('Ctrl Pts',(1.13565863606157,-2.43135141923565,
13.8235269408515));
#441808=CARTESIAN_POINT('',(1.15517944202808,-2.39847270543601,12.5969504640361));
#441809=CARTESIAN_POINT('Origin',(1.16999769376632,-2.42952569633287,12.584524458991));
#441810=CARTESIAN_POINT('Origin',(1.16999769376632,-2.42952569633287,12.584524458991));
#441811=CARTESIAN_POINT('Ctrl Pts',(1.19283550652461,-2.40381648963781,
12.5893111709658));
#441812=CARTESIAN_POINT('Ctrl Pts',(1.18436864725009,-2.3962818411002,12.5770542771492));
#441813=CARTESIAN_POINT('Ctrl Pts',(1.17140116758586,-2.4062642328984,12.5737548217797));
#441814=CARTESIAN_POINT('Ctrl Pts',(1.21134968619555,-2.42029223728633,
12.5663937883685));
#441815=CARTESIAN_POINT('Ctrl Pts',(1.20287202626619,-2.41274797725812,
12.5540940315304));
#441816=CARTESIAN_POINT('Ctrl Pts',(1.18986632182064,-2.42276384702507,
12.5508374392248));
#441817=CARTESIAN_POINT('Ctrl Pts',(1.22984518528617,-2.43675136110744,
12.5434499600944));
#441818=CARTESIAN_POINT('Ctrl Pts',(1.22133996146542,-2.42918257200328,
12.5311293540533));
#441819=CARTESIAN_POINT('Ctrl Pts',(1.20831422135804,-2.43924646087483,
12.5278936106989));
#441820=CARTESIAN_POINT('Ctrl Pts',(1.24832346707192,-2.45319516326835,
12.5204817579905));
#441821=CARTESIAN_POINT('Ctrl Pts',(1.23977614820573,-2.44558891383069,
12.5081597038247));
#441822=CARTESIAN_POINT('Ctrl Pts',(1.22674621653173,-2.45571338544483,
12.5049254088044));
#441823=CARTESIAN_POINT('Ctrl Pts',(1.23503843197073,-2.44137282548621,
12.5369868989719));
#441824=CARTESIAN_POINT('Ctrl Pts',(1.23573429812772,-2.44199207621274,
12.5342545179733));
#441825=CARTESIAN_POINT('Ctrl Pts',(1.23631547168388,-2.44267625046758,
12.5314872231885));
#441826=CARTESIAN_POINT('Ctrl Pts',(1.23670660961763,-2.44342299823417,
12.5287124745062));
#441827=CARTESIAN_POINT('Ctrl Pts',(1.23705935722064,-2.44409645243533,
12.5262100684184));
#441828=CARTESIAN_POINT('Ctrl Pts',(1.23725631536522,-2.4448205766146,12.5237004536639));
#441829=CARTESIAN_POINT('Ctrl Pts',(1.23723689927158,-2.44562520297928,
12.5212220730815));
#441830=CARTESIAN_POINT('Ctrl Pts',(1.23722203457226,-2.44624121406717,
12.5193246583486));
#441831=CARTESIAN_POINT('Ctrl Pts',(1.2370795359662,-2.44691175621377,12.517417831369));
#441832=CARTESIAN_POINT('Ctrl Pts',(1.23671217730368,-2.44763578129384,
12.5155812248348));
#441833=CARTESIAN_POINT('Ctrl Pts',(1.23655568053889,-2.4479442198696,12.5147988205793));
#441834=CARTESIAN_POINT('Ctrl Pts',(1.23635846421814,-2.44826280301348,
12.5140295443047));
#441835=CARTESIAN_POINT('Ctrl Pts',(1.23611403595814,-2.44859331410036,
12.5132817086137));
#441836=CARTESIAN_POINT('Ctrl Pts',(1.23574412685214,-2.44909349791982,
12.5121499604604));
#441837=CARTESIAN_POINT('Ctrl Pts',(1.23525235153957,-2.4496275486279,12.5110494206568));
#441838=CARTESIAN_POINT('Ctrl Pts',(1.23460465430036,-2.45018039616567,
12.5100666561695));
#441839=CARTESIAN_POINT('Ctrl Pts',(1.23423274803712,-2.45049783994877,
12.5095023550641));
#441840=CARTESIAN_POINT('Ctrl Pts',(1.2338047130377,-2.45082465239455,12.5089719619137));
#441841=CARTESIAN_POINT('Ctrl Pts',(1.23332469638038,-2.45114963131024,
12.5085043804652));
#441842=CARTESIAN_POINT('Ctrl Pts',(1.23262225452895,-2.45162519562188,
12.5078201359221));
#441843=CARTESIAN_POINT('Ctrl Pts',(1.23178744622585,-2.45210962632866,
12.5072563000949));
#441844=CARTESIAN_POINT('Ctrl Pts',(1.23087261002689,-2.4525627637421,12.5068768744332));
#441845=CARTESIAN_POINT('Ctrl Pts',(1.2302129501499,-2.45288950701127,12.5066032824114));
#441846=CARTESIAN_POINT('Ctrl Pts',(1.22950011797268,-2.45320577384133,
12.5064197834844));
#441847=CARTESIAN_POINT('Ctrl Pts',(1.22877496818874,-2.45349626581735,
12.5063282718343));
#441848=CARTESIAN_POINT('Ctrl Pts',(1.22771647400488,-2.4539202941683,12.5061946931565));
#441849=CARTESIAN_POINT('Ctrl Pts',(1.22660950568368,-2.45429945325867,
12.5062515701262));
#441850=CARTESIAN_POINT('Ctrl Pts',(1.22552777474128,-2.45462484192931,
12.5064436508398));
#441851=CARTESIAN_POINT('',(1.17140116758586,-2.4062642328984,12.5737548217797));
#441852=CARTESIAN_POINT('Origin',(1.17821023192281,-2.42025124983752,12.5893111709658));
#441853=CARTESIAN_POINT('Ctrl Pts',(1.22552777474128,-2.4546248419293,12.5064436508398));
#441854=CARTESIAN_POINT('Ctrl Pts',(1.21751531053644,-2.44746657362494,
12.5164271754438));
#441855=CARTESIAN_POINT('Ctrl Pts',(1.20949980939339,-2.44030531197305,
12.5264061185523));
#441856=CARTESIAN_POINT('Ctrl Pts',(1.20148116372314,-2.4331409522563,12.536380305637));
#441857=CARTESIAN_POINT('Ctrl Pts',(1.19145948299191,-2.42418695569907,
12.5488460165097));
#441858=CARTESIAN_POINT('Ctrl Pts',(1.18143288758693,-2.41522811732307,
12.5613043021964));
#441859=CARTESIAN_POINT('Ctrl Pts',(1.17140116758586,-2.4062642328984,12.5737548217797));
#441860=CARTESIAN_POINT('Ctrl Pts',(1.13565863606157,-2.43135141923565,
12.5893111709658));
#441861=CARTESIAN_POINT('Ctrl Pts',(1.13504681103698,-2.42003398557342,
12.5770542771492));
#441862=CARTESIAN_POINT('Ctrl Pts',(1.1509364505416,-2.416119521208,12.5737548217797));
#441863=CARTESIAN_POINT('Ctrl Pts',(1.135087808635,-2.42079235206263,12.5928319619712));
#441864=CARTESIAN_POINT('Ctrl Pts',(1.13792961703663,-2.41301047944868,
12.5821634970843));
#441865=CARTESIAN_POINT('Ctrl Pts',(1.15071908683469,-2.41227361814261,
12.5773203894503));
#441866=CARTESIAN_POINT('Ctrl Pts',(1.14124245786915,-2.40521337930624,
12.5969440695591));
#441867=CARTESIAN_POINT('Ctrl Pts',(1.14485617827555,-2.40345282048125,
12.5878292599214));
#441868=CARTESIAN_POINT('Ctrl Pts',(1.15291463227777,-2.40672170610216,
12.5813877129824));
#441869=CARTESIAN_POINT('Ctrl Pts',(1.16878594562417,-2.39188928354591,
12.596957478804));
#441870=CARTESIAN_POINT('Ctrl Pts',(1.16519896668808,-2.39363690343048,
12.5878468778671));
#441871=CARTESIAN_POINT('Ctrl Pts',(1.16277542598974,-2.40195819734556,
12.5814011370086));
#441872=CARTESIAN_POINT('Ctrl Pts',(1.18492453039319,-2.39677652088344,
12.5928371701607));
#441873=CARTESIAN_POINT('Ctrl Pts',(1.17707228826797,-2.39415404889869,
12.5821692192952));
#441874=CARTESIAN_POINT('Ctrl Pts',(1.16852082998896,-2.40368800837367,
12.5773318885715));
#441875=CARTESIAN_POINT('Ctrl Pts',(1.19283550652464,-2.40381648963776,
12.5893111709658));
#441876=CARTESIAN_POINT('Ctrl Pts',(1.18436864725012,-2.39628184110016,
12.5770542771492));
#441877=CARTESIAN_POINT('Ctrl Pts',(1.17140116758589,-2.40626423289836,
12.5737548217797));
#441878=CARTESIAN_POINT('',(1.1509364505416,-2.416119521208,12.5737548217797));
#441879=CARTESIAN_POINT('Origin',(1.15762655855612,-2.43016382449275,12.5893111709658));
#441880=CARTESIAN_POINT('Ctrl Pts',(1.17140116758589,-2.40626423289836,
12.5737548217797));
#441881=CARTESIAN_POINT('Ctrl Pts',(1.1706746487686,-2.40557395031917,12.5746934679442));
#441882=CARTESIAN_POINT('Ctrl Pts',(1.16974453062184,-2.40494290699951,
12.5756680099006));
#441883=CARTESIAN_POINT('Ctrl Pts',(1.16871850375878,-2.40444014209991,
12.5765688348656));
#441884=CARTESIAN_POINT('Ctrl Pts',(1.16844687450528,-2.40430704065853,
12.5768073183026));
#441885=CARTESIAN_POINT('Ctrl Pts',(1.16816868922902,-2.40418273344928,
12.5770407398754));
#441886=CARTESIAN_POINT('Ctrl Pts',(1.167886189766,-2.40406799376,12.5772674179684));
#441887=CARTESIAN_POINT('Ctrl Pts',(1.16672688836083,-2.40359713310213,
12.5781976435658));
#441888=CARTESIAN_POINT('Ctrl Pts',(1.16542484328481,-2.40327110227111,
12.5790594849312));
#441889=CARTESIAN_POINT('Ctrl Pts',(1.16405624123446,-2.40315875837296,
12.5797571720116));
#441890=CARTESIAN_POINT('Ctrl Pts',(1.16316454778811,-2.4030855622838,12.580211740231));
#441891=CARTESIAN_POINT('Ctrl Pts',(1.16220254220457,-2.40311845966298,
12.5806009430798));
#441892=CARTESIAN_POINT('Ctrl Pts',(1.16123855099109,-2.40327284102408,
12.5808812374708));
#441893=CARTESIAN_POINT('Ctrl Pts',(1.16041016273796,-2.40340550582875,
12.5811221033394));
#441894=CARTESIAN_POINT('Ctrl Pts',(1.15956336692619,-2.40363070930533,
12.581287365893));
#441895=CARTESIAN_POINT('Ctrl Pts',(1.15874810105404,-2.40394379849578,
12.581359338449));
#441896=CARTESIAN_POINT('Ctrl Pts',(1.15863479593241,-2.4039873114282,12.5813693411482));
#441897=CARTESIAN_POINT('Ctrl Pts',(1.15852206095077,-2.40403247634902,
12.5813775999465));
#441898=CARTESIAN_POINT('Ctrl Pts',(1.1584099895221,-2.40407923481949,12.5813841266931));
#441899=CARTESIAN_POINT('Ctrl Pts',(1.1582198467886,-2.40415856621996,12.5813952001081));
#441900=CARTESIAN_POINT('Ctrl Pts',(1.15803057506862,-2.40424357793756,
12.5814007534795));
#441901=CARTESIAN_POINT('Ctrl Pts',(1.15784233759719,-2.40433441284383,
12.5814005856065));
#441902=CARTESIAN_POINT('Ctrl Pts',(1.15698066004906,-2.40475021953056,
12.5813998171494));
#441903=CARTESIAN_POINT('Ctrl Pts',(1.15620004328975,-2.40525901524178,
12.58127954464));
#441904=CARTESIAN_POINT('Ctrl Pts',(1.1554887621719,-2.40583312261721,12.5810700125799));
#441905=CARTESIAN_POINT('Ctrl Pts',(1.15462961556737,-2.40652657895936,
12.5808169217085));
#441906=CARTESIAN_POINT('Ctrl Pts',(1.15388206277118,-2.40732841009892,
12.5804173076348));
#441907=CARTESIAN_POINT('Ctrl Pts',(1.15329256989121,-2.40815058618232,
12.5799304713245));
#441908=CARTESIAN_POINT('Ctrl Pts',(1.15256200250352,-2.40916952136183,
12.5793271277669));
#441909=CARTESIAN_POINT('Ctrl Pts',(1.1520027122323,-2.4102641478739,12.5785808224116));
#441910=CARTESIAN_POINT('Ctrl Pts',(1.15161003050752,-2.41137389420799,
12.5777485681082));
#441911=CARTESIAN_POINT('Ctrl Pts',(1.15102489171609,-2.41302753782757,
12.576508418016));
#441912=CARTESIAN_POINT('Ctrl Pts',(1.15080814330876,-2.41469853742023,
12.5750928681475));
#441913=CARTESIAN_POINT('Ctrl Pts',(1.1509364505416,-2.416119521208,12.5737548217797));
#441914=CARTESIAN_POINT('Ctrl Pts',(1.1509364505416,-2.416119521208,12.5737548217797));
#441915=CARTESIAN_POINT('Ctrl Pts',(1.13504681103698,-2.42003398557342,
12.5770542771492));
#441916=CARTESIAN_POINT('Ctrl Pts',(1.13565863606157,-2.43135141923565,
12.5893111709658));
#441917=CARTESIAN_POINT('Ctrl Pts',(1.15232332457213,-2.44083978687392,
12.5508408821982));
#441918=CARTESIAN_POINT('Ctrl Pts',(1.13638368550749,-2.44476325869343,
12.55409748406));
#441919=CARTESIAN_POINT('Ctrl Pts',(1.13699629106412,-2.45609513050247,
12.5663972313419));
#441920=CARTESIAN_POINT('Ctrl Pts',(1.15370766614038,-2.46553597002463,
12.52790050457));
#441921=CARTESIAN_POINT('Ctrl Pts',(1.13771799954522,-2.46944516936941,
12.5311362602938));
#441922=CARTESIAN_POINT('Ctrl Pts',(1.13833259659258,-2.48081387943054,
12.5434568539655));
#441923=CARTESIAN_POINT('Ctrl Pts',(1.1550896582248,-2.49020994295635,12.5049357605811));
#441924=CARTESIAN_POINT('Ctrl Pts',(1.13905002006211,-2.49408465489395,
12.5081700652078));
#441925=CARTESIAN_POINT('Ctrl Pts',(1.13966765833803,-2.50550962107533,
12.5204921097672));
#441926=CARTESIAN_POINT('Ctrl Pts',(1.15499890962265,-2.48858975326341,
12.5064436508395));
#441927=CARTESIAN_POINT('Ctrl Pts',(1.15399558653521,-2.48928415269658,
12.5062361689309));
#441928=CARTESIAN_POINT('Ctrl Pts',(1.15292260189464,-2.4899634873575,12.5061871075061));
#441929=CARTESIAN_POINT('Ctrl Pts',(1.15184870913824,-2.49056162696401,
12.5063648335164));
#441930=CARTESIAN_POINT('Ctrl Pts',(1.15136088080783,-2.49083333886806,
12.5064455676329));
#441931=CARTESIAN_POINT('Ctrl Pts',(1.15086595368983,-2.49109189321737,
12.506574497099));
#441932=CARTESIAN_POINT('Ctrl Pts',(1.15038466215084,-2.49132527247727,
12.5067492519495));
#441933=CARTESIAN_POINT('Ctrl Pts',(1.1494174881209,-2.49179425715915,12.5071004286051));
#441934=CARTESIAN_POINT('Ctrl Pts',(1.14846946575685,-2.49217809432416,
12.5076537929612));
#441935=CARTESIAN_POINT('Ctrl Pts',(1.14761529875447,-2.4924567420916,12.5083435010503));
#441936=CARTESIAN_POINT('Ctrl Pts',(1.14756152383705,-2.49247428463379,
12.5083869222963));
#441937=CARTESIAN_POINT('Ctrl Pts',(1.1475081113454,-2.49249140082923,12.5084308732336));
#441938=CARTESIAN_POINT('Ctrl Pts',(1.14745507574704,-2.49250808211731,
12.5084753333615));
#441939=CARTESIAN_POINT('Ctrl Pts',(1.14702966024818,-2.4926418880648,12.508831962269));
#441940=CARTESIAN_POINT('Ctrl Pts',(1.14662024509582,-2.4927516585159,12.509227847131));
#441941=CARTESIAN_POINT('Ctrl Pts',(1.14623972946254,-2.49283683395425,
12.5096423454524));
#441942=CARTESIAN_POINT('Ctrl Pts',(1.14504736187699,-2.49310373608097,
12.5109411997424));
#441943=CARTESIAN_POINT('Ctrl Pts',(1.14406753767241,-2.49315498662039,
12.5124831113042));
#441944=CARTESIAN_POINT('Ctrl Pts',(1.14326681185949,-2.493079114043,12.5140723025008));
#441945=CARTESIAN_POINT('Ctrl Pts',(1.14319178297381,-2.4930720046994,12.5142212114565));
#441946=CARTESIAN_POINT('Ctrl Pts',(1.14311830702035,-2.49306380147871,
12.5143705582413));
#441947=CARTESIAN_POINT('Ctrl Pts',(1.1430463464893,-2.49305459094164,12.5145201959299));
#441948=CARTESIAN_POINT('Ctrl Pts',(1.14212190632999,-2.49293626787997,
12.5164425148273));
#441949=CARTESIAN_POINT('Ctrl Pts',(1.14141452178073,-2.4926583022727,12.518463520594));
#441950=CARTESIAN_POINT('Ctrl Pts',(1.14085307427549,-2.49227619302178,
12.5205025929157));
#441951=CARTESIAN_POINT('Ctrl Pts',(1.14052741246874,-2.49205455451085,
12.5216853356836));
#441952=CARTESIAN_POINT('Ctrl Pts',(1.1402511668049,-2.49179867741584,12.5228750347131));
#441953=CARTESIAN_POINT('Ctrl Pts',(1.1400143670888,-2.49152384338772,12.5240609649613));
#441954=CARTESIAN_POINT('Ctrl Pts',(1.13943315488952,-2.49084927801005,
12.5269717671327));
#441955=CARTESIAN_POINT('Ctrl Pts',(1.13908109514514,-2.4900347395367,12.5299036066169));
#441956=CARTESIAN_POINT('Ctrl Pts',(1.13888520536176,-2.4891269513902,12.5328133004019));
#441957=CARTESIAN_POINT('Ctrl Pts',(1.13879116685943,-2.48869116022097,
12.5342101228452));
#441958=CARTESIAN_POINT('Ctrl Pts',(1.13873374826657,-2.48823431231207,
12.5356023438238));
#441959=CARTESIAN_POINT('Ctrl Pts',(1.13870826816973,-2.48776298739835,
12.5369868989719));
#441960=CARTESIAN_POINT('Origin',(1.8214655920365,-15.2154335410399,-1.24073622122997));
#441961=CARTESIAN_POINT('Ctrl Pts',(1.23500723661298,-2.4413450116302,12.5369868989719));
#441962=CARTESIAN_POINT('Ctrl Pts',(1.24644656774961,-2.45156386708624,
12.5369868989719));
#441963=CARTESIAN_POINT('Ctrl Pts',(1.25999060240651,-2.44436369841476,
12.5369868989719));
#441964=CARTESIAN_POINT('Ctrl Pts',(1.23887422203735,-2.44479933505252,
12.5218025310015));
#441965=CARTESIAN_POINT('Ctrl Pts',(1.24954275891247,-2.44988246250011,
12.5216901060418));
#441966=CARTESIAN_POINT('Ctrl Pts',(1.2599493234416,-2.444385661477,12.5161920673677));
#441967=CARTESIAN_POINT('Ctrl Pts',(1.23823476680908,-2.45079326266352,
12.5042015548895));
#441968=CARTESIAN_POINT('Ctrl Pts',(1.24445480582807,-2.45243291494978,
12.4980677368513));
#441969=CARTESIAN_POINT('Ctrl Pts',(1.25051277374003,-2.4493520377206,12.4907278922778));
#441970=CARTESIAN_POINT('Ctrl Pts',(1.22551884038576,-2.45460694722071,
12.506463626192));
#441971=CARTESIAN_POINT('Ctrl Pts',(1.22844143711359,-2.46046065260301,
12.4999376786891));
#441972=CARTESIAN_POINT('Ctrl Pts',(1.22840574184401,-2.46038915810304,
12.4906970594712));
#441973=CARTESIAN_POINT('Origin',(1.24966370657253,-2.4249380652865,12.5369868989719));
#441974=CARTESIAN_POINT('Origin',(1.24966370657253,-2.4249380652865,14.));
#441975=CARTESIAN_POINT('Origin',(1.24966370657253,-2.4249380652865,13.7435492065112));
#441976=CARTESIAN_POINT('Ctrl Pts',(1.21654179677687,-2.42491265430238,
13.793642941384));
#441977=CARTESIAN_POINT('Ctrl Pts',(1.22460084957725,-2.43212083624836,
13.8071662555867));
#441978=CARTESIAN_POINT('Ctrl Pts',(1.23769698055489,-2.42123457256189,
13.8103758687955));
#441979=CARTESIAN_POINT('Ctrl Pts',(1.22895834746436,-2.43596213276286,
13.7804579775006));
#441980=CARTESIAN_POINT('Ctrl Pts',(1.23890925070369,-2.44484881923482,
13.7901904343351));
#441981=CARTESIAN_POINT('Ctrl Pts',(1.25249575756948,-2.43686992486593,
13.7927914348262));
#441982=CARTESIAN_POINT('Ctrl Pts',(1.2362684381667,-2.44246737654277,13.7597120340895));
#441983=CARTESIAN_POINT('Ctrl Pts',(1.24778825257543,-2.45274750134554,
13.7635825532445));
#441984=CARTESIAN_POINT('Ctrl Pts',(1.26124114463959,-2.44607250237516,
13.7651073818884));
#441985=CARTESIAN_POINT('Ctrl Pts',(1.23483695502569,-2.44119350085692,
13.7381884353898));
#441986=CARTESIAN_POINT('Ctrl Pts',(1.24608652825463,-2.45123367081529,
13.7368803041982));
#441987=CARTESIAN_POINT('Ctrl Pts',(1.25952889624334,-2.4442700237841,13.7363986145813));
#441988=CARTESIAN_POINT('Origin',(1.23417990766365,-2.41115905006696,13.7902182540695));
#441989=CARTESIAN_POINT('Ctrl Pts',(1.1928325665529,-2.40381387234437,13.8235227101244));
#441990=CARTESIAN_POINT('Ctrl Pts',(1.20141832947106,-2.41146026779797,
13.8358800583119));
#441991=CARTESIAN_POINT('Ctrl Pts',(1.21448177232262,-2.40126357667189,
13.8390832900376));
#441992=CARTESIAN_POINT('Ctrl Pts',(1.20174288048452,-2.41174315068067,
13.8124254819052));
#441993=CARTESIAN_POINT('Ctrl Pts',(1.21034531701755,-2.41940439511813,
13.8247886449158));
#441994=CARTESIAN_POINT('Ctrl Pts',(1.22341477869201,-2.40918138417994,
13.8279860620657));
#441995=CARTESIAN_POINT('Ctrl Pts',(1.21064920110331,-2.4196688753724,13.8013225099955));
#441996=CARTESIAN_POINT('Ctrl Pts',(1.21926425094939,-2.42734135541361,
13.8136962257787));
#441997=CARTESIAN_POINT('Ctrl Pts',(1.23234346972625,-2.4170957289775,13.8168830918626));
#441998=CARTESIAN_POINT('Ctrl Pts',(1.21955168378293,-2.42759118468639,
13.7902140179785));
#441999=CARTESIAN_POINT('Ctrl Pts',(1.22817555201263,-2.43527152311001,
13.802602731458));
#442000=CARTESIAN_POINT('Ctrl Pts',(1.24126801376467,-2.42500674850007,
13.8057746032558));
#442001=CARTESIAN_POINT('Origin',(1.2074607811264,-2.38738172943809,13.8235269408515));
#442002=CARTESIAN_POINT('Ctrl Pts',(1.13565863606157,-2.43135141923565,
13.8235269408515));
#442003=CARTESIAN_POINT('Ctrl Pts',(1.13629602255825,-2.44314168459504,
13.8362179249168));
#442004=CARTESIAN_POINT('Ctrl Pts',(1.11961643194152,-2.44680968962709,
13.8391868794938));
#442005=CARTESIAN_POINT('Ctrl Pts',(1.13507545516088,-2.4205638396315,13.8400110824519));
#442006=CARTESIAN_POINT('Ctrl Pts',(1.13217047247447,-2.43020141912292,
13.8494522556837));
#442007=CARTESIAN_POINT('Ctrl Pts',(1.11876887391233,-2.42905031382129,
13.85569149686));
#442008=CARTESIAN_POINT('Ctrl Pts',(1.14093234808971,-2.40536204594572,
13.8586819406588));
#442009=CARTESIAN_POINT('Ctrl Pts',(1.13701571582525,-2.40726363352982,
13.868010383617));
#442010=CARTESIAN_POINT('Ctrl Pts',(1.1286276705421,-2.40386752353154,13.8744918421245));
#442011=CARTESIAN_POINT('Ctrl Pts',(1.16910085695503,-2.39173829439737,
13.8587686893867));
#442012=CARTESIAN_POINT('Ctrl Pts',(1.17298260663561,-2.38985358027126,
13.8680909899357));
#442013=CARTESIAN_POINT('Ctrl Pts',(1.17552108595147,-2.3811902942741,13.8745789365162));
#442014=CARTESIAN_POINT('Ctrl Pts',(1.18475191195684,-2.39662290792254,
13.8400379222776));
#442015=CARTESIAN_POINT('Ctrl Pts',(1.19409837626435,-2.40035303377248,
13.8494748685453));
#442016=CARTESIAN_POINT('Ctrl Pts',(1.20155166576407,-2.3891633250677,13.8557104837033));
#442017=CARTESIAN_POINT('Ctrl Pts',(1.19283550652889,-2.40381648963277,
13.8235269408542));
#442018=CARTESIAN_POINT('Ctrl Pts',(1.20165610319301,-2.41166592867512,
13.8362179249195));
#442019=CARTESIAN_POINT('Ctrl Pts',(1.21492341965357,-2.40091226334689,
13.8391868794965));
#442020=CARTESIAN_POINT('Origin',(1.11369071356702,-2.43253901397856,13.8235269408515));
#442021=CARTESIAN_POINT('Ctrl Pts',(1.13758917738513,-2.46706225337413,
13.7902140241682));
#442022=CARTESIAN_POINT('Ctrl Pts',(1.13821700711224,-2.4785932735036,13.8026027327198));
#442023=CARTESIAN_POINT('Ctrl Pts',(1.12202867321912,-2.48242938847038,
13.8057746032556));
#442024=CARTESIAN_POINT('Ctrl Pts',(1.13694587371134,-2.45516253307467,
13.8013225161808));
#442025=CARTESIAN_POINT('Ctrl Pts',(1.13757305769207,-2.4666817590964,13.8136962270464));
#442026=CARTESIAN_POINT('Ctrl Pts',(1.12140795129213,-2.47051945897936,
13.8168830918628));
#442027=CARTESIAN_POINT('Ctrl Pts',(1.13630229270357,-2.44325768269871,
13.8124254880875));
#442028=CARTESIAN_POINT('Ctrl Pts',(1.1369285566201,-2.45476004195875,13.8247886461867));
#442029=CARTESIAN_POINT('Ctrl Pts',(1.1207872151701,-2.45860421396228,13.8279860620656));
#442030=CARTESIAN_POINT('Ctrl Pts',(1.13565842313425,-2.43134749456069,
13.8235227163065));
#442031=CARTESIAN_POINT('Ctrl Pts',(1.13628347348943,-2.44282755968639,
13.8358800595847));
#442032=CARTESIAN_POINT('Ctrl Pts',(1.12016646235943,-2.44668343611513,
13.8390832900376));
#442033=CARTESIAN_POINT('Origin',(1.11562146849286,-2.46825378521705,13.7902182540695));
#442034=CARTESIAN_POINT('Ctrl Pts',(1.13869367316181,-2.48749352245962,
13.7382347919292));
#442035=CARTESIAN_POINT('Ctrl Pts',(1.13953223696443,-2.50256052878079,
13.7369371795943));
#442036=CARTESIAN_POINT('Ctrl Pts',(1.12569260757996,-2.50872562695685,
13.7364597369712));
#442037=CARTESIAN_POINT('Ctrl Pts',(1.13879578288449,-2.48938232302847,
13.7595490285574));
#442038=CARTESIAN_POINT('Ctrl Pts',(1.13965335022948,-2.50480887107615,
13.7633824266925));
#442039=CARTESIAN_POINT('Ctrl Pts',(1.12603045845521,-2.51115792455001,
13.7648920890506));
#442040=CARTESIAN_POINT('Ctrl Pts',(1.13827502890081,-2.47974954360394,
13.7803806590111));
#442041=CARTESIAN_POINT('Ctrl Pts',(1.139022184095,-2.49309265587658,13.7901039518745));
#442042=CARTESIAN_POINT('Ctrl Pts',(1.12431173525789,-2.49875729500326,
13.7926933640892));
#442043=CARTESIAN_POINT('Ctrl Pts',(1.13736984215328,-2.46300562266155,
13.7936647693663));
#442044=CARTESIAN_POINT('Ctrl Pts',(1.13798360340382,-2.47380361456152,
13.8072068914932));
#442045=CARTESIAN_POINT('Ctrl Pts',(1.12128698319839,-2.47724848662918,
13.8104111085397));
#442046=CARTESIAN_POINT('Origin',(1.11674034567518,-2.48895058214125,13.7435492065112));
#442047=CARTESIAN_POINT('Origin',(1.11674034567518,-2.48895058214125,14.));
#442048=CARTESIAN_POINT('Origin',(1.11674034567518,-2.48895058214125,12.5369868989719));
#442049=CARTESIAN_POINT('Ctrl Pts',(1.15499117054605,-2.48857307842948,
12.506462012331));
#442050=CARTESIAN_POINT('Ctrl Pts',(1.15774383942968,-2.49450404816529,
12.4999388158272));
#442051=CARTESIAN_POINT('Ctrl Pts',(1.15771127174688,-2.49443387701532,
12.4907030323752));
#442052=CARTESIAN_POINT('Ctrl Pts',(1.1440804381578,-2.49613512193016,12.5042014951932));
#442053=CARTESIAN_POINT('Ctrl Pts',(1.14148625048243,-2.50201825777945,
12.4980716682127));
#442054=CARTESIAN_POINT('Ctrl Pts',(1.13530546092887,-2.50483311225539,
12.4907355092743));
#442055=CARTESIAN_POINT('Ctrl Pts',(1.1389949678552,-2.49290035871678,12.5218047446509));
#442056=CARTESIAN_POINT('Ctrl Pts',(1.13631761128863,-2.50440473322178,
12.5216906929434));
#442057=CARTESIAN_POINT('Ctrl Pts',(1.12553862196712,-2.50911473784347,
12.5161988840776));
#442058=CARTESIAN_POINT('Ctrl Pts',(1.13870616091534,-2.4877246291098,12.5369868989719));
#442059=CARTESIAN_POINT('Ctrl Pts',(1.13956042115541,-2.50303069885232,
12.5369868989719));
#442060=CARTESIAN_POINT('Ctrl Pts',(1.12549728860093,-2.50913265216876,
12.5369868989719));
#442061=CARTESIAN_POINT('Origin',(2.23530940884416E-31,-9.79353041666012E-31,
12.5));
#442062=CARTESIAN_POINT('Origin',(1.33005753786835,-2.3306945761811,12.5));
#442063=CARTESIAN_POINT('',(1.33005753786835,-2.3306945761811,12.5893111709658));
#442064=CARTESIAN_POINT('',(1.33005753786835,-2.3306945761811,13.8235269408515));
#442065=CARTESIAN_POINT('',(1.33005753786835,-2.3306945761811,12.5));
#442066=CARTESIAN_POINT('',(1.33489295378215,-2.36613313501385,13.7902182540695));
#442067=CARTESIAN_POINT('',(1.33005753786835,-2.3306945761811,13.8235269408515));
#442068=CARTESIAN_POINT('',(1.33769508908196,-2.38666986617615,13.7435492065112));
#442069=CARTESIAN_POINT('Origin',(1.32847642374838,-2.31910424806525,13.7445212918691));
#442070=CARTESIAN_POINT('',(1.33769508908196,-2.38666986617615,12.5369868989719));
#442071=CARTESIAN_POINT('',(1.33769508908196,-2.38666986617615,12.5));
#442072=CARTESIAN_POINT('Ctrl Pts',(1.33769508908196,-2.38666986617615,
12.5369868989719));
#442073=CARTESIAN_POINT('Ctrl Pts',(1.33515109546587,-2.36802504450181,
12.5544431401645));
#442074=CARTESIAN_POINT('Ctrl Pts',(1.33260528231792,-2.34936688755546,
12.5718848856037));
#442075=CARTESIAN_POINT('Ctrl Pts',(1.33005753786835,-2.3306945761811,12.5893111709658));
#442076=CARTESIAN_POINT('Origin',(1.60445193644508,-2.46405362951698,12.5));
#442077=CARTESIAN_POINT('',(1.4299234933485,-2.33258226106547,13.7435492065112));
#442078=CARTESIAN_POINT('',(1.41336809784464,-2.32011116773803,13.7902182540695));
#442079=CARTESIAN_POINT('Origin',(1.36986337980535,-2.28733928990974,13.7418732680433));
#442080=CARTESIAN_POINT('',(1.38479980462764,-2.29859082104312,13.8235269408515));
#442081=CARTESIAN_POINT('',(1.41336809784464,-2.32011116773803,13.7902182540695));
#442082=CARTESIAN_POINT('',(1.38479980462764,-2.29859082104312,12.5893111709658));
#442083=CARTESIAN_POINT('',(1.38479980462764,-2.29859082104312,12.5));
#442084=CARTESIAN_POINT('',(1.4299234933485,-2.33258226106547,12.5369868989719));
#442085=CARTESIAN_POINT('Ctrl Pts',(1.38479980462764,-2.29859082104312,
12.5893111709658));
#442086=CARTESIAN_POINT('Ctrl Pts',(1.39985222447629,-2.30992973062655,
12.5718848856037));
#442087=CARTESIAN_POINT('Ctrl Pts',(1.4148932339329,-2.321260044821,12.5544431401645));
#442088=CARTESIAN_POINT('Ctrl Pts',(1.4299234933485,-2.33258226106547,12.5369868989719));
#442089=CARTESIAN_POINT('',(1.4299234933485,-2.33258226106547,12.5));
#442090=CARTESIAN_POINT('Origin',(1.36411695356841,-2.3260473375203,12.5));
#442091=CARTESIAN_POINT('',(1.34577128976252,-2.29697799298522,13.8587068136939));
#442092=CARTESIAN_POINT('Ctrl Pts',(1.3847998046315,-2.29859082103775,13.8235269408542));
#442093=CARTESIAN_POINT('Ctrl Pts',(1.38340018258377,-2.29753649302872,
13.8262006681044));
#442094=CARTESIAN_POINT('Ctrl Pts',(1.38186333792216,-2.29659631404677,
13.8288634856214));
#442095=CARTESIAN_POINT('Ctrl Pts',(1.38020039422952,-2.29576293072852,
13.8314912288862));
#442096=CARTESIAN_POINT('Ctrl Pts',(1.3784860708071,-2.2949037984869,13.8342001611531));
#442097=CARTESIAN_POINT('Ctrl Pts',(1.37663605428186,-2.29415676465242,
13.8368750301949));
#442098=CARTESIAN_POINT('Ctrl Pts',(1.37462670689041,-2.29354133620147,
13.8394886372969));
#442099=CARTESIAN_POINT('Ctrl Pts',(1.37447152011737,-2.29349380516939,
13.8396904925131));
#442100=CARTESIAN_POINT('Ctrl Pts',(1.37431537292207,-2.29344707888645,
13.8398919674349));
#442101=CARTESIAN_POINT('Ctrl Pts',(1.37415825014436,-2.29340117695641,
13.8400930404591));
#442102=CARTESIAN_POINT('Ctrl Pts',(1.37171017156055,-2.29268599400502,
13.8432258934518));
#442103=CARTESIAN_POINT('Ctrl Pts',(1.36903807042446,-2.29217349775966,
13.8462331177034));
#442104=CARTESIAN_POINT('Ctrl Pts',(1.3662109257099,-2.29197514260721,13.8489036603661));
#442105=CARTESIAN_POINT('Ctrl Pts',(1.36528585105815,-2.29191023849295,
13.8497774930041));
#442106=CARTESIAN_POINT('Ctrl Pts',(1.3643443752974,-2.29187911987411,13.85061494757));
#442107=CARTESIAN_POINT('Ctrl Pts',(1.36338949058611,-2.29188611370955,
13.8514076489583));
#442108=CARTESIAN_POINT('Ctrl Pts',(1.36136977170674,-2.29190090668017,
13.8530843267192));
#442109=CARTESIAN_POINT('Ctrl Pts',(1.35909169550347,-2.29209061940835,
13.8546805203176));
#442110=CARTESIAN_POINT('Ctrl Pts',(1.35669880437277,-2.29258021605276,
13.8559412814274));
#442111=CARTESIAN_POINT('Ctrl Pts',(1.35637855793619,-2.29264573996178,
13.8561100121513));
#442112=CARTESIAN_POINT('Ctrl Pts',(1.35605629207205,-2.29271656782227,
13.8562727473908));
#442113=CARTESIAN_POINT('Ctrl Pts',(1.35573237882863,-2.29279292867908,
13.8564289040185));
#442114=CARTESIAN_POINT('Ctrl Pts',(1.35426343596501,-2.29313922429353,
13.8571370725437));
#442115=CARTESIAN_POINT('Ctrl Pts',(1.35273531532566,-2.29360761478373,
13.8577210840554));
#442116=CARTESIAN_POINT('Ctrl Pts',(1.35121601586956,-2.29420795324734,
13.8581177131616));
#442117=CARTESIAN_POINT('Ctrl Pts',(1.35078812885002,-2.29437702922171,
13.8582294175695));
#442118=CARTESIAN_POINT('Ctrl Pts',(1.35036090986562,-2.29455639626784,
13.8583265086086));
#442119=CARTESIAN_POINT('Ctrl Pts',(1.34993577393002,-2.29474584738435,
13.8584082369006));
#442120=CARTESIAN_POINT('Ctrl Pts',(1.34932496759527,-2.29501803783546,
13.8585256585398));
#442121=CARTESIAN_POINT('Ctrl Pts',(1.34871099893909,-2.29531472312331,
13.8586122832068));
#442122=CARTESIAN_POINT('Ctrl Pts',(1.34811016067259,-2.29562890724788,
13.8586682984299));
#442123=CARTESIAN_POINT('Ctrl Pts',(1.34762954961857,-2.29588022340347,
13.8587131050557));
#442124=CARTESIAN_POINT('Ctrl Pts',(1.34715192292426,-2.29614530403958,
13.8587357943552));
#442125=CARTESIAN_POINT('Ctrl Pts',(1.34667746959686,-2.29642462347374,
13.8587355499465));
#442126=CARTESIAN_POINT('Ctrl Pts',(1.34637081909986,-2.29660515428332,
13.8587353919793));
#442127=CARTESIAN_POINT('Ctrl Pts',(1.34606879068543,-2.29678964756824,
13.8587257282814));
#442128=CARTESIAN_POINT('Ctrl Pts',(1.34577128976252,-2.29697799298522,
13.8587068136939));
#442129=CARTESIAN_POINT('Ctrl Pts',(1.34577128976252,-2.29697799298522,
13.8587068136939));
#442130=CARTESIAN_POINT('Ctrl Pts',(1.34479282544556,-2.29759745079387,
13.8586446046466));
#442131=CARTESIAN_POINT('Ctrl Pts',(1.3438632747108,-2.2982585267788,13.858482427929));
#442132=CARTESIAN_POINT('Ctrl Pts',(1.34297980313987,-2.29895776376923,
13.8582284286032));
#442133=CARTESIAN_POINT('Ctrl Pts',(1.34207346407774,-2.29967509958282,
13.8579678548414));
#442134=CARTESIAN_POINT('Ctrl Pts',(1.34121435705807,-2.30043555072053,
13.857615680862));
#442135=CARTESIAN_POINT('Ctrl Pts',(1.34042992937994,-2.30120188140978,
13.8571944833187));
#442136=CARTESIAN_POINT('Ctrl Pts',(1.33847230988447,-2.30311433801868,
13.8561433417727));
#442137=CARTESIAN_POINT('Ctrl Pts',(1.33688487323664,-2.30514944118479,
13.8546163505474));
#442138=CARTESIAN_POINT('Ctrl Pts',(1.33562829342631,-2.30710418516538,
13.8528973491086));
#442139=CARTESIAN_POINT('Ctrl Pts',(1.33539873483407,-2.30746128805108,
13.8525833129072));
#442140=CARTESIAN_POINT('Ctrl Pts',(1.33518007748481,-2.30781569617413,
13.8522628768812));
#442141=CARTESIAN_POINT('Ctrl Pts',(1.33497190318365,-2.30816618356834,
13.851937733538));
#442142=CARTESIAN_POINT('Ctrl Pts',(1.33370061160934,-2.31030656145685,
13.8499521282529));
#442143=CARTESIAN_POINT('Ctrl Pts',(1.33269743617666,-2.31251551658544,
13.847639871647));
#442144=CARTESIAN_POINT('Ctrl Pts',(1.33194194943937,-2.31464373378926,
13.8452109780794));
#442145=CARTESIAN_POINT('Ctrl Pts',(1.33160204031847,-2.31560126276115,
13.8441181685877));
#442146=CARTESIAN_POINT('Ctrl Pts',(1.3313115527633,-2.31654245669621,13.8430021611332));
#442147=CARTESIAN_POINT('Ctrl Pts',(1.33106549254158,-2.31745477819194,
13.8418824960098));
#442148=CARTESIAN_POINT('Ctrl Pts',(1.33048564534573,-2.31960468709359,
13.8392439765549));
#442149=CARTESIAN_POINT('Ctrl Pts',(1.33012114163059,-2.3216960510513,13.8364981347964));
#442150=CARTESIAN_POINT('Ctrl Pts',(1.32993730510416,-2.32372852519983,
13.8336931113419));
#442151=CARTESIAN_POINT('Ctrl Pts',(1.32975826000211,-2.32570802594645,
13.8309611966328));
#442152=CARTESIAN_POINT('Ctrl Pts',(1.32975096988766,-2.3276337010985,13.8281701127186));
#442153=CARTESIAN_POINT('Ctrl Pts',(1.32992114581565,-2.32949429007333,
13.8253580685121));
#442154=CARTESIAN_POINT('Ctrl Pts',(1.3299580401405,-2.32989766777108,13.8247484142933));
#442155=CARTESIAN_POINT('Ctrl Pts',(1.33000341022909,-2.33029787700102,
13.8241378483365));
#442156=CARTESIAN_POINT('Ctrl Pts',(1.33005753786835,-2.3306945761811,13.8235269408515));
#442157=CARTESIAN_POINT('',(1.34683346955762,-2.29633413668072,12.5969504640361));
#442158=CARTESIAN_POINT('Origin',(1.3641335218256,-2.32607597622948,12.584524458991));
#442159=CARTESIAN_POINT('Origin',(1.3641335218256,-2.32607597622948,12.584524458991));
#442160=CARTESIAN_POINT('Ctrl Pts',(1.38479980462764,-2.29859082104312,
12.5893111709658));
#442161=CARTESIAN_POINT('Ctrl Pts',(1.37574697432481,-2.29177137106032,
12.5770542771492));
#442162=CARTESIAN_POINT('Ctrl Pts',(1.36363630048298,-2.30277751725014,
12.5737548217797));
#442163=CARTESIAN_POINT('Ctrl Pts',(1.40459530627978,-2.31350266948006,
12.5663937883685));
#442164=CARTESIAN_POINT('Ctrl Pts',(1.39553092783467,-2.30667452034175,
12.5540940315304));
#442165=CARTESIAN_POINT('Ctrl Pts',(1.38338488516658,-2.31771714877968,
12.5508374392248));
#442166=CARTESIAN_POINT('Ctrl Pts',(1.42437083451345,-2.32839947204475,
12.5434499600945));
#442167=CARTESIAN_POINT('Ctrl Pts',(1.41527698454607,-2.321549122162,12.5311293540533));
#442168=CARTESIAN_POINT('Ctrl Pts',(1.40311488688602,-2.3326412430173,12.5278936106989));
#442169=CARTESIAN_POINT('Ctrl Pts',(1.4441279538738,-2.34328240730091,12.5204817579905));
#442170=CARTESIAN_POINT('Ctrl Pts',(1.43498909556389,-2.33639815286782,
12.5081597038247));
#442171=CARTESIAN_POINT('Ctrl Pts',(1.42282775834021,-2.34755099653329,
12.5049254088044));
#442172=CARTESIAN_POINT('Ctrl Pts',(1.4299234933485,-2.33258226106547,12.5369868989719));
#442173=CARTESIAN_POINT('Ctrl Pts',(1.4306675187513,-2.33314273173438,12.5342545179733));
#442174=CARTESIAN_POINT('Ctrl Pts',(1.43130252505372,-2.33377725841565,
12.5314872231885));
#442175=CARTESIAN_POINT('Ctrl Pts',(1.43175322838372,-2.3344896400679,12.5287124745063));
#442176=CARTESIAN_POINT('Ctrl Pts',(1.43215969501762,-2.33513210120137,
12.5262100684184));
#442177=CARTESIAN_POINT('Ctrl Pts',(1.43241502064328,-2.33583776199992,
12.5237004536639));
#442178=CARTESIAN_POINT('Ctrl Pts',(1.43246125367359,-2.33664129362863,
12.5212220730815));
#442179=CARTESIAN_POINT('Ctrl Pts',(1.43249664905777,-2.33725646660144,
12.5193246583486));
#442180=CARTESIAN_POINT('Ctrl Pts',(1.43240928001402,-2.33793639253365,
12.517417831369));
#442181=CARTESIAN_POINT('Ctrl Pts',(1.43210215847269,-2.33868795162138,
12.5155812248348));
#442182=CARTESIAN_POINT('Ctrl Pts',(1.4319713230453,-2.3390081198324,12.5147988205793));
#442183=CARTESIAN_POINT('Ctrl Pts',(1.4318007304294,-2.33934171787815,12.5140295443047));
#442184=CARTESIAN_POINT('Ctrl Pts',(1.43158405520617,-2.339691052389,12.5132817086137));
#442185=CARTESIAN_POINT('Ctrl Pts',(1.43125614656697,-2.34021972291427,
12.5121499604604));
#442186=CARTESIAN_POINT('Ctrl Pts',(1.43080953768677,-2.34079208086607,
12.5110494206568));
#442187=CARTESIAN_POINT('Ctrl Pts',(1.43020905781341,-2.34139588218719,
12.5100666561695));
#442188=CARTESIAN_POINT('Ctrl Pts',(1.42986426365291,-2.34174258351535,
12.5095023550641));
#442189=CARTESIAN_POINT('Ctrl Pts',(1.42946429115295,-2.34210319734582,
12.5089719619137));
#442190=CARTESIAN_POINT('Ctrl Pts',(1.42901236051004,-2.34246622073481,
12.5085043804652));
#442191=CARTESIAN_POINT('Ctrl Pts',(1.42835101888226,-2.34299745817747,
12.5078201359221));
#442192=CARTESIAN_POINT('Ctrl Pts',(1.42755847393475,-2.34354832160772,
12.5072563000949));
#442193=CARTESIAN_POINT('Ctrl Pts',(1.42668361668369,-2.34407451888694,
12.5068768744332));
#442194=CARTESIAN_POINT('Ctrl Pts',(1.4260527843803,-2.34445394334879,12.5066032824114));
#442195=CARTESIAN_POINT('Ctrl Pts',(1.42536810277607,-2.34482726026711,
12.5064197834844));
#442196=CARTESIAN_POINT('Ctrl Pts',(1.42466904366106,-2.3451758920944,12.5063282718343));
#442197=CARTESIAN_POINT('Ctrl Pts',(1.42364863377637,-2.34568478662856,
12.5061946931565));
#442198=CARTESIAN_POINT('Ctrl Pts',(1.42257625378674,-2.34615291229311,
12.5062515701262));
#442199=CARTESIAN_POINT('Ctrl Pts',(1.42152464441223,-2.34656538937389,
12.5064436508398));
#442200=CARTESIAN_POINT('',(1.36363630048298,-2.30277751725014,12.5737548217797));
#442201=CARTESIAN_POINT('Origin',(1.37156277994973,-2.31616299158851,12.5893111709658));
#442202=CARTESIAN_POINT('Ctrl Pts',(1.42152464441223,-2.34656538937389,
12.5064436508398));
#442203=CARTESIAN_POINT('Ctrl Pts',(1.41295537570013,-2.34008402983357,
12.5164271754438));
#442204=CARTESIAN_POINT('Ctrl Pts',(1.40438283616937,-2.33359993444451,
12.5264061185523));
#442205=CARTESIAN_POINT('Ctrl Pts',(1.39580691005351,-2.32711300760729,
12.536380305637));
#442206=CARTESIAN_POINT('Ctrl Pts',(1.38508874179391,-2.3190056647513,12.5488460165097));
#442207=CARTESIAN_POINT('Ctrl Pts',(1.37436528056057,-2.31089389677882,
12.5613043021964));
#442208=CARTESIAN_POINT('Ctrl Pts',(1.36363630048298,-2.30277751725014,
12.5737548217797));
#442209=CARTESIAN_POINT('Ctrl Pts',(1.33005753786835,-2.3306945761811,12.5893111709658));
#442210=CARTESIAN_POINT('Ctrl Pts',(1.32852527273166,-2.31946466976517,
12.5770542771492));
#442211=CARTESIAN_POINT('Ctrl Pts',(1.34404297558573,-2.31426807732516,
12.5737548217797));
#442212=CARTESIAN_POINT('Ctrl Pts',(1.32862794782275,-2.32021717116761,
12.5928319619712));
#442213=CARTESIAN_POINT('Ctrl Pts',(1.33082600547995,-2.31222955832602,
12.5821634970842));
#442214=CARTESIAN_POINT('Ctrl Pts',(1.34351285833518,-2.31045268834498,
12.5773203894503));
#442215=CARTESIAN_POINT('Ctrl Pts',(1.33349228706153,-2.30418837510834,
12.5969440695591));
#442216=CARTESIAN_POINT('Ctrl Pts',(1.33695048122292,-2.30213912263633,
12.5878292599214));
#442217=CARTESIAN_POINT('Ctrl Pts',(1.34524856590918,-2.30474029249778,
12.5813877129824));
#442218=CARTESIAN_POINT('Ctrl Pts',(1.35985808863388,-2.28866356422419,
12.596957478804));
#442219=CARTESIAN_POINT('Ctrl Pts',(1.356425492319,-2.29069774113094,12.5878468778671));
#442220=CARTESIAN_POINT('Ctrl Pts',(1.35468827845761,-2.29918888769294,
12.5814011370086));
#442221=CARTESIAN_POINT('Ctrl Pts',(1.37634132880733,-2.29221909520066,
12.5928371701607));
#442222=CARTESIAN_POINT('Ctrl Pts',(1.36830145855742,-2.29024537990497,
12.5821692192952));
#442223=CARTESIAN_POINT('Ctrl Pts',(1.36055556075656,-2.30044463915389,
12.5773318885715));
#442224=CARTESIAN_POINT('Ctrl Pts',(1.38479980462767,-2.29859082104307,
12.5893111709658));
#442225=CARTESIAN_POINT('Ctrl Pts',(1.37574697432484,-2.29177137106028,
12.5770542771492));
#442226=CARTESIAN_POINT('Ctrl Pts',(1.36363630048301,-2.3027775172501,12.5737548217797));
#442227=CARTESIAN_POINT('',(1.34404297558573,-2.31426807732516,12.5737548217797));
#442228=CARTESIAN_POINT('Origin',(1.35185556391639,-2.32772034343819,12.5893111709658));
#442229=CARTESIAN_POINT('Ctrl Pts',(1.36363630048301,-2.3027775172501,12.5737548217797));
#442230=CARTESIAN_POINT('Ctrl Pts',(1.36285593465867,-2.30214874955753,
12.5746934679442));
#442231=CARTESIAN_POINT('Ctrl Pts',(1.36187747551444,-2.30159561924621,
12.5756680099006));
#442232=CARTESIAN_POINT('Ctrl Pts',(1.36081388266436,-2.30117815796984,
12.5765688348656));
#442233=CARTESIAN_POINT('Ctrl Pts',(1.36053230823167,-2.30106763971838,
12.5768073183026));
#442234=CARTESIAN_POINT('Ctrl Pts',(1.36024491640241,-2.30096642081367,
12.5770407398754));
#442235=CARTESIAN_POINT('Ctrl Pts',(1.35995400458318,-2.30087508924008,
12.5772674179684));
#442236=CARTESIAN_POINT('Ctrl Pts',(1.35876018114294,-2.30050028915916,
12.5781976435658));
#442237=CARTESIAN_POINT('Ctrl Pts',(1.35743589397504,-2.30028147193012,
12.5790594849312));
#442238=CARTESIAN_POINT('Ctrl Pts',(1.35606268876446,-2.30028105561961,
12.5797571720116));
#442239=CARTESIAN_POINT('Ctrl Pts',(1.35516799619371,-2.30028078437835,
12.580211740231));
#442240=CARTESIAN_POINT('Ctrl Pts',(1.3542118730462,-2.3003919846801,12.5806009430798));
#442241=CARTESIAN_POINT('Ctrl Pts',(1.35326367294809,-2.30062442658311,
12.5808812374708));
#442242=CARTESIAN_POINT('Ctrl Pts',(1.35244885450172,-2.3008241712896,12.5811221033394));
#442243=CARTESIAN_POINT('Ctrl Pts',(1.35162323250718,-2.30111764714012,
12.581287365893));
#442244=CARTESIAN_POINT('Ctrl Pts',(1.35083619904058,-2.30149614628925,
12.581359338449));
#442245=CARTESIAN_POINT('Ctrl Pts',(1.35072681764034,-2.30154874985527,
12.5813693411482));
#442246=CARTESIAN_POINT('Ctrl Pts',(1.35061813913538,-2.30160295344113,
12.5813775999465));
#442247=CARTESIAN_POINT('Ctrl Pts',(1.35051025186457,-2.3016586911885,12.5813841266931));
#442248=CARTESIAN_POINT('Ctrl Pts',(1.35032720806094,-2.30175325701826,
12.5813952001081));
#442249=CARTESIAN_POINT('Ctrl Pts',(1.3501454953712,-2.30185341326867,12.5814007534795));
#442250=CARTESIAN_POINT('Ctrl Pts',(1.34996528813256,-2.30195928903071,
12.5814005856065));
#442251=CARTESIAN_POINT('Ctrl Pts',(1.34914036985051,-2.30244394687459,
12.5813998171494));
#442252=CARTESIAN_POINT('Ctrl Pts',(1.34840382210296,-2.30301467712284,
12.58127954464));
#442253=CARTESIAN_POINT('Ctrl Pts',(1.34774170279521,-2.30364485021765,
12.5810700125799));
#442254=CARTESIAN_POINT('Ctrl Pts',(1.34694193805975,-2.30440602756523,
12.5808169217085));
#442255=CARTESIAN_POINT('Ctrl Pts',(1.34626222936553,-2.30526612317064,
12.5804173076348));
#442256=CARTESIAN_POINT('Ctrl Pts',(1.345741712958,-2.30613361267326,12.5799304713245));
#442257=CARTESIAN_POINT('Ctrl Pts',(1.34509662914949,-2.30720870545437,
12.5793271277669));
#442258=CARTESIAN_POINT('Ctrl Pts',(1.34462842209326,-2.30834527703632,
12.5785808224116));
#442259=CARTESIAN_POINT('Ctrl Pts',(1.34432750161313,-2.30948333798708,
12.5777485681082));
#442260=CARTESIAN_POINT('Ctrl Pts',(1.34387909712944,-2.31117917348759,
12.576508418016));
#442261=CARTESIAN_POINT('Ctrl Pts',(1.34379927191416,-2.31286227997435,
12.5750928681475));
#442262=CARTESIAN_POINT('Ctrl Pts',(1.34404297558573,-2.31426807732516,
12.5737548217797));
#442263=CARTESIAN_POINT('Ctrl Pts',(1.34404297558573,-2.31426807732516,
12.5737548217797));
#442264=CARTESIAN_POINT('Ctrl Pts',(1.32852527273166,-2.31946466976517,
12.5770542771492));
#442265=CARTESIAN_POINT('Ctrl Pts',(1.33005753786835,-2.3306945761811,12.5893111709658));
#442266=CARTESIAN_POINT('Ctrl Pts',(1.34744016605087,-2.33879304523776,
12.5508408821982));
#442267=CARTESIAN_POINT('Ctrl Pts',(1.33187336419732,-2.3440026905886,12.55409748406));
#442268=CARTESIAN_POINT('Ctrl Pts',(1.33340758411188,-2.35524692348901,
12.5663972313419));
#442269=CARTESIAN_POINT('Ctrl Pts',(1.35083286953169,-2.36329421718692,
12.52790050457));
#442270=CARTESIAN_POINT('Ctrl Pts',(1.33521504327091,-2.36849371526164,
12.5311362602938));
#442271=CARTESIAN_POINT('Ctrl Pts',(1.33675425070924,-2.37977450151295,
12.5434568539655));
#442272=CARTESIAN_POINT('Ctrl Pts',(1.3542214210074,-2.3877734443245,12.5049357605811));
#442273=CARTESIAN_POINT('Ctrl Pts',(1.3385509784115,-2.39294264289276,12.5081700652078));
#442274=CARTESIAN_POINT('Ctrl Pts',(1.34009780235499,-2.4042792501883,12.5204921097672));
#442275=CARTESIAN_POINT('Ctrl Pts',(1.35399891386265,-2.38616604253264,
12.5064436508395));
#442276=CARTESIAN_POINT('Ctrl Pts',(1.3530555292503,-2.38693991155501,12.5062361689309));
#442277=CARTESIAN_POINT('Ctrl Pts',(1.35204148695911,-2.3877044439952,12.5061871075061));
#442278=CARTESIAN_POINT('Ctrl Pts',(1.35101992142306,-2.38838812557069,
12.5063648335164));
#442279=CARTESIAN_POINT('Ctrl Pts',(1.3505558633438,-2.3886986959135,12.5064455676329));
#442280=CARTESIAN_POINT('Ctrl Pts',(1.35008365763473,-2.38899673109934,
12.506574497099));
#442281=CARTESIAN_POINT('Ctrl Pts',(1.3496229901299,-2.38926856353753,12.5067492519495));
#442282=CARTESIAN_POINT('Ctrl Pts',(1.34869726089708,-2.38981482137387,
12.5071004286051));
#442283=CARTESIAN_POINT('Ctrl Pts',(1.34778367929148,-2.39027465397608,
12.5076537929613));
#442284=CARTESIAN_POINT('Ctrl Pts',(1.34695506683916,-2.39062199710647,
12.5083435010505));
#442285=CARTESIAN_POINT('Ctrl Pts',(1.34690290073347,-2.39064386443225,
12.5083869222964));
#442286=CARTESIAN_POINT('Ctrl Pts',(1.3468510610964,-2.39066527728885,12.5084308732337));
#442287=CARTESIAN_POINT('Ctrl Pts',(1.34679956164954,-2.39068622596491,
12.5084753333615));
#442288=CARTESIAN_POINT('Ctrl Pts',(1.34638646811256,-2.39085426199668,
12.5088319622689));
#442289=CARTESIAN_POINT('Ctrl Pts',(1.34598736256616,-2.39099703833141,
12.509227847131));
#442290=CARTESIAN_POINT('Ctrl Pts',(1.34561505565621,-2.39111294591216,
12.5096423454524));
#442291=CARTESIAN_POINT('Ctrl Pts',(1.34444841057657,-2.3914761489717,12.5109411997424));
#442292=CARTESIAN_POINT('Ctrl Pts',(1.34347602405095,-2.39160709374809,
12.5124831113042));
#442293=CARTESIAN_POINT('Ctrl Pts',(1.34267177826769,-2.39159674021777,
12.5140723025007));
#442294=CARTESIAN_POINT('Ctrl Pts',(1.34259641955694,-2.39159577008064,
12.5142212114565));
#442295=CARTESIAN_POINT('Ctrl Pts',(1.34252251945001,-2.39159358312782,
12.5143705582413));
#442296=CARTESIAN_POINT('Ctrl Pts',(1.34245004761741,-2.39159026868938,
12.5145201959299));
#442297=CARTESIAN_POINT('Ctrl Pts',(1.34151903902849,-2.391547689793,12.5164425148273));
#442298=CARTESIAN_POINT('Ctrl Pts',(1.34079135146546,-2.39132830750116,
12.5184635205941));
#442299=CARTESIAN_POINT('Ctrl Pts',(1.34020062667919,-2.39099323287115,
12.5205025929158));
#442300=CARTESIAN_POINT('Ctrl Pts',(1.33985798288901,-2.39079887630463,
12.5216853356836));
#442301=CARTESIAN_POINT('Ctrl Pts',(1.33956180005114,-2.39056636720568,
12.5228750347131));
#442302=CARTESIAN_POINT('Ctrl Pts',(1.33930338674184,-2.39031174904033,
12.5240609649613));
#442303=CARTESIAN_POINT('Ctrl Pts',(1.33866912513756,-2.38968680241326,
12.5269717671326));
#442304=CARTESIAN_POINT('Ctrl Pts',(1.33825184439555,-2.38890367038702,
12.5299036066169));
#442305=CARTESIAN_POINT('Ctrl Pts',(1.33798261325784,-2.38801486966659,
12.5328133004019));
#442306=CARTESIAN_POINT('Ctrl Pts',(1.33785336663488,-2.38758819356747,
12.5342101228451));
#442307=CARTESIAN_POINT('Ctrl Pts',(1.33775890175191,-2.38713754593067,
12.5356023438238));
#442308=CARTESIAN_POINT('Ctrl Pts',(1.33769508908196,-2.38666986617615,
12.5369868989719));
#442309=CARTESIAN_POINT('Origin',(3.05553750638695,-15.0158462982873,-1.24020005376493));
#442310=CARTESIAN_POINT('Ctrl Pts',(1.42989013470326,-2.33255708246902,
12.5369868989719));
#442311=CARTESIAN_POINT('Ctrl Pts',(1.4421243339961,-2.34180952384133,12.5369868989719));
#442312=CARTESIAN_POINT('Ctrl Pts',(1.45503642140515,-2.33352934857591,
12.5369868989719));
#442313=CARTESIAN_POINT('Ctrl Pts',(1.43402581247992,-2.33568471670369,
12.5218025310015));
#442314=CARTESIAN_POINT('Ctrl Pts',(1.44507317275512,-2.33988134566683,
12.5216901060417));
#442315=CARTESIAN_POINT('Ctrl Pts',(1.45499706998605,-2.33355460317673,
12.5161920673678));
#442316=CARTESIAN_POINT('Ctrl Pts',(1.43387704573138,-2.34171082155254,
12.5042015548895));
#442317=CARTESIAN_POINT('Ctrl Pts',(1.44021003496673,-2.34283802710698,
12.4980677368514));
#442318=CARTESIAN_POINT('Ctrl Pts',(1.44599672539461,-2.33927362061841,
12.4907278922777));
#442319=CARTESIAN_POINT('Ctrl Pts',(1.42151428120016,-2.34654828244138,
12.506463626192));
#442320=CARTESIAN_POINT('Ctrl Pts',(1.42490428456029,-2.35214429133653,
12.4999376786891));
#442321=CARTESIAN_POINT('Ctrl Pts',(1.42486288059831,-2.35207594422447,
12.4906970594712));
#442322=CARTESIAN_POINT('Origin',(1.44316051802641,-2.31501009052007,12.5369868989719));
#442323=CARTESIAN_POINT('Origin',(1.44316051802641,-2.31501009052007,14.));
#442324=CARTESIAN_POINT('Origin',(1.44316051802641,-2.31501009052007,13.7435492065112));
#442325=CARTESIAN_POINT('Ctrl Pts',(1.41014674742212,-2.31768450722606,
13.793642941384));
#442326=CARTESIAN_POINT('Ctrl Pts',(1.41876651813523,-2.32421181692144,
13.8071662555867));
#442327=CARTESIAN_POINT('Ctrl Pts',(1.4309317412638,-2.3122943201261,13.8103758687955));
#442328=CARTESIAN_POINT('Ctrl Pts',(1.42342261813437,-2.32768515530782,
13.7804579775006));
#442329=CARTESIAN_POINT('Ctrl Pts',(1.4340647580115,-2.33573118106993,13.7901904343351));
#442330=CARTESIAN_POINT('Ctrl Pts',(1.44695570293302,-2.3266714093733,13.7927914348263));
#442331=CARTESIAN_POINT('Ctrl Pts',(1.43123862287275,-2.33357291316989,
13.7597120340895));
#442332=CARTESIAN_POINT('Ctrl Pts',(1.44355803165682,-2.34287985988636,
13.7635825532445));
#442333=CARTESIAN_POINT('Ctrl Pts',(1.45642208594866,-2.33513053583062,
13.7651073818884));
#442334=CARTESIAN_POINT('Ctrl Pts',(1.42970807017931,-2.33241995536553,
13.7381884353898));
#442335=CARTESIAN_POINT('Ctrl Pts',(1.44173857844135,-2.34150977283253,
13.7368803041982));
#442336=CARTESIAN_POINT('Ctrl Pts',(1.45456861617911,-2.33347361897843,
13.7363986145813));
#442337=CARTESIAN_POINT('Origin',(1.42660512252255,-2.30253899719264,13.7902182540695));
#442338=CARTESIAN_POINT('Ctrl Pts',(1.38479666110474,-2.29858845209351,
13.8235227101244));
#442339=CARTESIAN_POINT('Ctrl Pts',(1.3939771078202,-2.30550958541284,13.8358800583119));
#442340=CARTESIAN_POINT('Ctrl Pts',(1.4061659581551,-2.29428203106783,13.8390832900376));
#442341=CARTESIAN_POINT('Ctrl Pts',(1.39432363649803,-2.30576507310551,
13.8124254819053));
#442342=CARTESIAN_POINT('Ctrl Pts',(1.40352191167836,-2.31269964694552,
13.8247886449157));
#442343=CARTESIAN_POINT('Ctrl Pts',(1.41571461549997,-2.30144536977546,
13.8279860620657));
#442344=CARTESIAN_POINT('Ctrl Pts',(1.40384634221089,-2.31293847778947,
13.8013225099955));
#442345=CARTESIAN_POINT('Ctrl Pts',(1.41305810454048,-2.31988322174559,
13.8136962257787));
#442346=CARTESIAN_POINT('Ctrl Pts',(1.42525868962555,-2.3086056090344,13.8168830918626));
#442347=CARTESIAN_POINT('Ctrl Pts',(1.41336494437003,-2.32010879128777,
13.7902140179785));
#442348=CARTESIAN_POINT('Ctrl Pts',(1.42258613627193,-2.32706064869805,
13.802602731458));
#442349=CARTESIAN_POINT('Ctrl Pts',(1.43479835951331,-2.31576287210157,
13.8057746032558));
#442350=CARTESIAN_POINT('Origin',(1.39803682930555,-2.28101865049772,13.8235269408515));
#442351=CARTESIAN_POINT('Ctrl Pts',(1.33005753786835,-2.3306945761811,13.8235269408515));
#442352=CARTESIAN_POINT('Ctrl Pts',(1.33165381959632,-2.34239365748845,
13.8362179249168));
#442353=CARTESIAN_POINT('Ctrl Pts',(1.3153287054036,-2.34740899901737,13.8391868794938));
#442354=CARTESIAN_POINT('Ctrl Pts',(1.32859700956926,-2.31999042601557,
13.8400110824519));
#442355=CARTESIAN_POINT('Ctrl Pts',(1.32648724517256,-2.32983272031377,
13.8494522556837));
#442356=CARTESIAN_POINT('Ctrl Pts',(1.31303641355566,-2.32977779991724,
13.85569149686));
#442357=CARTESIAN_POINT('Ctrl Pts',(1.33319532685806,-2.30436182389777,
13.8586819406588));
#442358=CARTESIAN_POINT('Ctrl Pts',(1.32944672390595,-2.30657632599586,
13.868010383617));
#442359=CARTESIAN_POINT('Ctrl Pts',(1.32080977465871,-2.30387521983483,
13.8744918421245));
#442360=CARTESIAN_POINT('Ctrl Pts',(1.36015964510595,-2.28848740928262,
13.8587686893867));
#442361=CARTESIAN_POINT('Ctrl Pts',(1.36387485688658,-2.28629256775191,
13.8680909899357));
#442362=CARTESIAN_POINT('Ctrl Pts',(1.36569875138713,-2.2774511984939,13.8745789365163));
#442363=CARTESIAN_POINT('Ctrl Pts',(1.37615676386221,-2.29208006337928,
13.8400379222776));
#442364=CARTESIAN_POINT('Ctrl Pts',(1.38577616846632,-2.2950359539338,13.8494748685453));
#442365=CARTESIAN_POINT('Ctrl Pts',(1.39229259262045,-2.28327596577443,
13.8557104837033));
#442366=CARTESIAN_POINT('Ctrl Pts',(1.3847998046315,-2.29859082103775,13.8235269408542));
#442367=CARTESIAN_POINT('Ctrl Pts',(1.39423085364046,-2.30569518120467,
13.8362179249195));
#442368=CARTESIAN_POINT('Ctrl Pts',(1.40657750064357,-2.29389588835141,
13.8391868794965));
#442369=CARTESIAN_POINT('Origin',(1.30825951182031,-2.33366880892402,13.8235269408515));
#442370=CARTESIAN_POINT('Ctrl Pts',(1.33489241998041,-2.36612922842478,
13.7902140241682));
#442371=CARTESIAN_POINT('Ctrl Pts',(1.33645804584523,-2.37757070608477,
13.8026027327198));
#442372=CARTESIAN_POINT('Ctrl Pts',(1.32063625628023,-2.3827135561929,13.8057746032556));
#442373=CARTESIAN_POINT('Ctrl Pts',(1.33328131917051,-2.3543215386845,13.8013225161808));
#442374=CARTESIAN_POINT('Ctrl Pts',(1.33484534010834,-2.36575131411499,
13.8136962270464));
#442375=CARTESIAN_POINT('Ctrl Pts',(1.31904682993434,-2.37089385060931,
13.8168830918628));
#442376=CARTESIAN_POINT('Ctrl Pts',(1.33166952380057,-2.34250875854296,
13.8124254880875));
#442377=CARTESIAN_POINT('Ctrl Pts',(1.33323125293798,-2.35392179832831,
13.8247886461868));
#442378=CARTESIAN_POINT('Ctrl Pts',(1.3174569561759,-2.35906884834368,13.8279860620656));
#442379=CARTESIAN_POINT('Ctrl Pts',(1.33005700575208,-2.33069068192072,
13.8235227163065));
#442380=CARTESIAN_POINT('Ctrl Pts',(1.33161570818725,-2.34208160067013,
13.8358800595847));
#442381=CARTESIAN_POINT('Ctrl Pts',(1.31586661480737,-2.34723833301827,
13.8390832900376));
#442382=CARTESIAN_POINT('Origin',(1.31309492773411,-2.36910736775677,13.7902182540695));
#442383=CARTESIAN_POINT('Ctrl Pts',(1.33765857874362,-2.38640248748842,
13.7382347919292));
#442384=CARTESIAN_POINT('Ctrl Pts',(1.33972245318481,-2.40135100885424,
13.7369371795943));
#442385=CARTESIAN_POINT('Ctrl Pts',(1.32643138676074,-2.40862365145039,
13.7364597369712));
#442386=CARTESIAN_POINT('Ctrl Pts',(1.33791430348575,-2.38827668033879,
13.7595490285574));
#442387=CARTESIAN_POINT('Ctrl Pts',(1.34002642422511,-2.40358199812056,
13.7633824266926));
#442388=CARTESIAN_POINT('Ctrl Pts',(1.32696636829928,-2.41102031779116,
13.7648920890506));
#442389=CARTESIAN_POINT('Ctrl Pts',(1.33661012131854,-2.37871839947734,
13.7803806590111));
#442390=CARTESIAN_POINT('Ctrl Pts',(1.33844237793711,-2.39195621356006,
13.7901039518744));
#442391=CARTESIAN_POINT('Ctrl Pts',(1.32424259758171,-2.39880104221269,
13.7926933640892));
#442392=CARTESIAN_POINT('Ctrl Pts',(1.33434316150546,-2.36210397367384,
13.7936647693663));
#442393=CARTESIAN_POINT('Ctrl Pts',(1.33583501709958,-2.37281600890674,
13.8072068914933));
#442394=CARTESIAN_POINT('Ctrl Pts',(1.31947474257465,-2.37761034799738,
13.8104111085397));
#442395=CARTESIAN_POINT('Origin',(1.31589706303392,-2.38964409891906,13.7435492065112));
#442396=CARTESIAN_POINT('Origin',(1.31589706303392,-2.38964409891906,14.));
#442397=CARTESIAN_POINT('Origin',(1.31589706303392,-2.38964409891906,12.5369868989719));
#442398=CARTESIAN_POINT('Ctrl Pts',(1.35398984138342,-2.38615005398945,
12.506462012331));
#442399=CARTESIAN_POINT('Ctrl Pts',(1.35721678008233,-2.39183692084418,
12.4999388158272));
#442400=CARTESIAN_POINT('Ctrl Pts',(1.35717860116565,-2.39176963775142,
12.4907030323752));
#442401=CARTESIAN_POINT('Ctrl Pts',(1.34373179030501,-2.39457626139414,
12.5042014951932));
#442402=CARTESIAN_POINT('Ctrl Pts',(1.3416257647632,-2.400651271973,12.4980716682127));
#442403=CARTESIAN_POINT('Ctrl Pts',(1.33569497804863,-2.40396055198117,
12.4907355092744));
#442404=CARTESIAN_POINT('Ctrl Pts',(1.33839957825335,-2.39176677462936,
12.5218047446509));
#442405=CARTESIAN_POINT('Ctrl Pts',(1.33666884369345,-2.4034510986928,12.5216906929434));
#442406=CARTESIAN_POINT('Ctrl Pts',(1.32630962967192,-2.4090240188596,12.5161988840775));
#442407=CARTESIAN_POINT('Ctrl Pts',(1.33768986228266,-2.38663180728245,
12.5369868989719));
#442408=CARTESIAN_POINT('Ctrl Pts',(1.33978886682089,-2.40181731720043,
12.5369868989719));
#442409=CARTESIAN_POINT('Ctrl Pts',(1.32626989402292,-2.40904524262952,
12.5369868989719));
#442410=CARTESIAN_POINT('Origin',(2.60621061928497E-31,-9.59588718149404E-31,
12.5));
#442411=CARTESIAN_POINT('Origin',(1.51560512620467,-2.21452734525961,12.5));
#442412=CARTESIAN_POINT('',(1.51560512620467,-2.21452734525961,12.5893111709658));
#442413=CARTESIAN_POINT('',(1.51560512620467,-2.21452734525961,13.8235269408515));
#442414=CARTESIAN_POINT('',(1.51560512620467,-2.21452734525961,12.5));
#442415=CARTESIAN_POINT('',(1.5233130242113,-2.24945385392453,13.7902182540695));
#442416=CARTESIAN_POINT('',(1.51560512620467,-2.21452734525961,13.8235269408515));
#442417=CARTESIAN_POINT('',(1.5277797698805,-2.26969385076736,13.7435492065112));
#442418=CARTESIAN_POINT('Origin',(1.51308455377141,-2.20310445848677,13.7445212918701));
#442419=CARTESIAN_POINT('',(1.5277797698805,-2.26969385076736,12.5369868989719));
#442420=CARTESIAN_POINT('',(1.5277797698805,-2.26969385076736,12.5));
#442421=CARTESIAN_POINT('Ctrl Pts',(1.5277797698805,-2.26969385076736,12.5369868989719));
#442422=CARTESIAN_POINT('Ctrl Pts',(1.52372451513676,-2.25131842729605,
12.5544431401645));
#442423=CARTESIAN_POINT('Ctrl Pts',(1.51966635996705,-2.23292986123348,
12.5718848856037));
#442424=CARTESIAN_POINT('Ctrl Pts',(1.51560512620467,-2.21452734525961,
12.5893111709658));
#442425=CARTESIAN_POINT('Origin',(1.79995650094799,-2.32507696650954,12.5));
#442426=CARTESIAN_POINT('',(1.6152926497988,-2.20826874654631,13.7435492065112));
#442427=CARTESIAN_POINT('',(1.59777583112559,-2.19718856817949,13.7902182540695));
#442428=CARTESIAN_POINT('Origin',(1.55174465916705,-2.16807177447116,13.7418732680445));
#442429=CARTESIAN_POINT('',(1.56754848850677,-2.17806840977518,13.8235269408515));
#442430=CARTESIAN_POINT('',(1.59777583112559,-2.19718856817949,13.7902182540695));
#442431=CARTESIAN_POINT('',(1.56754848850677,-2.17806840977518,12.5893111709658));
#442432=CARTESIAN_POINT('',(1.56754848850677,-2.17806840977518,12.5));
#442433=CARTESIAN_POINT('',(1.6152926497988,-2.20826874654631,12.5369868989719));
#442434=CARTESIAN_POINT('Ctrl Pts',(1.56754848850677,-2.17806840977518,
12.5893111709658));
#442435=CARTESIAN_POINT('Ctrl Pts',(1.58347504906646,-2.18814267811485,
12.5718848856037));
#442436=CARTESIAN_POINT('Ctrl Pts',(1.59938953659725,-2.19820930971887,
12.5544431401645));
#442437=CARTESIAN_POINT('Ctrl Pts',(1.6152926497988,-2.20826874654631,12.5369868989719));
#442438=CARTESIAN_POINT('',(1.6152926497988,-2.20826874654631,12.5));
#442439=CARTESIAN_POINT('Origin',(1.54917241891497,-2.20711941133033,12.5));
#442440=CARTESIAN_POINT('',(1.52851837734599,-2.17964213455397,13.8587068136939));
#442441=CARTESIAN_POINT('Ctrl Pts',(1.56754848851018,-2.17806840976952,
13.8235269408542));
#442442=CARTESIAN_POINT('Ctrl Pts',(1.56606758606871,-2.17713167214031,
13.8262006681044));
#442443=CARTESIAN_POINT('Ctrl Pts',(1.56445922181571,-2.17631988863365,
13.8288634856214));
#442444=CARTESIAN_POINT('Ctrl Pts',(1.56273388295384,-2.17562482367861,
13.8314912288862));
#442445=CARTESIAN_POINT('Ctrl Pts',(1.5609552365477,-2.17490828340259,13.8342001611531));
#442446=CARTESIAN_POINT('Ctrl Pts',(1.5590504856072,-2.17431452878308,13.8368750301949));
#442447=CARTESIAN_POINT('Ctrl Pts',(1.55699766102132,-2.17386492858581,
13.8394886372969));
#442448=CARTESIAN_POINT('Ctrl Pts',(1.5568391163991,-2.173830204872,13.8396904925131));
#442449=CARTESIAN_POINT('Ctrl Pts',(1.55667968014485,-2.17379636151293,
13.8398919674349));
#442450=CARTESIAN_POINT('Ctrl Pts',(1.55651933874679,-2.17376341928281,
13.8400930404591));
#442451=CARTESIAN_POINT('Ctrl Pts',(1.55402111189254,-2.17325015717513,
13.8432258934518));
#442452=CARTESIAN_POINT('Ctrl Pts',(1.55131612875077,-2.17295716726792,
13.8462331177034));
#442453=CARTESIAN_POINT('Ctrl Pts',(1.54848222334066,-2.17298991066604,
13.8489036603661));
#442454=CARTESIAN_POINT('Ctrl Pts',(1.54755493651065,-2.17300062468696,
13.8497774930041));
#442455=CARTESIAN_POINT('Ctrl Pts',(1.54661405697649,-2.17304634862749,
13.85061494757));
#442456=CARTESIAN_POINT('Ctrl Pts',(1.54566291962783,-2.17313115116021,
13.8514076489583));
#442457=CARTESIAN_POINT('Ctrl Pts',(1.54365112696084,-2.17331052074727,
13.8530843267192));
#442458=CARTESIAN_POINT('Ctrl Pts',(1.54139609421675,-2.17368528658119,
13.8546805203176));
#442459=CARTESIAN_POINT('Ctrl Pts',(1.53905107190559,-2.17436829697483,
13.8559412814274));
#442460=CARTESIAN_POINT('Ctrl Pts',(1.5387372318695,-2.17445970591605,13.8561100121513));
#442461=CARTESIAN_POINT('Ctrl Pts',(1.53842181144662,-2.17455656576237,
13.8562727473908));
#442462=CARTESIAN_POINT('Ctrl Pts',(1.53810520011653,-2.17465907447112,
13.8564289040185));
#442463=CARTESIAN_POINT('Ctrl Pts',(1.53666937134654,-2.17512395029587,
13.8571370725437));
#442464=CARTESIAN_POINT('Ctrl Pts',(1.53518451357584,-2.17571533827384,
13.8577210840553));
#442465=CARTESIAN_POINT('Ctrl Pts',(1.5337192026214,-2.17643751617089,13.8581177131616));
#442466=CARTESIAN_POINT('Ctrl Pts',(1.53330652062216,-2.17664090632331,
13.8582294175695));
#442467=CARTESIAN_POINT('Ctrl Pts',(1.5328953432531,-2.17685449885373,13.8583265086086));
#442468=CARTESIAN_POINT('Ctrl Pts',(1.53248706394703,-2.1770779721128,13.8584082369006));
#442469=CARTESIAN_POINT('Ctrl Pts',(1.53190047606862,-2.17739904325937,
13.8585256585398));
#442470=CARTESIAN_POINT('Ctrl Pts',(1.53131273294775,-2.17774478549668,
13.8586122832068));
#442471=CARTESIAN_POINT('Ctrl Pts',(1.53073950284391,-2.17810689809613,
13.8586682984299));
#442472=CARTESIAN_POINT('Ctrl Pts',(1.53028097558332,-2.17839655228062,
13.8587131050557));
#442473=CARTESIAN_POINT('Ctrl Pts',(1.52982654468516,-2.17869968189244,
13.8587357943552));
#442474=CARTESIAN_POINT('Ctrl Pts',(1.52937643718902,-2.17901674426501,
13.8587355499465));
#442475=CARTESIAN_POINT('Ctrl Pts',(1.52908552198329,-2.17922166923547,
13.8587353919793));
#442476=CARTESIAN_POINT('Ctrl Pts',(1.52879953645905,-2.17943016675381,
13.8587257282814));
#442477=CARTESIAN_POINT('Ctrl Pts',(1.52851837734599,-2.17964213455397,
13.8587068136939));
#442478=CARTESIAN_POINT('Ctrl Pts',(1.52851837734599,-2.17964213455397,
13.8587068136939));
#442479=CARTESIAN_POINT('Ctrl Pts',(1.52759366035041,-2.18033928509337,
13.8586446046466));
#442480=CARTESIAN_POINT('Ctrl Pts',(1.52672108644886,-2.18107392841697,
13.858482427929));
#442481=CARTESIAN_POINT('Ctrl Pts',(1.52589754886275,-2.18184284988884,
13.8582284286032));
#442482=CARTESIAN_POINT('Ctrl Pts',(1.5250526950973,-2.1826316738743,13.8579678548414));
#442483=CARTESIAN_POINT('Ctrl Pts',(1.52425843051278,-2.18345961987124,
13.857615680862));
#442484=CARTESIAN_POINT('Ctrl Pts',(1.52353907601848,-2.18428733879638,
13.8571944833187));
#442485=CARTESIAN_POINT('Ctrl Pts',(1.5217438533084,-2.18635299602621,13.8561433417727));
#442486=CARTESIAN_POINT('Ctrl Pts',(1.52032757852607,-2.18851071837825,
13.8546163505475));
#442487=CARTESIAN_POINT('Ctrl Pts',(1.51923450966278,-2.19056138102956,
13.8528973491086));
#442488=CARTESIAN_POINT('Ctrl Pts',(1.51903482210818,-2.19093600684125,
13.8525833129073));
#442489=CARTESIAN_POINT('Ctrl Pts',(1.5188457798754,-2.1913070583044,13.8522628768812));
#442490=CARTESIAN_POINT('Ctrl Pts',(1.51866686623345,-2.19167334761887,
13.851937733538));
#442491=CARTESIAN_POINT('Ctrl Pts',(1.51757426544519,-2.19391022564192,
13.8499521282529));
#442492=CARTESIAN_POINT('Ctrl Pts',(1.51675447834592,-2.19619359876534,
13.847639871647));
#442493=CARTESIAN_POINT('Ctrl Pts',(1.51617497488795,-2.19837631368465,
13.8452109780794));
#442494=CARTESIAN_POINT('Ctrl Pts',(1.51591424428709,-2.19935836230681,
13.8441181685877));
#442495=CARTESIAN_POINT('Ctrl Pts',(1.51570143934861,-2.20032010192919,
13.8430021611332));
#442496=CARTESIAN_POINT('Ctrl Pts',(1.51553056054347,-2.20124944394279,
13.8418824960098));
#442497=CARTESIAN_POINT('Ctrl Pts',(1.51512788027559,-2.20343946212943,
13.8392439765549));
#442498=CARTESIAN_POINT('Ctrl Pts',(1.51493505499432,-2.20555357768276,
13.8364981347964));
#442499=CARTESIAN_POINT('Ctrl Pts',(1.51491749568044,-2.20759427332479,
13.8336931113419));
#442500=CARTESIAN_POINT('Ctrl Pts',(1.51490039402384,-2.20958178128397,
13.8309611966328));
#442501=CARTESIAN_POINT('Ctrl Pts',(1.51505008856863,-2.21150164312281,
13.8281701127186));
#442502=CARTESIAN_POINT('Ctrl Pts',(1.51537135352457,-2.21334217022334,
13.8253580685121));
#442503=CARTESIAN_POINT('Ctrl Pts',(1.51544100411374,-2.2137411984851,13.8247484142933));
#442504=CARTESIAN_POINT('Ctrl Pts',(1.51551884400471,-2.21413637796842,
13.8241378483365));
#442505=CARTESIAN_POINT('Ctrl Pts',(1.51560512620467,-2.21452734525961,
13.8235269408515));
#442506=CARTESIAN_POINT('',(1.52952454255909,-2.17891384311432,12.5969504640361));
#442507=CARTESIAN_POINT('Origin',(1.54919126636332,-2.2071466042798,12.584524458991));
#442508=CARTESIAN_POINT('Origin',(1.54919126636332,-2.2071466042798,12.584524458991));
#442509=CARTESIAN_POINT('Ctrl Pts',(1.56754848850677,-2.17806840977518,
12.5893111709658));
#442510=CARTESIAN_POINT('Ctrl Pts',(1.55796993226768,-2.17200954066169,
12.5770542771492));
#442511=CARTESIAN_POINT('Ctrl Pts',(1.54679665878455,-2.18396619715613,
12.5737548217797));
#442512=CARTESIAN_POINT('Ctrl Pts',(1.58849357634264,-2.19131712310947,
12.5663937883685));
#442513=CARTESIAN_POINT('Ctrl Pts',(1.57890280132482,-2.18525052506698,
12.5540940315304));
#442514=CARTESIAN_POINT('Ctrl Pts',(1.56769725034417,-2.19724642530556,
12.5508374392248));
#442515=CARTESIAN_POINT('Ctrl Pts',(1.60941753084162,-2.2045524686544,12.5434499600945));
#442516=CARTESIAN_POINT('Ctrl Pts',(1.5997955727989,-2.1984661459413,12.5311293540533));
#442517=CARTESIAN_POINT('Ctrl Pts',(1.58857805433939,-2.21051268254624,
12.5278936106989));
#442518=CARTESIAN_POINT('Ctrl Pts',(1.63032200740699,-2.21777549352727,
12.5204817579905));
#442519=CARTESIAN_POINT('Ctrl Pts',(1.62065242724761,-2.21165904767617,
12.5081597038247));
#442520=CARTESIAN_POINT('Ctrl Pts',(1.60944061616698,-2.22376604305847,
12.5049254088044));
#442521=CARTESIAN_POINT('Ctrl Pts',(1.6152926497988,-2.20826874654631,12.5369868989719));
#442522=CARTESIAN_POINT('Ctrl Pts',(1.61607988308113,-2.20876670731779,
12.5342545179733));
#442523=CARTESIAN_POINT('Ctrl Pts',(1.61676449626765,-2.20934736375511,
12.5314872231885));
#442524=CARTESIAN_POINT('Ctrl Pts',(1.61727176563758,-2.21002063851066,
12.5287124745063));
#442525=CARTESIAN_POINT('Ctrl Pts',(1.61772924633399,-2.21062783110359,
12.5262100684184));
#442526=CARTESIAN_POINT('Ctrl Pts',(1.6180412402908,-2.21131033246523,12.5237004536639));
#442527=CARTESIAN_POINT('Ctrl Pts',(1.61815281477188,-2.21210742198755,
12.5212220730815));
#442528=CARTESIAN_POINT('Ctrl Pts',(1.61823823468911,-2.21271766297064,
12.5193246583486));
#442529=CARTESIAN_POINT('Ctrl Pts',(1.61820657663425,-2.21340244789356,
12.517417831369));
#442530=CARTESIAN_POINT('Ctrl Pts',(1.61796173605729,-2.21417653948722,
12.5155812248347));
#442531=CARTESIAN_POINT('Ctrl Pts',(1.61785743265549,-2.21450630666688,
12.5147988205793));
#442532=CARTESIAN_POINT('Ctrl Pts',(1.61771459901015,-2.21485269957456,
12.5140295443047));
#442533=CARTESIAN_POINT('Ctrl Pts',(1.61752711876154,-2.21521853274585,
12.5132817086137));
#442534=CARTESIAN_POINT('Ctrl Pts',(1.61724339276703,-2.21577217176181,
12.5121499604604));
#442535=CARTESIAN_POINT('Ctrl Pts',(1.61684492242763,-2.21637902800959,
12.5110494206568));
#442536=CARTESIAN_POINT('Ctrl Pts',(1.6162956560146,-2.21702976491589,12.5100666561695));
#442537=CARTESIAN_POINT('Ctrl Pts',(1.61598026850509,-2.21740341654897,
12.5095023550641));
#442538=CARTESIAN_POINT('Ctrl Pts',(1.61561102025558,-2.21779543193857,
12.5089719619137));
#442539=CARTESIAN_POINT('Ctrl Pts',(1.61519018315096,-2.2181940839401,12.5085043804652));
#442540=CARTESIAN_POINT('Ctrl Pts',(1.61457434286623,-2.21877745921626,
12.5078201359221));
#442541=CARTESIAN_POINT('Ctrl Pts',(1.61382933553101,-2.21939108946418,
12.5072563000953));
#442542=CARTESIAN_POINT('Ctrl Pts',(1.61300027925851,-2.21998684485305,
12.5068768744336));
#442543=CARTESIAN_POINT('Ctrl Pts',(1.6124024726136,-2.22041642550037,12.5066032824118));
#442544=CARTESIAN_POINT('Ctrl Pts',(1.61175049802467,-2.2208443081451,12.5064197834844));
#442545=CARTESIAN_POINT('Ctrl Pts',(1.61108218170166,-2.22124875973636,
12.5063282718343));
#442546=CARTESIAN_POINT('Ctrl Pts',(1.61010664677556,-2.22183913384456,
12.5061946931565));
#442547=CARTESIAN_POINT('Ctrl Pts',(1.60907599162941,-2.22239311078423,
12.5062515701262));
#442548=CARTESIAN_POINT('Ctrl Pts',(1.60806150210968,-2.22288993130823,
12.5064436508398));
#442549=CARTESIAN_POINT('',(1.54679665878455,-2.18396619715613,12.5737548217797));
#442550=CARTESIAN_POINT('Origin',(1.55578780396802,-2.19666105077048,12.5893111709658));
#442551=CARTESIAN_POINT('Ctrl Pts',(1.60806150210968,-2.22288993130823,
12.5064436508398));
#442552=CARTESIAN_POINT('Ctrl Pts',(1.59899245595975,-2.21712861291036,
12.5164271754438));
#442553=CARTESIAN_POINT('Ctrl Pts',(1.58991992687748,-2.21136483436914,
12.5264061185523));
#442554=CARTESIAN_POINT('Ctrl Pts',(1.58084379168938,-2.2055985098393,12.536380305637));
#442555=CARTESIAN_POINT('Ctrl Pts',(1.56950046354282,-2.19839177371363,
12.5488460165097));
#442556=CARTESIAN_POINT('Ctrl Pts',(1.55815149934638,-2.19118105862217,
12.5613043021964));
#442557=CARTESIAN_POINT('Ctrl Pts',(1.54679665878455,-2.18396619715613,
12.5737548217797));
#442558=CARTESIAN_POINT('Ctrl Pts',(1.51560512620467,-2.21452734525961,
12.5893111709658));
#442559=CARTESIAN_POINT('Ctrl Pts',(1.51316261792755,-2.20345969926437,
12.5770542771492));
#442560=CARTESIAN_POINT('Ctrl Pts',(1.52820511637882,-2.19701556121508,
12.5737548217797));
#442561=CARTESIAN_POINT('Ctrl Pts',(1.51332628722593,-2.20420132780736,
12.5928319619712));
#442562=CARTESIAN_POINT('Ctrl Pts',(1.51486596642762,-2.19606113098374,
12.5821634970843));
#442563=CARTESIAN_POINT('Ctrl Pts',(1.52736577342746,-2.19325607710428,
12.5773203894503));
#442564=CARTESIAN_POINT('Ctrl Pts',(1.51686794509426,-2.1878293774384,12.5969440695591));
#442565=CARTESIAN_POINT('Ctrl Pts',(1.52014759929905,-2.18550506875648,
12.5878292599214));
#442566=CARTESIAN_POINT('Ctrl Pts',(1.52863009228486,-2.18742121250222,
12.5813877129824));
#442567=CARTESIAN_POINT('Ctrl Pts',(1.54188060042453,-2.17020716648546,
12.596957478804));
#442568=CARTESIAN_POINT('Ctrl Pts',(1.538625230093,-2.1725143633027,12.5878468778671));
#442569=CARTESIAN_POINT('Ctrl Pts',(1.53758590394018,-2.18111885533219,
12.5814011370086));
#442570=CARTESIAN_POINT('Ctrl Pts',(1.55859880275859,-2.17240732962884,
12.5928371701607));
#442571=CARTESIAN_POINT('Ctrl Pts',(1.55042480839402,-2.17109550577187,
12.5821692192952));
#442572=CARTESIAN_POINT('Ctrl Pts',(1.54353601874319,-2.18189219040719,
12.5773318885715));
#442573=CARTESIAN_POINT('Ctrl Pts',(1.56754848850679,-2.17806840977513,
12.5893111709658));
#442574=CARTESIAN_POINT('Ctrl Pts',(1.55796993226771,-2.17200954066164,
12.5770542771492));
#442575=CARTESIAN_POINT('Ctrl Pts',(1.54679665878457,-2.18396619715608,
12.5737548217797));
#442576=CARTESIAN_POINT('',(1.52820511637882,-2.19701556121508,12.5737548217797));
#442577=CARTESIAN_POINT('Origin',(1.53708819353926,-2.20978626754487,12.5893111709658));
#442578=CARTESIAN_POINT('Ctrl Pts',(1.54679665878457,-2.18396619715608,
12.5737548217797));
#442579=CARTESIAN_POINT('Ctrl Pts',(1.545967639159,-2.18340312869539,12.5746934679442));
#442580=CARTESIAN_POINT('Ctrl Pts',(1.54494735050147,-2.18293159238338,
12.5756680099006));
#442581=CARTESIAN_POINT('Ctrl Pts',(1.54385326969933,-2.18260221286617,
12.5765688348656));
#442582=CARTESIAN_POINT('Ctrl Pts',(1.54356362391883,-2.18251501328534,
12.5768073183026));
#442583=CARTESIAN_POINT('Ctrl Pts',(1.54326893808177,-2.18243755628029,
12.5770407398754));
#442584=CARTESIAN_POINT('Ctrl Pts',(1.54297154987649,-2.18237024061894,
12.5772674179684));
#442585=CARTESIAN_POINT('Ctrl Pts',(1.54175114909918,-2.18209399534766,
12.5781976435658));
#442586=CARTESIAN_POINT('Ctrl Pts',(1.54041343275203,-2.18198384791316,
12.5790594849312));
#442587=CARTESIAN_POINT('Ctrl Pts',(1.53904476283533,-2.18209536196077,
12.5797571720116));
#442588=CARTESIAN_POINT('Ctrl Pts',(1.53815302517162,-2.18216801737248,
12.580211740231));
#442589=CARTESIAN_POINT('Ctrl Pts',(1.53720914730193,-2.18235678057714,
12.5806009430798));
#442590=CARTESIAN_POINT('Ctrl Pts',(1.53628304843442,-2.18266573615955,
12.5808812374708));
#442591=CARTESIAN_POINT('Ctrl Pts',(1.53548722227712,-2.18293123149979,
12.5811221033394));
#442592=CARTESIAN_POINT('Ctrl Pts',(1.53468826847797,-2.18329102669088,
12.581287365893));
#442593=CARTESIAN_POINT('Ctrl Pts',(1.53393470499476,-2.18373241694931,
12.581359338449));
#442594=CARTESIAN_POINT('Ctrl Pts',(1.53382997523109,-2.18379376108087,
12.5813693411482));
#442595=CARTESIAN_POINT('Ctrl Pts',(1.53372607644035,-2.18385664261584,
12.5813775999465));
#442596=CARTESIAN_POINT('Ctrl Pts',(1.53362309129939,-2.1839209887146,12.5813841266931));
#442597=CARTESIAN_POINT('Ctrl Pts',(1.53344836455195,-2.18403015965366,
12.5813952001081));
#442598=CARTESIAN_POINT('Ctrl Pts',(1.53327542016041,-2.18414479391356,
12.5814007534795));
#442599=CARTESIAN_POINT('Ctrl Pts',(1.53310444240399,-2.18426500594565,
12.5814005856065));
#442600=CARTESIAN_POINT('Ctrl Pts',(1.5323217730831,-2.18481528962869,12.5813998171494));
#442601=CARTESIAN_POINT('Ctrl Pts',(1.53163419595105,-2.18544415629832,
12.58127954464));
#442602=CARTESIAN_POINT('Ctrl Pts',(1.53102564474814,-2.18612620141454,
12.5810700125799));
#442603=CARTESIAN_POINT('Ctrl Pts',(1.53029058418412,-2.18695003425788,
12.5808169217085));
#442604=CARTESIAN_POINT('Ctrl Pts',(1.52968324294109,-2.18786267053481,
12.5804173076348));
#442605=CARTESIAN_POINT('Ctrl Pts',(1.52923516695681,-2.18876970045712,
12.5799304713245));
#442606=CARTESIAN_POINT('Ctrl Pts',(1.52867985965379,-2.18989379627475,
12.5793271277669));
#442607=CARTESIAN_POINT('Ctrl Pts',(1.52830585165326,-2.19106474923022,
12.5785808224116));
#442608=CARTESIAN_POINT('Ctrl Pts',(1.52809869499393,-2.19222355118979,
12.5777485681082));
#442609=CARTESIAN_POINT('Ctrl Pts',(1.52779000887583,-2.19395029306578,
12.576508418016));
#442610=CARTESIAN_POINT('Ctrl Pts',(1.52784763807624,-2.19563430565066,
12.5750928681475));
#442611=CARTESIAN_POINT('Ctrl Pts',(1.52820511637882,-2.19701556121508,
12.5737548217797));
#442612=CARTESIAN_POINT('Ctrl Pts',(1.52820511637882,-2.19701556121508,
12.5737548217797));
#442613=CARTESIAN_POINT('Ctrl Pts',(1.51316261792755,-2.20345969926437,
12.5770542771492));
#442614=CARTESIAN_POINT('Ctrl Pts',(1.51560512620467,-2.21452734525961,
12.5893111709658));
#442615=CARTESIAN_POINT('Ctrl Pts',(1.53359001553651,-2.22118202175923,
12.5508408821982));
#442616=CARTESIAN_POINT('Ctrl Pts',(1.51849964539203,-2.22764317131114,
12.55409748406));
#442617=CARTESIAN_POINT('Ctrl Pts',(1.52094526968415,-2.23872493678811,
12.5663972313419));
#442618=CARTESIAN_POINT('Ctrl Pts',(1.538968503048,-2.24532513124994,12.52790050457));
#442619=CARTESIAN_POINT('Ctrl Pts',(1.52382645117862,-2.25178032625288,
12.5311362602938));
#442620=CARTESIAN_POINT('Ctrl Pts',(1.52628002583636,-2.26289811692294,
12.5434568539655));
#442621=CARTESIAN_POINT('Ctrl Pts',(1.54434106366399,-2.26944670737555,
12.5049357605811));
#442622=CARTESIAN_POINT('Ctrl Pts',(1.52914410084493,-2.27587599241087,
12.5081700652078));
#442623=CARTESIAN_POINT('Ctrl Pts',(1.53160981659786,-2.28704879756943,
12.5204921097672));
#442624=CARTESIAN_POINT('Ctrl Pts',(1.54398827872498,-2.26786279047851,
12.5064436508395));
#442625=CARTESIAN_POINT('Ctrl Pts',(1.54311111065669,-2.26871097911941,
12.5062361689309));
#442626=CARTESIAN_POINT('Ctrl Pts',(1.54216275899901,-2.26955562150162,
12.5061871075061));
#442627=CARTESIAN_POINT('Ctrl Pts',(1.5412003190334,-2.270320295258,12.5063648335164));
#442628=CARTESIAN_POINT('Ctrl Pts',(1.54076311943526,-2.27066765724518,
12.5064455676329));
#442629=CARTESIAN_POINT('Ctrl Pts',(1.5403167775862,-2.27100318989256,12.506574497099));
#442630=CARTESIAN_POINT('Ctrl Pts',(1.53987979978177,-2.271311666509,12.5067492519495));
#442631=CARTESIAN_POINT('Ctrl Pts',(1.53900167592157,-2.27193156224391,
12.5071004286051));
#442632=CARTESIAN_POINT('Ctrl Pts',(1.53812861480944,-2.27246433017317,
12.5076537929612));
#442633=CARTESIAN_POINT('Ctrl Pts',(1.53733107118647,-2.27287805715525,
12.5083435010503));
#442634=CARTESIAN_POINT('Ctrl Pts',(1.53728086104917,-2.27290410374127,
12.5083869222963));
#442635=CARTESIAN_POINT('Ctrl Pts',(1.53723093925072,-2.27292967076007,
12.5084308732336));
#442636=CARTESIAN_POINT('Ctrl Pts',(1.53718131867551,-2.2729547474142,12.5084753333615));
#442637=CARTESIAN_POINT('Ctrl Pts',(1.53678329616976,-2.27315589527817,
12.508831962269));
#442638=CARTESIAN_POINT('Ctrl Pts',(1.53639715621091,-2.27333072734357,
12.509227847131));
#442639=CARTESIAN_POINT('Ctrl Pts',(1.53603553566535,-2.27347659572089,
12.5096423454524));
#442640=CARTESIAN_POINT('Ctrl Pts',(1.53490237692214,-2.27393368265681,
12.5109411997424));
#442641=CARTESIAN_POINT('Ctrl Pts',(1.53394389914738,-2.27414345025429,
12.5124831113042));
#442642=CARTESIAN_POINT('Ctrl Pts',(1.53314148551678,-2.27419868467208,
12.5140723025007));
#442643=CARTESIAN_POINT('Ctrl Pts',(1.53306629848073,-2.27420386019752,
12.5142212114565));
#442644=CARTESIAN_POINT('Ctrl Pts',(1.53299246601335,-2.27420770406637,
12.5143705582413));
#442645=CARTESIAN_POINT('Ctrl Pts',(1.5329199651673,-2.27421030778361,12.5145201959299));
#442646=CARTESIAN_POINT('Ctrl Pts',(1.53198858385732,-2.27424375640805,
12.5164425148273));
#442647=CARTESIAN_POINT('Ctrl Pts',(1.53124543592119,-2.2740844173846,12.5184635205941));
#442648=CARTESIAN_POINT('Ctrl Pts',(1.53062936502989,-2.27379860724189,
12.5205025929157));
#442649=CARTESIAN_POINT('Ctrl Pts',(1.53027201949417,-2.27363282603066,
12.5216853356836));
#442650=CARTESIAN_POINT('Ctrl Pts',(1.52995787053018,-2.27342523223747,
12.5228750347131));
#442651=CARTESIAN_POINT('Ctrl Pts',(1.52967956332561,-2.27319252437676,
12.5240609649613));
#442652=CARTESIAN_POINT('Ctrl Pts',(1.52899647322267,-2.27262135541698,
12.5269717671326));
#442653=CARTESIAN_POINT('Ctrl Pts',(1.52851674841753,-2.27187484145228,
12.5299036066169));
#442654=CARTESIAN_POINT('Ctrl Pts',(1.52817596761428,-2.27101094298007,
12.5328133004019));
#442655=CARTESIAN_POINT('Ctrl Pts',(1.52801237298565,-2.2705962214101,12.5342101228451));
#442656=CARTESIAN_POINT('Ctrl Pts',(1.52788149046078,-2.27015477303107,
12.5356023438238));
#442657=CARTESIAN_POINT('Ctrl Pts',(1.5277797698805,-2.26969385076736,12.5369868989719));
#442658=CARTESIAN_POINT('Origin',(4.26941344976037,-14.7173397586424,-1.24076534767543));
#442659=CARTESIAN_POINT('Ctrl Pts',(1.61525734986217,-2.20824637076874,
12.5369868989719));
#442660=CARTESIAN_POINT('Ctrl Pts',(1.62820500073349,-2.21647082458671,
12.5369868989719));
#442661=CARTESIAN_POINT('Ctrl Pts',(1.64039921308345,-2.20716574592753,
12.5369868989719));
#442662=CARTESIAN_POINT('Ctrl Pts',(1.61963419773785,-2.21102650192599,
12.5218025310016));
#442663=CARTESIAN_POINT('Ctrl Pts',(1.63098686305326,-2.21430870453147,
12.5216901060418));
#442664=CARTESIAN_POINT('Ctrl Pts',(1.64036205108736,-2.20719412400173,
12.5161920673678));
#442665=CARTESIAN_POINT('Ctrl Pts',(1.61997710948733,-2.21704468127927,
12.5042015548895));
#442666=CARTESIAN_POINT('Ctrl Pts',(1.62638090394062,-2.21765193873491,
12.4980677368514));
#442667=CARTESIAN_POINT('Ctrl Pts',(1.63185780741435,-2.21362772352397,
12.4907278922777));
#442668=CARTESIAN_POINT('Ctrl Pts',(1.60804977900648,-2.22287372599554,
12.5064636261921));
#442669=CARTESIAN_POINT('Ctrl Pts',(1.6118846290859,-2.22817479788771,12.4999376786892));
#442670=CARTESIAN_POINT('Ctrl Pts',(1.61183779196805,-2.2281100530023,12.4906970594712));
#442671=CARTESIAN_POINT('Origin',(1.62705333433755,-2.18967610555101,12.5369868989719));
#442672=CARTESIAN_POINT('Origin',(1.62705333433755,-2.18967610555102,14.));
#442673=CARTESIAN_POINT('Origin',(1.62705333433755,-2.18967610555102,13.7435492065112));
#442674=CARTESIAN_POINT('Ctrl Pts',(1.59436740412112,-2.19503255214519,
13.793642941384));
#442675=CARTESIAN_POINT('Ctrl Pts',(1.60349052959503,-2.20083555142084,
13.8071662555867));
#442676=CARTESIAN_POINT('Ctrl Pts',(1.61464388732173,-2.18796613049156,
13.8103758687955));
#442677=CARTESIAN_POINT('Ctrl Pts',(1.6084142461289,-2.20391781718522,13.7804579775006));
#442678=CARTESIAN_POINT('Ctrl Pts',(1.61967680095876,-2.21106963726357,
13.7901904343351));
#442679=CARTESIAN_POINT('Ctrl Pts',(1.6317863968244,-2.20098927952511,13.7927914348262));
#442680=CARTESIAN_POINT('Ctrl Pts',(1.61668415068134,-2.20914890707229,
13.7597120340895));
#442681=CARTESIAN_POINT('Ctrl Pts',(1.62972117020784,-2.21742073950764,
13.7635825532445));
#442682=CARTESIAN_POINT('Ctrl Pts',(1.64191077856844,-2.20864866083957,
13.7651073818884));
#442683=CARTESIAN_POINT('Ctrl Pts',(1.61506471401112,-2.20812453989338,
13.7381884353898));
#442684=CARTESIAN_POINT('Ctrl Pts',(1.62779609625867,-2.21620351363346,
13.7368803041982));
#442685=CARTESIAN_POINT('Ctrl Pts',(1.63992842196115,-2.2071483322345,13.7363986145813));
#442686=CARTESIAN_POINT('Origin',(1.60953651566434,-2.1785959271842,13.7902182540695));
#442687=CARTESIAN_POINT('Ctrl Pts',(1.56754516235229,-2.17806630493435,
13.8235227101244));
#442688=CARTESIAN_POINT('Ctrl Pts',(1.57725919850684,-2.1842161171191,13.8358800583119));
#442689=CARTESIAN_POINT('Ctrl Pts',(1.5884923415371,-2.17203241707691,13.8390832900376));
#442690=CARTESIAN_POINT('Ctrl Pts',(1.57762539875787,-2.1844425093933,13.8124254819052));
#442691=CARTESIAN_POINT('Ctrl Pts',(1.58735829958171,-2.19060426419111,
13.8247886449158));
#442692=CARTESIAN_POINT('Ctrl Pts',(1.59859310511821,-2.17839361614691,
13.8279860620657));
#442693=CARTESIAN_POINT('Ctrl Pts',(1.58770111752941,-2.19081585624484,
13.8013225099955));
#442694=CARTESIAN_POINT('Ctrl Pts',(1.59744828958404,-2.19698664799067,
13.8136962257787));
#442695=CARTESIAN_POINT('Ctrl Pts',(1.60868904809652,-2.1847520996563,13.8168830918626));
#442696=CARTESIAN_POINT('Ctrl Pts',(1.59777249444115,-2.19718645667412,
13.7902140179785));
#442697=CARTESIAN_POINT('Ctrl Pts',(1.60752964450452,-2.20336356960699,
13.802602731458));
#442698=CARTESIAN_POINT('Ctrl Pts',(1.61878035890445,-2.19110797586321,
13.8057746032558));
#442699=CARTESIAN_POINT('Origin',(1.57930917304552,-2.15947576877988,13.8235269408515));
#442700=CARTESIAN_POINT('Ctrl Pts',(1.51560512620467,-2.21452734525961,
13.8235269408515));
#442701=CARTESIAN_POINT('Ctrl Pts',(1.51814968017239,-2.22605738705903,
13.8362179249168));
#442702=CARTESIAN_POINT('Ctrl Pts',(1.50228768334518,-2.23238668881442,
13.8391868794938));
#442703=CARTESIAN_POINT('Ctrl Pts',(1.51327697008203,-2.20397785888597,
13.8400110824519));
#442704=CARTESIAN_POINT('Ctrl Pts',(1.51197646410904,-2.21395936914624,
13.8494522556837));
#442705=CARTESIAN_POINT('Ctrl Pts',(1.49856591250255,-2.21500099914103,
13.85569149686));
#442706=CARTESIAN_POINT('Ctrl Pts',(1.51658611068793,-2.18802645410473,
13.8586819406588));
#442707=CARTESIAN_POINT('Ctrl Pts',(1.51303048338233,-2.1905391335707,13.868010383617));
#442708=CARTESIAN_POINT('Ctrl Pts',(1.50420210764325,-2.18855100666276,
13.8744918421245));
#442709=CARTESIAN_POINT('Ctrl Pts',(1.54216679522923,-2.17000701803294,
13.8587686893867));
#442710=CARTESIAN_POINT('Ctrl Pts',(1.54569074498848,-2.1675166554059,13.8680909899357));
#442711=CARTESIAN_POINT('Ctrl Pts',(1.54678791695674,-2.15855604074073,
13.8745789365163));
#442712=CARTESIAN_POINT('Ctrl Pts',(1.55840351955395,-2.17228380418083,
13.8400379222776));
#442713=CARTESIAN_POINT('Ctrl Pts',(1.56823184890414,-2.17444578847591,
13.8494748685453));
#442714=CARTESIAN_POINT('Ctrl Pts',(1.57376804198508,-2.16219378164295,
13.8557104837033));
#442715=CARTESIAN_POINT('Ctrl Pts',(1.56754848851018,-2.17806840976952,
13.8235269408542));
#442716=CARTESIAN_POINT('Ctrl Pts',(1.57752722778883,-2.18438041271623,
13.8362179249195));
#442717=CARTESIAN_POINT('Ctrl Pts',(1.58887104043573,-2.17161401468514,
13.8391868794965));
#442718=CARTESIAN_POINT('Origin',(1.49412205887007,-2.21926842297435,13.8235269408515));
#442719=CARTESIAN_POINT('Ctrl Pts',(1.52331217376247,-2.24945000384412,
13.7902140241683));
#442720=CARTESIAN_POINT('Ctrl Pts',(1.52580517678315,-2.2607257978885,13.8026027327198));
#442721=CARTESIAN_POINT('Ctrl Pts',(1.51045522294544,-2.26714115831902,
13.8057746032556));
#442722=CARTESIAN_POINT('Ctrl Pts',(1.52074399742653,-2.23781292289012,
13.8013225161808));
#442723=CARTESIAN_POINT('Ctrl Pts',(1.52323444702014,-2.24907718445967,
13.8136962270464));
#442724=CARTESIAN_POINT('Ctrl Pts',(1.50790766955073,-2.25549033483342,
13.8168830918628));
#442725=CARTESIAN_POINT('Ctrl Pts',(1.51817471392669,-2.22617082508583,
13.8124254880875));
#442726=CARTESIAN_POINT('Ctrl Pts',(1.5206615152352,-2.23741859349969,13.8247886461867));
#442727=CARTESIAN_POINT('Ctrl Pts',(1.50535923850348,-2.24383426875828,
13.8279860620656));
#442728=CARTESIAN_POINT('Ctrl Pts',(1.5156042784406,-2.21452350732949,13.8235227163065));
#442729=CARTESIAN_POINT('Ctrl Pts',(1.51808626004819,-2.22574947501768,
13.8358800595847));
#442730=CARTESIAN_POINT('Ctrl Pts',(1.50280989203648,-2.23217274608223,
13.8390832900376));
#442731=CARTESIAN_POINT('Origin',(1.50182995687671,-2.25419493163927,13.7902182540695));
#442732=CARTESIAN_POINT('Ctrl Pts',(1.52772158718203,-2.26943033769167,
13.7382347919292));
#442733=CARTESIAN_POINT('Ctrl Pts',(1.53099703751788,-2.28416089415877,
13.7369371795943));
#442734=CARTESIAN_POINT('Ctrl Pts',(1.51834298390841,-2.29249268293844,
13.7364597369712));
#442735=CARTESIAN_POINT('Ctrl Pts',(1.52812922513764,-2.27127745037945,
13.7595490285574));
#442736=CARTESIAN_POINT('Ctrl Pts',(1.53148184345635,-2.2863596835307,13.7633824266925));
#442737=CARTESIAN_POINT('Ctrl Pts',(1.51907153589636,-2.29483776860776,
13.7648920890506));
#442738=CARTESIAN_POINT('Ctrl Pts',(1.52605029390404,-2.2618572768631,13.7803806590111));
#442739=CARTESIAN_POINT('Ctrl Pts',(1.52895545858147,-2.27490169728723,
13.7901039518745));
#442740=CARTESIAN_POINT('Ctrl Pts',(1.51536084390328,-2.28288116426049,
13.7926933640892));
#442741=CARTESIAN_POINT('Ctrl Pts',(1.52243664726894,-2.24548291246107,
13.7936647693663));
#442742=CARTESIAN_POINT('Ctrl Pts',(1.5247966691538,-2.25603770419978,13.8072068914932));
#442743=CARTESIAN_POINT('Ctrl Pts',(1.50888161523708,-2.26214960477777,
13.8104111085397));
#442744=CARTESIAN_POINT('Origin',(1.5062967025459,-2.27443492848209,13.7435492065112));
#442745=CARTESIAN_POINT('Origin',(1.5062967025459,-2.27443492848209,14.));
#442746=CARTESIAN_POINT('Origin',(1.5062967025459,-2.27443492848209,12.5369868989719));
#442747=CARTESIAN_POINT('Ctrl Pts',(1.54397793321899,-2.26784759462715,
12.506462012331));
#442748=CARTESIAN_POINT('Ctrl Pts',(1.54765766698853,-2.27325251344016,
12.4999388158272));
#442749=CARTESIAN_POINT('Ctrl Pts',(1.54761413091236,-2.27318856616249,
12.4907030323752));
#442750=CARTESIAN_POINT('Ctrl Pts',(1.53444082908789,-2.27708189091582,
12.5042014951932));
#442751=CARTESIAN_POINT('Ctrl Pts',(1.53283698093214,-2.28330834803118,
12.4980716682127));
#442752=CARTESIAN_POINT('Ctrl Pts',(1.52719566546365,-2.28709003085908,
12.4907355092743));
#442753=CARTESIAN_POINT('Ctrl Pts',(1.52889736027862,-2.27471637727053,
12.5218047446509));
#442754=CARTESIAN_POINT('Ctrl Pts',(1.52812476547835,-2.2865028936435,12.5216906929434));
#442755=CARTESIAN_POINT('Ctrl Pts',(1.51825426561694,-2.29290164249121,
12.5161988840776));
#442756=CARTESIAN_POINT('Ctrl Pts',(1.52777145831979,-2.26965634454415,
12.5369868989719));
#442757=CARTESIAN_POINT('Ctrl Pts',(1.53110123862728,-2.28462023757452,
12.5369868989719));
#442758=CARTESIAN_POINT('Ctrl Pts',(1.51821639211932,-2.29292603446506,
12.5369868989719));
#442759=CARTESIAN_POINT('Origin',(2.95976792804893E-31,-9.36866969595879E-31,
12.5));
#442760=CARTESIAN_POINT('Origin',(1.69106661248333,-2.08362280022671,12.5));
#442761=CARTESIAN_POINT('',(1.69106661248333,-2.08362280022671,12.5893111709658));
#442762=CARTESIAN_POINT('',(1.69106661248333,-2.08362280022671,13.8235269408515));
#442763=CARTESIAN_POINT('',(1.69106661248333,-2.08362280022671,12.5));
#442764=CARTESIAN_POINT('',(1.70159569779329,-2.1178048285711,13.7902182540695));
#442765=CARTESIAN_POINT('',(1.69106661248333,-2.08362280022671,13.8235269408515));
#442766=CARTESIAN_POINT('',(1.70769732837641,-2.13761339725484,13.7435492065112));
#442767=CARTESIAN_POINT('Origin',(1.68762335573118,-2.0724433722242,13.7445212918716));
#442768=CARTESIAN_POINT('',(1.70769732837641,-2.13761339725484,12.5369868989719));
#442769=CARTESIAN_POINT('',(1.70769732837641,-2.13761339725484,12.5));
#442770=CARTESIAN_POINT('Ctrl Pts',(1.70769732837641,-2.13761339725484,
12.5369868989719));
#442771=CARTESIAN_POINT('Ctrl Pts',(1.70215779955627,-2.11962965739802,
12.5544431401645));
#442772=CARTESIAN_POINT('Ctrl Pts',(1.69661430871789,-2.10163305509249,
12.5718848856037));
#442773=CARTESIAN_POINT('Ctrl Pts',(1.69106661248333,-2.08362280022671,
12.5893111709658));
#442774=CARTESIAN_POINT('Origin',(1.98348265190902,-2.17062729990068,12.5));
#442775=CARTESIAN_POINT('',(1.78991230016922,-2.06925956785759,13.7435492065112));
#442776=CARTESIAN_POINT('',(1.77155062986485,-2.05964404121031,13.7902182540695));
#442777=CARTESIAN_POINT('Origin',(1.72329933383918,-2.03437609907816,13.7418732680444));
#442778=CARTESIAN_POINT('',(1.73986539582218,-2.04305131259618,13.8235269408515));
#442779=CARTESIAN_POINT('',(1.77155062986485,-2.05964404121031,13.7902182540695));
#442780=CARTESIAN_POINT('',(1.73986539582218,-2.04305131259618,12.5893111709658));
#442781=CARTESIAN_POINT('',(1.73986539582218,-2.04305131259618,12.5));
#442782=CARTESIAN_POINT('',(1.78991230016922,-2.06925956785759,12.5369868989719));
#442783=CARTESIAN_POINT('Ctrl Pts',(1.73986539582218,-2.04305131259618,
12.5893111709658));
#442784=CARTESIAN_POINT('Ctrl Pts',(1.75656010846008,-2.05179389709843,
12.5718848856037));
#442785=CARTESIAN_POINT('Ctrl Pts',(1.77324216577624,-2.06052985433958,
12.5544431401645));
#442786=CARTESIAN_POINT('Ctrl Pts',(1.78991230016922,-2.06925956785759,
12.5369868989719));
#442787=CARTESIAN_POINT('',(1.78991230016922,-2.06925956785759,12.5));
#442788=CARTESIAN_POINT('Origin',(1.72391839740911,-2.07350346960704,12.5));
#442789=CARTESIAN_POINT('',(1.70109342731553,-2.04780111733327,13.8587068136939));
#442790=CARTESIAN_POINT('Ctrl Pts',(1.73986539582511,-2.04305131259026,
13.8235269408542));
#442791=CARTESIAN_POINT('Ctrl Pts',(1.73831306815132,-2.04223839917525,
13.8262006681044));
#442792=CARTESIAN_POINT('Ctrl Pts',(1.73664388770567,-2.04156041342918,
13.8288634856214));
#442793=CARTESIAN_POINT('Ctrl Pts',(1.73486763552003,-2.04100829237994,
13.8314912288862));
#442794=CARTESIAN_POINT('Ctrl Pts',(1.73303650272855,-2.04043911252683,
13.8342001611531));
#442795=CARTESIAN_POINT('Ctrl Pts',(1.73108969317603,-2.04000258846134,
13.8368750301949));
#442796=CARTESIAN_POINT('Ctrl Pts',(1.72900705260465,-2.03972180853287,
13.8394886372969));
#442797=CARTESIAN_POINT('Ctrl Pts',(1.72884620522155,-2.03970012321792,
13.8396904925131));
#442798=CARTESIAN_POINT('Ctrl Pts',(1.72868454093034,-2.03967938800469,
13.8398919674349));
#442799=CARTESIAN_POINT('Ctrl Pts',(1.72852204795747,-2.03965962469961,
13.8400930404591));
#442800=CARTESIAN_POINT('Ctrl Pts',(1.72599029812032,-2.03935169911028,
13.8432258934518));
#442801=CARTESIAN_POINT('Ctrl Pts',(1.72327043418938,-2.0392801653407,13.8462331177034));
#442802=CARTESIAN_POINT('Ctrl Pts',(1.72044862725666,-2.03954378938749,
13.8489036603661));
#442803=CARTESIAN_POINT('Ctrl Pts',(1.71952529918926,-2.03963005024354,
13.8497774930041));
#442804=CARTESIAN_POINT('Ctrl Pts',(1.71859127727977,-2.03975231245817,
13.85061494757));
#442805=CARTESIAN_POINT('Ctrl Pts',(1.71765021695585,-2.0399143593413,13.8514076489583));
#442806=CARTESIAN_POINT('Ctrl Pts',(1.71565973864956,-2.04025711186978,
13.8530843267192));
#442807=CARTESIAN_POINT('Ctrl Pts',(1.71344275623555,-2.04081443680464,
13.8546805203176));
#442808=CARTESIAN_POINT('Ctrl Pts',(1.71116120848055,-2.04168631562601,
13.8559412814273));
#442809=CARTESIAN_POINT('Ctrl Pts',(1.71085586339857,-2.04180300128801,
13.8561100121513));
#442810=CARTESIAN_POINT('Ctrl Pts',(1.71054938748777,-2.04192524853389,
13.8562727473908));
#442811=CARTESIAN_POINT('Ctrl Pts',(1.71024218506715,-2.04205322291605,
13.8564289040185));
#442812=CARTESIAN_POINT('Ctrl Pts',(1.70884902559436,-2.04263358527919,
13.8571370725437));
#442813=CARTESIAN_POINT('Ctrl Pts',(1.70741731217578,-2.0433440351555,13.8577210840554));
#442814=CARTESIAN_POINT('Ctrl Pts',(1.70601574112564,-2.04418324651125,
13.8581177131616));
#442815=CARTESIAN_POINT('Ctrl Pts',(1.70562101047732,-2.04441959731381,
13.8582294175695));
#442816=CARTESIAN_POINT('Ctrl Pts',(1.70522861104116,-2.04466599390546,
13.8583265086086));
#442817=CARTESIAN_POINT('Ctrl Pts',(1.70483990539604,-2.04492200212943,
13.8584082369006));
#442818=CARTESIAN_POINT('Ctrl Pts',(1.70428143961953,-2.04528981729594,
13.8585256585398));
#442819=CARTESIAN_POINT('Ctrl Pts',(1.70372383336746,-2.04568231562517,
13.8586122832068));
#442820=CARTESIAN_POINT('Ctrl Pts',(1.70318202617805,-2.04608994689989,
13.8586682984299));
#442821=CARTESIAN_POINT('Ctrl Pts',(1.70274863413415,-2.04641601151248,
13.8587131050557));
#442822=CARTESIAN_POINT('Ctrl Pts',(1.70232042319479,-2.04675517282245,
13.8587357943552));
#442823=CARTESIAN_POINT('Ctrl Pts',(1.70189765692105,-2.04710786813566,
13.8587355499465));
#442824=CARTESIAN_POINT('Ctrl Pts',(1.70162441299911,-2.04733582352524,
13.8587353919793));
#442825=CARTESIAN_POINT('Ctrl Pts',(1.70135637355137,-2.04756693776055,
13.8587257282814));
#442826=CARTESIAN_POINT('Ctrl Pts',(1.70109342731553,-2.04780111733327,
13.8587068136939));
#442827=CARTESIAN_POINT('Ctrl Pts',(1.70109342731553,-2.04780111733327,
13.8587068136939));
#442828=CARTESIAN_POINT('Ctrl Pts',(1.70022861148054,-2.04857132118149,
13.8586446046466));
#442829=CARTESIAN_POINT('Ctrl Pts',(1.6994188212477,-2.04937464291353,13.858482427929));
#442830=CARTESIAN_POINT('Ctrl Pts',(1.69866069815332,-2.05020813182118,
13.8582284286032));
#442831=CARTESIAN_POINT('Ctrl Pts',(1.69788295204698,-2.05106319448503,
13.8579678548414));
#442832=CARTESIAN_POINT('Ctrl Pts',(1.69715881559737,-2.0519531254972,13.857615680862));
#442833=CARTESIAN_POINT('Ctrl Pts',(1.69650932147237,-2.05283672432534,
13.8571944833187));
#442834=CARTESIAN_POINT('Ctrl Pts',(1.69488844245862,-2.05504183556806,
13.8561433417727));
#442835=CARTESIAN_POINT('Ctrl Pts',(1.6936527546168,-2.05730781781979,13.8546163505474));
#442836=CARTESIAN_POINT('Ctrl Pts',(1.69273047089348,-2.05944075232021,
13.8528973491086));
#442837=CARTESIAN_POINT('Ctrl Pts',(1.69256198326426,-2.05983040798492,
13.8525833129072));
#442838=CARTESIAN_POINT('Ctrl Pts',(1.69240381419284,-2.06021563350189,
13.8522628768812));
#442839=CARTESIAN_POINT('Ctrl Pts',(1.69225535185086,-2.06059528714164,
13.851937733538));
#442840=CARTESIAN_POINT('Ctrl Pts',(1.69134871292664,-2.06291377924506,
13.8499521282529));
#442841=CARTESIAN_POINT('Ctrl Pts',(1.69071776970868,-2.06525637489189,
13.847639871647));
#442842=CARTESIAN_POINT('Ctrl Pts',(1.69031810602992,-2.06747906191905,
13.8452109780794));
#442843=CARTESIAN_POINT('Ctrl Pts',(1.69013828906821,-2.06847909481989,
13.8441181685877));
#442844=CARTESIAN_POINT('Ctrl Pts',(1.6900045829282,-2.0694549799111,13.8430021611332));
#442845=CARTESIAN_POINT('Ctrl Pts',(1.68991002270988,-2.07039515782479,
13.8418824960098));
#442846=CARTESIAN_POINT('Ctrl Pts',(1.68968718914072,-2.07261071108671,
13.8392439765549));
#442847=CARTESIAN_POINT('Ctrl Pts',(1.68966732551376,-2.07473350914547,
13.8364981347964));
#442848=CARTESIAN_POINT('Ctrl Pts',(1.68981616026676,-2.07676884578819,
13.8336931113419));
#442849=CARTESIAN_POINT('Ctrl Pts',(1.68996111586431,-2.07875113442236,
13.8309611966328));
#442850=CARTESIAN_POINT('Ctrl Pts',(1.69026679887585,-2.08065240658422,
13.8281701127186));
#442851=CARTESIAN_POINT('Ctrl Pts',(1.69073701489446,-2.08246062340627,
13.8253580685121));
#442852=CARTESIAN_POINT('Ctrl Pts',(1.69083895823477,-2.08285264676478,
13.8247484142932));
#442853=CARTESIAN_POINT('Ctrl Pts',(1.69094874991648,-2.08324016664723,
13.8241378483365));
#442854=CARTESIAN_POINT('Ctrl Pts',(1.69106661248333,-2.08362280022671,
13.8235269408515));
#442855=CARTESIAN_POINT('',(1.70203688208365,-2.04699323741746,12.5969504640361));
#442856=CARTESIAN_POINT('Origin',(1.72393939862195,-2.07352903583219,12.584524458991));
#442857=CARTESIAN_POINT('Origin',(1.72393939862195,-2.07352903583219,12.584524458991));
#442858=CARTESIAN_POINT('Ctrl Pts',(1.73986539582218,-2.04305131259618,
12.5893111709658));
#442859=CARTESIAN_POINT('Ctrl Pts',(1.72982485735825,-2.03779334512631,
12.5770542771492));
#442860=CARTESIAN_POINT('Ctrl Pts',(1.71966334052538,-2.0506209423491,12.5737548217797));
#442861=CARTESIAN_POINT('Ctrl Pts',(1.76182068373786,-2.05454872282643,
12.5663937883685));
#442862=CARTESIAN_POINT('Ctrl Pts',(1.75176733717272,-2.04928404808883,
12.5540940315303));
#442863=CARTESIAN_POINT('Ctrl Pts',(1.74157684897256,-2.06215338939119,
12.5508374392248));
#442864=CARTESIAN_POINT('Ctrl Pts',(1.78375381903733,-2.06603453231078,
12.5434499600945));
#442865=CARTESIAN_POINT('Ctrl Pts',(1.77366778546239,-2.06075274024082,
12.5311293540533));
#442866=CARTESIAN_POINT('Ctrl Pts',(1.76346949693809,-2.07367352488174,
12.5278936106989));
#442867=CARTESIAN_POINT('Ctrl Pts',(1.80566653696509,-2.0775096497514,12.5204817579905));
#442868=CARTESIAN_POINT('Ctrl Pts',(1.79553058441682,-2.07220171642029,
12.5081597038247));
#442869=CARTESIAN_POINT('Ctrl Pts',(1.78534291223217,-2.08518229346266,
12.5049254088044));
#442870=CARTESIAN_POINT('Ctrl Pts',(1.78991230016922,-2.06925956785759,
12.5369868989719));
#442871=CARTESIAN_POINT('Ctrl Pts',(1.79073750242346,-2.06969170488486,
12.5342545179733));
#442872=CARTESIAN_POINT('Ctrl Pts',(1.79146716650627,-2.07021462690545,
12.5314872231885));
#442873=CARTESIAN_POINT('Ctrl Pts',(1.79202762612217,-2.07084431423188,
12.5287124745063));
#442874=CARTESIAN_POINT('Ctrl Pts',(1.79253307642253,-2.07141219751775,
12.5262100684184));
#442875=CARTESIAN_POINT('Ctrl Pts',(1.7928996624422,-2.07206699750852,12.5237004536639));
#442876=CARTESIAN_POINT('Ctrl Pts',(1.79307583586429,-2.0728523404252,12.5212220730815));
#442877=CARTESIAN_POINT('Ctrl Pts',(1.79321071185911,-2.07345358836549,
12.5193246583486));
#442878=CARTESIAN_POINT('Ctrl Pts',(1.79323497547226,-2.07413867514844,
12.5174178313691));
#442879=CARTESIAN_POINT('Ctrl Pts',(1.79305404523333,-2.07493014779619,
12.5155812248348));
#442880=CARTESIAN_POINT('Ctrl Pts',(1.79297696797904,-2.07526731939831,
12.5147988205794));
#442881=CARTESIAN_POINT('Ctrl Pts',(1.7928628438386,-2.07562420198027,12.5140295443047));
#442882=CARTESIAN_POINT('Ctrl Pts',(1.79270580621475,-2.07600409925261,
12.5132817086137));
#442883=CARTESIAN_POINT('Ctrl Pts',(1.79246815101462,-2.07657902238295,
12.5121499604604));
#442884=CARTESIAN_POINT('Ctrl Pts',(1.79212047097037,-2.07721633839851,
12.5110494206568));
#442885=CARTESIAN_POINT('Ctrl Pts',(1.79162607329503,-2.07790968034323,
12.5100666561695));
#442886=CARTESIAN_POINT('Ctrl Pts',(1.79134219128834,-2.07830779569127,
12.5095023550641));
#442887=CARTESIAN_POINT('Ctrl Pts',(1.79100612457548,-2.07872860384227,
12.5089719619137));
#442888=CARTESIAN_POINT('Ctrl Pts',(1.79061918161063,-2.07916023149304,
12.5085043804652));
#442889=CARTESIAN_POINT('Ctrl Pts',(1.79005294098444,-2.07979186233648,
12.5078201359221));
#442890=CARTESIAN_POINT('Ctrl Pts',(1.78936042916077,-2.08046417579513,
12.5072563000949));
#442891=CARTESIAN_POINT('Ctrl Pts',(1.78858269109955,-2.08112552463992,
12.5068768744332));
#442892=CARTESIAN_POINT('Ctrl Pts',(1.78802188841774,-2.08160240268443,
12.5066032824114));
#442893=CARTESIAN_POINT('Ctrl Pts',(1.78740695962903,-2.08208200356589,
12.5064197834844));
#442894=CARTESIAN_POINT('Ctrl Pts',(1.78677383363288,-2.08253958336252,
12.5063282718343));
#442895=CARTESIAN_POINT('Ctrl Pts',(1.78584966568937,-2.08320750820248,
12.5061946931565));
#442896=CARTESIAN_POINT('Ctrl Pts',(1.78486759422664,-2.08384364979212,
12.5062515701262));
#442897=CARTESIAN_POINT('Ctrl Pts',(1.78389697582206,-2.08442150750074,
12.5064436508398));
#442898=CARTESIAN_POINT('',(1.71966334052538,-2.05062094234911,12.5737548217797));
#442899=CARTESIAN_POINT('Origin',(1.72965931683782,-2.06254069308313,12.5893111709658));
#442900=CARTESIAN_POINT('Ctrl Pts',(1.78389697582206,-2.08442150750074,
12.5064436508398));
#442901=CARTESIAN_POINT('Ctrl Pts',(1.77438850524016,-2.0794185708687,12.5164271754438));
#442902=CARTESIAN_POINT('Ctrl Pts',(1.76487636279056,-2.07441346617056,
12.5264061185523));
#442903=CARTESIAN_POINT('Ctrl Pts',(1.75536041871244,-2.06940611788646,
12.536380305637));
#442904=CARTESIAN_POINT('Ctrl Pts',(1.7434674186562,-2.06314794813101,12.5488460165097));
#442905=CARTESIAN_POINT('Ctrl Pts',(1.73156847698094,-2.05688627203981,
12.5613043021964));
#442906=CARTESIAN_POINT('Ctrl Pts',(1.71966334052538,-2.0506209423491,12.5737548217797));
#442907=CARTESIAN_POINT('Ctrl Pts',(1.69106661248333,-2.08362280022671,
12.5893111709658));
#442908=CARTESIAN_POINT('Ctrl Pts',(1.68773011555539,-2.07279106801023,
12.5770542771492));
#442909=CARTESIAN_POINT('Ctrl Pts',(1.70219730425851,-2.06514226902717,
12.5737548217797));
#442910=CARTESIAN_POINT('Ctrl Pts',(1.68795368986888,-2.07351688827816,
12.5928319619712));
#442911=CARTESIAN_POINT('Ctrl Pts',(1.68882474430402,-2.06527827913933,
12.5821634970842));
#442912=CARTESIAN_POINT('Ctrl Pts',(1.7010543212952,-2.06146370853223,12.5773203894503));
#442913=CARTESIAN_POINT('Ctrl Pts',(1.69014909721797,-2.05691073622806,
12.5969440695591));
#442914=CARTESIAN_POINT('Ctrl Pts',(1.69322838590855,-2.05432683922702,
12.5878292599214));
#442915=CARTESIAN_POINT('Ctrl Pts',(1.70183883760259,-2.05554520523655,
12.5813877129824));
#442916=CARTESIAN_POINT('Ctrl Pts',(1.71364215121175,-2.03730839811275,
12.596957478804));
#442917=CARTESIAN_POINT('Ctrl Pts',(1.71058567081602,-2.03987326082631,
12.5878468778671));
#442918=CARTESIAN_POINT('Ctrl Pts',(1.71025114891585,-2.04853383684849,
12.5814011370086));
#442919=CARTESIAN_POINT('Ctrl Pts',(1.7304840588282,-2.03813855170033,12.5928371701607));
#442920=CARTESIAN_POINT('Ctrl Pts',(1.72223033693283,-2.0374973492534,12.5821692192951));
#442921=CARTESIAN_POINT('Ctrl Pts',(1.7162444991906,-2.0488196091202,12.5773318885715));
#442922=CARTESIAN_POINT('Ctrl Pts',(1.7398653958222,-2.04305131259613,12.5893111709658));
#442923=CARTESIAN_POINT('Ctrl Pts',(1.72982485735828,-2.03779334512626,
12.5770542771492));
#442924=CARTESIAN_POINT('Ctrl Pts',(1.71966334052541,-2.05062094234906,
12.5737548217797));
#442925=CARTESIAN_POINT('',(1.70219730425851,-2.06514226902717,12.5737548217797));
#442926=CARTESIAN_POINT('Origin',(1.71209175483583,-2.07714642863012,12.5893111709658));
#442927=CARTESIAN_POINT('Ctrl Pts',(1.71966334052541,-2.05062094234906,
12.5737548217797));
#442928=CARTESIAN_POINT('Ctrl Pts',(1.71879118408743,-2.05012732024794,
12.5746934679442));
#442929=CARTESIAN_POINT('Ctrl Pts',(1.71773585576928,-2.04974051593159,
12.5756680099006));
#442930=CARTESIAN_POINT('Ctrl Pts',(1.71661856794228,-2.04950141013988,
12.5765688348656));
#442931=CARTESIAN_POINT('Ctrl Pts',(1.71632277835887,-2.04943810952852,
12.5768073183026));
#442932=CARTESIAN_POINT('Ctrl Pts',(1.71602275959963,-2.04938492988671,
12.5770407398754));
#442933=CARTESIAN_POINT('Ctrl Pts',(1.71572087407775,-2.04934207811222,
12.5772674179684));
#442934=CARTESIAN_POINT('Ctrl Pts',(1.71448201752921,-2.04916622601729,
12.5781976435658));
#442935=CARTESIAN_POINT('Ctrl Pts',(1.71313977428438,-2.04916548139034,
12.5790594849312));
#442936=CARTESIAN_POINT('Ctrl Pts',(1.71178474793405,-2.04938818368848,
12.5797571720116));
#442937=CARTESIAN_POINT('Ctrl Pts',(1.71090189954441,-2.04953328224338,
12.580211740231));
#442938=CARTESIAN_POINT('Ctrl Pts',(1.70997654830403,-2.04979835216295,
12.5806009430798));
#442939=CARTESIAN_POINT('Ctrl Pts',(1.70907871370227,-2.05018176537634,
12.5808812374708));
#442940=CARTESIAN_POINT('Ctrl Pts',(1.70830717592583,-2.05051124452265,
12.5811221033394));
#442941=CARTESIAN_POINT('Ctrl Pts',(1.70754020722779,-2.05093496467668,
12.581287365893));
#442942=CARTESIAN_POINT('Ctrl Pts',(1.70682512856864,-2.05143630866505,
12.581359338449));
#442943=CARTESIAN_POINT('Ctrl Pts',(1.70672574740083,-2.05150598512708,
12.5813693411482));
#442944=CARTESIAN_POINT('Ctrl Pts',(1.70662731975361,-2.05157712614493,
12.5813775999465));
#442945=CARTESIAN_POINT('Ctrl Pts',(1.70652992209161,-2.05164965238241,
12.5813841266931));
#442946=CARTESIAN_POINT('Ctrl Pts',(1.70636467517804,-2.05177270191617,
12.5813952001081));
#442947=CARTESIAN_POINT('Ctrl Pts',(1.70620165000108,-2.05190105131348,
12.5814007534795));
#442948=CARTESIAN_POINT('Ctrl Pts',(1.70604103955566,-2.05203479962438,
12.5814005856065));
#442949=CARTESIAN_POINT('Ctrl Pts',(1.70530582773112,-2.05264704709946,
12.5813998171494));
#442950=CARTESIAN_POINT('Ctrl Pts',(1.70467179692695,-2.05332986518653,
12.58127954464));
#442951=CARTESIAN_POINT('Ctrl Pts',(1.70412086363673,-2.05405924342645,
12.5810700125799));
#442952=CARTESIAN_POINT('Ctrl Pts',(1.70345539895092,-2.0549402492939,12.5808169217085));
#442953=CARTESIAN_POINT('Ctrl Pts',(1.70292446691484,-2.05589935279849,
12.5804173076348));
#442954=CARTESIAN_POINT('Ctrl Pts',(1.70255181322556,-2.05683988700601,
12.5799304713245));
#442955=CARTESIAN_POINT('Ctrl Pts',(1.70208997790651,-2.05800550518796,
12.5793271277669));
#442956=CARTESIAN_POINT('Ctrl Pts',(1.70181265792322,-2.05920304701824,
12.5785808224116));
#442957=CARTESIAN_POINT('Ctrl Pts',(1.70170064367809,-2.06037487835076,
12.5777485681082));
#442958=CARTESIAN_POINT('Ctrl Pts',(1.70153373018076,-2.06212103541993,
12.576508418016));
#442959=CARTESIAN_POINT('Ctrl Pts',(1.70172843028403,-2.06379474727702,
12.5750928681475));
#442960=CARTESIAN_POINT('Ctrl Pts',(1.70219730425851,-2.06514226902717,
12.5737548217797));
#442961=CARTESIAN_POINT('Ctrl Pts',(1.70219730425851,-2.06514226902717,
12.5737548217797));
#442962=CARTESIAN_POINT('Ctrl Pts',(1.68773011555539,-2.07279106801023,
12.5770542771492));
#442963=CARTESIAN_POINT('Ctrl Pts',(1.69106661248333,-2.08362280022671,
12.5893111709658));
#442964=CARTESIAN_POINT('Ctrl Pts',(1.70953407649328,-2.08878939839514,
12.5508408821982));
#442965=CARTESIAN_POINT('Ctrl Pts',(1.69502056198147,-2.09645905426385,
12.55409748406));
#442966=CARTESIAN_POINT('Ctrl Pts',(1.69836131542497,-2.10730460499651,
12.5663972313419));
#442967=CARTESIAN_POINT('Ctrl Pts',(1.71686255508848,-2.11241377701704,
12.52790050457));
#442968=CARTESIAN_POINT('Ctrl Pts',(1.7022970454674,-2.12008171069044,12.5311362602938));
#442969=CARTESIAN_POINT('Ctrl Pts',(1.70564865921001,-2.13096251871672,
12.5434568539655));
#442970=CARTESIAN_POINT('Ctrl Pts',(1.72418337134024,-2.13601717702138,
12.5049357605811));
#442971=CARTESIAN_POINT('Ctrl Pts',(1.70956102157824,-2.14366376269259,
12.5081700652078));
#442972=CARTESIAN_POINT('Ctrl Pts',(1.71292922020911,-2.15459841253922,
12.5204921097672));
#442973=CARTESIAN_POINT('Ctrl Pts',(1.72370265633254,-2.13446728572477,
12.5064436508395));
#442974=CARTESIAN_POINT('Ctrl Pts',(1.72289754221706,-2.13538414942873,
12.5062361689309));
#442975=CARTESIAN_POINT('Ctrl Pts',(1.72202119231672,-2.13630328079726,
12.5061871075061));
#442976=CARTESIAN_POINT('Ctrl Pts',(1.72112428280073,-2.13714385795685,
12.5063648335164));
#442977=CARTESIAN_POINT('Ctrl Pts',(1.72071685117489,-2.13752569995169,
12.5064455676329));
#442978=CARTESIAN_POINT('Ctrl Pts',(1.72029934351721,-2.13789649714619,
12.506574497099));
#442979=CARTESIAN_POINT('Ctrl Pts',(1.71988896342837,-2.13823956507991,
12.5067492519495));
#442980=CARTESIAN_POINT('Ctrl Pts',(1.71906428871011,-2.13892897340961,
12.5071004286051));
#442981=CARTESIAN_POINT('Ctrl Pts',(1.71823755816902,-2.13953113118327,
12.5076537929612));
#442982=CARTESIAN_POINT('Ctrl Pts',(1.71747639089655,-2.14000848873226,
12.5083435010503));
#442983=CARTESIAN_POINT('Ctrl Pts',(1.71742847086791,-2.14003854124273,
12.5083869222963));
#442984=CARTESIAN_POINT('Ctrl Pts',(1.7173807991295,-2.14006809227941,12.5084308732336));
#442985=CARTESIAN_POINT('Ctrl Pts',(1.71733338764277,-2.14009713003058,
12.5084753333615));
#442986=CARTESIAN_POINT('Ctrl Pts',(1.71695308494236,-2.14033005112091,
12.508831962269));
#442987=CARTESIAN_POINT('Ctrl Pts',(1.71658248026876,-2.14053577543842,
12.509227847131));
#442988=CARTESIAN_POINT('Ctrl Pts',(1.71623395261267,-2.14071063388234,
12.5096423454524));
#442989=CARTESIAN_POINT('Ctrl Pts',(1.71514182119035,-2.14125856285648,
12.5109411997424));
#442990=CARTESIAN_POINT('Ctrl Pts',(1.7142036306779,-2.14154575730631,12.5124831113042));
#442991=CARTESIAN_POINT('Ctrl Pts',(1.71340838913029,-2.14166621209627,
12.5140723025008));
#442992=CARTESIAN_POINT('Ctrl Pts',(1.71333387412627,-2.14167749884202,
12.5142212114565));
#442993=CARTESIAN_POINT('Ctrl Pts',(1.71326060064133,-2.14168734795223,
12.5143705582413));
#442994=CARTESIAN_POINT('Ctrl Pts',(1.71318855326299,-2.14169585249783,
12.5145201959299));
#442995=CARTESIAN_POINT('Ctrl Pts',(1.71226299742089,-2.14180510604802,
12.5164425148273));
#442996=CARTESIAN_POINT('Ctrl Pts',(1.71150933463858,-2.14170687066787,
12.5184635205941));
#442997=CARTESIAN_POINT('Ctrl Pts',(1.71087201749238,-2.14147222703179,
12.5205025929158));
#442998=CARTESIAN_POINT('Ctrl Pts',(1.7105023482867,-2.14133612442246,12.5216853356836));
#442999=CARTESIAN_POINT('Ctrl Pts',(1.71017232380612,-2.14115482743748,
12.5228750347131));
#443000=CARTESIAN_POINT('Ctrl Pts',(1.70987597479482,-2.14094557851382,
12.5240609649613));
#443001=CARTESIAN_POINT('Ctrl Pts',(1.70914860204515,-2.14043198825653,
12.5269717671326));
#443002=CARTESIAN_POINT('Ctrl Pts',(1.7086096256663,-2.13972706028063,12.5299036066169));
#443003=CARTESIAN_POINT('Ctrl Pts',(1.70819956303754,-2.13889381315844,
12.5328133004019));
#443004=CARTESIAN_POINT('Ctrl Pts',(1.7080027090985,-2.13849380602126,12.5342101228451));
#443005=CARTESIAN_POINT('Ctrl Pts',(1.70783627993333,-2.13806449466612,
12.5356023438238));
#443006=CARTESIAN_POINT('Ctrl Pts',(1.70769732837641,-2.13761339725483,
12.5369868989719));
#443007=CARTESIAN_POINT('Origin',(5.45451214630952,-14.3194087425353,-1.23967887089177));
#443008=CARTESIAN_POINT('Ctrl Pts',(1.7898752938568,-2.06924014380621,12.5369868989719));
#443009=CARTESIAN_POINT('Ctrl Pts',(1.80345023182615,-2.07638187768624,
12.5369868989719));
#443010=CARTESIAN_POINT('Ctrl Pts',(1.8148454186455,-2.06611381939672,12.5369868989719));
#443011=CARTESIAN_POINT('Ctrl Pts',(1.79446418463105,-2.0716542705718,12.5218025310015));
#443012=CARTESIAN_POINT('Ctrl Pts',(1.80604660487188,-2.07400020430251,
12.5216901060418));
#443013=CARTESIAN_POINT('Ctrl Pts',(1.81481069337939,-2.06614513209288,
12.5161920673677));
#443014=CARTESIAN_POINT('Ctrl Pts',(1.79529649285718,-2.07762447443862,
12.5042015548895));
#443015=CARTESIAN_POINT('Ctrl Pts',(1.80172847633282,-2.07770774259735,
12.4980677368513));
#443016=CARTESIAN_POINT('Ctrl Pts',(1.80685914496331,-2.07325049915236,
12.4907278922778));
#443017=CARTESIAN_POINT('Ctrl Pts',(1.78388397084315,-2.08440631165171,
12.506463626192));
#443018=CARTESIAN_POINT('Ctrl Pts',(1.78813814734719,-2.0893771687819,12.4999376786891));
#443019=CARTESIAN_POINT('Ctrl Pts',(1.78808618876676,-2.08931645698968,
12.4906970594712));
#443020=CARTESIAN_POINT('Origin',(1.80011837915358,-2.04977018737064,12.5369868989719));
#443021=CARTESIAN_POINT('Origin',(1.80011837915358,-2.04977018737064,14.));
#443022=CARTESIAN_POINT('Origin',(1.80011837915358,-2.04977018737064,13.7435492065112));
#443023=CARTESIAN_POINT('Ctrl Pts',(1.7679778087978,-2.05777301758466,13.793642941384));
#443024=CARTESIAN_POINT('Ctrl Pts',(1.77754357613767,-2.06281308843785,
13.8071662555867));
#443025=CARTESIAN_POINT('Ctrl Pts',(1.78761084470702,-2.04907738724762,
13.8103758687955));
#443026=CARTESIAN_POINT('Ctrl Pts',(1.78270214268511,-2.0654837696101,13.7804579775006));
#443027=CARTESIAN_POINT('Ctrl Pts',(1.79451016202354,-2.07169378982202,
13.7901904343352));
#443028=CARTESIAN_POINT('Ctrl Pts',(1.80575782147073,-2.06065992915931,
13.7927914348262));
#443029=CARTESIAN_POINT('Ctrl Pts',(1.79137091220124,-2.07002337948204,
13.7597120340895));
#443030=CARTESIAN_POINT('Ctrl Pts',(1.80503878325616,-2.07720504995615,
13.7635825532445));
#443031=CARTESIAN_POINT('Ctrl Pts',(1.81647282585308,-2.067468593412,13.7651073818884));
#443032=CARTESIAN_POINT('Ctrl Pts',(1.78967336863811,-2.06913441992315,
13.7381884353898));
#443033=CARTESIAN_POINT('Ctrl Pts',(1.80302089962284,-2.07614878569902,
13.7368803041982));
#443034=CARTESIAN_POINT('Ctrl Pts',(1.81437477466417,-2.06613483749339,
13.7363986145813));
#443035=CARTESIAN_POINT('Origin',(1.78175670884921,-2.04015466072337,13.7902182540695));
#443036=CARTESIAN_POINT('Ctrl Pts',(1.73986190917114,-2.04304948587151,
13.8235227101244));
#443037=CARTESIAN_POINT('Ctrl Pts',(1.75004488945686,-2.04838705093622,
13.8358800583119));
#443038=CARTESIAN_POINT('Ctrl Pts',(1.76024757046897,-2.03532828571046,
13.8390832900376));
#443039=CARTESIAN_POINT('Ctrl Pts',(1.75042832427883,-2.04858284118871,
13.8124254819052));
#443040=CARTESIAN_POINT('Ctrl Pts',(1.76063107989705,-2.05393077148275,
13.8247886449158));
#443041=CARTESIAN_POINT('Ctrl Pts',(1.77083322137122,-2.04084501241255,
13.8279860620657));
#443042=CARTESIAN_POINT('Ctrl Pts',(1.76099000386301,-2.05411371663608,
13.8013225099955));
#443043=CARTESIAN_POINT('Ctrl Pts',(1.77120771982084,-2.05946949057065,
13.8136962257787));
#443044=CARTESIAN_POINT('Ctrl Pts',(1.78141384636739,-2.0463594255137,13.8168830918626));
#443045=CARTESIAN_POINT('Ctrl Pts',(1.77154713217567,-2.05964220870156,
13.7902140179785));
#443046=CARTESIAN_POINT('Ctrl Pts',(1.78177530817666,-2.06500346948959,
13.802602731458));
#443047=CARTESIAN_POINT('Ctrl Pts',(1.79198964208704,-2.05187161755285,
13.8057746032558));
#443048=CARTESIAN_POINT('Origin',(1.75007147480654,-2.02356193210923,13.8235269408515));
#443049=CARTESIAN_POINT('Ctrl Pts',(1.69106661248333,-2.08362280022671,
13.8235269408515));
#443050=CARTESIAN_POINT('Ctrl Pts',(1.69454250510398,-2.09490707199234,
13.8362179249168));
#443051=CARTESIAN_POINT('Ctrl Pts',(1.67924918461413,-2.10250821351529,
13.8391868794938));
#443052=CARTESIAN_POINT('Ctrl Pts',(1.68788632203204,-2.07329818273625,
13.8400110824519));
#443053=CARTESIAN_POINT('Ctrl Pts',(1.68740372913541,-2.08335248365463,
13.8494522556836));
#443054=CARTESIAN_POINT('Ctrl Pts',(1.67412270254772,-2.08548373216496,
13.85569149686));
#443055=CARTESIAN_POINT('Ctrl Pts',(1.68988426417026,-2.05713012925857,
13.8586819406588));
#443056=CARTESIAN_POINT('Ctrl Pts',(1.68654527462426,-2.05992426462513,
13.868010383617));
#443057=CARTESIAN_POINT('Ctrl Pts',(1.67758422377729,-2.05866234762686,
13.8744918421245));
#443058=CARTESIAN_POINT('Ctrl Pts',(1.71391107976988,-2.03708558810421,
13.8587686893867));
#443059=CARTESIAN_POINT('Ctrl Pts',(1.7172203162035,-2.03431627733324,13.8680909899357));
#443060=CARTESIAN_POINT('Ctrl Pts',(1.71758346414105,-2.02529604867311,
13.8745789365163));
#443061=CARTESIAN_POINT('Ctrl Pts',(1.73027935694154,-2.03803135466715,
13.8400379222776));
#443062=CARTESIAN_POINT('Ctrl Pts',(1.74025120512754,-2.03938504505403,
13.8494748685453));
#443063=CARTESIAN_POINT('Ctrl Pts',(1.74477032468373,-2.02672255463149,
13.8557104837033));
#443064=CARTESIAN_POINT('Ctrl Pts',(1.73986539582511,-2.04305131259026,
13.8235269408542));
#443065=CARTESIAN_POINT('Ctrl Pts',(1.75032541850993,-2.04852895297857,
13.8362179249195));
#443066=CARTESIAN_POINT('Ctrl Pts',(1.76059090559906,-2.03488040804223,
13.8391868794965));
#443067=CARTESIAN_POINT('Origin',(1.67004147013083,-2.0900991718233,13.8235269408515));
#443068=CARTESIAN_POINT('Ctrl Pts',(1.70159453635695,-2.11780106062099,
13.7902140241683));
#443069=CARTESIAN_POINT('Ctrl Pts',(1.70499832600973,-2.12883613250079,
13.8026027327198));
#443070=CARTESIAN_POINT('Ctrl Pts',(1.69022235930951,-2.1364813100885,13.8057746032556));
#443071=CARTESIAN_POINT('Ctrl Pts',(1.69808637528478,-2.10641203130704,
13.8013225161808));
#443072=CARTESIAN_POINT('Ctrl Pts',(1.70148668000303,-2.11743581721336,
13.8136962270464));
#443073=CARTESIAN_POINT('Ctrl Pts',(1.68673363241353,-2.12507690300892,
13.8168830918628));
#443074=CARTESIAN_POINT('Ctrl Pts',(1.69457670181281,-2.09501809208009,
13.8124254880875));
#443075=CARTESIAN_POINT('Ctrl Pts',(1.69797202604004,-2.10602573707947,
13.8247886461867));
#443076=CARTESIAN_POINT('Ctrl Pts',(1.68324360346558,-2.11366734232092,
13.8279860620656));
#443077=CARTESIAN_POINT('Ctrl Pts',(1.69106545471319,-2.08361904416762,
13.8235227163066));
#443078=CARTESIAN_POINT('Ctrl Pts',(1.69445419831512,-2.0946053538318,13.8358800595847));
#443079=CARTESIAN_POINT('Ctrl Pts',(1.67975221738026,-2.1022524178036,13.8390832900376));
#443080=CARTESIAN_POINT('Origin',(1.68057055544079,-2.12428120016769,13.7902182540695));
#443081=CARTESIAN_POINT('Ctrl Pts',(1.70761786051406,-2.13735550342723,
13.7382347919292));
#443082=CARTESIAN_POINT('Ctrl Pts',(1.71208308916302,-2.15177006557272,
13.7369371795942));
#443083=CARTESIAN_POINT('Ctrl Pts',(1.70015025900713,-2.16110555385622,
13.7364597369711));
#443084=CARTESIAN_POINT('Ctrl Pts',(1.70817469891981,-2.1391632437222,13.7595490285574));
#443085=CARTESIAN_POINT('Ctrl Pts',(1.71274550369607,-2.15392202246967,
13.7633824266926));
#443086=CARTESIAN_POINT('Ctrl Pts',(1.70106753305121,-2.16338345269585,
13.7648920890506));
#443087=CARTESIAN_POINT('Ctrl Pts',(1.70533485356418,-2.1299438672515,13.780380659011));
#443088=CARTESIAN_POINT('Ctrl Pts',(1.70929359290887,-2.14270808555131,
13.7901039518744));
#443089=CARTESIAN_POINT('Ctrl Pts',(1.69639461382563,-2.15176908880903,
13.7926933640892));
#443090=CARTESIAN_POINT('Ctrl Pts',(1.7003985683292,-2.11391853294447,13.7936647693663));
#443091=CARTESIAN_POINT('Ctrl Pts',(1.70361105094856,-2.1242458407914,13.8072068914933));
#443092=CARTESIAN_POINT('Ctrl Pts',(1.68824712969806,-2.13163462916677,
13.8104111085397));
#443093=CARTESIAN_POINT('Origin',(1.68667218602391,-2.14408976885142,13.7435492065112));
#443094=CARTESIAN_POINT('Origin',(1.68667218602391,-2.14408976885142,14.));
#443095=CARTESIAN_POINT('Origin',(1.68667218602391,-2.14408976885142,12.5369868989719));
#443096=CARTESIAN_POINT('Ctrl Pts',(1.72369110664741,-2.13445298369114,
12.506462012331));
#443097=CARTESIAN_POINT('Ctrl Pts',(1.72779914746646,-2.13953998561947,
12.4999388158272));
#443098=CARTESIAN_POINT('Ctrl Pts',(1.72775054395621,-2.13947979971546,
12.4907030323752));
#443099=CARTESIAN_POINT('Ctrl Pts',(1.71493841731808,-2.14443391614551,
12.5042014951932));
#443100=CARTESIAN_POINT('Ctrl Pts',(1.71384741989327,-2.15077038375256,
12.4980716682127));
#443101=CARTESIAN_POINT('Ctrl Pts',(1.70853311769454,-2.15499930292493,
12.4907355092743));
#443102=CARTESIAN_POINT('Ctrl Pts',(1.70922058262154,-2.14252811772274,
12.5218047446509));
#443103=CARTESIAN_POINT('Ctrl Pts',(1.70941126907183,-2.15433838908345,
12.5216906929434));
#443104=CARTESIAN_POINT('Ctrl Pts',(1.70009516991862,-2.16152038399417,
12.5161988840776));
#443105=CARTESIAN_POINT('Ctrl Pts',(1.70768598736634,-2.13757669329985,
12.5369868989719));
#443106=CARTESIAN_POINT('Ctrl Pts',(1.71222438430453,-2.15221938720337,
12.5369868989719));
#443107=CARTESIAN_POINT('Ctrl Pts',(1.70005941061424,-2.16154778184741,
12.5369868989719));
#443108=CARTESIAN_POINT('Origin',(3.29362846957905E-31,-9.11339005493236E-31,
12.5));
#443109=CARTESIAN_POINT('Origin',(1.85527432946228,-1.93885208923186,12.5));
#443110=CARTESIAN_POINT('',(1.85527432946228,-1.93885208923186,12.5893111709658));
#443111=CARTESIAN_POINT('',(1.85527432946228,-1.93885208923186,13.8235269408515));
#443112=CARTESIAN_POINT('',(1.85527432946228,-1.93885208923186,12.5));
#443113=CARTESIAN_POINT('',(1.86855453274999,-1.97206216149674,13.7902182540695));
#443114=CARTESIAN_POINT('',(1.85527432946228,-1.93885208923186,13.8235269408515));
#443115=CARTESIAN_POINT('',(1.87625044290219,-1.99130747926497,13.7435492065112));
#443116=CARTESIAN_POINT('Origin',(1.85093130269374,-1.92799051723916,13.7445212918696));
#443117=CARTESIAN_POINT('',(1.87625044290219,-1.99130747926497,12.5369868989719));
#443118=CARTESIAN_POINT('',(1.87625044290219,-1.99130747926497,12.5));
#443119=CARTESIAN_POINT('Ctrl Pts',(1.87625044290219,-1.99130747926497,
12.5369868989719));
#443120=CARTESIAN_POINT('Ctrl Pts',(1.869263504656,-1.97383510184429,12.5544431401645));
#443121=CARTESIAN_POINT('Ctrl Pts',(1.86227156916588,-1.9563502277149,12.5718848856037));
#443122=CARTESIAN_POINT('Ctrl Pts',(1.85527432946228,-1.93885208923186,
12.5893111709658));
#443123=CARTESIAN_POINT('Origin',(2.15380905307319,-2.00173246673928,12.5));
#443124=CARTESIAN_POINT('',(1.95262037949676,-1.91647980814857,13.7435492065112));
#443125=CARTESIAN_POINT('',(1.93353605144765,-1.90839292296423,13.7902182540695));
#443126=CARTESIAN_POINT('Origin',(1.88338573577249,-1.88714198639574,13.7418732680459));
#443127=CARTESIAN_POINT('',(1.90060378598597,-1.89443804601159,13.8235269408515));
#443128=CARTESIAN_POINT('',(1.93353605144765,-1.90839292296423,13.7902182540695));
#443129=CARTESIAN_POINT('',(1.90060378598597,-1.89443804601159,12.5893111709658));
#443130=CARTESIAN_POINT('',(1.90060378598597,-1.89443804601159,12.5));
#443131=CARTESIAN_POINT('',(1.95262037949676,-1.91647980814857,12.5369868989719));
#443132=CARTESIAN_POINT('Ctrl Pts',(1.90060378598597,-1.89443804601159,
12.5893111709658));
#443133=CARTESIAN_POINT('Ctrl Pts',(1.91795555014392,-1.90179076621899,
12.5718848856037));
#443134=CARTESIAN_POINT('Ctrl Pts',(1.93529416090636,-1.90913791274315,
12.5544431401645));
#443135=CARTESIAN_POINT('Ctrl Pts',(1.95262037949676,-1.91647980814857,
12.5369868989719));
#443136=CARTESIAN_POINT('',(1.95262037949676,-1.91647980814857,12.5));
#443137=CARTESIAN_POINT('Origin',(1.88719198339501,-1.9260887043975,12.5));
#443138=CARTESIAN_POINT('',(1.86234798118716,-1.90233232153995,13.8587068136939));
#443139=CARTESIAN_POINT('Ctrl Pts',(1.90060378598842,-1.89443804600545,
13.8235269408542));
#443140=CARTESIAN_POINT('Ctrl Pts',(1.89899036356686,-1.89375436660929,
13.8262006681044));
#443141=CARTESIAN_POINT('Ctrl Pts',(1.89727147504902,-1.8932146905071,13.8288634856214));
#443142=CARTESIAN_POINT('Ctrl Pts',(1.89545613020484,-1.89280918763816,
13.8314912288862));
#443143=CARTESIAN_POINT('Ctrl Pts',(1.89358469691463,-1.89239115600596,
13.8342001611531));
#443144=CARTESIAN_POINT('Ctrl Pts',(1.89160878444647,-1.89211476749012,
13.8368750301949));
#443145=CARTESIAN_POINT('Ctrl Pts',(1.88951018751899,-1.89200467637456,
13.8394886372969));
#443146=CARTESIAN_POINT('Ctrl Pts',(1.88934810778779,-1.89199617377066,
13.8396904925131));
#443147=CARTESIAN_POINT('Ctrl Pts',(1.8891852913088,-1.8919886846927,13.8398919674349));
#443148=CARTESIAN_POINT('Ctrl Pts',(1.88902172812506,-1.89198223183418,
13.8400930404591));
#443149=CARTESIAN_POINT('Ctrl Pts',(1.88647330368247,-1.89188169195719,
13.8432258934518));
#443150=CARTESIAN_POINT('Ctrl Pts',(1.88375665920809,-1.89203209037069,
13.8462331177034));
#443151=CARTESIAN_POINT('Ctrl Pts',(1.88096572941233,-1.8925248406916,13.8489036603661));
#443152=CARTESIAN_POINT('Ctrl Pts',(1.88005250470348,-1.89268607433102,
13.849777493004));
#443153=CARTESIAN_POINT('Ctrl Pts',(1.87913155618036,-1.89288406118488,
13.85061494757));
#443154=CARTESIAN_POINT('Ctrl Pts',(1.87820683548238,-1.89312227402315,
13.8514076489583));
#443155=CARTESIAN_POINT('Ctrl Pts',(1.87625091784147,-1.89362612853153,
13.8530843267192));
#443156=CARTESIAN_POINT('Ctrl Pts',(1.87408673940969,-1.89436230366186,
13.8546805203176));
#443157=CARTESIAN_POINT('Ctrl Pts',(1.87188384953468,-1.89541724870127,
13.8559412814273));
#443158=CARTESIAN_POINT('Ctrl Pts',(1.871589031428,-1.89555843456022,13.8561100121513));
#443159=CARTESIAN_POINT('Ctrl Pts',(1.87129353957594,-1.89570525567038,
13.8562727473908));
#443160=CARTESIAN_POINT('Ctrl Pts',(1.87099779044625,-1.89585784407755,
13.8564289040185));
#443161=CARTESIAN_POINT('Ctrl Pts',(1.86965657151709,-1.89654983076329,
13.8571370725437));
#443162=CARTESIAN_POINT('Ctrl Pts',(1.86828753026721,-1.89737461461124,
13.8577210840554));
#443163=CARTESIAN_POINT('Ctrl Pts',(1.86695902634548,-1.89832527461257,
13.8581177131616));
#443164=CARTESIAN_POINT('Ctrl Pts',(1.8665848739154,-1.89859301318967,13.8582294175695));
#443165=CARTESIAN_POINT('Ctrl Pts',(1.86621386376566,-1.89887057411389,
13.8583265086086));
#443166=CARTESIAN_POINT('Ctrl Pts',(1.86584731855342,-1.89915741361026,
13.8584082369006));
#443167=CARTESIAN_POINT('Ctrl Pts',(1.86532069137642,-1.89956952504748,
13.8585256585398));
#443168=CARTESIAN_POINT('Ctrl Pts',(1.86479693277076,-1.900006167457,13.8586122832068));
#443169=CARTESIAN_POINT('Ctrl Pts',(1.86429015413323,-1.90045660468811,
13.8586682984299));
#443170=CARTESIAN_POINT('Ctrl Pts',(1.86388478145856,-1.90081690982259,
13.8587131050557));
#443171=CARTESIAN_POINT('Ctrl Pts',(1.86348564015117,-1.90118984576816,
13.8587357943552));
#443172=CARTESIAN_POINT('Ctrl Pts',(1.86309302853961,-1.90157582689289,
13.8587355499465));
#443173=CARTESIAN_POINT('Ctrl Pts',(1.86283927429476,-1.90182529569603,
13.8587353919793));
#443174=CARTESIAN_POINT('Ctrl Pts',(1.86259096468191,-1.90207748862114,
13.8587257282814));
#443175=CARTESIAN_POINT('Ctrl Pts',(1.86234798118716,-1.90233232153995,
13.8587068136939));
#443176=CARTESIAN_POINT('Ctrl Pts',(1.86234798118716,-1.90233232153995,
13.8587068136939));
#443177=CARTESIAN_POINT('Ctrl Pts',(1.86154882171938,-1.90317045311751,
13.8586446046466));
#443178=CARTESIAN_POINT('Ctrl Pts',(1.86080720417558,-1.90403710728445,
13.858482427929));
#443179=CARTESIAN_POINT('Ctrl Pts',(1.86011954075697,-1.90492961689678,
13.8582284286032));
#443180=CARTESIAN_POINT('Ctrl Pts',(1.85941407808175,-1.90584522793806,
13.8579678548414));
#443181=CARTESIAN_POINT('Ctrl Pts',(1.85876488877565,-1.9067912216214,13.857615680862));
#443182=CARTESIAN_POINT('Ctrl Pts',(1.8581895772962,-1.90772482014813,13.8571944833187));
#443183=CARTESIAN_POINT('Ctrl Pts',(1.85675382866118,-1.91005471075223,
13.8561433417727));
#443184=CARTESIAN_POINT('Ctrl Pts',(1.85570695105859,-1.91241387316563,
13.8546163505474));
#443185=CARTESIAN_POINT('Ctrl Pts',(1.85496159012127,-1.91461488518797,
13.8528973491086));
#443186=CARTESIAN_POINT('Ctrl Pts',(1.85482542367479,-1.91501697761155,
13.8525833129072));
#443187=CARTESIAN_POINT('Ctrl Pts',(1.8546991803538,-1.91541381357007,13.8522628768812));
#443188=CARTESIAN_POINT('Ctrl Pts',(1.85458215730419,-1.91580430500278,
13.851937733538));
#443189=CARTESIAN_POINT('Ctrl Pts',(1.85386751377646,-1.91818898200413,
13.8499521282529));
#443190=CARTESIAN_POINT('Ctrl Pts',(1.85342961326282,-1.92057521058686,
13.847639871647));
#443191=CARTESIAN_POINT('Ctrl Pts',(1.85321244905911,-1.92282307810641,
13.8452109780794));
#443192=CARTESIAN_POINT('Ctrl Pts',(1.85311474238879,-1.92383444023199,
13.8441181685877));
#443193=CARTESIAN_POINT('Ctrl Pts',(1.85306102483953,-1.92481797643773,
13.8430021611332));
#443194=CARTESIAN_POINT('Ctrl Pts',(1.85304341249069,-1.92576273352262,
13.8418824960098));
#443195=CARTESIAN_POINT('Ctrl Pts',(1.85300190854089,-1.92798907771841,
13.8392439765549));
#443196=CARTESIAN_POINT('Ctrl Pts',(1.85315513875739,-1.93010643141176,
13.8364981347964));
#443197=CARTESIAN_POINT('Ctrl Pts',(1.85346937710656,-1.93212286422562,
13.8336931113419));
#443198=CARTESIAN_POINT('Ctrl Pts',(1.85377542530267,-1.934086741731,13.8309611966328));
#443199=CARTESIAN_POINT('Ctrl Pts',(1.85423506251094,-1.93595677156332,
13.8281701127185));
#443200=CARTESIAN_POINT('Ctrl Pts',(1.85485110038221,-1.93772064472228,
13.825358068512));
#443201=CARTESIAN_POINT('Ctrl Pts',(1.85498465805755,-1.93810305432676,
13.8247484142932));
#443202=CARTESIAN_POINT('Ctrl Pts',(1.85512567088447,-1.93848033572744,
13.8241378483365));
#443203=CARTESIAN_POINT('Ctrl Pts',(1.85527432946228,-1.93885208923186,
13.8235269408515));
#443204=CARTESIAN_POINT('',(1.86322244697428,-1.90145022945566,12.5969504640361));
#443205=CARTESIAN_POINT('Origin',(1.88721499861276,-1.92611247375935,12.584524458991));
#443206=CARTESIAN_POINT('Origin',(1.88721499861276,-1.92611247375935,12.584524458991));
#443207=CARTESIAN_POINT('Ctrl Pts',(1.90060378598597,-1.89443804601159,
12.5893111709658));
#443208=CARTESIAN_POINT('Ctrl Pts',(1.89016808342412,-1.89001597109135,
12.5770542771492));
#443209=CARTESIAN_POINT('Ctrl Pts',(1.8810859464595,-1.90362914349938,12.5737548217797));
#443210=CARTESIAN_POINT('Ctrl Pts',(1.92342316516287,-1.90410763976972,
12.5663937883685));
#443211=CARTESIAN_POINT('Ctrl Pts',(1.91297415041314,-1.89967992387878,
12.5540940315304));
#443212=CARTESIAN_POINT('Ctrl Pts',(1.90386654101103,-1.91333706290175,
12.5508374392248));
#443213=CARTESIAN_POINT('Ctrl Pts',(1.94621951986594,-1.91376747702629,
12.5434499600945));
#443214=CARTESIAN_POINT('Ctrl Pts',(1.9357365316482,-1.90932536505424,12.5311293540533));
#443215=CARTESIAN_POINT('Ctrl Pts',(1.92662534098664,-1.92303441204117,
12.5278936106989));
#443216=CARTESIAN_POINT('Ctrl Pts',(1.96899465363369,-1.9234183220214,12.5204817579905));
#443217=CARTESIAN_POINT('Ctrl Pts',(1.95845978178843,-1.91895422463086,
12.5081597038247));
#443218=CARTESIAN_POINT('Ctrl Pts',(1.94936404577731,-1.93272199973472,
12.5049254088044));
#443219=CARTESIAN_POINT('Ctrl Pts',(1.95262037949676,-1.91647980814857,
12.5369868989719));
#443220=CARTESIAN_POINT('Ctrl Pts',(1.95347805913806,-1.916843245631,12.5342545179733));
#443221=CARTESIAN_POINT('Ctrl Pts',(1.95424791832307,-1.91730495327509,
12.5314872231885));
#443222=CARTESIAN_POINT('Ctrl Pts',(1.95485783841868,-1.91788686270714,
12.5287124745063));
#443223=CARTESIAN_POINT('Ctrl Pts',(1.95540789463462,-1.91841165751637,
12.5262100684184));
#443224=CARTESIAN_POINT('Ctrl Pts',(1.95582663314767,-1.91903439855037,
12.5237004536639));
#443225=CARTESIAN_POINT('Ctrl Pts',(1.9560662331057,-1.91980276853386,12.5212220730815));
#443226=CARTESIAN_POINT('Ctrl Pts',(1.95624966760063,-1.92039102222554,
12.5193246583486));
#443227=CARTESIAN_POINT('Ctrl Pts',(1.95632969141146,-1.92107185172901,
12.517417831369));
#443228=CARTESIAN_POINT('Ctrl Pts',(1.95621387557143,-1.92187543831097,
12.5155812248347));
#443229=CARTESIAN_POINT('Ctrl Pts',(1.95616453740107,-1.92221777051417,
12.5147988205793));
#443230=CARTESIAN_POINT('Ctrl Pts',(1.95607988224286,-1.92258276777569,
12.5140295443047));
#443231=CARTESIAN_POINT('Ctrl Pts',(1.95595433230324,-1.9229742009954,12.5132817086137));
#443232=CARTESIAN_POINT('Ctrl Pts',(1.95576432945362,-1.92356658222155,
12.5121499604604));
#443233=CARTESIAN_POINT('Ctrl Pts',(1.95546975345786,-1.92423011677195,
12.5110494206568));
#443234=CARTESIAN_POINT('Ctrl Pts',(1.95503351465517,-1.92496144967886,
12.5100666561695));
#443235=CARTESIAN_POINT('Ctrl Pts',(1.95478302733923,-1.92538137934989,
12.5095023550641));
#443236=CARTESIAN_POINT('Ctrl Pts',(1.95448237863155,-1.92582817985345,
12.5089719619137));
#443237=CARTESIAN_POINT('Ctrl Pts',(1.95413190484807,-1.92628991074266,
12.5085043804652));
#443238=CARTESIAN_POINT('Ctrl Pts',(1.95361903211837,-1.92696559375433,
12.5078201359222));
#443239=CARTESIAN_POINT('Ctrl Pts',(1.95298362435897,-1.92769211628802,
12.5072563000949));
#443240=CARTESIAN_POINT('Ctrl Pts',(1.9522623802275,-1.92841465742125,12.5068768744332));
#443241=CARTESIAN_POINT('Ctrl Pts',(1.9517423135581,-1.92893565931821,12.5066032824114));
#443242=CARTESIAN_POINT('Ctrl Pts',(1.95116852281845,-1.9294637867723,12.5064197834844));
#443243=CARTESIAN_POINT('Ctrl Pts',(1.95057480049822,-1.92997144965625,
12.5063282718343));
#443244=CARTESIAN_POINT('Ctrl Pts',(1.94970814972246,-1.93071248029835,
12.5061946931565));
#443245=CARTESIAN_POINT('Ctrl Pts',(1.94878119746672,-1.93142655312066,
12.5062515701262));
#443246=CARTESIAN_POINT('Ctrl Pts',(1.94786090948263,-1.93208160246618,
12.5064436508398));
#443247=CARTESIAN_POINT('',(1.8810859464595,-1.90362914349938,12.5737548217797));
#443248=CARTESIAN_POINT('Origin',(1.89202023232776,-1.91469446737857,12.5893111709658));
#443249=CARTESIAN_POINT('Ctrl Pts',(1.94786090948263,-1.93208160246617,
12.5064436508398));
#443250=CARTESIAN_POINT('Ctrl Pts',(1.93797629177169,-1.92787034131781,
12.5164271754438));
#443251=CARTESIAN_POINT('Ctrl Pts',(1.92808783769337,-1.92365721860872,
12.5264061185523));
#443252=CARTESIAN_POINT('Ctrl Pts',(1.91819541176305,-1.91944216964704,
12.536380305637));
#443253=CARTESIAN_POINT('Ctrl Pts',(1.90583188575032,-1.91417421334899,
12.5488460165097));
#443254=CARTESIAN_POINT('Ctrl Pts',(1.89346215208989,-1.90890324667937,
12.5613043021964));
#443255=CARTESIAN_POINT('Ctrl Pts',(1.8810859464595,-1.90362914349938,12.5737548217797));
#443256=CARTESIAN_POINT('Ctrl Pts',(1.85527432946227,-1.93885208923186,
12.5893111709658));
#443257=CARTESIAN_POINT('Ctrl Pts',(1.85106604772008,-1.92832835418493,
12.5770542771492));
#443258=CARTESIAN_POINT('Ctrl Pts',(1.86486164992115,-1.91952579576338,
12.5737548217797));
#443259=CARTESIAN_POINT('Ctrl Pts',(1.85134803919851,-1.92903353596369,
12.5928319619712));
#443260=CARTESIAN_POINT('Ctrl Pts',(1.85154467214355,-1.92075134109419,
12.5821634970842));
#443261=CARTESIAN_POINT('Ctrl Pts',(1.86342263330893,-1.91595263909747,
12.5773203894503));
#443262=CARTESIAN_POINT('Ctrl Pts',(1.85218258595468,-1.9123036934345,12.5969440695591));
#443263=CARTESIAN_POINT('Ctrl Pts',(1.85504101697285,-1.90947740352257,
12.5878292599214));
#443264=CARTESIAN_POINT('Ctrl Pts',(1.86372212623972,-1.90998988377111,
12.5813877129824));
#443265=CARTESIAN_POINT('Ctrl Pts',(1.87399969621371,-1.89085167848282,
12.596957478804));
#443266=CARTESIAN_POINT('Ctrl Pts',(1.87116244612653,-1.89365713835452,
12.5878468778671));
#443267=CARTESIAN_POINT('Ctrl Pts',(1.87153495466706,-1.90231616366485,
12.5814011370086));
#443268=CARTESIAN_POINT('Ctrl Pts',(1.89085322899608,-1.89030629797944,
12.5928371701607));
#443269=CARTESIAN_POINT('Ctrl Pts',(1.88257470672739,-1.89033998403904,
12.5821692192952));
#443270=CARTESIAN_POINT('Ctrl Pts',(1.87753165565631,-1.90211247136596,
12.5773318885715));
#443271=CARTESIAN_POINT('Ctrl Pts',(1.90060378598599,-1.89443804601154,
12.5893111709658));
#443272=CARTESIAN_POINT('Ctrl Pts',(1.89016808342414,-1.8900159710913,12.5770542771492));
#443273=CARTESIAN_POINT('Ctrl Pts',(1.88108594645952,-1.90362914349933,
12.5737548217797));
#443274=CARTESIAN_POINT('',(1.86486164992115,-1.91952579576338,12.5737548217797));
#443275=CARTESIAN_POINT('Origin',(1.87570162797923,-1.93068352293787,12.5893111709658));
#443276=CARTESIAN_POINT('Ctrl Pts',(1.88108594645952,-1.90362914349933,
12.5737548217797));
#443277=CARTESIAN_POINT('Ctrl Pts',(1.88017645726634,-1.90320825273144,
12.5746934679442));
#443278=CARTESIAN_POINT('Ctrl Pts',(1.87909311232341,-1.90290875452966,
12.5756680099006));
#443279=CARTESIAN_POINT('Ctrl Pts',(1.87796005283771,-1.90276151367305,
12.5765688348656));
#443280=CARTESIAN_POINT('Ctrl Pts',(1.87766008788226,-1.90272253328627,
12.5768073183026));
#443281=CARTESIAN_POINT('Ctrl Pts',(1.87735673277619,-1.90269398490945,
12.5770407398754));
#443282=CARTESIAN_POINT('Ctrl Pts',(1.87705235893604,-1.9026758821933,12.5772674179684));
#443283=CARTESIAN_POINT('Ctrl Pts',(1.8758032910022,-1.9026015935414,12.5781976435658));
#443284=CARTESIAN_POINT('Ctrl Pts',(1.87446545326703,-1.90271025667737,
12.5790594849312));
#443285=CARTESIAN_POINT('Ctrl Pts',(1.87313308795987,-1.90304266517898,
12.5797571720116));
#443286=CARTESIAN_POINT('Ctrl Pts',(1.87226500405466,-1.90325924127013,
12.580211740231));
#443287=CARTESIAN_POINT('Ctrl Pts',(1.87136433750344,-1.90359885390805,
12.5806009430798));
#443288=CARTESIAN_POINT('Ctrl Pts',(1.87050074210857,-1.90405417320073,
12.5808812374708));
#443289=CARTESIAN_POINT('Ctrl Pts',(1.8697586271696,-1.90444544352375,12.5811221033394));
#443290=CARTESIAN_POINT('Ctrl Pts',(1.86902874762281,-1.904930268853,12.581287365893));
#443291=CARTESIAN_POINT('Ctrl Pts',(1.86835691251821,-1.9054882302098,12.581359338449));
#443292=CARTESIAN_POINT('Ctrl Pts',(1.86826354131154,-1.90556577531693,
12.5813693411482));
#443293=CARTESIAN_POINT('Ctrl Pts',(1.86817123982759,-1.90564470238592,
12.5813775999465));
#443294=CARTESIAN_POINT('Ctrl Pts',(1.86808007780993,-1.90572492611198,
12.5813841266931));
#443295=CARTESIAN_POINT('Ctrl Pts',(1.86792541042117,-1.9058610353661,12.5813952001081));
#443296=CARTESIAN_POINT('Ctrl Pts',(1.86777338936446,-1.90600224575675,
12.5814007534795));
#443297=CARTESIAN_POINT('Ctrl Pts',(1.86762421506604,-1.90614864027351,
12.5814005856065));
#443298=CARTESIAN_POINT('Ctrl Pts',(1.86694135345125,-1.9068187771347,12.5813998171494));
#443299=CARTESIAN_POINT('Ctrl Pts',(1.86636508834534,-1.90755100259751,
12.58127954464));
#443300=CARTESIAN_POINT('Ctrl Pts',(1.86587543933797,-1.90832286006927,
12.5810700125799));
#443301=CARTESIAN_POINT('Ctrl Pts',(1.86528399908806,-1.90925517601214,
12.5808169217085));
#443302=CARTESIAN_POINT('Ctrl Pts',(1.86483300952404,-1.91025436406882,
12.5804173076348));
#443303=CARTESIAN_POINT('Ctrl Pts',(1.86453825807857,-1.91122214346158,
12.5799304713245));
#443304=CARTESIAN_POINT('Ctrl Pts',(1.86417296818135,-1.91242152701115,
12.5793271277669));
#443305=CARTESIAN_POINT('Ctrl Pts',(1.86399418173403,-1.91363768827293,
12.5785808224116));
#443306=CARTESIAN_POINT('Ctrl Pts',(1.86397805533941,-1.91481475063423,
12.5777485681082));
#443307=CARTESIAN_POINT('Ctrl Pts',(1.86395402524464,-1.91656870250939,
12.576508418016));
#443308=CARTESIAN_POINT('Ctrl Pts',(1.86428450055372,-1.91822097536242,
12.5750928681475));
#443309=CARTESIAN_POINT('Ctrl Pts',(1.86486164992115,-1.91952579576338,
12.5737548217797));
#443310=CARTESIAN_POINT('Ctrl Pts',(1.86486164992115,-1.91952579576338,
12.5737548217797));
#443311=CARTESIAN_POINT('Ctrl Pts',(1.85106604772008,-1.92832835418493,
12.5770542771492));
#443312=CARTESIAN_POINT('Ctrl Pts',(1.85527432946227,-1.93885208923186,
12.5893111709658));
#443313=CARTESIAN_POINT('Ctrl Pts',(1.87410147022428,-1.94249622621072,
12.5508408821982));
#443314=CARTESIAN_POINT('Ctrl Pts',(1.86026139638963,-1.95132334810186,
12.55409748406));
#443315=CARTESIAN_POINT('Ctrl Pts',(1.86447504682153,-1.96186050873944,
12.5663972313419));
#443316=CARTESIAN_POINT('Ctrl Pts',(1.88333117008723,-1.96544465762183,
12.52790050457));
#443317=CARTESIAN_POINT('Ctrl Pts',(1.86943913377784,-1.97427430113219,
12.5311362602938));
#443318=CARTESIAN_POINT('Ctrl Pts',(1.87366648216885,-1.9848457165325,12.5434568539655));
#443319=CARTESIAN_POINT('Ctrl Pts',(1.89255152315046,-1.98837280477215,
12.5049357605811));
#443320=CARTESIAN_POINT('Ctrl Pts',(1.87860109577067,-1.99718580431321,
12.5081700652078));
#443321=CARTESIAN_POINT('Ctrl Pts',(1.88284936247329,-2.00780953055728,
12.5204921097672));
#443322=CARTESIAN_POINT('Ctrl Pts',(1.89194607715313,-1.98686725334684,
12.5064436508395));
#443323=CARTESIAN_POINT('Ctrl Pts',(1.89121837489207,-1.98784669053719,
12.5062361689309));
#443324=CARTESIAN_POINT('Ctrl Pts',(1.89041985871306,-1.98883419422443,
12.5061871075062));
#443325=CARTESIAN_POINT('Ctrl Pts',(1.88959444843154,-1.98974508088492,
12.5063648335164));
#443326=CARTESIAN_POINT('Ctrl Pts',(1.88921949616825,-1.99015886179194,
12.5064455676329));
#443327=CARTESIAN_POINT('Ctrl Pts',(1.88883360114652,-1.99056245593942,
12.506574497099));
#443328=CARTESIAN_POINT('Ctrl Pts',(1.88845254978506,-1.99093783212991,
12.5067492519495));
#443329=CARTESIAN_POINT('Ctrl Pts',(1.88768681228283,-1.99169216515579,
12.5071004286051));
#443330=CARTESIAN_POINT('Ctrl Pts',(1.88691191406805,-1.99235970551328,
12.5076537929613));
#443331=CARTESIAN_POINT('Ctrl Pts',(1.88619218858864,-1.99289751689347,
12.5083435010505));
#443332=CARTESIAN_POINT('Ctrl Pts',(1.88614687756862,-1.99293137533383,
12.5083869222964));
#443333=CARTESIAN_POINT('Ctrl Pts',(1.8861017731379,-1.99296471373106,12.5084308732337));
#443334=CARTESIAN_POINT('Ctrl Pts',(1.88605688625536,-1.99299751933776,
12.5084753333615));
#443335=CARTESIAN_POINT('Ctrl Pts',(1.885696834212,-1.99326066360302,12.5088319622689));
#443336=CARTESIAN_POINT('Ctrl Pts',(1.8853442311366,-1.99349591111127,12.509227847131));
#443337=CARTESIAN_POINT('Ctrl Pts',(1.88501111576401,-1.99369859596769,
12.5096423454524));
#443338=CARTESIAN_POINT('Ctrl Pts',(1.88396727961702,-1.99433372060314,
12.5109411997424));
#443339=CARTESIAN_POINT('Ctrl Pts',(1.88305561986995,-1.99469643067363,
12.5124831113042));
#443340=CARTESIAN_POINT('Ctrl Pts',(1.88227284260661,-1.99488130422901,
12.5140723025008));
#443341=CARTESIAN_POINT('Ctrl Pts',(1.88219949551968,-1.99489862708363,
12.5142212114565));
#443342=CARTESIAN_POINT('Ctrl Pts',(1.88212726864014,-1.994914415891,12.5143705582413));
#443343=CARTESIAN_POINT('Ctrl Pts',(1.88205615419293,-1.99492876466862,
12.5145201959299));
#443344=CARTESIAN_POINT('Ctrl Pts',(1.88114258324015,-1.99511309608021,
12.5164425148273));
#443345=CARTESIAN_POINT('Ctrl Pts',(1.88038342111312,-1.9950766180836,12.518463520594));
#443346=CARTESIAN_POINT('Ctrl Pts',(1.87972909895249,-1.99489470246884,
12.5205025929157));
#443347=CARTESIAN_POINT('Ctrl Pts',(1.87934956616441,-1.99478918420182,
12.5216853356836));
#443348=CARTESIAN_POINT('Ctrl Pts',(1.87900586242571,-1.99463539052657,
12.5228750347131));
#443349=CARTESIAN_POINT('Ctrl Pts',(1.87869344376144,-1.99445099305703,
12.5240609649613));
#443350=CARTESIAN_POINT('Ctrl Pts',(1.87792662891068,-1.99399839936065,
12.5269717671327));
#443351=CARTESIAN_POINT('Ctrl Pts',(1.877331987757,-1.99333974855292,12.5299036066169));
#443352=CARTESIAN_POINT('Ctrl Pts',(1.87685537220185,-1.99254269790286,
12.532813300402));
#443353=CARTESIAN_POINT('Ctrl Pts',(1.8766265689829,-1.99216006717997,12.5342101228452));
#443354=CARTESIAN_POINT('Ctrl Pts',(1.87642570073608,-1.99174574984497,
12.5356023438238));
#443355=CARTESIAN_POINT('Ctrl Pts',(1.87625044290219,-1.99130747926497,
12.5369868989719));
#443356=CARTESIAN_POINT('Origin',(6.6038514439667,-13.8279828798786,-1.24062368834839));
#443357=CARTESIAN_POINT('Ctrl Pts',(1.95258191307926,-1.91646346508713,
12.5369868989719));
#443358=CARTESIAN_POINT('Ctrl Pts',(1.96669379917423,-1.92247495196876,
12.5369868989719));
#443359=CARTESIAN_POINT('Ctrl Pts',(1.97721412737488,-1.9113122462826,12.5369868989719));
#443360=CARTESIAN_POINT('Ctrl Pts',(1.95735230844105,-1.91849552184576,
12.5218025310016));
#443361=CARTESIAN_POINT('Ctrl Pts',(1.96908740451166,-1.91988957489999,
12.5216901060418));
#443362=CARTESIAN_POINT('Ctrl Pts',(1.97718206992965,-1.91134628521992,
12.5161920673677));
#443363=CARTESIAN_POINT('Ctrl Pts',(1.95866847427007,-1.92437801950455,
12.5042015548895));
#443364=CARTESIAN_POINT('Ctrl Pts',(1.96508584297928,-1.92393674423044,
12.4980677368513));
#443365=CARTESIAN_POINT('Ctrl Pts',(1.96983613301335,-1.91907613477113,
12.4907278922778));
#443366=CARTESIAN_POINT('Ctrl Pts',(1.94784670917394,-1.93206751720659,
12.506463626192));
#443367=CARTESIAN_POINT('Ctrl Pts',(1.95249190125991,-1.93667507934082,
12.4999376786891));
#443368=CARTESIAN_POINT('Ctrl Pts',(1.95243516699269,-1.93661880466874,
12.4906970594712));
#443369=CARTESIAN_POINT('Origin',(1.96120393315497,-1.8962233867816,12.5369868989719));
#443370=CARTESIAN_POINT('Origin',(1.96120393315497,-1.8962233867816,14.));
#443371=CARTESIAN_POINT('Origin',(1.96120393315497,-1.8962233867816,13.7435492065112));
#443372=CARTESIAN_POINT('Ctrl Pts',(1.92982261285273,-1.90681934310076,
13.793642941384));
#443373=CARTESIAN_POINT('Ctrl Pts',(1.93976736345518,-1.9110629446915,13.8071662555867));
#443374=CARTESIAN_POINT('Ctrl Pts',(1.94868154685581,-1.89655237206551,
13.8103758687955));
#443375=CARTESIAN_POINT('Ctrl Pts',(1.94512645060691,-1.91330426832906,
13.7804579775006));
#443376=CARTESIAN_POINT('Ctrl Pts',(1.95740135403334,-1.91853116201464,
13.7901904343352));
#443377=CARTESIAN_POINT('Ctrl Pts',(1.96771222574423,-1.90661722694993,
13.7927914348263));
#443378=CARTESIAN_POINT('Ctrl Pts',(1.95413639585587,-1.91712218783116,
13.7597120340895));
#443379=CARTESIAN_POINT('Ctrl Pts',(1.9683441610124,-1.9231659035119,13.7635825532445));
#443380=CARTESIAN_POINT('Ctrl Pts',(1.97894654617859,-1.91252986360357,
13.7651073818884));
#443381=CARTESIAN_POINT('Ctrl Pts',(1.95237204227213,-1.91637455177148,
13.7381884353898));
#443382=CARTESIAN_POINT('Ctrl Pts',(1.96624689637753,-1.92227763013618,
13.7368803041982));
#443383=CARTESIAN_POINT('Ctrl Pts',(1.97674676259257,-1.91137155629702,
13.7363986145813));
#443384=CARTESIAN_POINT('Origin',(1.94211960510586,-1.88813650159725,13.7902182540695));
#443385=CARTESIAN_POINT('Ctrl Pts',(1.90060016204145,-1.89443650955962,
13.8235227101244));
#443386=CARTESIAN_POINT('Ctrl Pts',(1.91118432040462,-1.89892630688945,
13.8358800583119));
#443387=CARTESIAN_POINT('Ctrl Pts',(1.92028864223977,-1.88507938040814,
13.8390832900376));
#443388=CARTESIAN_POINT('Ctrl Pts',(1.91158243810205,-1.89909019216838,
13.8124254819053));
#443389=CARTESIAN_POINT('Ctrl Pts',(1.92218715085937,-1.90358870836491,
13.8247886449157));
#443390=CARTESIAN_POINT('Ctrl Pts',(1.93128873470291,-1.8897149218363,13.8279860620657));
#443391=CARTESIAN_POINT('Ctrl Pts',(1.92255979226383,-1.90374178914802,
13.8013225099955));
#443392=CARTESIAN_POINT('Ctrl Pts',(1.93318005491093,-1.90824690347943,
13.8136962257787));
#443393=CARTESIAN_POINT('Ctrl Pts',(1.94228362940331,-1.89434856701984,
13.8168830918626));
#443394=CARTESIAN_POINT('Ctrl Pts',(1.93353241603026,-1.90839138164714,
13.7902140179785));
#443395=CARTESIAN_POINT('Ctrl Pts',(1.94416355114511,-1.91290111198434,
13.802602731458));
#443396=CARTESIAN_POINT('Ctrl Pts',(1.95327352985902,-1.89898039216267,
13.8057746032558));
#443397=CARTESIAN_POINT('Origin',(1.90918733964419,-1.87418162464462,13.8235269408515));
#443398=CARTESIAN_POINT('Ctrl Pts',(1.85527432946228,-1.93885208923186,
13.8235269408515));
#443399=CARTESIAN_POINT('Ctrl Pts',(1.85965842924394,-1.94981549599689,
13.8362179249168));
#443400=CARTESIAN_POINT('Ctrl Pts',(1.84503555961608,-1.95863789294465,
13.8391868794938));
#443401=CARTESIAN_POINT('Ctrl Pts',(1.85126306899057,-1.92882104925058,
13.8400110824519));
#443402=CARTESIAN_POINT('Ctrl Pts',(1.85160160074639,-1.93888123111336,
13.8494522556837));
#443403=CARTESIAN_POINT('Ctrl Pts',(1.83853848221819,-1.94208791503196,
13.85569149686));
#443404=CARTESIAN_POINT('Ctrl Pts',(1.85193651668582,-1.91254394280478,
13.8586819406588));
#443405=CARTESIAN_POINT('Ctrl Pts',(1.84883638532394,-1.91560093956207,
13.868010383617));
#443406=CARTESIAN_POINT('Ctrl Pts',(1.83980229368401,-1.91507363032288,
13.8744918421245));
#443407=CARTESIAN_POINT('Ctrl Pts',(1.87424956885007,-1.89060768968211,
13.8587686893867));
#443408=CARTESIAN_POINT('Ctrl Pts',(1.8773220695356,-1.88757786007349,13.8680909899357));
#443409=CARTESIAN_POINT('Ctrl Pts',(1.87694877675283,-1.87855804555188,
13.8745789365163));
#443410=CARTESIAN_POINT('Ctrl Pts',(1.89064047068469,-1.89021614273967,
13.8400379222776));
#443411=CARTESIAN_POINT('Ctrl Pts',(1.90068947670203,-1.89075253063221,
13.8494748685453));
#443412=CARTESIAN_POINT('Ctrl Pts',(1.90416144873845,-1.87776382340465,
13.8557104837033));
#443413=CARTESIAN_POINT('Ctrl Pts',(1.90060378598842,-1.89443804600545,
13.8235269408542));
#443414=CARTESIAN_POINT('Ctrl Pts',(1.91147548235422,-1.89904487104231,
13.8362179249195));
#443415=CARTESIAN_POINT('Ctrl Pts',(1.92059432876269,-1.88460500801543,
13.8391868794965));
#443416=CARTESIAN_POINT('Origin',(1.83484703094532,-1.94702065552585,13.8235269408515));
#443417=CARTESIAN_POINT('Ctrl Pts',(1.86855306805532,-1.97205850075201,
13.7902140241682));
#443418=CARTESIAN_POINT('Ctrl Pts',(1.87284499268163,-1.98277941388451,
13.8026027327198));
#443419=CARTESIAN_POINT('Ctrl Pts',(1.85874134473945,-1.99160353123393,
13.8057746032556));
#443420=CARTESIAN_POINT('Ctrl Pts',(1.86412826848003,-1.96099331518913,
13.8013225161808));
#443421=CARTESIAN_POINT('Ctrl Pts',(1.86841579985604,-1.97170326395582,
13.8136962270464));
#443422=CARTESIAN_POINT('Ctrl Pts',(1.85433466124407,-1.9805214350079,13.8168830918628));
#443423=CARTESIAN_POINT('Ctrl Pts',(1.85970156133385,-1.94992335932521,
13.8124254880875));
#443424=CARTESIAN_POINT('Ctrl Pts',(1.86398281315726,-1.96061762684874,
13.8247886461867));
#443425=CARTESIAN_POINT('Ctrl Pts',(1.84992625996228,-1.96943430845097,
13.8279860620656));
#443426=CARTESIAN_POINT('Ctrl Pts',(1.85527286939083,-1.93884844003976,
13.8235227163065));
#443427=CARTESIAN_POINT('Ctrl Pts',(1.85954582345754,-1.94952197960172,
13.8358800595848));
#443428=CARTESIAN_POINT('Ctrl Pts',(1.84551606885698,-1.95834194653172,
13.8390832900376));
#443429=CARTESIAN_POINT('Origin',(1.84812723423304,-1.98023072779073,13.7902182540695));
#443430=CARTESIAN_POINT('Ctrl Pts',(1.87615021872148,-1.99105692092633,
13.7382347919292));
#443431=CARTESIAN_POINT('Ctrl Pts',(1.88177551032358,-2.00505956221734,
13.7369371795942));
#443432=CARTESIAN_POINT('Ctrl Pts',(1.87064331463721,-2.01533662387039,
13.7364597369711));
#443433=CARTESIAN_POINT('Ctrl Pts',(1.87685255190966,-1.99281325861511,
13.7595490285574));
#443434=CARTESIAN_POINT('Ctrl Pts',(1.88261112519184,-2.00715036572127,
13.7633824266926));
#443435=CARTESIAN_POINT('Ctrl Pts',(1.87174320642998,-2.01753217683941,
13.7648920890506));
#443436=CARTESIAN_POINT('Ctrl Pts',(1.87327069113429,-1.98385603261937,
13.7803806590111));
#443437=CARTESIAN_POINT('Ctrl Pts',(1.87825666038903,-1.99625510502802,
13.7901039518744));
#443438=CARTESIAN_POINT('Ctrl Pts',(1.86613915747838,-2.00633734508844,
13.7926933640892));
#443439=CARTESIAN_POINT('Ctrl Pts',(1.86704461746326,-1.96828637436314,
13.7936647693663));
#443440=CARTESIAN_POINT('Ctrl Pts',(1.87108818227528,-1.97831747178844,
13.8072068914933));
#443441=CARTESIAN_POINT('Ctrl Pts',(1.85637763805206,-1.98693397679362,
13.8104111085397));
#443442=CARTESIAN_POINT('Origin',(1.85582314438524,-1.99947604555896,13.7435492065112));
#443443=CARTESIAN_POINT('Origin',(1.85582314438524,-1.99947604555896,14.));
#443444=CARTESIAN_POINT('Origin',(1.85582314438524,-1.99947604555896,12.5369868989719));
#443445=CARTESIAN_POINT('Ctrl Pts',(1.8919334001501,-1.9868539403086,12.506462012331));
#443446=CARTESIAN_POINT('Ctrl Pts',(1.8964424096848,-1.99158917219372,12.4999388158272));
#443447=CARTESIAN_POINT('Ctrl Pts',(1.8963890621888,-1.99153314819065,12.4907030323752));
#443448=CARTESIAN_POINT('Ctrl Pts',(1.88402337332597,-1.99751508746996,
12.5042014951932));
#443449=CARTESIAN_POINT('Ctrl Pts',(1.88345248703998,-2.00391939742223,
12.4980716682127));
#443450=CARTESIAN_POINT('Ctrl Pts',(1.87850056391531,-2.00856741017965,
12.4907355092743));
#443451=CARTESIAN_POINT('Ctrl Pts',(1.87816922398865,-1.99608168704376,
12.5218047446509));
#443452=CARTESIAN_POINT('Ctrl Pts',(1.87932192270261,-2.00783711798486,
12.5216906929434));
#443453=CARTESIAN_POINT('Ctrl Pts',(1.87062222136042,-2.01575456396743,
12.5161988840776));
#443454=CARTESIAN_POINT('Ctrl Pts',(1.87623614791533,-1.99127182183696,
12.5369868989719));
#443455=CARTESIAN_POINT('Ctrl Pts',(1.88195295920137,-2.00549587190157,
12.5369868989719));
#443456=CARTESIAN_POINT('Ctrl Pts',(1.87058881422157,-2.01578478537184,
12.5369868989719));
#443457=CARTESIAN_POINT('Origin',(3.60557045705457E-31,-8.83174710230759E-31,
12.5));
#443458=CARTESIAN_POINT('Origin',(2.00713550187736,-1.78117863747125,12.5));
#443459=CARTESIAN_POINT('',(2.00713550187736,-1.78117863747125,12.5893111709658));
#443460=CARTESIAN_POINT('',(2.00713550187736,-1.78117863747125,13.8235269408515));
#443461=CARTESIAN_POINT('',(2.00713550187736,-1.78117863747125,12.5));
#443462=CARTESIAN_POINT('',(2.02307844558103,-1.81319574610497,13.7902182540695));
#443463=CARTESIAN_POINT('',(2.00713550187736,-1.78117863747125,13.8235269408515));
#443464=CARTESIAN_POINT('',(2.03231742029,-1.8317497385432,13.7435492065112));
#443465=CARTESIAN_POINT('Origin',(2.00192160722038,-1.77070720346282,13.7445212918691));
#443466=CARTESIAN_POINT('',(2.03231742029,-1.8317497385432,12.5369868989719));
#443467=CARTESIAN_POINT('',(2.03231742029,-1.8317497385432,12.5));
#443468=CARTESIAN_POINT('Ctrl Pts',(2.03231742029,-1.8317497385432,12.5369868989719));
#443469=CARTESIAN_POINT('Ctrl Pts',(2.02392956953902,-1.81490499934765,
12.5544431401645));
#443470=CARTESIAN_POINT('Ctrl Pts',(2.01553571957424,-1.79804821234693,
12.5718848856037));
#443471=CARTESIAN_POINT('Ctrl Pts',(2.00713550187736,-1.78117863747125,
12.5893111709658));
#443472=CARTESIAN_POINT('Origin',(2.30980221034265,-1.81951643427433,12.5));
#443473=CARTESIAN_POINT('',(2.10233409235843,-1.75094619151324,13.7435492065112));
#443474=CARTESIAN_POINT('',(2.08265410961905,-1.74444176467848,13.7902182540695));
#443475=CARTESIAN_POINT('Origin',(2.03093851636564,-1.72734925514798,13.741873268045));
#443476=CARTESIAN_POINT('',(2.04869397153158,-1.73321760679108,13.8235269408515));
#443477=CARTESIAN_POINT('',(2.08265410961905,-1.74444176467848,13.7902182540695));
#443478=CARTESIAN_POINT('',(2.04869397153158,-1.73321760679108,12.5893111709658));
#443479=CARTESIAN_POINT('',(2.04869397153158,-1.73321760679108,12.5));
#443480=CARTESIAN_POINT('',(2.10233409235843,-1.75094619151324,12.5369868989719));
#443481=CARTESIAN_POINT('Ctrl Pts',(2.04869397153158,-1.73321760679108,
12.5893111709658));
#443482=CARTESIAN_POINT('Ctrl Pts',(2.06658731408194,-1.73913153156374,
12.5718848856037));
#443483=CARTESIAN_POINT('Ctrl Pts',(2.0844670926967,-1.74504097332299,12.5544431401645));
#443484=CARTESIAN_POINT('Ctrl Pts',(2.10233409235843,-1.75094619151324,
12.5369868989719));
#443485=CARTESIAN_POINT('',(2.10233409235843,-1.75094619151324,12.5));
#443486=CARTESIAN_POINT('Origin',(2.03790661809618,-1.76585613664246,12.5));
#443487=CARTESIAN_POINT('',(2.01120891650976,-1.74420381800956,13.8587068136939));
#443488=CARTESIAN_POINT('Ctrl Pts',(2.04869397153352,-1.73321760678476,
13.8235269408542));
#443489=CARTESIAN_POINT('Ctrl Pts',(2.04703019142421,-1.73266771118102,
13.8262006681044));
#443490=CARTESIAN_POINT('Ctrl Pts',(2.04527303375369,-1.73226993617813,
13.8288634856214));
#443491=CARTESIAN_POINT('Ctrl Pts',(2.0434306770714,-1.73201375004417,13.8314912288862));
#443492=CARTESIAN_POINT('Ctrl Pts',(2.04153139736224,-1.73174964856444,
13.8342001611531));
#443493=CARTESIAN_POINT('Ctrl Pts',(2.03953953134991,-1.73163523491821,
13.8368750301949));
#443494=CARTESIAN_POINT('Ctrl Pts',(2.03743894388263,-1.73169656525377,
13.8394886372968));
#443495=CARTESIAN_POINT('Ctrl Pts',(2.03727671041721,-1.73170130194435,
13.8396904925131));
#443496=CARTESIAN_POINT('Ctrl Pts',(2.03711382526724,-1.73170710884023,
13.8398919674349));
#443497=CARTESIAN_POINT('Ctrl Pts',(2.03695028035863,-1.73171400937099,
13.8400930404591));
#443498=CARTESIAN_POINT('Ctrl Pts',(2.0344021406548,-1.73182152428264,13.8432258934518));
#443499=CARTESIAN_POINT('Ctrl Pts',(2.03170679445772,-1.73219285400258,
13.8462331177034));
#443500=CARTESIAN_POINT('Ctrl Pts',(2.02896531497625,-1.73291145142553,
13.8489036603661));
#443501=CARTESIAN_POINT('Ctrl Pts',(2.02806827098571,-1.73314658486506,
13.8497774930041));
#443502=CARTESIAN_POINT('Ctrl Pts',(2.02716652460944,-1.73341897878829,
13.85061494757));
#443503=CARTESIAN_POINT('Ctrl Pts',(2.02626429740108,-1.73373177231457,
13.8514076489583));
#443504=CARTESIAN_POINT('Ctrl Pts',(2.02435595673476,-1.73439337573422,
13.8530843267192));
#443505=CARTESIAN_POINT('Ctrl Pts',(2.02225898453563,-1.73530350193597,
13.8546805203176));
#443506=CARTESIAN_POINT('Ctrl Pts',(2.02014941240931,-1.73653449270823,
13.8559412814273));
#443507=CARTESIAN_POINT('Ctrl Pts',(2.01986708324376,-1.73669923919554,
13.8561100121513));
#443508=CARTESIAN_POINT('Ctrl Pts',(2.01958454189996,-1.73686965709972,
13.8562727473908));
#443509=CARTESIAN_POINT('Ctrl Pts',(2.01930221422283,-1.73704584408123,
13.8564289040185));
#443510=CARTESIAN_POINT('Ctrl Pts',(2.01802186142799,-1.73784485003235,
13.8571370725437));
#443511=CARTESIAN_POINT('Ctrl Pts',(2.01672460309047,-1.73877847905152,
13.8577210840554));
#443512=CARTESIAN_POINT('Ctrl Pts',(2.01547800727154,-1.73983426121297,
13.8581177131616));
#443513=CARTESIAN_POINT('Ctrl Pts',(2.01512692298241,-1.74013160580855,
13.8582294175695));
#443514=CARTESIAN_POINT('Ctrl Pts',(2.01477977113041,-1.74043848394319,
13.8583265086086));
#443515=CARTESIAN_POINT('Ctrl Pts',(2.01443782564897,-1.74075424584243,
13.8584082369006));
#443516=CARTESIAN_POINT('Ctrl Pts',(2.01394654168844,-1.74120791101673,
13.8585256585398));
#443517=CARTESIAN_POINT('Ctrl Pts',(2.01346011625631,-1.74168579172336,
13.8586122832068));
#443518=CARTESIAN_POINT('Ctrl Pts',(2.01299173869888,-1.7421760373254,13.8586682984299));
#443519=CARTESIAN_POINT('Ctrl Pts',(2.01261708308171,-1.74256818521055,
13.8587131050557));
#443520=CARTESIAN_POINT('Ctrl Pts',(2.01224966762582,-1.74297241396452,
13.8587357943552));
#443521=CARTESIAN_POINT('Ctrl Pts',(2.01188982344196,-1.74338911226008,
13.8587355499465));
#443522=CARTESIAN_POINT('Ctrl Pts',(2.01165724756682,-1.74365843430307,
13.8587353919793));
#443523=CARTESIAN_POINT('Ctrl Pts',(2.01143032024835,-1.74393002761568,
13.8587257282814));
#443524=CARTESIAN_POINT('Ctrl Pts',(2.01120891650976,-1.74420381800956,
13.8587068136939));
#443525=CARTESIAN_POINT('Ctrl Pts',(2.01120891650976,-1.74420381800956,
13.8587068136939));
#443526=CARTESIAN_POINT('Ctrl Pts',(2.0104807316836,-1.74510429968908,13.8586446046466));
#443527=CARTESIAN_POINT('Ctrl Pts',(2.00981222217124,-1.74602851885042,
13.858482427929));
#443528=CARTESIAN_POINT('Ctrl Pts',(2.009199594715,-1.74697410966319,13.8582284286032));
#443529=CARTESIAN_POINT('Ctrl Pts',(2.00857111020862,-1.74794417584149,
13.8579678548414));
#443530=CARTESIAN_POINT('Ctrl Pts',(2.00800118829375,-1.74893993676411,
13.857615680862));
#443531=CARTESIAN_POINT('Ctrl Pts',(2.00750388806282,-1.74991732204527,
13.8571944833187));
#443532=CARTESIAN_POINT('Ctrl Pts',(2.00626282447684,-1.75235648697316,
13.8561433417727));
#443533=CARTESIAN_POINT('Ctrl Pts',(2.00541172391119,-1.75479312971158,
13.8546163505475));
#443534=CARTESIAN_POINT('Ctrl Pts',(2.00484824601392,-1.75704757188396,
13.8528973491086));
#443535=CARTESIAN_POINT('Ctrl Pts',(2.00474530691543,-1.75745942520767,
13.8525833129073));
#443536=CARTESIAN_POINT('Ctrl Pts',(2.00465182947333,-1.75786523072994,
13.8522628768812));
#443537=CARTESIAN_POINT('Ctrl Pts',(2.00456702448517,-1.75826396129958,
13.851937733538));
#443538=CARTESIAN_POINT('Ctrl Pts',(2.00404913218869,-1.76069895356687,
13.8499521282529));
#443539=CARTESIAN_POINT('Ctrl Pts',(2.00380718853504,-1.76311293512796,
13.847639871647));
#443540=CARTESIAN_POINT('Ctrl Pts',(2.00377396899834,-1.76537102395243,
13.8452109780794));
#443541=CARTESIAN_POINT('Ctrl Pts',(2.00375902284116,-1.76638698485467,
13.8441181685877));
#443542=CARTESIAN_POINT('Ctrl Pts',(2.00378565136409,-1.76737162690378,
13.8430021611332));
#443543=CARTESIAN_POINT('Ctrl Pts',(2.003845104092,-1.76831467595735,13.8418824960098));
#443544=CARTESIAN_POINT('Ctrl Pts',(2.0039852059635,-1.77053699513369,13.8392439765549));
#443545=CARTESIAN_POINT('Ctrl Pts',(2.00431051030166,-1.77263481382212,
13.8364981347964));
#443546=CARTESIAN_POINT('Ctrl Pts',(2.00478806104262,-1.77461892377942,
13.8336931113419));
#443547=CARTESIAN_POINT('Ctrl Pts',(2.00525316513704,-1.77655132087521,
13.8309611966328));
#443548=CARTESIAN_POINT('Ctrl Pts',(2.00586369773226,-1.77837766363799,
13.8281701127186));
#443549=CARTESIAN_POINT('Ctrl Pts',(2.00662145782579,-1.78008545484899,
13.8253580685121));
#443550=CARTESIAN_POINT('Ctrl Pts',(2.00678574103186,-1.78045570582664,
13.8247484142933));
#443551=CARTESIAN_POINT('Ctrl Pts',(2.00695703658691,-1.78082023800011,
13.8241378483365));
#443552=CARTESIAN_POINT('Ctrl Pts',(2.00713550187736,-1.78117863747125,
13.8235269408515));
#443553=CARTESIAN_POINT('',(2.01200857389031,-1.7432533839341,12.5969504640361));
#443554=CARTESIAN_POINT('Origin',(2.03793149415634,-1.76587795095981,12.584524458991));
#443555=CARTESIAN_POINT('Origin',(2.03793149415634,-1.76587795095981,12.584524458991));
#443556=CARTESIAN_POINT('Ctrl Pts',(2.04869397153158,-1.73321760679108,
12.5893111709658));
#443557=CARTESIAN_POINT('Ctrl Pts',(2.03793255275058,-1.72966085259946,
12.5770542771492));
#443558=CARTESIAN_POINT('Ctrl Pts',(2.02999023577727,-1.74396900677638,
12.5737548217797));
#443559=CARTESIAN_POINT('Ctrl Pts',(2.07222558276616,-1.74099503452596,
12.5663937883685));
#443560=CARTESIAN_POINT('Ctrl Pts',(2.06145043630097,-1.73743374320043,
12.5540940315304));
#443561=CARTESIAN_POINT('Ctrl Pts',(2.0534863153349,-1.7517877939371,12.5508374392248));
#443562=CARTESIAN_POINT('Ctrl Pts',(2.09573345089345,-1.74876461493159,
12.5434499600945));
#443563=CARTESIAN_POINT('Ctrl Pts',(2.08492327059005,-1.74519174457971,
12.5311293540533));
#443564=CARTESIAN_POINT('Ctrl Pts',(2.07695981126174,-1.75959782246685,
12.5278936106989));
#443565=CARTESIAN_POINT('Ctrl Pts',(2.11921943574361,-1.75652696270004,
12.5204817579905));
#443566=CARTESIAN_POINT('Ctrl Pts',(2.10835575243537,-1.75293640908167,
12.5081597038247));
#443567=CARTESIAN_POINT('Ctrl Pts',(2.10041248322022,-1.76739975997523,
12.5049254088044));
#443568=CARTESIAN_POINT('Ctrl Pts',(2.10233409235843,-1.75094619151324,
12.5369868989719));
#443569=CARTESIAN_POINT('Ctrl Pts',(2.10321854167028,-1.75123851083435,
12.5342545179733));
#443570=CARTESIAN_POINT('Ctrl Pts',(2.10402347267165,-1.75163593151374,
12.5314872231885));
#443571=CARTESIAN_POINT('Ctrl Pts',(2.10467879432935,-1.75216619054014,
12.5287124745063));
#443572=CARTESIAN_POINT('Ctrl Pts',(2.10526979592752,-1.75264440444987,
12.5262100684184));
#443573=CARTESIAN_POINT('Ctrl Pts',(2.10573790029822,-1.75323094228825,
12.5237004536639));
#443574=CARTESIAN_POINT('Ctrl Pts',(2.10603933229401,-1.75397722596309,
12.5212220730815));
#443575=CARTESIAN_POINT('Ctrl Pts',(2.10627010456274,-1.75454857067487,
12.5193246583486));
#443576=CARTESIAN_POINT('Ctrl Pts',(2.10640535602598,-1.75522061209085,
12.517417831369));
#443577=CARTESIAN_POINT('Ctrl Pts',(2.10635542532018,-1.75603096487088,
12.5155812248348));
#443578=CARTESIAN_POINT('Ctrl Pts',(2.10633415457113,-1.75637617951085,
12.5147988205793));
#443579=CARTESIAN_POINT('Ctrl Pts',(2.10627953176126,-1.75674686245539,
12.5140295443047));
#443580=CARTESIAN_POINT('Ctrl Pts',(2.10618630501999,-1.75714722669898,
12.5132817086137));
#443581=CARTESIAN_POINT('Ctrl Pts',(2.10604521895852,-1.75775312382161,
12.5121499604604));
#443582=CARTESIAN_POINT('Ctrl Pts',(2.1058057073659,-1.7584384611939,12.5110494206568));
#443583=CARTESIAN_POINT('Ctrl Pts',(2.10543053053311,-1.75920291816315,
12.5100666561695));
#443584=CARTESIAN_POINT('Ctrl Pts',(2.10521510485967,-1.75964186759451,
12.5095023550641));
#443585=CARTESIAN_POINT('Ctrl Pts',(2.10495187492468,-1.76011168706704,
12.5089719619137));
#443586=CARTESIAN_POINT('Ctrl Pts',(2.10464020266777,-1.76060044845179,
12.5085043804652));
#443587=CARTESIAN_POINT('Ctrl Pts',(2.10418411091795,-1.76131568707273,
12.5078201359221));
#443588=CARTESIAN_POINT('Ctrl Pts',(2.10361003575668,-1.76209158379383,
12.5072563000949));
#443589=CARTESIAN_POINT('Ctrl Pts',(2.10295008531567,-1.76287050882346,
12.5068768744332));
#443590=CARTESIAN_POINT('Ctrl Pts',(2.10247421561655,-1.76343216739121,
12.5066032824114));
#443591=CARTESIAN_POINT('Ctrl Pts',(2.10194538140866,-1.76400530681686,
12.5064197834844));
#443592=CARTESIAN_POINT('Ctrl Pts',(2.10139501388842,-1.76455967437539,
12.5063282718343));
#443593=CARTESIAN_POINT('Ctrl Pts',(2.10059164769835,-1.76536887938298,
12.5061946931565));
#443594=CARTESIAN_POINT('Ctrl Pts',(2.09972598336392,-1.76615613140112,
12.5062515701262));
#443595=CARTESIAN_POINT('Ctrl Pts',(2.09886215016502,-1.76688401313822,
12.5064436508398));
#443596=CARTESIAN_POINT('',(2.02999023577727,-1.74396900677638,12.5737548217797));
#443597=CARTESIAN_POINT('Origin',(2.04179006533292,-1.75410626589596,12.5893111709658));
#443598=CARTESIAN_POINT('Ctrl Pts',(2.09886215016502,-1.76688401313822,
12.5064436508398));
#443599=CARTESIAN_POINT('Ctrl Pts',(2.08866716582506,-1.76349245272168,
12.5164271754438));
#443600=CARTESIAN_POINT('Ctrl Pts',(2.07846820614843,-1.76009934963816,
12.5264061185523));
#443601=CARTESIAN_POINT('Ctrl Pts',(2.06826513082835,-1.75670465045431,
12.536380305637));
#443602=CARTESIAN_POINT('Ctrl Pts',(2.05551335608489,-1.75246196499368,
12.5488460165097));
#443603=CARTESIAN_POINT('Ctrl Pts',(2.04275514897594,-1.74821678515915,
12.5613043021964));
#443604=CARTESIAN_POINT('Ctrl Pts',(2.02999023577727,-1.74396900677638,
12.5737548217797));
#443605=CARTESIAN_POINT('Ctrl Pts',(2.00713550187736,-1.78117863747125,
12.5893111709658));
#443606=CARTESIAN_POINT('Ctrl Pts',(2.00208344074159,-1.77103293331431,
12.5770542771492));
#443607=CARTESIAN_POINT('Ctrl Pts',(2.01511564898407,-1.76113519502824,
12.5737548217797));
#443608=CARTESIAN_POINT('Ctrl Pts',(2.0024219727782,-1.7717127837355,12.5928319619712));
#443609=CARTESIAN_POINT('Ctrl Pts',(2.00194287567332,-1.76344211977573,
12.5821634970843));
#443610=CARTESIAN_POINT('Ctrl Pts',(2.01339017514108,-1.75769122095944,
12.5773203894503));
#443611=CARTESIAN_POINT('Ctrl Pts',(2.00189010517047,-1.75497058506903,
12.5969440695591));
#443612=CARTESIAN_POINT('Ctrl Pts',(2.00450865612942,-1.75192071073927,
12.5878292599214));
#443613=CARTESIAN_POINT('Ctrl Pts',(2.01320265161924,-1.75172389475533,
12.5813877129824));
#443614=CARTESIAN_POINT('Ctrl Pts',(2.02188608242554,-1.73181165290116,
12.596957478804));
#443615=CARTESIAN_POINT('Ctrl Pts',(2.01928694407814,-1.73483904005842,
12.5878468778671));
#443616=CARTESIAN_POINT('Ctrl Pts',(2.02036400407649,-1.74343889027209,
12.5814011370086));
#443617=CARTESIAN_POINT('Ctrl Pts',(2.03863908289381,-1.72989436772409,
12.5928371701607));
#443618=CARTESIAN_POINT('Ctrl Pts',(2.03039085245162,-1.73060271811505,
12.5821692192952));
#443619=CARTESIAN_POINT('Ctrl Pts',(2.02632414872455,-1.74274708894124,
12.5773318885715));
#443620=CARTESIAN_POINT('Ctrl Pts',(2.0486939715316,-1.73321760679102,12.5893111709658));
#443621=CARTESIAN_POINT('Ctrl Pts',(2.0379325527506,-1.72966085259941,12.5770542771492));
#443622=CARTESIAN_POINT('Ctrl Pts',(2.02999023577729,-1.74396900677632,
12.5737548217797));
#443623=CARTESIAN_POINT('',(2.01511564898407,-1.76113519502824,12.5737548217797));
#443624=CARTESIAN_POINT('Origin',(2.0268290162574,-1.77137223694082,12.5893111709658));
#443625=CARTESIAN_POINT('Ctrl Pts',(2.02999023577729,-1.74396900677632,
12.5737548217797));
#443626=CARTESIAN_POINT('Ctrl Pts',(2.02904946632942,-1.74362364830027,
12.5746934679442));
#443627=CARTESIAN_POINT('Ctrl Pts',(2.02794531424358,-1.74341344932419,
12.5756680099006));
#443628=CARTESIAN_POINT('Ctrl Pts',(2.02680402342312,-1.74335905326627,
12.5765688348656));
#443629=CARTESIAN_POINT('Ctrl Pts',(2.0265018793129,-1.74334465251212,12.5768073183026));
#443630=CARTESIAN_POINT('Ctrl Pts',(2.02619720663819,-1.74334092538503,
12.5770407398754));
#443631=CARTESIAN_POINT('Ctrl Pts',(2.02589237003745,-1.74334769219781,
12.5772674179684));
#443632=CARTESIAN_POINT('Ctrl Pts',(2.02464140305933,-1.74337546136766,
12.5781976435658));
#443633=CARTESIAN_POINT('Ctrl Pts',(2.02331687392322,-1.74359280913131,
12.5790594849312));
#443634=CARTESIAN_POINT('Ctrl Pts',(2.02201603633051,-1.74403271171266,
12.5797571720116));
#443635=CARTESIAN_POINT('Ctrl Pts',(2.02116849386492,-1.74431932406191,
12.580211740231));
#443636=CARTESIAN_POINT('Ctrl Pts',(2.02029850579014,-1.74473121935209,
12.5806009430798));
#443637=CARTESIAN_POINT('Ctrl Pts',(2.01947489668704,-1.7452554146493,12.5808812374708));
#443638=CARTESIAN_POINT('Ctrl Pts',(2.018767143238,-1.74570587230958,12.5811221033394));
#443639=CARTESIAN_POINT('Ctrl Pts',(2.01807921007043,-1.74624857638148,
12.581287365893));
#443640=CARTESIAN_POINT('Ctrl Pts',(2.01745508947216,-1.74685944196594,
12.581359338449));
#443641=CARTESIAN_POINT('Ctrl Pts',(2.0173683495966,-1.74694433966828,12.5813693411482));
#443642=CARTESIAN_POINT('Ctrl Pts',(2.01728278852707,-1.74703052754178,
12.5813775999465));
#443643=CARTESIAN_POINT('Ctrl Pts',(2.01719846882195,-1.74711791488075,
12.5813841266931));
#443644=CARTESIAN_POINT('Ctrl Pts',(2.01705541024395,-1.7472661780706,12.5813952001081));
#443645=CARTESIAN_POINT('Ctrl Pts',(2.01691540498254,-1.74741930972274,
12.5814007534795));
#443646=CARTESIAN_POINT('Ctrl Pts',(2.01677865956146,-1.74757737621402,
12.5814005856065));
#443647=CARTESIAN_POINT('Ctrl Pts',(2.0161526924878,-1.74830094281106,12.5813998171494));
#443648=CARTESIAN_POINT('Ctrl Pts',(2.01563802802936,-1.74907770280997,
12.58127954464));
#443649=CARTESIAN_POINT('Ctrl Pts',(2.01521292183819,-1.74988690292945,
12.5810700125799));
#443650=CARTESIAN_POINT('Ctrl Pts',(2.01469944196147,-1.75086432453896,
12.5808169217085));
#443651=CARTESIAN_POINT('Ctrl Pts',(2.01433139613065,-1.75189694771605,
12.5804173076348));
#443652=CARTESIAN_POINT('Ctrl Pts',(2.01411650845123,-1.75288553188186,
12.5799304713245));
#443653=CARTESIAN_POINT('Ctrl Pts',(2.01385019491983,-1.75411069909943,
12.5793271277669));
#443654=CARTESIAN_POINT('Ctrl Pts',(2.01377113180279,-1.75533738644016,
12.5785808224116));
#443655=CARTESIAN_POINT('Ctrl Pts',(2.01385100057718,-1.75651184667443,
12.5777485681082));
#443656=CARTESIAN_POINT('Ctrl Pts',(2.01397001380129,-1.75826192109522,
12.576508418016));
#443657=CARTESIAN_POINT('Ctrl Pts',(2.01443406505751,-1.75988175934096,
12.5750928681475));
#443658=CARTESIAN_POINT('Ctrl Pts',(2.01511564898407,-1.76113519502824,
12.5737548217797));
#443659=CARTESIAN_POINT('Ctrl Pts',(2.01511564898407,-1.76113519502824,
12.5737548217797));
#443660=CARTESIAN_POINT('Ctrl Pts',(2.00208344074159,-1.77103293331431,
12.5770542771492));
#443661=CARTESIAN_POINT('Ctrl Pts',(2.00713550187736,-1.78117863747125,
12.5893111709658));
#443662=CARTESIAN_POINT('Ctrl Pts',(2.02619702787589,-1.78327606213019,
12.5508408821982));
#443663=CARTESIAN_POINT('Ctrl Pts',(2.01312249812634,-1.79320190700391,
12.55409748406));
#443664=CARTESIAN_POINT('Ctrl Pts',(2.01818100439823,-1.80336055448091,
12.5663972313419));
#443665=CARTESIAN_POINT('Ctrl Pts',(2.03726652687681,-1.80539582830571,
12.52790050457));
#443666=CARTESIAN_POINT('Ctrl Pts',(2.02414041308868,-1.81532842183225,
12.5311362602938));
#443667=CARTESIAN_POINT('Ctrl Pts',(2.02921536382205,-1.82552009358126,
12.5434568539655));
#443668=CARTESIAN_POINT('Ctrl Pts',(2.04832505682313,-1.82749613956558,
12.5049357605811));
#443669=CARTESIAN_POINT('Ctrl Pts',(2.03513938961812,-1.8374169039186,12.5081700652078));
#443670=CARTESIAN_POINT('Ctrl Pts',(2.04023945287848,-1.84765900741473,
12.5204921097672));
#443671=CARTESIAN_POINT('Ctrl Pts',(2.04759890897939,-1.82604494720791,
12.5064436508395));
#443672=CARTESIAN_POINT('Ctrl Pts',(2.04695346131124,-1.82708043989174,
12.5062361689309));
#443673=CARTESIAN_POINT('Ctrl Pts',(2.04623809284699,-1.82812974422357,
12.5061871075061));
#443674=CARTESIAN_POINT('Ctrl Pts',(2.04548967476918,-1.82910487858453,
12.5063648335164));
#443675=CARTESIAN_POINT('Ctrl Pts',(2.04514969711389,-1.82954784476006,
12.5064455676329));
#443676=CARTESIAN_POINT('Ctrl Pts',(2.04479798279581,-1.82998155000805,
12.506574497099));
#443677=CARTESIAN_POINT('Ctrl Pts',(2.04444879599567,-1.8303867363887,12.5067492519495));
#443678=CARTESIAN_POINT('Ctrl Pts',(2.04374709156639,-1.83120097414877,
12.5071004286051));
#443679=CARTESIAN_POINT('Ctrl Pts',(2.04302918249784,-1.83192945471904,
12.5076537929612));
#443680=CARTESIAN_POINT('Ctrl Pts',(2.04235568846594,-1.83252414088437,
12.5083435010503));
#443681=CARTESIAN_POINT('Ctrl Pts',(2.04231328799173,-1.83256157993241,
12.5083869222963));
#443682=CARTESIAN_POINT('Ctrl Pts',(2.04227105103109,-1.83259848382877,
12.5084308732336));
#443683=CARTESIAN_POINT('Ctrl Pts',(2.04222898746737,-1.83263483897522,
12.5084753333615));
#443684=CARTESIAN_POINT('Ctrl Pts',(2.04189158216802,-1.83292645523374,
12.508831962269));
#443685=CARTESIAN_POINT('Ctrl Pts',(2.04155932720612,-1.83318966039935,
12.509227847131));
#443686=CARTESIAN_POINT('Ctrl Pts',(2.04124384094489,-1.83341882283399,
12.5096423454524));
#443687=CARTESIAN_POINT('Ctrl Pts',(2.04025524663057,-1.8341369164811,12.5109411997424));
#443688=CARTESIAN_POINT('Ctrl Pts',(2.03937618459408,-1.83457272839657,
12.5124831113042));
#443689=CARTESIAN_POINT('Ctrl Pts',(2.03861108086855,-1.83482079041435,
12.5140723025008));
#443690=CARTESIAN_POINT('Ctrl Pts',(2.03853938981148,-1.83484403409711,
12.5142212114565));
#443691=CARTESIAN_POINT('Ctrl Pts',(2.0384686901953,-1.83486565752973,12.5143705582413));
#443692=CARTESIAN_POINT('Ctrl Pts',(2.03839898193412,-1.83488575505061,
12.5145201959299));
#443693=CARTESIAN_POINT('Ctrl Pts',(2.03750347553461,-1.83514393762847,
12.5164425148273));
#443694=CARTESIAN_POINT('Ctrl Pts',(2.03674386616156,-1.83516945977046,
12.5184635205941));
#443695=CARTESIAN_POINT('Ctrl Pts',(2.03607689339251,-1.83504148279542,
12.5205025929158));
#443696=CARTESIAN_POINT('Ctrl Pts',(2.03569002275014,-1.83496725107737,
12.5216853356836));
#443697=CARTESIAN_POINT('Ctrl Pts',(2.03533492704499,-1.83484198418337,
12.5228750347131));
#443698=CARTESIAN_POINT('Ctrl Pts',(2.03500851782243,-1.8346836653027,12.5240609649613));
#443699=CARTESIAN_POINT('Ctrl Pts',(2.0342073638969,-1.83429508010361,12.5269717671326));
#443700=CARTESIAN_POINT('Ctrl Pts',(2.03356101520716,-1.83368708967651,
12.5299036066169));
#443701=CARTESIAN_POINT('Ctrl Pts',(2.03302101852352,-1.83293153973917,
12.5328133004019));
#443702=CARTESIAN_POINT('Ctrl Pts',(2.03276178867231,-1.83256883177489,
12.5342101228451));
#443703=CARTESIAN_POINT('Ctrl Pts',(2.03252781808887,-1.83217226567353,
12.5356023438238));
#443704=CARTESIAN_POINT('Ctrl Pts',(2.03231742029,-1.8317497385432,12.5369868989719));
#443705=CARTESIAN_POINT('Origin',(7.70874349513571,-13.2432058369479,-1.24003354080236));
#443706=CARTESIAN_POINT('Ctrl Pts',(2.10229442182352,-1.75093303820211,
12.5369868989719));
#443707=CARTESIAN_POINT('Ctrl Pts',(2.11684934377043,-1.75577427263197,
12.5369868989719));
#443708=CARTESIAN_POINT('Ctrl Pts',(2.12642480230394,-1.7437912055138,12.5369868989719));
#443709=CARTESIAN_POINT('Ctrl Pts',(2.10721457557878,-1.75256950195134,
12.5218025310016));
#443710=CARTESIAN_POINT('Ctrl Pts',(2.119024252351,-1.75300239713597,12.5216901060418));
#443711=CARTESIAN_POINT('Ctrl Pts',(2.12639562601662,-1.74382774416875,
12.5161920673678));
#443712=CARTESIAN_POINT('Ctrl Pts',(2.10900584014426,-1.75832514635071,
12.5042015548894));
#443713=CARTESIAN_POINT('Ctrl Pts',(2.11536588755699,-1.75736226425788,
12.4980677368513));
#443714=CARTESIAN_POINT('Ctrl Pts',(2.11970418659824,-1.75213063533829,
12.4907278922777));
#443715=CARTESIAN_POINT('Ctrl Pts',(2.09884684902727,-1.76687113220315,
12.506463626192));
#443716=CARTESIAN_POINT('Ctrl Pts',(2.10385214370824,-1.77108473677562,
12.4999376786891));
#443717=CARTESIAN_POINT('Ctrl Pts',(2.1037910113114,-1.77103327372235,12.4906970594712));
#443718=CARTESIAN_POINT('Origin',(2.10923799855709,-1.73005753240835,12.5369868989719));
#443719=CARTESIAN_POINT('Origin',(2.10923799855709,-1.73005753240835,14.));
#443720=CARTESIAN_POINT('Origin',(2.10923799855709,-1.73005753240835,13.7435492065112));
#443721=CARTESIAN_POINT('Ctrl Pts',(2.07882476581745,-1.74317610049156,
13.793642941384));
#443722=CARTESIAN_POINT('Ctrl Pts',(2.08908231900796,-1.74659499235143,
13.8071662555867));
#443723=CARTESIAN_POINT('Ctrl Pts',(2.09678409482011,-1.73140611375641,
13.8103758687955));
#443724=CARTESIAN_POINT('Ctrl Pts',(2.09460626292319,-1.74839204281527,
13.7804579775006));
#443725=CARTESIAN_POINT('Ctrl Pts',(2.10726636298059,-1.75260102585943,
13.7901904343352));
#443726=CARTESIAN_POINT('Ctrl Pts',(2.11657182980508,-1.73988630166491,
13.7927914348262));
#443727=CARTESIAN_POINT('Ctrl Pts',(2.10389742420584,-1.75146286432314,
13.7597120340895));
#443728=CARTESIAN_POINT('Ctrl Pts',(2.11855053313096,-1.75632840527981,
13.7635825532445));
#443729=CARTESIAN_POINT('Ctrl Pts',(2.12825070374247,-1.74486356309809,
13.7651073818884));
#443730=CARTESIAN_POINT('Ctrl Pts',(2.10207800208354,-1.75086152715731,
13.7381884353898));
#443731=CARTESIAN_POINT('Ctrl Pts',(2.11638784444474,-1.75561403409828,
13.7368803041982));
#443732=CARTESIAN_POINT('Ctrl Pts',(2.12596382695618,-1.7438884127476,13.7363986145813));
#443733=CARTESIAN_POINT('Origin',(2.08955801581772,-1.7235531055736,13.7902182540695));
#443734=CARTESIAN_POINT('Ctrl Pts',(2.04869023441034,-1.73321637083664,
13.8235227101244));
#443735=CARTESIAN_POINT('Ctrl Pts',(2.05960513502331,-1.7368285215711,13.8358800583119));
#443736=CARTESIAN_POINT('Ctrl Pts',(2.06755050992179,-1.72228558284541,
13.8390832900376));
#443737=CARTESIAN_POINT('Ctrl Pts',(2.06001528618862,-1.73695941124701,
13.8124254819052));
#443738=CARTESIAN_POINT('Ctrl Pts',(2.07095138347126,-1.74057857646292,
13.8247886449157));
#443739=CARTESIAN_POINT('Ctrl Pts',(2.07889184014536,-1.72600909023626,
13.8279860620657));
#443740=CARTESIAN_POINT('Ctrl Pts',(2.07133526244714,-1.74070077414845,
13.8013225099955));
#443741=CARTESIAN_POINT('Ctrl Pts',(2.08228739568786,-1.74432524808412,
13.8136962257787));
#443742=CARTESIAN_POINT('Ctrl Pts',(2.09022783533978,-1.72973113135799,
13.8168830918626));
#443743=CARTESIAN_POINT('Ctrl Pts',(2.08265036066656,-1.74444052481026,
13.7902140179785));
#443744=CARTESIAN_POINT('Ctrl Pts',(2.09361370644511,-1.74806871318529,
13.802602731458));
#443745=CARTESIAN_POINT('Ctrl Pts',(2.10155870455724,-1.73345176557235,
13.8057746032558));
#443746=CARTESIAN_POINT('Origin',(2.05559787773024,-1.71232894768619,13.8235269408515));
#443747=CARTESIAN_POINT('Ctrl Pts',(2.00713550187736,-1.78117863747125,
13.8235269408515));
#443748=CARTESIAN_POINT('Ctrl Pts',(2.01239863335932,-1.79174821957248,
13.8362179249168));
#443749=CARTESIAN_POINT('Ctrl Pts',(1.99854352737823,-1.80173316034896,
13.8391868794938));
#443750=CARTESIAN_POINT('Ctrl Pts',(2.00231996566185,-1.77150792991513,
13.8400110824519));
#443751=CARTESIAN_POINT('Ctrl Pts',(2.0034773691972,-1.78150704387178,13.8494522556837));
#443752=CARTESIAN_POINT('Ctrl Pts',(1.99071909162703,-1.78576782324635,
13.85569149686));
#443753=CARTESIAN_POINT('Ctrl Pts',(2.00166443723085,-1.75523009195916,
13.8586819406588));
#443754=CARTESIAN_POINT('Ctrl Pts',(1.99882379491583,-1.75852960629814,
13.868010383617));
#443755=CARTESIAN_POINT('Ctrl Pts',(1.98977678287228,-1.758740413974,13.8744918421245));
#443756=CARTESIAN_POINT('Ctrl Pts',(2.02211523627899,-1.73154810901348,
13.8587686893867));
#443757=CARTESIAN_POINT('Ctrl Pts',(2.02493055423129,-1.72827792358337,
13.8680909899357));
#443758=CARTESIAN_POINT('Ctrl Pts',(2.02382330493006,-1.71931854857778,
13.8745789365162));
#443759=CARTESIAN_POINT('Ctrl Pts',(2.03841968402915,-1.72982185424597,
13.8400379222776));
#443760=CARTESIAN_POINT('Ctrl Pts',(2.04847897340077,-1.72953737007122,
13.8494748685453));
#443761=CARTESIAN_POINT('Ctrl Pts',(2.05088069251635,-1.71630888374227,
13.8557104837033));
#443762=CARTESIAN_POINT('Ctrl Pts',(2.04869397153352,-1.73321760678476,
13.8235269408542));
#443763=CARTESIAN_POINT('Ctrl Pts',(2.0599049922347,-1.73692295880962,13.8362179249195));
#443764=CARTESIAN_POINT('Ctrl Pts',(2.06781651354415,-1.72178787259823,
13.8391868794965));
#443765=CARTESIAN_POINT('Origin',(1.98744198749732,-1.79098503800168,13.8235269408515));
#443766=CARTESIAN_POINT('Ctrl Pts',(2.02307668737534,-1.81319221692728,
13.7902140241682));
#443767=CARTESIAN_POINT('Ctrl Pts',(2.02822818492491,-1.82352762540441,
13.8026027327198));
#443768=CARTESIAN_POINT('Ctrl Pts',(2.01489071319087,-1.83347195947046,
13.8057746032556));
#443769=CARTESIAN_POINT('Ctrl Pts',(2.01776469560807,-1.80252451209978,
13.8013225161808));
#443770=CARTESIAN_POINT('Ctrl Pts',(2.02291092082792,-1.8128493507848,13.8136962270464));
#443771=CARTESIAN_POINT('Ctrl Pts',(2.00959539884771,-1.82278592361994,
13.8168830918628));
#443772=CARTESIAN_POINT('Ctrl Pts',(2.01245041379337,-1.79185220832873,
13.8124254880875));
#443773=CARTESIAN_POINT('Ctrl Pts',(2.01758910218842,-1.80216192979049,
13.8247886461868));
#443774=CARTESIAN_POINT('Ctrl Pts',(2.00429796241527,-1.81209501419208,
13.8279860620656));
#443775=CARTESIAN_POINT('Ctrl Pts',(2.00713374922116,-1.78117511943091,
13.8235227163065));
#443776=CARTESIAN_POINT('Ctrl Pts',(2.0122624779483,-1.79146485824588,13.8358800595847));
#443777=CARTESIAN_POINT('Ctrl Pts',(1.99899831538418,-1.80139903270935,
13.8390832900376));
#443778=CARTESIAN_POINT('Origin',(2.00338493120099,-1.82300214663539,13.7902182540695));
#443779=CARTESIAN_POINT('Ctrl Pts',(2.03219710676631,-1.83150818311793,
13.7382347919292));
#443780=CARTESIAN_POINT('Ctrl Pts',(2.03894502593405,-1.84500571828694,
13.7369371795943));
#443781=CARTESIAN_POINT('Ctrl Pts',(2.02868754764281,-1.85615596115984,
13.7364597369712));
#443782=CARTESIAN_POINT('Ctrl Pts',(2.03304026082543,-1.83320143006296,
13.7595490285574));
#443783=CARTESIAN_POINT('Ctrl Pts',(2.0399482802584,-1.84702145444543,13.7633824266925));
#443784=CARTESIAN_POINT('Ctrl Pts',(2.02996273758586,-1.85825455721548,
13.7648920890506));
#443785=CARTESIAN_POINT('Ctrl Pts',(2.02874022132283,-1.82456596340339,
13.7803806590111));
#443786=CARTESIAN_POINT('Ctrl Pts',(2.03472023968487,-1.83651737613972,
13.7901039518745));
#443787=CARTESIAN_POINT('Ctrl Pts',(2.02346485292937,-1.84755375735866,
13.7926933640892));
#443788=CARTESIAN_POINT('Ctrl Pts',(2.02126579270878,-1.80955559470482,
13.7936647693663));
#443789=CARTESIAN_POINT('Ctrl Pts',(2.02611353045677,-1.81922372641012,
13.8072068914932));
#443790=CARTESIAN_POINT('Ctrl Pts',(2.01215425950561,-1.82901060662593,
13.8104111085397));
#443791=CARTESIAN_POINT('Origin',(2.01262390590996,-1.84155613907362,13.7435492065112));
#443792=CARTESIAN_POINT('Origin',(2.01262390590996,-1.84155613907362,14.));
#443793=CARTESIAN_POINT('Origin',(2.01262390590996,-1.84155613907362,12.5369868989719));
#443794=CARTESIAN_POINT('Ctrl Pts',(2.04758518902183,-1.82603271176115,
12.506462012331));
#443795=CARTESIAN_POINT('Ctrl Pts',(2.05246516055766,-1.83038466141612,
12.4999388158272));
#443796=CARTESIAN_POINT('Ctrl Pts',(2.0524074240947,-1.83033317214447,12.4907030323752));
#443797=CARTESIAN_POINT('Ctrl Pts',(2.04057046462635,-1.83730312545407,
12.5042014951932));
#443798=CARTESIAN_POINT('Ctrl Pts',(2.04052348863317,-1.84373265812542,
12.4980716682127));
#443799=CARTESIAN_POINT('Ctrl Pts',(2.03596689881399,-1.84876883270994,
12.4907355092744));
#443800=CARTESIAN_POINT('Ctrl Pts',(2.03461895904624,-1.83635166206782,
12.5218047446509));
#443801=CARTESIAN_POINT('Ctrl Pts',(2.03672599900411,-1.8479740221359,12.5216906929434));
#443802=CARTESIAN_POINT('Ctrl Pts',(2.02870059055002,-1.85657422989357,
12.5161988840775));
#443803=CARTESIAN_POINT('Ctrl Pts',(2.03230026645711,-1.83171536493648,
12.5369868989719));
#443804=CARTESIAN_POINT('Ctrl Pts',(2.03915744765511,-1.8454261124558,12.5369868989719));
#443805=CARTESIAN_POINT('Ctrl Pts',(2.02866975789569,-1.85660707373071,
12.5369868989719));
#443806=CARTESIAN_POINT('Origin',(3.89351796801565E-31,-8.5256151254664E-31,
12.5));
#443807=CARTESIAN_POINT('Origin',(2.14563951868151,-1.61165173575206,12.5));
#443808=CARTESIAN_POINT('',(2.14563951868151,-1.61165173575206,12.5893111709658));
#443809=CARTESIAN_POINT('',(2.14563951868151,-1.61165173575206,13.8235269408515));
#443810=CARTESIAN_POINT('',(2.14563951868151,-1.61165173575206,12.5));
#443811=CARTESIAN_POINT('',(2.16413910514119,-1.64226281217911,13.7902182540695));
#443812=CARTESIAN_POINT('',(2.14563951868151,-1.61165173575206,13.8235269408515));
#443813=CARTESIAN_POINT('',(2.17485966055454,-1.66000200552886,13.7435492065112));
#443814=CARTESIAN_POINT('Origin',(2.13958945374545,-1.60164012539495,13.7445212918695));
#443815=CARTESIAN_POINT('',(2.17485966055454,-1.66000200552886,12.5369868989719));
#443816=CARTESIAN_POINT('',(2.17485966055454,-1.66000200552886,12.5));
#443817=CARTESIAN_POINT('Ctrl Pts',(2.17485966055454,-1.66000200552886,
12.5369868989719));
#443818=CARTESIAN_POINT('Ctrl Pts',(2.16512671706162,-1.64389700351861,
12.5544431401645));
#443819=CARTESIAN_POINT('Ctrl Pts',(2.15538681230883,-1.62778048278287,
12.5718848856037));
#443820=CARTESIAN_POINT('Ctrl Pts',(2.14563951868151,-1.61165173575206,
12.5893111709658));
#443821=CARTESIAN_POINT('Origin',(2.45042401499281,-1.62519182013837,12.5));
#443822=CARTESIAN_POINT('',(2.23805711869617,-1.57376031685917,13.7435492065112));
#443823=CARTESIAN_POINT('',(2.21791244830468,-1.56888163426144,13.7902182540695));
#443824=CARTESIAN_POINT('Origin',(2.16497573621185,-1.55606129959972,13.7418732680434));
#443825=CARTESIAN_POINT('',(2.18315043670736,-1.56046289035814,13.8235269408515));
#443826=CARTESIAN_POINT('',(2.21791244830468,-1.56888163426144,13.7902182540695));
#443827=CARTESIAN_POINT('',(2.18315043670736,-1.56046289035814,12.5893111709658));
#443828=CARTESIAN_POINT('',(2.18315043670736,-1.56046289035814,12.5));
#443829=CARTESIAN_POINT('',(2.23805711869617,-1.57376031685917,12.5369868989719));
#443830=CARTESIAN_POINT('Ctrl Pts',(2.18315043670736,-1.56046289035814,
12.5893111709658));
#443831=CARTESIAN_POINT('Ctrl Pts',(2.20146628040765,-1.56489866350245,
12.5718848856037));
#443832=CARTESIAN_POINT('Ctrl Pts',(2.21976823989801,-1.56933107413687,
12.5544431401645));
#443833=CARTESIAN_POINT('Ctrl Pts',(2.23805711869617,-1.57376031685917,
12.5369868989719));
#443834=CARTESIAN_POINT('',(2.23805711869617,-1.57376031685917,12.5));
#443835=CARTESIAN_POINT('Origin',(2.17505932048484,-1.59387208764382,12.5));
#443836=CARTESIAN_POINT('',(2.14668558831924,-1.5744679258435,13.8587068136939));
#443837=CARTESIAN_POINT('Ctrl Pts',(2.18315043670878,-1.56046289035168,
13.8235269408542));
#443838=CARTESIAN_POINT('Ctrl Pts',(2.18144737109385,-1.5600504380049,13.8262006681044));
#443839=CARTESIAN_POINT('Ctrl Pts',(2.17966363786502,-1.55979721122832,
13.8288634856214));
#443840=CARTESIAN_POINT('Ctrl Pts',(2.17780652992437,-1.5596920467058,13.8314912288862));
#443841=CARTESIAN_POINT('Ctrl Pts',(2.17589204318937,-1.5595836329303,13.834200161153));
#443842=CARTESIAN_POINT('Ctrl Pts',(2.17389747917255,-1.55963195555763,
13.8368750301949));
#443843=CARTESIAN_POINT('Ctrl Pts',(2.17180888022849,-1.55986429920104,
13.8394886372968));
#443844=CARTESIAN_POINT('Ctrl Pts',(2.1716475726658,-1.55988224366421,13.8396904925131));
#443845=CARTESIAN_POINT('Ctrl Pts',(2.17148570281865,-1.55990130789,13.8398919674349));
#443846=CARTESIAN_POINT('Ctrl Pts',(2.17132326454954,-1.55992151588814,
13.8400930404591));
#443847=CARTESIAN_POINT('Ctrl Pts',(2.16879236703379,-1.56023637009442,
13.8432258934518));
#443848=CARTESIAN_POINT('Ctrl Pts',(2.16613625619827,-1.56082615998279,
13.8462331177034));
#443849=CARTESIAN_POINT('Ctrl Pts',(2.16346247112471,-1.56176582236049,
13.8489036603661));
#443850=CARTESIAN_POINT('Ctrl Pts',(2.16258757753225,-1.56207329082587,
13.8497774930041));
#443851=CARTESIAN_POINT('Ctrl Pts',(2.16171103427618,-1.56241827908187,
13.85061494757));
#443852=CARTESIAN_POINT('Ctrl Pts',(2.16083730473066,-1.56280357170684,
13.8514076489583));
#443853=CARTESIAN_POINT('Ctrl Pts',(2.15898924073119,-1.56361852117618,
13.8530843267192));
#443854=CARTESIAN_POINT('Ctrl Pts',(2.15697342976868,-1.56469654170965,
13.8546805203176));
#443855=CARTESIAN_POINT('Ctrl Pts',(2.15497121424547,-1.56609538617429,
13.8559412814274));
#443856=CARTESIAN_POINT('Ctrl Pts',(2.15470325287509,-1.56628259692925,
13.8561100121513));
#443857=CARTESIAN_POINT('Ctrl Pts',(2.1544355423056,-1.5664754775244,13.8562727473908));
#443858=CARTESIAN_POINT('Ctrl Pts',(2.15416851492518,-1.56667409058494,
13.8564289040185));
#443859=CARTESIAN_POINT('Ctrl Pts',(2.15295754880127,-1.56757479854867,
13.8571370725437));
#443860=CARTESIAN_POINT('Ctrl Pts',(2.1517407064163,-1.56861105959196,13.8577210840553));
#443861=CARTESIAN_POINT('Ctrl Pts',(2.15058431458969,-1.56976493785743,
13.8581177131616));
#443862=CARTESIAN_POINT('Ctrl Pts',(2.15025863484952,-1.57008990969228,
13.8582294175695));
#443863=CARTESIAN_POINT('Ctrl Pts',(2.14993765153355,-1.57042406281398,
13.8583265086086));
#443864=CARTESIAN_POINT('Ctrl Pts',(2.14962258137367,-1.57076664577275,
13.8584082369006));
#443865=CARTESIAN_POINT('Ctrl Pts',(2.14916991004332,-1.57125884561726,
13.8585256585398));
#443866=CARTESIAN_POINT('Ctrl Pts',(2.1487240548657,-1.57177478440373,13.8586122832068));
#443867=CARTESIAN_POINT('Ctrl Pts',(2.14829719536374,-1.57230157587311,
13.8586682984299));
#443868=CARTESIAN_POINT('Ctrl Pts',(2.1479557500754,-1.57272295682945,13.8587131050557));
#443869=CARTESIAN_POINT('Ctrl Pts',(2.14762250556025,-1.57315578831616,
13.8587357943552));
#443870=CARTESIAN_POINT('Ctrl Pts',(2.14729782350775,-1.57360043072413,
13.8587355499465));
#443871=CARTESIAN_POINT('Ctrl Pts',(2.14708797375645,-1.57388781371314,
13.8587353919793));
#443872=CARTESIAN_POINT('Ctrl Pts',(2.14688393889627,-1.57417700000451,
13.8587257282814));
#443873=CARTESIAN_POINT('Ctrl Pts',(2.14668558831924,-1.5744679258435,13.8587068136939));
#443874=CARTESIAN_POINT('Ctrl Pts',(2.14668558831924,-1.5744679258435,13.8587068136939));
#443875=CARTESIAN_POINT('Ctrl Pts',(2.14603322408453,-1.57542476506803,
13.8586446046466));
#443876=CARTESIAN_POINT('Ctrl Pts',(2.14544227142407,-1.5764003986978,13.858482427929));
#443877=CARTESIAN_POINT('Ctrl Pts',(2.1449087568648,-1.57739277796024,13.8582284286032));
#443878=CARTESIAN_POINT('Ctrl Pts',(2.14436143298796,-1.57841084364519,
13.8579678548414));
#443879=CARTESIAN_POINT('Ctrl Pts',(2.14387457120063,-1.57944974518245,
13.857615680862));
#443880=CARTESIAN_POINT('Ctrl Pts',(2.14345859166921,-1.58046441288024,
13.8571944833187));
#443881=CARTESIAN_POINT('Ctrl Pts',(2.14242047220565,-1.58299661989181,
13.8561433417727));
#443882=CARTESIAN_POINT('Ctrl Pts',(2.14177081261079,-1.58549452749989,
13.8546163505474));
#443883=CARTESIAN_POINT('Ctrl Pts',(2.14139296760601,-1.58778739688165,
13.8528973491086));
#443884=CARTESIAN_POINT('Ctrl Pts',(2.14132394089822,-1.58820627028954,
13.8525833129072));
#443885=CARTESIAN_POINT('Ctrl Pts',(2.14126385141198,-1.58861834480671,
13.8522628768811));
#443886=CARTESIAN_POINT('Ctrl Pts',(2.14121182884849,-1.58902266102707,
13.851937733538));
#443887=CARTESIAN_POINT('Ctrl Pts',(2.14089413427106,-1.5914917640885,13.8499521282529));
#443888=CARTESIAN_POINT('Ctrl Pts',(2.1408497575725,-1.59391743397896,13.847639871647));
#443889=CARTESIAN_POINT('Ctrl Pts',(2.14100070377333,-1.59617071689979,
13.8452109780794));
#443890=CARTESIAN_POINT('Ctrl Pts',(2.14106861759351,-1.5971845155265,13.8441181685877));
#443891=CARTESIAN_POINT('Ctrl Pts',(2.1411754149802,-1.59816371078859,13.8430021611332));
#443892=CARTESIAN_POINT('Ctrl Pts',(2.14131153713677,-1.59909877597496,
13.8418824960098));
#443893=CARTESIAN_POINT('Ctrl Pts',(2.14163231247473,-1.60130228096441,
13.8392439765549));
#443894=CARTESIAN_POINT('Ctrl Pts',(2.14212752608784,-1.60336660401069,
13.8364981347964));
#443895=CARTESIAN_POINT('Ctrl Pts',(2.14276521119921,-1.60530518718705,
13.8336931113419));
#443896=CARTESIAN_POINT('Ctrl Pts',(2.14338627600093,-1.60719324408941,
13.8309611966327));
#443897=CARTESIAN_POINT('Ctrl Pts',(2.14414364098942,-1.60896374577289,
13.8281701127185));
#443898=CARTESIAN_POINT('Ctrl Pts',(2.1450380805368,-1.6106040899672,13.825358068512));
#443899=CARTESIAN_POINT('Ctrl Pts',(2.14523199599598,-1.61095971835882,
13.8247484142932));
#443900=CARTESIAN_POINT('Ctrl Pts',(2.14543243433548,-1.61130907540357,
13.8241378483365));
#443901=CARTESIAN_POINT('Ctrl Pts',(2.14563951868151,-1.61165173575206,
13.8235269408515));
#443902=CARTESIAN_POINT('',(2.14740511570521,-1.57345547475895,12.5969504640361));
#443903=CARTESIAN_POINT('Origin',(2.17508589184132,-1.59389180174597,12.584524458991));
#443904=CARTESIAN_POINT('Origin',(2.17508589184132,-1.59389180174597,12.584524458991));
#443905=CARTESIAN_POINT('Ctrl Pts',(2.18315043670736,-1.56046289035814,
12.5893111709658));
#443906=CARTESIAN_POINT('Ctrl Pts',(2.17213491717369,-1.55779512650747,
12.5770542771492));
#443907=CARTESIAN_POINT('Ctrl Pts',(2.16538527500076,-1.57270304404791,
12.5737548217797));
#443908=CARTESIAN_POINT('Ctrl Pts',(2.20723768100929,-1.56629639457139,
12.5663937883685));
#443909=CARTESIAN_POINT('Ctrl Pts',(2.19620810965064,-1.56362522761743,
12.5540940315304));
#443910=CARTESIAN_POINT('Ctrl Pts',(2.18944047703163,-1.57858066622843,
12.5508374392248));
#443911=CARTESIAN_POINT('Ctrl Pts',(2.23130062157697,-1.57212401285039,
12.5434499600945));
#443912=CARTESIAN_POINT('Ctrl Pts',(2.22023518915413,-1.5694441609814,12.5311293540533));
#443913=CARTESIAN_POINT('Ctrl Pts',(2.21347245666714,-1.58445139969722,
12.5278936106989));
#443914=CARTESIAN_POINT('Ctrl Pts',(2.25534116215525,-1.57794620624846,
12.5204817579905));
#443915=CARTESIAN_POINT('Ctrl Pts',(2.24422096340405,-1.57525309094419,
12.5081597038247));
#443916=CARTESIAN_POINT('Ctrl Pts',(2.23748302213097,-1.59031576641355,
12.5049254088044));
#443917=CARTESIAN_POINT('Ctrl Pts',(2.23805711869617,-1.57376031685917,
12.5369868989719));
#443918=CARTESIAN_POINT('Ctrl Pts',(2.23896245181433,-1.57397957268211,
12.5342545179733));
#443919=CARTESIAN_POINT('Ctrl Pts',(2.23979709794904,-1.57431006162775,
12.5314872231885));
#443920=CARTESIAN_POINT('Ctrl Pts',(2.24049346011131,-1.57478514146218,
12.5287124745062));
#443921=CARTESIAN_POINT('Ctrl Pts',(2.24112147407358,-1.57521359203772,
12.5262100684184));
#443922=CARTESIAN_POINT('Ctrl Pts',(2.24163582914458,-1.57576002336795,
12.5237004536639));
#443923=CARTESIAN_POINT('Ctrl Pts',(2.24199708719794,-1.57647925433941,
12.5212220730815));
#443924=CARTESIAN_POINT('Ctrl Pts',(2.24227366148909,-1.57702988786651,
12.5193246583486));
#443925=CARTESIAN_POINT('Ctrl Pts',(2.24246324052858,-1.57768866887025,
12.517417831369));
#443926=CARTESIAN_POINT('Ctrl Pts',(2.2424795272376,-1.57850039508432,12.5155812248348));
#443927=CARTESIAN_POINT('Ctrl Pts',(2.24248646546319,-1.57884619481456,
12.5147988205793));
#443928=CARTESIAN_POINT('Ctrl Pts',(2.24246223850744,-1.57922009660828,
12.5140295443047));
#443929=CARTESIAN_POINT('Ctrl Pts',(2.24240195537312,-1.57962672751777,
12.5132817086137));
#443930=CARTESIAN_POINT('Ctrl Pts',(2.24231072500425,-1.58024210839149,
12.5121499604604));
#443931=CARTESIAN_POINT('Ctrl Pts',(2.2421278717249,-1.58094468777853,12.5110494206568));
#443932=CARTESIAN_POINT('Ctrl Pts',(2.24181625360193,-1.58173718147512,
12.5100666561695));
#443933=CARTESIAN_POINT('Ctrl Pts',(2.24163732319332,-1.58219222953076,
12.5095023550641));
#443934=CARTESIAN_POINT('Ctrl Pts',(2.24141326378282,-1.58268194140116,
12.5089719619137));
#443935=CARTESIAN_POINT('Ctrl Pts',(2.24114246717993,-1.58319448065509,
12.5085043804652));
#443936=CARTESIAN_POINT('Ctrl Pts',(2.24074619162535,-1.58394451509028,
12.5078201359221));
#443937=CARTESIAN_POINT('Ctrl Pts',(2.24023726943766,-1.58476462253414,
12.5072563000949));
#443938=CARTESIAN_POINT('Ctrl Pts',(2.2396430045484,-1.58559474784262,12.5068768744332));
#443939=CARTESIAN_POINT('Ctrl Pts',(2.23921449865391,-1.58619332533605,
12.5066032824114));
#443940=CARTESIAN_POINT('Ctrl Pts',(2.23873414028217,-1.58680766258495,
12.5064197834844));
#443941=CARTESIAN_POINT('Ctrl Pts',(2.23823079016697,-1.58740504559342,
12.5063282718343));
#443942=CARTESIAN_POINT('Ctrl Pts',(2.23749605483204,-1.58827703984068,
12.5061946931565));
#443943=CARTESIAN_POINT('Ctrl Pts',(2.23669743927224,-1.58913223202237,
12.5062515701262));
#443944=CARTESIAN_POINT('Ctrl Pts',(2.23589580952595,-1.58992810221818,
12.5064436508398));
#443945=CARTESIAN_POINT('',(2.16538527500076,-1.57270304404791,12.5737548217797));
#443946=CARTESIAN_POINT('Origin',(2.17797212232495,-1.58184477662098,12.5893111709658));
#443947=CARTESIAN_POINT('Ctrl Pts',(2.23589580952594,-1.58992810221818,
12.5064436508398));
#443948=CARTESIAN_POINT('Ctrl Pts',(2.22545830449568,-1.58737881280847,
12.5164271754438));
#443949=CARTESIAN_POINT('Ctrl Pts',(2.21501671161468,-1.58482830989171,
12.5264061185523));
#443950=CARTESIAN_POINT('Ctrl Pts',(2.2045708866877,-1.58227655164866,12.536380305637));
#443951=CARTESIAN_POINT('Ctrl Pts',(2.19151572417055,-1.57908737139719,
12.5488460165097));
#443952=CARTESIAN_POINT('Ctrl Pts',(2.17845394737643,-1.57589622936917,
12.5613043021964));
#443953=CARTESIAN_POINT('Ctrl Pts',(2.16538527500076,-1.57270304404791,
12.5737548217797));
#443954=CARTESIAN_POINT('Ctrl Pts',(2.14563951868151,-1.61165173575206,
12.5893111709658));
#443955=CARTESIAN_POINT('Ctrl Pts',(2.13977729878549,-1.60195158047235,
12.5770542771492));
#443956=CARTESIAN_POINT('Ctrl Pts',(2.15195938587369,-1.59102453013704,
12.5737548217797));
#443957=CARTESIAN_POINT('Ctrl Pts',(2.14017011850542,-1.60260157524359,
12.5928319619712));
#443958=CARTESIAN_POINT('Ctrl Pts',(2.13901847966281,-1.59439748209764,
12.5821634970843));
#443959=CARTESIAN_POINT('Ctrl Pts',(2.14995893754366,-1.58773265774458,
12.5773203894503));
#443960=CARTESIAN_POINT('Ctrl Pts',(2.13827537602497,-1.5859584370097,12.5969440695591));
#443961=CARTESIAN_POINT('Ctrl Pts',(2.14063662090009,-1.58270527467258,
12.5878292599214));
#443962=CARTESIAN_POINT('Ctrl Pts',(2.14928564550728,-1.58180047223405,
12.5813877129824));
#443963=CARTESIAN_POINT('Ctrl Pts',(2.15631715034656,-1.56124670649826,
12.596957478804));
#443964=CARTESIAN_POINT('Ctrl Pts',(2.1539734205758,-1.56447587417903,12.5878468778671));
#443965=CARTESIAN_POINT('Ctrl Pts',(2.15574786437539,-1.57295931871175,
12.5814011370086));
#443966=CARTESIAN_POINT('Ctrl Pts',(2.17285813004666,-1.55797027586401,
12.5928371701607));
#443967=CARTESIAN_POINT('Ctrl Pts',(2.16469508204371,-1.55934857663135,
12.5821692192952));
#443968=CARTESIAN_POINT('Ctrl Pts',(2.16163178890298,-1.57178401217266,
12.5773318885715));
#443969=CARTESIAN_POINT('Ctrl Pts',(2.18315043670737,-1.56046289035808,
12.5893111709658));
#443970=CARTESIAN_POINT('Ctrl Pts',(2.1721349171737,-1.55779512650742,12.5770542771492));
#443971=CARTESIAN_POINT('Ctrl Pts',(2.16538527500077,-1.57270304404785,
12.5737548217797));
#443972=CARTESIAN_POINT('',(2.15195938587369,-1.59102453013704,12.5737548217797));
#443973=CARTESIAN_POINT('Origin',(2.16446819183564,-1.60027276096279,12.5893111709658));
#443974=CARTESIAN_POINT('Ctrl Pts',(2.16538527500077,-1.57270304404785,
12.5737548217797));
#443975=CARTESIAN_POINT('Ctrl Pts',(2.16441948596369,-1.57243551616732,
12.5746934679442));
#443976=CARTESIAN_POINT('Ctrl Pts',(2.16330187468488,-1.57231601525643,
12.5756680099006));
#443977=CARTESIAN_POINT('Ctrl Pts',(2.16215994763177,-1.572354825994,12.5765688348656));
#443978=CARTESIAN_POINT('Ctrl Pts',(2.161857635086,-1.57236510070712,12.5768073183026));
#443979=CARTESIAN_POINT('Ctrl Pts',(2.16155367238901,-1.57238621963317,
12.5770407398754));
#443980=CARTESIAN_POINT('Ctrl Pts',(2.16125040166498,-1.57241781094287,
12.5772674179684));
#443981=CARTESIAN_POINT('Ctrl Pts',(2.16000586062142,-1.57254745313522,
12.5781976435658));
#443982=CARTESIAN_POINT('Ctrl Pts',(2.15870345460724,-1.57287203911304,
12.5790594849312));
#443983=CARTESIAN_POINT('Ctrl Pts',(2.15744280158855,-1.57341650829504,
12.5797571720116));
#443984=CARTESIAN_POINT('Ctrl Pts',(2.15662144081783,-1.57377124954448,
12.580211740231));
#443985=CARTESIAN_POINT('Ctrl Pts',(2.1557879208466,-1.57425268639174,12.5806009430798));
#443986=CARTESIAN_POINT('Ctrl Pts',(2.15500977901797,-1.57484226926025,
12.5808812374708));
#443987=CARTESIAN_POINT('Ctrl Pts',(2.1543410970413,-1.57534891653639,12.5811221033394));
#443988=CARTESIAN_POINT('Ctrl Pts',(2.15369968833467,-1.57594588774487,
12.581287365893));
#443989=CARTESIAN_POINT('Ctrl Pts',(2.15312743566234,-1.5766055923473,12.581359338449));
#443990=CARTESIAN_POINT('Ctrl Pts',(2.15304790435745,-1.57669727766465,
12.5813693411482));
#443991=CARTESIAN_POINT('Ctrl Pts',(2.15296965309714,-1.57679015277659,
12.5813775999465));
#443992=CARTESIAN_POINT('Ctrl Pts',(2.15289273683827,-1.57688412218016,
12.5813841266931));
#443993=CARTESIAN_POINT('Ctrl Pts',(2.15276223910227,-1.57704355263867,
12.5813952001081));
#443994=CARTESIAN_POINT('Ctrl Pts',(2.15263518134807,-1.57720758648643,
12.5814007534795));
#443995=CARTESIAN_POINT('Ctrl Pts',(2.15251177482256,-1.57737627304579,
12.5814005856065));
#443996=CARTESIAN_POINT('Ctrl Pts',(2.15194686799762,-1.57814845416237,
12.5813998171494));
#443997=CARTESIAN_POINT('Ctrl Pts',(2.15149722919371,-1.57896457948774,
12.58127954464));
#443998=CARTESIAN_POINT('Ctrl Pts',(2.1511394948303,-1.57980573716164,12.5810700125799));
#443999=CARTESIAN_POINT('Ctrl Pts',(2.15070739245063,-1.58082175985825,
12.5808169217085));
#444000=CARTESIAN_POINT('Ctrl Pts',(2.15042473963729,-1.58188094621889,
12.5804173076348));
#444001=CARTESIAN_POINT('Ctrl Pts',(2.15029114576598,-1.58288375629323,
12.5799304713245));
#444002=CARTESIAN_POINT('Ctrl Pts',(2.15012558087302,-1.58412655389309,
12.5793271277669));
#444003=CARTESIAN_POINT('Ctrl Pts',(2.15014676723826,-1.58535560391092,
12.5785808224116));
#444004=CARTESIAN_POINT('Ctrl Pts',(2.15032209966813,-1.58651964617907,
12.5777485681082));
#444005=CARTESIAN_POINT('Ctrl Pts',(2.15058336419775,-1.58825419668896,
12.576508418016));
#444006=CARTESIAN_POINT('Ctrl Pts',(2.15117790321657,-1.58983082057114,
12.5750928681475));
#444007=CARTESIAN_POINT('Ctrl Pts',(2.15195938587369,-1.59102453013704,
12.5737548217797));
#444008=CARTESIAN_POINT('Ctrl Pts',(2.15195938587369,-1.59102453013704,
12.5737548217797));
#444009=CARTESIAN_POINT('Ctrl Pts',(2.13977729878549,-1.60195158047235,
12.5770542771492));
#444010=CARTESIAN_POINT('Ctrl Pts',(2.14563951868151,-1.61165173575206,
12.5893111709658));
#444011=CARTESIAN_POINT('Ctrl Pts',(2.16480857860599,-1.61218849007602,
12.5508408821982));
#444012=CARTESIAN_POINT('Ctrl Pts',(2.15258660177983,-1.62314700307234,
12.55409748406));
#444013=CARTESIAN_POINT('Ctrl Pts',(2.15845630036708,-1.63285953326585,
12.5663972313419));
#444014=CARTESIAN_POINT('Ctrl Pts',(2.17764421105535,-1.63333238762155,
12.52790050457));
#444015=CARTESIAN_POINT('Ctrl Pts',(2.16537137191014,-1.64430183139314,
12.5311362602938));
#444016=CARTESIAN_POINT('Ctrl Pts',(2.171260152026,-1.65404593559684,12.5434568539655));
#444017=CARTESIAN_POINT('Ctrl Pts',(2.19046732519249,-1.65445778906585,
12.5049357605811));
#444018=CARTESIAN_POINT('Ctrl Pts',(2.17813416660201,-1.66542029718085,
12.5081700652078));
#444019=CARTESIAN_POINT('Ctrl Pts',(2.18405208634059,-1.67521261842012,
12.5204921097672));
#444020=CARTESIAN_POINT('Ctrl Pts',(2.18962530789643,-1.65307061322152,
12.5064436508395));
#444021=CARTESIAN_POINT('Ctrl Pts',(2.18906641016893,-1.65415527036587,
12.5062361689309));
#444022=CARTESIAN_POINT('Ctrl Pts',(2.18843895007854,-1.65525939239509,
12.5061871075061));
#444023=CARTESIAN_POINT('Ctrl Pts',(2.18777250480326,-1.65629228509822,
12.5063648335164));
#444024=CARTESIAN_POINT('Ctrl Pts',(2.18746976425118,-1.65676148867544,
12.5064455676329));
#444025=CARTESIAN_POINT('Ctrl Pts',(2.18715457123752,-1.65722241878708,
12.506574497099));
#444026=CARTESIAN_POINT('Ctrl Pts',(2.18683957277924,-1.65765471890938,
12.5067492519495));
#444027=CARTESIAN_POINT('Ctrl Pts',(2.18620657115002,-1.65852344278577,
12.5071004286051));
#444028=CARTESIAN_POINT('Ctrl Pts',(2.18555042879403,-1.65930801565087,
12.5076537929612));
#444029=CARTESIAN_POINT('Ctrl Pts',(2.18492764820123,-1.65995561906305,
12.5083435010503));
#444030=CARTESIAN_POINT('Ctrl Pts',(2.18488844044109,-1.65999638956802,
12.5083869222963));
#444031=CARTESIAN_POINT('Ctrl Pts',(2.1848493520306,-1.66003661337411,12.5084308732336));
#444032=CARTESIAN_POINT('Ctrl Pts',(2.18481039171186,-1.66007627612276,
12.5084753333615));
#444033=CARTESIAN_POINT('Ctrl Pts',(2.18449787853311,-1.66039442371644,
12.508831962269));
#444034=CARTESIAN_POINT('Ctrl Pts',(2.18418818278667,-1.66068383495248,
12.509227847131));
#444035=CARTESIAN_POINT('Ctrl Pts',(2.18389242514581,-1.66093794992714,
12.5096423454524));
#444036=CARTESIAN_POINT('Ctrl Pts',(2.18296565159621,-1.66173423379116,
12.5109411997424));
#444037=CARTESIAN_POINT('Ctrl Pts',(2.18212503728312,-1.66224024729522,
12.5124831113042));
#444038=CARTESIAN_POINT('Ctrl Pts',(2.18138269873447,-1.66254984696361,
12.5140723025008));
#444039=CARTESIAN_POINT('Ctrl Pts',(2.1813131407994,-1.66257885679163,12.5142212114565));
#444040=CARTESIAN_POINT('Ctrl Pts',(2.18124443894086,-1.66260617094912,
12.5143705582413));
#444041=CARTESIAN_POINT('Ctrl Pts',(2.18117660076271,-1.66263188346759,
12.5145201959299));
#444042=CARTESIAN_POINT('Ctrl Pts',(2.18030511836381,-1.66296219904925,
12.5164425148273));
#444043=CARTESIAN_POINT('Ctrl Pts',(2.1795501168198,-1.66304955148419,12.518463520594));
#444044=CARTESIAN_POINT('Ctrl Pts',(2.17887493203607,-1.66297636481453,
12.5205025929157));
#444045=CARTESIAN_POINT('Ctrl Pts',(2.17848329809969,-1.66293391364528,
12.5216853356836));
#444046=CARTESIAN_POINT('Ctrl Pts',(2.17811917353142,-1.66283800716306,
12.5228750347131));
#444047=CARTESIAN_POINT('Ctrl Pts',(2.17778094595008,-1.66270682045728,
12.5240609649613));
#444048=CARTESIAN_POINT('Ctrl Pts',(2.17695078449697,-1.66238482972586,
12.5269717671327));
#444049=CARTESIAN_POINT('Ctrl Pts',(2.17625702961506,-1.66183154575537,
12.5299036066169));
#444050=CARTESIAN_POINT('Ctrl Pts',(2.17565724539176,-1.66112252459092,
12.532813300402));
#444051=CARTESIAN_POINT('Ctrl Pts',(2.1753693140402,-1.66078215314692,12.5342101228452));
#444052=CARTESIAN_POINT('Ctrl Pts',(2.17510379815577,-1.66040597736117,
12.5356023438238));
#444053=CARTESIAN_POINT('Ctrl Pts',(2.17485966055454,-1.66000200552886,
12.5369868989719));
#444054=CARTESIAN_POINT('Origin',(8.762946539626,-12.571485399216,-1.24088865030942));
#444055=CARTESIAN_POINT('Ctrl Pts',(2.23801650804472,-1.57375044083148,
12.5369868989719));
#444056=CARTESIAN_POINT('Ctrl Pts',(2.25291760523941,-1.57738920519317,
12.5369868989719));
#444057=CARTESIAN_POINT('Ctrl Pts',(2.26148447100907,-1.5646655219776,12.5369868989719));
#444058=CARTESIAN_POINT('Ctrl Pts',(2.24305367738201,-1.57498042117505,
12.5218025310016));
#444059=CARTESIAN_POINT('Ctrl Pts',(2.25485934340535,-1.57444927764403,
12.5216901060418));
#444060=CARTESIAN_POINT('Ctrl Pts',(2.26145837004303,-1.56470431719146,
12.5161920673678));
#444061=CARTESIAN_POINT('Ctrl Pts',(2.24530812011375,-1.58057090945112,
12.5042015548894));
#444062=CARTESIAN_POINT('Ctrl Pts',(2.25156852116383,-1.57909282836108,
12.4980677368513));
#444063=CARTESIAN_POINT('Ctrl Pts',(2.25546595854791,-1.57352499560848,
12.4907278922777));
#444064=CARTESIAN_POINT('Ctrl Pts',(2.23587950938567,-1.58991651132813,
12.506463626192));
#444065=CARTESIAN_POINT('Ctrl Pts',(2.24121159725135,-1.5937081174956,12.4999376786891));
#444066=CARTESIAN_POINT('Ctrl Pts',(2.24114647355092,-1.59366180853925,
12.4906970594712));
#444067=CARTESIAN_POINT('Origin',(2.24323543307858,-1.55237843059634,12.5369868989719));
#444068=CARTESIAN_POINT('Origin',(2.24323543307858,-1.55237843059634,14.));
#444069=CARTESIAN_POINT('Origin',(2.24323543307858,-1.55237843059634,13.7435492065112));
#444070=CARTESIAN_POINT('Ctrl Pts',(2.21399268294759,-1.56793230853741,
13.793642941384));
#444071=CARTESIAN_POINT('Ctrl Pts',(2.22449477640208,-1.57050373850516,
13.8071662555867));
#444072=CARTESIAN_POINT('Ctrl Pts',(2.23093289057839,-1.55473763342218,
13.8103758687955));
#444073=CARTESIAN_POINT('Ctrl Pts',(2.23014681614542,-1.57184455672094,
13.7804579775006));
#444074=CARTESIAN_POINT('Ctrl Pts',(2.24310786195665,-1.5750076190359,13.7901904343351));
#444075=CARTESIAN_POINT('Ctrl Pts',(2.25134599754834,-1.56157672010332,
13.7927914348263));
#444076=CARTESIAN_POINT('Ctrl Pts',(2.23965736231638,-1.57414784442409,
13.7597120340895));
#444077=CARTESIAN_POINT('Ctrl Pts',(2.25465830098779,-1.57780283128438,
13.7635825532445));
#444078=CARTESIAN_POINT('Ctrl Pts',(2.26339170400959,-1.56558548346241,
13.7651073818884));
#444079=CARTESIAN_POINT('Ctrl Pts',(2.23779497960954,-1.57369680795173,
13.7381884353898));
#444080=CARTESIAN_POINT('Ctrl Pts',(2.25244458058657,-1.57726711631938,
13.7368803041982));
#444081=CARTESIAN_POINT('Ctrl Pts',(2.26103295281073,-1.56479997953268,
13.7363986145813));
#444082=CARTESIAN_POINT('Origin',(2.2230907626871,-1.5474997479986,13.7902182540695));
#444083=CARTESIAN_POINT('Ctrl Pts',(2.18314661127931,-1.56046196312631,
13.8235227101244));
#444084=CARTESIAN_POINT('Ctrl Pts',(2.19431961727935,-1.56317242899826,
13.8358800583119));
#444085=CARTESIAN_POINT('Ctrl Pts',(2.2010531700821,-1.54803025888596,13.8390832900376));
#444086=CARTESIAN_POINT('Ctrl Pts',(2.19473907242423,-1.56326945202192,
13.8124254819053));
#444087=CARTESIAN_POINT('Ctrl Pts',(2.2059337763091,-1.56598518130984,13.8247886449158));
#444088=CARTESIAN_POINT('Ctrl Pts',(2.21266026338467,-1.55081695291213,
13.8279860620657));
#444089=CARTESIAN_POINT('Ctrl Pts',(2.20632633820512,-1.56607568269234,
13.8013225099955));
#444090=CARTESIAN_POINT('Ctrl Pts',(2.21753745739973,-1.56879539595624,
13.8136962257787));
#444091=CARTESIAN_POINT('Ctrl Pts',(2.22426191989538,-1.5536026204025,13.8168830918626));
#444092=CARTESIAN_POINT('Ctrl Pts',(2.21790861076574,-1.5688807040932,13.7902140179785));
#444093=CARTESIAN_POINT('Ctrl Pts',(2.22913120795064,-1.57160320551105,
13.802602731458));
#444094=CARTESIAN_POINT('Ctrl Pts',(2.23585835280941,-1.55638730348156,
13.8057746032558));
#444095=CARTESIAN_POINT('Origin',(2.18832875108978,-1.5390810040953,13.8235269408515));
#444096=CARTESIAN_POINT('Ctrl Pts',(2.14563951868151,-1.61165173575206,
13.8235269408515));
#444097=CARTESIAN_POINT('Ctrl Pts',(2.1517466565921,-1.62175715436447,13.8362179249168));
#444098=CARTESIAN_POINT('Ctrl Pts',(2.13875151770214,-1.63283819083621,
13.8391868794938));
#444099=CARTESIAN_POINT('Ctrl Pts',(2.14005175332123,-1.60240571758443,
13.8400110824519));
#444100=CARTESIAN_POINT('Ctrl Pts',(2.14202032630649,-1.61227722118133,
13.8494522556837));
#444101=CARTESIAN_POINT('Ctrl Pts',(2.1296517939266,-1.61756374122801,13.85569149686));
#444102=CARTESIAN_POINT('Ctrl Pts',(2.13807161119749,-1.58623547444414,
13.8586819406588));
#444103=CARTESIAN_POINT('Ctrl Pts',(2.13550936193527,-1.58975554864125,
13.868010383617));
#444104=CARTESIAN_POINT('Ctrl Pts',(2.12650963586058,-1.59070307034188,
13.8744918421245));
#444105=CARTESIAN_POINT('Ctrl Pts',(2.156524060436,-1.56096536136471,13.8587686893867));
#444106=CARTESIAN_POINT('Ctrl Pts',(2.15906346017857,-1.55747658265759,
13.8680909899357));
#444107=CARTESIAN_POINT('Ctrl Pts',(2.15722962292033,-1.54863727033049,
13.8745789365163));
#444108=CARTESIAN_POINT('Ctrl Pts',(2.17263355069197,-1.55791588671278,
13.8400379222776));
#444109=CARTESIAN_POINT('Ctrl Pts',(2.1826361805068,-1.55681242366595,13.8494748685453));
#444110=CARTESIAN_POINT('Ctrl Pts',(2.18395166365704,-1.54343219162963,
13.8557104837033));
#444111=CARTESIAN_POINT('Ctrl Pts',(2.18315043670878,-1.56046289035168,
13.8235269408542));
#444112=CARTESIAN_POINT('Ctrl Pts',(2.19462617425226,-1.56324211085818,
13.8362179249195));
#444113=CARTESIAN_POINT('Ctrl Pts',(2.20127772059369,-1.54751252296389,
13.8391868794965));
#444114=CARTESIAN_POINT('Origin',(2.12681084552738,-1.62303071054133,13.8235269408515));
#444115=CARTESIAN_POINT('Ctrl Pts',(2.16413706512503,-1.64225943805455,
13.7902140241682));
#444116=CARTESIAN_POINT('Ctrl Pts',(2.17011385323161,-1.65214056143813,
13.8026027327198));
#444117=CARTESIAN_POINT('Ctrl Pts',(2.15763131637958,-1.66313893431829,
13.8057746032556));
#444118=CARTESIAN_POINT('Ctrl Pts',(2.15797323159458,-1.632060205778,13.8013225161808));
#444119=CARTESIAN_POINT('Ctrl Pts',(2.16394390337851,-1.64193122428339,
13.8136962270464));
#444120=CARTESIAN_POINT('Ctrl Pts',(2.15148261063193,-1.65292007264879,
13.8168830918628));
#444121=CARTESIAN_POINT('Ctrl Pts',(2.15180674078005,-1.62185657652063,
13.8124254880875));
#444122=CARTESIAN_POINT('Ctrl Pts',(2.15776866862328,-1.63171314242527,
13.8247886461867));
#444123=CARTESIAN_POINT('Ctrl Pts',(2.14533139261428,-1.64269652658836,
13.8279860620656));
#444124=CARTESIAN_POINT('Ctrl Pts',(2.14563748510417,-1.61164837227547,
13.8235227163065));
#444125=CARTESIAN_POINT('Ctrl Pts',(2.15158785764826,-1.62148583382931,
13.8358800595847));
#444126=CARTESIAN_POINT('Ctrl Pts',(2.13917755793401,-1.63246810553422,
13.8390832900376));
#444127=CARTESIAN_POINT('Origin',(2.14531043198705,-1.65364178696838,13.7902182540695));
#444128=CARTESIAN_POINT('Ctrl Pts',(2.17472005835453,-1.65977106052845,
13.7382347919292));
#444129=CARTESIAN_POINT('Ctrl Pts',(2.18254569879919,-1.67267366570587,
13.7369371795942));
#444130=CARTESIAN_POINT('Ctrl Pts',(2.17323119972871,-1.68462288677196,
13.7364597369711));
#444131=CARTESIAN_POINT('Ctrl Pts',(2.17569842223343,-1.66138994845068,
13.7595490285574));
#444132=CARTESIAN_POINT('Ctrl Pts',(2.18370991608764,-1.6746009201274,13.7633824266926));
#444133=CARTESIAN_POINT('Ctrl Pts',(2.17467320164337,-1.6866105601037,13.7648920890506));
#444134=CARTESIAN_POINT('Ctrl Pts',(2.17070882005703,-1.65313370873311,
13.780380659011));
#444135=CARTESIAN_POINT('Ctrl Pts',(2.17764309149078,-1.66455792711719,
13.7901039518744));
#444136=CARTESIAN_POINT('Ctrl Pts',(2.16732472363235,-1.67647500419857,
13.7926933640891));
#444137=CARTESIAN_POINT('Ctrl Pts',(2.1620357775892,-1.63878252111939,13.7936647693663));
#444138=CARTESIAN_POINT('Ctrl Pts',(2.1676554273783,-1.64802334728335,13.8072068914933));
#444139=CARTESIAN_POINT('Ctrl Pts',(2.15454032634419,-1.65891547263667,
13.8104111085397));
#444140=CARTESIAN_POINT('Origin',(2.15603098740041,-1.67138098031813,13.7435492065112));
#444141=CARTESIAN_POINT('Origin',(2.15603098740041,-1.67138098031813,14.));
#444142=CARTESIAN_POINT('Origin',(2.15603098740041,-1.67138098031813,12.5369868989719));
#444143=CARTESIAN_POINT('Ctrl Pts',(2.1896106362884,-1.65305953679111,12.506462012331));
#444144=CARTESIAN_POINT('Ctrl Pts',(2.19482909441992,-1.656999242709,12.4999388158272));
#444145=CARTESIAN_POINT('Ctrl Pts',(2.19476735321664,-1.65695263082138,
12.4907030323752));
#444146=CARTESIAN_POINT('Ctrl Pts',(2.18353789615505,-1.66486421427197,
12.5042014951932));
#444147=CARTESIAN_POINT('Ctrl Pts',(2.18401514307223,-1.67127618218332,
12.4980716682127));
#444148=CARTESIAN_POINT('Ctrl Pts',(2.17988420991196,-1.67666700368392,
12.4907355092744));
#444149=CARTESIAN_POINT('Ctrl Pts',(2.17752864061987,-1.66440101975751,
12.5218047446509));
#444150=CARTESIAN_POINT('Ctrl Pts',(2.18057599981837,-1.67581296406388,
12.5216906929434));
#444151=CARTESIAN_POINT('Ctrl Pts',(2.17327829202155,-1.68503870063296,
12.5161988840775));
#444152=CARTESIAN_POINT('Ctrl Pts',(2.17483976203157,-1.65996914449412,
12.5369868989719));
#444153=CARTESIAN_POINT('Ctrl Pts',(2.182791679732,-1.67307534670552,12.5369868989719));
#444154=CARTESIAN_POINT('Ctrl Pts',(2.17325023903797,-1.6850739483325,12.5369868989719));
#444155=CARTESIAN_POINT('Origin',(4.15555475928483E-31,-8.19703138220645E-31,
12.5));
#444156=CARTESIAN_POINT('Origin',(2.26986465849443,-1.43139955763526,12.5));
#444157=CARTESIAN_POINT('',(2.26986465849443,-1.43139955763526,12.5893111709658));
#444158=CARTESIAN_POINT('',(2.26986465849443,-1.43139955763526,13.8235269408515));
#444159=CARTESIAN_POINT('',(2.26986465849443,-1.43139955763526,12.5));
#444160=CARTESIAN_POINT('',(2.29079777601444,-1.46040089019248,13.7902182540695));
#444161=CARTESIAN_POINT('',(2.26986465849443,-1.43139955763526,13.8235269408515));
#444162=CARTESIAN_POINT('',(2.30292856860469,-1.47720723304878,13.7435492065112));
#444163=CARTESIAN_POINT('Origin',(2.26301868546698,-1.42191439654958,13.7445212918718));
#444164=CARTESIAN_POINT('',(2.30292856860469,-1.47720723304878,12.5369868989719));
#444165=CARTESIAN_POINT('',(2.30292856860469,-1.47720723304878,12.5));
#444166=CARTESIAN_POINT('Ctrl Pts',(2.30292856860469,-1.47720723304878,
12.5369868989719));
#444167=CARTESIAN_POINT('Ctrl Pts',(2.29191530350295,-1.46194914435506,
12.5544431401645));
#444168=CARTESIAN_POINT('Ctrl Pts',(2.28089416142129,-1.44668014267077,
12.5718848856037));
#444169=CARTESIAN_POINT('Ctrl Pts',(2.26986465849443,-1.43139955763526,
12.5893111709658));
#444170=CARTESIAN_POINT('Origin',(2.5747386521147,-1.42005182257716,12.5));
#444171=CARTESIAN_POINT('',(2.35888624416241,-1.38610132694858,13.7435492065112));
#444172=CARTESIAN_POINT('',(2.33841094557665,-1.38288085541563,13.7902182540695));
#444173=CARTESIAN_POINT('Origin',(2.28460539973481,-1.37441801283617,13.7418732680441));
#444174=CARTESIAN_POINT('',(2.30307839592133,-1.37732355084812,13.8235269408515));
#444175=CARTESIAN_POINT('',(2.33841094557665,-1.38288085541563,13.7902182540695));
#444176=CARTESIAN_POINT('',(2.30307839592133,-1.37732355084812,12.5893111709658));
#444177=CARTESIAN_POINT('',(2.30307839592133,-1.37732355084812,12.5));
#444178=CARTESIAN_POINT('',(2.35888624416241,-1.38610132694858,12.5369868989719));
#444179=CARTESIAN_POINT('Ctrl Pts',(2.30307839592133,-1.37732355084812,
12.5893111709658));
#444180=CARTESIAN_POINT('Ctrl Pts',(2.32169485185363,-1.38025165302565,
12.5718848856037));
#444181=CARTESIAN_POINT('Ctrl Pts',(2.34029719569878,-1.38317753557376,
12.5544431401645));
#444182=CARTESIAN_POINT('Ctrl Pts',(2.35888624416241,-1.38610132694858,
12.5369868989719));
#444183=CARTESIAN_POINT('',(2.35888624416241,-1.38610132694858,12.5));
#444184=CARTESIAN_POINT('Origin',(2.2977373619552,-1.4112810828723,12.5));
#444185=CARTESIAN_POINT('',(2.26787642171629,-1.39425420940044,13.8587068136939));
#444186=CARTESIAN_POINT('Ctrl Pts',(2.30307839592221,-1.37732355084157,
13.8235269408542));
#444187=CARTESIAN_POINT('Ctrl Pts',(2.30134737842234,-1.37705128655405,
13.8262006681044));
#444188=CARTESIAN_POINT('Ctrl Pts',(2.29954894008554,-1.3769442931862,13.8288634856214));
#444189=CARTESIAN_POINT('Ctrl Pts',(2.29768943963348,-1.37699085012767,
13.8314912288862));
#444190=CARTESIAN_POINT('Ctrl Pts',(2.29577248646598,-1.37703884553219,
13.8342001611531));
#444191=CARTESIAN_POINT('Ctrl Pts',(2.29378849793912,-1.37724958285397,
13.8368750301949));
#444192=CARTESIAN_POINT('Ctrl Pts',(2.29172578679966,-1.37765139359663,
13.8394886372969));
#444193=CARTESIAN_POINT('Ctrl Pts',(2.29156647861492,-1.37768242641494,
13.8396904925131));
#444194=CARTESIAN_POINT('Ctrl Pts',(2.29140670128772,-1.37771462110135,
13.8398919674349));
#444195=CARTESIAN_POINT('Ctrl Pts',(2.29124645065801,-1.37774800208598,
13.8400930404591));
#444196=CARTESIAN_POINT('Ctrl Pts',(2.28874963803573,-1.37826810028411,
13.8432258934518));
#444197=CARTESIAN_POINT('Ctrl Pts',(2.28615043854114,-1.3790724253865,13.8462331177034));
#444198=CARTESIAN_POINT('Ctrl Pts',(2.28356214147404,-1.38022689942086,
13.8489036603661));
#444199=CARTESIAN_POINT('Ctrl Pts',(2.28271522055215,-1.38060465676019,
13.8497774930041));
#444200=CARTESIAN_POINT('Ctrl Pts',(2.28186971366704,-1.38101994350902,
13.85061494757));
#444201=CARTESIAN_POINT('Ctrl Pts',(2.28103029631031,-1.38147517117384,
13.8514076489583));
#444202=CARTESIAN_POINT('Ctrl Pts',(2.27925480753871,-1.3824380433386,13.8530843267192));
#444203=CARTESIAN_POINT('Ctrl Pts',(2.27733357270221,-1.38367678415501,
13.8546805203176));
#444204=CARTESIAN_POINT('Ctrl Pts',(2.27545203819607,-1.38523417323291,
13.8559412814274));
#444205=CARTESIAN_POINT('Ctrl Pts',(2.27520022785957,-1.38544260239883,
13.8561100121513));
#444206=CARTESIAN_POINT('Ctrl Pts',(2.27494912963404,-1.38565666209643,
13.8562727473908));
#444207=CARTESIAN_POINT('Ctrl Pts',(2.27469917957348,-1.38587637949884,
13.8564289040185));
#444208=CARTESIAN_POINT('Ctrl Pts',(2.27356565890027,-1.38687279541228,
13.8571370725437));
#444209=CARTESIAN_POINT('Ctrl Pts',(2.27243733035316,-1.38800479233342,
13.8577210840553));
#444210=CARTESIAN_POINT('Ctrl Pts',(2.27137883811568,-1.38924908783344,
13.8581177131616));
#444211=CARTESIAN_POINT('Ctrl Pts',(2.2710807302694,-1.3895995242736,13.8582294175695));
#444212=CARTESIAN_POINT('Ctrl Pts',(2.27078805158048,-1.38995872864847,
13.8583265086086));
#444213=CARTESIAN_POINT('Ctrl Pts',(2.27050195348209,-1.39032585283371,
13.8584082369006));
#444214=CARTESIAN_POINT('Ctrl Pts',(2.27009090723494,-1.39085331183966,
13.8585256585398));
#444215=CARTESIAN_POINT('Ctrl Pts',(2.26968858940448,-1.39140387521847,
13.8586122832068));
#444216=CARTESIAN_POINT('Ctrl Pts',(2.26930608863755,-1.39196370684487,
13.8586682984299));
#444217=CARTESIAN_POINT('Ctrl Pts',(2.26900012594009,-1.39241151665167,
13.8587131050557));
#444218=CARTESIAN_POINT('Ctrl Pts',(2.26870327005296,-1.39287007044899,
13.8587357943552));
#444219=CARTESIAN_POINT('Ctrl Pts',(2.26841591083731,-1.39333969794751,
13.8587355499465));
#444220=CARTESIAN_POINT('Ctrl Pts',(2.26823018372519,-1.39364322939636,
13.8587353919793));
#444221=CARTESIAN_POINT('Ctrl Pts',(2.26805039914152,-1.39394808417961,
13.8587257282814));
#444222=CARTESIAN_POINT('Ctrl Pts',(2.26787642171629,-1.39425420940044,
13.8587068136939));
#444223=CARTESIAN_POINT('Ctrl Pts',(2.26787642171629,-1.39425420940044,
13.8587068136939));
#444224=CARTESIAN_POINT('Ctrl Pts',(2.26730421944952,-1.39526103856263,
13.8586446046466));
#444225=CARTESIAN_POINT('Ctrl Pts',(2.26679475633354,-1.3962815939798,13.858482427929));
#444226=CARTESIAN_POINT('Ctrl Pts',(2.2663439051227,-1.39731415757145,13.8582284286032));
#444227=CARTESIAN_POINT('Ctrl Pts',(2.26588138422549,-1.39837344770389,
13.8579678548414));
#444228=CARTESIAN_POINT('Ctrl Pts',(2.26548082255058,-1.39944857613745,
13.857615680862));
#444229=CARTESIAN_POINT('Ctrl Pts',(2.26514893199382,-1.40049377380576,
13.8571944833187));
#444230=CARTESIAN_POINT('Ctrl Pts',(2.26432066516643,-1.4031021714811,13.8561433417727));
#444231=CARTESIAN_POINT('Ctrl Pts',(2.26387676991979,-1.4056447207958,13.8546163505474));
#444232=CARTESIAN_POINT('Ctrl Pts',(2.26368707230366,-1.40796075871947,
13.8528973491086));
#444233=CARTESIAN_POINT('Ctrl Pts',(2.26365241734792,-1.40838386467815,
13.8525833129072));
#444234=CARTESIAN_POINT('Ctrl Pts',(2.26362611570316,-1.40879946590234,
13.8522628768811));
#444235=CARTESIAN_POINT('Ctrl Pts',(2.2636072217659,-1.4092066771157,13.851937733538));
#444236=CARTESIAN_POINT('Ctrl Pts',(2.26349183911251,-1.41169345949778,
13.8499521282529));
#444237=CARTESIAN_POINT('Ctrl Pts',(2.26364532468864,-1.41411467528469,
13.847639871647));
#444238=CARTESIAN_POINT('Ctrl Pts',(2.26397943210495,-1.41634815707579,
13.8452109780794));
#444239=CARTESIAN_POINT('Ctrl Pts',(2.26412975394722,-1.41735304676438,
13.8441181685877));
#444240=CARTESIAN_POINT('Ctrl Pts',(2.26431600947868,-1.41832027885654,
13.8430021611332));
#444241=CARTESIAN_POINT('Ctrl Pts',(2.26452789519342,-1.41924113747119,
13.8418824960098));
#444242=CARTESIAN_POINT('Ctrl Pts',(2.26502720929088,-1.42141116431158,
13.8392439765549));
#444243=CARTESIAN_POINT('Ctrl Pts',(2.26568903661406,-1.4234282539864,13.8364981347964));
#444244=CARTESIAN_POINT('Ctrl Pts',(2.26648261240662,-1.4253084094306,13.8336931113419));
#444245=CARTESIAN_POINT('Ctrl Pts',(2.26725550483186,-1.42713956143234,
13.8309611966328));
#444246=CARTESIAN_POINT('Ctrl Pts',(2.26815466207456,-1.42884243963993,
13.8281701127185));
#444247=CARTESIAN_POINT('Ctrl Pts',(2.26917982872818,-1.43040442059757,
13.8253580685121));
#444248=CARTESIAN_POINT('Ctrl Pts',(2.26940208596508,-1.43074305975492,
13.8247484142932));
#444249=CARTESIAN_POINT('Ctrl Pts',(2.26963033320496,-1.43107491675748,
13.8241378483365));
#444250=CARTESIAN_POINT('Ctrl Pts',(2.26986465849443,-1.43139955763526,
13.8235269408515));
#444251=CARTESIAN_POINT('',(2.26851103077193,-1.39318647900124,12.5969504640361));
#444252=CARTESIAN_POINT('Origin',(2.29776545178004,-1.41129856556518,12.584524458991));
#444253=CARTESIAN_POINT('Origin',(2.29776545178004,-1.41129856556518,12.584524458991));
#444254=CARTESIAN_POINT('Ctrl Pts',(2.30307839592133,-1.37732355084812,
12.5893111709658));
#444255=CARTESIAN_POINT('Ctrl Pts',(2.29188208210004,-1.37556253086668,
12.5770542771492));
#444256=CARTESIAN_POINT('Ctrl Pts',(2.28637003248253,-1.39097100203903,
12.5737548217797));
#444257=CARTESIAN_POINT('Ctrl Pts',(2.32756097665388,-1.38117431053166,
12.5663937883685));
#444258=CARTESIAN_POINT('Ctrl Pts',(2.31635038037941,-1.37941104412465,
12.5540940315304));
#444259=CARTESIAN_POINT('Ctrl Pts',(2.31082427358596,-1.39486834463351,
12.5508374392248));
#444260=CARTESIAN_POINT('Ctrl Pts',(2.35201885476263,-1.38502118484589,
12.5434499600945));
#444261=CARTESIAN_POINT('Ctrl Pts',(2.34077180884744,-1.3832521854319,12.5311293540533));
#444262=CARTESIAN_POINT('Ctrl Pts',(2.33525480807067,-1.39876071427864,
12.5278936106989));
#444263=CARTESIAN_POINT('Ctrl Pts',(2.37645396523784,-1.38886447813709,
12.5204817579905));
#444264=CARTESIAN_POINT('Ctrl Pts',(2.36515125413168,-1.38708672338494,
12.5081597038247));
#444265=CARTESIAN_POINT('Ctrl Pts',(2.35966348068816,-1.40264848381001,
12.5049254088044));
#444266=CARTESIAN_POINT('Ctrl Pts',(2.35888624416241,-1.38610132694858,
12.5369868989719));
#444267=CARTESIAN_POINT('Ctrl Pts',(2.35980643624434,-1.38624606016203,
12.5342545179733));
#444268=CARTESIAN_POINT('Ctrl Pts',(2.36066524308006,-1.3865074180245,12.5314872231885));
#444269=CARTESIAN_POINT('Ctrl Pts',(2.36139801157162,-1.38692415708904,
12.5287124745063));
#444270=CARTESIAN_POINT('Ctrl Pts',(2.3620588585687,-1.38729999306251,12.5262100684184));
#444271=CARTESIAN_POINT('Ctrl Pts',(2.36261604139187,-1.38780268147425,
12.5237004536639));
#444272=CARTESIAN_POINT('Ctrl Pts',(2.36303472139004,-1.38849007337888,
12.5212220730815));
#444273=CARTESIAN_POINT('Ctrl Pts',(2.36335525714735,-1.38901633134602,
12.5193246583486));
#444274=CARTESIAN_POINT('Ctrl Pts',(2.36359790214585,-1.38965746785863,
12.517417831369));
#444275=CARTESIAN_POINT('Ctrl Pts',(2.36368029788434,-1.39046516560269,
12.5155812248348));
#444276=CARTESIAN_POINT('Ctrl Pts',(2.36371539891181,-1.39080924918306,
12.5147988205793));
#444277=CARTESIAN_POINT('Ctrl Pts',(2.36372172903659,-1.39118388157121,
12.5140295443047));
#444278=CARTESIAN_POINT('Ctrl Pts',(2.36369479068353,-1.39159407308499,
12.5132817086137));
#444279=CARTESIAN_POINT('Ctrl Pts',(2.3636540231303,-1.39221484245163,12.5121499604604));
#444280=CARTESIAN_POINT('Ctrl Pts',(2.36352904502263,-1.3929299883035,12.5110494206568));
#444281=CARTESIAN_POINT('Ctrl Pts',(2.36328305937668,-1.39374524481264,
12.5100666561695));
#444282=CARTESIAN_POINT('Ctrl Pts',(2.36314181498524,-1.39421336322282,
12.5095023550641));
#444283=CARTESIAN_POINT('Ctrl Pts',(2.36295841717765,-1.39471970853939,
12.5089719619137));
#444284=CARTESIAN_POINT('Ctrl Pts',(2.36273029833549,-1.39525261479832,
12.5085043804652));
#444285=CARTESIAN_POINT('Ctrl Pts',(2.36239647612457,-1.39603245369234,
12.5078201359221));
#444286=CARTESIAN_POINT('Ctrl Pts',(2.36195609370366,-1.39689131417924,
12.5072563000949));
#444287=CARTESIAN_POINT('Ctrl Pts',(2.36143146910095,-1.3977671154196,12.5068768744332));
#444288=CARTESIAN_POINT('Ctrl Pts',(2.36105317864711,-1.39839862840426,
12.5066032824114));
#444289=CARTESIAN_POINT('Ctrl Pts',(2.36062449281724,-1.39905007516336,
12.5064197834844));
#444290=CARTESIAN_POINT('Ctrl Pts',(2.36017150981905,-1.39968649813641,
12.5063282718343));
#444291=CARTESIAN_POINT('Ctrl Pts',(2.35951029488168,-1.4006154786455,12.5061946931565));
#444292=CARTESIAN_POINT('Ctrl Pts',(2.3587840427513,-1.40153291982786,12.5062515701262));
#444293=CARTESIAN_POINT('Ctrl Pts',(2.35804995117132,-1.40239148209754,
12.5064436508398));
#444294=CARTESIAN_POINT('',(2.28637003248253,-1.39097100203903,12.5737548217797));
#444295=CARTESIAN_POINT('Origin',(2.299660134183,-1.39905637134359,12.5893111709658));
#444296=CARTESIAN_POINT('Ctrl Pts',(2.35804995117132,-1.40239148209754,
12.5064436508398));
#444297=CARTESIAN_POINT('Ctrl Pts',(2.34743938532467,-1.40070142879506,
12.5164271754438));
#444298=CARTESIAN_POINT('Ctrl Pts',(2.33682464631719,-1.39901049922118,
12.5264061185523));
#444299=CARTESIAN_POINT('Ctrl Pts',(2.32620558702475,-1.39731866344904,
12.536380305637));
#444300=CARTESIAN_POINT('Ctrl Pts',(2.3129339166865,-1.39520421187513,12.5488460165097));
#444301=CARTESIAN_POINT('Ctrl Pts',(2.29965549417674,-1.3930883441773,12.5613043021964));
#444302=CARTESIAN_POINT('Ctrl Pts',(2.28637003248253,-1.39097100203903,
12.5737548217797));
#444303=CARTESIAN_POINT('Ctrl Pts',(2.26986465849443,-1.43139955763526,
12.5893111709658));
#444304=CARTESIAN_POINT('Ctrl Pts',(2.26323129194437,-1.42220950416576,
12.5770542771492));
#444305=CARTESIAN_POINT('Ctrl Pts',(2.27448218809862,-1.41032585949835,
12.5737548217797));
#444306=CARTESIAN_POINT('Ctrl Pts',(2.2636757851972,-1.42282531767908,12.5928319619712));
#444307=CARTESIAN_POINT('Ctrl Pts',(2.26185926858336,-1.41474239223324,
12.5821634970842));
#444308=CARTESIAN_POINT('Ctrl Pts',(2.27222007793515,-1.40720799564986,
12.5773203894503));
#444309=CARTESIAN_POINT('Ctrl Pts',(2.26043077704263,-1.40639199721679,
12.5969440695591));
#444310=CARTESIAN_POINT('Ctrl Pts',(2.26251900213886,-1.40295719613093,
12.5878292599214));
#444311=CARTESIAN_POINT('Ctrl Pts',(2.27106549803164,-1.40135042854875,
12.5813877129824));
#444312=CARTESIAN_POINT('Ctrl Pts',(2.27639828339932,-1.38029192085117,
12.596957478804));
#444313=CARTESIAN_POINT('Ctrl Pts',(2.27432555934013,-1.38370137947732,
12.5878468778671));
#444314=CARTESIAN_POINT('Ctrl Pts',(2.27678557831023,-1.39201196240539,
12.5814011370086));
#444315=CARTESIAN_POINT('Ctrl Pts',(2.2926171648404,-1.37567814886506,12.5928371701607));
#444316=CARTESIAN_POINT('Ctrl Pts',(2.28459362301432,-1.37771722764459,
12.5821692192951));
#444317=CARTESIAN_POINT('Ctrl Pts',(2.28255412617039,-1.39036097212917,
12.5773318885715));
#444318=CARTESIAN_POINT('Ctrl Pts',(2.30307839592133,-1.37732355084807,
12.5893111709658));
#444319=CARTESIAN_POINT('Ctrl Pts',(2.29188208210005,-1.37556253086663,
12.5770542771492));
#444320=CARTESIAN_POINT('Ctrl Pts',(2.28637003248254,-1.39097100203898,
12.5737548217797));
#444321=CARTESIAN_POINT('',(2.27448218809862,-1.41032585949835,12.5737548217797));
#444322=CARTESIAN_POINT('Origin',(2.28770318870932,-1.41852373378696,12.5893111709658));
#444323=CARTESIAN_POINT('Ctrl Pts',(2.28637003248254,-1.39097100203898,
12.5737548217797));
#444324=CARTESIAN_POINT('Ctrl Pts',(2.28538565102293,-1.39078308510786,
12.5746934679442));
#444325=CARTESIAN_POINT('Ctrl Pts',(2.28426201806981,-1.39075507752102,
12.5756680099006));
#444326=CARTESIAN_POINT('Ctrl Pts',(2.28312705412017,-1.39088683677503,
12.5765688348656));
#444327=CARTESIAN_POINT('Ctrl Pts',(2.28282658497898,-1.3909217185789,12.5768073183026));
#444328=CARTESIAN_POINT('Ctrl Pts',(2.28252535508133,-1.39096754301512,
12.5770407398754));
#444329=CARTESIAN_POINT('Ctrl Pts',(2.28222566845064,-1.39102374858678,
12.5772674179684));
#444330=CARTESIAN_POINT('Ctrl Pts',(2.28099583555695,-1.39125440105424,
12.5781976435658));
#444331=CARTESIAN_POINT('Ctrl Pts',(2.27972421996184,-1.39168406518009,
12.5790594849312));
#444332=CARTESIAN_POINT('Ctrl Pts',(2.27851214095502,-1.39232947761016,
12.5797571720116));
#444333=CARTESIAN_POINT('Ctrl Pts',(2.27772242789959,-1.39274998701531,
12.580211740231));
#444334=CARTESIAN_POINT('Ctrl Pts',(2.2769309229698,-1.39329776153685,12.5806009430798));
#444335=CARTESIAN_POINT('Ctrl Pts',(2.27620342682111,-1.39394880839996,
12.5808812374708));
#444336=CARTESIAN_POINT('Ctrl Pts',(2.27557826628506,-1.39450827363791,
12.5811221033394));
#444337=CARTESIAN_POINT('Ctrl Pts',(2.27498765050849,-1.39515553923808,
12.581287365893));
#444338=CARTESIAN_POINT('Ctrl Pts',(2.27447107400921,-1.39585969263319,
12.581359338449));
#444339=CARTESIAN_POINT('Ctrl Pts',(2.27439928054271,-1.39595755541491,
12.5813693411482));
#444340=CARTESIAN_POINT('Ctrl Pts',(2.27432885984084,-1.39605649969674,
12.5813775999465));
#444341=CARTESIAN_POINT('Ctrl Pts',(2.27425985889324,-1.39615642581402,
12.5813841266931));
#444342=CARTESIAN_POINT('Ctrl Pts',(2.27414279044014,-1.39632596255781,
12.5813952001081));
#444343=CARTESIAN_POINT('Ctrl Pts',(2.27402952574154,-1.39649980698298,
12.5814007534795));
#444344=CARTESIAN_POINT('Ctrl Pts',(2.27392027936166,-1.39667799102921,
12.5814005856065));
#444345=CARTESIAN_POINT('Ctrl Pts',(2.27342019214716,-1.3974936479274,12.5813998171494));
#444346=CARTESIAN_POINT('Ctrl Pts',(2.27303857126983,-1.39834370739983,
12.58127954464));
#444347=CARTESIAN_POINT('Ctrl Pts',(2.27275058939736,-1.39921122486263,
12.5810700125799));
#444348=CARTESIAN_POINT('Ctrl Pts',(2.27240274008478,-1.40025908718291,
12.5808169217085));
#444349=CARTESIAN_POINT('Ctrl Pts',(2.27220736129675,-1.40133778801662,
12.5804173076348));
#444350=CARTESIAN_POINT('Ctrl Pts',(2.27215595027872,-1.40234815046391,
12.5799304713245));
#444351=CARTESIAN_POINT('Ctrl Pts',(2.27209223583124,-1.40360030783308,
12.5793271277669));
#444352=CARTESIAN_POINT('Ctrl Pts',(2.272213530687,-1.40482354140291,12.5785808224116));
#444353=CARTESIAN_POINT('Ctrl Pts',(2.27248315996397,-1.4059694191957,12.5777485681082));
#444354=CARTESIAN_POINT('Ctrl Pts',(2.27288493712676,-1.40767690264723,
12.576508418016));
#444355=CARTESIAN_POINT('Ctrl Pts',(2.2736060073491,-1.40919981999404,12.5750928681475));
#444356=CARTESIAN_POINT('Ctrl Pts',(2.27448218809862,-1.41032585949835,
12.5737548217797));
#444357=CARTESIAN_POINT('Ctrl Pts',(2.27448218809862,-1.41032585949835,
12.5737548217797));
#444358=CARTESIAN_POINT('Ctrl Pts',(2.26323129194437,-1.42220950416576,
12.5770542771492));
#444359=CARTESIAN_POINT('Ctrl Pts',(2.26986465849443,-1.43139955763526,
12.5893111709658));
#444360=CARTESIAN_POINT('Ctrl Pts',(2.28901368541375,-1.43037206961276,
12.5508408821982));
#444361=CARTESIAN_POINT('Ctrl Pts',(2.27772559675031,-1.44229032363573,
12.5540974840599));
#444362=CARTESIAN_POINT('Ctrl Pts',(2.2843674257772,-1.45149210125976,12.5663972313419));
#444363=CARTESIAN_POINT('Ctrl Pts',(2.30353003229531,-1.45039938937864,
12.52790050457));
#444364=CARTESIAN_POINT('Ctrl Pts',(2.29219214151271,-1.46233268355682,
12.5311362602938));
#444365=CARTESIAN_POINT('Ctrl Pts',(2.29885556215093,-1.47156437480941,
12.5434568539655));
#444366=CARTESIAN_POINT('Ctrl Pts',(2.31803239491436,-1.4704092949462,12.5049357605811));
#444367=CARTESIAN_POINT('Ctrl Pts',(2.30663382007401,-1.48234059314037,
12.5081700652078));
#444368=CARTESIAN_POINT('Ctrl Pts',(2.31333021351133,-1.49161796584055,
12.5204921097672));
#444369=CARTESIAN_POINT('Ctrl Pts',(2.31708011165217,-1.4690953670416,12.5064436508395));
#444370=CARTESIAN_POINT('Ctrl Pts',(2.31661148323748,-1.47022197043212,
12.5062361689309));
#444371=CARTESIAN_POINT('Ctrl Pts',(2.31607610716433,-1.47137356240879,
12.5061871075061));
#444372=CARTESIAN_POINT('Ctrl Pts',(2.31549606977494,-1.47245733972357,
12.5063648335164));
#444373=CARTESIAN_POINT('Ctrl Pts',(2.31523258101449,-1.4729496582301,12.5064455676329));
#444374=CARTESIAN_POINT('Ctrl Pts',(2.31495600686275,-1.47343474579154,
12.506574497099));
#444375=CARTESIAN_POINT('Ctrl Pts',(2.3146772930091,-1.47389128276949,12.5067492519495));
#444376=CARTESIAN_POINT('Ctrl Pts',(2.31411720670134,-1.47480871154813,
12.5071004286051));
#444377=CARTESIAN_POINT('Ctrl Pts',(2.31352719757705,-1.47564415550508,
12.5076537929612));
#444378=CARTESIAN_POINT('Ctrl Pts',(2.31295927492544,-1.47634036647026,
12.5083435010503));
#444379=CARTESIAN_POINT('Ctrl Pts',(2.31292352080054,-1.47638419711118,
12.5083869222963));
#444380=CARTESIAN_POINT('Ctrl Pts',(2.31288784106712,-1.47642747314421,
12.5084308732336));
#444381=CARTESIAN_POINT('Ctrl Pts',(2.31285224326785,-1.476470179546,12.5084753333615));
#444382=CARTESIAN_POINT('Ctrl Pts',(2.31256670193335,-1.47681274125511,
12.508831962269));
#444383=CARTESIAN_POINT('Ctrl Pts',(2.31228162637645,-1.47712643257754,
12.509227847131));
#444384=CARTESIAN_POINT('Ctrl Pts',(2.31200756557427,-1.477403808999,12.5096423454524));
#444385=CARTESIAN_POINT('Ctrl Pts',(2.31114878031446,-1.47827298394218,
12.5109411997424));
#444386=CARTESIAN_POINT('Ctrl Pts',(2.31035220787434,-1.47884583159845,
12.5124831113042));
#444387=CARTESIAN_POINT('Ctrl Pts',(2.30963757464312,-1.47921490858273,
12.5140723025008));
#444388=CARTESIAN_POINT('Ctrl Pts',(2.30957061272664,-1.4792494915004,12.5142212114565));
#444389=CARTESIAN_POINT('Ctrl Pts',(2.30950436582528,-1.47928231461156,
12.5143705582413));
#444390=CARTESIAN_POINT('Ctrl Pts',(2.30943884918202,-1.47931347101504,
12.5145201959299));
#444391=CARTESIAN_POINT('Ctrl Pts',(2.30859719035533,-1.47971372140481,
12.5164425148273));
#444392=CARTESIAN_POINT('Ctrl Pts',(2.30785182105105,-1.47986232281666,
12.518463520594));
#444393=CARTESIAN_POINT('Ctrl Pts',(2.30717291749599,-1.47984441349759,
12.5205025929157));
#444394=CARTESIAN_POINT('Ctrl Pts',(2.30677912652483,-1.47983402538267,
12.5216853356836));
#444395=CARTESIAN_POINT('Ctrl Pts',(2.30640839628238,-1.47976811755404,
12.5228750347131));
#444396=CARTESIAN_POINT('Ctrl Pts',(2.30606060119101,-1.47966493604902,
12.5240609649613));
#444397=CARTESIAN_POINT('Ctrl Pts',(2.30520695679783,-1.47941168258047,
12.5269717671327));
#444398=CARTESIAN_POINT('Ctrl Pts',(2.30447041254802,-1.47891678708014,
12.5299036066169));
#444399=CARTESIAN_POINT('Ctrl Pts',(2.30381483225012,-1.47825901310745,
12.5328133004019));
#444400=CARTESIAN_POINT('Ctrl Pts',(2.30350011553383,-1.47794324329952,
12.5342101228451));
#444401=CARTESIAN_POINT('Ctrl Pts',(2.30320482131282,-1.47758996121718,
12.5356023438238));
#444402=CARTESIAN_POINT('Ctrl Pts',(2.30292856860469,-1.47720723304878,
12.5369868989719));
#444403=CARTESIAN_POINT('Origin',(9.75800831304548,-11.8147356748686,-1.24001512903272));
#444404=CARTESIAN_POINT('Ctrl Pts',(2.35884496365163,-1.38609479392766,
12.5369868989719));
#444405=CARTESIAN_POINT('Ctrl Pts',(2.37399307175077,-1.3885068728447,12.5369868989719));
#444406=CARTESIAN_POINT('Ctrl Pts',(2.38149433367832,-1.37512724754428,
12.5369868989719));
#444407=CARTESIAN_POINT('Ctrl Pts',(2.36396562704008,-1.38691010554931,
12.5218025310016));
#444408=CARTESIAN_POINT('Ctrl Pts',(2.37568871755491,-1.38541845797521,
12.5216901060417));
#444409=CARTESIAN_POINT('Ctrl Pts',(2.38147148173117,-1.37516804114132,
12.5161920673677));
#444410=CARTESIAN_POINT('Ctrl Pts',(2.36666824499362,-1.39229823392494,
12.5042015548895));
#444411=CARTESIAN_POINT('Ctrl Pts',(2.37278733774504,-1.39031479022351,
12.4980677368514));
#444412=CARTESIAN_POINT('Ctrl Pts',(2.37621797666913,-1.38444780664622,
12.4907278922778));
#444413=CARTESIAN_POINT('Ctrl Pts',(2.35803276050328,-1.40238125838799,
12.506463626192));
#444414=CARTESIAN_POINT('Ctrl Pts',(2.36365615738865,-1.40572563363697,
12.4999376786891));
#444415=CARTESIAN_POINT('Ctrl Pts',(2.3635874757721,-1.40568478695602,12.4906970594712));
#444416=CARTESIAN_POINT('Origin',(2.36230450590074,-1.36436850645311,12.5369868989719));
#444417=CARTESIAN_POINT('Origin',(2.36230450590074,-1.36436850645311,14.));
#444418=CARTESIAN_POINT('Origin',(2.36230450590074,-1.36436850645311,13.7435492065112));
#444419=CARTESIAN_POINT('Ctrl Pts',(2.33442684405581,-1.38225418576057,
13.793642941384));
#444420=CARTESIAN_POINT('Ctrl Pts',(2.34510358807504,-1.38396104139399,
13.8071662555867));
#444421=CARTESIAN_POINT('Ctrl Pts',(2.3502351960279,-1.36772263065117,13.8103758687955));
#444422=CARTESIAN_POINT('Ctrl Pts',(2.35084611025453,-1.38483670443772,
13.7804579775006));
#444423=CARTESIAN_POINT('Ctrl Pts',(2.36402184819816,-1.38693279636566,
13.7901904343351));
#444424=CARTESIAN_POINT('Ctrl Pts',(2.37113782912386,-1.37287510311147,
13.7927914348262));
#444425=CARTESIAN_POINT('Ctrl Pts',(2.36051275019819,-1.38635713033652,
13.7597120340895));
#444426=CARTESIAN_POINT('Ctrl Pts',(2.375761689844,-1.3887772397659,13.7635825532445));
#444427=CARTESIAN_POINT('Ctrl Pts',(2.38347020591987,-1.37588869073771,
13.7651073818884));
#444428=CARTESIAN_POINT('Ctrl Pts',(2.35861980075643,-1.38605939613093,
13.7381884353898));
#444429=CARTESIAN_POINT('Ctrl Pts',(2.37351166967181,-1.38842374611212,
13.7368803041982));
#444430=CARTESIAN_POINT('Ctrl Pts',(2.38105527740852,-1.37529806062779,
13.7363986145813));
#444431=CARTESIAN_POINT('Origin',(2.34182920731497,-1.36114803492016,13.7902182540695));
#444432=CARTESIAN_POINT('Ctrl Pts',(2.30307450764407,-1.37732293850948,
13.8235227101244));
#444433=CARTESIAN_POINT('Ctrl Pts',(2.31443126451965,-1.37911368181571,
13.8358800583119));
#444434=CARTESIAN_POINT('Ctrl Pts',(2.31990818454372,-1.36347304896064,
13.8390832900376));
#444435=CARTESIAN_POINT('Ctrl Pts',(2.31485723223927,-1.37917619251492,
13.8124254819053));
#444436=CARTESIAN_POINT('Ctrl Pts',(2.32623604381905,-1.38097041314449,
13.8247886449158));
#444437=CARTESIAN_POINT('Ctrl Pts',(2.33170379763438,-1.36530438463317,
13.8279860620657));
#444438=CARTESIAN_POINT('Ctrl Pts',(2.3266346762006,-1.38102861595222,13.8013225099955));
#444439=CARTESIAN_POINT('Ctrl Pts',(2.33803017320052,-1.38282546930125,
13.8136962257787));
#444440=CARTESIAN_POINT('Ctrl Pts',(2.34349390835148,-1.36713514033461,
13.8168830918626));
#444441=CARTESIAN_POINT('Ctrl Pts',(2.33840704498945,-1.3828802411375,13.7902140179785));
#444442=CARTESIAN_POINT('Ctrl Pts',(2.34981420904804,-1.38467893780039,
13.802602731458));
#444443=CARTESIAN_POINT('Ctrl Pts',(2.3552787326143,-1.36896534067192,13.8057746032558));
#444444=CARTESIAN_POINT('Origin',(2.30649665765965,-1.35559073035265,13.8235269408515));
#444445=CARTESIAN_POINT('Ctrl Pts',(2.26986465849443,-1.43139955763526,
13.8235269408515));
#444446=CARTESIAN_POINT('Ctrl Pts',(2.27677516083846,-1.44097356286526,
13.8362179249168));
#444447=CARTESIAN_POINT('Ctrl Pts',(2.26472646954491,-1.45307695256277,
13.8391868794938));
#444448=CARTESIAN_POINT('Ctrl Pts',(2.26354184964589,-1.42263975958145,
13.8400110824519));
#444449=CARTESIAN_POINT('Ctrl Pts',(2.26630849155264,-1.43231795959079,
13.8494522556836));
#444450=CARTESIAN_POINT('Ctrl Pts',(2.25441201490543,-1.438595039391,13.85569149686));
#444451=CARTESIAN_POINT('Ctrl Pts',(2.2602502713486,-1.40668472155711,13.8586819406588));
#444452=CARTESIAN_POINT('Ctrl Pts',(2.25798346648526,-1.41040193009935,
13.868010383617));
#444453=CARTESIAN_POINT('Ctrl Pts',(2.24909091807164,-1.41207986022415,
13.8744918421245));
#444454=CARTESIAN_POINT('Ctrl Pts',(2.27658157277223,-1.3799946467772,13.8587686893867));
#444455=CARTESIAN_POINT('Ctrl Pts',(2.27882815501878,-1.37631049203977,
13.8680909899357));
#444456=CARTESIAN_POINT('Ctrl Pts',(2.2762799336879,-1.36765006655631,13.8745789365163));
#444457=CARTESIAN_POINT('Ctrl Pts',(2.29238889953424,-1.37564224599154,
13.8400379222776));
#444458=CARTESIAN_POINT('Ctrl Pts',(2.30226830394115,-1.37372714743718,
13.8494748685453));
#444459=CARTESIAN_POINT('Ctrl Pts',(2.30248879680276,-1.36028421293006,
13.8557104837033));
#444460=CARTESIAN_POINT('Ctrl Pts',(2.30307839592221,-1.37732355084157,
13.8235269408542));
#444461=CARTESIAN_POINT('Ctrl Pts',(2.314742481168,-1.37915814457576,13.8362179249195));
#444462=CARTESIAN_POINT('Ctrl Pts',(2.32008978759794,-1.36293873281082,
13.8391868794965));
#444463=CARTESIAN_POINT('Origin',(2.25202612827954,-1.44427538148356,13.8235269408515));
#444464=CARTESIAN_POINT('Ctrl Pts',(2.29079546776379,-1.4603976935753,13.7902140241682));
#444465=CARTESIAN_POINT('Ctrl Pts',(2.29755777188865,-1.46975877461948,
13.8026027327198));
#444466=CARTESIAN_POINT('Ctrl Pts',(2.28601323914189,-1.48173799395684,
13.8057746032556));
#444467=CARTESIAN_POINT('Ctrl Pts',(2.28382081176535,-1.45073480805775,
13.8013225161808));
#444468=CARTESIAN_POINT('Ctrl Pts',(2.2905761962777,-1.46008631638396,13.8136962270464));
#444469=CARTESIAN_POINT('Ctrl Pts',(2.27905206061203,-1.47205431130678,
13.8168830918628));
#444470=CARTESIAN_POINT('Ctrl Pts',(2.27684314892995,-1.44106775678328,
13.8124254880875));
#444471=CARTESIAN_POINT('Ctrl Pts',(2.28358864057524,-1.45040557331093,
13.8247886461867));
#444472=CARTESIAN_POINT('Ctrl Pts',(2.27208799635021,-1.46236616462606,
13.8279860620656));
#444473=CARTESIAN_POINT('Ctrl Pts',(2.26986235752908,-1.43139637110578,
13.8235227163065));
#444474=CARTESIAN_POINT('Ctrl Pts',(2.27659477514258,-1.44071608871494,
13.8358800595847));
#444475=CARTESIAN_POINT('Ctrl Pts',(2.26512092677523,-1.45267337245503,
13.8390832900376));
#444476=CARTESIAN_POINT('Origin',(2.27295924579955,-1.47327671404078,13.7902182540695));
#444477=CARTESIAN_POINT('Ctrl Pts',(2.30277060675796,-1.47698843537411,
13.7382347919292));
#444478=CARTESIAN_POINT('Ctrl Pts',(2.31162189013352,-1.48921024585125,
13.7369371795943));
#444479=CARTESIAN_POINT('Ctrl Pts',(2.30331235673834,-1.50187892501582,
13.7364597369711));
#444480=CARTESIAN_POINT('Ctrl Pts',(2.30387766960643,-1.47852219084149,
13.7595490285574));
#444481=CARTESIAN_POINT('Ctrl Pts',(2.31293932271206,-1.49103619297559,
13.7633824266926));
#444482=CARTESIAN_POINT('Ctrl Pts',(2.30491157433978,-1.50374244798558,
13.7648920890506));
#444483=CARTESIAN_POINT('Ctrl Pts',(2.2982317097355,-1.47070012197909,13.780380659011));
#444484=CARTESIAN_POINT('Ctrl Pts',(2.30607408780867,-1.48152111972245,
13.7901039518744));
#444485=CARTESIAN_POINT('Ctrl Pts',(2.29676140588295,-1.49423958648444,
13.7926933640892));
#444486=CARTESIAN_POINT('Ctrl Pts',(2.28841777108056,-1.45710362023598,
13.7936647693663));
#444487=CARTESIAN_POINT('Ctrl Pts',(2.29477193506858,-1.4658556446851,13.8072068914933));
#444488=CARTESIAN_POINT('Ctrl Pts',(2.2825882827851,-1.47778052987879,13.8104111085397));
#444489=CARTESIAN_POINT('Origin',(2.2850900383898,-1.49008305689707,13.7435492065112));
#444490=CARTESIAN_POINT('Origin',(2.2850900383898,-1.49008305689707,14.));
#444491=CARTESIAN_POINT('Origin',(2.2850900383898,-1.49008305689707,12.5369868989719));
#444492=CARTESIAN_POINT('Ctrl Pts',(2.3170645860308,-1.46908552333935,12.506462012331));
#444493=CARTESIAN_POINT('Ctrl Pts',(2.32258680278013,-1.47258676742728,
12.4999388158272));
#444494=CARTESIAN_POINT('Ctrl Pts',(2.32252146771405,-1.47254534311812,
12.4907030323752));
#444495=CARTESIAN_POINT('Ctrl Pts',(2.31197424324324,-1.48134590642715,
12.5042014951932));
#444496=CARTESIAN_POINT('Ctrl Pts',(2.31297253707128,-1.48769763898994,
12.4980716682127));
#444497=CARTESIAN_POINT('Ctrl Pts',(2.30929475124855,-1.49340723237897,
12.4907355092743));
#444498=CARTESIAN_POINT('Ctrl Pts',(2.30594722835712,-1.48137406326756,
12.5218047446509));
#444499=CARTESIAN_POINT('Ctrl Pts',(2.30991462712355,-1.49249964720568,
12.5216906929434));
#444500=CARTESIAN_POINT('Ctrl Pts',(2.30339318502536,-1.50228951683145,
12.5161988840776));
#444501=CARTESIAN_POINT('Ctrl Pts',(2.30290605781301,-1.47717610327077,
12.5369868989719));
#444502=CARTESIAN_POINT('Ctrl Pts',(2.31189979331555,-1.48959054056091,
12.5369868989719));
#444503=CARTESIAN_POINT('Ctrl Pts',(2.3033680984005,-1.50232693382577,12.5369868989719));
#444504=CARTESIAN_POINT('Origin',(4.38993701924924E-31,-7.84818254312661E-31,
12.5));
#444505=CARTESIAN_POINT('Origin',(2.37898422350637,-1.2416216516267,12.5));
#444506=CARTESIAN_POINT('',(2.37898422350637,-1.2416216516267,12.5893111709658));
#444507=CARTESIAN_POINT('',(2.37898422350637,-1.2416216516267,13.8235269408515));
#444508=CARTESIAN_POINT('',(2.37898422350637,-1.2416216516267,12.5));
#444509=CARTESIAN_POINT('',(2.40221156564335,-1.26882024123082,13.7902182540695));
#444510=CARTESIAN_POINT('',(2.37898422350637,-1.2416216516267,13.8235269408515));
#444511=CARTESIAN_POINT('',(2.41567186698724,-1.28458189015479,13.7435492065112));
#444512=CARTESIAN_POINT('Origin',(2.37138790120177,-1.23272606198494,13.7445212918702));
#444513=CARTESIAN_POINT('',(2.41567186698724,-1.28458189015479,12.5369868989719));
#444514=CARTESIAN_POINT('',(2.41567186698724,-1.28458189015479,12.5));
#444515=CARTESIAN_POINT('Ctrl Pts',(2.41567186698724,-1.28458189015479,
12.5369868989719));
#444516=CARTESIAN_POINT('Ctrl Pts',(2.40345157173887,-1.27027225484046,
12.5544431401645));
#444517=CARTESIAN_POINT('Ctrl Pts',(2.39122253621055,-1.25595238489461,
12.5718848856037));
#444518=CARTESIAN_POINT('Ctrl Pts',(2.37898422350637,-1.2416216516267,12.5893111709658));
#444519=CARTESIAN_POINT('Origin',(2.68191882830874,-1.20546161442877,12.5));
#444520=CARTESIAN_POINT('',(2.46401737086259,-1.18921806139777,13.7435492065112));
#444521=CARTESIAN_POINT('',(2.44334770381644,-1.18767723263631,13.7902182540695));
#444522=CARTESIAN_POINT('Origin',(2.38903139125129,-1.1836282009596,13.7418732680428));
#444523=CARTESIAN_POINT('',(2.40767974839162,-1.1850183503496,13.8235269408515));
#444524=CARTESIAN_POINT('',(2.44334770381644,-1.18767723263631,13.7902182540695));
#444525=CARTESIAN_POINT('',(2.40767974839162,-1.1850183503496,12.5893111709658));
#444526=CARTESIAN_POINT('',(2.40767974839162,-1.1850183503496,12.5));
#444527=CARTESIAN_POINT('',(2.46401737086259,-1.18921806139777,12.5369868989719));
#444528=CARTESIAN_POINT('Ctrl Pts',(2.40767974839162,-1.1850183503496,12.5893111709658));
#444529=CARTESIAN_POINT('Ctrl Pts',(2.4264729271132,-1.18641929552346,12.5718848856037));
#444530=CARTESIAN_POINT('Ctrl Pts',(2.44525185978403,-1.18781917871965,
12.5544431401645));
#444531=CARTESIAN_POINT('Ctrl Pts',(2.46401737086259,-1.18921806139777,
12.5369868989719));
#444532=CARTESIAN_POINT('',(2.46401737086259,-1.18921806139777,12.5));
#444533=CARTESIAN_POINT('Origin',(2.40512434038173,-1.21929823533924,12.5));
#444534=CARTESIAN_POINT('',(2.37397491170063,-1.20476196122863,13.8587068136939));
#444535=CARTESIAN_POINT('Ctrl Pts',(2.40767974839197,-1.185018350343,13.8235269408542));
#444536=CARTESIAN_POINT('Ctrl Pts',(2.40593229864302,-1.18488808598866,
13.8262006681044));
#444537=CARTESIAN_POINT('Ctrl Pts',(2.40413112350867,-1.18492803805275,
13.8288634856214));
#444538=CARTESIAN_POINT('Ctrl Pts',(2.40228160521392,-1.18512600662944,
13.8314912288862));
#444539=CARTESIAN_POINT('Ctrl Pts',(2.40037494262099,-1.18533009181249,
13.834200161153));
#444540=CARTESIAN_POINT('Ctrl Pts',(2.39841473270039,-1.1857018414066,13.8368750301949));
#444541=CARTESIAN_POINT('Ctrl Pts',(2.39639163636785,-1.1862704452643,13.8394886372968));
#444542=CARTESIAN_POINT('Ctrl Pts',(2.39623538773073,-1.18631435991947,
13.839690492513));
#444543=CARTESIAN_POINT('Ctrl Pts',(2.39607876621522,-1.18635947081619,
13.8398919674349));
#444544=CARTESIAN_POINT('Ctrl Pts',(2.3959217696664,-1.18640580264236,13.8400930404591));
#444545=CARTESIAN_POINT('Ctrl Pts',(2.39347565781365,-1.18712768366463,
13.8432258934518));
#444546=CARTESIAN_POINT('Ctrl Pts',(2.3909506669038,-1.1881411913302,13.8462331177034));
#444547=CARTESIAN_POINT('Ctrl Pts',(2.38846508253307,-1.18950279418699,
13.8489036603661));
#444548=CARTESIAN_POINT('Ctrl Pts',(2.38765177040077,-1.1899483264875,13.8497774930041));
#444549=CARTESIAN_POINT('Ctrl Pts',(2.38684292659544,-1.19043114806438,
13.85061494757));
#444550=CARTESIAN_POINT('Ctrl Pts',(2.38604340761153,-1.19095328130404,
13.8514076489583));
#444551=CARTESIAN_POINT('Ctrl Pts',(2.38435230965268,-1.1920576684088,13.8530843267192));
#444552=CARTESIAN_POINT('Ctrl Pts',(2.38253843644308,-1.19344888589235,
13.8546805203176));
#444553=CARTESIAN_POINT('Ctrl Pts',(2.38079010425577,-1.19515445541609,
13.8559412814273));
#444554=CARTESIAN_POINT('Ctrl Pts',(2.38055612070934,-1.19538271593131,
13.8561100121513));
#444555=CARTESIAN_POINT('Ctrl Pts',(2.380323305845,-1.19561653019941,13.8562727473908));
#444556=CARTESIAN_POINT('Ctrl Pts',(2.38009209648068,-1.19585588976069,
13.8564289040185));
#444557=CARTESIAN_POINT('Ctrl Pts',(2.37904356465121,-1.19694138264033,
13.8571370725437));
#444558=CARTESIAN_POINT('Ctrl Pts',(2.37801125878228,-1.19816158218658,
13.8577210840553));
#444559=CARTESIAN_POINT('Ctrl Pts',(2.37705771022512,-1.19948801433989,
13.8581177131616));
#444560=CARTESIAN_POINT('Ctrl Pts',(2.37678915813128,-1.19986158328867,
13.8582294175695));
#444561=CARTESIAN_POINT('Ctrl Pts',(2.3765267317978,-1.20024344847086,13.8583265086086));
#444562=CARTESIAN_POINT('Ctrl Pts',(2.37627150969654,-1.20063267073169,
13.8584082369006));
#444563=CARTESIAN_POINT('Ctrl Pts',(2.37590482397754,-1.20119187874641,
13.8585256585398));
#444564=CARTESIAN_POINT('Ctrl Pts',(2.37554872085303,-1.20177340280912,
13.8586122832068));
#444565=CARTESIAN_POINT('Ctrl Pts',(2.37521312430062,-1.20236254900543,
13.8586682984299));
#444566=CARTESIAN_POINT('Ctrl Pts',(2.37494468032531,-1.2028338075623,13.8587131050557));
#444567=CARTESIAN_POINT('Ctrl Pts',(2.37468618859314,-1.20331503207037,
13.8587357943552));
#444568=CARTESIAN_POINT('Ctrl Pts',(2.37443806454252,-1.20380651936591,
13.8587355499465));
#444569=CARTESIAN_POINT('Ctrl Pts',(2.37427769605307,-1.20412417932257,
13.8587353919793));
#444570=CARTESIAN_POINT('Ctrl Pts',(2.37412335818282,-1.20444267383911,
13.8587257282814));
#444571=CARTESIAN_POINT('Ctrl Pts',(2.37397491170063,-1.20476196122863,
13.8587068136939));
#444572=CARTESIAN_POINT('Ctrl Pts',(2.37397491170063,-1.20476196122863,
13.8587068136939));
#444573=CARTESIAN_POINT('Ctrl Pts',(2.37348667931325,-1.20581208004682,
13.8586446046466));
#444574=CARTESIAN_POINT('Ctrl Pts',(2.37306209613455,-1.20687076562378,
13.858482427929));
#444575=CARTESIAN_POINT('Ctrl Pts',(2.37269690861243,-1.20793664200463,
13.8582284286032));
#444576=CARTESIAN_POINT('Ctrl Pts',(2.37232226869512,-1.20903010718349,
13.8579678548414));
#444577=CARTESIAN_POINT('Ctrl Pts',(2.37201067280447,-1.21013430771103,
13.857615680862));
#444578=CARTESIAN_POINT('Ctrl Pts',(2.37176507989927,-1.21120307973182,
13.8571944833187));
#444579=CARTESIAN_POINT('Ctrl Pts',(2.37115217768716,-1.21387030961473,
13.8561433417727));
#444580=CARTESIAN_POINT('Ctrl Pts',(2.37091700083835,-1.21644058038983,
13.8546163505475));
#444581=CARTESIAN_POINT('Ctrl Pts',(2.37091671301721,-1.21876437400513,
13.8528973491086));
#444582=CARTESIAN_POINT('Ctrl Pts',(2.37091666043654,-1.21918889681428,
13.8525833129073));
#444583=CARTESIAN_POINT('Ctrl Pts',(2.37092432166635,-1.21960525898792,
13.8522628768812));
#444584=CARTESIAN_POINT('Ctrl Pts',(2.37093868209137,-1.22001265527087,
13.851937733538));
#444585=CARTESIAN_POINT('Ctrl Pts',(2.37102637921453,-1.22250056784713,
13.8499521282529));
#444586=CARTESIAN_POINT('Ctrl Pts',(2.37137670564418,-1.2249012167389,13.847639871647));
#444587=CARTESIAN_POINT('Ctrl Pts',(2.37189175084623,-1.22710003394746,
13.8452109780794));
#444588=CARTESIAN_POINT('Ctrl Pts',(2.37212348034353,-1.22808932732284,
13.8441181685877));
#444589=CARTESIAN_POINT('Ctrl Pts',(2.37238795451993,-1.22903815947508,
13.8430021611332));
#444590=CARTESIAN_POINT('Ctrl Pts',(2.37267419372836,-1.22993868335585,
13.8418824960098));
#444591=CARTESIAN_POINT('Ctrl Pts',(2.37334872373239,-1.2320607908766,13.8392439765549));
#444592=CARTESIAN_POINT('Ctrl Pts',(2.37417276041399,-1.23401722378097,
13.8364981347964));
#444593=CARTESIAN_POINT('Ctrl Pts',(2.37511694577178,-1.23582643936874,
13.8336931113419));
#444594=CARTESIAN_POINT('Ctrl Pts',(2.37603652234896,-1.23758850045541,
13.8309611966328));
#444595=CARTESIAN_POINT('Ctrl Pts',(2.37707148810278,-1.23921242281359,
13.8281701127186));
#444596=CARTESIAN_POINT('Ctrl Pts',(2.3782205595477,-1.24068564580899,13.8253580685121));
#444597=CARTESIAN_POINT('Ctrl Pts',(2.37846967947708,-1.24100504214435,
13.8247484142933));
#444598=CARTESIAN_POINT('Ctrl Pts',(2.37872421666962,-1.24131719065112,
13.8241378483365));
#444599=CARTESIAN_POINT('Ctrl Pts',(2.37898422350637,-1.2416216516267,13.8235269408515));
#444600=CARTESIAN_POINT('',(2.3745203792069,-1.20364605708527,12.5969504640361));
#444601=CARTESIAN_POINT('Origin',(2.40515376174178,-1.21931337027842,12.584524458991));
#444602=CARTESIAN_POINT('Origin',(2.40515376174178,-1.21931337027842,12.584524458991));
#444603=CARTESIAN_POINT('Ctrl Pts',(2.40767974839162,-1.1850183503496,12.5893111709658));
#444604=CARTESIAN_POINT('Ctrl Pts',(2.39637714990395,-1.18417579353482,
12.5770542771492));
#444605=CARTESIAN_POINT('Ctrl Pts',(2.39213937462264,-1.19998227750565,
12.5737548217797));
#444606=CARTESIAN_POINT('Ctrl Pts',(2.43239473801938,-1.18686073933307,
12.5663937883685));
#444607=CARTESIAN_POINT('Ctrl Pts',(2.42107772149766,-1.18601710772004,
12.5540940315304));
#444608=CARTESIAN_POINT('Ctrl Pts',(2.41682991585875,-1.20187340434213,
12.5508374392248));
#444609=CARTESIAN_POINT('Ctrl Pts',(2.45708479052556,-1.18870126936863,
12.5434499600945));
#444610=CARTESIAN_POINT('Ctrl Pts',(2.44573097835296,-1.18785489480888,
12.5311293540532));
#444611=CARTESIAN_POINT('Ctrl Pts',(2.44149642401639,-1.20376150708586,
12.5278936106989));
#444612=CARTESIAN_POINT('Ctrl Pts',(2.48175185926909,-1.19054008607023,
12.5204817579905));
#444613=CARTESIAN_POINT('Ctrl Pts',(2.47034185348555,-1.18968952253476,
12.5081597038247));
#444614=CARTESIAN_POINT('Ctrl Pts',(2.46614076809843,-1.20564680696742,
12.5049254088044));
#444615=CARTESIAN_POINT('Ctrl Pts',(2.46401737086259,-1.18921806139777,
12.5369868989719));
#444616=CARTESIAN_POINT('Ctrl Pts',(2.46494629818181,-1.18928730882606,
12.5342545179733));
#444617=CARTESIAN_POINT('Ctrl Pts',(2.46582355050076,-1.18947779631193,
12.5314872231885));
#444618=CARTESIAN_POINT('Ctrl Pts',(2.46658784886818,-1.18983342127685,
12.5287124745063));
#444619=CARTESIAN_POINT('Ctrl Pts',(2.46727713107232,-1.19015414152186,
12.5262100684184));
#444620=CARTESIAN_POINT('Ctrl Pts',(2.4678734336879,-1.19060974170665,12.5237004536639));
#444621=CARTESIAN_POINT('Ctrl Pts',(2.46834674938458,-1.19126072006474,
12.5212220730815));
#444622=CARTESIAN_POINT('Ctrl Pts',(2.46870911349547,-1.19175910031199,
12.5193246583486));
#444623=CARTESIAN_POINT('Ctrl Pts',(2.46900320969055,-1.19237832567575,
12.517417831369));
#444624=CARTESIAN_POINT('Ctrl Pts',(2.46915116612845,-1.1931766198546,12.5155812248347));
#444625=CARTESIAN_POINT('Ctrl Pts',(2.46921419636627,-1.19351669746564,
12.5147988205793));
#444626=CARTESIAN_POINT('Ctrl Pts',(2.46925104144563,-1.19388956733148,
12.5140295443047));
#444627=CARTESIAN_POINT('Ctrl Pts',(2.46925762714412,-1.19430058969269,
12.5132817086137));
#444628=CARTESIAN_POINT('Ctrl Pts',(2.46926759370789,-1.19492261643452,
12.5121499604604));
#444629=CARTESIAN_POINT('Ctrl Pts',(2.46920132248057,-1.19564556957359,
12.5110494206568));
#444630=CARTESIAN_POINT('Ctrl Pts',(2.46902260630554,-1.19647816349771,
12.5100666561695));
#444631=CARTESIAN_POINT('Ctrl Pts',(2.46891998788939,-1.19695623701165,
12.5095023550641));
#444632=CARTESIAN_POINT('Ctrl Pts',(2.46877847216687,-1.19747584612982,
12.5089719619137));
#444633=CARTESIAN_POINT('Ctrl Pts',(2.46859454917871,-1.19802557299053,
12.5085043804652));
#444634=CARTESIAN_POINT('Ctrl Pts',(2.46832540184319,-1.1988300266442,12.5078201359221));
#444635=CARTESIAN_POINT('Ctrl Pts',(2.46795648986139,-1.19972192459933,
12.5072563000949));
#444636=CARTESIAN_POINT('Ctrl Pts',(2.46750499683539,-1.2006375734588,12.5068768744332));
#444637=CARTESIAN_POINT('Ctrl Pts',(2.46717943928276,-1.20129781931997,
12.5066032824114));
#444638=CARTESIAN_POINT('Ctrl Pts',(2.46680527882823,-1.20198204031858,
12.5064197834844));
#444639=CARTESIAN_POINT('Ctrl Pts',(2.46640567747417,-1.20265326796633,
12.5063282718343));
#444640=CARTESIAN_POINT('Ctrl Pts',(2.46582238321068,-1.20363305252523,
12.5061946931565));
#444641=CARTESIAN_POINT('Ctrl Pts',(2.46517332759782,-1.20460663728856,
12.5062515701262));
#444642=CARTESIAN_POINT('Ctrl Pts',(2.46451165944249,-1.20552217804185,
12.5064436508398));
#444643=CARTESIAN_POINT('',(2.39213937462264,-1.19998227750565,12.5737548217797));
#444644=CARTESIAN_POINT('Origin',(2.40604428726529,-1.20695747674297,12.5893111709658));
#444645=CARTESIAN_POINT('Ctrl Pts',(2.46451165944249,-1.20552217804185,
12.5064436508398));
#444646=CARTESIAN_POINT('Ctrl Pts',(2.45379864434455,-1.20470260787252,
12.5164271754438));
#444647=CARTESIAN_POINT('Ctrl Pts',(2.44308139854736,-1.20388250449884,
12.5264061185523));
#444648=CARTESIAN_POINT('Ctrl Pts',(2.43235977297705,-1.20306185008553,
12.536380305637));
#444649=CARTESIAN_POINT('Ctrl Pts',(2.41895991559413,-1.20203619851555,
12.5488460165097));
#444650=CARTESIAN_POINT('Ctrl Pts',(2.40555321307975,-1.20100968589834,
12.5613043021964));
#444651=CARTESIAN_POINT('Ctrl Pts',(2.39213937462264,-1.19998227750565,
12.5737548217797));
#444652=CARTESIAN_POINT('Ctrl Pts',(2.37898422350637,-1.2416216516267,12.5893111709658));
#444653=CARTESIAN_POINT('Ctrl Pts',(2.37162385426224,-1.23300285825699,
12.5770542771492));
#444654=CARTESIAN_POINT('Ctrl Pts',(2.3818686866249,-1.22024170295209,12.5737548217797));
#444655=CARTESIAN_POINT('Ctrl Pts',(2.37211706301871,-1.23358039237507,
12.5928319619712));
#444656=CARTESIAN_POINT('Ctrl Pts',(2.369647757252,-1.2256724251646,12.5821634970843));
#444657=CARTESIAN_POINT('Ctrl Pts',(2.3793599685979,-1.21731859651707,12.5773203894503));
#444658=CARTESIAN_POINT('Ctrl Pts',(2.3675433841839,-1.21746625072075,12.5969440695591));
#444659=CARTESIAN_POINT('Ctrl Pts',(2.36934469270774,-1.21387266892067,
12.5878292599214));
#444660=CARTESIAN_POINT('Ctrl Pts',(2.37773178436604,-1.21157462896802,
12.5813877129824));
#444661=CARTESIAN_POINT('Ctrl Pts',(2.38133036145532,-1.19015152020297,
12.596957478804));
#444662=CARTESIAN_POINT('Ctrl Pts',(2.37954243674436,-1.19371858038985,
12.5878468778671));
#444663=CARTESIAN_POINT('Ctrl Pts',(2.3826716598646,-1.20180099615504,12.5814011370086));
#444664=CARTESIAN_POINT('Ctrl Pts',(2.39711921065734,-1.18423111075633,
12.5928371701607));
#444665=CARTESIAN_POINT('Ctrl Pts',(2.38928857035522,-1.18691739781518,
12.5821692192952));
#444666=CARTESIAN_POINT('Ctrl Pts',(2.38828644232307,-1.19968530920957,
12.5773318885715));
#444667=CARTESIAN_POINT('Ctrl Pts',(2.40767974839162,-1.18501835034955,
12.5893111709658));
#444668=CARTESIAN_POINT('Ctrl Pts',(2.39637714990395,-1.18417579353476,
12.5770542771492));
#444669=CARTESIAN_POINT('Ctrl Pts',(2.39213937462264,-1.19998227750559,
12.5737548217797));
#444670=CARTESIAN_POINT('',(2.3818686866249,-1.22024170295209,12.5737548217797));
#444671=CARTESIAN_POINT('Origin',(2.3957138983066,-1.22733466520273,12.5893111709658));
#444672=CARTESIAN_POINT('Ctrl Pts',(2.39213937462264,-1.19998227750559,
12.5737548217797));
#444673=CARTESIAN_POINT('Ctrl Pts',(2.39114295163672,-1.19987522208008,
12.5746934679442));
#444674=CARTESIAN_POINT('Ctrl Pts',(2.39002077460124,-1.19993889420315,
12.5756680099006));
#444675=CARTESIAN_POINT('Ctrl Pts',(2.38890032675292,-1.20016272513749,
12.5765688348656));
#444676=CARTESIAN_POINT('Ctrl Pts',(2.38860370058883,-1.20022198189947,
12.5768073183026));
#444677=CARTESIAN_POINT('Ctrl Pts',(2.38830720812578,-1.2002922068918,12.5770407398754));
#444678=CARTESIAN_POINT('Ctrl Pts',(2.38801309995349,-1.20037265268661,
12.5772674179684));
#444679=CARTESIAN_POINT('Ctrl Pts',(2.38680615954468,-1.20070278047506,
12.5781976435658));
#444680=CARTESIAN_POINT('Ctrl Pts',(2.38557379676062,-1.20123466340508,
12.5790594849312));
#444681=CARTESIAN_POINT('Ctrl Pts',(2.38441835795147,-1.20197672396998,
12.5797571720116));
#444682=CARTESIAN_POINT('Ctrl Pts',(2.38366554802143,-1.20246020311013,
12.580211740231));
#444683=CARTESIAN_POINT('Ctrl Pts',(2.3829213254678,-1.20307066995689,12.5806009430798));
#444684=CARTESIAN_POINT('Ctrl Pts',(2.3822493163659,-1.20377884820513,12.5808812374708));
#444685=CARTESIAN_POINT('Ctrl Pts',(2.38167183761066,-1.20438740825606,
12.5811221033394));
#444686=CARTESIAN_POINT('Ctrl Pts',(2.3811359452147,-1.20508066080214,12.581287365893));
#444687=CARTESIAN_POINT('Ctrl Pts',(2.38067848261986,-1.20582457696527,
12.581359338449));
#444688=CARTESIAN_POINT('Ctrl Pts',(2.38061490476542,-1.20592796595066,
12.5813693411482));
#444689=CARTESIAN_POINT('Ctrl Pts',(2.38055278326015,-1.20603232094451,
12.5813775999465));
#444690=CARTESIAN_POINT('Ctrl Pts',(2.38049215681373,-1.20613753878369,
12.5813841266931));
#444691=CARTESIAN_POINT('Ctrl Pts',(2.38038929671477,-1.20631605357368,
12.5813952001081));
#444692=CARTESIAN_POINT('Ctrl Pts',(2.38029057882966,-1.2064985516703,12.5814007534795));
#444693=CARTESIAN_POINT('Ctrl Pts',(2.38019621961205,-1.20668504741797,
12.5814005856065));
#444694=CARTESIAN_POINT('Ctrl Pts',(2.37976428000589,-1.20753875203569,
12.5813998171494));
#444695=CARTESIAN_POINT('Ctrl Pts',(2.37945321667912,-1.20841708864965,
12.58127954464));
#444696=CARTESIAN_POINT('Ctrl Pts',(2.37923690376943,-1.20930519271575,
12.5810700125799));
#444697=CARTESIAN_POINT('Ctrl Pts',(2.37897562240372,-1.21037792130886,
12.5808169217085));
#444698=CARTESIAN_POINT('Ctrl Pts',(2.37886881785461,-1.21146895803957,
12.5804173076348));
#444699=CARTESIAN_POINT('Ctrl Pts',(2.3788999318217,-1.2124801490644,12.5799304713245));
#444700=CARTESIAN_POINT('Ctrl Pts',(2.37893849182884,-1.21373333330219,
12.5793271277669));
#444701=CARTESIAN_POINT('Ctrl Pts',(2.37915908797786,-1.21494261000644,
12.5785808224116));
#444702=CARTESIAN_POINT('Ctrl Pts',(2.37952121976358,-1.21606269769621,
12.5777485681082));
#444703=CARTESIAN_POINT('Ctrl Pts',(2.3800608357988,-1.21773175106873,12.576508418016));
#444704=CARTESIAN_POINT('Ctrl Pts',(2.38090363862131,-1.21919082711649,
12.5750928681475));
#444705=CARTESIAN_POINT('Ctrl Pts',(2.3818686866249,-1.22024170295209,12.5737548217797));
#444706=CARTESIAN_POINT('Ctrl Pts',(2.3818686866249,-1.22024170295209,12.5737548217797));
#444707=CARTESIAN_POINT('Ctrl Pts',(2.37162385426224,-1.23300285825699,
12.5770542771492));
#444708=CARTESIAN_POINT('Ctrl Pts',(2.37898422350637,-1.2416216516267,12.5893111709658));
#444709=CARTESIAN_POINT('Ctrl Pts',(2.39798578380574,-1.239036759021,12.5508408821982));
#444710=CARTESIAN_POINT('Ctrl Pts',(2.38770670367268,-1.25183544005648,
12.55409748406));
#444711=CARTESIAN_POINT('Ctrl Pts',(2.39507646286288,-1.26046522879915,
12.5663972313419));
#444712=CARTESIAN_POINT('Ctrl Pts',(2.41408624122604,-1.25781422249849,
12.52790050457));
#444713=CARTESIAN_POINT('Ctrl Pts',(2.40375875059848,-1.27063195297933,
12.5311362602938));
#444714=CARTESIAN_POINT('Ctrl Pts',(2.4111524677942,-1.27928979589865,12.5434568539655));
#444715=CARTESIAN_POINT('Ctrl Pts',(2.4301713414965,-1.27657546956914,12.5049357605811));
#444716=CARTESIAN_POINT('Ctrl Pts',(2.41978320604121,-1.28939615702153,
12.5081700652078));
#444717=CARTESIAN_POINT('Ctrl Pts',(2.42721350978378,-1.29809684179795,
12.5204921097672));
#444718=CARTESIAN_POINT('Ctrl Pts',(2.42911512955617,-1.27534353357769,
12.5064436508395));
#444719=CARTESIAN_POINT('Ctrl Pts',(2.42873988909907,-1.27650458585469,
12.5062361689309));
#444720=CARTESIAN_POINT('Ctrl Pts',(2.42830015988261,-1.27769598412422,
12.5061871075061));
#444721=CARTESIAN_POINT('Ctrl Pts',(2.42781039043223,-1.27882343369142,
12.5063648335164));
#444722=CARTESIAN_POINT('Ctrl Pts',(2.42758790693764,-1.27933559082882,
12.5064455676329));
#444723=CARTESIAN_POINT('Ctrl Pts',(2.42735179220316,-1.27984160766237,
12.506574497099));
#444724=CARTESIAN_POINT('Ctrl Pts',(2.42711121774885,-1.28031934331772,
12.5067492519495));
#444725=CARTESIAN_POINT('Ctrl Pts',(2.42662777404454,-1.28127937166144,
12.5071004286051));
#444726=CARTESIAN_POINT('Ctrl Pts',(2.42610782456531,-1.28216012696854,
12.5076537929612));
#444727=CARTESIAN_POINT('Ctrl Pts',(2.42559853928645,-1.28290031231761,
12.5083435010503));
#444728=CARTESIAN_POINT('Ctrl Pts',(2.42556647673458,-1.28294691140879,
12.5083869222963));
#444729=CARTESIAN_POINT('Ctrl Pts',(2.42553444312098,-1.28299295167391,
12.5084308732336));
#444730=CARTESIAN_POINT('Ctrl Pts',(2.42550244473866,-1.28303841752479,
12.5084753333615));
#444731=CARTESIAN_POINT('Ctrl Pts',(2.42524577547887,-1.28340311365768,
12.508831962269));
#444732=CARTESIAN_POINT('Ctrl Pts',(2.42498721724232,-1.28373899750251,
12.509227847131));
#444733=CARTESIAN_POINT('Ctrl Pts',(2.42473667710823,-1.28403778947644,
12.5096423454524));
#444734=CARTESIAN_POINT('Ctrl Pts',(2.42395159521243,-1.28497407128295,
12.5109411997424));
#444735=CARTESIAN_POINT('Ctrl Pts',(2.42320436570342,-1.28560994088479,
12.5124831113042));
#444736=CARTESIAN_POINT('Ctrl Pts',(2.4225221935559,-1.28603603903853,12.5140723025008));
#444737=CARTESIAN_POINT('Ctrl Pts',(2.42245827327851,-1.28607596490223,
12.5142212114565));
#444738=CARTESIAN_POINT('Ctrl Pts',(2.42239492219652,-1.28611407853466,
12.5143705582413));
#444739=CARTESIAN_POINT('Ctrl Pts',(2.42233216309062,-1.28615047148243,
12.5145201959299));
#444740=CARTESIAN_POINT('Ctrl Pts',(2.42152592893674,-1.28661799308,12.5164425148273));
#444741=CARTESIAN_POINT('Ctrl Pts',(2.42079515218195,-1.28682685455088,
12.5184635205941));
#444742=CARTESIAN_POINT('Ctrl Pts',(2.42011704784669,-1.28686434176596,
12.5205025929158));
#444743=CARTESIAN_POINT('Ctrl Pts',(2.4197237204547,-1.28688608583656,12.5216853356836));
#444744=CARTESIAN_POINT('Ctrl Pts',(2.41934885168665,-1.28685061526725,
12.5228750347131));
#444745=CARTESIAN_POINT('Ctrl Pts',(2.41899380360422,-1.2867761256189,12.5240609649613));
#444746=CARTESIAN_POINT('Ctrl Pts',(2.41812235713356,-1.28659329477327,
12.5269717671326));
#444747=CARTESIAN_POINT('Ctrl Pts',(2.41734792509633,-1.28616008119099,
12.5299036066169));
#444748=CARTESIAN_POINT('Ctrl Pts',(2.41664091150253,-1.28555793178732,
12.5328133004019));
#444749=CARTESIAN_POINT('Ctrl Pts',(2.41630150380934,-1.28526886501145,
12.5342101228451));
#444750=CARTESIAN_POINT('Ctrl Pts',(2.41597839638607,-1.28494082766648,
12.5356023438238));
#444751=CARTESIAN_POINT('Ctrl Pts',(2.41567186698724,-1.28458189015479,
12.5369868989719));
#444752=CARTESIAN_POINT('Origin',(10.6884466934502,-10.9799334864268,-1.23984329704211));
#444753=CARTESIAN_POINT('Ctrl Pts',(2.46397569520746,-1.18921491485979,
12.5369868989719));
#444754=CARTESIAN_POINT('Ctrl Pts',(2.47927000605091,-1.19038425634496,
12.5369868989719));
#444755=CARTESIAN_POINT('Ctrl Pts',(2.48565574447584,-1.17643772815858,
12.5369868989719));
#444756=CARTESIAN_POINT('Ctrl Pts',(2.46914577547705,-1.1896101319952,12.5218025310015));
#444757=CARTESIAN_POINT('Ctrl Pts',(2.48070827525023,-1.18716790704654,
12.5216901060418));
#444758=CARTESIAN_POINT('Ctrl Pts',(2.48563629362352,-1.17648024866413,
12.5161920673677));
#444759=CARTESIAN_POINT('Ctrl Pts',(2.47227858317585,-1.19476004336506,
12.5042015548895));
#444760=CARTESIAN_POINT('Ctrl Pts',(2.47821564607589,-1.19228443654281,
12.4980677368513));
#444761=CARTESIAN_POINT('Ctrl Pts',(2.48115665620399,-1.18615734594856,
12.4907278922778));
#444762=CARTESIAN_POINT('Ctrl Pts',(2.46449369264775,-1.20551338954989,
12.506463626192));
#444763=CARTESIAN_POINT('Ctrl Pts',(2.47037097577434,-1.20838827761489,
12.4999376786891));
#444764=CARTESIAN_POINT('Ctrl Pts',(2.47029919330651,-1.20835316503726,
12.4906970594712));
#444765=CARTESIAN_POINT('Origin',(2.46565283198893,-1.1672789350044,12.5369868989719));
#444766=CARTESIAN_POINT('Origin',(2.46565283198893,-1.1672789350044,14.));
#444767=CARTESIAN_POINT('Origin',(2.46565283198893,-1.1672789350044,13.7435492065112));
#444768=CARTESIAN_POINT('Ctrl Pts',(2.43932577967014,-1.18737738943337,
13.793642941384));
#444769=CARTESIAN_POINT('Ctrl Pts',(2.45010612228422,-1.18820831188987,
13.8071662555867));
#444770=CARTESIAN_POINT('Ctrl Pts',(2.45389707400936,-1.17160565943152,
13.8103758687955));
#444771=CARTESIAN_POINT('Ctrl Pts',(2.4559009113622,-1.18861299236844,13.7804579775006));
#444772=CARTESIAN_POINT('Ctrl Pts',(2.46920365907604,-1.18962816476343,
13.7901904343352));
#444773=CARTESIAN_POINT('Ctrl Pts',(2.47515012965678,-1.17503722881686,
13.7927914348262));
#444774=CARTESIAN_POINT('Ctrl Pts',(2.46565931518457,-1.18934043827937,
13.7597120340895));
#444775=CARTESIAN_POINT('Ctrl Pts',(2.48105477662738,-1.1905095648489,13.7635825532445));
#444776=CARTESIAN_POINT('Ctrl Pts',(2.48768710685466,-1.17703558578182,
13.7651073818884));
#444777=CARTESIAN_POINT('Ctrl Pts',(2.46374839627415,-1.18919798771258,
13.7381884353898));
#444778=CARTESIAN_POINT('Ctrl Pts',(2.47878343019723,-1.19034064494829,
13.7368803041982));
#444779=CARTESIAN_POINT('Ctrl Pts',(2.48523207198161,-1.17664376003763,
13.7363986145813));
#444780=CARTESIAN_POINT('Origin',(2.44498316494277,-1.16573810624294,13.7902182540695));
#444781=CARTESIAN_POINT('Ctrl Pts',(2.40767582314102,-1.18501805697917,
13.8235227101244));
#444782=CARTESIAN_POINT('Ctrl Pts',(2.41914075354885,-1.1858771606184,13.8358800583119));
#444783=CARTESIAN_POINT('Ctrl Pts',(2.42332459279512,-1.1698421508517,13.8390832900376));
#444784=CARTESIAN_POINT('Ctrl Pts',(2.41957039909833,-1.1859047429948,13.8124254819052));
#444785=CARTESIAN_POINT('Ctrl Pts',(2.43105759425929,-1.18676551472373,
13.8247886449157));
#444786=CARTESIAN_POINT('Ctrl Pts',(2.43523022781489,-1.17070594093384,
13.8279860620657));
#444787=CARTESIAN_POINT('Ctrl Pts',(2.43145964429365,-1.18679103162661,
13.8013225099955));
#444788=CARTESIAN_POINT('Ctrl Pts',(2.44296368394646,-1.18765306729825,
13.8136962257787));
#444789=CARTESIAN_POINT('Ctrl Pts',(2.44713033149677,-1.17156960146922,
13.8168830918626));
#444790=CARTESIAN_POINT('Ctrl Pts',(2.44334376613877,-1.18767693833621,
13.7902140179785));
#444791=CARTESIAN_POINT('Ctrl Pts',(2.45485958427629,-1.1885398602146,13.802602731458));
#444792=CARTESIAN_POINT('Ctrl Pts',(2.45902512104727,-1.1724331393835,13.8057746032558));
#444793=CARTESIAN_POINT('Origin',(2.40931520951795,-1.16307922395623,13.8235269408515));
#444794=CARTESIAN_POINT('Ctrl Pts',(2.37898422350637,-1.2416216516267,13.8235269408515));
#444795=CARTESIAN_POINT('Ctrl Pts',(2.38665210203091,-1.25060053004909,
13.8362179249168));
#444796=CARTESIAN_POINT('Ctrl Pts',(2.37563004038642,-1.26364572691086,
13.8391868794938));
#444797=CARTESIAN_POINT('Ctrl Pts',(2.37196844841931,-1.23340636869753,
13.8400110824519));
#444798=CARTESIAN_POINT('Ctrl Pts',(2.37551474770213,-1.24282685829509,
13.8494522556836));
#444799=CARTESIAN_POINT('Ctrl Pts',(2.36416949587685,-1.25005272491833,
13.85569149686));
#444800=CARTESIAN_POINT('Ctrl Pts',(2.36738733885893,-1.21777271393477,
13.8586819406588));
#444801=CARTESIAN_POINT('Ctrl Pts',(2.36543106360686,-1.22166231941259,
13.868010383617));
#444802=CARTESIAN_POINT('Ctrl Pts',(2.3567048712968,-1.22405949161342,13.8744918421245));
#444803=CARTESIAN_POINT('Ctrl Pts',(2.38148881035118,-1.18984029549848,
13.8587686893867));
#444804=CARTESIAN_POINT('Ctrl Pts',(2.38342762446751,-1.18598528217267,
13.8680909899357));
#444805=CARTESIAN_POINT('Ctrl Pts',(2.38018197705652,-1.17756137723557,
13.8745789365163));
#444806=CARTESIAN_POINT('Ctrl Pts',(2.39688877846764,-1.18421393308822,
13.8400379222776));
#444807=CARTESIAN_POINT('Ctrl Pts',(2.40657921166029,-1.18149994369126,
13.8494748685452));
#444808=CARTESIAN_POINT('Ctrl Pts',(2.40570324688965,-1.16808376722457,
13.8557104837033));
#444809=CARTESIAN_POINT('Ctrl Pts',(2.40767974839197,-1.185018350343,13.8235269408542));
#444810=CARTESIAN_POINT('Ctrl Pts',(2.4194545587772,-1.18589610838626,13.8362179249195));
#444811=CARTESIAN_POINT('Ctrl Pts',(2.4234620398536,-1.16929481025995,13.8391868794965));
#444812=CARTESIAN_POINT('Origin',(2.36225454870615,-1.25590863805067,13.8235269408515));
#444813=CARTESIAN_POINT('Ctrl Pts',(2.40220900451924,-1.26881724339398,
13.7902140241683));
#444814=CARTESIAN_POINT('Ctrl Pts',(2.4097118226441,-1.27759598564887,13.8026027327198));
#444815=CARTESIAN_POINT('Ctrl Pts',(2.39918212096335,-1.29047633171518,
13.8057746032556));
#444816=CARTESIAN_POINT('Ctrl Pts',(2.39446994123773,-1.25975500954427,
13.8013225161808));
#444817=CARTESIAN_POINT('Ctrl Pts',(2.40196508250914,-1.2685247749463,13.8136962270464));
#444818=CARTESIAN_POINT('Ctrl Pts',(2.39145479514589,-1.2813922713949,13.8168830918628));
#444819=CARTESIAN_POINT('Ctrl Pts',(2.3867275415764,-1.25068886888398,13.8124254880875));
#444820=CARTESIAN_POINT('Ctrl Pts',(2.39421170688976,-1.25944579440626,
13.8247886461867));
#444821=CARTESIAN_POINT('Ctrl Pts',(2.38372422933855,-1.27230399711159,
13.8279860620656));
#444822=CARTESIAN_POINT('Ctrl Pts',(2.37898167046557,-1.24161866325018,
13.8235227163066));
#444823=CARTESIAN_POINT('Ctrl Pts',(2.38645133002003,-1.25035861573159,
13.8358800595847));
#444824=CARTESIAN_POINT('Ctrl Pts',(2.37599028956742,-1.2632113377564,13.8390832900376));
#444825=CARTESIAN_POINT('Origin',(2.38548189084313,-1.28310722765479,13.7902182540695));
#444826=CARTESIAN_POINT('Ctrl Pts',(2.41549659670382,-1.28437669586829,
13.7382347919292));
#444827=CARTESIAN_POINT('Ctrl Pts',(2.42531461917976,-1.29583637751289,
13.7369371795942));
#444828=CARTESIAN_POINT('Ctrl Pts',(2.41806535003366,-1.30914020680628,
13.7364597369711));
#444829=CARTESIAN_POINT('Ctrl Pts',(2.41672499120129,-1.28581511199128,
13.7595490285574));
#444830=CARTESIAN_POINT('Ctrl Pts',(2.42677649975199,-1.2975488659632,13.7633824266926));
#444831=CARTESIAN_POINT('Ctrl Pts',(2.4198111407926,-1.31086717797616,13.7648920890506));
#444832=CARTESIAN_POINT('Ctrl Pts',(2.41046024656722,-1.27847926856174,
13.780380659011));
#444833=CARTESIAN_POINT('Ctrl Pts',(2.41915854154762,-1.28862503370973,
13.7901039518744));
#444834=CARTESIAN_POINT('Ctrl Pts',(2.41091351991637,-1.30206025085443,
13.7926933640891));
#444835=CARTESIAN_POINT('Ctrl Pts',(2.39957072186774,-1.2657279351651,13.7936647693663));
#444836=CARTESIAN_POINT('Ctrl Pts',(2.4066171141417,-1.27393291462065,13.8072068914933));
#444837=CARTESIAN_POINT('Ctrl Pts',(2.39544599080463,-1.2868112015112,13.8104111085397));
#444838=CARTESIAN_POINT('Origin',(2.39894219218701,-1.29886887657876,13.7435492065112));
#444839=CARTESIAN_POINT('Origin',(2.39894219218701,-1.29886887657876,14.));
#444840=CARTESIAN_POINT('Origin',(2.39894219218701,-1.29886887657876,12.5369868989719));
#444841=CARTESIAN_POINT('Ctrl Pts',(2.42909885324192,-1.27533498811183,
12.506462012331));
#444842=CARTESIAN_POINT('Ctrl Pts',(2.43488807916769,-1.27837447016805,
12.4999388158272));
#444843=CARTESIAN_POINT('Ctrl Pts',(2.43481958503289,-1.27833850910929,
12.4907030323752));
#444844=CARTESIAN_POINT('Ctrl Pts',(2.42502478319153,-1.28796948597993,
12.5042014951932));
#444845=CARTESIAN_POINT('Ctrl Pts',(2.4265374804497,-1.2942187134619,12.4980716682128));
#444846=CARTESIAN_POINT('Ctrl Pts',(2.42333731702239,-1.30020908233739,
12.4907355092744));
#444847=CARTESIAN_POINT('Ctrl Pts',(2.41902011774416,-1.28848880679608,
12.5218047446509));
#444848=CARTESIAN_POINT('Ctrl Pts',(2.42388115369431,-1.29925399144045,
12.5216906929433));
#444849=CARTESIAN_POINT('Ctrl Pts',(2.41817937641594,-1.30954284415575,
12.5161988840775));
#444850=CARTESIAN_POINT('Ctrl Pts',(2.41564689373247,-1.28455269879707,
12.5369868989719));
#444851=CARTESIAN_POINT('Ctrl Pts',(2.4256225952112,-1.29619275513402,12.5369868989719));
#444852=CARTESIAN_POINT('Ctrl Pts',(2.41815742309716,-1.30958218144093,
12.5369868989719));
#444853=CARTESIAN_POINT('Origin',(4.59510497263918E-31,-7.48139013969497E-31,
12.5));
#444854=CARTESIAN_POINT('Origin',(2.47227204101565,-1.04358095837972,12.5));
#444855=CARTESIAN_POINT('',(2.47227204101565,-1.04358095837972,12.5893111709658));
#444856=CARTESIAN_POINT('',(2.47227204101565,-1.04358095837972,13.8235269408515));
#444857=CARTESIAN_POINT('',(2.47227204101565,-1.04358095837972,12.5));
#444858=CARTESIAN_POINT('',(2.49763903363991,-1.06879580290437,13.7902182540695));
#444859=CARTESIAN_POINT('',(2.47227204101565,-1.04358095837972,13.8235269408515));
#444860=CARTESIAN_POINT('',(2.51233926765279,-1.08340786672292,13.7435492065112));
#444861=CARTESIAN_POINT('Origin',(2.46397592170674,-1.03533413886561,13.7445212918693));
#444862=CARTESIAN_POINT('',(2.51233926765279,-1.08340786672292,12.5369868989719));
#444863=CARTESIAN_POINT('',(2.51233926765279,-1.08340786672292,12.5));
#444864=CARTESIAN_POINT('Ctrl Pts',(2.51233926765279,-1.08340786672292,
12.5369868989719));
#444865=CARTESIAN_POINT('Ctrl Pts',(2.49899326630647,-1.07014191305006,
12.5544431401645));
#444866=CARTESIAN_POINT('Ctrl Pts',(2.48563771954526,-1.05686647121454,
12.5718848856037));
#444867=CARTESIAN_POINT('Ctrl Pts',(2.47227204101565,-1.04358095837972,
12.5893111709658));
#444868=CARTESIAN_POINT('Origin',(2.77125127718585,-0.982849258123515,12.5));
#444869=CARTESIAN_POINT('',(2.55275086849393,-0.984420745855523,13.7435492065112));
#444870=CARTESIAN_POINT('',(2.53202438621133,-0.984569813826745,13.7902182540695));
#444871=CARTESIAN_POINT('Origin',(2.47755877302977,-0.984961538690983,13.7418732680449));
#444872=CARTESIAN_POINT('',(2.49625838937557,-0.984827048243774,13.8235269408515));
#444873=CARTESIAN_POINT('',(2.53202438621133,-0.984569813826745,13.7902182540695));
#444874=CARTESIAN_POINT('',(2.49625838937557,-0.984827048243774,12.5893111709658));
#444875=CARTESIAN_POINT('',(2.49625838937557,-0.984827048243774,12.5));
#444876=CARTESIAN_POINT('',(2.55275086849393,-0.984420745855523,12.5369868989719));
#444877=CARTESIAN_POINT('Ctrl Pts',(2.49625838937557,-0.984827048243774,
12.5893111709658));
#444878=CARTESIAN_POINT('Ctrl Pts',(2.51510322538268,-0.984691513354965,
12.5718848856037));
#444879=CARTESIAN_POINT('Ctrl Pts',(2.53393377618058,-0.984556081207524,
12.5544431401645));
#444880=CARTESIAN_POINT('Ctrl Pts',(2.55275086849393,-0.984420745855523,
12.5369868989719));
#444881=CARTESIAN_POINT('',(2.55275086849393,-0.984420745855523,12.5));
#444882=CARTESIAN_POINT('Origin',(2.4965056131406,-1.01920115922006,12.5));
#444883=CARTESIAN_POINT('',(2.46427499032543,-1.0072522209775,13.8587068136939));
#444884=CARTESIAN_POINT('Ctrl Pts',(2.49625838937537,-0.984827048237167,
13.8235269408542));
#444885=CARTESIAN_POINT('Ctrl Pts',(2.49450613636711,-0.984839650703789,
13.8262006681044));
#444886=CARTESIAN_POINT('Ctrl Pts',(2.49271421095855,-0.985026282325426,
13.8288634856214));
#444887=CARTESIAN_POINT('Ctrl Pts',(2.49088698306019,-0.98537434508912,
13.8314912288862));
#444888=CARTESIAN_POINT('Ctrl Pts',(2.4890032995668,-0.985733161897478,
13.8342001611531));
#444889=CARTESIAN_POINT('Ctrl Pts',(2.48707991312608,-0.986263449831712,
13.8368750301949));
#444890=CARTESIAN_POINT('Ctrl Pts',(2.48510989497275,-0.986995062839595,
13.8394886372969));
#444891=CARTESIAN_POINT('Ctrl Pts',(2.48495774569217,-0.987051567086838,
13.8396904925131));
#444892=CARTESIAN_POINT('Ctrl Pts',(2.48480532227872,-0.987109293988284,
13.8398919674349));
#444893=CARTESIAN_POINT('Ctrl Pts',(2.48465262459692,-0.987168268325339,
13.8400930404591));
#444894=CARTESIAN_POINT('Ctrl Pts',(2.48227349198451,-0.988087128172655,
13.8432258934518));
#444895=CARTESIAN_POINT('Ctrl Pts',(2.4798395130573,-0.989303073675097,
13.8462331177034));
#444896=CARTESIAN_POINT('Ctrl Pts',(2.47747318253686,-0.990862744111962,
13.8489036603661));
#444897=CARTESIAN_POINT('Ctrl Pts',(2.4766988916522,-0.9913730864297,13.8497774930041));
#444898=CARTESIAN_POINT('Ctrl Pts',(2.47593209364871,-0.991920229736684,
13.85061494757));
#444899=CARTESIAN_POINT('Ctrl Pts',(2.47517779370455,-0.992505793840622,
13.8514076489583));
#444900=CARTESIAN_POINT('Ctrl Pts',(2.4735823405363,-0.993744346371441,
13.8530843267192));
#444901=CARTESIAN_POINT('Ctrl Pts',(2.4718878999805,-0.995278782199361,
13.8546805203176));
#444902=CARTESIAN_POINT('Ctrl Pts',(2.47028440497422,-0.997121181885222,
13.8559412814274));
#444903=CARTESIAN_POINT('Ctrl Pts',(2.47006980533981,-0.997367754713618,
13.8561100121513));
#444904=CARTESIAN_POINT('Ctrl Pts',(2.46985682318122,-0.997619767556806,
13.8562727473908));
#444905=CARTESIAN_POINT('Ctrl Pts',(2.46964589317334,-0.997877176378507,
13.8564289040185));
#444906=CARTESIAN_POINT('Ctrl Pts',(2.46868932799395,-0.999044522448343,
13.8571370725437));
#444907=CARTESIAN_POINT('Ctrl Pts',(2.46775991462844,-1.00034480439304,
13.8577210840553));
#444908=CARTESIAN_POINT('Ctrl Pts',(2.46691765545993,-1.00174454601251,
13.8581177131616));
#444909=CARTESIAN_POINT('Ctrl Pts',(2.46668044628841,-1.00213876143019,
13.8582294175695));
#444910=CARTESIAN_POINT('Ctrl Pts',(2.46645001871431,-1.00254074616991,
13.8583265086086));
#444911=CARTESIAN_POINT('Ctrl Pts',(2.46622737107116,-1.00294947629639,
13.8584082369006));
#444912=CARTESIAN_POINT('Ctrl Pts',(2.46590748611328,-1.00353671188281,
13.8585256585398));
#444913=CARTESIAN_POINT('Ctrl Pts',(2.46559996750226,-1.00414532668273,
13.8586122832068));
#444914=CARTESIAN_POINT('Ctrl Pts',(2.46531350850406,-1.00475986677822,
13.8586682984299));
#444915=CARTESIAN_POINT('Ctrl Pts',(2.46508436970126,-1.00525143793722,
13.8587131050557));
#444916=CARTESIAN_POINT('Ctrl Pts',(2.46486596234389,-1.00575213068633,
13.8587357943552));
#444917=CARTESIAN_POINT('Ctrl Pts',(2.4646587246829,-1.00626220701203,13.8587355499465));
#444918=CARTESIAN_POINT('Ctrl Pts',(2.4645247820418,-1.00659188150221,13.8587353919793));
#444919=CARTESIAN_POINT('Ctrl Pts',(2.46439691797788,-1.00692189622389,
13.8587257282814));
#444920=CARTESIAN_POINT('Ctrl Pts',(2.46427499032543,-1.0072522209775,13.8587068136939));
#444921=CARTESIAN_POINT('Ctrl Pts',(2.46427499032543,-1.0072522209775,13.8587068136939));
#444922=CARTESIAN_POINT('Ctrl Pts',(2.46387397692363,-1.00833864108392,
13.8586446046466));
#444923=CARTESIAN_POINT('Ctrl Pts',(2.46353709921336,-1.00942841144252,
13.858482427929));
#444924=CARTESIAN_POINT('Ctrl Pts',(2.46326000564278,-1.01052050738079,
13.8582284286032));
#444925=CARTESIAN_POINT('Ctrl Pts',(2.4629757398722,-1.01164087077572,13.8579678548414));
#444926=CARTESIAN_POINT('Ctrl Pts',(2.46275518338507,-1.01276679512489,
13.857615680862));
#444927=CARTESIAN_POINT('Ctrl Pts',(2.46259752251169,-1.0138520289967,13.8571944833187));
#444928=CARTESIAN_POINT('Ctrl Pts',(2.46220406367794,-1.0165603411124,13.8561433417727));
#444929=CARTESIAN_POINT('Ctrl Pts',(2.46217917029009,-1.01914122861999,
13.8546163505475));
#444930=CARTESIAN_POINT('Ctrl Pts',(2.46236829417935,-1.02145731346383,
13.8528973491086));
#444931=CARTESIAN_POINT('Ctrl Pts',(2.46240284432366,-1.02188042799416,
13.8525833129072));
#444932=CARTESIAN_POINT('Ctrl Pts',(2.46244441744383,-1.02229478029566,
13.8522628768812));
#444933=CARTESIAN_POINT('Ctrl Pts',(2.46249193666486,-1.02269965049313,
13.851937733538));
#444934=CARTESIAN_POINT('Ctrl Pts',(2.4627821299547,-1.02517213661585,13.8499521282529));
#444935=CARTESIAN_POINT('Ctrl Pts',(2.46332696587327,-1.02753624269018,
13.847639871647));
#444936=CARTESIAN_POINT('Ctrl Pts',(2.46401952132021,-1.02968576255045,
13.8452109780794));
#444937=CARTESIAN_POINT('Ctrl Pts',(2.46433111635098,-1.03065287602844,
13.8441181685877));
#444938=CARTESIAN_POINT('Ctrl Pts',(2.46467204914031,-1.03157699391933,
13.8430021611332));
#444939=CARTESIAN_POINT('Ctrl Pts',(2.46503073696772,-1.03245119022838,
13.8418824960098));
#444940=CARTESIAN_POINT('Ctrl Pts',(2.46587599399244,-1.03451125615405,
13.8392439765549));
#444941=CARTESIAN_POINT('Ctrl Pts',(2.4668567562043,-1.0363940125498,13.8364981347964));
#444942=CARTESIAN_POINT('Ctrl Pts',(2.46794526772955,-1.0381202482499,13.8336931113419));
#444943=CARTESIAN_POINT('Ctrl Pts',(2.46900540882826,-1.0398014921957,13.8309611966328));
#444944=CARTESIAN_POINT('Ctrl Pts',(2.47016929556687,-1.04133565176911,
13.8281701127186));
#444945=CARTESIAN_POINT('Ctrl Pts',(2.47143462492222,-1.0427103127463,13.8253580685121));
#444946=CARTESIAN_POINT('Ctrl Pts',(2.47170894969204,-1.04300834072974,
13.8247484142932));
#444947=CARTESIAN_POINT('Ctrl Pts',(2.47198808293421,-1.0432987034439,13.8241378483365));
#444948=CARTESIAN_POINT('Ctrl Pts',(2.47227204101566,-1.04358095837972,
13.8235269408515));
#444949=CARTESIAN_POINT('',(2.4647276862865,-1.00609556924708,12.5969504640361));
#444950=CARTESIAN_POINT('Origin',(2.49653617024153,-1.01921384568499,12.584524458991));
#444951=CARTESIAN_POINT('Origin',(2.49653617024153,-1.01921384568499,12.584524458991));
#444952=CARTESIAN_POINT('Ctrl Pts',(2.49625838937557,-0.984827048243774,
12.5893111709658));
#444953=CARTESIAN_POINT('Ctrl Pts',(2.48492472314964,-0.984908561672236,
12.5770542771492));
#444954=CARTESIAN_POINT('Ctrl Pts',(2.48198942389985,-1.00100786889861,
12.5737548217797));
#444955=CARTESIAN_POINT('Ctrl Pts',(2.52104131372023,-0.984648805732449,
12.5663937883685));
#444956=CARTESIAN_POINT('Ctrl Pts',(2.50969318982903,-0.9847304231426,12.5540940315304));
#444957=CARTESIAN_POINT('Ctrl Pts',(2.50675195379035,-1.00088019484002,
12.5508374392248));
#444958=CARTESIAN_POINT('Ctrl Pts',(2.54579923239804,-0.984470743065631,
12.5434499600945));
#444959=CARTESIAN_POINT('Ctrl Pts',(2.53441421171488,-0.984552625843129,
12.5311293540533));
#444960=CARTESIAN_POINT('Ctrl Pts',(2.53149028407887,-1.00075146567008,
12.5278936106989));
#444961=CARTESIAN_POINT('Ctrl Pts',(2.57053410413713,-0.984292846155857,
12.5204817579905));
#444962=CARTESIAN_POINT('Ctrl Pts',(2.55909273538219,-0.984375134197071,
12.5081597038247));
#444963=CARTESIAN_POINT('Ctrl Pts',(2.55620629558159,-1.00062174954219,
12.5049254088044));
#444964=CARTESIAN_POINT('Ctrl Pts',(2.55275086849393,-0.984420745855524,
12.5369868989719));
#444965=CARTESIAN_POINT('Ctrl Pts',(2.5536823491924,-0.984414046668457,
12.5342545179733));
#444966=CARTESIAN_POINT('Ctrl Pts',(2.55457220902511,-0.984532396114919,
12.5314872231885));
#444967=CARTESIAN_POINT('Ctrl Pts',(2.55536295098887,-0.984824540354759,
12.5287124745063));
#444968=CARTESIAN_POINT('Ctrl Pts',(2.55607608134073,-0.985088010530996,
12.5262100684185));
#444969=CARTESIAN_POINT('Ctrl Pts',(2.5567075354532,-0.985493490544782,
12.5237004536639));
#444970=CARTESIAN_POINT('Ctrl Pts',(2.55723233701052,-0.986103723202764,
12.5212220730815));
#444971=CARTESIAN_POINT('Ctrl Pts',(2.5576341180016,-0.986570909091784,
12.5193246583486));
#444972=CARTESIAN_POINT('Ctrl Pts',(2.55797770823161,-0.987164102464083,
12.517417831369));
#444973=CARTESIAN_POINT('Ctrl Pts',(2.55819024074325,-0.987947680561655,
12.5155812248347));
#444974=CARTESIAN_POINT('Ctrl Pts',(2.55828078073558,-0.98828148904297,
12.5147988205793));
#444975=CARTESIAN_POINT('Ctrl Pts',(2.55834789557159,-0.988650114999075,
12.5140295443047));
#444976=CARTESIAN_POINT('Ctrl Pts',(2.5583879614949,-0.989059232921712,
12.5132817086137));
#444977=CARTESIAN_POINT('Ctrl Pts',(2.55844859584983,-0.989678377553405,
12.5121499604604));
#444978=CARTESIAN_POINT('Ctrl Pts',(2.55844147252695,-0.990404326845799,
12.5110494206568));
#444979=CARTESIAN_POINT('Ctrl Pts',(2.55833121514949,-0.991248717409707,
12.5100666561695));
#444980=CARTESIAN_POINT('Ctrl Pts',(2.55826790561726,-0.991733564527043,
12.5095023550641));
#444981=CARTESIAN_POINT('Ctrl Pts',(2.55816921374356,-0.992262979533925,
12.5089719619137));
#444982=CARTESIAN_POINT('Ctrl Pts',(2.55803071058653,-0.992825868654841,
12.5085043804652));
#444983=CARTESIAN_POINT('Ctrl Pts',(2.55782802925753,-0.993649583561836,
12.5078201359221));
#444984=CARTESIAN_POINT('Ctrl Pts',(2.55753304276325,-0.99456858355139,
12.5072563000949));
#444985=CARTESIAN_POINT('Ctrl Pts',(2.55715768592557,-0.995517986537896,
12.5068768744332));
#444986=CARTESIAN_POINT('Ctrl Pts',(2.55688702780595,-0.996202571448291,
12.5066032824114));
#444987=CARTESIAN_POINT('Ctrl Pts',(2.55656988270285,-0.996915013308555,
12.5064197834844));
#444988=CARTESIAN_POINT('Ctrl Pts',(2.55622632227399,-0.997616578721758,
12.5063282718343));
#444989=CARTESIAN_POINT('Ctrl Pts',(2.55572483041147,-0.998640647025872,
12.5061946931565));
#444990=CARTESIAN_POINT('Ctrl Pts',(2.55515729067415,-0.999663896324203,
12.5062515701262));
#444991=CARTESIAN_POINT('Ctrl Pts',(2.55457244923589,-1.00063032278845,
12.5064436508398));
#444992=CARTESIAN_POINT('',(2.48198942389985,-1.00100786889861,12.5737548217797));
#444993=CARTESIAN_POINT('Origin',(2.49641661258519,-1.0068264792686,12.5893111709658));
#444994=CARTESIAN_POINT('Ctrl Pts',(2.55457244923589,-1.00063032278845,
12.5064436508398));
#444995=CARTESIAN_POINT('Ctrl Pts',(2.5438282782346,-1.00068668985652,12.5164271754438));
#444996=CARTESIAN_POINT('Ctrl Pts',(2.53307984715027,-1.00074287033569,
12.5264061185523));
#444997=CARTESIAN_POINT('Ctrl Pts',(2.5223270059513,-1.00079885860094,12.536380305637));
#444998=CARTESIAN_POINT('Ctrl Pts',(2.50888813536377,-1.00086883257686,
12.5488460165097));
#444999=CARTESIAN_POINT('Ctrl Pts',(2.49544237223805,-1.00093850631237,
12.5613043021964));
#445000=CARTESIAN_POINT('Ctrl Pts',(2.48198942389985,-1.00100786889861,
12.5737548217797));
#445001=CARTESIAN_POINT('Ctrl Pts',(2.47227204101565,-1.04358095837972,
12.5893111709658));
#445002=CARTESIAN_POINT('Ctrl Pts',(2.46423365112039,-1.03559078175768,
12.5770542771492));
#445003=CARTESIAN_POINT('Ctrl Pts',(2.47340424202237,-1.02203703919839,
12.5737548217797));
#445004=CARTESIAN_POINT('Ctrl Pts',(2.46477229315759,-1.03612619308624,
12.5928319619712));
#445005=CARTESIAN_POINT('Ctrl Pts',(2.46166663106047,-1.02844581032821,
12.5821634970842));
#445006=CARTESIAN_POINT('Ctrl Pts',(2.4706656112364,-1.0193281429679,12.5773203894503));
#445007=CARTESIAN_POINT('Ctrl Pts',(2.45890038072059,-1.02043846719395,
12.5969440695591));
#445008=CARTESIAN_POINT('Ctrl Pts',(2.46040278526102,-1.01671001937364,
12.5878292599214));
#445009=CARTESIAN_POINT('Ctrl Pts',(2.46857465797361,-1.01373600012724,
12.5813877129824));
#445010=CARTESIAN_POINT('Ctrl Pts',(2.4704150788477,-0.992090857548991,
12.596957478804));
#445011=CARTESIAN_POINT('Ctrl Pts',(2.46892385182892,-0.995791781099588,
12.5878468778671));
#445012=CARTESIAN_POINT('Ctrl Pts',(2.47270145463572,-1.00359224255848,
12.5814011370086));
#445013=CARTESIAN_POINT('Ctrl Pts',(2.48566882362419,-0.984903209989894,
12.5928371701607));
#445014=CARTESIAN_POINT('Ctrl Pts',(2.47808319646526,-0.988218828530895,
12.5821692192952));
#445015=CARTESIAN_POINT('Ctrl Pts',(2.47812510624161,-1.00102593849133,
12.5773318885715));
#445016=CARTESIAN_POINT('Ctrl Pts',(2.49625838937556,-0.984827048243718,
12.5893111709658));
#445017=CARTESIAN_POINT('Ctrl Pts',(2.48492472314964,-0.984908561672181,
12.5770542771492));
#445018=CARTESIAN_POINT('Ctrl Pts',(2.48198942389985,-1.00100786889855,
12.5737548217797));
#445019=CARTESIAN_POINT('',(2.47340424202237,-1.02203703919839,12.5737548217797));
#445020=CARTESIAN_POINT('Origin',(2.48778152717562,-1.02797788691754,12.5893111709658));
#445021=CARTESIAN_POINT('Ctrl Pts',(2.48198942389985,-1.00100786889855,
12.5737548217797));
#445022=CARTESIAN_POINT('Ctrl Pts',(2.48098759041817,-1.00098238741483,
12.5746934679442));
#445023=CARTESIAN_POINT('Ctrl Pts',(2.47987433720332,-1.00113731552034,
12.5756680099006));
#445024=CARTESIAN_POINT('Ctrl Pts',(2.47877586185187,-1.00145172857708,
12.5765688348656));
#445025=CARTESIAN_POINT('Ctrl Pts',(2.47848505266311,-1.00153496595319,
12.5768073183026));
#445026=CARTESIAN_POINT('Ctrl Pts',(2.47819527074308,-1.00162912416589,
12.5770407398754));
#445027=CARTESIAN_POINT('Ctrl Pts',(2.47790869827059,-1.00173327483036,
12.5772674179684));
#445028=CARTESIAN_POINT('Ctrl Pts',(2.47673268233593,-1.00216068099383,
12.5781976435658));
#445029=CARTESIAN_POINT('Ctrl Pts',(2.47554777353394,-1.00279124313488,
12.5790594849312));
#445030=CARTESIAN_POINT('Ctrl Pts',(2.4744566641771,-1.00362501354398,12.5797571720116));
#445031=CARTESIAN_POINT('Ctrl Pts',(2.47374576719832,-1.00416824494522,
12.580211740231));
#445032=CARTESIAN_POINT('Ctrl Pts',(2.47305377969915,-1.00483734156105,
12.5806009430798));
#445033=CARTESIAN_POINT('Ctrl Pts',(2.47244172975373,-1.00559793838503,
12.5808812374708));
#445034=CARTESIAN_POINT('Ctrl Pts',(2.47191577580516,-1.00625154338219,
12.5811221033394));
#445035=CARTESIAN_POINT('Ctrl Pts',(2.47143817306529,-1.00698616939287,
12.581287365893));
#445036=CARTESIAN_POINT('Ctrl Pts',(2.47104286871297,-1.0077648976847,12.581359338449));
#445037=CARTESIAN_POINT('Ctrl Pts',(2.47098792957072,-1.00787312483713,
12.5813693411482));
#445038=CARTESIAN_POINT('Ctrl Pts',(2.47093452067042,-1.00798219607774,
12.5813775999465));
#445039=CARTESIAN_POINT('Ctrl Pts',(2.47088267218419,-1.00809200543144,
12.5813841266931));
#445040=CARTESIAN_POINT('Ctrl Pts',(2.47079470495636,-1.00827831028117,
12.5813952001081));
#445041=CARTESIAN_POINT('Ctrl Pts',(2.47071119083597,-1.00846824755452,
12.5814007534795));
#445042=CARTESIAN_POINT('Ctrl Pts',(2.47063234672565,-1.00866181390519,
12.5814005856065));
#445043=CARTESIAN_POINT('Ctrl Pts',(2.47027142921465,-1.00954788497905,
12.5813998171494));
#445044=CARTESIAN_POINT('Ctrl Pts',(2.47003299351355,-1.01044865354929,
12.58127954464));
#445045=CARTESIAN_POINT('Ctrl Pts',(2.46988978909337,-1.01135143403267,
12.5810700125799));
#445046=CARTESIAN_POINT('Ctrl Pts',(2.46971681445891,-1.0124418900668,12.5808169217085));
#445047=CARTESIAN_POINT('Ctrl Pts',(2.46969929491538,-1.01353800202507,
12.5804173076348));
#445048=CARTESIAN_POINT('Ctrl Pts',(2.46981272680927,-1.01454329231802,
12.5799304713245));
#445049=CARTESIAN_POINT('Ctrl Pts',(2.46995330466054,-1.01578916369008,
12.5793271277669));
#445050=CARTESIAN_POINT('Ctrl Pts',(2.47027173407184,-1.01697643599179,
12.5785808224116));
#445051=CARTESIAN_POINT('Ctrl Pts',(2.47072395843903,-1.01806327957977,
12.5777485681082));
#445052=CARTESIAN_POINT('Ctrl Pts',(2.471397822291,-1.01968279559846,12.576508418016));
#445053=CARTESIAN_POINT('Ctrl Pts',(2.47235674899993,-1.02106832043681,
12.5750928681475));
#445054=CARTESIAN_POINT('Ctrl Pts',(2.47340424202237,-1.02203703919839,
12.5737548217797));
#445055=CARTESIAN_POINT('Ctrl Pts',(2.47340424202237,-1.02203703919839,
12.5737548217797));
#445056=CARTESIAN_POINT('Ctrl Pts',(2.46423365112038,-1.03559078175768,
12.5770542771492));
#445057=CARTESIAN_POINT('Ctrl Pts',(2.47227204101565,-1.04358095837972,
12.5893111709658));
#445058=CARTESIAN_POINT('Ctrl Pts',(2.49099968244631,-1.03945586322464,
12.5508408821982));
#445059=CARTESIAN_POINT('Ctrl Pts',(2.481798016426,-1.05304979816196,12.55409748406));
#445060=CARTESIAN_POINT('Ctrl Pts',(2.48984666124802,-1.061050168203,12.5663972313419));
#445061=CARTESIAN_POINT('Ctrl Pts',(2.50857710451762,-1.05685850949234,
12.52790050457));
#445062=CARTESIAN_POINT('Ctrl Pts',(2.49932874179139,-1.07047537639426,
12.5311362602938));
#445063=CARTESIAN_POINT('Ctrl Pts',(2.50740355157646,-1.07850175446413,
12.5434568539655));
#445064=CARTESIAN_POINT('Ctrl Pts',(2.52613789875103,-1.07424624506223,
12.5049357605811));
#445065=CARTESIAN_POINT('Ctrl Pts',(2.51682933400834,-1.08787100221311,
12.5081700652078));
#445066=CARTESIAN_POINT('Ctrl Pts',(2.52494410061065,-1.09593709744409,
12.5204921097672));
#445067=CARTESIAN_POINT('Ctrl Pts',(2.52498478704876,-1.07310449931469,
12.5064436508395));
#445068=CARTESIAN_POINT('Ctrl Pts',(2.52470543171259,-1.07429227386684,
12.5062361689309));
#445069=CARTESIAN_POINT('Ctrl Pts',(2.52436427567818,-1.07551554987029,
12.5061871075061));
#445070=CARTESIAN_POINT('Ctrl Pts',(2.52396803350171,-1.07667916869908,
12.5063648335164));
#445071=CARTESIAN_POINT('Ctrl Pts',(2.52378803586393,-1.0772077561461,12.5064455676329));
#445072=CARTESIAN_POINT('Ctrl Pts',(2.52359395185131,-1.07773133479322,
12.506574497099));
#445073=CARTESIAN_POINT('Ctrl Pts',(2.52339311777965,-1.078227089874,12.5067492519495));
#445074=CARTESIAN_POINT('Ctrl Pts',(2.52298953391681,-1.07922332895268,
12.5071004286051));
#445075=CARTESIAN_POINT('Ctrl Pts',(2.5225431042606,-1.08014353432877,12.5076537929613));
#445076=CARTESIAN_POINT('Ctrl Pts',(2.52209584556394,-1.0809227682504,12.5083435010505));
#445077=CARTESIAN_POINT('Ctrl Pts',(2.52206768795615,-1.0809718256825,12.5083869222964));
#445078=CARTESIAN_POINT('Ctrl Pts',(2.52203951364083,-1.08102032378924,
12.5084308732337));
#445079=CARTESIAN_POINT('Ctrl Pts',(2.52201132761947,-1.08106824652138,
12.5084753333615));
#445080=CARTESIAN_POINT('Ctrl Pts',(2.52178523852597,-1.08145265008544,
12.5088319622689));
#445081=CARTESIAN_POINT('Ctrl Pts',(2.52155491827216,-1.08180849120113,
12.509227847131));
#445082=CARTESIAN_POINT('Ctrl Pts',(2.52132956610943,-1.08212671031624,
12.5096423454524));
#445083=CARTESIAN_POINT('Ctrl Pts',(2.52062341216811,-1.08312386818513,
12.5109411997424));
#445084=CARTESIAN_POINT('Ctrl Pts',(2.51993049827934,-1.08381852812525,
12.5124831113042));
#445085=CARTESIAN_POINT('Ctrl Pts',(2.51928532695859,-1.08429881183553,
12.5140723025008));
#445086=CARTESIAN_POINT('Ctrl Pts',(2.5192248736992,-1.08434381494523,12.5142212114565));
#445087=CARTESIAN_POINT('Ctrl Pts',(2.51916484002758,-1.08438696545899,
12.5143705582413));
#445088=CARTESIAN_POINT('Ctrl Pts',(2.51910525611052,-1.08442835276199,
12.5145201959299));
#445089=CARTESIAN_POINT('Ctrl Pts',(2.51833981198475,-1.08496003428826,
12.5164425148273));
#445090=CARTESIAN_POINT('Ctrl Pts',(2.51762849097818,-1.08522776587955,
12.518463520594));
#445091=CARTESIAN_POINT('Ctrl Pts',(2.51695569853521,-1.08532040015755,
12.5205025929157));
#445092=CARTESIAN_POINT('Ctrl Pts',(2.51656545225128,-1.08537413171047,
12.5216853356836));
#445093=CARTESIAN_POINT('Ctrl Pts',(2.51618893964744,-1.08536933445125,
12.5228750347131));
#445094=CARTESIAN_POINT('Ctrl Pts',(2.51582900136034,-1.08532403237589,
12.5240609649613));
#445095=CARTESIAN_POINT('Ctrl Pts',(2.51494555214468,-1.08521284086229,
12.5269717671326));
#445096=CARTESIAN_POINT('Ctrl Pts',(2.51413838603744,-1.08484419216298,
12.5299036066169));
#445097=CARTESIAN_POINT('Ctrl Pts',(2.51338464420658,-1.08430167453326,
12.5328133004019));
#445098=CARTESIAN_POINT('Ctrl Pts',(2.51302280423869,-1.08404123448114,
12.5342101228451));
#445099=CARTESIAN_POINT('Ctrl Pts',(2.51267403383975,-1.08374062490796,
12.5356023438238));
#445100=CARTESIAN_POINT('Ctrl Pts',(2.51233926765279,-1.08340786672292,
12.5369868989719));
#445101=CARTESIAN_POINT('Origin',(11.5484677779407,-10.072808883968,-1.24078673491164));
#445102=CARTESIAN_POINT('Ctrl Pts',(2.55270907503905,-0.984421006740184,
12.5369868989719));
#445103=CARTESIAN_POINT('Ctrl Pts',(2.56804780751154,-0.984339829018829,
12.5369868989719));
#445104=CARTESIAN_POINT('Ctrl Pts',(2.5732755263982,-0.969919209790542,
12.5369868989719));
#445105=CARTESIAN_POINT('Ctrl Pts',(2.5578941661586,-0.984393499284525,
12.5218025310015));
#445106=CARTESIAN_POINT('Ctrl Pts',(2.56921912866175,-0.981016949565382,
12.5216901060419));
#445107=CARTESIAN_POINT('Ctrl Pts',(2.57325960608293,-0.969963174237659,
12.5161920673677));
#445108=CARTESIAN_POINT('Ctrl Pts',(2.5614363152843,-0.989270921838109,
12.5042015548895));
#445109=CARTESIAN_POINT('Ctrl Pts',(2.5671518381589,-0.98631962664998,12.4980677368512));
#445110=CARTESIAN_POINT('Ctrl Pts',(2.56958364755384,-0.979973203815791,
12.4907278922778));
#445111=CARTESIAN_POINT('Ctrl Pts',(2.55455382588049,-1.00062302800004,
12.506463626192));
#445112=CARTESIAN_POINT('Ctrl Pts',(2.56064588289877,-1.00300929697532,
12.4999376786891));
#445113=CARTESIAN_POINT('Ctrl Pts',(2.56057147728013,-1.00298015216942,
12.4906970594712));
#445114=CARTESIAN_POINT('Origin',(2.55259264528431,-0.9624213148307,12.5369868989719));
#445115=CARTESIAN_POINT('Origin',(2.55259264528431,-0.962421314830701,14.));
#445116=CARTESIAN_POINT('Origin',(2.55259264528431,-0.962421314830701,13.7435492065112));
#445117=CARTESIAN_POINT('Ctrl Pts',(2.5279914046812,-0.984598792482975,
13.793642941384));
#445118=CARTESIAN_POINT('Ctrl Pts',(2.53880360448866,-0.984548252110673,
13.8071662555867));
#445119=CARTESIAN_POINT('Ctrl Pts',(2.5412286718278,-0.967691845849694,
13.8103758687955));
#445120=CARTESIAN_POINT('Ctrl Pts',(2.54461209709991,-0.98447925694229,
13.7804579775006));
#445121=CARTESIAN_POINT('Ctrl Pts',(2.55795332699271,-0.984406753999513,
13.7901904343352));
#445122=CARTESIAN_POINT('Ctrl Pts',(2.56269071444785,-0.969379675631967,
13.7927914348262));
#445123=CARTESIAN_POINT('Ctrl Pts',(2.55439732423357,-0.984408881832837,
13.7597120340895));
#445124=CARTESIAN_POINT('Ctrl Pts',(2.56983685321751,-0.984319245198071,
13.7635825532445));
#445125=CARTESIAN_POINT('Ctrl Pts',(2.57534886053281,-0.970349503199748,
13.7651073818885));
#445126=CARTESIAN_POINT('Ctrl Pts',(2.55248115270456,-0.984422662889864,
13.7381884353898));
#445127=CARTESIAN_POINT('Ctrl Pts',(2.56755929596518,-0.9843360231847,13.7368803041982));
#445128=CARTESIAN_POINT('Ctrl Pts',(2.5728700571501,-0.970159089356977,
13.7363986145813));
#445129=CARTESIAN_POINT('Origin',(2.53186616300171,-0.962570382801922,13.7902182540695));
#445130=CARTESIAN_POINT('Ctrl Pts',(2.4962544532735,-0.984827075793866,
13.8235227101244));
#445131=CARTESIAN_POINT('Ctrl Pts',(2.50775125999332,-0.984748822573145,
13.8358800583119));
#445132=CARTESIAN_POINT('Ctrl Pts',(2.51061417570188,-0.96842614623922,
13.8390832900376));
#445133=CARTESIAN_POINT('Ctrl Pts',(2.5081817241524,-0.98474129307055,13.8124254819053));
#445134=CARTESIAN_POINT('Ctrl Pts',(2.51970085750601,-0.984662887605033,
13.8247886449158));
#445135=CARTESIAN_POINT('Ctrl Pts',(2.522550602614,-0.968316642350489,13.8279860620657));
#445136=CARTESIAN_POINT('Ctrl Pts',(2.52010364961653,-0.984655548792273,
13.8013225099955));
#445137=CARTESIAN_POINT('Ctrl Pts',(2.53163967443641,-0.984577030081323,
13.8136962257787));
#445138=CARTESIAN_POINT('Ctrl Pts',(2.53448150603402,-0.968207460201438,
13.8168830918626));
#445139=CARTESIAN_POINT('Ctrl Pts',(2.53202043764777,-0.984569841463197,
13.7902140179785));
#445140=CARTESIAN_POINT('Ctrl Pts',(2.54356827399449,-0.984491245954365,
13.802602731458));
#445141=CARTESIAN_POINT('Ctrl Pts',(2.54640710301026,-0.968098588990335,
13.8057746032558));
#445142=CARTESIAN_POINT('Origin',(2.49610016616594,-0.962827617218951,13.8235269408515));
#445143=CARTESIAN_POINT('Ctrl Pts',(2.47227204101566,-1.04358095837972,
13.8235269408515));
#445144=CARTESIAN_POINT('Ctrl Pts',(2.48064626725422,-1.05190495704,13.8362179249168));
#445145=CARTESIAN_POINT('Ctrl Pts',(2.47072418526053,-1.06580514743322,
13.8391868794938));
#445146=CARTESIAN_POINT('Ctrl Pts',(2.46460998851574,-1.03596486192765,
13.8400110824519));
#445147=CARTESIAN_POINT('Ctrl Pts',(2.46891234513801,-1.04506494930942,
13.8494522556836));
#445148=CARTESIAN_POINT('Ctrl Pts',(2.45819381891372,-1.05319151580552,
13.85569149686));
#445149=CARTESIAN_POINT('Ctrl Pts',(2.45876983422057,-1.02075662981956,
13.8586819406588));
#445150=CARTESIAN_POINT('Ctrl Pts',(2.45713710726879,-1.02479274755023,
13.868010383617));
#445151=CARTESIAN_POINT('Ctrl Pts',(2.44863534243242,-1.02789320904161,
13.8744918421245));
#445152=CARTESIAN_POINT('Ctrl Pts',(2.47054763281524,-0.991767753363052,
13.8587686893867));
#445153=CARTESIAN_POINT('Ctrl Pts',(2.4721657763133,-0.987767535926515,
13.8680909899357));
#445154=CARTESIAN_POINT('Ctrl Pts',(2.46824430207023,-0.979636211233281,
13.8745789365163));
#445155=CARTESIAN_POINT('Ctrl Pts',(2.48543775803918,-0.984904871841751,
13.8400379222776));
#445156=CARTESIAN_POINT('Ctrl Pts',(2.49487473178347,-0.981410052753833,
13.8494748685453));
#445157=CARTESIAN_POINT('Ctrl Pts',(2.49290813878161,-0.968109916768434,
13.8557104837033));
#445158=CARTESIAN_POINT('Ctrl Pts',(2.49625838937537,-0.984827048237167,
13.8235269408542));
#445159=CARTESIAN_POINT('Ctrl Pts',(2.50806556547963,-0.984742129254546,
13.8362179249195));
#445160=CARTESIAN_POINT('Ctrl Pts',(2.51070655207712,-0.967869423666875,
13.8391868794965));
#445161=CARTESIAN_POINT('Origin',(2.45676255485569,-1.0591840298419,13.8235269408515));
#445162=CARTESIAN_POINT('Ctrl Pts',(2.4976362366862,-1.06879302379797,13.7902140241683));
#445163=CARTESIAN_POINT('Ctrl Pts',(2.50582963879433,-1.07693100618227,
13.8026027327198));
#445164=CARTESIAN_POINT('Ctrl Pts',(2.49638484160699,-1.09062676239955,
13.8057746032556));
#445165=CARTESIAN_POINT('Ctrl Pts',(2.4891842683109,-1.06039174928721,13.8013225161808));
#445166=CARTESIAN_POINT('Ctrl Pts',(2.49736928741284,-1.06852141042319,
13.8136962270464));
#445167=CARTESIAN_POINT('Ctrl Pts',(2.48794279258032,-1.08220277733172,
13.8168830918628));
#445168=CARTESIAN_POINT('Ctrl Pts',(2.48072865621599,-1.05198685291141,
13.8124254880875));
#445169=CARTESIAN_POINT('Ctrl Pts',(2.48890168931206,-1.06010461153378,
13.8247886461867));
#445170=CARTESIAN_POINT('Ctrl Pts',(2.47949717086747,-1.07377485641174,
13.8279860620656));
#445171=CARTESIAN_POINT('Ctrl Pts',(2.47226925288946,-1.0435781880433,13.8235227163065));
#445172=CARTESIAN_POINT('Ctrl Pts',(2.48042644503294,-1.0516802124552,13.8358800595848));
#445173=CARTESIAN_POINT('Ctrl Pts',(2.47104782899334,-1.06534284002019,
13.8390832900376));
#445174=CARTESIAN_POINT('Origin',(2.48212954747995,-1.08439887436654,13.7902182540695));
#445175=CARTESIAN_POINT('Ctrl Pts',(2.51214785532751,-1.08321764135872,
13.7382347919292));
#445176=CARTESIAN_POINT('Ctrl Pts',(2.52286727958409,-1.09383893188013,
13.7369371795943));
#445177=CARTESIAN_POINT('Ctrl Pts',(2.51672651737721,-1.10768937651337,
13.7364597369711));
#445178=CARTESIAN_POINT('Ctrl Pts',(2.51348940671125,-1.08455114571532,
13.7595490285573));
#445179=CARTESIAN_POINT('Ctrl Pts',(2.52446387957603,-1.09542656532835,
13.7633824266925));
#445180=CARTESIAN_POINT('Ctrl Pts',(2.51860726334418,-1.10926830317516,
13.7648920890506));
#445181=CARTESIAN_POINT('Ctrl Pts',(2.506647568156,-1.07775034654637,13.7803806590111));
#445182=CARTESIAN_POINT('Ctrl Pts',(2.51614389432564,-1.08715336070585,
13.7901039518745));
#445183=CARTESIAN_POINT('Ctrl Pts',(2.50902140224746,-1.10121591907983,
13.7926933640892));
#445184=CARTESIAN_POINT('Ctrl Pts',(2.49475492540219,-1.06592903951609,
13.7936647693663));
#445185=CARTESIAN_POINT('Ctrl Pts',(2.50244665338408,-1.07353237119353,
13.8072068914932));
#445186=CARTESIAN_POINT('Ctrl Pts',(2.49236240097613,-1.08727835690645,
13.8104111085397));
#445187=CARTESIAN_POINT('Origin',(2.49682978149282,-1.0990109381851,13.7435492065112));
#445188=CARTESIAN_POINT('Origin',(2.49682978149282,-1.0990109381851,14.));
#445189=CARTESIAN_POINT('Origin',(2.49682978149282,-1.0990109381851,12.5369868989719));
#445190=CARTESIAN_POINT('Ctrl Pts',(2.52496786835779,-1.07309730895387,
12.506462012331));
#445191=CARTESIAN_POINT('Ctrl Pts',(2.53098557711664,-1.07565480172679,
12.4999388158272));
#445192=CARTESIAN_POINT('Ctrl Pts',(2.53091437973029,-1.07562454323334,
12.4907030323752));
#445193=CARTESIAN_POINT('Ctrl Pts',(2.52193718330867,-1.08602184110352,
12.5042014951932));
#445194=CARTESIAN_POINT('Ctrl Pts',(2.52395421724622,-1.09212697592684,
12.4980716682127));
#445195=CARTESIAN_POINT('Ctrl Pts',(2.52125297277396,-1.09835825537226,
12.4907355092744));
#445196=CARTESIAN_POINT('Ctrl Pts',(2.51599482735783,-1.08702886990104,
12.5218047446509));
#445197=CARTESIAN_POINT('Ctrl Pts',(2.5217171510995,-1.09736201472395,12.5216906929434));
#445198=CARTESIAN_POINT('Ctrl Pts',(2.516872983028,-1.10808137991155,12.5161988840775));
#445199=CARTESIAN_POINT('Ctrl Pts',(2.5123119981278,-1.08338080804912,12.5369868989719));
#445200=CARTESIAN_POINT('Ctrl Pts',(2.52320327893529,-1.09416902077844,
12.5369868989719));
#445201=CARTESIAN_POINT('Ctrl Pts',(2.516854309111,-1.10812237570445,12.5369868989719));
#445202=CARTESIAN_POINT('Origin',(4.76969326057516E-31,-7.09909511483988E-31,
12.5));
#445203=CARTESIAN_POINT('Origin',(2.54910729598815,-0.838595406033455,12.5));
#445204=CARTESIAN_POINT('',(2.54910729598815,-0.838595406033455,12.5893111709658));
#445205=CARTESIAN_POINT('',(2.54910729598815,-0.838595406033455,13.8235269408515));
#445206=CARTESIAN_POINT('',(2.54910729598815,-0.838595406033455,12.5));
#445207=CARTESIAN_POINT('',(2.57644512594904,-0.86165870484848,13.7902182540695));
#445208=CARTESIAN_POINT('',(2.54910729598815,-0.838595406033455,13.8235269408515));
#445209=CARTESIAN_POINT('',(2.59228746499891,-0.875023942687729,13.7435492065112));
#445210=CARTESIAN_POINT('Origin',(2.54016658898052,-0.831052237871044,13.7445212918687));
#445211=CARTESIAN_POINT('',(2.59228746499891,-0.875023942687729,12.5369868989719));
#445212=CARTESIAN_POINT('',(2.59228746499891,-0.875023942687729,12.5));
#445213=CARTESIAN_POINT('Ctrl Pts',(2.59228746499891,-0.875023942687729,
12.5369868989719));
#445214=CARTESIAN_POINT('Ctrl Pts',(2.57790457299166,-0.862889953389305,
12.5544431401645));
#445215=CARTESIAN_POINT('Ctrl Pts',(2.56351139395777,-0.850747285539233,
12.5718848856037));
#445216=CARTESIAN_POINT('Ctrl Pts',(2.54910729598815,-0.838595406033455,
12.5893111709658));
#445217=CARTESIAN_POINT('Origin',(2.84214150603756,-0.753696202164162,12.5));
#445218=CARTESIAN_POINT('',(2.62449623026969,-0.7730722726676,13.7435492065112));
#445219=CARTESIAN_POINT('',(2.60385086407061,-0.774910245348751,13.7902182540695));
#445220=CARTESIAN_POINT('Origin',(2.54959840993456,-0.779740119889402,13.7418732680441));
#445221=CARTESIAN_POINT('',(2.56822484263186,-0.778081884616907,13.8235269408515));
#445222=CARTESIAN_POINT('',(2.60385086407061,-0.774910245348751,13.7902182540695));
#445223=CARTESIAN_POINT('',(2.56822484263186,-0.778081884616907,12.5893111709658));
#445224=CARTESIAN_POINT('',(2.56822484263186,-0.778081884616907,12.5));
#445225=CARTESIAN_POINT('',(2.62449623026969,-0.7730722726676,12.5369868989719));
#445226=CARTESIAN_POINT('Ctrl Pts',(2.56822484263186,-0.778081884616907,
12.5893111709658));
#445227=CARTESIAN_POINT('Ctrl Pts',(2.58699592665007,-0.776410771627757,
12.5718848856037));
#445228=CARTESIAN_POINT('Ctrl Pts',(2.60575278136629,-0.774740925415281,
12.5544431401645));
#445229=CARTESIAN_POINT('Ctrl Pts',(2.62449623026969,-0.7730722726676,12.5369868989719));
#445230=CARTESIAN_POINT('',(2.62449623026969,-0.7730722726676,12.5));
#445231=CARTESIAN_POINT('Origin',(2.57127305293845,-0.812321467542621,12.5));
#445232=CARTESIAN_POINT('',(2.53817572546673,-0.803039383379718,13.8587068136939));
#445233=CARTESIAN_POINT('Ctrl Pts',(2.56822484263113,-0.778081884610338,
13.8235269408542));
#445234=CARTESIAN_POINT('Ctrl Pts',(2.56647944731823,-0.778237270030589,
13.8262006681044));
#445235=CARTESIAN_POINT('Ctrl Pts',(2.56470869660341,-0.778569339207121,
13.8288634856214));
#445236=CARTESIAN_POINT('Ctrl Pts',(2.56291591900165,-0.779065179857554,
13.8314912288862));
#445237=CARTESIAN_POINT('Ctrl Pts',(2.56106775021066,-0.779576340424559,
13.8342001611531));
#445238=CARTESIAN_POINT('Ctrl Pts',(2.55919398706925,-0.780261637720204,
13.8368750301949));
#445239=CARTESIAN_POINT('Ctrl Pts',(2.55729015724091,-0.781151391114411,
13.8394886372969));
#445240=CARTESIAN_POINT('Ctrl Pts',(2.55714311984523,-0.781220108927285,
13.8396904925131));
#445241=CARTESIAN_POINT('Ctrl Pts',(2.55699590888648,-0.781290067670456,
13.8398919674349));
#445242=CARTESIAN_POINT('Ctrl Pts',(2.55684852624958,-0.781361292053912,
13.8400930404591));
#445243=CARTESIAN_POINT('Ctrl Pts',(2.55455220561251,-0.782471015865588,
13.8432258934518));
#445244=CARTESIAN_POINT('Ctrl Pts',(2.55222543639613,-0.783881307288202,
13.8462331177034));
#445245=CARTESIAN_POINT('Ctrl Pts',(2.54999410726517,-0.785628665955706,
13.8489036603661));
#445246=CARTESIAN_POINT('Ctrl Pts',(2.54926399040623,-0.78620042204675,
13.849777493004));
#445247=CARTESIAN_POINT('Ctrl Pts',(2.54854434111879,-0.786808245935407,
13.85061494757));
#445248=CARTESIAN_POINT('Ctrl Pts',(2.54784027995605,-0.787453344071125,
13.8514076489583));
#445249=CARTESIAN_POINT('Ctrl Pts',(2.54635108905603,-0.788817819665242,
13.8530843267192));
#445250=CARTESIAN_POINT('Ctrl Pts',(2.54478735737639,-0.790485262420232,
13.8546805203176));
#445251=CARTESIAN_POINT('Ctrl Pts',(2.54333937054587,-0.792452231402247,
13.8559412814273));
#445252=CARTESIAN_POINT('Ctrl Pts',(2.54314558294863,-0.792715475642356,
13.8561100121513));
#445253=CARTESIAN_POINT('Ctrl Pts',(2.54295385085688,-0.792984009956763,
13.8562727473908));
#445254=CARTESIAN_POINT('Ctrl Pts',(2.54276460390983,-0.793257755025675,
13.8564289040185));
#445255=CARTESIAN_POINT('Ctrl Pts',(2.54190637116397,-0.794499185790202,
13.8571370725437));
#445256=CARTESIAN_POINT('Ctrl Pts',(2.54108603539448,-0.795870896971541,
13.8577210840554));
#445257=CARTESIAN_POINT('Ctrl Pts',(2.54036067071043,-0.797334633007628,
13.8581177131616));
#445258=CARTESIAN_POINT('Ctrl Pts',(2.54015638304911,-0.797746871455648,
13.8582294175695));
#445259=CARTESIAN_POINT('Ctrl Pts',(2.53995948769189,-0.798166300610782,
13.8583265086086));
#445260=CARTESIAN_POINT('Ctrl Pts',(2.53977089619018,-0.798591818571351,
13.8584082369006));
#445261=CARTESIAN_POINT('Ctrl Pts',(2.53949994077503,-0.799203173773543,
13.8585256585398));
#445262=CARTESIAN_POINT('Ctrl Pts',(2.53924305316311,-0.799834829079575,
13.8586122832068));
#445263=CARTESIAN_POINT('Ctrl Pts',(2.53900763805649,-0.80047067341131,
13.8586682984299));
#445264=CARTESIAN_POINT('Ctrl Pts',(2.53881932930715,-0.800979285847475,
13.8587131050557));
#445265=CARTESIAN_POINT('Ctrl Pts',(2.5386424597895,-0.801496114809985,
13.8587357943552));
#445266=CARTESIAN_POINT('Ctrl Pts',(2.53847748765059,-0.802021385692067,
13.8587355499465));
#445267=CARTESIAN_POINT('Ctrl Pts',(2.53837086222413,-0.802360880786095,
13.8587353919793));
#445268=CARTESIAN_POINT('Ctrl Pts',(2.53827032288092,-0.80270021951906,
13.8587257282814));
#445269=CARTESIAN_POINT('Ctrl Pts',(2.53817572546673,-0.803039383379718,
13.8587068136939));
#445270=CARTESIAN_POINT('Ctrl Pts',(2.53817572546673,-0.803039383379718,
13.8587068136939));
#445271=CARTESIAN_POINT('Ctrl Pts',(2.53786459972836,-0.804154874828118,
13.8586446046466));
#445272=CARTESIAN_POINT('Ctrl Pts',(2.53761766935199,-0.805268477726748,
13.858482427929));
#445273=CARTESIAN_POINT('Ctrl Pts',(2.53743051374488,-0.806379525504473,
13.8582284286032));
#445274=CARTESIAN_POINT('Ctrl Pts',(2.53723851386283,-0.807519331281929,
13.8579678548414));
#445275=CARTESIAN_POINT('Ctrl Pts',(2.53711046454625,-0.808659486611959,
13.857615680862));
#445276=CARTESIAN_POINT('Ctrl Pts',(2.53704178491179,-0.809753960282416,
13.8571944833187));
#445277=CARTESIAN_POINT('Ctrl Pts',(2.53687038786002,-0.812485331260639,
13.8561433417727));
#445278=CARTESIAN_POINT('Ctrl Pts',(2.53705594359453,-0.815059660120175,
13.8546163505474));
#445279=CARTESIAN_POINT('Ctrl Pts',(2.53743322060591,-0.817352623030055,
13.8528973491086));
#445280=CARTESIAN_POINT('Ctrl Pts',(2.53750214354969,-0.817771513524167,
13.8525833129072));
#445281=CARTESIAN_POINT('Ctrl Pts',(2.53757735189796,-0.818181098507309,
13.8522628768812));
#445282=CARTESIAN_POINT('Ctrl Pts',(2.53765771368243,-0.818580748274922,
13.851937733538));
#445283=CARTESIAN_POINT('Ctrl Pts',(2.53814847195048,-0.821021353956894,
13.8499521282529));
#445284=CARTESIAN_POINT('Ctrl Pts',(2.53888419156482,-0.823333184477915,
13.847639871647));
#445285=CARTESIAN_POINT('Ctrl Pts',(2.53974964841443,-0.825419102289882,
13.8452109780794));
#445286=CARTESIAN_POINT('Ctrl Pts',(2.54013903536514,-0.826357599889833,
13.8441181685877));
#445287=CARTESIAN_POINT('Ctrl Pts',(2.54055415791594,-0.827250853667279,
13.8430021611332));
#445288=CARTESIAN_POINT('Ctrl Pts',(2.54098290735402,-0.828092904772393,
13.8418824960098));
#445289=CARTESIAN_POINT('Ctrl Pts',(2.54199326635338,-0.83007721970415,
13.8392439765549));
#445290=CARTESIAN_POINT('Ctrl Pts',(2.54312422728481,-0.831873770158096,
13.8364981347964));
#445291=CARTESIAN_POINT('Ctrl Pts',(2.5443498211129,-0.83350553815676,13.8336931113419));
#445292=CARTESIAN_POINT('Ctrl Pts',(2.54554347166906,-0.835094776560609,
13.8309611966327));
#445293=CARTESIAN_POINT('Ctrl Pts',(2.54682853391824,-0.836528963770409,
13.8281701127185));
#445294=CARTESIAN_POINT('Ctrl Pts',(2.54820170062591,-0.837795914587397,
13.825358068512));
#445295=CARTESIAN_POINT('Ctrl Pts',(2.54849940465008,-0.838070590891845,
13.8247484142932));
#445296=CARTESIAN_POINT('Ctrl Pts',(2.54880127635621,-0.838337235497436,
13.8241378483365));
#445297=CARTESIAN_POINT('Ctrl Pts',(2.54910729598815,-0.838595406033455,
13.8235269408515));
#445298=CARTESIAN_POINT('',(2.5385326372653,-0.801849681389652,12.5969504640361));
#445299=CARTESIAN_POINT('Origin',(2.57130454242783,-0.812331621106978,12.584524458991));
#445300=CARTESIAN_POINT('Origin',(2.57130454242783,-0.812331621106978,12.584524458991));
#445301=CARTESIAN_POINT('Ctrl Pts',(2.56822484263186,-0.778081884616907,
12.5893111709658));
#445302=CARTESIAN_POINT('Ctrl Pts',(2.55693553234649,-0.779086925830197,
12.5770542771492));
#445303=CARTESIAN_POINT('Ctrl Pts',(2.55532224306044,-0.79537191807872,
12.5737548217797));
#445304=CARTESIAN_POINT('Ctrl Pts',(2.59291077542083,-0.775884196785299,
12.5663937883685));
#445305=CARTESIAN_POINT('Ctrl Pts',(2.58160706405235,-0.77689052006824,
12.5540940315304));
#445306=CARTESIAN_POINT('Ctrl Pts',(2.57999197105446,-0.793226292774825,
12.5508374392248));
#445307=CARTESIAN_POINT('Ctrl Pts',(2.61757180040624,-0.77368872639377,
12.5434499600945));
#445308=CARTESIAN_POINT('Ctrl Pts',(2.60623133664677,-0.774698321592072,
12.5311293540533));
#445309=CARTESIAN_POINT('Ctrl Pts',(2.60463749396728,-0.791081588362601,
12.5278936106989));
#445310=CARTESIAN_POINT('Ctrl Pts',(2.64220986865041,-0.771495299747208,
12.5204817579905));
#445311=CARTESIAN_POINT('Ctrl Pts',(2.63081327734545,-0.772509891751767,
12.5081597038247));
#445312=CARTESIAN_POINT('Ctrl Pts',(2.62926069191201,-0.788937719464725,
12.5049254088044));
#445313=CARTESIAN_POINT('Ctrl Pts',(2.62449623026969,-0.773072272667601,
12.5369868989719));
#445314=CARTESIAN_POINT('Ctrl Pts',(2.62542406549704,-0.772989671447156,
12.5342545179733));
#445315=CARTESIAN_POINT('Ctrl Pts',(2.62632061097316,-0.773035095258176,
12.5314872231885));
#445316=CARTESIAN_POINT('Ctrl Pts',(2.62713253427595,-0.773261814601223,
12.5287124745063));
#445317=CARTESIAN_POINT('Ctrl Pts',(2.62786476701068,-0.773466281358128,
12.5262100684184));
#445318=CARTESIAN_POINT('Ctrl Pts',(2.6285271703971,-0.773818942798318,
12.5237004536639));
#445319=CARTESIAN_POINT('Ctrl Pts',(2.62909996534728,-0.774384368758529,
12.5212220730815));
#445320=CARTESIAN_POINT('Ctrl Pts',(2.62953848943233,-0.774817251244295,
12.5193246583487));
#445321=CARTESIAN_POINT('Ctrl Pts',(2.62992928716097,-0.775380465021055,
12.5174178313692));
#445322=CARTESIAN_POINT('Ctrl Pts',(2.63020498137755,-0.776144112454325,
12.515581224835));
#445323=CARTESIAN_POINT('Ctrl Pts',(2.6303224285957,-0.776469430365577,
12.5147988205795));
#445324=CARTESIAN_POINT('Ctrl Pts',(2.63041936655023,-0.776831359267061,
12.5140295443048));
#445325=CARTESIAN_POINT('Ctrl Pts',(2.63049264606625,-0.777235850138907,
12.5132817086137));
#445326=CARTESIAN_POINT('Ctrl Pts',(2.6306035447007,-0.777847992355085,
12.5121499604604));
#445327=CARTESIAN_POINT('Ctrl Pts',(2.6306556166868,-0.77857210672806,12.5110494206568));
#445328=CARTESIAN_POINT('Ctrl Pts',(2.63061455185156,-0.779422674651865,
12.5100666561695));
#445329=CARTESIAN_POINT('Ctrl Pts',(2.63059097251774,-0.77991106879503,
12.5095023550641));
#445330=CARTESIAN_POINT('Ctrl Pts',(2.63053576127102,-0.780446766521068,
12.5089719619137));
#445331=CARTESIAN_POINT('Ctrl Pts',(2.63044359966078,-0.781019071967967,
12.5085043804652));
#445332=CARTESIAN_POINT('Ctrl Pts',(2.6303087331491,-0.781856566441477,
12.5078201359221));
#445333=CARTESIAN_POINT('Ctrl Pts',(2.63008963522878,-0.782796552672182,
12.5072563000949));
#445334=CARTESIAN_POINT('Ctrl Pts',(2.62979291251723,-0.783773391665485,
12.5068768744332));
#445335=CARTESIAN_POINT('Ctrl Pts',(2.62957895501575,-0.784477759825482,
12.5066032824114));
#445336=CARTESIAN_POINT('Ctrl Pts',(2.62932093581241,-0.785213681364361,
12.5064197834844));
#445337=CARTESIAN_POINT('Ctrl Pts',(2.62903570264673,-0.785940915740938,
12.5063282718343));
#445338=CARTESIAN_POINT('Ctrl Pts',(2.62861935053079,-0.787002452784669,
12.5061946931565));
#445339=CARTESIAN_POINT('Ctrl Pts',(2.62813710355232,-0.788068557062745,
12.5062515701262));
#445340=CARTESIAN_POINT('Ctrl Pts',(2.6276329808544,-0.789079437829282,
12.5064436508398));
#445341=CARTESIAN_POINT('',(2.55532224306044,-0.79537191807872,12.5737548217797));
#445342=CARTESIAN_POINT('Origin',(2.57017569722808,-0.799995217689364,12.5893111709658));
#445343=CARTESIAN_POINT('Ctrl Pts',(2.6276329808544,-0.789079437829282,
12.5064436508398));
#445344=CARTESIAN_POINT('Ctrl Pts',(2.61692915463513,-0.790011367021186,
12.5164271754438));
#445345=CARTESIAN_POINT('Ctrl Pts',(2.60622106729915,-0.790943457481382,
12.5264061185523));
#445346=CARTESIAN_POINT('Ctrl Pts',(2.59550856885561,-0.791875715832526,
12.536380305637));
#445347=CARTESIAN_POINT('Ctrl Pts',(2.58212011852998,-0.79304084968909,
12.5488460165097));
#445348=CARTESIAN_POINT('Ctrl Pts',(2.56872477412813,-0.794206246110122,
12.5613043021964));
#445349=CARTESIAN_POINT('Ctrl Pts',(2.55532224306044,-0.79537191807872,
12.5737548217797));
#445350=CARTESIAN_POINT('Ctrl Pts',(2.54910729598815,-0.838595406033455,
12.5893111709658));
#445351=CARTESIAN_POINT('Ctrl Pts',(2.54044437960026,-0.83128701946622,
12.5770542771492));
#445352=CARTESIAN_POINT('Ctrl Pts',(2.54847970027215,-0.81703088757307,
12.5737548217797));
#445353=CARTESIAN_POINT('Ctrl Pts',(2.54102487034432,-0.831776744931215,
12.5928319619712));
#445354=CARTESIAN_POINT('Ctrl Pts',(2.53730351958565,-0.824375058305697,
12.5821634970843));
#445355=CARTESIAN_POINT('Ctrl Pts',(2.54552938186325,-0.814554228804583,
12.5773203894503));
#445356=CARTESIAN_POINT('Ctrl Pts',(2.53389380091358,-0.816619834028473,
12.5969440695591));
#445357=CARTESIAN_POINT('Ctrl Pts',(2.53508730321628,-0.812781332393018,
12.5878292599214));
#445358=CARTESIAN_POINT('Ctrl Pts',(2.54298957451851,-0.809151125460285,
12.5813877129824));
#445359=CARTESIAN_POINT('Ctrl Pts',(2.54305959148014,-0.787427993921494,
12.596957478804));
#445360=CARTESIAN_POINT('Ctrl Pts',(2.54187498602332,-0.791238151800188,
12.5878468778671));
#445361=CARTESIAN_POINT('Ctrl Pts',(2.54627582919326,-0.798704748168761,
12.5814011370086));
#445362=CARTESIAN_POINT('Ctrl Pts',(2.5576767206763,-0.779020940858569,
12.5928371701607));
#445363=CARTESIAN_POINT('Ctrl Pts',(2.55038658775776,-0.782943825987378,
12.5821692192952));
#445364=CARTESIAN_POINT('Ctrl Pts',(2.55147225643998,-0.795704905310084,
12.5773318885715));
#445365=CARTESIAN_POINT('Ctrl Pts',(2.56822484263185,-0.778081884616852,
12.5893111709658));
#445366=CARTESIAN_POINT('Ctrl Pts',(2.55693553234648,-0.779086925830142,
12.5770542771492));
#445367=CARTESIAN_POINT('Ctrl Pts',(2.55532224306043,-0.795371918078664,
12.5737548217797));
#445368=CARTESIAN_POINT('',(2.54847970027215,-0.81703088757307,12.5737548217797));
#445369=CARTESIAN_POINT('Origin',(2.56329338043634,-0.821780085399321,12.5893111709658));
#445370=CARTESIAN_POINT('Ctrl Pts',(2.55532224306043,-0.795371918078664,
12.5737548217797));
#445371=CARTESIAN_POINT('Ctrl Pts',(2.55432166611954,-0.795428180111798,
12.5746934679442));
#445372=CARTESIAN_POINT('Ctrl Pts',(2.55322474524181,-0.795673333178764,
12.5756680099006));
#445373=CARTESIAN_POINT('Ctrl Pts',(2.55215555255946,-0.796076235990892,
12.5765688348656));
#445374=CARTESIAN_POINT('Ctrl Pts',(2.55187249563317,-0.79618290005012,
12.5768073183026));
#445375=CARTESIAN_POINT('Ctrl Pts',(2.55159135270704,-0.79630036487582,
12.5770407398754));
#445376=CARTESIAN_POINT('Ctrl Pts',(2.55131422302685,-0.796427527304466,
12.5772674179684));
#445377=CARTESIAN_POINT('Ctrl Pts',(2.55017695775837,-0.796949367525463,
12.5781976435658));
#445378=CARTESIAN_POINT('Ctrl Pts',(2.54904738831101,-0.797674412590524,
12.5790594849312));
#445379=CARTESIAN_POINT('Ctrl Pts',(2.54802786955923,-0.798594344239317,
12.5797571720116));
#445380=CARTESIAN_POINT('Ctrl Pts',(2.54736361643382,-0.7991937127863,12.580211740231));
#445381=CARTESIAN_POINT('Ctrl Pts',(2.54672846905175,-0.799916986443622,
12.5806009430798));
#445382=CARTESIAN_POINT('Ctrl Pts',(2.54618045135423,-0.800724940196953,
12.5808812374708));
#445383=CARTESIAN_POINT('Ctrl Pts',(2.54570952234908,-0.801419240506932,
12.5811221033394));
#445384=CARTESIAN_POINT('Ctrl Pts',(2.54529338763273,-0.802190351167311,
12.581287365893));
#445385=CARTESIAN_POINT('Ctrl Pts',(2.54496287220817,-0.802998709279525,
12.581359338449));
#445386=CARTESIAN_POINT('Ctrl Pts',(2.54491693738904,-0.803111054365166,
12.5813693411482));
#445387=CARTESIAN_POINT('Ctrl Pts',(2.54487259652113,-0.803224116001412,
12.5813775999465));
#445388=CARTESIAN_POINT('Ctrl Pts',(2.54482987103821,-0.803337786106517,
12.5813841266931));
#445389=CARTESIAN_POINT('Ctrl Pts',(2.5447573820889,-0.803530641187942,
12.5813952001081));
#445390=CARTESIAN_POINT('Ctrl Pts',(2.54468962750592,-0.803726753636801,
12.5814007534795));
#445391=CARTESIAN_POINT('Ctrl Pts',(2.54462682319744,-0.803926102438358,
12.5814005856065));
#445392=CARTESIAN_POINT('Ctrl Pts',(2.54433932962808,-0.804838643311557,
12.5813998171494));
#445393=CARTESIAN_POINT('Ctrl Pts',(2.54417510830291,-0.805755849371853,
12.58127954464));
#445394=CARTESIAN_POINT('Ctrl Pts',(2.54410596537402,-0.806667298417337,
12.5810700125799));
#445395=CARTESIAN_POINT('Ctrl Pts',(2.54402244858848,-0.807768225087497,
12.5808169217085));
#445396=CARTESIAN_POINT('Ctrl Pts',(2.54409433064018,-0.808862117829087,
12.5804173076348));
#445397=CARTESIAN_POINT('Ctrl Pts',(2.54428932559034,-0.809854817349115,
12.5799304713245));
#445398=CARTESIAN_POINT('Ctrl Pts',(2.54453098576334,-0.811085084787029,
12.5793271277669));
#445399=CARTESIAN_POINT('Ctrl Pts',(2.54494512934173,-0.812242451584925,
12.5785808224116));
#445400=CARTESIAN_POINT('Ctrl Pts',(2.54548443681182,-0.81328881830635,
12.5777485681082));
#445401=CARTESIAN_POINT('Ctrl Pts',(2.5462880640278,-0.814848019359306,
12.576508418016));
#445402=CARTESIAN_POINT('Ctrl Pts',(2.54735673312412,-0.81615077254903,
12.5750928681475));
#445403=CARTESIAN_POINT('Ctrl Pts',(2.54847970027215,-0.81703088757307,
12.5737548217797));
#445404=CARTESIAN_POINT('Ctrl Pts',(2.54847970027215,-0.81703088757307,
12.5737548217797));
#445405=CARTESIAN_POINT('Ctrl Pts',(2.54044437960026,-0.831287019466221,
12.5770542771492));
#445406=CARTESIAN_POINT('Ctrl Pts',(2.54910729598815,-0.838595406033455,
12.5893111709658));
#445407=CARTESIAN_POINT('Ctrl Pts',(2.5674363891862,-0.832957560156687,
12.5508408821982));
#445408=CARTESIAN_POINT('Ctrl Pts',(2.5593733728478,-0.847256283601681,
12.55409748406));
#445409=CARTESIAN_POINT('Ctrl Pts',(2.56804734089832,-0.854573993798405,
12.5663972313419));
#445410=CARTESIAN_POINT('Ctrl Pts',(2.58637380106472,-0.848869577474897,
12.52790050457));
#445411=CARTESIAN_POINT('Ctrl Pts',(2.57826611256788,-0.863194962795343,
12.5311362602938));
#445412=CARTESIAN_POINT('Ctrl Pts',(2.58696827841544,-0.870536461793924,
12.5434568539655));
#445413=CARTESIAN_POINT('Ctrl Pts',(2.60529342507279,-0.86476808903258,
12.5049357605811));
#445414=CARTESIAN_POINT('Ctrl Pts',(2.59712637800524,-0.87910624537103,
12.5081700652078));
#445415=CARTESIAN_POINT('Ctrl Pts',(2.60587160503441,-0.886484072523638,
12.5204921097672));
#445416=CARTESIAN_POINT('Ctrl Pts',(2.60405108737671,-0.86372413165853,
12.5064436508395));
#445417=CARTESIAN_POINT('Ctrl Pts',(2.60386947622514,-0.864930724042148,
12.5062361689309));
#445418=CARTESIAN_POINT('Ctrl Pts',(2.60362916370991,-0.866177737079556,
12.5061871075061));
#445419=CARTESIAN_POINT('Ctrl Pts',(2.60332908573365,-0.867369781478595,
12.5063648335164));
#445420=CARTESIAN_POINT('Ctrl Pts',(2.60319277180725,-0.867911281572986,
12.5064455676329));
#445421=CARTESIAN_POINT('Ctrl Pts',(2.60304201011359,-0.868448937704168,
12.506574497099));
#445422=CARTESIAN_POINT('Ctrl Pts',(2.60288225294218,-0.868959413042104,
12.5067492519495));
#445423=CARTESIAN_POINT('Ctrl Pts',(2.60256121470493,-0.869985233048843,
12.5071004286051));
#445424=CARTESIAN_POINT('Ctrl Pts',(2.60219127578753,-0.87093876467881,
12.5076537929612));
#445425=CARTESIAN_POINT('Ctrl Pts',(2.601809020106,-0.871751861499721,12.5083435010503));
#445426=CARTESIAN_POINT('Ctrl Pts',(2.60178495482643,-0.871803050803785,
12.5083869222963));
#445427=CARTESIAN_POINT('Ctrl Pts',(2.60176082730472,-0.871853684005415,
12.5084308732336));
#445428=CARTESIAN_POINT('Ctrl Pts',(2.60173664121753,-0.871903744701114,
12.5084753333615));
#445429=CARTESIAN_POINT('Ctrl Pts',(2.60154263687595,-0.872305297554053,
12.508831962269));
#445430=CARTESIAN_POINT('Ctrl Pts',(2.60134208734818,-0.872678727876636,
12.509227847131));
#445431=CARTESIAN_POINT('Ctrl Pts',(2.60114342283827,-0.873014256437226,
12.5096423454524));
#445432=CARTESIAN_POINT('Ctrl Pts',(2.60052089618941,-0.874065654447397,
12.5109411997424));
#445433=CARTESIAN_POINT('Ctrl Pts',(2.59988690914847,-0.874814481878505,
12.5124831113042));
#445434=CARTESIAN_POINT('Ctrl Pts',(2.59928303216319,-0.875345754936481,
12.5140723025008));
#445435=CARTESIAN_POINT('Ctrl Pts',(2.59922644822826,-0.8753955358039,12.5142212114565));
#445436=CARTESIAN_POINT('Ctrl Pts',(2.5991701314812,-0.875443436039455,
12.5143705582413));
#445437=CARTESIAN_POINT('Ctrl Pts',(2.59911411927412,-0.875489542272007,
12.5145201959299));
#445438=CARTESIAN_POINT('Ctrl Pts',(2.59839455908081,-0.876081845474152,
12.5164425148273));
#445439=CARTESIAN_POINT('Ctrl Pts',(2.5977074275464,-0.876406665476267,
12.5184635205941));
#445440=CARTESIAN_POINT('Ctrl Pts',(2.59704442431841,-0.876553830351355,
12.5205025929158));
#445441=CARTESIAN_POINT('Ctrl Pts',(2.59665985616718,-0.876639191811976,
12.5216853356836));
#445442=CARTESIAN_POINT('Ctrl Pts',(2.59628420535681,-0.87666509978783,
12.5228750347131));
#445443=CARTESIAN_POINT('Ctrl Pts',(2.59592177219496,-0.876649286763289,
12.5240609649613));
#445444=CARTESIAN_POINT('Ctrl Pts',(2.59503219944308,-0.876610474542893,
12.5269717671326));
#445445=CARTESIAN_POINT('Ctrl Pts',(2.59419767082312,-0.876308844022821,
12.5299036066169));
#445446=CARTESIAN_POINT('Ctrl Pts',(2.59340221678271,-0.875829568532383,
12.5328133004019));
#445447=CARTESIAN_POINT('Ctrl Pts',(2.59302035252541,-0.875599488389593,
12.5342101228451));
#445448=CARTESIAN_POINT('Ctrl Pts',(2.59264824016026,-0.8753283070953,12.5356023438238));
#445449=CARTESIAN_POINT('Ctrl Pts',(2.59228746499891,-0.875023942687728,
12.5369868989719));
#445450=CARTESIAN_POINT('Origin',(12.3313552281263,-9.09822770945204,-1.24119156191802));
#445451=CARTESIAN_POINT('Ctrl Pts',(2.62445459714358,-0.773075939238756,
12.5369868989719));
#445452=CARTESIAN_POINT('Ctrl Pts',(2.63973567451123,-0.771744782535234,
12.5369868989719));
#445453=CARTESIAN_POINT('Ctrl Pts',(2.64377058425296,-0.756946039106763,
12.5369868989719));
#445454=CARTESIAN_POINT('Ctrl Pts',(2.62962019318718,-0.772625890249611,
12.5218025310016));
#445455=CARTESIAN_POINT('Ctrl Pts',(2.64063225266344,-0.768337486141284,
12.5216901060418));
#445456=CARTESIAN_POINT('Ctrl Pts',(2.64375830042182,-0.756991154919283,
12.5161920673678));
#445457=CARTESIAN_POINT('Ctrl Pts',(2.63354811132182,-0.777198365544579,
12.5042015548894));
#445458=CARTESIAN_POINT('Ctrl Pts',(2.63900405830915,-0.773791022373099,
12.4980677368513));
#445459=CARTESIAN_POINT('Ctrl Pts',(2.64091048368067,-0.767267501695844,
12.4907278922777));
#445460=CARTESIAN_POINT('Ctrl Pts',(2.62761382487369,-0.789073685290027,
12.506463626192));
#445461=CARTESIAN_POINT('Ctrl Pts',(2.63388011414934,-0.790955454949259,
12.4999376786891));
#445462=CARTESIAN_POINT('Ctrl Pts',(2.63380358053701,-0.790932471868963,
12.4906970594712));
#445463=CARTESIAN_POINT('Origin',(2.62254537567347,-0.751158939595144,12.5369868989719));
#445464=CARTESIAN_POINT('Origin',(2.62254537567347,-0.751158939595144,14.));
#445465=CARTESIAN_POINT('Origin',(2.62254537567347,-0.751158939595144,13.7435492065112));
#445466=CARTESIAN_POINT('Ctrl Pts',(2.59983366398332,-0.775267853015973,
13.793642941384));
#445467=CARTESIAN_POINT('Ctrl Pts',(2.61060576757833,-0.77433618615272,
13.8071662555867));
#445468=CARTESIAN_POINT('Ctrl Pts',(2.61164881210845,-0.757338202691648,
13.8103758687955));
#445469=CARTESIAN_POINT('Ctrl Pts',(2.61638930916283,-0.773793974488835,
13.7804579775006));
#445470=CARTESIAN_POINT('Ctrl Pts',(2.62968023755084,-0.772634278703411,
13.7901904343352));
#445471=CARTESIAN_POINT('Ctrl Pts',(2.63317701534847,-0.757271060642142,
13.7927914348263));
#445472=CARTESIAN_POINT('Ctrl Pts',(2.62613624053571,-0.772926246693739,
13.7597120340895));
#445473=CARTESIAN_POINT('Ctrl Pts',(2.64151708954274,-0.771578443371696,
13.7635825532444));
#445474=CARTESIAN_POINT('Ctrl Pts',(2.64587209244678,-0.75720590477026,
13.7651073818884));
#445475=CARTESIAN_POINT('Ctrl Pts',(2.62422756819345,-0.773096167663921,
13.7381884353898));
#445476=CARTESIAN_POINT('Ctrl Pts',(2.63924847823593,-0.771780807590837,
13.7368803041982));
#445477=CARTESIAN_POINT('Ctrl Pts',(2.64338601658193,-0.757218170001641,
13.7363986145813));
#445478=CARTESIAN_POINT('Origin',(2.60190000947439,-0.752996912276295,13.7902182540695));
#445479=CARTESIAN_POINT('Ctrl Pts',(2.56822092187241,-0.77808223290419,
13.8235227101244));
#445480=CARTESIAN_POINT('Ctrl Pts',(2.57967309555235,-0.777067143585816,
13.8358800583119));
#445481=CARTESIAN_POINT('Ctrl Pts',(2.58119603549153,-0.760565425402582,
13.8390832900376));
#445482=CARTESIAN_POINT('Ctrl Pts',(2.58010151365312,-0.777024552311795,
13.8124254819053));
#445483=CARTESIAN_POINT('Ctrl Pts',(2.59157592726744,-0.776007491427277,
13.8247886449158));
#445484=CARTESIAN_POINT('Ctrl Pts',(2.59308381934425,-0.759483356273273,
13.8279860620657));
#445485=CARTESIAN_POINT('Ctrl Pts',(2.59197678093904,-0.775967345737449,
13.8013225099955));
#445486=CARTESIAN_POINT('Ctrl Pts',(2.60346802058414,-0.774948795172976,
13.8136962257787));
#445487=CARTESIAN_POINT('Ctrl Pts',(2.60496612430866,-0.758402058028986,
13.8168830918626));
#445488=CARTESIAN_POINT('Ctrl Pts',(2.60384693089817,-0.774910594737833,
13.7902140179785));
#445489=CARTESIAN_POINT('Ctrl Pts',(2.61534993650848,-0.773891004881955,
13.802602731458));
#445490=CARTESIAN_POINT('Ctrl Pts',(2.61684316583032,-0.757321502212462,
13.8057746032558));
#445491=CARTESIAN_POINT('Origin',(2.56627398803564,-0.756168551544451,13.8235269408515));
#445492=CARTESIAN_POINT('Ctrl Pts',(2.54910729598815,-0.838595406033456,
13.8235269408515));
#445493=CARTESIAN_POINT('Ctrl Pts',(2.55813214084678,-0.84620913009391,
13.8362179249168));
#445494=CARTESIAN_POINT('Ctrl Pts',(2.54937606832253,-0.860871810544881,
13.8391868794938));
#445495=CARTESIAN_POINT('Ctrl Pts',(2.54084995577065,-0.831629179923846,
13.8400110824519));
#445496=CARTESIAN_POINT('Ctrl Pts',(2.54587973825889,-0.840348305509752,
13.8494522556837));
#445497=CARTESIAN_POINT('Ctrl Pts',(2.53585926765915,-0.849321490919388,
13.85569149686));
#445498=CARTESIAN_POINT('Ctrl Pts',(2.53378962200395,-0.816947578745872,
13.8586819406588));
#445499=CARTESIAN_POINT('Ctrl Pts',(2.53249130888095,-0.821103349031829,
13.868010383617));
#445500=CARTESIAN_POINT('Ctrl Pts',(2.52427054936054,-0.824886466754057,
13.8744918421245));
#445501=CARTESIAN_POINT('Ctrl Pts',(2.54316536839459,-0.787095160459156,
13.8587686893867));
#445502=CARTESIAN_POINT('Ctrl Pts',(2.54445207279634,-0.782976359698941,
13.8680909899357));
#445503=CARTESIAN_POINT('Ctrl Pts',(2.5398808684853,-0.775191727873839,
13.8745789365163));
#445504=CARTESIAN_POINT('Ctrl Pts',(2.55744655939933,-0.779041431171037,
13.8400379222776));
#445505=CARTESIAN_POINT('Ctrl Pts',(2.566567272192,-0.774789039836563,13.8494748685453));
#445506=CARTESIAN_POINT('Ctrl Pts',(2.56352313831086,-0.761693454543098,
13.8557104837033));
#445507=CARTESIAN_POINT('Ctrl Pts',(2.56822484263113,-0.778081884610338,
13.8235269408542));
#445508=CARTESIAN_POINT('Ctrl Pts',(2.57998580964549,-0.777034853723655,
13.8362179249195));
#445509=CARTESIAN_POINT('Ctrl Pts',(2.58124272643399,-0.760003025746507,
13.8391868794965));
#445510=CARTESIAN_POINT('Origin',(2.53492121153996,-0.855410726667589,13.8235269408515));
#445511=CARTESIAN_POINT('Ctrl Pts',(2.57644211177897,-0.861656162967016,
13.7902140241682));
#445512=CARTESIAN_POINT('Ctrl Pts',(2.58527157213118,-0.869099228550608,
13.8026027327198));
#445513=CARTESIAN_POINT('Ctrl Pts',(2.57697453300423,-0.883519251920907,
13.8057746032556));
#445514=CARTESIAN_POINT('Ctrl Pts',(2.56733348476496,-0.853971756890975,
13.8013225161807));
#445515=CARTESIAN_POINT('Ctrl Pts',(2.57615391174576,-0.861407212207343,
13.8136962270464));
#445516=CARTESIAN_POINT('Ctrl Pts',(2.5678739412118,-0.875811402336283,
13.8168830918628));
#445517=CARTESIAN_POINT('Ctrl Pts',(2.55822093093989,-0.846284037998324,
13.8124254880875));
#445518=CARTESIAN_POINT('Ctrl Pts',(2.5670284416319,-0.853708607376477,
13.8247886461868));
#445519=CARTESIAN_POINT('Ctrl Pts',(2.5587694678125,-0.868099921202852,
13.8279860620656));
#445520=CARTESIAN_POINT('Ctrl Pts',(2.54910429133106,-0.838592872173261,
13.8235227163065));
#445521=CARTESIAN_POINT('Ctrl Pts',(2.55789473129573,-0.846003050879926,
13.8358800595847));
#445522=CARTESIAN_POINT('Ctrl Pts',(2.5496609528115,-0.860384661452853,
13.8390832900376));
#445523=CARTESIAN_POINT('Origin',(2.56225904150084,-0.878474025482613,13.7902182540695));
#445524=CARTESIAN_POINT('Ctrl Pts',(2.59208118444921,-0.874849952164235,
13.7382347919292));
#445525=CARTESIAN_POINT('Ctrl Pts',(2.60363067448662,-0.884562168626437,
13.7369371795943));
#445526=CARTESIAN_POINT('Ctrl Pts',(2.59863928497826,-0.898867056175656,
13.7364597369711));
#445527=CARTESIAN_POINT('Ctrl Pts',(2.59352696491608,-0.876069670502942,
13.7595490285574));
#445528=CARTESIAN_POINT('Ctrl Pts',(2.60535136878867,-0.886014381633853,
13.7633824266926));
#445529=CARTESIAN_POINT('Ctrl Pts',(2.60064247009915,-0.900287430832924,
13.7648920890506));
#445530=CARTESIAN_POINT('Ctrl Pts',(2.58615356374644,-0.869849173791011,
13.7803806590111));
#445531=CARTESIAN_POINT('Ctrl Pts',(2.59638472462146,-0.878446861454142,
13.7901039518744));
#445532=CARTESIAN_POINT('Ctrl Pts',(2.59043216110599,-0.893043177051566,
13.7926933640892));
#445533=CARTESIAN_POINT('Ctrl Pts',(2.57333694651367,-0.859036561975015,
13.7936647693663));
#445534=CARTESIAN_POINT('Ctrl Pts',(2.58162282302282,-0.865987646956492,
13.8072068914933));
#445535=CARTESIAN_POINT('Ctrl Pts',(2.57269255057998,-0.880509854224789,
13.8104111085397));
#445536=CARTESIAN_POINT('Origin',(2.57810138055072,-0.891839263321863,13.7435492065112));
#445537=CARTESIAN_POINT('Origin',(2.57810138055072,-0.891839263321863,14.));
#445538=CARTESIAN_POINT('Origin',(2.57810138055072,-0.891839263321863,12.5369868989719));
#445539=CARTESIAN_POINT('Ctrl Pts',(2.60403363890013,-0.863718344253423,
12.506462012331));
#445540=CARTESIAN_POINT('Ctrl Pts',(2.61023978363311,-0.865776828050595,
12.4999388158272));
#445541=CARTESIAN_POINT('Ctrl Pts',(2.61016635680206,-0.865752473487739,
12.4907030323752));
#445542=CARTESIAN_POINT('Ctrl Pts',(2.60206650756118,-0.876846900055558,
12.5042014951932));
#445543=CARTESIAN_POINT('Ctrl Pts',(2.60457445515015,-0.882767313555237,
12.4980716682127));
#445544=CARTESIAN_POINT('Ctrl Pts',(2.60239010596918,-0.889198035433974,
12.4907355092743));
#445545=CARTESIAN_POINT('Ctrl Pts',(2.59622600650535,-0.878334935223942,
12.5218047446509));
#445546=CARTESIAN_POINT('Ctrl Pts',(2.60277153691815,-0.888167274851517,
12.5216906929434));
#445547=CARTESIAN_POINT('Ctrl Pts',(2.59881721519281,-0.899245816904604,
12.5161988840776));
#445548=CARTESIAN_POINT('Ctrl Pts',(2.5922580806779,-0.874999196768876,
12.5369868989719));
#445549=CARTESIAN_POINT('Ctrl Pts',(2.60399246113729,-0.884863772114773,
12.5369868989719));
#445550=CARTESIAN_POINT('Ctrl Pts',(2.59880194494944,-0.899288198384969,
12.5369868989719));
#445551=CARTESIAN_POINT('Origin',(4.912540026806E-31,-6.7038415788775E-31,
12.5));
#445552=CARTESIAN_POINT('Origin',(2.60897866247895,-0.628029139618544,12.5));
#445553=CARTESIAN_POINT('',(2.60897866247895,-0.628029139618544,12.5893111709658));
#445554=CARTESIAN_POINT('',(2.60897866247895,-0.628029139618544,13.8235269408515));
#445555=CARTESIAN_POINT('',(2.60897866247895,-0.628029139618544,12.5));
#445556=CARTESIAN_POINT('',(2.63810540102849,-0.648787410275507,13.7902182540695));
#445557=CARTESIAN_POINT('',(2.60897866247895,-0.628029139618544,13.8235269408515));
#445558=CARTESIAN_POINT('',(2.6549844169628,-0.660816878682736,13.7435492065112));
#445559=CARTESIAN_POINT('Origin',(2.59945286671001,-0.621239821352992,13.7445212918713));
#445560=CARTESIAN_POINT('',(2.6549844169628,-0.660816878682736,12.5369868989719));
#445561=CARTESIAN_POINT('',(2.6549844169628,-0.660816878682736,12.5));
#445562=CARTESIAN_POINT('Ctrl Pts',(2.6549844169628,-0.660816878682736,
12.5369868989719));
#445563=CARTESIAN_POINT('Ctrl Pts',(2.63966035006791,-0.649895603455565,
12.5544431401645));
#445564=CARTESIAN_POINT('Ctrl Pts',(2.62432532299309,-0.638966517042081,
12.5718848856037));
#445565=CARTESIAN_POINT('Ctrl Pts',(2.60897866247895,-0.628029139618544,
12.5893111709658));
#445566=CARTESIAN_POINT('Origin',(2.89411775208694,-0.519527422330528,12.5));
#445567=CARTESIAN_POINT('',(2.6787760026444,-0.556579131053022,13.7435492065112));
#445568=CARTESIAN_POINT('',(2.65834914403464,-0.560093777039152,13.7902182540695));
#445569=CARTESIAN_POINT('Origin',(2.60467089007809,-0.569329659237933,13.7418732680443));
#445570=CARTESIAN_POINT('',(2.62310018328771,-0.56615871442239,13.8235269408515));
#445571=CARTESIAN_POINT('',(2.65834914403464,-0.560093777039152,13.7902182540695));
#445572=CARTESIAN_POINT('',(2.62310018328771,-0.56615871442239,12.5893111709658));
#445573=CARTESIAN_POINT('',(2.62310018328771,-0.56615871442239,12.5));
#445574=CARTESIAN_POINT('',(2.6787760026444,-0.556579131053022,12.5369868989719));
#445575=CARTESIAN_POINT('Ctrl Pts',(2.62310018328771,-0.56615871442239,
12.5893111709658));
#445576=CARTESIAN_POINT('Ctrl Pts',(2.64167259684989,-0.562963144314128,
12.5718848856037));
#445577=CARTESIAN_POINT('Ctrl Pts',(2.66023093171096,-0.559769996587656,
12.5544431401645));
#445578=CARTESIAN_POINT('Ctrl Pts',(2.6787760026444,-0.556579131053022,
12.5369868989719));
#445579=CARTESIAN_POINT('',(2.6787760026444,-0.556579131053022,12.5));
#445580=CARTESIAN_POINT('Origin',(2.62892909479919,-0.600035910522293,12.5));
#445581=CARTESIAN_POINT('',(2.59518531992423,-0.593482451178893,13.8587068136939));
#445582=CARTESIAN_POINT('Ctrl Pts',(2.62310018328645,-0.566158714415902,
13.8235269408542));
#445583=CARTESIAN_POINT('Ctrl Pts',(2.62137326098674,-0.566455848725446,
13.8262006681044));
#445584=CARTESIAN_POINT('Ctrl Pts',(2.61963546901952,-0.566931145591292,
13.8288634856214));
#445585=CARTESIAN_POINT('Ctrl Pts',(2.61788907235351,-0.567571464390742,
13.8314912288862));
#445586=CARTESIAN_POINT('Ctrl Pts',(2.61608871752331,-0.568231567027153,
13.8342001611531));
#445587=CARTESIAN_POINT('Ctrl Pts',(2.61427704726576,-0.569067313143771,
13.8368750301949));
#445588=CARTESIAN_POINT('Ctrl Pts',(2.61245207543582,-0.570109285762259,
13.8394886372968));
#445589=CARTESIAN_POINT('Ctrl Pts',(2.61231112843463,-0.570189759835059,
13.8396904925131));
#445590=CARTESIAN_POINT('Ctrl Pts',(2.61217010959524,-0.570271484856063,
13.8398919674349));
#445591=CARTESIAN_POINT('Ctrl Pts',(2.61202902281037,-0.570354485299402,
13.8400930404591));
#445592=CARTESIAN_POINT('Ctrl Pts',(2.6098307957836,-0.571647688046562,
13.8432258934518));
#445593=CARTESIAN_POINT('Ctrl Pts',(2.6076267205433,-0.573242940132615,
13.8462331177034));
#445594=CARTESIAN_POINT('Ctrl Pts',(2.60554524192903,-0.575166358647123,
13.8489036603661));
#445595=CARTESIAN_POINT('Ctrl Pts',(2.60486415790306,-0.575795723569018,
13.849777493004));
#445596=CARTESIAN_POINT('Ctrl Pts',(2.60419644647895,-0.576460183071652,
13.85061494757));
#445597=CARTESIAN_POINT('Ctrl Pts',(2.6035473095085,-0.577160522217488,
13.8514076489583));
#445598=CARTESIAN_POINT('Ctrl Pts',(2.60217429119645,-0.578641840514945,
13.8530843267192));
#445599=CARTESIAN_POINT('Ctrl Pts',(2.6007516747693,-0.580431193640579,
13.8546805203176));
#445600=CARTESIAN_POINT('Ctrl Pts',(2.599468832228,-0.582509642064698,13.8559412814273));
#445601=CARTESIAN_POINT('Ctrl Pts',(2.5992971462924,-0.582787805869536,
13.8561100121513));
#445602=CARTESIAN_POINT('Ctrl Pts',(2.59912794021294,-0.583071074603606,
13.8562727473908));
#445603=CARTESIAN_POINT('Ctrl Pts',(2.59896163573393,-0.583359334191462,
13.8564289040185));
#445604=CARTESIAN_POINT('Ctrl Pts',(2.59820744681892,-0.584666588133763,
13.8571370725437));
#445605=CARTESIAN_POINT('Ctrl Pts',(2.59750164784465,-0.586100600040144,
13.8577210840554));
#445606=CARTESIAN_POINT('Ctrl Pts',(2.59689800482735,-0.587618589571027,
13.8581177131616));
#445607=CARTESIAN_POINT('Ctrl Pts',(2.59672799817692,-0.588046107670531,
13.8582294175695));
#445608=CARTESIAN_POINT('Ctrl Pts',(2.5965659453427,-0.588480190009253,
13.8583265086086));
#445609=CARTESIAN_POINT('Ctrl Pts',(2.59641266502776,-0.588919664052098,
13.8584082369006));
#445610=CARTESIAN_POINT('Ctrl Pts',(2.59619244231892,-0.58955107040205,
13.8585256585398));
#445611=CARTESIAN_POINT('Ctrl Pts',(2.59598789525078,-0.590201562652359,
13.8586122832068));
#445612=CARTESIAN_POINT('Ctrl Pts',(2.59580509068444,-0.59085447978121,
13.8586682984299));
#445613=CARTESIAN_POINT('Ctrl Pts',(2.5956588651522,-0.591376748762697,
13.8587131050557));
#445614=CARTESIAN_POINT('Ctrl Pts',(2.59552471051172,-0.591906274527134,
13.8587357943552));
#445615=CARTESIAN_POINT('Ctrl Pts',(2.59540310175727,-0.592443244374535,
13.8587355499465));
#445616=CARTESIAN_POINT('Ctrl Pts',(2.59532450311996,-0.592790300788972,
13.8587353919793));
#445617=CARTESIAN_POINT('Ctrl Pts',(2.59525195757008,-0.593136705290338,
13.8587257282814));
#445618=CARTESIAN_POINT('Ctrl Pts',(2.59518531992423,-0.593482451178892,
13.8587068136939));
#445619=CARTESIAN_POINT('Ctrl Pts',(2.59518531992423,-0.593482451178892,
13.8587068136939));
#445620=CARTESIAN_POINT('Ctrl Pts',(2.59496615233992,-0.594619590557335,
13.8586446046466));
#445621=CARTESIAN_POINT('Ctrl Pts',(2.59481081257847,-0.595749615152042,
13.858482427929));
#445622=CARTESIAN_POINT('Ctrl Pts',(2.59471484042457,-0.596872220929184,
13.8582284286032));
#445623=CARTESIAN_POINT('Ctrl Pts',(2.59461638415859,-0.598023883869769,
13.8579678548414));
#445624=CARTESIAN_POINT('Ctrl Pts',(2.59458169415963,-0.599170682635047,
13.857615680862));
#445625=CARTESIAN_POINT('Ctrl Pts',(2.59460245281572,-0.600267112562453,
13.8571944833187));
#445626=CARTESIAN_POINT('Ctrl Pts',(2.59465425816504,-0.60300336557997,
13.8561433417727));
#445627=CARTESIAN_POINT('Ctrl Pts',(2.59504902817911,-0.605554004057623,
13.8546163505474));
#445628=CARTESIAN_POINT('Ctrl Pts',(2.59561194759635,-0.607808585743686,
13.8528973491086));
#445629=CARTESIAN_POINT('Ctrl Pts',(2.59571478466877,-0.60822046455446,
13.8525833129072));
#445630=CARTESIAN_POINT('Ctrl Pts',(2.595823127746,-0.608622556498766,13.8522628768811));
#445631=CARTESIAN_POINT('Ctrl Pts',(2.59593579729948,-0.609014326233263,
13.851937733538));
#445632=CARTESIAN_POINT('Ctrl Pts',(2.59662385463044,-0.611406809646339,
13.8499521282529));
#445633=CARTESIAN_POINT('Ctrl Pts',(2.59754556184791,-0.613650979763354,
13.847639871647));
#445634=CARTESIAN_POINT('Ctrl Pts',(2.59857816062764,-0.615659414088125,
13.8452109780794));
#445635=CARTESIAN_POINT('Ctrl Pts',(2.59904274819237,-0.61656305026336,
13.8441181685877));
#445636=CARTESIAN_POINT('Ctrl Pts',(2.59952929793255,-0.617419495470851,
13.8430021611332));
#445637=CARTESIAN_POINT('Ctrl Pts',(2.60002525572454,-0.61822379766086,
13.8418824960098));
#445638=CARTESIAN_POINT('Ctrl Pts',(2.60119399292609,-0.620119156310212,
13.8392439765549));
#445639=CARTESIAN_POINT('Ctrl Pts',(2.60246762621868,-0.621817545075485,
13.8364981347964));
#445640=CARTESIAN_POINT('Ctrl Pts',(2.6038221462249,-0.623343986225896,
13.8336931113419));
#445641=CARTESIAN_POINT('Ctrl Pts',(2.60514136269098,-0.62483064296842,
13.8309611966328));
#445642=CARTESIAN_POINT('Ctrl Pts',(2.60653904857348,-0.626155313535347,
13.8281701127185));
#445643=CARTESIAN_POINT('Ctrl Pts',(2.60801091443559,-0.627306122843475,
13.825358068512));
#445644=CARTESIAN_POINT('Ctrl Pts',(2.60833001654297,-0.627555619543461,
13.8247484142932));
#445645=CARTESIAN_POINT('Ctrl Pts',(2.60865261780666,-0.627796771564635,
13.8241378483365));
#445646=CARTESIAN_POINT('Ctrl Pts',(2.60897866247895,-0.628029139618544,
13.8235269408515));
#445647=CARTESIAN_POINT('',(2.59544407237152,-0.592267616198399,12.5969504640361));
#445648=CARTESIAN_POINT('Origin',(2.62896130711964,-0.600043463615782,12.584524458991));
#445649=CARTESIAN_POINT('Origin',(2.62896130711964,-0.600043463615782,12.584524458991));
#445650=CARTESIAN_POINT('Ctrl Pts',(2.62310018328771,-0.56615871442239,
12.5893111709658));
#445651=CARTESIAN_POINT('Ctrl Pts',(2.61193035744025,-0.568080595037053,
12.5770542771492));
#445652=CARTESIAN_POINT('Ctrl Pts',(2.61164981429195,-0.584442898371147,
12.5737548217797));
#445653=CARTESIAN_POINT('Ctrl Pts',(2.64752484371117,-0.561956206520423,
12.5663937883685));
#445654=CARTESIAN_POINT('Ctrl Pts',(2.63634076919958,-0.563880538760725,
12.5540940315304));
#445655=CARTESIAN_POINT('Ctrl Pts',(2.6360625674199,-0.580293600604353,
12.5508374392248));
#445656=CARTESIAN_POINT('Ctrl Pts',(2.67192485995163,-0.557757938897418,
12.5434499600945));
#445657=CARTESIAN_POINT('Ctrl Pts',(2.66070442203105,-0.559688527827123,
12.5311293540533));
#445658=CARTESIAN_POINT('Ctrl Pts',(2.66045127106828,-0.576147193603881,
12.5278936106989));
#445659=CARTESIAN_POINT('Ctrl Pts',(2.69630216242177,-0.553563579406506,
12.5204817579905));
#445660=CARTESIAN_POINT('Ctrl Pts',(2.6850261910016,-0.555503723432015,
12.5081597038247));
#445661=CARTESIAN_POINT('Ctrl Pts',(2.68481779213524,-0.572003439029782,
12.5049254088044));
#445662=CARTESIAN_POINT('Ctrl Pts',(2.6787760026444,-0.556579131053022,
12.5369868989719));
#445663=CARTESIAN_POINT('Ctrl Pts',(2.67969401781028,-0.556421177496693,
12.5342545179733));
#445664=CARTESIAN_POINT('Ctrl Pts',(2.68059128256758,-0.556393373384302,
12.5314872231885));
#445665=CARTESIAN_POINT('Ctrl Pts',(2.68141898399378,-0.556553159050733,
12.5287124745063));
#445666=CARTESIAN_POINT('Ctrl Pts',(2.68216544622336,-0.556697261695773,
12.5262100684184));
#445667=CARTESIAN_POINT('Ctrl Pts',(2.68285439069847,-0.556994757658666,
12.5237004536639));
#445668=CARTESIAN_POINT('Ctrl Pts',(2.68347136718562,-0.55751161410463,
12.5212220730815));
#445669=CARTESIAN_POINT('Ctrl Pts',(2.68394371605926,-0.557907312425665,
12.5193246583486));
#445670=CARTESIAN_POINT('Ctrl Pts',(2.68437912059213,-0.558436798512218,
12.517417831369));
#445671=CARTESIAN_POINT('Ctrl Pts',(2.68471614181412,-0.559175433333651,
12.5155812248347));
#445672=CARTESIAN_POINT('Ctrl Pts',(2.68485971466618,-0.559490095737757,
12.5147988205793));
#445673=CARTESIAN_POINT('Ctrl Pts',(2.6849858306331,-0.559842919007419,
12.5140295443047));
#445674=CARTESIAN_POINT('Ctrl Pts',(2.68509183607873,-0.560240091008357,
12.5132817086137));
#445675=CARTESIAN_POINT('Ctrl Pts',(2.6852522609806,-0.560841157103569,
12.5121499604604));
#445676=CARTESIAN_POINT('Ctrl Pts',(2.68536318174522,-0.5615586176954,12.5110494206568));
#445677=CARTESIAN_POINT('Ctrl Pts',(2.68539158273191,-0.562409702589905,
12.5100666561695));
#445678=CARTESIAN_POINT('Ctrl Pts',(2.68540789051307,-0.562898393576455,
12.5095023550641));
#445679=CARTESIAN_POINT('Ctrl Pts',(2.68539652731508,-0.563436809041634,
12.5089719619137));
#445680=CARTESIAN_POINT('Ctrl Pts',(2.68535132057195,-0.564014722216191,
12.5085043804652));
#445681=CARTESIAN_POINT('Ctrl Pts',(2.68528516639196,-0.56486042286867,
12.5078201359221));
#445682=CARTESIAN_POINT('Ctrl Pts',(2.68514341510609,-0.565815139887281,
12.5072563000949));
#445683=CARTESIAN_POINT('Ctrl Pts',(2.68492730116138,-0.566812914185047,
12.5068768744332));
#445684=CARTESIAN_POINT('Ctrl Pts',(2.68477146812991,-0.567532378140754,
12.5066032824114));
#445685=CARTESIAN_POINT('Ctrl Pts',(2.68457429190157,-0.568286881921826,
12.5064197834844));
#445686=CARTESIAN_POINT('Ctrl Pts',(2.68434928417872,-0.569034945636987,
12.5063282718343));
#445687=CARTESIAN_POINT('Ctrl Pts',(2.68402084256399,-0.570126887066449,
12.5061946931565));
#445688=CARTESIAN_POINT('Ctrl Pts',(2.68362709761846,-0.571228751576195,
12.5062515701262));
#445689=CARTESIAN_POINT('Ctrl Pts',(2.68320704851426,-0.572277359400301,
12.5064436508398));
#445690=CARTESIAN_POINT('',(2.61164981429195,-0.584442898371147,12.5737548217797));
#445691=CARTESIAN_POINT('Origin',(2.62683068665506,-0.587840119926328,12.5893111709658));
#445692=CARTESIAN_POINT('Ctrl Pts',(2.68320704851426,-0.572277359400301,
12.5064436508398));
#445693=CARTESIAN_POINT('Ctrl Pts',(2.67261479927447,-0.574078648881047,
12.5164271754438));
#445694=CARTESIAN_POINT('Ctrl Pts',(2.66201831624136,-0.575880446414043,
12.5264061185523));
#445695=CARTESIAN_POINT('Ctrl Pts',(2.65141745046296,-0.577682770825561,
12.536380305637));
#445696=CARTESIAN_POINT('Ctrl Pts',(2.6381685183272,-0.57993531078918,12.5488460165097));
#445697=CARTESIAN_POINT('Ctrl Pts',(2.62491273645613,-0.582188674374818,
12.5613043021964));
#445698=CARTESIAN_POINT('Ctrl Pts',(2.61164981429195,-0.584442898371146,
12.5737548217797));
#445699=CARTESIAN_POINT('Ctrl Pts',(2.60897866247895,-0.628029139618544,
12.5893111709658));
#445700=CARTESIAN_POINT('Ctrl Pts',(2.59974886987772,-0.621451179212918,
12.5770542771492));
#445701=CARTESIAN_POINT('Ctrl Pts',(2.60659544658617,-0.606587530191557,
12.5737548217797));
#445702=CARTESIAN_POINT('Ctrl Pts',(2.6003673462585,-0.621891959772177,
12.5928319619712));
#445703=CARTESIAN_POINT('Ctrl Pts',(2.59605507181361,-0.614818226282471,
12.5821634970842));
#445704=CARTESIAN_POINT('Ctrl Pts',(2.60345307443658,-0.604359590640562,
12.5773203894503));
#445705=CARTESIAN_POINT('Ctrl Pts',(2.59202457592455,-0.607366730600327,
12.5969440695591));
#445706=CARTESIAN_POINT('Ctrl Pts',(2.59290123342859,-0.603443719744806,
12.5878292599214));
#445707=CARTESIAN_POINT('Ctrl Pts',(2.60048131500874,-0.59918148355393,
12.5813877129824));
#445708=CARTESIAN_POINT('Ctrl Pts',(2.59878046210658,-0.577524926910923,
12.596957478804));
#445709=CARTESIAN_POINT('Ctrl Pts',(2.59791036156559,-0.581418963145663,
12.5878468778671));
#445710=CARTESIAN_POINT('Ctrl Pts',(2.60290515821347,-0.588502005456986,
12.5814011370086));
#445711=CARTESIAN_POINT('Ctrl Pts',(2.61266370113927,-0.567954415895238,
12.5928371701607));
#445712=CARTESIAN_POINT('Ctrl Pts',(2.60571757709291,-0.572458461458544,
12.5821692192952));
#445713=CARTESIAN_POINT('Ctrl Pts',(2.60783977973503,-0.585088587266066,
12.5773318885715));
#445714=CARTESIAN_POINT('Ctrl Pts',(2.6231001832877,-0.566158714422335,
12.5893111709658));
#445715=CARTESIAN_POINT('Ctrl Pts',(2.61193035744023,-0.568080595036999,
12.5770542771492));
#445716=CARTESIAN_POINT('Ctrl Pts',(2.61164981429194,-0.584442898371092,
12.5737548217797));
#445717=CARTESIAN_POINT('',(2.60659544658617,-0.606587530191557,12.5737548217797));
#445718=CARTESIAN_POINT('Origin',(2.6217469391639,-0.610113472996944,12.5893111709658));
#445719=CARTESIAN_POINT('Ctrl Pts',(2.61164981429194,-0.584442898371092,
12.5737548217797));
#445720=CARTESIAN_POINT('Ctrl Pts',(2.61065715256629,-0.584580529506537,
12.5746934679442));
#445721=CARTESIAN_POINT('Ctrl Pts',(2.60958386385314,-0.584914276081746,
12.5756680099006));
#445722=CARTESIAN_POINT('Ctrl Pts',(2.60855106914081,-0.585402987397514,
12.5765688348656));
#445723=CARTESIAN_POINT('Ctrl Pts',(2.60827764817413,-0.58553236830815,
12.5768073183026));
#445724=CARTESIAN_POINT('Ctrl Pts',(2.60800701520167,-0.585672358037817,
12.5770407398754));
#445725=CARTESIAN_POINT('Ctrl Pts',(2.60774117256608,-0.585821685985655,
12.5772674179684));
#445726=CARTESIAN_POINT('Ctrl Pts',(2.6066502262765,-0.586434487503603,
12.5781976435658));
#445727=CARTESIAN_POINT('Ctrl Pts',(2.60558351328209,-0.587249190437393,
12.5790594849312));
#445728=CARTESIAN_POINT('Ctrl Pts',(2.60464236986446,-0.588249161332534,
12.5797571720116));
#445729=CARTESIAN_POINT('Ctrl Pts',(2.60402918108738,-0.588900678326468,
12.580211740231));
#445730=CARTESIAN_POINT('Ctrl Pts',(2.60345510062344,-0.58967331575842,
12.5806009430798));
#445731=CARTESIAN_POINT('Ctrl Pts',(2.60297476214117,-0.590523249642185,
12.5808812374708));
#445732=CARTESIAN_POINT('Ctrl Pts',(2.60256199203427,-0.591253624810969,
12.5811221033394));
#445733=CARTESIAN_POINT('Ctrl Pts',(2.60221009464932,-0.592056088506825,
12.581287365893));
#445734=CARTESIAN_POINT('Ctrl Pts',(2.60194656767815,-0.592888696949562,
12.581359338449));
#445735=CARTESIAN_POINT('Ctrl Pts',(2.60190994287078,-0.593004412330396,
12.5813693411482));
#445736=CARTESIAN_POINT('Ctrl Pts',(2.60187496511642,-0.59312071195575,
12.5813775999465));
#445737=CARTESIAN_POINT('Ctrl Pts',(2.60184164696784,-0.59323748635646,
12.5813841266931));
#445738=CARTESIAN_POINT('Ctrl Pts',(2.60178511869904,-0.593435608250835,
12.5813952001081));
#445739=CARTESIAN_POINT('Ctrl Pts',(2.60173357454906,-0.593636590779214,
12.5814007534795));
#445740=CARTESIAN_POINT('Ctrl Pts',(2.60168722799472,-0.593840395398267,
12.5814005856065));
#445741=CARTESIAN_POINT('Ctrl Pts',(2.60147507158928,-0.594773333261852,
12.5813998171494));
#445742=CARTESIAN_POINT('Ctrl Pts',(2.60138615750586,-0.595700872957205,
12.58127954464));
#445743=CARTESIAN_POINT('Ctrl Pts',(2.60139153620305,-0.596614925021774,
12.5810700125799));
#445744=CARTESIAN_POINT('Ctrl Pts',(2.60139803305684,-0.597718995842614,
12.5808169217085));
#445745=CARTESIAN_POINT('Ctrl Pts',(2.60155883834059,-0.598803389691812,
12.5804173076348));
#445746=CARTESIAN_POINT('Ctrl Pts',(2.6018340986878,-0.599776892187396,
12.5799304713245));
#445747=CARTESIAN_POINT('Ctrl Pts',(2.60217523297394,-0.600983368464338,
12.5793271277669));
#445748=CARTESIAN_POINT('Ctrl Pts',(2.60268233466224,-0.602103127673329,
12.5785808224116));
#445749=CARTESIAN_POINT('Ctrl Pts',(2.603305136233,-0.60310205413031,12.5777485681082));
#445750=CARTESIAN_POINT('Ctrl Pts',(2.60423317880645,-0.604590563991775,
12.576508418016));
#445751=CARTESIAN_POINT('Ctrl Pts',(2.60540447847364,-0.605801875925339,
12.5750928681475));
#445752=CARTESIAN_POINT('Ctrl Pts',(2.60659544658617,-0.606587530191557,
12.5737548217797));
#445753=CARTESIAN_POINT('Ctrl Pts',(2.60659544658617,-0.606587530191557,
12.5737548217797));
#445754=CARTESIAN_POINT('Ctrl Pts',(2.59974886987772,-0.621451179212918,
12.5770542771492));
#445755=CARTESIAN_POINT('Ctrl Pts',(2.60897866247895,-0.628029139618544,
12.5893111709658));
#445756=CARTESIAN_POINT('Ctrl Pts',(2.62678723035326,-0.620916061954205,
12.5508408821982));
#445757=CARTESIAN_POINT('Ctrl Pts',(2.6199165217402,-0.635824418261484,
12.55409748406));
#445758=CARTESIAN_POINT('Ctrl Pts',(2.62915808919293,-0.642410770459861,
12.5663972313419));
#445759=CARTESIAN_POINT('Ctrl Pts',(2.64695860668738,-0.635231558472971,
12.52790050457));
#445760=CARTESIAN_POINT('Ctrl Pts',(2.64004554774912,-0.650170129136117,
12.5311362602938));
#445761=CARTESIAN_POINT('Ctrl Pts',(2.64931715818131,-0.656777892598899,
12.5434568539655));
#445762=CARTESIAN_POINT('Ctrl Pts',(2.66711115349385,-0.649535044047112,
12.5049357605811));
#445763=CARTESIAN_POINT('Ctrl Pts',(2.66013997445222,-0.664491181508331,
12.5081700652078));
#445764=CARTESIAN_POINT('Ctrl Pts',(2.66945746386522,-0.671131642360113,
12.5204921097672));
#445765=CARTESIAN_POINT('Ctrl Pts',(2.66578785735636,-0.648595822410635,
12.5064436508395));
#445766=CARTESIAN_POINT('Ctrl Pts',(2.66570519898163,-0.649813202952483,
12.5062361689309));
#445767=CARTESIAN_POINT('Ctrl Pts',(2.66556732922572,-0.651075654357824,
12.5061871075061));
#445768=CARTESIAN_POINT('Ctrl Pts',(2.6653654124191,-0.652288191468314,
12.5063648335164));
#445769=CARTESIAN_POINT('Ctrl Pts',(2.66527368935078,-0.65283900061629,
12.5064455676329));
#445770=CARTESIAN_POINT('Ctrl Pts',(2.66516725327026,-0.653387156218686,
12.506574497099));
#445771=CARTESIAN_POINT('Ctrl Pts',(2.66504963615673,-0.65390895468463,
12.5067492519495));
#445772=CARTESIAN_POINT('Ctrl Pts',(2.6648132800015,-0.654957528956749,
12.5071004286051));
#445773=CARTESIAN_POINT('Ctrl Pts',(2.66452229370529,-0.655938041245078,
12.5076537929613));
#445774=CARTESIAN_POINT('Ctrl Pts',(2.66420758488729,-0.65677958994019,
12.5083435010505));
#445775=CARTESIAN_POINT('Ctrl Pts',(2.66418777208649,-0.656832570459665,
12.5083869222964));
#445776=CARTESIAN_POINT('Ctrl Pts',(2.66416785192314,-0.656885001800406,
12.5084308732337));
#445777=CARTESIAN_POINT('Ctrl Pts',(2.66414782672464,-0.656936867313813,
12.5084753333615));
#445778=CARTESIAN_POINT('Ctrl Pts',(2.66398719820184,-0.657352897187647,
12.5088319622689));
#445779=CARTESIAN_POINT('Ctrl Pts',(2.66381775402414,-0.657741431599982,
12.509227847131));
#445780=CARTESIAN_POINT('Ctrl Pts',(2.66364709924657,-0.658092036718835,
12.5096423454524));
#445781=CARTESIAN_POINT('Ctrl Pts',(2.66311234270232,-0.659190677989998,
12.5109411997424));
#445782=CARTESIAN_POINT('Ctrl Pts',(2.66254150158836,-0.659988689589087,
12.5124831113042));
#445783=CARTESIAN_POINT('Ctrl Pts',(2.66198293764026,-0.660567416460211,
12.5140723025008));
#445784=CARTESIAN_POINT('Ctrl Pts',(2.66193059958655,-0.660621643801897,
12.5142212114565));
#445785=CARTESIAN_POINT('Ctrl Pts',(2.66187837454269,-0.660673974991074,
12.5143705582413));
#445786=CARTESIAN_POINT('Ctrl Pts',(2.6618263067976,-0.66072449332381,12.5145201959299));
#445787=CARTESIAN_POINT('Ctrl Pts',(2.66115741909112,-0.661373476521739,
12.5164425148273));
#445788=CARTESIAN_POINT('Ctrl Pts',(2.66049904977585,-0.661753223311166,
12.5184635205941));
#445789=CARTESIAN_POINT('Ctrl Pts',(2.65985024793994,-0.661953939425375,
12.5205025929158));
#445790=CARTESIAN_POINT('Ctrl Pts',(2.65947391715901,-0.662070362727258,
12.5216853356836));
#445791=CARTESIAN_POINT('Ctrl Pts',(2.65910162803627,-0.662126803524878,
12.5228750347131));
#445792=CARTESIAN_POINT('Ctrl Pts',(2.65873911193257,-0.662140584784227,
12.5240609649613));
#445793=CARTESIAN_POINT('Ctrl Pts',(2.65784933560436,-0.662174410145961,
12.5269717671326));
#445794=CARTESIAN_POINT('Ctrl Pts',(2.65699299812196,-0.661941805106474,
12.5299036066169));
#445795=CARTESIAN_POINT('Ctrl Pts',(2.6561611254874,-0.66152896125462,12.5328133004019));
#445796=CARTESIAN_POINT('Ctrl Pts',(2.65576177818431,-0.66133077216655,
12.5342101228451));
#445797=CARTESIAN_POINT('Ctrl Pts',(2.65536880019935,-0.661090823817926,
12.5356023438238));
#445798=CARTESIAN_POINT('Ctrl Pts',(2.6549844169628,-0.660816878682735,
12.5369868989719));
#445799=CARTESIAN_POINT('Origin',(13.0312014533464,-8.06232477624549,-1.24024740340327));
#445800=CARTESIAN_POINT('Ctrl Pts',(2.6787348069087,-0.556586178910241,
12.5369868989719));
#445801=CARTESIAN_POINT('Ctrl Pts',(2.6938565361228,-0.554013901852757,
12.5369868989719));
#445802=CARTESIAN_POINT('Ctrl Pts',(2.69667178506096,-0.538935517420025,
12.5369868989719));
#445803=CARTESIAN_POINT('Ctrl Pts',(2.68384653168693,-0.555716583389367,
12.5218025310016));
#445804=CARTESIAN_POINT('Ctrl Pts',(2.69447240469724,-0.55054486351365,
12.5216901060418));
#445805=CARTESIAN_POINT('Ctrl Pts',(2.6966632194608,-0.538981484359688,
12.5161920673677));
#445806=CARTESIAN_POINT('Ctrl Pts',(2.68813407918327,-0.559953682356989,
12.5042015548895));
#445807=CARTESIAN_POINT('Ctrl Pts',(2.69329414185644,-0.556112966508837,
12.4980677368513));
#445808=CARTESIAN_POINT('Ctrl Pts',(2.69466249625818,-0.549455760942315,
12.4907278922778));
#445809=CARTESIAN_POINT('Ctrl Pts',(2.68318748738815,-0.572273187392411,
12.506463626192));
#445810=CARTESIAN_POINT('Ctrl Pts',(2.68958630779988,-0.573637934868978,
12.4999376786891));
#445811=CARTESIAN_POINT('Ctrl Pts',(2.68950815551243,-0.573621266462893,
12.4906970594712));
#445812=CARTESIAN_POINT('Origin',(2.67504549927705,-0.534897725549083,12.5369868989719));
#445813=CARTESIAN_POINT('Origin',(2.67504549927706,-0.534897725549084,14.));
#445814=CARTESIAN_POINT('Origin',(2.67504549927706,-0.534897725549084,13.7435492065112));
#445815=CARTESIAN_POINT('Ctrl Pts',(2.654374459194,-0.560777633897341,13.793642941384));
#445816=CARTESIAN_POINT('Ctrl Pts',(2.66503478000441,-0.558971040632395,
13.8071662555867));
#445817=CARTESIAN_POINT('Ctrl Pts',(2.66468886043623,-0.541944598746695,
13.8103758687955));
#445818=CARTESIAN_POINT('Ctrl Pts',(2.67075488204713,-0.557959220802175,
13.7804579775006));
#445819=CARTESIAN_POINT('Ctrl Pts',(2.68390705999472,-0.555720049758236,
13.7901904343351));
#445820=CARTESIAN_POINT('Ctrl Pts',(2.68613995765557,-0.540122931684682,
13.7927914348263));
#445821=CARTESIAN_POINT('Ctrl Pts',(2.68039865343904,-0.55629991490675,
13.7597120340895));
#445822=CARTESIAN_POINT('Ctrl Pts',(2.6956184654567,-0.553702914306182,
13.7635825532445));
#445823=CARTESIAN_POINT('Ctrl Pts',(2.69878748212368,-0.539023225974718,
13.7651073818884));
#445824=CARTESIAN_POINT('Ctrl Pts',(2.67851018218309,-0.556624844994064,
13.7381884353898));
#445825=CARTESIAN_POINT('Ctrl Pts',(2.69337389732938,-0.554089518057324,
13.7368803041982));
#445826=CARTESIAN_POINT('Ctrl Pts',(2.6963106782014,-0.539238088657145,
13.7363986145813));
#445827=CARTESIAN_POINT('Origin',(2.6546186406673,-0.538412371535213,13.7902182540695));
#445828=CARTESIAN_POINT('Ctrl Pts',(2.62309630396294,-0.566159381129065,
13.8235227101244));
#445829=CARTESIAN_POINT('Ctrl Pts',(2.6344276322766,-0.564214210964931,
13.8358800583119));
#445830=CARTESIAN_POINT('Ctrl Pts',(2.63460046153234,-0.547643267144351,
13.8390832900376));
#445831=CARTESIAN_POINT('Ctrl Pts',(2.63485115326723,-0.564136841357434,
13.8124254819052));
#445832=CARTESIAN_POINT('Ctrl Pts',(2.64620448681279,-0.562187893426261,
13.8247886449157));
#445833=CARTESIAN_POINT('Ctrl Pts',(2.6463604910855,-0.545595833766022,
13.8279860620657));
#445834=CARTESIAN_POINT('Ctrl Pts',(2.64660073443048,-0.562115208022343,
13.8013225099955));
#445835=CARTESIAN_POINT('Ctrl Pts',(2.65797071659684,-0.560163403890322,
13.8136962257787));
#445836=CARTESIAN_POINT('Ctrl Pts',(2.65811512281515,-0.543549615287902,
13.8168830918626));
#445837=CARTESIAN_POINT('Ctrl Pts',(2.65834525242799,-0.560094445855734,
13.7902140179785));
#445838=CARTESIAN_POINT('Ctrl Pts',(2.66972687669737,-0.558140646855038,
13.802602731458));
#445839=CARTESIAN_POINT('Ctrl Pts',(2.66986456913051,-0.541504565786618,
13.8057746032558));
#445840=CARTESIAN_POINT('Origin',(2.61936967992036,-0.544477308918452,13.8235269408515));
#445841=CARTESIAN_POINT('Ctrl Pts',(2.60897866247895,-0.628029139618544,
13.8235269408515));
#445842=CARTESIAN_POINT('Ctrl Pts',(2.6185940671041,-0.634881921001724,
13.8362179249168));
#445843=CARTESIAN_POINT('Ctrl Pts',(2.61106227426729,-0.650209513791218,
13.8391868794938));
#445844=CARTESIAN_POINT('Ctrl Pts',(2.60018098578061,-0.621759142936774,
13.8400110824519));
#445845=CARTESIAN_POINT('Ctrl Pts',(2.60590472176222,-0.63003928238457,
13.8494522556837));
#445846=CARTESIAN_POINT('Ctrl Pts',(2.59664899136563,-0.639799371639376,
13.85569149686));
#445847=CARTESIAN_POINT('Ctrl Pts',(2.59194745789874,-0.607701876322504,
13.8586819406588));
#445848=CARTESIAN_POINT('Ctrl Pts',(2.59099219866414,-0.611949643198133,
13.868010383617));
#445849=CARTESIAN_POINT('Ctrl Pts',(2.583107152258,-0.616390241126949,13.8744918421245));
#445850=CARTESIAN_POINT('Ctrl Pts',(2.59885875804002,-0.57718457912396,
13.8587686893867));
#445851=CARTESIAN_POINT('Ctrl Pts',(2.59980546053999,-0.572974604979576,
13.8680909899357));
#445852=CARTESIAN_POINT('Ctrl Pts',(2.59461494677144,-0.565588471463025,
13.8745789365162));
#445853=CARTESIAN_POINT('Ctrl Pts',(2.61243597585564,-0.56799359830867,
13.8400379222776));
#445854=CARTESIAN_POINT('Ctrl Pts',(2.62117973085788,-0.563011933690384,
13.8494748685453));
#445855=CARTESIAN_POINT('Ctrl Pts',(2.6170783143062,-0.550208048048356,
13.8557104837033));
#445856=CARTESIAN_POINT('Ctrl Pts',(2.62310018328645,-0.566158714415902,
13.8235269408542));
#445857=CARTESIAN_POINT('Ctrl Pts',(2.63473667391585,-0.564156539442959,
13.8362179249195));
#445858=CARTESIAN_POINT('Ctrl Pts',(2.63460115632152,-0.547078933081472,
13.8391868794965));
#445859=CARTESIAN_POINT('Origin',(2.59621038579399,-0.645944806240145,13.8235269408515));
#445860=CARTESIAN_POINT('Ctrl Pts',(2.63810218970091,-0.648785122534795,
13.7902140241682));
#445861=CARTESIAN_POINT('Ctrl Pts',(2.64750894969526,-0.65548373894426,
13.8026027327198));
#445862=CARTESIAN_POINT('Ctrl Pts',(2.64041488405521,-0.670532066591146,
13.8057746032556));
#445863=CARTESIAN_POINT('Ctrl Pts',(2.62839752045813,-0.641868723348059,
13.8013225161808));
#445864=CARTESIAN_POINT('Ctrl Pts',(2.63779465683145,-0.648560491116481,
13.8136962270464));
#445865=CARTESIAN_POINT('Ctrl Pts',(2.63071631243388,-0.663591646957016,
13.8168830918628));
#445866=CARTESIAN_POINT('Ctrl Pts',(2.61868866744511,-0.634949342439386,
13.8124254880875));
#445867=CARTESIAN_POINT('Ctrl Pts',(2.62807204320249,-0.641631313289075,
13.8247886461867));
#445868=CARTESIAN_POINT('Ctrl Pts',(2.62101357611648,-0.656647924244738,
13.8279860620656));
#445869=CARTESIAN_POINT('Ctrl Pts',(2.60897546128649,-0.628026859097017,
13.8235227163066));
#445870=CARTESIAN_POINT('Ctrl Pts',(2.61834065014465,-0.634695878581757,
13.8358800595847));
#445871=CARTESIAN_POINT('Ctrl Pts',(2.61130650365315,-0.649700764917019,
13.8390832900376));
#445872=CARTESIAN_POINT('Origin',(2.62533712434353,-0.666703076897107,13.7902182540695));
#445873=CARTESIAN_POINT('Ctrl Pts',(2.65476464095167,-0.660660280878158,
13.7382347919292));
#445874=CARTESIAN_POINT('Ctrl Pts',(2.66706733681926,-0.669398790083003,
13.7369371795943));
#445875=CARTESIAN_POINT('Ctrl Pts',(2.66325853688308,-0.684062923881726,
13.7364597369711));
#445876=CARTESIAN_POINT('Ctrl Pts',(2.65630502907124,-0.661758096174705,
13.7595490285574));
#445877=CARTESIAN_POINT('Ctrl Pts',(2.66890067449476,-0.670705918411684,
13.7633824266926));
#445878=CARTESIAN_POINT('Ctrl Pts',(2.66537083029141,-0.68531529417547,
13.7648920890506));
#445879=CARTESIAN_POINT('Ctrl Pts',(2.64844913405539,-0.656159298299035,
13.780380659011));
#445880=CARTESIAN_POINT('Ctrl Pts',(2.65934704294824,-0.663894443272945,
13.7901039518744));
#445881=CARTESIAN_POINT('Ctrl Pts',(2.6546040213236,-0.67892738002177,13.7926933640891));
#445882=CARTESIAN_POINT('Ctrl Pts',(2.63479383481681,-0.646427337845055,
13.7936647693663));
#445883=CARTESIAN_POINT('Ctrl Pts',(2.64361871871215,-0.652679917806856,
13.8072068914933));
#445884=CARTESIAN_POINT('Ctrl Pts',(2.6359018557241,-0.667881703737182,
13.8104111085397));
#445885=CARTESIAN_POINT('Origin',(2.64221614027784,-0.678732545304336,13.7435492065112));
#445886=CARTESIAN_POINT('Origin',(2.64221614027784,-0.678732545304336,14.));
#445887=CARTESIAN_POINT('Origin',(2.64221614027784,-0.678732545304336,12.5369868989719));
#445888=CARTESIAN_POINT('Ctrl Pts',(2.6657699952109,-0.648591476475466,
12.506462012331));
#445889=CARTESIAN_POINT('Ctrl Pts',(2.67212327504875,-0.650137252426841,
12.4999388158272));
#445890=CARTESIAN_POINT('Ctrl Pts',(2.67204810741645,-0.650118963870176,
12.4907030323752));
#445891=CARTESIAN_POINT('Ctrl Pts',(2.66487950851664,-0.661836687557277,
12.5042014951932));
#445892=CARTESIAN_POINT('Ctrl Pts',(2.66786167977953,-0.667532980358285,
12.4980716682127));
#445893=CARTESIAN_POINT('Ctrl Pts',(2.66620876237332,-0.674120349277227,
12.4907355092743));
#445894=CARTESIAN_POINT('Ctrl Pts',(2.65917972992674,-0.663795826468017,
12.5218047446509));
#445895=CARTESIAN_POINT('Ctrl Pts',(2.6665049075857,-0.673061928302202,
12.5216906929434));
#445896=CARTESIAN_POINT('Ctrl Pts',(2.66346674756517,-0.684425921351274,
12.5161988840776));
#445897=CARTESIAN_POINT('Ctrl Pts',(2.65495311339357,-0.66079461019884,
12.5369868989719));
#445898=CARTESIAN_POINT('Ctrl Pts',(2.66745250313894,-0.66966990103993,
12.5369868989719));
#445899=CARTESIAN_POINT('Ctrl Pts',(2.66345498261638,-0.684469406477355,
12.5369868989719));
#445900=CARTESIAN_POINT('Origin',(5.0226946496705E-31,-6.29825987887742E-31,
12.5));
#445901=CARTESIAN_POINT('Origin',(2.65148770642212,-0.413283442896987,12.5));
#445902=CARTESIAN_POINT('',(2.65148770642212,-0.413283442896987,12.5893111709658));
#445903=CARTESIAN_POINT('',(2.65148770642212,-0.413283442896987,13.8235269408515));
#445904=CARTESIAN_POINT('',(2.65148770642212,-0.413283442896987,12.5));
#445905=CARTESIAN_POINT('',(2.68220951992086,-0.431598542529539,13.7902182540695));
#445906=CARTESIAN_POINT('',(2.65148770642212,-0.413283442896987,13.8235269408515));
#445907=CARTESIAN_POINT('',(2.70001288567339,-0.442212187377219,13.7435492065112));
#445908=CARTESIAN_POINT('Origin',(2.64144021448603,-0.407293156316728,13.7445212918719));
#445909=CARTESIAN_POINT('',(2.70001288567339,-0.442212187377219,12.5369868989719));
#445910=CARTESIAN_POINT('',(2.70001288567339,-0.442212187377219,12.5));
#445911=CARTESIAN_POINT('Ctrl Pts',(2.70001288567339,-0.442212187377219,
12.5369868989719));
#445912=CARTESIAN_POINT('Ctrl Pts',(2.68384962302776,-0.432576305506054,
12.5544431401645));
#445913=CARTESIAN_POINT('Ctrl Pts',(2.66767479998709,-0.422933531796069,
12.5718848856037));
#445914=CARTESIAN_POINT('Ctrl Pts',(2.65148770642212,-0.413283442896987,
12.5893111709658));
#445915=CARTESIAN_POINT('Origin',(2.92683412199199,-0.281901273217275,12.5));
#445916=CARTESIAN_POINT('',(2.71522896268845,-0.336382047150378,13.7435492065112));
#445917=CARTESIAN_POINT('',(2.69515654904187,-0.341549977052325,13.7902182540695));
#445918=CARTESIAN_POINT('Origin',(2.6424097151889,-0.355130403636861,13.7418732680445));
#445919=CARTESIAN_POINT('',(2.66051922500485,-0.350467851393004,13.8235269408515));
#445920=CARTESIAN_POINT('',(2.69515654904187,-0.341549977052325,13.7902182540695));
#445921=CARTESIAN_POINT('',(2.66051922500485,-0.350467851393004,12.5893111709658));
#445922=CARTESIAN_POINT('',(2.66051922500485,-0.350467851393004,12.5));
#445923=CARTESIAN_POINT('',(2.71522896268845,-0.336382047150378,12.5369868989719));
#445924=CARTESIAN_POINT('Ctrl Pts',(2.66051922500485,-0.350467851393004,
12.5893111709658));
#445925=CARTESIAN_POINT('Ctrl Pts',(2.67876937176296,-0.345769090157469,
12.5718848856037));
#445926=CARTESIAN_POINT('Ctrl Pts',(2.6970056841123,-0.341073890788288,
12.5544431401645));
#445927=CARTESIAN_POINT('Ctrl Pts',(2.71522896268845,-0.336382047150378,
12.5369868989719));
#445928=CARTESIAN_POINT('',(2.71522896268845,-0.336382047150378,12.5));
#445929=CARTESIAN_POINT('Origin',(2.66909004727682,-0.383757213516397,12.5));
#445930=CARTESIAN_POINT('',(2.63492438425327,-0.379975991182365,13.8587068136939));
#445931=CARTESIAN_POINT('Ctrl Pts',(2.66051922500306,-0.35046785138664,
13.8235269408542));
#445932=CARTESIAN_POINT('Ctrl Pts',(2.65882226809953,-0.350904757205673,
13.8262006681044));
#445933=CARTESIAN_POINT('Ctrl Pts',(2.65712899959872,-0.351520118738613,
13.8288634856214));
#445934=CARTESIAN_POINT('Ctrl Pts',(2.65544060585013,-0.352300654471122,
13.8314912288862));
#445935=CARTESIAN_POINT('Ctrl Pts',(2.65370004604506,-0.35310530630281,
13.8342001611531));
#445936=CARTESIAN_POINT('Ctrl Pts',(2.65196252503803,-0.354085939487892,
13.8368750301949));
#445937=CARTESIAN_POINT('Ctrl Pts',(2.65022855609291,-0.355273197174807,
13.8394886372969));
#445938=CARTESIAN_POINT('Ctrl Pts',(2.65009463746527,-0.355364891965846,
13.8396904925131));
#445939=CARTESIAN_POINT('Ctrl Pts',(2.64996074920235,-0.355457839398141,
13.8398919674349));
#445940=CARTESIAN_POINT('Ctrl Pts',(2.6498268971788,-0.355552063547096,
13.8400930404591));
#445941=CARTESIAN_POINT('Ctrl Pts',(2.64774139260054,-0.35702013917882,
13.8432258934518));
#445942=CARTESIAN_POINT('Ctrl Pts',(2.64567467909338,-0.358789735788876,
13.8462331177034));
#445943=CARTESIAN_POINT('Ctrl Pts',(2.64375690289258,-0.360876414117512,
13.8489036603661));
#445944=CARTESIAN_POINT('Ctrl Pts',(2.64312938420138,-0.361559199550543,
13.849777493004));
#445945=CARTESIAN_POINT('Ctrl Pts',(2.64251805414996,-0.362275872798793,
13.85061494757));
#445946=CARTESIAN_POINT('Ctrl Pts',(2.64192816127125,-0.363026792313282,
13.8514076489583));
#445947=CARTESIAN_POINT('Ctrl Pts',(2.64068045275748,-0.36461509538524,
13.8530843267192));
#445948=CARTESIAN_POINT('Ctrl Pts',(2.63940841886039,-0.366514451031733,
13.8546805203176));
#445949=CARTESIAN_POINT('Ctrl Pts',(2.63829925771375,-0.368690547166666,
13.8559412814274));
#445950=CARTESIAN_POINT('Ctrl Pts',(2.63815081598139,-0.368981779401964,
13.8561100121513));
#445951=CARTESIAN_POINT('Ctrl Pts',(2.63800526195279,-0.369277897448965,
13.8562727473908));
#445952=CARTESIAN_POINT('Ctrl Pts',(2.63786300667071,-0.369578753235722,
13.8564289040185));
#445953=CARTESIAN_POINT('Ctrl Pts',(2.63721788058935,-0.370943130796488,
13.8571370725437));
#445954=CARTESIAN_POINT('Ctrl Pts',(2.63663131538603,-0.372429900315262,
13.8577210840553));
#445955=CARTESIAN_POINT('Ctrl Pts',(2.63615341118017,-0.373992041371059,
13.8581177131616));
#445956=CARTESIAN_POINT('Ctrl Pts',(2.63601881690684,-0.374431994059635,
13.8582294175695));
#445957=CARTESIAN_POINT('Ctrl Pts',(2.63589268503048,-0.374877840835603,
13.8583265086086));
#445958=CARTESIAN_POINT('Ctrl Pts',(2.63577573595751,-0.375328346333484,
13.8584082369006));
#445959=CARTESIAN_POINT('Ctrl Pts',(2.63560771150078,-0.375975601926112,
13.8585256585398));
#445960=CARTESIAN_POINT('Ctrl Pts',(2.63545686620342,-0.376640602202095,
13.8586122832068));
#445961=CARTESIAN_POINT('Ctrl Pts',(2.63532788871157,-0.377306247072293,
13.8586682984299));
#445962=CARTESIAN_POINT('Ctrl Pts',(2.63522471950323,-0.377838696985198,
13.8587131050557));
#445963=CARTESIAN_POINT('Ctrl Pts',(2.63513417251693,-0.378377395644967,
13.8587357943552));
#445964=CARTESIAN_POINT('Ctrl Pts',(2.63505673643312,-0.378922491011946,
13.8587355499465));
#445965=CARTESIAN_POINT('Ctrl Pts',(2.63500668764599,-0.37927479914334,
13.8587353919793));
#445966=CARTESIAN_POINT('Ctrl Pts',(2.63496261866818,-0.379625964148031,
13.8587257282814));
#445967=CARTESIAN_POINT('Ctrl Pts',(2.63492438425327,-0.379975991182365,
13.8587068136939));
#445968=CARTESIAN_POINT('Ctrl Pts',(2.63492438425327,-0.379975991182365,
13.8587068136939));
#445969=CARTESIAN_POINT('Ctrl Pts',(2.63479863334703,-0.381127211016178,
13.8586446046466));
#445970=CARTESIAN_POINT('Ctrl Pts',(2.63473591796092,-0.382266137179996,
13.858482427929));
#445971=CARTESIAN_POINT('Ctrl Pts',(2.63473176793904,-0.383392830200595,
13.8582284286032));
#445972=CARTESIAN_POINT('Ctrl Pts',(2.63472751049935,-0.384548686177452,
13.8579678548414));
#445973=CARTESIAN_POINT('Ctrl Pts',(2.63478641067422,-0.385694496621405,
13.857615680862));
#445974=CARTESIAN_POINT('Ctrl Pts',(2.63489646947545,-0.38678558624549,
13.8571944833187));
#445975=CARTESIAN_POINT('Ctrl Pts',(2.6351711324698,-0.389508511989885,
13.8561433417727));
#445976=CARTESIAN_POINT('Ctrl Pts',(2.6357724896341,-0.392018486007384,
13.8546163505474));
#445977=CARTESIAN_POINT('Ctrl Pts',(2.63651730532133,-0.394219682600469,
13.8528973491086));
#445978=CARTESIAN_POINT('Ctrl Pts',(2.63665337215866,-0.394621808742403,
13.8525833129072));
#445979=CARTESIAN_POINT('Ctrl Pts',(2.63679412895954,-0.395013731792354,
13.8522628768812));
#445980=CARTESIAN_POINT('Ctrl Pts',(2.63693835648476,-0.395395014330815,
13.851937733538));
#445981=CARTESIAN_POINT('Ctrl Pts',(2.63781913397061,-0.397723453892613,
13.8499521282529));
#445982=CARTESIAN_POINT('Ctrl Pts',(2.63892069498174,-0.399885029023759,
13.847639871647));
#445983=CARTESIAN_POINT('Ctrl Pts',(2.64011356391708,-0.40180261406227,
13.8452109780794));
#445984=CARTESIAN_POINT('Ctrl Pts',(2.64065026034225,-0.402665375263132,
13.8441181685877));
#445985=CARTESIAN_POINT('Ctrl Pts',(2.64120499936357,-0.403479312399116,
13.8430021611332));
#445986=CARTESIAN_POINT('Ctrl Pts',(2.64176486499218,-0.404240513175644,
13.8418824960098));
#445987=CARTESIAN_POINT('Ctrl Pts',(2.64308420264268,-0.406034302243487,
13.8392439765549));
#445988=CARTESIAN_POINT('Ctrl Pts',(2.64449203247698,-0.407623226823063,
13.8364981347964));
#445989=CARTESIAN_POINT('Ctrl Pts',(2.64596646455416,-0.409034182911206,
13.8336931113419));
#445990=CARTESIAN_POINT('Ctrl Pts',(2.64740246776224,-0.41040836453706,
13.8309611966328));
#445991=CARTESIAN_POINT('Ctrl Pts',(2.64890347590911,-0.411614702997043,
13.8281701127186));
#445992=CARTESIAN_POINT('Ctrl Pts',(2.65046424590118,-0.412641712350236,
13.8253580685121));
#445993=CARTESIAN_POINT('Ctrl Pts',(2.6508026225199,-0.412864369086392,
13.8247484142933));
#445994=CARTESIAN_POINT('Ctrl Pts',(2.65114380648299,-0.413078423696242,
13.8241378483365));
#445995=CARTESIAN_POINT('Ctrl Pts',(2.65148770642212,-0.413283442896987,
13.8235269408515));
#445996=CARTESIAN_POINT('',(2.63508325539423,-0.378744107738709,12.5969504640361));
#445997=CARTESIAN_POINT('Origin',(2.66912276806067,-0.383762115874432,12.584524458991));
#445998=CARTESIAN_POINT('Origin',(2.66912276806067,-0.383762115874432,12.584524458991));
#445999=CARTESIAN_POINT('Ctrl Pts',(2.66051922500485,-0.350467851393004,
12.5893111709658));
#446000=CARTESIAN_POINT('Ctrl Pts',(2.64954321694341,-0.353293781610638,
12.5770542771492));
#446001=CARTESIAN_POINT('Ctrl Pts',(2.65059728690124,-0.369624507601204,
12.5737548217797));
#446002=CARTESIAN_POINT('Ctrl Pts',(2.68452007097744,-0.344288490417406,
12.5663937883685));
#446003=CARTESIAN_POINT('Ctrl Pts',(2.67353006149338,-0.347118025501498,
12.5540940315304));
#446004=CARTESIAN_POINT('Ctrl Pts',(2.67459060231887,-0.363499150263564,
12.5508374392248));
#446005=CARTESIAN_POINT('Ctrl Pts',(2.70849670039065,-0.338115364341283,
12.5434499600945));
#446006=CARTESIAN_POINT('Ctrl Pts',(2.69747095847214,-0.340954099251498,
12.5311293540533));
#446007=CARTESIAN_POINT('Ctrl Pts',(2.69856018390388,-0.357378634329323,
12.5278936106989));
#446008=CARTESIAN_POINT('Ctrl Pts',(2.73245101016076,-0.331947984776416,
12.5204817579905));
#446009=CARTESIAN_POINT('Ctrl Pts',(2.72137069835478,-0.334800769484485,
12.5081597038247));
#446010=CARTESIAN_POINT('Ctrl Pts',(2.72250787291556,-0.351262570082021,
12.5049254088044));
#446011=CARTESIAN_POINT('Ctrl Pts',(2.71522896268845,-0.336382047150378,
12.5369868989719));
#446012=CARTESIAN_POINT('Ctrl Pts',(2.71613104855338,-0.336149792413019,
12.5342545179733));
#446013=CARTESIAN_POINT('Ctrl Pts',(2.71702306144293,-0.336048945408998,
12.5314872231885));
#446014=CARTESIAN_POINT('Ctrl Pts',(2.71786103277611,-0.336140734051564,
12.5287124745063));
#446015=CARTESIAN_POINT('Ctrl Pts',(2.71861675691755,-0.336223513605412,
12.5262100684184));
#446016=CARTESIAN_POINT('Ctrl Pts',(2.71932765766955,-0.336463864304461,
12.5237004536639));
#446017=CARTESIAN_POINT('Ctrl Pts',(2.71998470981695,-0.336928711641806,
12.5212220730815));
#446018=CARTESIAN_POINT('Ctrl Pts',(2.72048774007532,-0.337284592491046,
12.5193246583486));
#446019=CARTESIAN_POINT('Ctrl Pts',(2.72096485386709,-0.337776827244795,
12.517417831369));
#446020=CARTESIAN_POINT('Ctrl Pts',(2.72136095927387,-0.338485533961445,
12.5155812248347));
#446021=CARTESIAN_POINT('Ctrl Pts',(2.72152970230623,-0.338787446832053,
12.5147988205793));
#446022=CARTESIAN_POINT('Ctrl Pts',(2.7216841570046,-0.339128816489286,
12.5140295443047));
#446023=CARTESIAN_POINT('Ctrl Pts',(2.72182218293109,-0.339516026505234,
12.5132817086137));
#446024=CARTESIAN_POINT('Ctrl Pts',(2.72203106649912,-0.340102016483784,
12.5121499604604));
#446025=CARTESIAN_POINT('Ctrl Pts',(2.72220009788286,-0.34080804871263,
12.5110494206568));
#446026=CARTESIAN_POINT('Ctrl Pts',(2.7222977756876,-0.341653986748281,
12.5100666561695));
#446027=CARTESIAN_POINT('Ctrl Pts',(2.72235386205816,-0.342139722420329,
12.5095023550641));
#446028=CARTESIAN_POINT('Ctrl Pts',(2.72238642252909,-0.342677272558588,
12.5089719619137));
#446029=CARTESIAN_POINT('Ctrl Pts',(2.72238847149647,-0.343256947543976,
12.5085043804652));
#446030=CARTESIAN_POINT('Ctrl Pts',(2.72239146989334,-0.344105226377113,
12.5078201359221));
#446031=CARTESIAN_POINT('Ctrl Pts',(2.72232800857336,-0.345068320699357,
12.5072563000949));
#446032=CARTESIAN_POINT('Ctrl Pts',(2.72219394159812,-0.346080390278256,
12.5068768744332));
#446033=CARTESIAN_POINT('Ctrl Pts',(2.72209727007977,-0.34681016211575,
12.5066032824114));
#446034=CARTESIAN_POINT('Ctrl Pts',(2.7219622490017,-0.347578227040838,
12.5064197834844));
#446035=CARTESIAN_POINT('Ctrl Pts',(2.72179896411096,-0.34834214185398,
12.5063282718343));
#446036=CARTESIAN_POINT('Ctrl Pts',(2.7215606187222,-0.349457220979117,
12.5061946931565));
#446037=CARTESIAN_POINT('Ctrl Pts',(2.72125799611724,-0.350587512994016,
12.5062515701262));
#446038=CARTESIAN_POINT('Ctrl Pts',(2.72092481596425,-0.351666869563629,
12.5064436508398));
#446039=CARTESIAN_POINT('',(2.65059728690124,-0.369624507601204,12.5737548217797));
#446040=CARTESIAN_POINT('Origin',(2.66600455125891,-0.371773043151976,12.5893111709658));
#446041=CARTESIAN_POINT('Ctrl Pts',(2.72092481596425,-0.351666869563629,
12.5064436508398));
#446042=CARTESIAN_POINT('Ctrl Pts',(2.71051463337505,-0.354325532048914,
12.5164271754438));
#446043=CARTESIAN_POINT('Ctrl Pts',(2.70010027249109,-0.356985045989405,
12.5264061185523));
#446044=CARTESIAN_POINT('Ctrl Pts',(2.68968158639056,-0.3596454422897,12.536380305637));
#446045=CARTESIAN_POINT('Ctrl Pts',(2.67666034190212,-0.362970398078559,
12.5488460165097));
#446046=CARTESIAN_POINT('Ctrl Pts',(2.66363233760314,-0.366296733065921,
12.5613043021964));
#446047=CARTESIAN_POINT('Ctrl Pts',(2.65059728690124,-0.369624507601204,
12.5737548217797));
#446048=CARTESIAN_POINT('Ctrl Pts',(2.65148770642212,-0.413283442896986,
12.5893111709658));
#446049=CARTESIAN_POINT('Ctrl Pts',(2.64175246035451,-0.40747968389418,
12.5770542771492));
#446050=CARTESIAN_POINT('Ctrl Pts',(2.64736473026114,-0.392107432876518,
12.5737548217797));
#446051=CARTESIAN_POINT('Ctrl Pts',(2.64240480651373,-0.407868586225798,
12.5928319619712));
#446052=CARTESIAN_POINT('Ctrl Pts',(2.63753030585758,-0.401169880401203,
12.5821634970842));
#446053=CARTESIAN_POINT('Ctrl Pts',(2.64405121633907,-0.390143039113135,
12.5773203894503));
#446054=CARTESIAN_POINT('Ctrl Pts',(2.63290585503669,-0.394071701788491,
12.5969440695591));
#446055=CARTESIAN_POINT('Ctrl Pts',(2.63345983373103,-0.390090288702896,
12.5878292599214));
#446056=CARTESIAN_POINT('Ctrl Pts',(2.64066728139681,-0.38522438773251,
12.5813877129824));
#446057=CARTESIAN_POINT('Ctrl Pts',(2.6372068775263,-0.363778526796667,
12.596957478804));
#446058=CARTESIAN_POINT('Ctrl Pts',(2.63665707227668,-0.367730527218781,
12.5878468778671));
#446059=CARTESIAN_POINT('Ctrl Pts',(2.64221258285488,-0.374382878994892,
12.5814011370086));
#446060=CARTESIAN_POINT('Ctrl Pts',(2.65026383573032,-0.353108248000009,
12.5928371701607));
#446061=CARTESIAN_POINT('Ctrl Pts',(2.64370794586564,-0.358163480317713,
12.5821692192952));
#446062=CARTESIAN_POINT('Ctrl Pts',(2.64685255955922,-0.370578601206617,
12.5773318885715));
#446063=CARTESIAN_POINT('Ctrl Pts',(2.66051922500483,-0.350467851392951,
12.5893111709658));
#446064=CARTESIAN_POINT('Ctrl Pts',(2.64954321694339,-0.353293781610586,
12.5770542771492));
#446065=CARTESIAN_POINT('Ctrl Pts',(2.65059728690122,-0.369624507601151,
12.5737548217797));
#446066=CARTESIAN_POINT('',(2.64736473026114,-0.392107432876518,12.5737548217797));
#446067=CARTESIAN_POINT('Origin',(2.66275320456913,-0.394386656093409,12.5893111709658));
#446068=CARTESIAN_POINT('Ctrl Pts',(2.65059728690122,-0.369624507601151,
12.5737548217797));
#446069=CARTESIAN_POINT('Ctrl Pts',(2.64961914639082,-0.369842591926409,
12.5746934679442));
#446070=CARTESIAN_POINT('Ctrl Pts',(2.64857663240156,-0.370262710981469,
12.5756680099006));
#446071=CARTESIAN_POINT('Ctrl Pts',(2.64758710873764,-0.370833978507702,
12.5765688348656));
#446072=CARTESIAN_POINT('Ctrl Pts',(2.64732514330201,-0.370985215261131,
12.5768073183026));
#446073=CARTESIAN_POINT('Ctrl Pts',(2.647066821301,-0.371146798286212,12.5770407398754));
#446074=CARTESIAN_POINT('Ctrl Pts',(2.6468140348489,-0.371317298000386,
12.5772674179684));
#446075=CARTESIAN_POINT('Ctrl Pts',(2.64577666760578,-0.372016982722287,
12.5781976435658));
#446076=CARTESIAN_POINT('Ctrl Pts',(2.6447799098633,-0.372915921811197,
12.5790594849312));
#446077=CARTESIAN_POINT('Ctrl Pts',(2.64392340493399,-0.373989277311363,
12.5797571720116));
#446078=CARTESIAN_POINT('Ctrl Pts',(2.64336536117536,-0.374688607014145,
12.580211740231));
#446079=CARTESIAN_POINT('Ctrl Pts',(2.64285616804033,-0.375505466446094,
12.5806009430798));
#446080=CARTESIAN_POINT('Ctrl Pts',(2.64244670534667,-0.376391724290526,
12.5808812374708));
#446081=CARTESIAN_POINT('Ctrl Pts',(2.64209484105497,-0.37715331379187,
12.5811221033394));
#446082=CARTESIAN_POINT('Ctrl Pts',(2.64180952282047,-0.377981790259704,
12.581287365893));
#446083=CARTESIAN_POINT('Ctrl Pts',(2.6416147380312,-0.378833108161147,
12.581359338449));
#446084=CARTESIAN_POINT('Ctrl Pts',(2.64158766696764,-0.378951423770407,
12.5813693411482));
#446085=CARTESIAN_POINT('Ctrl Pts',(2.64156228509801,-0.379070187430052,
12.5813775999465));
#446086=CARTESIAN_POINT('Ctrl Pts',(2.64153859601056,-0.379189289011997,
12.5813841266931));
#446087=CARTESIAN_POINT('Ctrl Pts',(2.64149840460858,-0.379391359250802,
12.5813952001081));
#446088=CARTESIAN_POINT('Ctrl Pts',(2.64146341390939,-0.379595874353134,
12.5814007534795));
#446089=CARTESIAN_POINT('Ctrl Pts',(2.64143383353787,-0.37980277850357,
12.5814005856065));
#446090=CARTESIAN_POINT('Ctrl Pts',(2.64129842616222,-0.380749904809983,
12.5813998171494));
#446091=CARTESIAN_POINT('Ctrl Pts',(2.64128541102912,-0.381681605516752,
12.58127954464));
#446092=CARTESIAN_POINT('Ctrl Pts',(2.64136527555804,-0.382592177734726,
12.5810700125799));
#446093=CARTESIAN_POINT('Ctrl Pts',(2.64146174281568,-0.383692045297091,
12.5808169217085));
#446094=CARTESIAN_POINT('Ctrl Pts',(2.64171040119885,-0.384759723791743,
12.5804173076348));
#446095=CARTESIAN_POINT('Ctrl Pts',(2.6420640951309,-0.385707550764392,
12.5799304713245));
#446096=CARTESIAN_POINT('Ctrl Pts',(2.6425024333378,-0.386882206979792,
12.5793271277669));
#446097=CARTESIAN_POINT('Ctrl Pts',(2.64309911845793,-0.387956906787091,
12.5785808224116));
#446098=CARTESIAN_POINT('Ctrl Pts',(2.64380126948767,-0.388901745288867,
12.5777485681082));
#446099=CARTESIAN_POINT('Ctrl Pts',(2.64484755144837,-0.390309658171298,
12.576508418016));
#446100=CARTESIAN_POINT('Ctrl Pts',(2.6461136868804,-0.391421467767638,
12.5750928681475));
#446101=CARTESIAN_POINT('Ctrl Pts',(2.64736473026114,-0.392107432876518,
12.5737548217797));
#446102=CARTESIAN_POINT('Ctrl Pts',(2.64736473026114,-0.392107432876518,
12.5737548217797));
#446103=CARTESIAN_POINT('Ctrl Pts',(2.64175246035451,-0.407479683894181,
12.5770542771492));
#446104=CARTESIAN_POINT('Ctrl Pts',(2.65148770642212,-0.413283442896987,
12.5893111709658));
#446105=CARTESIAN_POINT('Ctrl Pts',(2.66865723589171,-0.404742469803349,
12.5508408821982));
#446106=CARTESIAN_POINT('Ctrl Pts',(2.66302455843625,-0.420161246321361,
12.55409748406));
#446107=CARTESIAN_POINT('Ctrl Pts',(2.67277222418453,-0.425972409434243,
12.5663972313419));
#446108=CARTESIAN_POINT('Ctrl Pts',(2.68992833949995,-0.417366178255246,
12.52790050457));
#446109=CARTESIAN_POINT('Ctrl Pts',(2.68425591538701,-0.432818520538048,
12.5311362602938));
#446110=CARTESIAN_POINT('Ctrl Pts',(2.69403526936601,-0.438648574889328,
12.5434568539655));
#446111=CARTESIAN_POINT('Ctrl Pts',(2.71117969723077,-0.429979450509249,
12.5049357605811));
#446112=CARTESIAN_POINT('Ctrl Pts',(2.70545077826142,-0.445454038466022,
12.5081700652078));
#446113=CARTESIAN_POINT('Ctrl Pts',(2.71527852370348,-0.451312941845609,
12.5204921097672));
#446114=CARTESIAN_POINT('Ctrl Pts',(2.70978424896933,-0.429151214975375,
12.5064436508395));
#446115=CARTESIAN_POINT('Ctrl Pts',(2.7098010934493,-0.4303712822088,12.5062361689309));
#446116=CARTESIAN_POINT('Ctrl Pts',(2.70976658395257,-0.431640770578446,
12.5061871075068));
#446117=CARTESIAN_POINT('Ctrl Pts',(2.70966417203871,-0.432865731165968,
12.5063648335171));
#446118=CARTESIAN_POINT('Ctrl Pts',(2.7096176502304,-0.433422183823524,
12.5064455676336));
#446119=CARTESIAN_POINT('Ctrl Pts',(2.70955624807807,-0.433977191009861,
12.506574497099));
#446120=CARTESIAN_POINT('Ctrl Pts',(2.70948155374489,-0.434506840121112,
12.5067492519495));
#446121=CARTESIAN_POINT('Ctrl Pts',(2.70933145258294,-0.435571190569707,
12.5071004286051));
#446122=CARTESIAN_POINT('Ctrl Pts',(2.70912135537376,-0.436572158368801,
12.5076537929613));
#446123=CARTESIAN_POINT('Ctrl Pts',(2.7088762877546,-0.437436558570328,
12.5083435010505));
#446124=CARTESIAN_POINT('Ctrl Pts',(2.70886085928344,-0.437490977728702,
12.5083869222964));
#446125=CARTESIAN_POINT('Ctrl Pts',(2.7088452790438,-0.437544858286733,
12.5084308732337));
#446126=CARTESIAN_POINT('Ctrl Pts',(2.70882954799834,-0.437598183461513,
12.5084753333615));
#446127=CARTESIAN_POINT('Ctrl Pts',(2.70870336425065,-0.438025921746073,
12.5088319622689));
#446128=CARTESIAN_POINT('Ctrl Pts',(2.70856615304605,-0.438426974615727,
12.509227847131));
#446129=CARTESIAN_POINT('Ctrl Pts',(2.70842464368023,-0.438790323073624,
12.5096423454524));
#446130=CARTESIAN_POINT('Ctrl Pts',(2.70798121595715,-0.439928896329383,
12.5109411997424));
#446131=CARTESIAN_POINT('Ctrl Pts',(2.70747731962361,-0.440770781460926,
12.5124831113042));
#446132=CARTESIAN_POINT('Ctrl Pts',(2.7069677858636,-0.441393110813353,
12.5140723025008));
#446133=CARTESIAN_POINT('Ctrl Pts',(2.70692004199221,-0.441451423755293,
12.5142212114565));
#446134=CARTESIAN_POINT('Ctrl Pts',(2.70687225620062,-0.441507837642663,
12.5143705582413));
#446135=CARTESIAN_POINT('Ctrl Pts',(2.70682447941976,-0.441562431884413,
12.5145201959299));
#446136=CARTESIAN_POINT('Ctrl Pts',(2.70621071553744,-0.442263776202016,
12.5164425148273));
#446137=CARTESIAN_POINT('Ctrl Pts',(2.7055854897805,-0.442695922626524,
12.5184635205941));
#446138=CARTESIAN_POINT('Ctrl Pts',(2.70495520700584,-0.44294885424723,
12.5205025929158));
#446139=CARTESIAN_POINT('Ctrl Pts',(2.70458961801446,-0.443095564612512,
12.5216853356836));
#446140=CARTESIAN_POINT('Ctrl Pts',(2.70422316810204,-0.4431821626277,12.5228750347131));
#446141=CARTESIAN_POINT('Ctrl Pts',(2.70386298154135,-0.443225446458932,
12.5240609649613));
#446142=CARTESIAN_POINT('Ctrl Pts',(2.70297892295147,-0.443331684300595,
12.5269717671326));
#446143=CARTESIAN_POINT('Ctrl Pts',(2.70210647539127,-0.443169652689853,
12.5299036066169));
#446144=CARTESIAN_POINT('Ctrl Pts',(2.7012437201377,-0.442825987884302,
12.5328133004019));
#446145=CARTESIAN_POINT('Ctrl Pts',(2.70082954737924,-0.442661008766634,
12.5342101228451));
#446146=CARTESIAN_POINT('Ctrl Pts',(2.70041831897813,-0.442453890180351,
12.5356023438238));
#446147=CARTESIAN_POINT('Ctrl Pts',(2.70001288567339,-0.442212187377219,
12.5369868989719));
#446148=CARTESIAN_POINT('Origin',(13.6445776740604,-6.97308410522103,-1.23972230381871));
#446149=CARTESIAN_POINT('Ctrl Pts',(2.71518847849396,-0.336392429391334,
12.5369868989719));
#446150=CARTESIAN_POINT('Ctrl Pts',(2.7300502269415,-0.332596150059323,
12.5369868989719));
#446151=CARTESIAN_POINT('Ctrl Pts',(2.7316270800589,-0.317338468782966,
12.5369868989719));
#446152=CARTESIAN_POINT('Ctrl Pts',(2.72021231432179,-0.335109074353454,
12.5218025310015));
#446153=CARTESIAN_POINT('Ctrl Pts',(2.73038128743446,-0.329088455652839,
12.5216901060417));
#446154=CARTESIAN_POINT('Ctrl Pts',(2.7316222896924,-0.317384980947354,
12.5161920673678));
#446155=CARTESIAN_POINT('Ctrl Pts',(2.72483095825869,-0.338982599799196,
12.5042015548895));
#446156=CARTESIAN_POINT('Ctrl Pts',(2.72966079725187,-0.334734070604651,
12.4980677368514));
#446157=CARTESIAN_POINT('Ctrl Pts',(2.73048197451111,-0.32798748275355,
12.4907278922777));
#446158=CARTESIAN_POINT('Ctrl Pts',(2.72090497986881,-0.351664305851125,
12.506463626192));
#446159=CARTESIAN_POINT('Ctrl Pts',(2.72739374832251,-0.352502948975741,
12.4999376786891));
#446160=CARTESIAN_POINT('Ctrl Pts',(2.72731449745051,-0.352492706169361,
12.4906970594712));
#446161=CARTESIAN_POINT('Origin',(2.70974363643439,-0.315076855391407,12.5369868989719));
#446162=CARTESIAN_POINT('Origin',(2.70974363643439,-0.315076855391407,14.));
#446163=CARTESIAN_POINT('Origin',(2.70974363643439,-0.315076855391407,13.7435492065112));
#446164=CARTESIAN_POINT('Ctrl Pts',(2.6912508303197,-0.342555532146921,
13.793642941384));
#446165=CARTESIAN_POINT('Ctrl Pts',(2.70172842566934,-0.339886035060387,
13.8071662555867));
#446166=CARTESIAN_POINT('Ctrl Pts',(2.69999584404053,-0.322944442911652,
13.8103758687955));
#446167=CARTESIAN_POINT('Ctrl Pts',(2.70734702183498,-0.338411340557862,
13.7804579775006));
#446168=CARTESIAN_POINT('Ctrl Pts',(2.72027292376789,-0.335107595569272,
13.7901904343351));
#446169=CARTESIAN_POINT('Ctrl Pts',(2.72122708172638,-0.319380373730858,
13.7927914348263));
#446170=CARTESIAN_POINT('Ctrl Pts',(2.71682345553838,-0.335971498969084,
13.7597120340895));
#446171=CARTESIAN_POINT('Ctrl Pts',(2.73178094522877,-0.332142583700462,
13.7635825532445));
#446172=CARTESIAN_POINT('Ctrl Pts',(2.73374288637564,-0.317253436542894,
13.7651073818884));
#446173=CARTESIAN_POINT('Ctrl Pts',(2.71496775283338,-0.336449275817405,
13.7381884353898));
#446174=CARTESIAN_POINT('Ctrl Pts',(2.72957535751151,-0.332710854199482,
13.7368803041982));
#446175=CARTESIAN_POINT('Ctrl Pts',(2.73129183711739,-0.317669466800656,
13.7363986145813));
#446176=CARTESIAN_POINT('Origin',(2.68967122278781,-0.320244785293354,13.7902182540695));
#446177=CARTESIAN_POINT('Ctrl Pts',(2.66051541293097,-0.350468832082256,
13.8235227101244));
#446178=CARTESIAN_POINT('Ctrl Pts',(2.671650487758,-0.347606525858912,13.8358800583119));
#446179=CARTESIAN_POINT('Ctrl Pts',(2.67047205618014,-0.331076633298055,
13.8390832900376));
#446180=CARTESIAN_POINT('Ctrl Pts',(2.67206629317621,-0.347494892799863,
13.8124254819053));
#446181=CARTESIAN_POINT('Ctrl Pts',(2.68322299209147,-0.344627027748994,
13.8247886449158));
#446182=CARTESIAN_POINT('Ctrl Pts',(2.68202607037732,-0.328077461002008,
13.8279860620657));
#446183=CARTESIAN_POINT('Ctrl Pts',(2.68361199669266,-0.34452228634033,
13.8013225099955));
#446184=CARTESIAN_POINT('Ctrl Pts',(2.69478505602488,-0.34165021757521,
13.8136962257787));
#446185=CARTESIAN_POINT('Ctrl Pts',(2.69357480373744,-0.325079939536435,
13.8168830918626));
#446186=CARTESIAN_POINT('Ctrl Pts',(2.69515272489896,-0.341550960845551,
13.7902140179785));
#446187=CARTESIAN_POINT('Ctrl Pts',(2.70633722499578,-0.33867595491007,
13.802602731458));
#446188=CARTESIAN_POINT('Ctrl Pts',(2.70511846421978,-0.322084005817429,
13.8057746032558));
#446189=CARTESIAN_POINT('Origin',(2.65503389875079,-0.329162659634033,13.8235269408515));
#446190=CARTESIAN_POINT('Ctrl Pts',(2.65148770642212,-0.413283442896987,
13.8235269408515));
#446191=CARTESIAN_POINT('Ctrl Pts',(2.66162968188245,-0.419329677473419,
13.8362179249168));
#446192=CARTESIAN_POINT('Ctrl Pts',(2.65537229157174,-0.435220180000298,
13.8391868794938));
#446193=CARTESIAN_POINT('Ctrl Pts',(2.64220824032984,-0.407751401436477,
13.8400110824519));
#446194=CARTESIAN_POINT('Ctrl Pts',(2.64858783928619,-0.415537451784206,
13.8494522556836));
#446195=CARTESIAN_POINT('Ctrl Pts',(2.64015844445153,-0.426019493100529,
13.85569149686));
#446196=CARTESIAN_POINT('Ctrl Pts',(2.63285631110245,-0.394412018175957,
13.8586819406588));
#446197=CARTESIAN_POINT('Ctrl Pts',(2.63225046284887,-0.398723513453536,
13.868010383617));
#446198=CARTESIAN_POINT('Ctrl Pts',(2.62475360323986,-0.403792040142369,
13.8744918421245));
#446199=CARTESIAN_POINT('Ctrl Pts',(2.6372571714322,-0.363432929643449,
13.8587686893867));
#446200=CARTESIAN_POINT('Ctrl Pts',(2.63785757188144,-0.359159798798226,
13.8680909899357));
#446201=CARTESIAN_POINT('Ctrl Pts',(2.63208229066815,-0.352221317090155,
13.8745789365163));
#446202=CARTESIAN_POINT('Ctrl Pts',(2.65004006191426,-0.3531658617619,13.8400379222776));
#446203=CARTESIAN_POINT('Ctrl Pts',(2.65834867087912,-0.347488076015957,
13.8494748685453));
#446204=CARTESIAN_POINT('Ctrl Pts',(2.65321726590736,-0.33506109777179,
13.8557104837033));
#446205=CARTESIAN_POINT('Ctrl Pts',(2.66051922500306,-0.35046785138664,
13.8235269408542));
#446206=CARTESIAN_POINT('Ctrl Pts',(2.67195380032226,-0.347523856471547,
13.8362179249195));
#446207=CARTESIAN_POINT('Ctrl Pts',(2.67042675019232,-0.330514120378444,
13.8391868794965));
#446208=CARTESIAN_POINT('Origin',(2.64022220827512,-0.432180229700564,13.8235269408515));
#446209=CARTESIAN_POINT('Ctrl Pts',(2.68220613280659,-0.4315965241541,13.7902140241682));
#446210=CARTESIAN_POINT('Ctrl Pts',(2.69212759200737,-0.437506113202412,
13.8026027327198));
#446211=CARTESIAN_POINT('Ctrl Pts',(2.68628370969059,-0.453082600988223,
13.8057746032556));
#446212=CARTESIAN_POINT('Ctrl Pts',(2.67197000430769,-0.425494159352134,
13.8013225161807));
#446213=CARTESIAN_POINT('Ctrl Pts',(2.68188131368142,-0.431397706962145,
13.8136962270464));
#446214=CARTESIAN_POINT('Ctrl Pts',(2.67605170063436,-0.44695579865218,
13.8168830918628));
#446215=CARTESIAN_POINT('Ctrl Pts',(2.66172946292172,-0.419389163765796,
13.8124254880875));
#446216=CARTESIAN_POINT('Ctrl Pts',(2.67162625892701,-0.425284068673469,
13.8247886461868));
#446217=CARTESIAN_POINT('Ctrl Pts',(2.6658152715082,-0.440826043690079,
13.8279860620656));
#446218=CARTESIAN_POINT('Ctrl Pts',(2.65148432999768,-0.413281430890604,
13.8235227163065));
#446219=CARTESIAN_POINT('Ctrl Pts',(2.66136194396267,-0.419164909929044,
13.8358800595847));
#446220=CARTESIAN_POINT('Ctrl Pts',(2.65557424054823,-0.434693216983744,
13.8390832900376));
#446221=CARTESIAN_POINT('Origin',(2.67094402177386,-0.450495329333115,13.7902182540695));
#446222=CARTESIAN_POINT('Ctrl Pts',(2.69978107677395,-0.442074024424127,
13.7382347919292));
#446223=CARTESIAN_POINT('Ctrl Pts',(2.71275510606049,-0.449780673034605,
13.7369371795943));
#446224=CARTESIAN_POINT('Ctrl Pts',(2.71015424263167,-0.464706465691778,
13.7364597369712));
#446225=CARTESIAN_POINT('Ctrl Pts',(2.70140582151744,-0.443042630898841,
13.7595490285574));
#446226=CARTESIAN_POINT('Ctrl Pts',(2.71468888654972,-0.450934017961181,
13.7633824266926));
#446227=CARTESIAN_POINT('Ctrl Pts',(2.71236158736332,-0.465782497304353,
13.7648920890506));
#446228=CARTESIAN_POINT('Ctrl Pts',(2.6931197123406,-0.438102790935586,
13.7803806590111));
#446229=CARTESIAN_POINT('Ctrl Pts',(2.70461184546554,-0.444923917106686,
13.7901039518744));
#446230=CARTESIAN_POINT('Ctrl Pts',(2.70110992975812,-0.460293433293067,
13.7926933640892));
#446231=CARTESIAN_POINT('Ctrl Pts',(2.67871660485965,-0.429516246434742,
13.7936647693663));
#446232=CARTESIAN_POINT('Ctrl Pts',(2.68802176799482,-0.435028711488828,
13.8072068914933));
#446233=CARTESIAN_POINT('Ctrl Pts',(2.68156966891159,-0.450808910703906,
13.8104111085397));
#446234=CARTESIAN_POINT('Origin',(2.68874738752638,-0.461108974180797,13.7435492065112));
#446235=CARTESIAN_POINT('Origin',(2.68874738752638,-0.461108974180797,14.));
#446236=CARTESIAN_POINT('Origin',(2.68874738752638,-0.461108974180797,12.5369868989719));
#446237=CARTESIAN_POINT('Ctrl Pts',(2.70976609202462,-0.429148339431626,
12.506462012331));
#446238=CARTESIAN_POINT('Ctrl Pts',(2.71622422693825,-0.430171120653283,
12.4999388158272));
#446239=CARTESIAN_POINT('Ctrl Pts',(2.7161478187329,-0.430159019810136,
12.4907030323752));
#446240=CARTESIAN_POINT('Ctrl Pts',(2.7099581760171,-0.442422061098678,
12.5042014951932));
#446241=CARTESIAN_POINT('Ctrl Pts',(2.71339472509621,-0.44785632531225,
12.4980716682127));
#446242=CARTESIAN_POINT('Ctrl Pts',(2.71228423935735,-0.45455650341807,
12.4907355092743));
#446243=CARTESIAN_POINT('Ctrl Pts',(2.70443705097922,-0.444839266005536,
12.5218047446509));
#446244=CARTESIAN_POINT('Ctrl Pts',(2.71249312803559,-0.45347746566743,
12.5216906929434));
#446245=CARTESIAN_POINT('Ctrl Pts',(2.71039134817357,-0.465051284213677,
12.5161988840776));
#446246=CARTESIAN_POINT('Ctrl Pts',(2.69997987117604,-0.442192544521366,
12.5369868989719));
#446247=CARTESIAN_POINT('Ctrl Pts',(2.71316108883089,-0.450019487261421,
12.5369868989719));
#446248=CARTESIAN_POINT('Ctrl Pts',(2.71038316681315,-0.465095583599136,
12.5369868989719));
#446249=CARTESIAN_POINT('Origin',(5.09942406832774E-31,-5.88504909413687E-31,
12.5));
#446250=CARTESIAN_POINT('Origin',(2.67635153714374,-0.195787413049918,12.5));
#446251=CARTESIAN_POINT('',(2.67635153714374,-0.195787413049918,12.5893111709658));
#446252=CARTESIAN_POINT('',(2.67635153714374,-0.195787413049918,13.8235269408515));
#446253=CARTESIAN_POINT('',(2.67635153714374,-0.195787413049918,12.5));
#446254=CARTESIAN_POINT('',(2.70846397699157,-0.211537457691783,13.7902182540695));
#446255=CARTESIAN_POINT('',(2.67635153714374,-0.195787413049918,13.8235269408515));
#446256=CARTESIAN_POINT('',(2.72707321410059,-0.220664646924583,13.7435492065112));
#446257=CARTESIAN_POINT('Origin',(2.66584921343154,-0.190636022518706,13.744521291868));
#446258=CARTESIAN_POINT('',(2.72707321410059,-0.220664646924583,12.5369868989719));
#446259=CARTESIAN_POINT('',(2.72707321410059,-0.220664646924583,12.5));
#446260=CARTESIAN_POINT('Ctrl Pts',(2.72707321410059,-0.220664646924583,
12.5369868989719));
#446261=CARTESIAN_POINT('Ctrl Pts',(2.71017831955038,-0.212378283613468,
12.5544431401645));
#446262=CARTESIAN_POINT('Ctrl Pts',(2.69327134132254,-0.204085993675075,
12.5718848856037));
#446263=CARTESIAN_POINT('Ctrl Pts',(2.67635153714374,-0.195787413049918,
12.5893111709658));
#446264=CARTESIAN_POINT('Origin',(2.94007289370883,-0.042399117641198,12.5));
#446265=CARTESIAN_POINT('',(2.73361252196705,-0.11394639622308,13.7435492065112));
#446266=CARTESIAN_POINT('',(2.71402813188475,-0.120733218319995,13.7902182540695));
#446267=CARTESIAN_POINT('Origin',(2.66256373961082,-0.138567813792271,13.7418732680442));
#446268=CARTESIAN_POINT('',(2.68023295023436,-0.132444682635723,13.8235269408515));
#446269=CARTESIAN_POINT('',(2.71402813188475,-0.120733218319995,13.7902182540695));
#446270=CARTESIAN_POINT('',(2.68023295023436,-0.132444682635723,12.5893111709658));
#446271=CARTESIAN_POINT('',(2.68023295023436,-0.132444682635723,12.5));
#446272=CARTESIAN_POINT('',(2.73361252196705,-0.11394639622308,12.5369868989719));
#446273=CARTESIAN_POINT('Ctrl Pts',(2.68023295023436,-0.132444682635723,
12.5893111709658));
#446274=CARTESIAN_POINT('Ctrl Pts',(2.6980393784728,-0.126273999753697,
12.5718848856037));
#446275=CARTESIAN_POINT('Ctrl Pts',(2.71583230866049,-0.120107994518955,
12.5544431401645));
#446276=CARTESIAN_POINT('Ctrl Pts',(2.73361252196705,-0.11394639622308,
12.5369868989719));
#446277=CARTESIAN_POINT('',(2.73361252196705,-0.11394639622308,12.5));
#446278=CARTESIAN_POINT('Origin',(2.69148864585867,-0.164924675570032,12.5));
#446279=CARTESIAN_POINT('',(2.657128461537,-0.163940853655835,13.8587068136939));
#446280=CARTESIAN_POINT('Ctrl Pts',(2.68023295023206,-0.132444682629526,
13.8235269408542));
#446281=CARTESIAN_POINT('Ctrl Pts',(2.67857725169292,-0.133018452421904,
13.8262006681044));
#446282=CARTESIAN_POINT('Ctrl Pts',(2.67693977508105,-0.133769783492457,
13.8288634856214));
#446283=CARTESIAN_POINT('Ctrl Pts',(2.67532062023171,-0.134685341821493,
13.8314912288862));
#446284=CARTESIAN_POINT('Ctrl Pts',(2.67365143859012,-0.135629188023266,
13.8342001611531));
#446285=CARTESIAN_POINT('Ctrl Pts',(2.67199962974925,-0.136748182324745,
13.8368750301949));
#446286=CARTESIAN_POINT('Ctrl Pts',(2.6703682029662,-0.138072824076052,
13.8394886372968));
#446287=CARTESIAN_POINT('Ctrl Pts',(2.67024220391846,-0.138175129371639,
13.8396904925131));
#446288=CARTESIAN_POINT('Ctrl Pts',(2.67011633723629,-0.138278680665416,
13.8398919674349));
#446289=CARTESIAN_POINT('Ctrl Pts',(2.66999061073717,-0.138383501473838,
13.8400930404591));
#446290=CARTESIAN_POINT('Ctrl Pts',(2.66803170729628,-0.140016680189018,
13.8432258934518));
#446291=CARTESIAN_POINT('Ctrl Pts',(2.66611610915967,-0.141948844949605,
13.8462331177034));
#446292=CARTESIAN_POINT('Ctrl Pts',(2.66437479785653,-0.144184896592378,
13.8489036603661));
#446293=CARTESIAN_POINT('Ctrl Pts',(2.66380502053348,-0.144916558712134,
13.8497774930041));
#446294=CARTESIAN_POINT('Ctrl Pts',(2.66325414015538,-0.14568067636377,
13.85061494757));
#446295=CARTESIAN_POINT('Ctrl Pts',(2.66272741700819,-0.14647717900143,
13.8514076489583));
#446296=CARTESIAN_POINT('Ctrl Pts',(2.66161332158704,-0.14816189695295,
13.8530843267192));
#446297=CARTESIAN_POINT('Ctrl Pts',(2.66050033539577,-0.15015861522178,
13.8546805203176));
#446298=CARTESIAN_POINT('Ctrl Pts',(2.65957223692824,-0.1524178775067,13.8559412814273));
#446299=CARTESIAN_POINT('Ctrl Pts',(2.65944802725433,-0.152720240070046,
13.8561100121513));
#446300=CARTESIAN_POINT('Ctrl Pts',(2.6593270939146,-0.153027236813295,
13.8562727473908));
#446301=CARTESIAN_POINT('Ctrl Pts',(2.65920983451485,-0.153338686653399,
13.8564289040185));
#446302=CARTESIAN_POINT('Ctrl Pts',(2.65867806447477,-0.154751108125077,
13.8571370725437));
#446303=CARTESIAN_POINT('Ctrl Pts',(2.65821463653706,-0.156280741050408,
13.8577210840554));
#446304=CARTESIAN_POINT('Ctrl Pts',(2.65786565151628,-0.157876637840136,
13.8581177131616));
#446305=CARTESIAN_POINT('Ctrl Pts',(2.65776736532273,-0.15832609730522,
13.8582294175695));
#446306=CARTESIAN_POINT('Ctrl Pts',(2.65767799379106,-0.158780741481692,
13.8583265086086));
#446307=CARTESIAN_POINT('Ctrl Pts',(2.65759815423685,-0.159239280394839,
13.8584082369006));
#446308=CARTESIAN_POINT('Ctrl Pts',(2.65748344620727,-0.159898077850963,
13.8585256585398));
#446309=CARTESIAN_POINT('Ctrl Pts',(2.65738730653124,-0.160573160685501,
13.8586122832068));
#446310=CARTESIAN_POINT('Ctrl Pts',(2.65731301443783,-0.161247103540259,
13.8586682984299));
#446311=CARTESIAN_POINT('Ctrl Pts',(2.65725358812744,-0.16178619101826,
13.8587131050557));
#446312=CARTESIAN_POINT('Ctrl Pts',(2.65720725137057,-0.162330477622658,
13.8587357943552));
#446313=CARTESIAN_POINT('Ctrl Pts',(2.65717450328177,-0.162880070989482,
13.8587355499465));
#446314=CARTESIAN_POINT('Ctrl Pts',(2.65715333741124,-0.163235286285242,
13.8587353919793));
#446315=CARTESIAN_POINT('Ctrl Pts',(2.65713803827726,-0.163588874847986,
13.8587257282814));
#446316=CARTESIAN_POINT('Ctrl Pts',(2.657128461537,-0.163940853655835,13.8587068136939));
#446317=CARTESIAN_POINT('Ctrl Pts',(2.657128461537,-0.163940853655835,13.8587068136939));
#446318=CARTESIAN_POINT('Ctrl Pts',(2.65709696416037,-0.165098492767069,
13.8586446046466));
#446319=CARTESIAN_POINT('Ctrl Pts',(2.65712729051015,-0.166238741134392,
13.858482427929));
#446320=CARTESIAN_POINT('Ctrl Pts',(2.65721499023803,-0.167362023442386,
13.8582284286032));
#446321=CARTESIAN_POINT('Ctrl Pts',(2.65730495995717,-0.168514380424691,
13.8579678548414));
#446322=CARTESIAN_POINT('Ctrl Pts',(2.65745705833494,-0.169651577367859,
13.857615680862));
#446323=CARTESIAN_POINT('Ctrl Pts',(2.65765568485813,-0.170730065667193,
13.8571944833187));
#446324=CARTESIAN_POINT('Ctrl Pts',(2.6581513776606,-0.173421543516925,
13.8561433417727));
#446325=CARTESIAN_POINT('Ctrl Pts',(2.65895532004245,-0.175874149611331,
13.8546163505474));
#446326=CARTESIAN_POINT('Ctrl Pts',(2.65987707537418,-0.178007312511304,
13.8528973491086));
#446327=CARTESIAN_POINT('Ctrl Pts',(2.66004546647405,-0.178397009901237,
13.8525833129072));
#446328=CARTESIAN_POINT('Ctrl Pts',(2.66021770028529,-0.178776155873566,
13.8522628768812));
#446329=CARTESIAN_POINT('Ctrl Pts',(2.66039252597185,-0.179144413843575,
13.851937733538));
#446330=CARTESIAN_POINT('Ctrl Pts',(2.66146016218374,-0.181393314172981,
13.8499521282529));
#446331=CARTESIAN_POINT('Ctrl Pts',(2.66273424628176,-0.183457909392397,
13.847639871647));
#446332=CARTESIAN_POINT('Ctrl Pts',(2.66407944702675,-0.1852718839326,13.8452109780794));
#446333=CARTESIAN_POINT('Ctrl Pts',(2.66468468068619,-0.186088028625637,
13.8441181685877));
#446334=CARTESIAN_POINT('Ctrl Pts',(2.66530391729198,-0.186854041072759,
13.8430021611332));
#446335=CARTESIAN_POINT('Ctrl Pts',(2.66592396494383,-0.187567074770224,
13.8418824960098));
#446336=CARTESIAN_POINT('Ctrl Pts',(2.66738512306889,-0.189247356886282,
13.8392439765549));
#446337=CARTESIAN_POINT('Ctrl Pts',(2.66891778056966,-0.190716243249255,
13.8364981347963));
#446338=CARTESIAN_POINT('Ctrl Pts',(2.67050231261561,-0.192002324595168,
13.8336931113419));
#446339=CARTESIAN_POINT('Ctrl Pts',(2.67204554620127,-0.193254886152371,
13.8309611966327));
#446340=CARTESIAN_POINT('Ctrl Pts',(2.67363988765096,-0.194334864522001,
13.8281701127185));
#446341=CARTESIAN_POINT('Ctrl Pts',(2.67527917510622,-0.195231239342457,
13.825358068512));
#446342=CARTESIAN_POINT('Ctrl Pts',(2.67563457439567,-0.195425574370919,
13.8247484142932));
#446343=CARTESIAN_POINT('Ctrl Pts',(2.67599207053514,-0.195611107071313,
13.8241378483365));
#446344=CARTESIAN_POINT('Ctrl Pts',(2.67635153714374,-0.195787413049918,
13.8235269408515));
#446345=CARTESIAN_POINT('',(2.65718639411042,-0.162700119730359,12.5969504640361));
#446346=CARTESIAN_POINT('Origin',(2.69152165735451,-0.164926894568226,12.584524458991));
#446347=CARTESIAN_POINT('Origin',(2.69152165735451,-0.164926894568226,12.584524458991));
#446348=CARTESIAN_POINT('Ctrl Pts',(2.68023295023436,-0.132444682635723,
12.5893111709658));
#446349=CARTESIAN_POINT('Ctrl Pts',(2.66952380348168,-0.136155856356976,
12.5770542771492));
#446350=CARTESIAN_POINT('Ctrl Pts',(2.67190547188397,-0.152346326716927,
12.5737548217797));
#446351=CARTESIAN_POINT('Ctrl Pts',(2.703650260086,-0.124329591214261,12.5663937883685));
#446352=CARTESIAN_POINT('Ctrl Pts',(2.69292745232941,-0.128045499053006,
12.5540940315304));
#446353=CARTESIAN_POINT('Ctrl Pts',(2.6953196780358,-0.144285673050915,
12.5508374392248));
#446354=CARTESIAN_POINT('Ctrl Pts',(2.72704394215907,-0.116222687820561,
12.5434499600945));
#446355=CARTESIAN_POINT('Ctrl Pts',(2.7162862707359,-0.119950677398965,
12.5311293540533));
#446356=CARTESIAN_POINT('Ctrl Pts',(2.71871062394669,-0.136231779206612,
12.5278936106989));
#446357=CARTESIAN_POINT('Ctrl Pts',(2.75041584724981,-0.108123331075201,
12.5204817579905));
#446358=CARTESIAN_POINT('Ctrl Pts',(2.73960493270498,-0.111869771654276,
12.5081597038247));
#446359=CARTESIAN_POINT('Ctrl Pts',(2.74208011298381,-0.128184106684609,
12.5049254088044));
#446360=CARTESIAN_POINT('Ctrl Pts',(2.73361252196705,-0.11394639622308,
12.5369868989719));
#446361=CARTESIAN_POINT('Ctrl Pts',(2.73449267529843,-0.113641385921656,
12.5342545179733));
#446362=CARTESIAN_POINT('Ctrl Pts',(2.73537350012164,-0.113468167146179,
12.5314872231885));
#446363=CARTESIAN_POINT('Ctrl Pts',(2.73621616480082,-0.113491347926608,
12.5287124745063));
#446364=CARTESIAN_POINT('Ctrl Pts',(2.73697612163466,-0.11351225350499,
12.5262100684185));
#446365=CARTESIAN_POINT('Ctrl Pts',(2.73770424773633,-0.113693859445946,
12.5237004536639));
#446366=CARTESIAN_POINT('Ctrl Pts',(2.73839700297034,-0.114103604192337,
12.5212220730815));
#446367=CARTESIAN_POINT('Ctrl Pts',(2.73892736703007,-0.114417299241446,
12.5193246583486));
#446368=CARTESIAN_POINT('Ctrl Pts',(2.73944301496718,-0.11486900692132,
12.517417831369));
#446369=CARTESIAN_POINT('Ctrl Pts',(2.7398955685426,-0.115543069206918,
12.5155812248347));
#446370=CARTESIAN_POINT('Ctrl Pts',(2.74008835879822,-0.115830223363684,
12.5147988205793));
#446371=CARTESIAN_POINT('Ctrl Pts',(2.74027012435751,-0.116157867649738,
12.5140295443047));
#446372=CARTESIAN_POINT('Ctrl Pts',(2.7404392522251,-0.11653253886192,12.5132817086137));
#446373=CARTESIAN_POINT('Ctrl Pts',(2.74069520437361,-0.117099553057184,
12.5121499604604));
#446374=CARTESIAN_POINT('Ctrl Pts',(2.7409212215005,-0.117789458395046,
12.5110494206568));
#446375=CARTESIAN_POINT('Ctrl Pts',(2.74108752609361,-0.118624619993785,
12.5100666561695));
#446376=CARTESIAN_POINT('Ctrl Pts',(2.74118301780802,-0.119104167860575,
12.5095023550641));
#446377=CARTESIAN_POINT('Ctrl Pts',(2.74125928526331,-0.119637275364437,
12.5089719619137));
#446378=CARTESIAN_POINT('Ctrl Pts',(2.74130857630567,-0.120214854519267,
12.5085043804652));
#446379=CARTESIAN_POINT('Ctrl Pts',(2.74138070732556,-0.121060066377384,
12.5078201359221));
#446380=CARTESIAN_POINT('Ctrl Pts',(2.74139595829608,-0.122025128769444,
12.5072563000949));
#446381=CARTESIAN_POINT('Ctrl Pts',(2.74134483048392,-0.123044758473408,
12.5068768744332));
#446382=CARTESIAN_POINT('Ctrl Pts',(2.7413079638117,-0.123779981681515,
12.5066032824114));
#446383=CARTESIAN_POINT('Ctrl Pts',(2.74123599642688,-0.124556496405264,
12.5064197834844));
#446384=CARTESIAN_POINT('Ctrl Pts',(2.74113552100225,-0.125331178589341,
12.5063282718343));
#446385=CARTESIAN_POINT('Ctrl Pts',(2.7409888579887,-0.126461974742552,
12.5061946931565));
#446386=CARTESIAN_POINT('Ctrl Pts',(2.74077937162784,-0.127613172355728,
12.5062515701262));
#446387=CARTESIAN_POINT('Ctrl Pts',(2.740535277685,-0.128716094730959,12.5064436508398));
#446388=CARTESIAN_POINT('',(2.67190547188397,-0.152346326716927,12.5737548217797));
#446389=CARTESIAN_POINT('Origin',(2.68743659543392,-0.153231878113681,12.5893111709658));
#446390=CARTESIAN_POINT('Ctrl Pts',(2.740535277685,-0.128716094730959,12.5064436508398));
#446391=CARTESIAN_POINT('Ctrl Pts',(2.73037643979395,-0.132214437260586,
12.5164271754438));
#446392=CARTESIAN_POINT('Ctrl Pts',(2.72021350691258,-0.135713968982086,
12.5264061185523));
#446393=CARTESIAN_POINT('Ctrl Pts',(2.71004633512696,-0.139214732672717,
12.536380305637));
#446394=CARTESIAN_POINT('Ctrl Pts',(2.69733943251955,-0.143589977254623,
12.5488460165097));
#446395=CARTESIAN_POINT('Ctrl Pts',(2.6846259050118,-0.147967147433176,
12.5613043021964));
#446396=CARTESIAN_POINT('Ctrl Pts',(2.67190547188397,-0.152346326716927,
12.5737548217797));
#446397=CARTESIAN_POINT('Ctrl Pts',(2.67635153714374,-0.195787413049918,
12.5893111709658));
#446398=CARTESIAN_POINT('Ctrl Pts',(2.66617562406611,-0.190796478508543,
12.5770542771492));
#446399=CARTESIAN_POINT('Ctrl Pts',(2.67051623844066,-0.175017925288858,
12.5737548217797));
#446400=CARTESIAN_POINT('Ctrl Pts',(2.66685749874773,-0.191130914531672,
12.5928319619712));
#446401=CARTESIAN_POINT('Ctrl Pts',(2.66145321087793,-0.184851815154235,
12.5821634970842));
#446402=CARTESIAN_POINT('Ctrl Pts',(2.66705363363455,-0.173330150029483,
12.5773203894503));
#446403=CARTESIAN_POINT('Ctrl Pts',(2.65626558008246,-0.178154190818509,
12.5969440695591));
#446404=CARTESIAN_POINT('Ctrl Pts',(2.65649319333027,-0.174140871150037,
12.5878292599214));
#446405=CARTESIAN_POINT('Ctrl Pts',(2.66328004270661,-0.16870368716828,
12.5813877129824));
#446406=CARTESIAN_POINT('Ctrl Pts',(2.65808311628459,-0.147611240605811,
12.596957478804));
#446407=CARTESIAN_POINT('Ctrl Pts',(2.65785726518957,-0.151594905304524,
12.5878468778671));
#446408=CARTESIAN_POINT('Ctrl Pts',(2.66393651869179,-0.157772296241913,
12.5814011370086));
#446409=CARTESIAN_POINT('Ctrl Pts',(2.67022690175735,-0.135912202973097,
12.5928371701607));
#446410=CARTESIAN_POINT('Ctrl Pts',(2.66410487443975,-0.141484980308176,
12.5821692192952));
#446411=CARTESIAN_POINT('Ctrl Pts',(2.66825097229948,-0.153602475697303,
12.5773318885715));
#446412=CARTESIAN_POINT('Ctrl Pts',(2.68023295023433,-0.132444682635672,
12.5893111709658));
#446413=CARTESIAN_POINT('Ctrl Pts',(2.66952380348166,-0.136155856356925,
12.5770542771492));
#446414=CARTESIAN_POINT('Ctrl Pts',(2.67190547188395,-0.152346326716875,
12.5737548217797));
#446415=CARTESIAN_POINT('',(2.67051623844066,-0.175017925288858,12.5737548217797));
#446416=CARTESIAN_POINT('Origin',(2.6860392867213,-0.176035261062791,12.5893111709658));
#446417=CARTESIAN_POINT('Ctrl Pts',(2.67190547188395,-0.152346326716875,
12.5737548217797));
#446418=CARTESIAN_POINT('Ctrl Pts',(2.67094836195251,-0.152643412916743,
12.5746934679442));
#446419=CARTESIAN_POINT('Ctrl Pts',(2.66994356044573,-0.153147108628655,
12.5756680099006));
#446420=CARTESIAN_POINT('Ctrl Pts',(2.66900389294695,-0.153797130674218,
12.5765688348656));
#446421=CARTESIAN_POINT('Ctrl Pts',(2.66875512637911,-0.153969216814801,
12.5768073183026));
#446422=CARTESIAN_POINT('Ctrl Pts',(2.66851083443986,-0.154151317826923,
12.5770407398754));
#446423=CARTESIAN_POINT('Ctrl Pts',(2.66827278642337,-0.154341854659967,
12.5772674179684));
#446424=CARTESIAN_POINT('Ctrl Pts',(2.66729590173457,-0.155123766299436,
12.5781976435658));
#446425=CARTESIAN_POINT('Ctrl Pts',(2.66637573250234,-0.156100959252145,
12.5790594849312));
#446426=CARTESIAN_POINT('Ctrl Pts',(2.66560956596033,-0.157240556353572,
12.5797571720116));
#446427=CARTESIAN_POINT('Ctrl Pts',(2.66511038090932,-0.157983044841412,
12.580211740231));
#446428=CARTESIAN_POINT('Ctrl Pts',(2.66466946369949,-0.158838690208611,
12.5806009430798));
#446429=CARTESIAN_POINT('Ctrl Pts',(2.6643336017011,-0.159755374113976,
12.5808812374708));
#446430=CARTESIAN_POINT('Ctrl Pts',(2.66404498482342,-0.160543109695404,
12.5811221033394));
#446431=CARTESIAN_POINT('Ctrl Pts',(2.66382814448513,-0.161392085561016,
12.581287365893));
#446432=CARTESIAN_POINT('Ctrl Pts',(2.6637033981384,-0.162256447540992,
12.581359338449));
#446433=CARTESIAN_POINT('Ctrl Pts',(2.66368606097211,-0.162376576007816,
12.5813693411482));
#446434=CARTESIAN_POINT('Ctrl Pts',(2.66367044389937,-0.162497013349188,
12.5813775999465));
#446435=CARTESIAN_POINT('Ctrl Pts',(2.66365654152002,-0.162617649510988,
12.5813841266931));
#446436=CARTESIAN_POINT('Ctrl Pts',(2.663632954452,-0.162822323350123,12.5813952001081));
#446437=CARTESIAN_POINT('Ctrl Pts',(2.66361475006095,-0.163029010012145,
12.5814007534795));
#446438=CARTESIAN_POINT('Ctrl Pts',(2.66360213272474,-0.163237636780978,
12.5814005856065));
#446439=CARTESIAN_POINT('Ctrl Pts',(2.66354437549263,-0.164192648560916,
12.5813998171494));
#446440=CARTESIAN_POINT('Ctrl Pts',(2.66360734592339,-0.165122309964617,
12.58127954464));
#446441=CARTESIAN_POINT('Ctrl Pts',(2.66376116479879,-0.16602334262812,
12.5810700125799));
#446442=CARTESIAN_POINT('Ctrl Pts',(2.66394696048659,-0.167111687494848,
12.5808169217085));
#446443=CARTESIAN_POINT('Ctrl Pts',(2.66428181718866,-0.168155545410726,
12.5804173076348));
#446444=CARTESIAN_POINT('Ctrl Pts',(2.6647115909308,-0.169071389228317,
12.5799304713245));
#446445=CARTESIAN_POINT('Ctrl Pts',(2.66524421599,-0.170206408238868,12.5793271277669));
#446446=CARTESIAN_POINT('Ctrl Pts',(2.66592651370094,-0.171228896694569,
12.5785808224116));
#446447=CARTESIAN_POINT('Ctrl Pts',(2.6667033414904,-0.172113359496798,
12.5777485681082));
#446448=CARTESIAN_POINT('Ctrl Pts',(2.66786090000453,-0.173431305972252,
12.576508418016));
#446449=CARTESIAN_POINT('Ctrl Pts',(2.669213445279,-0.174436214321939,12.5750928681475));
#446450=CARTESIAN_POINT('Ctrl Pts',(2.67051623844066,-0.175017925288858,
12.5737548217797));
#446451=CARTESIAN_POINT('Ctrl Pts',(2.67051623844066,-0.175017925288858,
12.5737548217797));
#446452=CARTESIAN_POINT('Ctrl Pts',(2.66617562406611,-0.190796478508544,
12.5770542771492));
#446453=CARTESIAN_POINT('Ctrl Pts',(2.67635153714374,-0.195787413049918,
12.5893111709658));
#446454=CARTESIAN_POINT('Ctrl Pts',(2.69276776782275,-0.185875383293774,
12.5508408821982));
#446455=CARTESIAN_POINT('Ctrl Pts',(2.68841060606402,-0.201701970608707,
12.55409748406));
#446456=CARTESIAN_POINT('Ctrl Pts',(2.69859950100054,-0.206699272304328,
12.5663972313419));
#446457=CARTESIAN_POINT('Ctrl Pts',(2.71499704302009,-0.196723294981798,
12.52790050457));
#446458=CARTESIAN_POINT('Ctrl Pts',(2.71060300277904,-0.212586576095784,
12.5311362602938));
#446459=CARTESIAN_POINT('Ctrl Pts',(2.72082502031763,-0.217600123285803,
12.5434568539655));
#446460=CARTESIAN_POINT('Ctrl Pts',(2.73720578739579,-0.207562414669864,
12.5049357605811));
#446461=CARTESIAN_POINT('Ctrl Pts',(2.73275725350924,-0.223452472292466,
12.5081700652078));
#446462=CARTESIAN_POINT('Ctrl Pts',(2.74302985295592,-0.228490828164516,
12.5204921097672));
#446463=CARTESIAN_POINT('Ctrl Pts',(2.73574747348835,-0.206850677009421,
12.5064436508395));
#446464=CARTESIAN_POINT('Ctrl Pts',(2.73586370872577,-0.208065311588282,
12.5062361689309));
#446465=CARTESIAN_POINT('Ctrl Pts',(2.73593278914447,-0.209333388682228,
12.5061871075061));
#446466=CARTESIAN_POINT('Ctrl Pts',(2.73593056365757,-0.210562620836186,
12.5063648335164));
#446467=CARTESIAN_POINT('Ctrl Pts',(2.73592955270414,-0.211121013902697,
12.5064455676329));
#446468=CARTESIAN_POINT('Ctrl Pts',(2.73591359310022,-0.211679179196062,
12.506574497099));
#446469=CARTESIAN_POINT('Ctrl Pts',(2.73588231862587,-0.21221315422517,
12.5067492519495));
#446470=CARTESIAN_POINT('Ctrl Pts',(2.73581947135566,-0.213286197773626,
12.5071004286051));
#446471=CARTESIAN_POINT('Ctrl Pts',(2.73569166139577,-0.214300959807943,
12.5076537929613));
#446472=CARTESIAN_POINT('Ctrl Pts',(2.73551786586002,-0.21518245907517,
12.5083435010505));
#446473=CARTESIAN_POINT('Ctrl Pts',(2.73550692439244,-0.215237954721908,
12.5083869222964));
#446474=CARTESIAN_POINT('Ctrl Pts',(2.73549578776044,-0.215292925930993,
12.5084308732337));
#446475=CARTESIAN_POINT('Ctrl Pts',(2.73548445555553,-0.215347355896893,
12.5084753333615));
#446476=CARTESIAN_POINT('Ctrl Pts',(2.73539355631497,-0.215783956064467,
12.5088319622689));
#446477=CARTESIAN_POINT('Ctrl Pts',(2.73528949120141,-0.216194858450765,
12.509227847131));
#446478=CARTESIAN_POINT('Ctrl Pts',(2.7351780689688,-0.216568532223665,
12.5096423454524));
#446479=CARTESIAN_POINT('Ctrl Pts',(2.73482892100524,-0.217739460446853,
12.5109411997424));
#446480=CARTESIAN_POINT('Ctrl Pts',(2.73439532279908,-0.218619616504199,
12.5124831113042));
#446481=CARTESIAN_POINT('Ctrl Pts',(2.73393821009027,-0.219281406838765,
12.5140723025008));
#446482=CARTESIAN_POINT('Ctrl Pts',(2.7338953781288,-0.219343417317953,
12.5142212114565));
#446483=CARTESIAN_POINT('Ctrl Pts',(2.73385234959602,-0.219403538478404,
12.5143705582413));
#446484=CARTESIAN_POINT('Ctrl Pts',(2.73380918172599,-0.219461845313496,
12.5145201959299));
#446485=CARTESIAN_POINT('Ctrl Pts',(2.73325462616521,-0.220210883420053,
12.5164425148273));
#446486=CARTESIAN_POINT('Ctrl Pts',(2.73266670474085,-0.220692553616486,
12.5184635205941));
#446487=CARTESIAN_POINT('Ctrl Pts',(2.73205913545531,-0.220996017525484,
12.5205025929158));
#446488=CARTESIAN_POINT('Ctrl Pts',(2.73170672118791,-0.221172038620888,
12.5216853356836));
#446489=CARTESIAN_POINT('Ctrl Pts',(2.73134854914952,-0.221288217558141,
12.5228750347131));
#446490=CARTESIAN_POINT('Ctrl Pts',(2.73099308911396,-0.221360715914502,
12.5240609649613));
#446491=CARTESIAN_POINT('Ctrl Pts',(2.73012063152647,-0.221538659240786,
12.5269717671327));
#446492=CARTESIAN_POINT('Ctrl Pts',(2.72923787988305,-0.221448279352425,
12.5299036066169));
#446493=CARTESIAN_POINT('Ctrl Pts',(2.72834998350432,-0.221176080625759,
12.5328133004019));
#446494=CARTESIAN_POINT('Ctrl Pts',(2.72792374154188,-0.221045409387302,
12.5342101228451));
#446495=CARTESIAN_POINT('Ctrl Pts',(2.72749699938177,-0.220872498903379,
12.5356023438238));
#446496=CARTESIAN_POINT('Ctrl Pts',(2.72707321410059,-0.220664646924583,
12.5369868989719));
#446497=CARTESIAN_POINT('Origin',(14.1679839010907,-5.83793691405242,-1.24024679429017));
#446498=CARTESIAN_POINT('Ctrl Pts',(2.73357301872941,-0.113960043755668,
12.5369868989719));
#446499=CARTESIAN_POINT('Ctrl Pts',(2.74807588392649,-0.108965025761739,
12.5369868989719));
#446500=CARTESIAN_POINT('Ctrl Pts',(2.7484038475258,-0.0936295849933097,
12.5369868989719));
#446501=CARTESIAN_POINT('Ctrl Pts',(2.7384755328083,-0.112271469716813,
12.5218025310015));
#446502=CARTESIAN_POINT('Ctrl Pts',(2.74811993318496,-0.105442018415441,
12.5216901060417));
#446503=CARTESIAN_POINT('Ctrl Pts',(2.74840286427204,-0.0936763328516556,
12.5161920673677));
#446504=CARTESIAN_POINT('Ctrl Pts',(2.74339453687234,-0.115755643967929,
12.5042015548895));
#446505=CARTESIAN_POINT('Ctrl Pts',(2.74786201040398,-0.111127574687816,
12.4980677368515));
#446506=CARTESIAN_POINT('Ctrl Pts',(2.74813054572147,-0.104336501981173,
12.4907278922778));
#446507=CARTESIAN_POINT('Ctrl Pts',(2.74051529862617,-0.128715156374926,
12.506463626192));
#446508=CARTESIAN_POINT('Ctrl Pts',(2.74705083343836,-0.129022114115963,
12.4999376786891));
#446509=CARTESIAN_POINT('Ctrl Pts',(2.74697101138329,-0.129018365073473,
12.4906970594712));
#446510=CARTESIAN_POINT('Origin',(2.72640887676749,-0.0931592007451217,
12.5369868989719));
#446511=CARTESIAN_POINT('Origin',(2.72640887676749,-0.0931592007451217,
14.));
#446512=CARTESIAN_POINT('Origin',(2.72640887676749,-0.0931592007451218,
13.7435492065112));
#446513=CARTESIAN_POINT('Ctrl Pts',(2.71021737119475,-0.122053779847747,
13.793642941384));
#446514=CARTESIAN_POINT('Ctrl Pts',(2.72044251441526,-0.118539144002311,
13.8071662555867));
#446515=CARTESIAN_POINT('Ctrl Pts',(2.7173348007707,-0.101795145091112,
13.8103758687955));
#446516=CARTESIAN_POINT('Ctrl Pts',(2.72592221387328,-0.11661138867609,
13.7804579775006));
#446517=CARTESIAN_POINT('Ctrl Pts',(2.73853582004678,-0.112265055620661,
13.7901904343351));
#446518=CARTESIAN_POINT('Ctrl Pts',(2.73820488853917,-0.0965123920839132,
13.7927914348262));
#446519=CARTESIAN_POINT('Ctrl Pts',(2.73516824578542,-0.113407248137176,
13.7597120340895));
#446520=CARTESIAN_POINT('Ctrl Pts',(2.74976387352248,-0.108371898999924,
13.7635825532445));
#446521=CARTESIAN_POINT('Ctrl Pts',(2.75050568275459,-0.0933723778340084,
13.7651073818884));
#446522=CARTESIAN_POINT('Ctrl Pts',(2.7333576610267,-0.114034692220408,
13.7381884353898));
#446523=CARTESIAN_POINT('Ctrl Pts',(2.74761194403764,-0.109118054500371,
13.7368803041982));
#446524=CARTESIAN_POINT('Ctrl Pts',(2.7480966994888,-0.0939868070543812,
13.7363986145813));
#446525=CARTESIAN_POINT('Origin',(2.70682448668519,-0.0999460228420377,
13.7902182540695));
#446526=CARTESIAN_POINT('Ctrl Pts',(2.68022923078013,-0.13244597078122,
13.8235227101244));
#446527=CARTESIAN_POINT('Ctrl Pts',(2.69109395003468,-0.128685576674305,
13.8358800583119));
#446528=CARTESIAN_POINT('Ctrl Pts',(2.68857209989094,-0.112306739080959,
13.8390832900376));
#446529=CARTESIAN_POINT('Ctrl Pts',(2.69149927276398,-0.128540423063339,
13.8124254819052));
#446530=CARTESIAN_POINT('Ctrl Pts',(2.70238509105835,-0.124772726061514,
13.8247886449158));
#446531=CARTESIAN_POINT('Ctrl Pts',(2.69984320867394,-0.108375786864014,
13.8279860620657));
#446532=CARTESIAN_POINT('Ctrl Pts',(2.70276426388169,-0.124636625684892,
13.8013225099955));
#446533=CARTESIAN_POINT('Ctrl Pts',(2.71366604551334,-0.12086340543045,
13.8136962257787));
#446534=CARTESIAN_POINT('Ctrl Pts',(2.71110918874942,-0.104446910421774,
13.8168830918626));
#446535=CARTESIAN_POINT('Ctrl Pts',(2.71402440065465,-0.120734510542875,
13.7902140179785));
#446536=CARTESIAN_POINT('Ctrl Pts',(2.72493734557605,-0.11695743036274,
13.802602731458));
#446537=CARTESIAN_POINT('Ctrl Pts',(2.7223702422428,-0.100520029929646,
13.8057746032558));
#446538=CARTESIAN_POINT('Origin',(2.67302930503479,-0.111657487157766,13.8235269408515));
#446539=CARTESIAN_POINT('Ctrl Pts',(2.67635153714374,-0.195787413049918,
13.8235269408515));
#446540=CARTESIAN_POINT('Ctrl Pts',(2.68695259026586,-0.200986864126054,
13.8362179249168));
#446541=CARTESIAN_POINT('Ctrl Pts',(2.68201124438138,-0.217334527717751,
13.8391868794938));
#446542=CARTESIAN_POINT('Ctrl Pts',(2.66665203497342,-0.191030141633907,
13.8400110824519));
#446543=CARTESIAN_POINT('Ctrl Pts',(2.67364504172606,-0.198270288001189,
13.8494522556837));
#446544=CARTESIAN_POINT('Ctrl Pts',(2.66609807868506,-0.209404525123416,
13.85569149686));
#446545=CARTESIAN_POINT('Ctrl Pts',(2.65624393994649,-0.178497413121852,
13.8586819406588));
#446546=CARTESIAN_POINT('Ctrl Pts',(2.65599153449409,-0.182843944511659,
13.868010383617));
#446547=CARTESIAN_POINT('Ctrl Pts',(2.64893275204602,-0.188506669751641,
13.8744918421245));
#446548=CARTESIAN_POINT('Ctrl Pts',(2.65810507346531,-0.147262693978375,
13.8587686893867));
#446549=CARTESIAN_POINT('Ctrl Pts',(2.65835517629788,-0.142954843413072,
13.8680909899357));
#446550=CARTESIAN_POINT('Ctrl Pts',(2.65203356118348,-0.136510187964475,
13.8745789365163));
#446551=CARTESIAN_POINT('Ctrl Pts',(2.67000856858662,-0.135987864673384,
13.8400379222776));
#446552=CARTESIAN_POINT('Ctrl Pts',(2.67782673909229,-0.129651742527106,
13.8494748685453));
#446553=CARTESIAN_POINT('Ctrl Pts',(2.67169949435394,-0.117684371170747,
13.8557104837033));
#446554=CARTESIAN_POINT('Ctrl Pts',(2.68023295023206,-0.132444682629526,
13.8235269408542));
#446555=CARTESIAN_POINT('Ctrl Pts',(2.69138951502887,-0.128578459572717,
13.8362179249195));
#446556=CARTESIAN_POINT('Ctrl Pts',(2.68848109462999,-0.11174979073529,
13.8391868794965));
#446557=CARTESIAN_POINT('Origin',(2.66666378756618,-0.215539565037045,13.8235269408515));
#446558=CARTESIAN_POINT('Ctrl Pts',(2.70846043663131,-0.211535722113581,
13.7902140241682));
#446559=CARTESIAN_POINT('Ctrl Pts',(2.71883056936445,-0.216616956460646,
13.8026027327198));
#446560=CARTESIAN_POINT('Ctrl Pts',(2.71427576044359,-0.232617945429092,
13.8057746032556));
#446561=CARTESIAN_POINT('Ctrl Pts',(2.69776096862262,-0.206288001927323,
13.8013225161807));
#446562=CARTESIAN_POINT('Ctrl Pts',(2.7081204928681,-0.21136404224361,13.8136962270464));
#446563=CARTESIAN_POINT('Ctrl Pts',(2.70357840628457,-0.227345533249815,
13.8168830918628));
#446564=CARTESIAN_POINT('Ctrl Pts',(2.68705688797703,-0.201038019401679,
13.8124254880876));
#446565=CARTESIAN_POINT('Ctrl Pts',(2.69740124268566,-0.206106628747746,
13.8247886461868));
#446566=CARTESIAN_POINT('Ctrl Pts',(2.69287640609661,-0.222070538545837,
13.8279860620656));
#446567=CARTESIAN_POINT('Ctrl Pts',(2.67634800795688,-0.195785682948258,
13.8235227163065));
#446568=CARTESIAN_POINT('Ctrl Pts',(2.68667231313743,-0.200844467958111,
13.8358800595847));
#446569=CARTESIAN_POINT('Ctrl Pts',(2.68216956901137,-0.216792857410774,
13.8390832900376));
#446570=CARTESIAN_POINT('Origin',(2.69877622741402,-0.23128960967891,13.7902182540695));
#446571=CARTESIAN_POINT('Ctrl Pts',(2.72683091496282,-0.22054583827463,
13.7382347919292));
#446572=CARTESIAN_POINT('Ctrl Pts',(2.74038993764399,-0.227169339815741,
13.7369371795942));
#446573=CARTESIAN_POINT('Ctrl Pts',(2.73901431903953,-0.24225746264383,
13.7364597369711));
#446574=CARTESIAN_POINT('Ctrl Pts',(2.728529203922,-0.221378790011213,13.7595490285574));
#446575=CARTESIAN_POINT('Ctrl Pts',(2.74241129195678,-0.228161226020016,
13.7633824266926));
#446576=CARTESIAN_POINT('Ctrl Pts',(2.74130202557949,-0.243149994762358,
13.7648920890506));
#446577=CARTESIAN_POINT('Ctrl Pts',(2.71986802327364,-0.217130781780323,
13.7803806590111));
#446578=CARTESIAN_POINT('Ctrl Pts',(2.73187790238087,-0.222992495679346,
13.7901039518744));
#446579=CARTESIAN_POINT('Ctrl Pts',(2.72964039726187,-0.238596309708886,
13.7926933640892));
#446580=CARTESIAN_POINT('Ctrl Pts',(2.70481295785426,-0.209746795269595,
13.7936647693663));
#446581=CARTESIAN_POINT('Ctrl Pts',(2.71453647590386,-0.214482460870521,
13.8072068914933));
#446582=CARTESIAN_POINT('Ctrl Pts',(2.70939207838032,-0.230736058748131,
13.8104111085397));
#446583=CARTESIAN_POINT('Origin',(2.71738546452303,-0.24041679891171,13.7435492065112));
#446584=CARTESIAN_POINT('Origin',(2.71738546452303,-0.24041679891171,14.));
#446585=CARTESIAN_POINT('Origin',(2.71738546452303,-0.240416798911709,12.5369868989719));
#446586=CARTESIAN_POINT('Ctrl Pts',(2.73572914257587,-0.206849290993361,
12.506462012331));
#446587=CARTESIAN_POINT('Ctrl Pts',(2.74224915474292,-0.207342271045017,
12.4999388158272));
#446588=CARTESIAN_POINT('Ctrl Pts',(2.74217201444852,-0.207336438444502,
12.4907030323752));
#446589=CARTESIAN_POINT('Ctrl Pts',(2.73700251896777,-0.220063188817957,
12.5042014951932));
#446590=CARTESIAN_POINT('Ctrl Pts',(2.74087057619595,-0.225199260312364,
12.4980716682127));
#446591=CARTESIAN_POINT('Ctrl Pts',(2.74030991222385,-0.231967659025219,
12.4907355092744));
#446592=CARTESIAN_POINT('Ctrl Pts',(2.73169678965818,-0.222922373621123,
12.5218047446509));
#446593=CARTESIAN_POINT('Ctrl Pts',(2.74043015424828,-0.230875185317147,
12.5216906929434));
#446594=CARTESIAN_POINT('Ctrl Pts',(2.73927874154297,-0.242581807507696,
12.5161988840775));
#446595=CARTESIAN_POINT('Ctrl Pts',(2.72703870838115,-0.22064776041674,
12.5369868989719));
#446596=CARTESIAN_POINT('Ctrl Pts',(2.74081403511674,-0.227374268043183,
12.5369868989719));
#446597=CARTESIAN_POINT('Ctrl Pts',(2.73927419821652,-0.242626626347441,
12.5369868989719));
#446598=CARTESIAN_POINT('Origin',(5.142217661156E-31,-5.46695907425333E-31,
12.5));
#446599=CARTESIAN_POINT('Origin',(2.68340468995259,0.0230115497283485,12.5));
#446600=CARTESIAN_POINT('',(2.68340468995259,0.0230115497283485,12.5893111709658));
#446601=CARTESIAN_POINT('',(2.68340468995259,0.0230115497283485,13.8235269408515));
#446602=CARTESIAN_POINT('',(2.68340468995259,0.0230115497283485,12.5));
#446603=CARTESIAN_POINT('',(2.71669405316051,0.00993137402568675,13.7902182540695));
#446604=CARTESIAN_POINT('',(2.68340468995259,0.0230115497283485,13.8235269408515));
#446605=CARTESIAN_POINT('',(2.73598532022336,0.00235138034623294,13.7435492065112));
#446606=CARTESIAN_POINT('Origin',(2.67251742570531,0.0272897625509187,13.7445212918684));
#446607=CARTESIAN_POINT('',(2.73598532022336,0.00235138034623295,12.5369868989719));
#446608=CARTESIAN_POINT('',(2.73598532022336,0.00235138034623294,12.5));
#446609=CARTESIAN_POINT('Ctrl Pts',(2.73598532022336,0.00235138034623295,
12.5369868989719));
#446610=CARTESIAN_POINT('Ctrl Pts',(2.71847122650434,0.00923308071661556,
12.5544431401645));
#446611=CARTESIAN_POINT('Ctrl Pts',(2.70094460623998,0.0161197030620077,
12.5718848856037));
#446612=CARTESIAN_POINT('Ctrl Pts',(2.68340468995259,0.0230115497283485,
12.5893111709658));
#446613=CARTESIAN_POINT('Origin',(2.93374596539591,0.19738519706742,12.5));
#446614=CARTESIAN_POINT('',(2.73380434092627,0.109247549171251,13.7435492065112));
#446615=CARTESIAN_POINT('',(2.71483830529306,0.100887000060675,13.7902182540695));
#446616=CARTESIAN_POINT('Origin',(2.66499884163794,0.0789169219910335,13.7418732680441));
#446617=CARTESIAN_POINT('',(2.68211016738736,0.0864598836326638,13.8235269408515));
#446618=CARTESIAN_POINT('',(2.71483830529306,0.100887000060675,13.7902182540695));
#446619=CARTESIAN_POINT('',(2.68211016738736,0.0864598836326638,12.5893111709658));
#446620=CARTESIAN_POINT('',(2.68211016738736,0.0864598836326638,12.5));
#446621=CARTESIAN_POINT('',(2.73380434092627,0.109247549171251,12.5369868989719));
#446622=CARTESIAN_POINT('Ctrl Pts',(2.68211016738736,0.0864598836326638,
12.5893111709658));
#446623=CARTESIAN_POINT('Ctrl Pts',(2.69935437826406,0.0940614232846936,
12.5718848856037));
#446624=CARTESIAN_POINT('Ctrl Pts',(2.71658551727533,0.101657200637478,
12.5544431401645));
#446625=CARTESIAN_POINT('Ctrl Pts',(2.73380434092627,0.109247549171251,
12.5369868989719));
#446626=CARTESIAN_POINT('',(2.73380434092627,0.109247549171251,12.5));
#446627=CARTESIAN_POINT('Origin',(2.69597583156671,0.0550054088815945,12.5));
#446628=CARTESIAN_POINT('',(2.6616497873045,0.0531852832027369,13.8587068136939));
#446629=CARTESIAN_POINT('Ctrl Pts',(2.68211016738456,0.0864598836386525,
13.8235269408542));
#446630=CARTESIAN_POINT('Ctrl Pts',(2.68050674561044,0.0857530682162323,
13.8262006681044));
#446631=CARTESIAN_POINT('Ctrl Pts',(2.67893595802417,0.084870767592378,
13.8288634856214));
#446632=CARTESIAN_POINT('Ctrl Pts',(2.67739681728247,0.0838262795564332,
13.8314912288862));
#446633=CARTESIAN_POINT('Ctrl Pts',(2.67581012193278,0.0827495201253175,
13.834200161153));
#446634=CARTESIAN_POINT('Ctrl Pts',(2.67425501777337,0.0814996114298888,
13.8368750301949));
#446635=CARTESIAN_POINT('Ctrl Pts',(2.67273699002846,0.080046400886488,
13.8394886372968));
#446636=CARTESIAN_POINT('Ctrl Pts',(2.6726197490635,0.0799341659112227,
13.8396904925131));
#446637=CARTESIAN_POINT('Ctrl Pts',(2.6725027415841,0.0798206998727481,
13.8398919674349));
#446638=CARTESIAN_POINT('Ctrl Pts',(2.67238597729853,0.0797059799700521,
13.8400930404591));
#446639=CARTESIAN_POINT('Ctrl Pts',(2.67056671117422,0.0779185667063149,
13.8432258934518));
#446640=CARTESIAN_POINT('Ctrl Pts',(2.66881497639772,0.0758366920328991,
13.8462331177034));
#446641=CARTESIAN_POINT('Ctrl Pts',(2.66726171813167,0.0734661476307544,
13.8489036603661));
#446642=CARTESIAN_POINT('Ctrl Pts',(2.66675347395084,0.0726904779149612,
13.8497774930041));
#446643=CARTESIAN_POINT('Ctrl Pts',(2.66626670926407,0.071884000936835,
13.85061494757));
#446644=CARTESIAN_POINT('Ctrl Pts',(2.66580666110405,0.0710472157696396,
13.8514076489583));
#446645=CARTESIAN_POINT('Ctrl Pts',(2.66483359289672,0.0692772944585522,
13.8530843267192));
#446646=CARTESIAN_POINT('Ctrl Pts',(2.66388706115073,0.0671965013980083,
13.8546805203176));
#446647=CARTESIAN_POINT('Ctrl Pts',(2.66314620170448,0.06486910798083,13.8559412814273));
#446648=CARTESIAN_POINT('Ctrl Pts',(2.66304705068392,0.0645576272624292,
13.8561100121513));
#446649=CARTESIAN_POINT('Ctrl Pts',(2.66295154282448,0.0642417948356269,
13.8562727473908));
#446650=CARTESIAN_POINT('Ctrl Pts',(2.66286005964904,0.0639218235894991,
13.8564289040185));
#446651=CARTESIAN_POINT('Ctrl Pts',(2.66244518449213,0.0624707576387723,
13.8571370725437));
#446652=CARTESIAN_POINT('Ctrl Pts',(2.66210797785648,0.0609084407616356,
13.8577210840554));
#446653=CARTESIAN_POINT('Ctrl Pts',(2.66189023445851,0.0592894086678096,
13.8581177131616));
#446654=CARTESIAN_POINT('Ctrl Pts',(2.66182891042314,0.0588334335047998,
13.8582294175695));
#446655=CARTESIAN_POINT('Ctrl Pts',(2.66177689398897,0.0583730175098042,
13.8583265086086));
#446656=CARTESIAN_POINT('Ctrl Pts',(2.66173469527258,0.0579094966822024,
13.8584082369006));
#446657=CARTESIAN_POINT('Ctrl Pts',(2.66167406703315,0.0572435415509584,
13.8585256585398));
#446658=CARTESIAN_POINT('Ctrl Pts',(2.66163327277214,0.0565628687227481,
13.8586122832068));
#446659=CARTESIAN_POINT('Ctrl Pts',(2.66161416047878,0.0558851128619351,
13.8586682984299));
#446660=CARTESIAN_POINT('Ctrl Pts',(2.66159887253864,0.0553429753570626,
13.8587131050557));
#446661=CARTESIAN_POINT('Ctrl Pts',(2.66159705437468,0.0547967229455865,
13.8587357943552));
#446662=CARTESIAN_POINT('Ctrl Pts',(2.66160921221402,0.0542462890320964,
13.8587355499465));
#446663=CARTESIAN_POINT('Ctrl Pts',(2.66161707011544,0.0538905304709234,
13.8587353919793));
#446664=CARTESIAN_POINT('Ctrl Pts',(2.66163064263848,0.0535368714234389,
13.8587257282814));
#446665=CARTESIAN_POINT('Ctrl Pts',(2.6616497873045,0.0531852832027369,
13.8587068136939));
#446666=CARTESIAN_POINT('Ctrl Pts',(2.6616497873045,0.0531852832027369,
13.8587068136939));
#446667=CARTESIAN_POINT('Ctrl Pts',(2.66171275306735,0.0520289287116105,
13.8586446046466));
#446668=CARTESIAN_POINT('Ctrl Pts',(2.66183591933619,0.050894946305773,
13.858482427929));
#446669=CARTESIAN_POINT('Ctrl Pts',(2.6620148851866,0.0497825499690413,
13.8582284286032));
#446670=CARTESIAN_POINT('Ctrl Pts',(2.66219848333093,0.0486413607268808,
13.8579678548414));
#446671=CARTESIAN_POINT('Ctrl Pts',(2.66244276772199,0.0475203451425292,
13.857615680862));
#446672=CARTESIAN_POINT('Ctrl Pts',(2.6627286401404,0.0464616353296411,
13.8571944833187));
#446673=CARTESIAN_POINT('Ctrl Pts',(2.66344206399718,0.0438195167156177,
13.8561433417727));
#446674=CARTESIAN_POINT('Ctrl Pts',(2.66444324149264,0.0414406002332273,
13.8546163505474));
#446675=CARTESIAN_POINT('Ctrl Pts',(2.66553580233921,0.0393896668735282,
13.8528973491086));
#446676=CARTESIAN_POINT('Ctrl Pts',(2.66573539708665,0.0390149916074136,
13.8525833129072));
#446677=CARTESIAN_POINT('Ctrl Pts',(2.66593796172065,0.0386511458665826,
13.8522628768812));
#446678=CARTESIAN_POINT('Ctrl Pts',(2.66614222213246,0.0382983631610421,
13.851937733538));
#446679=CARTESIAN_POINT('Ctrl Pts',(2.66738961212755,0.0361439681246803,
13.8499521282529));
#446680=CARTESIAN_POINT('Ctrl Pts',(2.66882774049298,0.0341900923575475,
13.847639871647));
#446681=CARTESIAN_POINT('Ctrl Pts',(2.67031632095861,0.0324918000169361,
13.8452109780794));
#446682=CARTESIAN_POINT('Ctrl Pts',(2.67098606412217,0.0317277031399972,
13.8441181685877));
#446683=CARTESIAN_POINT('Ctrl Pts',(2.671665677395,0.0310147130681858,13.8430021611332));
#446684=CARTESIAN_POINT('Ctrl Pts',(2.67234178075526,0.0303545915713946,
13.8418824960098));
#446685=CARTESIAN_POINT('Ctrl Pts',(2.67393503558863,0.0287989984073904,
13.8392439765549));
#446686=CARTESIAN_POINT('Ctrl Pts',(2.67558232117306,0.027459925457429,
13.8364981347964));
#446687=CARTESIAN_POINT('Ctrl Pts',(2.67726640838843,0.0263072775129246,
13.8336931113419));
#446688=CARTESIAN_POINT('Ctrl Pts',(2.67890660238676,0.0251846716148906,
13.8309611966327));
#446689=CARTESIAN_POINT('Ctrl Pts',(2.68058366705995,0.0242382404134886,
13.8281701127185));
#446690=CARTESIAN_POINT('Ctrl Pts',(2.68229056279083,0.0234784653523076,
13.825358068512));
#446691=CARTESIAN_POINT('Ctrl Pts',(2.68266061962742,0.0233137452990747,
13.8247484142932));
#446692=CARTESIAN_POINT('Ctrl Pts',(2.68303204886546,0.0231579691976311,
13.8241378483365));
#446693=CARTESIAN_POINT('Ctrl Pts',(2.68340468995259,0.0230115497283485,
13.8235269408515));
#446694=CARTESIAN_POINT('',(2.66160639577871,0.0544266107312119,12.5969504640361));
#446695=CARTESIAN_POINT('Origin',(2.69600891408846,0.0550058880103093,12.584524458991));
#446696=CARTESIAN_POINT('Origin',(2.69600891408846,0.0550058880103093,12.584524458991));
#446697=CARTESIAN_POINT('Ctrl Pts',(2.68211016738736,0.0864598836326638,
12.5893111709658));
#446698=CARTESIAN_POINT('Ctrl Pts',(2.6717391495482,0.0818881636566073,
12.5770542771492));
#446699=CARTESIAN_POINT('Ctrl Pts',(2.67543256678469,0.0659456938362765,
12.5737548217797));
#446700=CARTESIAN_POINT('Ctrl Pts',(2.70478810278459,0.0964567009054791,
12.5663937883685));
#446701=CARTESIAN_POINT('Ctrl Pts',(2.69440385527188,0.0918791490656717,
12.5540940315304));
#446702=CARTESIAN_POINT('Ctrl Pts',(2.69811184599185,0.0758880015104283,
12.5508374392248));
#446703=CARTESIAN_POINT('Ctrl Pts',(2.72744315642296,0.106443431512196,
12.5434499600945));
#446704=CARTESIAN_POINT('Ctrl Pts',(2.71702514602361,0.101850996421177,
12.5311293540532));
#446705=CARTESIAN_POINT('Ctrl Pts',(2.72076849334283,0.0858216759300503,
12.5278936106989));
#446706=CARTESIAN_POINT('Ctrl Pts',(2.75007712066208,0.116420865555225,
12.5204817579905));
#446707=CARTESIAN_POINT('Ctrl Pts',(2.73960754823101,0.111805701049081,
12.5081597038247));
#446708=CARTESIAN_POINT('Ctrl Pts',(2.74340426231153,0.0957474007938997,
12.5049254088044));
#446709=CARTESIAN_POINT('Ctrl Pts',(2.73380434092627,0.109247549171251,
12.5369868989719));
#446710=CARTESIAN_POINT('Ctrl Pts',(2.73465670444891,0.109623285243511,
12.5342545179733));
#446711=CARTESIAN_POINT('Ctrl Pts',(2.7355204794619,0.109867723048072,12.5314872231885));
#446712=CARTESIAN_POINT('Ctrl Pts',(2.73636222969268,0.109913304394048,
12.5287124745063));
#446713=CARTESIAN_POINT('Ctrl Pts',(2.73712136183156,0.109954411914307,
12.5262100684185));
#446714=CARTESIAN_POINT('Ctrl Pts',(2.73786186772383,0.109832759289019,
12.5237004536639));
#446715=CARTESIAN_POINT('Ctrl Pts',(2.73858571587266,0.109480843917267,
12.5212220730815));
#446716=CARTESIAN_POINT('Ctrl Pts',(2.73913988424842,0.109211422257096,
12.5193246583487));
#446717=CARTESIAN_POINT('Ctrl Pts',(2.73969063477889,0.108803247691215,
12.5174178313692));
#446718=CARTESIAN_POINT('Ctrl Pts',(2.74019662485357,0.108168315610022,
12.515581224835));
#446719=CARTESIAN_POINT('Ctrl Pts',(2.74041217934513,0.107897831130618,
12.5147988205795));
#446720=CARTESIAN_POINT('Ctrl Pts',(2.74062004614556,0.107586092634382,
12.5140295443048));
#446721=CARTESIAN_POINT('Ctrl Pts',(2.74081915043622,0.107226453601027,
12.5132817086137));
#446722=CARTESIAN_POINT('Ctrl Pts',(2.74112046784587,0.106682188574971,
12.5121499604604));
#446723=CARTESIAN_POINT('Ctrl Pts',(2.74140196660921,0.106013001334265,
12.5110494206568));
#446724=CARTESIAN_POINT('Ctrl Pts',(2.74163579126107,0.105194174035085,
12.5100666561695));
#446725=CARTESIAN_POINT('Ctrl Pts',(2.74177005283772,0.104724005285488,
12.5095023550641));
#446726=CARTESIAN_POINT('Ctrl Pts',(2.74188951973004,0.104198888158505,
12.5089719619137));
#446727=CARTESIAN_POINT('Ctrl Pts',(2.74198572482363,0.103627248528214,
12.5085043804652));
#446728=CARTESIAN_POINT('Ctrl Pts',(2.7421265084465,0.102790728390582,12.5078201359221));
#446729=CARTESIAN_POINT('Ctrl Pts',(2.74222037021483,0.1018301202597,12.5072563000949));
#446730=CARTESIAN_POINT('Ctrl Pts',(2.7422525218129,0.100809715898123,12.5068768744332));
#446731=CARTESIAN_POINT('Ctrl Pts',(2.74227570532843,0.100073934108551,
12.5066032824114));
#446732=CARTESIAN_POINT('Ctrl Pts',(2.74226727056795,0.0992941371635123,
12.5064197834844));
#446733=CARTESIAN_POINT('Ctrl Pts',(2.74223027325681,0.0985138429906198,
12.5063282718343));
#446734=CARTESIAN_POINT('Ctrl Pts',(2.74217626863662,0.0973748550711673,
12.5061946931565));
#446735=CARTESIAN_POINT('Ctrl Pts',(2.74206131261701,0.0962104128898943,
12.5062515701262));
#446736=CARTESIAN_POINT('Ctrl Pts',(2.74190792928924,0.095091264475483,
12.5064436508398));
#446737=CARTESIAN_POINT('',(2.67543256678469,0.0659456938362764,12.5737548217797));
#446738=CARTESIAN_POINT('Origin',(2.69098419246214,0.0663290197919795,12.5893111709658));
#446739=CARTESIAN_POINT('Ctrl Pts',(2.74190792928924,0.095091264475483,
12.5064436508398));
#446740=CARTESIAN_POINT('Ctrl Pts',(2.73206804148642,0.0907765227938596,
12.5164271754438));
#446741=CARTESIAN_POINT('Ctrl Pts',(2.72222416924921,0.0864602620975741,
12.5264061185523));
#446742=CARTESIAN_POINT('Ctrl Pts',(2.71237617262926,0.082142428021385,
12.536380305637));
#446743=CARTESIAN_POINT('Ctrl Pts',(2.70006817424325,0.0767460111772602,
12.5488460165097));
#446744=CARTESIAN_POINT('Ctrl Pts',(2.6877537299547,0.0713471351528752,
12.5613043021964));
#446745=CARTESIAN_POINT('Ctrl Pts',(2.67543256678469,0.0659456938362766,
12.5737548217797));
#446746=CARTESIAN_POINT('Ctrl Pts',(2.68340468995259,0.0230115497283483,
12.5893111709658));
#446747=CARTESIAN_POINT('Ctrl Pts',(2.67285582888757,0.027156445962365,
12.5770542771492));
#446748=CARTESIAN_POINT('Ctrl Pts',(2.67589590165752,0.0432362977156746,
12.5737548217797));
#446749=CARTESIAN_POINT('Ctrl Pts',(2.67356269432808,0.0268787018642816,
12.5928319619712));
#446750=CARTESIAN_POINT('Ctrl Pts',(2.66766458388877,0.0326964084241776,
12.5821634970843));
#446751=CARTESIAN_POINT('Ctrl Pts',(2.67230724903108,0.04463622260515,12.5773203894503));
#446752=CARTESIAN_POINT('Ctrl Pts',(2.66194829594574,0.0389489068979987,
12.5969440695591));
#446753=CARTESIAN_POINT('Ctrl Pts',(2.66184802901843,0.0429674251691045,
12.5878292599214));
#446754=CARTESIAN_POINT('Ctrl Pts',(2.66816911474248,0.0489397085999056,
12.5813877129824));
#446755=CARTESIAN_POINT('Ctrl Pts',(2.66127025045685,0.069538374037137,
12.596957478804));
#446756=CARTESIAN_POINT('Ctrl Pts',(2.6613698565182,0.0655495556931358,
12.5878468778671));
#446757=CARTESIAN_POINT('Ctrl Pts',(2.66793239651539,0.0598882351119593,
12.5814011370086));
#446758=CARTESIAN_POINT('Ctrl Pts',(2.6724200483096,0.0821883153406641,
12.5928371701607));
#446759=CARTESIAN_POINT('Ctrl Pts',(2.66677262462082,0.0761350789019351,
12.5821692192952));
#446760=CARTESIAN_POINT('Ctrl Pts',(2.6718926150495,0.064395848945155,12.5773318885715));
#446761=CARTESIAN_POINT('Ctrl Pts',(2.68211016738734,0.0864598836327133,
12.5893111709658));
#446762=CARTESIAN_POINT('Ctrl Pts',(2.67173914954817,0.0818881636566572,
12.5770542771492));
#446763=CARTESIAN_POINT('Ctrl Pts',(2.67543256678466,0.0659456938363268,
12.5737548217797));
#446764=CARTESIAN_POINT('',(2.67589590165752,0.0432362977156746,12.5737548217797));
#446765=CARTESIAN_POINT('Origin',(2.69145022058562,0.0434876195864259,12.5893111709658));
#446766=CARTESIAN_POINT('Ctrl Pts',(2.67543256678466,0.0659456938363268,
12.5737548217797));
#446767=CARTESIAN_POINT('Ctrl Pts',(2.67450285684086,0.0655715828214908,
12.5746934679442));
#446768=CARTESIAN_POINT('Ctrl Pts',(2.6735424546048,0.0649876624645773,
12.5756680099006));
#446769=CARTESIAN_POINT('Ctrl Pts',(2.67265889660333,0.0642632116891434,
12.5765688348656));
#446770=CARTESIAN_POINT('Ctrl Pts',(2.67242498440375,0.0640714213662866,
12.5768073183026));
#446771=CARTESIAN_POINT('Ctrl Pts',(2.67219634824882,0.0638700142193212,
12.5770407398754));
#446772=CARTESIAN_POINT('Ctrl Pts',(2.67197462283821,0.0636607082586026,
12.5772674179684));
#446773=CARTESIAN_POINT('Ctrl Pts',(2.67106472171016,0.0628017731945181,
12.5781976435658));
#446774=CARTESIAN_POINT('Ctrl Pts',(2.6702272645626,0.0617528294358856,
12.5790594849312));
#446775=CARTESIAN_POINT('Ctrl Pts',(2.66955653511983,0.0605545745638861,
12.5797571720116));
#446776=CARTESIAN_POINT('Ctrl Pts',(2.66911953077058,0.0597738684293732,
12.580211740231));
#446777=CARTESIAN_POINT('Ctrl Pts',(2.66874982371725,0.0588851313056713,
12.5806009430798));
#446778=CARTESIAN_POINT('Ctrl Pts',(2.66848979752031,0.0579441217195207,
12.5808812374708));
#446779=CARTESIAN_POINT('Ctrl Pts',(2.66826634875435,0.0571354823083379,
12.5811221033394));
#446780=CARTESIAN_POINT('Ctrl Pts',(2.66811942934896,0.0562716568392671,
12.581287365893));
#446781=CARTESIAN_POINT('Ctrl Pts',(2.66806555161111,0.055400002967128,
12.581359338449));
#446782=CARTESIAN_POINT('Ctrl Pts',(2.66805806371808,0.0552788610778637,
12.5813693411482));
#446783=CARTESIAN_POINT('Ctrl Pts',(2.66805231537126,0.055157551545398,
12.5813775999465));
#446784=CARTESIAN_POINT('Ctrl Pts',(2.66804829221806,0.0550361836174935,
12.5813841266931));
#446785=CARTESIAN_POINT('Ctrl Pts',(2.66804146645205,0.0548302682486581,
12.5813952001081));
#446786=CARTESIAN_POINT('Ctrl Pts',(2.66804016951635,0.0546227854925812,
12.5814007534795));
#446787=CARTESIAN_POINT('Ctrl Pts',(2.66804459918174,0.0544138244820763,
12.5814005856065));
#446788=CARTESIAN_POINT('Ctrl Pts',(2.66806487645801,0.0534572826744447,
12.5813998171494));
#446789=CARTESIAN_POINT('Ctrl Pts',(2.66820341339482,0.0525358473170682,
12.58127954464));
#446790=CARTESIAN_POINT('Ctrl Pts',(2.66843016297746,0.0516503504317533,
12.5810700125799));
#446791=CARTESIAN_POINT('Ctrl Pts',(2.66870405065577,0.0505807710161861,
12.5808169217085));
#446792=CARTESIAN_POINT('Ctrl Pts',(2.66912287726063,0.0495676803812869,
12.5804173076348));
#446793=CARTESIAN_POINT('Ctrl Pts',(2.66962587073952,0.0486899145082565,
12.5799304713245));
#446794=CARTESIAN_POINT('Ctrl Pts',(2.67024923811913,0.047602086066806,
12.5793271277669));
#446795=CARTESIAN_POINT('Ctrl Pts',(2.67101260784219,0.0466386134546762,
12.5785808224116));
#446796=CARTESIAN_POINT('Ctrl Pts',(2.67185894273059,0.0458204123060168,
12.5777485681082));
#446797=CARTESIAN_POINT('Ctrl Pts',(2.67312007443723,0.0446012029538864,
12.576508418016));
#446798=CARTESIAN_POINT('Ctrl Pts',(2.67455002858849,0.0437098833501206,
12.5750928681475));
#446799=CARTESIAN_POINT('Ctrl Pts',(2.67589590165752,0.0432362977156746,
12.5737548217797));
#446800=CARTESIAN_POINT('Ctrl Pts',(2.67589590165752,0.0432362977156746,
12.5737548217797));
#446801=CARTESIAN_POINT('Ctrl Pts',(2.67285582888757,0.0271564459623653,
12.5770542771492));
#446802=CARTESIAN_POINT('Ctrl Pts',(2.68340468995259,0.0230115497283485,
12.5893111709658));
#446803=CARTESIAN_POINT('Ctrl Pts',(2.69895837453433,0.0342286732243589,
12.5508408821982));
#446804=CARTESIAN_POINT('Ctrl Pts',(2.69590572466494,0.0180995984398426,
12.55409748406));
#446805=CARTESIAN_POINT('Ctrl Pts',(2.70646804337498,0.013949414379792,
12.5663972313419));
#446806=CARTESIAN_POINT('Ctrl Pts',(2.72199788916192,0.0252287493626836,
12.52790050457));
#446807=CARTESIAN_POINT('Ctrl Pts',(2.7189114744056,0.00906009693604175,
12.5311362602938));
#446808=CARTESIAN_POINT('Ctrl Pts',(2.72950812966358,0.00489642123669558,
12.5434568539655));
#446809=CARTESIAN_POINT('Ctrl Pts',(2.74501622465285,0.0162359147937623,
12.5049357605811));
#446810=CARTESIAN_POINT('Ctrl Pts',(2.74187768010818,3.61332171347901E-5,
12.5081700652078));
#446811=CARTESIAN_POINT('Ctrl Pts',(2.75252677110501,-0.00414814572032211,
12.5204921097672));
#446812=CARTESIAN_POINT('Ctrl Pts',(2.74350474993786,0.0168264180840729,
12.5064436508395));
#446813=CARTESIAN_POINT('Ctrl Pts',(2.74371960240641,0.0156252993524972,
12.5062361689309));
#446814=CARTESIAN_POINT('Ctrl Pts',(2.74389181302113,0.0143670723759075,
12.5061871075061));
#446815=CARTESIAN_POINT('Ctrl Pts',(2.74398978877153,0.0131417489926944,
12.5063648335164));
#446816=CARTESIAN_POINT('Ctrl Pts',(2.74403429540076,0.0125851315309581,
12.5064455676329));
#446817=CARTESIAN_POINT('Ctrl Pts',(2.74406388455427,0.0120275226306801,
12.506574497099));
#446818=CARTESIAN_POINT('Ctrl Pts',(2.7440762380652,0.0114927751994334,
12.5067492519495));
#446819=CARTESIAN_POINT('Ctrl Pts',(2.74410106292495,0.0104181794789025,
12.5071004286051));
#446820=CARTESIAN_POINT('Ctrl Pts',(2.74405639076854,0.0093963762832862,
12.5076537929613));
#446821=CARTESIAN_POINT('Ctrl Pts',(2.74395502389682,0.0085036441825537,
12.5083435010505));
#446822=CARTESIAN_POINT('Ctrl Pts',(2.74394864224647,0.00844744136181337,
12.5083869222964));
#446823=CARTESIAN_POINT('Ctrl Pts',(2.74394202333457,0.00839174532599308,
12.5084308732337));
#446824=CARTESIAN_POINT('Ctrl Pts',(2.74393516538416,0.00833657279140646,
12.5084753333615));
#446825=CARTESIAN_POINT('Ctrl Pts',(2.74388015557018,0.00789401624290068,
12.5088319622689));
#446826=CARTESIAN_POINT('Ctrl Pts',(2.74380992908381,0.00747599882754801,
12.509227847131));
#446827=CARTESIAN_POINT('Ctrl Pts',(2.74372933548101,0.00709448647694972,
12.5096423454524));
#446828=CARTESIAN_POINT('Ctrl Pts',(2.74347679079905,0.0058989956204657,
12.5109411997424));
#446829=CARTESIAN_POINT('Ctrl Pts',(2.7431163762448,0.0049864259306605,
12.5124831113042));
#446830=CARTESIAN_POINT('Ctrl Pts',(2.74271472659684,0.00428957871944309,
12.5140723025008));
#446831=CARTESIAN_POINT('Ctrl Pts',(2.74267709158492,0.00422428337251766,
12.5142212114565));
#446832=CARTESIAN_POINT('Ctrl Pts',(2.74263910665875,0.00416085503539146,
12.5143705582413));
#446833=CARTESIAN_POINT('Ctrl Pts',(2.7426008349746,0.00409922362932547,
12.5145201959299));
#446834=CARTESIAN_POINT('Ctrl Pts',(2.74210917821111,0.00330747645882913,
12.5164425148273));
#446835=CARTESIAN_POINT('Ctrl Pts',(2.74156247363941,0.00277948792615719,
12.5184635205941));
#446836=CARTESIAN_POINT('Ctrl Pts',(2.74098166111635,0.00242751123111316,
12.5205025929158));
#446837=CARTESIAN_POINT('Ctrl Pts',(2.74064476683173,0.00222335079693576,
12.5216853356836));
#446838=CARTESIAN_POINT('Ctrl Pts',(2.74029725624319,0.00207836408927715,
12.5228750347131));
#446839=CARTESIAN_POINT('Ctrl Pts',(2.73994888826066,0.00197713367238996,
12.5240609649613));
#446840=CARTESIAN_POINT('Ctrl Pts',(2.73909383773684,0.00172866904496134,
12.5269717671327));
#446841=CARTESIAN_POINT('Ctrl Pts',(2.73820665657674,0.00174679574769686,
12.529903606617));
#446842=CARTESIAN_POINT('Ctrl Pts',(2.73729952787676,0.00194571695786728,
12.532813300402));
#446843=CARTESIAN_POINT('Ctrl Pts',(2.73686405328027,0.00204121072158028,
12.5342101228452));
#446844=CARTESIAN_POINT('Ctrl Pts',(2.73642463725985,0.00217876241240093,
12.5356023438239));
#446845=CARTESIAN_POINT('Ctrl Pts',(2.73598532022336,0.00235138034623309,
12.5369868989719));
#446846=CARTESIAN_POINT('Origin',(14.5962335163271,-4.66351031667956,-1.239720872067));
#446847=CARTESIAN_POINT('Ctrl Pts',(2.73376608153298,0.109230727169096,
12.5369868989719));
#446848=CARTESIAN_POINT('Ctrl Pts',(2.74781354930456,0.115391242804295,
12.5369868989719));
#446849=CARTESIAN_POINT('Ctrl Pts',(2.74689044084213,0.130702388236675,
12.5369868989719));
#446850=CARTESIAN_POINT('Ctrl Pts',(2.73851464844057,0.11131328302727,12.5218025310015));
#446851=CARTESIAN_POINT('Ctrl Pts',(2.74757029418805,0.118906118057779,
12.5216901060417));
#446852=CARTESIAN_POINT('Ctrl Pts',(2.7468932712445,0.130655715783667,12.5161920673678));
#446853=CARTESIAN_POINT('Ctrl Pts',(2.74370127747141,0.108241646575592,
12.5042015548895));
#446854=CARTESIAN_POINT('Ctrl Pts',(2.74777665524214,0.113218456903791,
12.4980677368514));
#446855=CARTESIAN_POINT('Ctrl Pts',(2.74749076155969,0.120008820997566,
12.4907278922777));
#446856=CARTESIAN_POINT('Ctrl Pts',(2.74188794022434,0.0950905712304433,
12.506463626192));
#446857=CARTESIAN_POINT('Ctrl Pts',(2.74842674848915,0.0953173416261057,
12.4999376786891));
#446858=CARTESIAN_POINT('Ctrl Pts',(2.74834688645362,0.0953145719554462,
12.4906970594712));
#446859=CARTESIAN_POINT('Origin',(2.72493031585149,0.129378413011936,12.5369868989719));
#446860=CARTESIAN_POINT('Origin',(2.72493031585149,0.129378413011936,14.));
#446861=CARTESIAN_POINT('Origin',(2.72493031585149,0.129378413011936,13.7435492065112));
#446862=CARTESIAN_POINT('Ctrl Pts',(2.7111478626189,0.0992602202188586,
13.793642941384));
#446863=CARTESIAN_POINT('Ctrl Pts',(2.72105250706917,0.103596605501525,
13.8071662555867));
#446864=CARTESIAN_POINT('Ctrl Pts',(2.71659034273042,0.120031582624993,
13.8103758687955));
#446865=CARTESIAN_POINT('Ctrl Pts',(2.72635684332379,0.105964592757806,
13.7804579775006));
#446866=CARTESIAN_POINT('Ctrl Pts',(2.73857421226988,0.111324589750697,
13.7901904343351));
#446867=CARTESIAN_POINT('Ctrl Pts',(2.73696039359074,0.126997863608927,
13.7927914348262));
#446868=CARTESIAN_POINT('Ctrl Pts',(2.73531094262778,0.10991170922021,13.7597120340895));
#446869=CARTESIAN_POINT('Ctrl Pts',(2.74944757691701,0.116119982808342,
13.7635825532445));
#446870=CARTESIAN_POINT('Ctrl Pts',(2.74896431761631,0.13113005864401,13.7651073818884));
#446871=CARTESIAN_POINT('Ctrl Pts',(2.73355752495816,0.10913877343892,13.7381884353898));
#446872=CARTESIAN_POINT('Ctrl Pts',(2.74736362640026,0.115200907848243,
13.7368803041982));
#446873=CARTESIAN_POINT('Ctrl Pts',(2.74661343172915,0.130321319386107,
13.7363986145813));
#446874=CARTESIAN_POINT('Origin',(2.70596428021828,0.121017863901359,13.7902182540695));
#446875=CARTESIAN_POINT('Ctrl Pts',(2.68210656530513,0.0864582966033172,
13.8235227101244));
#446876=CARTESIAN_POINT('Ctrl Pts',(2.69262862607313,0.0910917537914321,
13.8358800583119));
#446877=CARTESIAN_POINT('Ctrl Pts',(2.68878013986014,0.107210537955413,
13.8390832900376));
#446878=CARTESIAN_POINT('Ctrl Pts',(2.69302076875767,0.0912694619810058,
13.8124254819052));
#446879=CARTESIAN_POINT('Ctrl Pts',(2.70356326310642,0.0959119175318677,
13.8247886449158));
#446880=CARTESIAN_POINT('Ctrl Pts',(2.6996933358596,0.11204711025482,13.8279860620657));
#446881=CARTESIAN_POINT('Ctrl Pts',(2.70393008081926,0.0960784711508696,
13.8013225099955));
#446882=CARTESIAN_POINT('Ctrl Pts',(2.71448803519229,0.100727732736346,
13.8136962257787));
#446883=CARTESIAN_POINT('Ctrl Pts',(2.7106015894118,0.116881195649208,13.8168830918626));
#446884=CARTESIAN_POINT('Ctrl Pts',(2.71483469180648,0.10088540800767,13.7902140179785));
#446885=CARTESIAN_POINT('Ctrl Pts',(2.72540345770452,0.105539426587026,
13.802602731458));
#446886=CARTESIAN_POINT('Ctrl Pts',(2.72150509546317,0.121712890172682,
13.8057746032558));
#446887=CARTESIAN_POINT('Origin',(2.67323614231258,0.106590747473348,13.8235269408515));
#446888=CARTESIAN_POINT('Ctrl Pts',(2.68340468995259,0.0230115497283484,
13.8235269408515));
#446889=CARTESIAN_POINT('Ctrl Pts',(2.69439427247702,0.0186934836415734,
13.8362179249168));
#446890=CARTESIAN_POINT('Ctrl Pts',(2.69080185486037,0.00199744998909402,
13.8391868794938));
#446891=CARTESIAN_POINT('Ctrl Pts',(2.67334970029081,0.0269623922435091,
13.8400110824519));
#446892=CARTESIAN_POINT('Ctrl Pts',(2.68090957753351,0.0203163318362425,
13.8494522556837));
#446893=CARTESIAN_POINT('Ctrl Pts',(2.67429527008017,0.00860399541908111,
13.85569149686));
#446894=CARTESIAN_POINT('Ctrl Pts',(2.66195470361959,0.0386050627665757,
13.8586819406588));
#446895=CARTESIAN_POINT('Ctrl Pts',(2.662057420685,0.0342524207138181,13.868010383617));
#446896=CARTESIAN_POINT('Ctrl Pts',(2.65548369043046,0.0280331814248738,
13.8744918421245));
#446897=CARTESIAN_POINT('Ctrl Pts',(2.66126372479098,0.0698875506184945,
13.8587686893867));
#446898=CARTESIAN_POINT('Ctrl Pts',(2.6611618656138,0.0742014528691105,
13.8680909899357));
#446899=CARTESIAN_POINT('Ctrl Pts',(2.65433598590387,0.0801093939395106,
13.8745789365163));
#446900=CARTESIAN_POINT('Ctrl Pts',(2.67220860875548,0.0820951092181263,
13.8400379222776));
#446901=CARTESIAN_POINT('Ctrl Pts',(2.67948431216712,0.089047401917223,
13.8494748685453));
#446902=CARTESIAN_POINT('Ctrl Pts',(2.67240200346499,0.10047552550389,13.8557104837033));
#446903=CARTESIAN_POINT('Ctrl Pts',(2.68211016738456,0.0864598836386525,
13.8235269408542));
#446904=CARTESIAN_POINT('Ctrl Pts',(2.69291447656097,0.0912226057606148,
13.8362179249195));
#446905=CARTESIAN_POINT('Ctrl Pts',(2.68864404095105,0.107758215327781,
13.8391868794965));
#446906=CARTESIAN_POINT('Origin',(2.67535915931955,0.00253547987027109,
13.8235269408515));
#446907=CARTESIAN_POINT('Ctrl Pts',(2.71669038311477,0.00993281525666357,
13.7902140241682));
#446908=CARTESIAN_POINT('Ctrl Pts',(2.72744017785787,0.00571375038707416,
13.8026027327198));
#446909=CARTESIAN_POINT('Ctrl Pts',(2.72420475383482,-0.0106052558223891,
13.8057746032556));
#446910=CARTESIAN_POINT('Ctrl Pts',(2.70559877879061,0.0142909681151822,
13.8013225161808));
#446911=CARTESIAN_POINT('Ctrl Pts',(2.71633757698319,0.0100762153034338,
13.8136962270464));
#446912=CARTESIAN_POINT('Ctrl Pts',(2.7131132437,-0.00622232083304009,13.8168830918628));
#446913=CARTESIAN_POINT('Ctrl Pts',(2.69450239277601,0.018650999812628,
13.8124254880875));
#446914=CARTESIAN_POINT('Ctrl Pts',(2.70522546621405,0.014442416787074,
13.8247886461867));
#446915=CARTESIAN_POINT('Ctrl Pts',(2.70201689249577,-0.00183719060661763,
13.8279860620656));
#446916=CARTESIAN_POINT('Ctrl Pts',(2.68340103148947,0.0230129864117414,
13.8235227163065));
#446917=CARTESIAN_POINT('Ctrl Pts',(2.69410332133798,0.0188125608100677,
13.8358800595847));
#446918=CARTESIAN_POINT('Ctrl Pts',(2.69091550151957,0.00255022285996103,
13.8390832900376));
#446919=CARTESIAN_POINT('Origin',(2.70864852252747,-0.0105446958323901,
13.7902182540695));
#446920=CARTESIAN_POINT('Ctrl Pts',(2.73573414330807,0.00245004404107459,
13.7382347919292));
#446921=CARTESIAN_POINT('Ctrl Pts',(2.74978792632498,-0.00304623212072527,
13.7369371795943));
#446922=CARTESIAN_POINT('Ctrl Pts',(2.74964670705973,-0.0181962761516587,
13.7364597369711));
#446923=CARTESIAN_POINT('Ctrl Pts',(2.73749467465009,0.00175829019900498,
13.7595490285573));
#446924=CARTESIAN_POINT('Ctrl Pts',(2.75188340268191,-0.00387005876363533,
13.7633824266925));
#446925=CARTESIAN_POINT('Ctrl Pts',(2.75199955109843,-0.018899369122145,
13.7648920890506));
#446926=CARTESIAN_POINT('Ctrl Pts',(2.72851606125849,0.00528619690360507,
13.7803806590111));
#446927=CARTESIAN_POINT('Ctrl Pts',(2.74096376258398,0.000422904015543165,
13.7901039518745));
#446928=CARTESIAN_POINT('Ctrl Pts',(2.74000555828081,-0.0153113670492094,
13.7926933640892));
#446929=CARTESIAN_POINT('Ctrl Pts',(2.71290922687708,0.0114184862122857,
13.7936647693663));
#446930=CARTESIAN_POINT('Ctrl Pts',(2.72298639143274,0.0074911351377519,
13.8072068914933));
#446931=CARTESIAN_POINT('Ctrl Pts',(2.71918393058566,-0.00912769639016085,
13.8104111085397));
#446932=CARTESIAN_POINT('Origin',(2.72793978959033,-0.0181246895118446,
13.7435492065112));
#446933=CARTESIAN_POINT('Origin',(2.72793978959033,-0.0181246895118447,
14.));
#446934=CARTESIAN_POINT('Origin',(2.72793978959033,-0.0181246895118445,
12.5369868989719));
#446935=CARTESIAN_POINT('Ctrl Pts',(2.7434863670468,0.0168263053487349,
12.506462012331));
#446936=CARTESIAN_POINT('Ctrl Pts',(2.75002486686205,0.0168664071679876,
12.4999388158272));
#446937=CARTESIAN_POINT('Ctrl Pts',(2.74994750783452,0.0168659327108754,
12.4907030323752));
#446938=CARTESIAN_POINT('Ctrl Pts',(2.74583256172836,0.00376016767646571,
12.5042014951932));
#446939=CARTESIAN_POINT('Ctrl Pts',(2.75010638582298,-0.00104353139032467,
12.4980716682127));
#446940=CARTESIAN_POINT('Ctrl Pts',(2.75009927474382,-0.00783510813351349,
12.4907355092743));
#446941=CARTESIAN_POINT('Ctrl Pts',(2.74077753690017,0.000478030380158065,
12.5218047446509));
#446942=CARTESIAN_POINT('Ctrl Pts',(2.75013006992358,-0.00673646870034738,
12.5216906929434));
#446943=CARTESIAN_POINT('Ctrl Pts',(2.74993668683658,-0.0184979888959359,
12.5161988840776));
#446944=CARTESIAN_POINT('Ctrl Pts',(2.7359495529117,0.00236539812914527,
12.5369868989719));
#446945=CARTESIAN_POINT('Ctrl Pts',(2.75022731620137,-0.00321591058522313,
12.5369868989719));
#446946=CARTESIAN_POINT('Ctrl Pts',(2.74993581177919,-0.01854302892797,
12.5369868989719));
#446947=CARTESIAN_POINT('Origin',(5.15079064385546E-31,-5.04677213932911E-31,
12.5));
#446948=CARTESIAN_POINT('Origin',(2.67260022728041,0.241657374439811,12.5));
#446949=CARTESIAN_POINT('',(2.67260022728041,0.241657374439811,12.5893111709658));
#446950=CARTESIAN_POINT('',(2.67260022728041,0.241657374439811,13.8235269408515));
#446951=CARTESIAN_POINT('',(2.67260022728041,0.241657374439811,12.5));
#446952=CARTESIAN_POINT('',(2.70684497862863,0.231334114087577,13.7902182540695));
#446953=CARTESIAN_POINT('',(2.67260022728041,0.241657374439811,13.8235269408515));
#446954=CARTESIAN_POINT('',(2.72668989544585,0.225351759568795,13.7435492065112));
#446955=CARTESIAN_POINT('Origin',(2.66140047544984,0.245033938752029,13.7445212918703));
#446956=CARTESIAN_POINT('',(2.72668989544585,0.225351759568795,12.5369868989719));
#446957=CARTESIAN_POINT('',(2.72668989544585,0.225351759568795,12.5));
#446958=CARTESIAN_POINT('Ctrl Pts',(2.72668989544585,0.225351759568795,
12.5369868989719));
#446959=CARTESIAN_POINT('Ctrl Pts',(2.70867315596209,0.230783000417881,
12.5544431401645));
#446960=CARTESIAN_POINT('Ctrl Pts',(2.69064353042739,0.236218125834777,
12.5718848856037));
#446961=CARTESIAN_POINT('Ctrl Pts',(2.67260022728041,0.241657374439811,
12.5893111709658));
#446962=CARTESIAN_POINT('Origin',(2.90789544171731,0.435855945855819,12.5));
#446963=CARTESIAN_POINT('',(2.71580314304261,0.331714470150425,13.7435492065112));
#446964=CARTESIAN_POINT('',(2.69758167769643,0.321835832101125,13.7902182540695));
#446965=CARTESIAN_POINT('Origin',(2.64969881607086,0.295876478680461,13.7418732680453));
#446966=CARTESIAN_POINT('',(2.66613838389343,0.304789073640352,13.8235269408515));
#446967=CARTESIAN_POINT('',(2.69758167769643,0.321835832101125,13.7902182540695));
#446968=CARTESIAN_POINT('',(2.66613838389343,0.304789073640352,12.5893111709658));
#446969=CARTESIAN_POINT('',(2.66613838389343,0.304789073640352,12.5));
#446970=CARTESIAN_POINT('',(2.71580314304261,0.331714470150425,12.5369868989719));
#446971=CARTESIAN_POINT('Ctrl Pts',(2.66613838389343,0.304789073640352,
12.5893111709658));
#446972=CARTESIAN_POINT('Ctrl Pts',(2.68270562003009,0.313770883070166,
12.5718848856037));
#446973=CARTESIAN_POINT('Ctrl Pts',(2.69926029747776,0.322745883895925,
12.5544431401645));
#446974=CARTESIAN_POINT('Ctrl Pts',(2.71580314304261,0.331714470150425,
12.5369868989719));
#446975=CARTESIAN_POINT('',(2.71580314304261,0.331714470150425,12.5));
#446976=CARTESIAN_POINT('Origin',(2.68252174292037,0.274569441412368,12.5));
#446977=CARTESIAN_POINT('',(2.64845827287882,0.269957480776539,13.8587068136939));
#446978=CARTESIAN_POINT('Ctrl Pts',(2.66613838389016,0.304789073646093,
13.8235269408542));
#446979=CARTESIAN_POINT('Ctrl Pts',(2.66459790938839,0.303953916333649,
13.8262006681044));
#446980=CARTESIAN_POINT('Ctrl Pts',(2.66310426415996,0.302946517721572,
13.8288634856214));
#446981=CARTESIAN_POINT('Ctrl Pts',(2.66165538025358,0.301780050874266,
13.8314912288862));
#446982=CARTESIAN_POINT('Ctrl Pts',(2.66016173039156,0.300577543870169,
13.8342001611531));
#446983=CARTESIAN_POINT('Ctrl Pts',(2.65871367987522,0.299205038716938,
13.8368750301949));
#446984=CARTESIAN_POINT('Ctrl Pts',(2.65731915339264,0.297632930257845,
13.8394886372969));
#446985=CARTESIAN_POINT('Ctrl Pts',(2.65721145072974,0.297511512508148,
13.8396904925131));
#446986=CARTESIAN_POINT('Ctrl Pts',(2.65710408111859,0.297388886822745,
13.8398919674349));
#446987=CARTESIAN_POINT('Ctrl Pts',(2.65699705609362,0.297265031267804,
13.8400930404591));
#446988=CARTESIAN_POINT('Ctrl Pts',(2.65532953420179,0.295335278395877,
13.8432258934518));
#446989=CARTESIAN_POINT('Ctrl Pts',(2.65375332029132,0.293117548342098,
13.8462331177034));
#446990=CARTESIAN_POINT('Ctrl Pts',(2.65239845173984,0.290628286762467,
13.8489036603661));
#446991=CARTESIAN_POINT('Ctrl Pts',(2.6519551229824,0.289813771404618,13.8497774930041));
#446992=CARTESIAN_POINT('Ctrl Pts',(2.65153571332566,0.288970302071231,
13.85061494757));
#446993=CARTESIAN_POINT('Ctrl Pts',(2.6511454016974,0.288098803041728,13.8514076489583));
#446994=CARTESIAN_POINT('Ctrl Pts',(2.65031983631224,0.286255456905349,
13.8530843267192));
#446995=CARTESIAN_POINT('Ctrl Pts',(2.64954605802412,0.284104436387558,
13.8546805203176));
#446996=CARTESIAN_POINT('Ctrl Pts',(2.64899736789653,0.281724400257269,
13.8559412814274));
#446997=CARTESIAN_POINT('Ctrl Pts',(2.64892393536301,0.281405874236645,
13.8561100121513));
#446998=CARTESIAN_POINT('Ctrl Pts',(2.64885448857294,0.281083307939024,
13.8562727473908));
#446999=CARTESIAN_POINT('Ctrl Pts',(2.64878939042725,0.280756944642768,
13.8564289040185));
#447000=CARTESIAN_POINT('Ctrl Pts',(2.64849417107922,0.279276890817491,
13.8571370725437));
#447001=CARTESIAN_POINT('Ctrl Pts',(2.64828542980016,0.277692286949607,
13.8577210840553));
#447002=CARTESIAN_POINT('Ctrl Pts',(2.64820037707139,0.276060893943153,
13.8581177131616));
#447003=CARTESIAN_POINT('Ctrl Pts',(2.64817642329555,0.27560143752169,13.8582294175695));
#447004=CARTESIAN_POINT('Ctrl Pts',(2.64816210811965,0.275138313700649,
13.8583265086086));
#447005=CARTESIAN_POINT('Ctrl Pts',(2.64815783106657,0.274672895613218,
13.8584082369006));
#447006=CARTESIAN_POINT('Ctrl Pts',(2.64815168608824,0.274004214628378,
13.8585256585398));
#447007=CARTESIAN_POINT('Ctrl Pts',(2.64816650872132,0.273322481571864,
13.8586122832068));
#447008=CARTESIAN_POINT('Ctrl Pts',(2.64820270341718,0.272645423058428,
13.8586682984299));
#447009=CARTESIAN_POINT('Ctrl Pts',(2.648231655586,0.272103843362332,13.8587131050557));
#447010=CARTESIAN_POINT('Ctrl Pts',(2.64827436811453,0.271559260363451,
13.8587357943552));
#447011=CARTESIAN_POINT('Ctrl Pts',(2.64833135097359,0.271011648950174,
13.8587355499465));
#447012=CARTESIAN_POINT('Ctrl Pts',(2.64836818035393,0.270657714638112,
13.8587353919793));
#447013=CARTESIAN_POINT('Ctrl Pts',(2.64841053421112,0.270306338648496,
13.8587257282814));
#447014=CARTESIAN_POINT('Ctrl Pts',(2.64845827287882,0.269957480776539,
13.8587068136939));
#447015=CARTESIAN_POINT('Ctrl Pts',(2.64845827287882,0.269957480776539,
13.8587068136939));
#447016=CARTESIAN_POINT('Ctrl Pts',(2.64861528275439,0.268810106253877,
13.8586446046466));
#447017=CARTESIAN_POINT('Ctrl Pts',(2.64883046929107,0.267689936275346,
13.858482427929));
#447018=CARTESIAN_POINT('Ctrl Pts',(2.64909951027578,0.266595828723968,
13.8582284286032));
#447019=CARTESIAN_POINT('Ctrl Pts',(2.64937551502996,0.265473401648074,
13.8579678548414));
#447020=CARTESIAN_POINT('Ctrl Pts',(2.64971035976198,0.264376027596299,
13.857615680862));
#447021=CARTESIAN_POINT('Ctrl Pts',(2.65008157564184,0.263344141808986,
13.8571944833187));
#447022=CARTESIAN_POINT('Ctrl Pts',(2.65100798283486,0.260768965294124,
13.8561433417727));
#447023=CARTESIAN_POINT('Ctrl Pts',(2.6521997327729,0.25847956972044,13.8546163505474));
#447024=CARTESIAN_POINT('Ctrl Pts',(2.65345582832213,0.256524514524141,
13.8528973491086));
#447025=CARTESIAN_POINT('Ctrl Pts',(2.65368529844701,0.256167354783928,
13.8525833129072));
#447026=CARTESIAN_POINT('Ctrl Pts',(2.65391684586957,0.255821230607973,
13.8522628768812));
#447027=CARTESIAN_POINT('Ctrl Pts',(2.65414918168728,0.255486270877606,
13.851937733538));
#447028=CARTESIAN_POINT('Ctrl Pts',(2.65556802429095,0.25344071827781,13.8499521282529));
#447029=CARTESIAN_POINT('Ctrl Pts',(2.6571606264168,0.251610564683827,13.847639871647));
#447030=CARTESIAN_POINT('Ctrl Pts',(2.65878268034566,0.250039256398138,
13.8452109780794));
#447031=CARTESIAN_POINT('Ctrl Pts',(2.6595124759831,0.249332292275942,13.8441181685877));
#447032=CARTESIAN_POINT('Ctrl Pts',(2.66024794320876,0.248677069410731,
13.8430021611332));
#447033=CARTESIAN_POINT('Ctrl Pts',(2.66097560292113,0.248074253114259,
13.8418824960098));
#447034=CARTESIAN_POINT('Ctrl Pts',(2.66269035161476,0.246653701118163,
13.8392439765549));
#447035=CARTESIAN_POINT('Ctrl Pts',(2.66444130286906,0.245453352890766,
13.8364981347964));
#447036=CARTESIAN_POINT('Ctrl Pts',(2.66621373793127,0.244441809029569,
13.8336931113419));
#447037=CARTESIAN_POINT('Ctrl Pts',(2.66793997712183,0.243456629547738,
13.8309611966328));
#447038=CARTESIAN_POINT('Ctrl Pts',(2.66968860442981,0.242650043858058,
13.8281701127186));
#447039=CARTESIAN_POINT('Ctrl Pts',(2.67145174932685,0.242031924733829,
13.8253580685121));
#447040=CARTESIAN_POINT('Ctrl Pts',(2.67183400104338,0.241897915840601,
13.8247484142933));
#447041=CARTESIAN_POINT('Ctrl Pts',(2.67221689157971,0.241772933002361,
13.8241378483365));
#447042=CARTESIAN_POINT('Ctrl Pts',(2.67260022728041,0.241657374439811,
13.8235269408515));
#447043=CARTESIAN_POINT('',(2.64831384601723,0.271191141078042,12.5969504640361));
#447044=CARTESIAN_POINT('Origin',(2.68255467630933,0.274572615479468,12.584524458991));
#447045=CARTESIAN_POINT('Origin',(2.68255467630933,0.274572615479468,12.584524458991));
#447046=CARTESIAN_POINT('Ctrl Pts',(2.66613838389343,0.304789073640352,
12.5893111709658));
#447047=CARTESIAN_POINT('Ctrl Pts',(2.65617451238041,0.299387231451652,
12.5770542771492));
#447048=CARTESIAN_POINT('Ctrl Pts',(2.66115509936875,0.283798856677273,
12.5737548217797));
#447049=CARTESIAN_POINT('Ctrl Pts',(2.68792602691775,0.316601089594918,
12.5663937883685));
#447050=CARTESIAN_POINT('Ctrl Pts',(2.67794944510285,0.311192356606314,
12.5540940315304));
#447051=CARTESIAN_POINT('Ctrl Pts',(2.68294852476992,0.295556653942359,
12.5508374392248));
#447052=CARTESIAN_POINT('Ctrl Pts',(2.70969168647735,0.328401187370187,
12.5434499600945));
#447053=CARTESIAN_POINT('Ctrl Pts',(2.69968266724224,0.322974868664596,
12.5311293540533));
#447054=CARTESIAN_POINT('Ctrl Pts',(2.70472009731098,0.307304001972979,
12.5278936106989));
#447055=CARTESIAN_POINT('Ctrl Pts',(2.73143708456714,0.340190300533473,
12.5204817579905));
#447056=CARTESIAN_POINT('Ctrl Pts',(2.721378527527,0.334737125258597,12.5081597038247));
#447057=CARTESIAN_POINT('Ctrl Pts',(2.7264715089034,0.319041725117335,12.5049254088044));
#447058=CARTESIAN_POINT('Ctrl Pts',(2.7158031430426,0.331714470150424,12.5369868989719));
#447059=CARTESIAN_POINT('Ctrl Pts',(2.71662204441789,0.332158431531958,
12.5342545179733));
#447060=CARTESIAN_POINT('Ctrl Pts',(2.71746302134045,0.332472461672344,
12.5314872231885));
#447061=CARTESIAN_POINT('Ctrl Pts',(2.71829825541393,0.332586501808387,
12.5287124745063));
#447062=CARTESIAN_POINT('Ctrl Pts',(2.71905151095872,0.332689348863517,
12.5262100684184));
#447063=CARTESIAN_POINT('Ctrl Pts',(2.71979946869705,0.332628459132043,
12.5237004536639));
#447064=CARTESIAN_POINT('Ctrl Pts',(2.72054959267069,0.332336715073668,
12.5212220730815));
#447065=CARTESIAN_POINT('Ctrl Pts',(2.72112387746341,0.332113359759108,
12.5193246583486));
#447066=CARTESIAN_POINT('Ctrl Pts',(2.72170606543337,0.331751434641541,
12.517417831369));
#447067=CARTESIAN_POINT('Ctrl Pts',(2.72226212472689,0.331159858132885,
12.5155812248348));
#447068=CARTESIAN_POINT('Ctrl Pts',(2.72249900897475,0.33090784336046,12.5147988205793));
#447069=CARTESIAN_POINT('Ctrl Pts',(2.72273159369701,0.330614085222352,
12.5140295443047));
#447070=CARTESIAN_POINT('Ctrl Pts',(2.72295934940448,0.330271871706331,
12.5132817086137));
#447071=CARTESIAN_POINT('Ctrl Pts',(2.72330402685765,0.329753977843431,
12.5121499604604));
#447072=CARTESIAN_POINT('Ctrl Pts',(2.72363913392964,0.329109962030609,
12.5110494206568));
#447073=CARTESIAN_POINT('Ctrl Pts',(2.72393892257576,0.328312918191567,
12.5100666561695));
#447074=CARTESIAN_POINT('Ctrl Pts',(2.72411106052602,0.327855257454619,
12.5095023550641));
#447075=CARTESIAN_POINT('Ctrl Pts',(2.72427293182291,0.327341625272324,
12.5089719619137));
#447076=CARTESIAN_POINT('Ctrl Pts',(2.7244154107387,0.326779729333997,12.5085043804652));
#447077=CARTESIAN_POINT('Ctrl Pts',(2.72462391007277,0.32595746782035,12.5078201359221));
#447078=CARTESIAN_POINT('Ctrl Pts',(2.72479575800432,0.325007706639303,
12.5072563000949));
#447079=CARTESIAN_POINT('Ctrl Pts',(2.72491097504904,0.323993318242785,
12.5068768744332));
#447080=CARTESIAN_POINT('Ctrl Pts',(2.72499405446985,0.32326187437816,12.5066032824114));
#447081=CARTESIAN_POINT('Ctrl Pts',(2.72504920846564,0.322483984631845,
12.5064197834844));
#447082=CARTESIAN_POINT('Ctrl Pts',(2.72507593547899,0.321703271199118,
12.5063282718343));
#447083=CARTESIAN_POINT('Ctrl Pts',(2.725114948644,0.320563671290108,12.5061946931565));
#447084=CARTESIAN_POINT('Ctrl Pts',(2.72509528797899,0.319393733711336,
12.5062515701262));
#447085=CARTESIAN_POINT('Ctrl Pts',(2.72503363600704,0.318265807005796,
12.5064436508398));
#447086=CARTESIAN_POINT('',(2.66115509936875,0.283798856677273,12.5737548217797));
#447087=CARTESIAN_POINT('Origin',(2.67662373367067,0.285448509014443,12.5893111709658));
#447088=CARTESIAN_POINT('Ctrl Pts',(2.72503363600704,0.318265807005796,
12.5064436508398));
#447089=CARTESIAN_POINT('Ctrl Pts',(2.71557818112231,0.313163380066183,
12.5164271754438));
#447090=CARTESIAN_POINT('Ctrl Pts',(2.70611887887486,0.308059114397915,
12.5264061185523));
#447091=CARTESIAN_POINT('Ctrl Pts',(2.69665559421328,0.302952944409553,
12.536380305637));
#447092=CARTESIAN_POINT('Ctrl Pts',(2.68482840774724,0.296571267566963,
12.5488460165097));
#447093=CARTESIAN_POINT('Ctrl Pts',(2.6729949972729,0.290186614325933,12.5613043021964));
#447094=CARTESIAN_POINT('Ctrl Pts',(2.66115509936875,0.283798856677273,
12.5737548217797));
#447095=CARTESIAN_POINT('Ctrl Pts',(2.67260022728041,0.241657374439812,
12.5893111709658));
#447096=CARTESIAN_POINT('Ctrl Pts',(2.66174861915796,0.244928648765893,
12.5770542771492));
#447097=CARTESIAN_POINT('Ctrl Pts',(2.66346791914059,0.261202790292396,
12.5737548217797));
#447098=CARTESIAN_POINT('Ctrl Pts',(2.66247577128447,0.244709444934003,
12.5928319619712));
#447099=CARTESIAN_POINT('Ctrl Pts',(2.6561230892275,0.250027042799071,12.5821634970842));
#447100=CARTESIAN_POINT('Ctrl Pts',(2.65977710058497,0.262305548542808,
12.5773203894503));
#447101=CARTESIAN_POINT('Ctrl Pts',(2.64991618509006,0.255792806065218,
12.5969440695591));
#447102=CARTESIAN_POINT('Ctrl Pts',(2.64948870524748,0.259789780362872,
12.5878292599214));
#447103=CARTESIAN_POINT('Ctrl Pts',(2.65530196153665,0.266257418681842,
12.5813877129824));
#447104=CARTESIAN_POINT('Ctrl Pts',(2.646747070191,0.286225222273891,12.596957478804));
#447105=CARTESIAN_POINT('Ctrl Pts',(2.64717147054681,0.282257795212573,
12.5878468778671));
#447106=CARTESIAN_POINT('Ctrl Pts',(2.65417362441804,0.277150220142025,
12.5814011370086));
#447107=CARTESIAN_POINT('Ctrl Pts',(2.65682868035863,0.299741883975949,
12.5928371701607));
#447108=CARTESIAN_POINT('Ctrl Pts',(2.65169344297155,0.29324847172335,12.5821692192952));
#447109=CARTESIAN_POINT('Ctrl Pts',(2.65775325327763,0.281965629837448,
12.5773318885715));
#447110=CARTESIAN_POINT('Ctrl Pts',(2.6661383838934,0.304789073640399,12.5893111709658));
#447111=CARTESIAN_POINT('Ctrl Pts',(2.65617451238038,0.299387231451699,
12.5770542771492));
#447112=CARTESIAN_POINT('Ctrl Pts',(2.66115509936873,0.283798856677322,
12.5737548217797));
#447113=CARTESIAN_POINT('',(2.66346791914059,0.261202790292396,12.5737548217797));
#447114=CARTESIAN_POINT('Origin',(2.67894999728998,0.262721097302248,12.5893111709658));
#447115=CARTESIAN_POINT('Ctrl Pts',(2.66115509936873,0.283798856677322,
12.5737548217797));
#447116=CARTESIAN_POINT('Ctrl Pts',(2.66025897647886,0.283350210494603,
12.5746934679442));
#447117=CARTESIAN_POINT('Ctrl Pts',(2.65934936483196,0.282689951386333,
12.5756680099006));
#447118=CARTESIAN_POINT('Ctrl Pts',(2.65852779626052,0.281895892981424,
12.5765688348656));
#447119=CARTESIAN_POINT('Ctrl Pts',(2.65831029507629,0.281685674809241,
12.5768073183026));
#447120=CARTESIAN_POINT('Ctrl Pts',(2.65809883624155,0.281466301858757,
12.5770407398754));
#447121=CARTESIAN_POINT('Ctrl Pts',(2.65789490898285,0.281239619666989,
12.5772674179684));
#447122=CARTESIAN_POINT('Ctrl Pts',(2.65705804665743,0.280309377249427,
12.5781976435658));
#447123=CARTESIAN_POINT('Ctrl Pts',(2.65630887473369,0.27919566323252,12.5790594849312));
#447124=CARTESIAN_POINT('Ctrl Pts',(2.65573804598393,0.277946724778423,
12.5797571720116));
#447125=CARTESIAN_POINT('Ctrl Pts',(2.65536613052829,0.277132996467755,
12.580211740231));
#447126=CARTESIAN_POINT('Ctrl Pts',(2.65507009397089,0.276217081986477,
12.5806009430798));
#447127=CARTESIAN_POINT('Ctrl Pts',(2.65488763400685,0.275258008983081,
12.5808812374708));
#447128=CARTESIAN_POINT('Ctrl Pts',(2.65473084036728,0.274433847104006,
12.5811221033394));
#447129=CARTESIAN_POINT('Ctrl Pts',(2.65465481961918,0.273560920647447,
12.581287365893));
#447130=CARTESIAN_POINT('Ctrl Pts',(2.65467216903768,0.272687775595847,
12.581359338449));
#447131=CARTESIAN_POINT('Ctrl Pts',(2.6546745802486,0.272566426463433,12.5813693411482));
#447132=CARTESIAN_POINT('Ctrl Pts',(2.65467873888201,0.272445052034801,
12.5813775999465));
#447133=CARTESIAN_POINT('Ctrl Pts',(2.65468462172837,0.272323760024331,
12.5813841266931));
#447134=CARTESIAN_POINT('Ctrl Pts',(2.65469460268872,0.272117973458602,
12.5813952001081));
#447135=CARTESIAN_POINT('Ctrl Pts',(2.65471022183926,0.27191107537198,12.5814007534795));
#447136=CARTESIAN_POINT('Ctrl Pts',(2.65473166902756,0.271703170720852,
12.5814005856065));
#447137=CARTESIAN_POINT('Ctrl Pts',(2.65482984587029,0.270751464513437,
12.5813998171494));
#447138=CARTESIAN_POINT('Ctrl Pts',(2.65504302737269,0.269844387202663,
12.58127954464));
#447139=CARTESIAN_POINT('Ctrl Pts',(2.6553411986815,0.268980318931211,12.5810700125799));
#447140=CARTESIAN_POINT('Ctrl Pts',(2.65570135567302,0.267936622841347,
12.5808169217085));
#447141=CARTESIAN_POINT('Ctrl Pts',(2.65620136495872,0.266961041438454,
12.5804173076348));
#447142=CARTESIAN_POINT('Ctrl Pts',(2.65677423083573,0.266127194897048,
12.5799304713245));
#447143=CARTESIAN_POINT('Ctrl Pts',(2.6574841921287,0.265093796343496,12.5793271277669));
#447144=CARTESIAN_POINT('Ctrl Pts',(2.6583235537643,0.26419575132621,12.5785808224116));
#447145=CARTESIAN_POINT('Ctrl Pts',(2.65923376353261,0.263449256824771,
12.5777485681082));
#447146=CARTESIAN_POINT('Ctrl Pts',(2.66059007580831,0.262336898233048,
12.576508418016));
#447147=CARTESIAN_POINT('Ctrl Pts',(2.66208792272741,0.26156509896011,12.5750928681475));
#447148=CARTESIAN_POINT('Ctrl Pts',(2.66346791914059,0.261202790292396,
12.5737548217797));
#447149=CARTESIAN_POINT('Ctrl Pts',(2.66346791914059,0.261202790292396,
12.5737548217797));
#447150=CARTESIAN_POINT('Ctrl Pts',(2.66174861915796,0.244928648765893,
12.5770542771492));
#447151=CARTESIAN_POINT('Ctrl Pts',(2.67260022728041,0.241657374439811,
12.5893111709658));
#447152=CARTESIAN_POINT('Ctrl Pts',(2.68718785856017,0.254104943569506,
12.5508408821982));
#447153=CARTESIAN_POINT('Ctrl Pts',(2.68546003546135,0.237780717647012,
12.55409748406));
#447154=CARTESIAN_POINT('Ctrl Pts',(2.69632548745655,0.234505270012706,
12.5663972313419));
#447155=CARTESIAN_POINT('Ctrl Pts',(2.71088428844942,0.247012900542605,
12.52790050457));
#447156=CARTESIAN_POINT('Ctrl Pts',(2.70912603875879,0.230646476517585,
12.5311362602938));
#447157=CARTESIAN_POINT('Ctrl Pts',(2.72002681274373,0.227360380883723,
12.5434568539655));
#447158=CARTESIAN_POINT('Ctrl Pts',(2.73455903183065,0.239926196923173,
12.5049357605811));
#447159=CARTESIAN_POINT('Ctrl Pts',(2.73275136312396,0.223524498266137,
12.5081700652078));
#447160=CARTESIAN_POINT('Ctrl Pts',(2.74370607772735,0.220222141949245,
12.5204921097672));
#447161=CARTESIAN_POINT('Ctrl Pts',(2.73300445492295,0.240391536141379,
12.5064436508395));
#447162=CARTESIAN_POINT('Ctrl Pts',(2.73331649481491,0.239211926504078,
12.5062361689309));
#447163=CARTESIAN_POINT('Ctrl Pts',(2.73359068959241,0.237971922937781,
12.5061871075061));
#447164=CARTESIAN_POINT('Ctrl Pts',(2.73378821456767,0.236758662650264,
12.5063648335164));
#447165=CARTESIAN_POINT('Ctrl Pts',(2.73387794259528,0.236207524990675,
12.5064455676329));
#447166=CARTESIAN_POINT('Ctrl Pts',(2.73395288359528,0.235654183278717,
12.506574497099));
#447167=CARTESIAN_POINT('Ctrl Pts',(2.73400878288092,0.235122222101259,
12.5067492519495));
#447168=CARTESIAN_POINT('Ctrl Pts',(2.73412111466528,0.234053225465864,
12.5071004286051));
#447169=CARTESIAN_POINT('Ctrl Pts',(2.73415987759819,0.233031181040618,
12.5076537929613));
#447170=CARTESIAN_POINT('Ctrl Pts',(2.7341316139703,0.232133157091211,12.5083435010505));
#447171=CARTESIAN_POINT('Ctrl Pts',(2.73412983460602,0.23207662111698,12.5083869222964));
#447172=CARTESIAN_POINT('Ctrl Pts',(2.73412777746198,0.232020570902364,
12.5084308732337));
#447173=CARTESIAN_POINT('Ctrl Pts',(2.7341254394046,0.231965022963218,12.5084753333615));
#447174=CARTESIAN_POINT('Ctrl Pts',(2.73410668509844,0.231519455174593,
12.5088319622689));
#447175=CARTESIAN_POINT('Ctrl Pts',(2.73407076458494,0.231097104567115,
12.509227847131));
#447176=CARTESIAN_POINT('Ctrl Pts',(2.73402153594906,0.230710292540567,
12.5096423454524));
#447177=CARTESIAN_POINT('Ctrl Pts',(2.73386727519189,0.229498194845199,
12.5109411997424));
#447178=CARTESIAN_POINT('Ctrl Pts',(2.73358244278894,0.22855928452366,12.5124831113042));
#447179=CARTESIAN_POINT('Ctrl Pts',(2.73323892911399,0.227832017839011,
12.5140723025008));
#447180=CARTESIAN_POINT('Ctrl Pts',(2.73320674150641,0.227763872154106,
12.5142212114565));
#447181=CARTESIAN_POINT('Ctrl Pts',(2.73317405297027,0.227697558745421,
12.5143705582413));
#447182=CARTESIAN_POINT('Ctrl Pts',(2.73314093216374,0.227633012915218,
12.5145201959299));
#447183=CARTESIAN_POINT('Ctrl Pts',(2.73271544609219,0.226803825627575,
12.5164425148273));
#447184=CARTESIAN_POINT('Ctrl Pts',(2.73221359660187,0.226233032435239,
12.518463520594));
#447185=CARTESIAN_POINT('Ctrl Pts',(2.73166340605281,0.225834885300983,
12.5205025929157));
#447186=CARTESIAN_POINT('Ctrl Pts',(2.73134427372684,0.225603944182036,
12.5216853356836));
#447187=CARTESIAN_POINT('Ctrl Pts',(2.73100973721378,0.225431114566588,
12.5228750347131));
#447188=CARTESIAN_POINT('Ctrl Pts',(2.73067077961574,0.225301825760895,
12.5240609649613));
#447189=CARTESIAN_POINT('Ctrl Pts',(2.72983882637577,0.224984493323426,
12.5269717671327));
#447190=CARTESIAN_POINT('Ctrl Pts',(2.72895311974325,0.224930246210316,
12.5299036066169));
#447191=CARTESIAN_POINT('Ctrl Pts',(2.72803279551388,0.225054566116146,
12.532813300402));
#447192=CARTESIAN_POINT('Ctrl Pts',(2.72759098629491,0.225114246909874,
12.5342101228452));
#447193=CARTESIAN_POINT('Ctrl Pts',(2.72714182065526,0.225215524423788,
12.5356023438238));
#447194=CARTESIAN_POINT('Ctrl Pts',(2.72668989544585,0.225351759568795,
12.5369868989719));
#447195=CARTESIAN_POINT('Origin',(14.9277716845705,-3.45826025389702,-1.23970570397459));
#447196=CARTESIAN_POINT('Ctrl Pts',(2.71576638210363,0.331694585626358,
12.5369868989719));
#447197=CARTESIAN_POINT('Ctrl Pts',(2.72926496886933,0.3389796016877,12.5369868989719));
#447198=CARTESIAN_POINT('Ctrl Pts',(2.72709693147968,0.354164558637326,
12.5369868989719));
#447199=CARTESIAN_POINT('Ctrl Pts',(2.72032940091062,0.334157264238229,
12.5218025310016));
#447200=CARTESIAN_POINT('Ctrl Pts',(2.72873602820049,0.342462953933468,
12.5216901060417));
#447201=CARTESIAN_POINT('Ctrl Pts',(2.72710355670233,0.354118272187117,
12.5161920673678));
#447202=CARTESIAN_POINT('Ctrl Pts',(2.72574913874772,0.331518606819774,
12.5042015548895));
#447203=CARTESIAN_POINT('Ctrl Pts',(2.72940529979091,0.336811038344444,
12.4980677368514));
#447204=CARTESIAN_POINT('Ctrl Pts',(2.7285668796838,0.343555505072639,12.4907278922777));
#447205=CARTESIAN_POINT('Ctrl Pts',(2.72501376996001,0.318263486773113,
12.506463626192));
#447206=CARTESIAN_POINT('Ctrl Pts',(2.73151233698725,0.319022476185907,
12.4999376786891));
#447207=CARTESIAN_POINT('Ctrl Pts',(2.73143296643992,0.319013206233799,
12.4906970594712));
#447208=CARTESIAN_POINT('Origin',(2.70531779326537,0.351055034776334,12.5369868989719));
#447209=CARTESIAN_POINT('Origin',(2.70531779326537,0.351055034776334,14.));
#447210=CARTESIAN_POINT('Origin',(2.70531779326537,0.351055034776334,13.7435492065112));
#447211=CARTESIAN_POINT('Ctrl Pts',(2.69403611232523,0.319913659896689,
13.793642941384));
#447212=CARTESIAN_POINT('Ctrl Pts',(2.70355434423058,0.325042936687985,
13.8071662555867));
#447213=CARTESIAN_POINT('Ctrl Pts',(2.69776742416513,0.341059519962545,
13.8103758687955));
#447214=CARTESIAN_POINT('Ctrl Pts',(2.70864801779921,0.327835397309829,
13.7804579775006));
#447215=CARTESIAN_POINT('Ctrl Pts',(2.72038784494332,0.334173388344512,
13.7901904343351));
#447216=CARTESIAN_POINT('Ctrl Pts',(2.71750187878964,0.349662969472621,
13.7927914348262));
#447217=CARTESIAN_POINT('Ctrl Pts',(2.71725059644146,0.332499222286879,
13.7597120340895));
#447218=CARTESIAN_POINT('Ctrl Pts',(2.73083416031405,0.339839105289468,
13.7635825532445));
#447219=CARTESIAN_POINT('Ctrl Pts',(2.72912904849147,0.354759846216685,
13.7651073818884));
#447220=CARTESIAN_POINT('Ctrl Pts',(2.71556601456628,0.331585938567642,
13.7381884353898));
#447221=CARTESIAN_POINT('Ctrl Pts',(2.72883205711228,0.338753227161935,
13.7368803041982));
#447222=CARTESIAN_POINT('Ctrl Pts',(2.72685190474066,0.353762178947586,
13.7363986145813));
#447223=CARTESIAN_POINT('Origin',(2.68709632791919,0.341176396727035,13.7902182540695));
#447224=CARTESIAN_POINT('Ctrl Pts',(2.66613492315446,0.304787198288574,
13.8235227101244));
#447225=CARTESIAN_POINT('Ctrl Pts',(2.67624430285751,0.310262883664768,
13.8358800583119));
#447226=CARTESIAN_POINT('Ctrl Pts',(2.67109479161606,0.326014346550185,
13.8390832900376));
#447227=CARTESIAN_POINT('Ctrl Pts',(2.67662065585239,0.310471963814255,
13.8124254819053));
#447228=CARTESIAN_POINT('Ctrl Pts',(2.68674966769504,0.315958283138429,
13.8247886449157));
#447229=CARTESIAN_POINT('Ctrl Pts',(2.68157744931315,0.331724352341378,
13.8279860620657));
#447230=CARTESIAN_POINT('Ctrl Pts',(2.68710168918608,0.316154181612971,
13.8013225099955));
#447231=CARTESIAN_POINT('Ctrl Pts',(2.69724555485603,0.321648544460721,
13.8136962257787));
#447232=CARTESIAN_POINT('Ctrl Pts',(2.69205538371444,0.337431476647197,
13.8168830918626));
#447233=CARTESIAN_POINT('Ctrl Pts',(2.69757820600054,0.321833950812844,
13.7902140179785));
#447234=CARTESIAN_POINT('Ctrl Pts',(2.70773245948189,0.327333936065635,
13.802602731458));
#447235=CARTESIAN_POINT('Ctrl Pts',(2.70252878128997,0.343135831072125,
13.8057746032558));
#447236=CARTESIAN_POINT('Origin',(2.6556530341162,0.324129638266262,13.8235269408515));
#447237=CARTESIAN_POINT('Ctrl Pts',(2.67260022728041,0.241657374439811,
13.8235269408515));
#447238=CARTESIAN_POINT('Ctrl Pts',(2.68390520534861,0.238249429359771,
13.8362179249168));
#447239=CARTESIAN_POINT('Ctrl Pts',(2.68168562294632,0.221316134995806,
13.8391868794938));
#447240=CARTESIAN_POINT('Ctrl Pts',(2.66225666442441,0.244775495849028,
13.8400110824519));
#447241=CARTESIAN_POINT('Ctrl Pts',(2.67033310242142,0.238767749837299,
13.8494522556836));
#447242=CARTESIAN_POINT('Ctrl Pts',(2.66469546768055,0.226555257791658,
13.85569149686));
#447243=CARTESIAN_POINT('Ctrl Pts',(2.6499505979317,0.255450628331682,13.8586819406588));
#447244=CARTESIAN_POINT('Ctrl Pts',(2.65040775394981,0.251120841730696,
13.868010383617));
#447245=CARTESIAN_POINT('Ctrl Pts',(2.64436282297905,0.244386476404156,
13.8744918421245));
#447246=CARTESIAN_POINT('Ctrl Pts',(2.64671210510577,0.286572705096629,
13.8587686893867));
#447247=CARTESIAN_POINT('Ctrl Pts',(2.64625896177486,0.290863950724822,
13.8680909899357));
#447248=CARTESIAN_POINT('Ctrl Pts',(2.63897424257269,0.296195861043949,
13.8745789365163));
#447249=CARTESIAN_POINT('Ctrl Pts',(2.65662554151646,0.29963175370253,13.8400379222776));
#447250=CARTESIAN_POINT('Ctrl Pts',(2.66331035922829,0.307153950593571,
13.8494748685453));
#447251=CARTESIAN_POINT('Ctrl Pts',(2.65532011815827,0.317966774133587,
13.8557104837033));
#447252=CARTESIAN_POINT('Ctrl Pts',(2.66613838389016,0.304789073646093,
13.8235269408542));
#447253=CARTESIAN_POINT('Ctrl Pts',(2.67651853655118,0.310416599703283,
13.8362179249195));
#447254=CARTESIAN_POINT('Ctrl Pts',(2.67091450477463,0.326549108246711,
13.8391868794965));
#447255=CARTESIAN_POINT('Origin',(2.66625045727084,0.220593651577375,13.8235269408515));
#447256=CARTESIAN_POINT('Ctrl Pts',(2.70684120332097,0.231335251380178,
13.7902140241682));
#447257=CARTESIAN_POINT('Ctrl Pts',(2.71789912196361,0.228006433168682,
13.8026027327198));
#447258=CARTESIAN_POINT('Ctrl Pts',(2.71600461405142,0.211478010012068,
13.8057746032556));
#447259=CARTESIAN_POINT('Ctrl Pts',(2.6954312754781,0.234774834122735,13.8013225161808));
#447260=CARTESIAN_POINT('Ctrl Pts',(2.7064778826876,0.231449417300115,13.8136962270464));
#447261=CARTESIAN_POINT('Ctrl Pts',(2.70459276011078,0.214942300102255,
13.8168830918628));
#447262=CARTESIAN_POINT('Ctrl Pts',(2.6840164287127,0.238215899700367,13.8124254880875));
#447263=CARTESIAN_POINT('Ctrl Pts',(2.69504686059561,0.234895350420997,
13.8247886461868));
#447264=CARTESIAN_POINT('Ctrl Pts',(2.69317590227677,0.218408383532957,
13.8279860620656));
#447265=CARTESIAN_POINT('Ctrl Pts',(2.67259646388749,0.241658508144051,
13.8235227163065));
#447266=CARTESIAN_POINT('Ctrl Pts',(2.6836055164308,0.238344395089921,13.8358800595847));
#447267=CARTESIAN_POINT('Ctrl Pts',(2.68175383533497,0.22187633181832,13.8390832900376));
#447268=CARTESIAN_POINT('Origin',(2.70049520861906,0.210270391225142,13.7902182540695));
#447269=CARTESIAN_POINT('Ctrl Pts',(2.72643151229394,0.225429621717924,
13.7382347919292));
#447270=CARTESIAN_POINT('Ctrl Pts',(2.74088653003935,0.221097147746479,
13.7369371795943));
#447271=CARTESIAN_POINT('Ctrl Pts',(2.74198064990422,0.205986003556125,
13.7364597369711));
#447272=CARTESIAN_POINT('Ctrl Pts',(2.7282425699732,0.224883669278053,13.7595490285574));
#447273=CARTESIAN_POINT('Ctrl Pts',(2.74304218339098,0.220446863095312,
13.7633824266926));
#447274=CARTESIAN_POINT('Ctrl Pts',(2.74438297365277,0.205477028701391,
13.7648920890506));
#447275=CARTESIAN_POINT('Ctrl Pts',(2.71900627502906,0.227667996819329,
13.7803806590111));
#447276=CARTESIAN_POINT('Ctrl Pts',(2.73180896117424,0.223835489354001,
13.7901039518744));
#447277=CARTESIAN_POINT('Ctrl Pts',(2.73213643437849,0.208075470231991,
13.7926933640892));
#447278=CARTESIAN_POINT('Ctrl Pts',(2.70295153259354,0.232507779552342,
13.7936647693663));
#447279=CARTESIAN_POINT('Ctrl Pts',(2.71331528178779,0.229414878877652,
13.8072068914933));
#447280=CARTESIAN_POINT('Ctrl Pts',(2.71088006236672,0.212541409281315,
13.8104111085397));
#447281=CARTESIAN_POINT('Origin',(2.72034012543628,0.204288036706358,13.7435492065112));
#447282=CARTESIAN_POINT('Origin',(2.72034012543628,0.204288036706358,14.));
#447283=CARTESIAN_POINT('Origin',(2.72034012543628,0.204288036706358,12.5369868989719));
#447284=CARTESIAN_POINT('Ctrl Pts',(2.73298614238843,0.240389925404879,
12.506462012331));
#447285=CARTESIAN_POINT('Ctrl Pts',(2.73949961721437,0.24096284222405,12.4999388158272));
#447286=CARTESIAN_POINT('Ctrl Pts',(2.73942255426528,0.240956063866745,
12.4907030323752));
#447287=CARTESIAN_POINT('Ctrl Pts',(2.73638954182112,0.227558500875394,
12.5042014951932));
#447288=CARTESIAN_POINT('Ctrl Pts',(2.74104069118792,0.223119142060907,
12.4980716682127));
#447289=CARTESIAN_POINT('Ctrl Pts',(2.7415871803248,0.216349584110118,12.4907355092743));
#447290=CARTESIAN_POINT('Ctrl Pts',(2.73161886183057,0.223875253168118,
12.5218047446509));
#447291=CARTESIAN_POINT('Ctrl Pts',(2.74152832372308,0.217447078004261,
12.5216906929434));
#447292=CARTESIAN_POINT('Ctrl Pts',(2.74229425718691,0.205708930779974,
12.5161988840776));
#447293=CARTESIAN_POINT('Ctrl Pts',(2.72665310456753,0.225362815340743,
12.5369868989719));
#447294=CARTESIAN_POINT('Ctrl Pts',(2.74133828825224,0.22096384822709,12.5369868989719));
#447295=CARTESIAN_POINT('Ctrl Pts',(2.74229705622194,0.20566396928963,12.5369868989719));
#447296=CARTESIAN_POINT('Origin',(5.1250859646407E-31,-4.62728456409018E-31,
12.5));
#447297=CARTESIAN_POINT('Origin',(2.64401005104368,0.45869500919504,12.5));
#447298=CARTESIAN_POINT('',(2.64401005104368,0.45869500919504,12.5893111709658));
#447299=CARTESIAN_POINT('',(2.64401005104368,0.45869500919504,13.8235269408515));
#447300=CARTESIAN_POINT('',(2.64401005104368,0.45869500919504,12.5));
#447301=CARTESIAN_POINT('',(2.67898229736196,0.45119736378766,13.7902182540695));
#447302=CARTESIAN_POINT('',(2.64401005104368,0.45869500919504,13.8235269408515));
#447303=CARTESIAN_POINT('',(2.69924879928632,0.446852460011852,13.7435492065112));
#447304=CARTESIAN_POINT('Origin',(2.63257234412928,0.461147454519627,13.7445212918716));
#447305=CARTESIAN_POINT('',(2.69924879928632,0.446852460011852,12.5369868989719));
#447306=CARTESIAN_POINT('',(2.69924879928632,0.446852460011852,12.5));
#447307=CARTESIAN_POINT('Ctrl Pts',(2.69924879928632,0.446852460011852,
12.5369868989719));
#447308=CARTESIAN_POINT('Ctrl Pts',(2.68084931246653,0.450797097327883,
12.5544431401645));
#447309=CARTESIAN_POINT('Ctrl Pts',(2.66243666584474,0.454744555953365,
12.5718848856037));
#447310=CARTESIAN_POINT('Ctrl Pts',(2.64401005104368,0.45869500919504,12.5893111709658));
#447311=CARTESIAN_POINT('Origin',(2.86269335364304,0.671426145235719,12.5));
#447312=CARTESIAN_POINT('',(2.67972872331796,0.551973886059784,13.7435492065112));
#447313=CARTESIAN_POINT('',(2.66237308910438,0.540642899778119,13.7902182540695));
#447314=CARTESIAN_POINT('Origin',(2.61676548204774,0.510867026218055,13.7418732680447));
#447315=CARTESIAN_POINT('',(2.63242388933657,0.521089942649624,13.8235269408515));
#447316=CARTESIAN_POINT('',(2.66237308910438,0.540642899778119,13.7902182540695));
#447317=CARTESIAN_POINT('',(2.63242388933657,0.521089942649624,12.5893111709658));
#447318=CARTESIAN_POINT('',(2.63242388933657,0.521089942649624,12.5));
#447319=CARTESIAN_POINT('',(2.67972872331796,0.551973886059784,12.5369868989719));
#447320=CARTESIAN_POINT('Ctrl Pts',(2.63242388933657,0.521089942649624,
12.5893111709658));
#447321=CARTESIAN_POINT('Ctrl Pts',(2.6482038985101,0.531392249397362,12.5718848856037));
#447322=CARTESIAN_POINT('Ctrl Pts',(2.66397194574709,0.541686746546371,
12.5544431401645));
#447323=CARTESIAN_POINT('Ctrl Pts',(2.67972872331796,0.551973886059784,
12.5369868989719));
#447324=CARTESIAN_POINT('',(2.67972872331796,0.551973886059784,12.5));
#447325=CARTESIAN_POINT('Origin',(2.65121591465983,0.492306259611314,12.5));
#447326=CARTESIAN_POINT('',(2.61764170561193,0.484933155856055,13.8587068136939));
#447327=CARTESIAN_POINT('Ctrl Pts',(2.63242388933283,0.521089942655079,
13.8235269408542));
#447328=CARTESIAN_POINT('Ctrl Pts',(2.63095661370707,0.520132001286734,
13.8262006681044));
#447329=CARTESIAN_POINT('Ctrl Pts',(2.62955005079904,0.519006208757991,
13.8288634856214));
#447330=CARTESIAN_POINT('Ctrl Pts',(2.62820106581135,0.51772552574374,13.8314912288862));
#447331=CARTESIAN_POINT('Ctrl Pts',(2.62681040143038,0.516405273652374,
13.8342001611531));
#447332=CARTESIAN_POINT('Ctrl Pts',(2.62547904109438,0.514919305836688,
13.8368750301949));
#447333=CARTESIAN_POINT('Ctrl Pts',(2.62421729621779,0.51323876158432,13.8394886372969));
#447334=CARTESIAN_POINT('Ctrl Pts',(2.62411984860041,0.513108969075282,
13.8396904925131));
#447335=CARTESIAN_POINT('Ctrl Pts',(2.62402283138454,0.512977999796652,
13.8398919674349));
#447336=CARTESIAN_POINT('Ctrl Pts',(2.62392625785407,0.512845832827748,
13.8400930404591));
#447337=CARTESIAN_POINT('Ctrl Pts',(2.62242157727778,0.510786582534607,
13.8432258934518));
#447338=CARTESIAN_POINT('Ctrl Pts',(2.62103137367685,0.508447755728073,
13.8462331177034));
#447339=CARTESIAN_POINT('Ctrl Pts',(2.61988391126663,0.505856342596067,
13.8489036603661));
#447340=CARTESIAN_POINT('Ctrl Pts',(2.61950844821232,0.505008402061483,
13.8497774930041));
#447341=CARTESIAN_POINT('Ctrl Pts',(2.61915918468767,0.504133553522089,
13.85061494757));
#447342=CARTESIAN_POINT('Ctrl Pts',(2.61884120705065,0.503233140312533,
13.8514076489583));
#447343=CARTESIAN_POINT('Ctrl Pts',(2.61816863848912,0.501328636515285,
13.8530843267192));
#447344=CARTESIAN_POINT('Ctrl Pts',(2.61757276302572,0.499121703226922,
13.8546805203176));
#447345=CARTESIAN_POINT('Ctrl Pts',(2.61721989365905,0.496704863131317,
13.8559412814274));
#447346=CARTESIAN_POINT('Ctrl Pts',(2.61717266829397,0.496381411546564,
13.8561100121513));
#447347=CARTESIAN_POINT('Ctrl Pts',(2.61712974473018,0.496054258003594,
13.8562727473908));
#447348=CARTESIAN_POINT('Ctrl Pts',(2.61709146483165,0.495723674551077,
13.8564289040185));
#447349=CARTESIAN_POINT('Ctrl Pts',(2.61691786592856,0.494224482365258,
13.8571370725437));
#447350=CARTESIAN_POINT('Ctrl Pts',(2.61683897914486,0.492628136783919,
13.8577210840553));
#447351=CARTESIAN_POINT('Ctrl Pts',(2.61688718309717,0.490995239516125,
13.8581177131616));
#447352=CARTESIAN_POINT('Ctrl Pts',(2.61690075898927,0.490535359442897,
13.8582294175695));
#447353=CARTESIAN_POINT('Ctrl Pts',(2.6169242403368,0.490072609808437,13.8583265086086));
#447354=CARTESIAN_POINT('Ctrl Pts',(2.61695791341011,0.489608391741768,
13.8584082369006));
#447355=CARTESIAN_POINT('Ctrl Pts',(2.61700629258668,0.48894143486496,13.8585256585398));
#447356=CARTESIAN_POINT('Ctrl Pts',(2.61707663347169,0.488263178401156,
13.8586122832068));
#447357=CARTESIAN_POINT('Ctrl Pts',(2.61716789428703,0.487591322947798,
13.8586682984299));
#447358=CARTESIAN_POINT('Ctrl Pts',(2.61724089389291,0.487053905184001,
13.8587131050557));
#447359=CARTESIAN_POINT('Ctrl Pts',(2.61732785286909,0.486514615707723,
13.8587357943552));
#447360=CARTESIAN_POINT('Ctrl Pts',(2.61742928153635,0.485973471058265,
13.8587355499465));
#447361=CARTESIAN_POINT('Ctrl Pts',(2.61749483730215,0.485623716369912,
13.8587353919793));
#447362=CARTESIAN_POINT('Ctrl Pts',(2.61756569063552,0.485276961787545,
13.8587257282814));
#447363=CARTESIAN_POINT('Ctrl Pts',(2.61764170561193,0.484933155856055,
13.8587068136939));
#447364=CARTESIAN_POINT('Ctrl Pts',(2.61764170561193,0.484933155856055,
13.8587068136939));
#447365=CARTESIAN_POINT('Ctrl Pts',(2.6178917147254,0.483802396889853,13.8586446046466));
#447366=CARTESIAN_POINT('Ctrl Pts',(2.61819748949905,0.482703493884876,
13.858482427929));
#447367=CARTESIAN_POINT('Ctrl Pts',(2.61855481519474,0.481634956223954,
13.8582284286032));
#447368=CARTESIAN_POINT('Ctrl Pts',(2.61892138979266,0.480538760881331,
13.8579678548414));
#447369=CARTESIAN_POINT('Ctrl Pts',(2.6193445665292,0.479472331205392,13.857615680862));
#447370=CARTESIAN_POINT('Ctrl Pts',(2.61979865549006,0.47847413647332,13.8571944833187));
#447371=CARTESIAN_POINT('Ctrl Pts',(2.62093188093231,0.475983039432451,
13.8561433417727));
#447372=CARTESIAN_POINT('Ctrl Pts',(2.6223062724137,0.473798400317295,13.8546163505474));
#447373=CARTESIAN_POINT('Ctrl Pts',(2.62371754355696,0.471952233854166,
13.8528973491086));
#447374=CARTESIAN_POINT('Ctrl Pts',(2.62397536197347,0.471614966478998,
13.8525833129072));
#447375=CARTESIAN_POINT('Ctrl Pts',(2.62423435127468,0.471288867267204,
13.8522628768812));
#447376=CARTESIAN_POINT('Ctrl Pts',(2.62449321634177,0.470973959613751,
13.851937733538));
#447377=CARTESIAN_POINT('Ctrl Pts',(2.62607406939059,0.469050862265577,
13.8499521282529));
#447378=CARTESIAN_POINT('Ctrl Pts',(2.62781054677247,0.467356610214955,
13.847639871647));
#447379=CARTESIAN_POINT('Ctrl Pts',(2.62955527966329,0.465922742781579,
13.8452109780794));
#447380=CARTESIAN_POINT('Ctrl Pts',(2.63034027110504,0.465277616143722,
13.8441181685877));
#447381=CARTESIAN_POINT('Ctrl Pts',(2.63112669787049,0.464684520885177,
13.8430021611332));
#447382=CARTESIAN_POINT('Ctrl Pts',(2.63190107147962,0.464143021432023,
13.8418824960098));
#447383=CARTESIAN_POINT('Ctrl Pts',(2.63372590266388,0.462866964142988,
13.8392439765549));
#447384=CARTESIAN_POINT('Ctrl Pts',(2.63556886729635,0.46181332875756,13.8364981347964));
#447385=CARTESIAN_POINT('Ctrl Pts',(2.63741785494251,0.46094962063717,13.8336931113419));
#447386=CARTESIAN_POINT('Ctrl Pts',(2.6392186514883,0.460108423778447,13.8309611966328));
#447387=CARTESIAN_POINT('Ctrl Pts',(2.64102720460484,0.459447051295175,
13.8281701127186));
#447388=CARTESIAN_POINT('Ctrl Pts',(2.64283486522965,0.458974701588688,
13.8253580685121));
#447389=CARTESIAN_POINT('Ctrl Pts',(2.643226768004,0.458872295662546,13.8247484142933));
#447390=CARTESIAN_POINT('Ctrl Pts',(2.64361857176526,0.458778937827683,
13.8241378483365));
#447391=CARTESIAN_POINT('Ctrl Pts',(2.64401005104368,0.45869500919504,13.8235269408515));
#447392=CARTESIAN_POINT('',(2.61739720455155,0.48615093912443,12.5969504640361));
#447393=CARTESIAN_POINT('Origin',(2.65124847974971,0.492312107493906,12.584524458991));
#447394=CARTESIAN_POINT('Origin',(2.65124847974971,0.492312107493906,12.584524458991));
#447395=CARTESIAN_POINT('Ctrl Pts',(2.63242388933657,0.521089942649624,
12.5893111709658));
#447396=CARTESIAN_POINT('Ctrl Pts',(2.62293347207067,0.514893926616804,
12.5770542771492));
#447397=CARTESIAN_POINT('Ctrl Pts',(2.62916808382621,0.499763384950601,
12.5737548217797));
#447398=CARTESIAN_POINT('Ctrl Pts',(2.65317624681838,0.53463855026862,12.5663937883685));
#447399=CARTESIAN_POINT('Ctrl Pts',(2.64367372320726,0.528434630356866,
12.5540940315304));
#447400=CARTESIAN_POINT('Ctrl Pts',(2.64993062377102,0.513258425605721,
12.5508374392248));
#447401=CARTESIAN_POINT('Ctrl Pts',(2.67390766542586,0.548173487508601,
12.5434499600944));
#447402=CARTESIAN_POINT('Ctrl Pts',(2.66437424572655,0.541949396444004,
12.5311293540533));
#447403=CARTESIAN_POINT('Ctrl Pts',(2.67067223527891,0.526741270584369,
12.5278936106989));
#447404=CARTESIAN_POINT('Ctrl Pts',(2.69461978532979,0.561695825189121,
12.5204817579905));
#447405=CARTESIAN_POINT('Ctrl Pts',(2.68503918171815,0.555440929127259,
12.5081597038247));
#447406=CARTESIAN_POINT('Ctrl Pts',(2.69139453743966,0.540212879398297,
12.5049254088044));
#447407=CARTESIAN_POINT('Ctrl Pts',(2.67972872331796,0.551973886059784,
12.5369868989719));
#447408=CARTESIAN_POINT('Ctrl Pts',(2.68050871289234,0.552483118260842,
12.5342545179733));
#447409=CARTESIAN_POINT('Ctrl Pts',(2.68132129516182,0.552864650918281,
12.5314872231885));
#447410=CARTESIAN_POINT('Ctrl Pts',(2.68214445473304,0.553046390926102,
12.5287124745063));
#447411=CARTESIAN_POINT('Ctrl Pts',(2.68288682089236,0.553210293085923,
12.5262100684184));
#447412=CARTESIAN_POINT('Ctrl Pts',(2.6836372529414,0.553210571459382,12.5237004536639));
#447413=CARTESIAN_POINT('Ctrl Pts',(2.68440866078858,0.552980940222957,
12.5212220730815));
#447414=CARTESIAN_POINT('Ctrl Pts',(2.68499924022769,0.552805137646787,
12.5193246583486));
#447415=CARTESIAN_POINT('Ctrl Pts',(2.68560899127225,0.552491870529511,
12.517417831369));
#447416=CARTESIAN_POINT('Ctrl Pts',(2.68621141930172,0.551947586437506,
12.5155812248347));
#447417=CARTESIAN_POINT('Ctrl Pts',(2.68646805688034,0.551715718488774,
12.5147988205793));
#447418=CARTESIAN_POINT('Ctrl Pts',(2.68672381171149,0.551441895620714,
12.5140295443047));
#447419=CARTESIAN_POINT('Ctrl Pts',(2.68697870315914,0.551119384996479,
12.5132817086137));
#447420=CARTESIAN_POINT('Ctrl Pts',(2.68736444688424,0.550631308794947,
12.5121499604604));
#447421=CARTESIAN_POINT('Ctrl Pts',(2.68775093218258,0.550016750228963,
12.5110494206568));
#447422=CARTESIAN_POINT('Ctrl Pts',(2.68811468977899,0.549246794045306,
12.5100666561695));
#447423=CARTESIAN_POINT('Ctrl Pts',(2.6883235585532,0.548804686977702,12.509502355064));
#447424=CARTESIAN_POINT('Ctrl Pts',(2.68852675702788,0.548305957877592,
12.5089719619137));
#447425=CARTESIAN_POINT('Ctrl Pts',(2.68871456159219,0.547757544955994,
12.5085043804652));
#447426=CARTESIAN_POINT('Ctrl Pts',(2.68898938910879,0.546955014081043,
12.5078201359221));
#447427=CARTESIAN_POINT('Ctrl Pts',(2.68923807958395,0.546022420353721,
12.5072563000949));
#447428=CARTESIAN_POINT('Ctrl Pts',(2.68943559532489,0.545020798509679,
12.5068768744332));
#447429=CARTESIAN_POINT('Ctrl Pts',(2.68957801777114,0.544298560208242,
12.5066032824114));
#447430=CARTESIAN_POINT('Ctrl Pts',(2.68969639348246,0.543527754388567,
12.5064197834844));
#447431=CARTESIAN_POINT('Ctrl Pts',(2.68978666695644,0.542751817215093,
12.5063282718343));
#447432=CARTESIAN_POINT('Ctrl Pts',(2.68991843828047,0.541619189165899,
12.5061946931565));
#447433=CARTESIAN_POINT('Ctrl Pts',(2.68999420380854,0.540451541931188,
12.5062515701262));
#447434=CARTESIAN_POINT('Ctrl Pts',(2.6900246934761,0.53932234310065,12.5064436508398));
#447435=CARTESIAN_POINT('',(2.62916808382621,0.499763384950601,12.5737548217797));
#447436=CARTESIAN_POINT('Origin',(2.64445078554345,0.502668385505106,12.5893111709658));
#447437=CARTESIAN_POINT('Ctrl Pts',(2.6900246934761,0.539322343100649,12.5064436508398));
#447438=CARTESIAN_POINT('Ctrl Pts',(2.68101659600168,0.533466186712491,
12.5164271754438));
#447439=CARTESIAN_POINT('Ctrl Pts',(2.67200481383978,0.527607884118116,
12.5264061185523));
#447440=CARTESIAN_POINT('Ctrl Pts',(2.66298921773467,0.521747358936393,
12.536380305637));
#447441=CARTESIAN_POINT('Ctrl Pts',(2.65172155116319,0.514422891101821,
12.5488460165097));
#447442=CARTESIAN_POINT('Ctrl Pts',(2.64044792389739,0.507094949458075,
12.5613043021964));
#447443=CARTESIAN_POINT('Ctrl Pts',(2.62916808382621,0.499763384950601,
12.5737548217797));
#447444=CARTESIAN_POINT('Ctrl Pts',(2.64401005104368,0.45869500919504,12.5893111709658));
#447445=CARTESIAN_POINT('Ctrl Pts',(2.63292791152546,0.461070891822268,
12.5770542771492));
#447446=CARTESIAN_POINT('Ctrl Pts',(2.63331499706306,0.477431021395151,
12.5737548217797));
#447447=CARTESIAN_POINT('Ctrl Pts',(2.63367051126054,0.460911687021908,
12.5928319619712));
#447448=CARTESIAN_POINT('Ctrl Pts',(2.62690553363688,0.465693788455673,
12.5821634970843));
#447449=CARTESIAN_POINT('Ctrl Pts',(2.62954657436679,0.478229274332287,
12.5773203894503));
#447450=CARTESIAN_POINT('Ctrl Pts',(2.620249319228,0.470934446310918,12.5969440695591));
#447451=CARTESIAN_POINT('Ctrl Pts',(2.61949747127797,0.474883277430624,
12.5878292599214));
#447452=CARTESIAN_POINT('Ctrl Pts',(2.62476421187078,0.481803229571837,
12.5813877129824));
#447453=CARTESIAN_POINT('Ctrl Pts',(2.61461022485556,0.501007288880253,
12.596957478804));
#447454=CARTESIAN_POINT('Ctrl Pts',(2.61535659519149,0.497087655674131,
12.5878468778671));
#447455=CARTESIAN_POINT('Ctrl Pts',(2.62275176475801,0.492567816183614,
12.5814011370086));
#447456=CARTESIAN_POINT('Ctrl Pts',(2.62355655588574,0.515300719827306,
12.5928371701607));
#447457=CARTESIAN_POINT('Ctrl Pts',(2.61896767895793,0.508410344348033,
12.5821692192951));
#447458=CARTESIAN_POINT('Ctrl Pts',(2.62592698210361,0.497658975984226,
12.5773318885715));
#447459=CARTESIAN_POINT('Ctrl Pts',(2.63242388933653,0.521089942649668,
12.5893111709658));
#447460=CARTESIAN_POINT('Ctrl Pts',(2.62293347207064,0.514893926616848,
12.5770542771492));
#447461=CARTESIAN_POINT('Ctrl Pts',(2.62916808382617,0.499763384950647,
12.5737548217797));
#447462=CARTESIAN_POINT('',(2.63331499706306,0.477431021395151,12.5737548217797));
#447463=CARTESIAN_POINT('Origin',(2.64862180375801,0.480206209461455,12.5893111709658));
#447464=CARTESIAN_POINT('Ctrl Pts',(2.62916808382617,0.499763384950647,
12.5737548217797));
#447465=CARTESIAN_POINT('Ctrl Pts',(2.62831151154022,0.499243189266367,
12.5746934679442));
#447466=CARTESIAN_POINT('Ctrl Pts',(2.6274587437979,0.498510985322169,12.5756680099006));
#447467=CARTESIAN_POINT('Ctrl Pts',(2.62670463205979,0.497652603615456,
12.5765688348656));
#447468=CARTESIAN_POINT('Ctrl Pts',(2.62650498932542,0.497425356561201,
12.5768073183026));
#447469=CARTESIAN_POINT('Ctrl Pts',(2.62631211503452,0.497189477697991,
12.5770407398754));
#447470=CARTESIAN_POINT('Ctrl Pts',(2.62612734303,0.496946927807763,12.5772674179684));
#447471=CARTESIAN_POINT('Ctrl Pts',(2.62536908868791,0.495951568646533,
12.5781976435658));
#447472=CARTESIAN_POINT('Ctrl Pts',(2.62471318760354,0.494780495954386,
12.5790594849312));
#447473=CARTESIAN_POINT('Ctrl Pts',(2.62424605831794,0.493489185397544,
12.5797571720116));
#447474=CARTESIAN_POINT('Ctrl Pts',(2.6239417067919,0.492647850138372,12.580211740231));
#447475=CARTESIAN_POINT('Ctrl Pts',(2.62372131080489,0.491710853559276,
12.5806009430798));
#447476=CARTESIAN_POINT('Ctrl Pts',(2.62361763131471,0.490740099611236,
12.5808812374708));
#447477=CARTESIAN_POINT('Ctrl Pts',(2.62352853623733,0.489905899925599,
12.5811221033394));
#447478=CARTESIAN_POINT('Ctrl Pts',(2.62352392005206,0.489029681663102,
12.581287365893));
#447479=CARTESIAN_POINT('Ctrl Pts',(2.62361238116939,0.488160856068305,
12.581359338449));
#447480=CARTESIAN_POINT('Ctrl Pts',(2.62362467543805,0.488040107251192,
12.5813693411482));
#447481=CARTESIAN_POINT('Ctrl Pts',(2.62363871337667,0.487919475653187,
12.5813775999465));
#447482=CARTESIAN_POINT('Ctrl Pts',(2.62365446307321,0.487799066738467,
12.5813841266931));
#447483=CARTESIAN_POINT('Ctrl Pts',(2.62368118433827,0.487594778451487,
12.5813952001081));
#447484=CARTESIAN_POINT('Ctrl Pts',(2.62371361563218,0.48738984190695,12.5814007534795));
#447485=CARTESIAN_POINT('Ctrl Pts',(2.62375193761589,0.48718437718635,12.5814005856065));
#447486=CARTESIAN_POINT('Ctrl Pts',(2.6239273606744,0.486243840026943,12.5813998171494));
#447487=CARTESIAN_POINT('Ctrl Pts',(2.62421376805465,0.485357157212617,
12.58127954464));
#447488=CARTESIAN_POINT('Ctrl Pts',(2.62458137680877,0.484520267786813,
12.5810700125799));
#447489=CARTESIAN_POINT('Ctrl Pts',(2.62502540632814,0.483509400647933,
12.5808169217085));
#447490=CARTESIAN_POINT('Ctrl Pts',(2.62560327081538,0.482577820810323,
12.5804173076348));
#447491=CARTESIAN_POINT('Ctrl Pts',(2.62624219676262,0.481793442711699,
12.5799304713245));
#447492=CARTESIAN_POINT('Ctrl Pts',(2.62703402729368,0.480821351142921,
12.5793271277669));
#447493=CARTESIAN_POINT('Ctrl Pts',(2.62794379502863,0.479994710061901,
12.5785808224116));
#447494=CARTESIAN_POINT('Ctrl Pts',(2.628911822381,0.479324890005427,12.5777485681082));
#447495=CARTESIAN_POINT('Ctrl Pts',(2.63035428919136,0.478326784737014,
12.576508418016));
#447496=CARTESIAN_POINT('Ctrl Pts',(2.63191006095418,0.477679641991726,
12.5750928681475));
#447497=CARTESIAN_POINT('Ctrl Pts',(2.63331499706306,0.477431021395151,
12.5737548217797));
#447498=CARTESIAN_POINT('Ctrl Pts',(2.63331499706306,0.477431021395151,
12.5737548217797));
#447499=CARTESIAN_POINT('Ctrl Pts',(2.63292791152546,0.461070891822268,
12.5770542771492));
#447500=CARTESIAN_POINT('Ctrl Pts',(2.64401005104368,0.45869500919504,12.5893111709658));
#447501=CARTESIAN_POINT('Ctrl Pts',(2.6575345507421,0.472290187439575,12.5508408821982));
#447502=CARTESIAN_POINT('Ctrl Pts',(2.6571430527915,0.455879445409314,12.55409748406));
#447503=CARTESIAN_POINT('Ctrl Pts',(2.66823933028148,0.453500531764334,
12.5663972313419));
#447504=CARTESIAN_POINT('Ctrl Pts',(2.6817302000617,0.467153221623685,12.52790050457));
#447505=CARTESIAN_POINT('Ctrl Pts',(2.6813118162984,0.450697941851895,12.5311362602938));
#447506=CARTESIAN_POINT('Ctrl Pts',(2.69244416615794,0.448311294707787,
12.5434568539655));
#447507=CARTESIAN_POINT('Ctrl Pts',(2.70590379982209,0.462019809797098,
12.5049357605811));
#447508=CARTESIAN_POINT('Ctrl Pts',(2.70543903669039,0.445525344658126,
12.5081700652078));
#447509=CARTESIAN_POINT('Ctrl Pts',(2.71662647308205,0.443126887598238,
12.5204921097672));
#447510=CARTESIAN_POINT('Ctrl Pts',(2.70431646617453,0.462356888187479,
12.5064436508395));
#447511=CARTESIAN_POINT('Ctrl Pts',(2.70472361691589,0.461206637751966,
12.5062361689309));
#447512=CARTESIAN_POINT('Ctrl Pts',(2.70509797113518,0.45999310961511,12.5061871075061));
#447513=CARTESIAN_POINT('Ctrl Pts',(2.70539373083916,0.458799986470328,
12.5063648335164));
#447514=CARTESIAN_POINT('Ctrl Pts',(2.70552808313993,0.458257996343081,
12.5064455676329));
#447515=CARTESIAN_POINT('Ctrl Pts',(2.70564787726643,0.45771260421724,12.506574497099));
#447516=CARTESIAN_POINT('Ctrl Pts',(2.70574695032627,0.45718696940744,12.5067492519495));
#447517=CARTESIAN_POINT('Ctrl Pts',(2.70594604148572,0.456130685853542,
12.5071004286051));
#447518=CARTESIAN_POINT('Ctrl Pts',(2.70606798154703,0.455115201735787,
12.5076537929612));
#447519=CARTESIAN_POINT('Ctrl Pts',(2.70611300925277,0.454217862139002,
12.5083435010503));
#447520=CARTESIAN_POINT('Ctrl Pts',(2.70611584401593,0.454161369248753,
12.5083869222963));
#447521=CARTESIAN_POINT('Ctrl Pts',(2.70611836232971,0.454105337860168,
12.5084308732336));
#447522=CARTESIAN_POINT('Ctrl Pts',(2.70612055972475,0.454049784178728,
12.5084753333615));
#447523=CARTESIAN_POINT('Ctrl Pts',(2.70613818573322,0.453604170330105,
12.508831962269));
#447524=CARTESIAN_POINT('Ctrl Pts',(2.70613681023768,0.453180297204131,
12.509227847131));
#447525=CARTESIAN_POINT('Ctrl Pts',(2.70611927417718,0.452790759671851,
12.5096423454524));
#447526=CARTESIAN_POINT('Ctrl Pts',(2.70606432392469,0.451570121447775,
12.5109411997424));
#447527=CARTESIAN_POINT('Ctrl Pts',(2.70585696918569,0.450611118787778,
12.5124831113042));
#447528=CARTESIAN_POINT('Ctrl Pts',(2.70557387751056,0.449858272469493,
12.5140723025008));
#447529=CARTESIAN_POINT('Ctrl Pts',(2.70554735151054,0.449787729944901,
12.5142212114565));
#447530=CARTESIAN_POINT('Ctrl Pts',(2.70552017690124,0.449718972769453,
12.5143705582413));
#447531=CARTESIAN_POINT('Ctrl Pts',(2.70549242738584,0.449651942056966,
12.5145201959299));
#447532=CARTESIAN_POINT('Ctrl Pts',(2.70513594354584,0.448790832756771,
12.5164425148273));
#447533=CARTESIAN_POINT('Ctrl Pts',(2.70468228886246,0.448181033439291,
12.518463520594));
#447534=CARTESIAN_POINT('Ctrl Pts',(2.70416638171473,0.447739365469311,
12.5205025929157));
#447535=CARTESIAN_POINT('Ctrl Pts',(2.70386713512039,0.447483180540639,
12.5216853356836));
#447536=CARTESIAN_POINT('Ctrl Pts',(2.70354779896811,0.44728365816998,12.5228750347131));
#447537=CARTESIAN_POINT('Ctrl Pts',(2.70322050746143,0.447127171371152,
12.5240609649613));
#447538=CARTESIAN_POINT('Ctrl Pts',(2.70241718801687,0.446743082918657,
12.5269717671326));
#447539=CARTESIAN_POINT('Ctrl Pts',(2.70153885014343,0.44661682299529,12.5299036066169));
#447540=CARTESIAN_POINT('Ctrl Pts',(2.70061145499055,0.44666571426832,12.5328133004019));
#447541=CARTESIAN_POINT('Ctrl Pts',(2.70016625131657,0.446689184926227,
12.5342101228451));
#447542=CARTESIAN_POINT('Ctrl Pts',(2.69971032518094,0.446753514278087,
12.5356023438238));
#447543=CARTESIAN_POINT('Ctrl Pts',(2.69924879928632,0.446852460011852,
12.5369868989719));
#447544=CARTESIAN_POINT('Origin',(15.1599677223619,-2.22999831842861,-1.23969099894504));
#447545=CARTESIAN_POINT('Ctrl Pts',(2.67969370547127,0.551951071342014,
12.5369868989719));
#447546=CARTESIAN_POINT('Ctrl Pts',(2.6925535803633,0.560312107249547,12.5369868989719));
#447547=CARTESIAN_POINT('Ctrl Pts',(2.68915504197755,0.575269822333287,
12.5369868989719));
#447548=CARTESIAN_POINT('Ctrl Pts',(2.68404081004032,0.554777483987707,
12.5218025310016));
#447549=CARTESIAN_POINT('Ctrl Pts',(2.69174247415498,0.563740755353107,
12.5216901060418));
#447550=CARTESIAN_POINT('Ctrl Pts',(2.68916541793071,0.575224229914571,
12.5161920673678));
#447551=CARTESIAN_POINT('Ctrl Pts',(2.68965758922266,0.552589365432291,
12.5042015548894));
#447552=CARTESIAN_POINT('Ctrl Pts',(2.69287020238977,0.558162197894824,
12.4980677368513));
#447553=CARTESIAN_POINT('Ctrl Pts',(2.69148483540545,0.564815883944122,
12.4907278922777));
#447554=CARTESIAN_POINT('Ctrl Pts',(2.69000508265219,0.539318411321086,
12.506463626192));
#447555=CARTESIAN_POINT('Ctrl Pts',(2.69642016155051,0.540604568801698,
12.4999376786891));
#447556=CARTESIAN_POINT('Ctrl Pts',(2.69634181068928,0.540588860258143,
12.4906970594712));
#447557=CARTESIAN_POINT('Origin',(2.66770182711108,0.570395443204302,12.5369868989719));
#447558=CARTESIAN_POINT('Origin',(2.66770182711108,0.570395443204303,14.));
#447559=CARTESIAN_POINT('Origin',(2.66770182711108,0.570395443204303,13.7435492065112));
#447560=CARTESIAN_POINT('Ctrl Pts',(2.65899599618871,0.538438126949952,
13.793642941384));
#447561=CARTESIAN_POINT('Ctrl Pts',(2.66806447328623,0.544326160759092,
13.8071662555867));
#447562=CARTESIAN_POINT('Ctrl Pts',(2.66099130849232,0.559817762465603,
13.8103758687955));
#447563=CARTESIAN_POINT('Ctrl Pts',(2.67291358661161,0.547524511381774,
13.7804579775006));
#447564=CARTESIAN_POINT('Ctrl Pts',(2.68409774534096,0.554798318173647,
13.7901904343351));
#447565=CARTESIAN_POINT('Ctrl Pts',(2.67995883734142,0.570001125964826,
13.7927914348263));
#447566=CARTESIAN_POINT('Ctrl Pts',(2.68110739585066,0.552874007887763,
13.7597120340895));
#447567=CARTESIAN_POINT('Ctrl Pts',(2.6940474929302,0.56129665459444,13.7635825532445));
#447568=CARTESIAN_POINT('Ctrl Pts',(2.69113187582353,0.576028765544045,
13.7651073818884));
#447569=CARTESIAN_POINT('Ctrl Pts',(2.6795028603843,0.551826453983024,13.7381884353898));
#447570=CARTESIAN_POINT('Ctrl Pts',(2.6921405607098,0.560051199639204,13.7368803041982));
#447571=CARTESIAN_POINT('Ctrl Pts',(2.68894362822502,0.574848809574822,
13.7363986145813));
#447572=CARTESIAN_POINT('Origin',(2.6503461928975,0.559064456922638,13.7902182540695));
#447573=CARTESIAN_POINT('Ctrl Pts',(2.63242059297149,0.521087791455569,
13.8235227101244));
#447574=CARTESIAN_POINT('Ctrl Pts',(2.64205001535561,0.527369265237085,
13.8358800583119));
#447575=CARTESIAN_POINT('Ctrl Pts',(2.6356337482334,0.54264858345725,13.8390832900376));
#447576=CARTESIAN_POINT('Ctrl Pts',(2.64240807409376,0.527608325952603,
13.8124254819052));
#447577=CARTESIAN_POINT('Ctrl Pts',(2.65205619652767,0.533901998500128,
13.8247886449158));
#447578=CARTESIAN_POINT('Ctrl Pts',(2.64561610727068,0.549194023593774,
13.8279860620657));
#447579=CARTESIAN_POINT('Ctrl Pts',(2.65239107915191,0.534125938158196,
13.8013225099955));
#447580=CARTESIAN_POINT('Ctrl Pts',(2.6620533503664,0.540428838189978,13.8136962257787));
#447581=CARTESIAN_POINT('Ctrl Pts',(2.65559399359633,0.555736206840366,
13.8168830918626));
#447582=CARTESIAN_POINT('Ctrl Pts',(2.66236978230273,0.540640741774223,
13.7902140179785));
#447583=CARTESIAN_POINT('Ctrl Pts',(2.67204194848582,0.546950092206022,
13.802602731458));
#447584=CARTESIAN_POINT('Ctrl Pts',(2.66556758396314,0.562275259629211,
13.8057746032558));
#447585=CARTESIAN_POINT('Origin',(2.62039699312968,0.539511499794142,13.8235269408515));
#447586=CARTESIAN_POINT('Ctrl Pts',(2.64401005104368,0.45869500919504,13.8235269408515));
#447587=CARTESIAN_POINT('Ctrl Pts',(2.6555551918918,0.456219864433972,13.8362179249168));
#447588=CARTESIAN_POINT('Ctrl Pts',(2.65472321565854,0.439161997638721,
13.8391868794938));
#447589=CARTESIAN_POINT('Ctrl Pts',(2.63344674969771,0.460959658914779,
13.8400110824519));
#447590=CARTESIAN_POINT('Ctrl Pts',(2.64198600108674,0.455630207857054,
13.8494522556837));
#447591=CARTESIAN_POINT('Ctrl Pts',(2.63736255658733,0.4429988323026,13.85569149686));
#447592=CARTESIAN_POINT('Ctrl Pts',(2.62031150822566,0.470596212111629,
13.8586819406588));
#447593=CARTESIAN_POINT('Ctrl Pts',(2.62112006089859,0.46631809497788,13.868010383617));
#447594=CARTESIAN_POINT('Ctrl Pts',(2.61564415722987,0.4591134197039,13.8744918421245));
#447595=CARTESIAN_POINT('Ctrl Pts',(2.61454705303784,0.501350765503517,
13.8587686893867));
#447596=CARTESIAN_POINT('Ctrl Pts',(2.6137456411473,0.505590796977642,13.8680909899357));
#447597=CARTESIAN_POINT('Ctrl Pts',(2.60605056105728,0.51031119356202,13.8745789365163));
#447598=CARTESIAN_POINT('Ctrl Pts',(2.62336306961101,0.515174398301808,
13.8400379222776));
#447599=CARTESIAN_POINT('Ctrl Pts',(2.62941251526406,0.523216440405561,
13.8494748685453));
#447600=CARTESIAN_POINT('Ctrl Pts',(2.62056751556218,0.533342006342256,
13.8557104837033));
#447601=CARTESIAN_POINT('Ctrl Pts',(2.63242388933283,0.521089942655079,
13.8235269408542));
#447602=CARTESIAN_POINT('Ctrl Pts',(2.64231080727512,0.527544822390061,
13.8362179249195));
#447603=CARTESIAN_POINT('Ctrl Pts',(2.63541047323881,0.543166870727066,
13.8391868794965));
#447604=CARTESIAN_POINT('Origin',(2.63939829832935,0.437183808928625,13.8235269408515));
#447605=CARTESIAN_POINT('Ctrl Pts',(2.67897844191641,0.451198189573393,
13.7902140241682));
#447606=CARTESIAN_POINT('Ctrl Pts',(2.69027089583447,0.448781770755981,
13.8026027327198));
#447607=CARTESIAN_POINT('Ctrl Pts',(2.68972991167073,0.432153924581312,
13.8057746032556));
#447608=CARTESIAN_POINT('Ctrl Pts',(2.66732612174214,0.453696312344323,
13.8013225161807));
#447609=CARTESIAN_POINT('Ctrl Pts',(2.67860702462015,0.45128236161113,13.8136962270464));
#447610=CARTESIAN_POINT('Ctrl Pts',(2.67807365792942,0.434676515493367,
13.8168830918628));
#447611=CARTESIAN_POINT('Ctrl Pts',(2.65566877814783,0.456195512078463,
13.8124254880875));
#447612=CARTESIAN_POINT('Ctrl Pts',(2.66693316277136,0.453785094252894,
13.8247886461868));
#447613=CARTESIAN_POINT('Ctrl Pts',(2.66641227077088,0.437200485914964,
13.8279860620656));
#447614=CARTESIAN_POINT('Ctrl Pts',(2.64400620776571,0.458695832375514,
13.8235227163065));
#447615=CARTESIAN_POINT('Ctrl Pts',(2.65524875957551,0.456290086744523,
13.8358800595847));
#447616=CARTESIAN_POINT('Ctrl Pts',(2.65474553983445,0.439725890395448,
13.8390832900376));
#447617=CARTESIAN_POINT('Origin',(2.67437054464763,0.429686163521245,13.7902182540695));
#447618=CARTESIAN_POINT('Ctrl Pts',(2.69898492939505,0.446909002455508,
13.7382347919292));
#447619=CARTESIAN_POINT('Ctrl Pts',(2.71374498611075,0.443769162573877,
13.7369371795943));
#447620=CARTESIAN_POINT('Ctrl Pts',(2.71606716391856,0.428797480395553,
13.7364597369711));
#447621=CARTESIAN_POINT('Ctrl Pts',(2.70083446112151,0.446512484641241,
13.7595490285573));
#447622=CARTESIAN_POINT('Ctrl Pts',(2.71594647093971,0.443296747451537,
13.7633824266926));
#447623=CARTESIAN_POINT('Ctrl Pts',(2.71850298030877,0.428486010800249,
13.7648920890506));
#447624=CARTESIAN_POINT('Ctrl Pts',(2.69140195064382,0.448534703778785,
13.7803806590111));
#447625=CARTESIAN_POINT('Ctrl Pts',(2.70447442184469,0.445758486441053,
13.7901039518744));
#447626=CARTESIAN_POINT('Ctrl Pts',(2.70608539327615,0.430077599588828,
13.7926933640892));
#447627=CARTESIAN_POINT('Ctrl Pts',(2.67500614181622,0.452049771980561,
13.7936647693663));
#447628=CARTESIAN_POINT('Ctrl Pts',(2.68558750660803,0.449811904449398,
13.8072068914933));
#447629=CARTESIAN_POINT('Ctrl Pts',(2.68453573459646,0.432796086940902,
13.8104111085397));
#447630=CARTESIAN_POINT('Origin',(2.69463704657198,0.425341259745436,13.7435492065112));
#447631=CARTESIAN_POINT('Origin',(2.69463704657198,0.425341259745436,14.));
#447632=CARTESIAN_POINT('Origin',(2.69463704657198,0.425341259745437,12.5369868989719));
#447633=CARTESIAN_POINT('Ctrl Pts',(2.70429834586343,0.462353790169003,
12.506462012331));
#447634=CARTESIAN_POINT('Ctrl Pts',(2.71074344959975,0.463455709321185,
12.4999388158272));
#447635=CARTESIAN_POINT('Ctrl Pts',(2.71066719557032,0.463442672172536,
12.4907030323752));
#447636=CARTESIAN_POINT('Ctrl Pts',(2.70873630098556,0.449842469795504,
12.5042014951932));
#447637=CARTESIAN_POINT('Ctrl Pts',(2.71373382299294,0.445796994433825,
12.4980716682127));
#447638=CARTESIAN_POINT('Ctrl Pts',(2.71483027555077,0.43909450556667,12.4907355092743));
#447639=CARTESIAN_POINT('Ctrl Pts',(2.70428171392088,0.445782623083065,
12.5218047446509));
#447640=CARTESIAN_POINT('Ctrl Pts',(2.71468215884852,0.440183550280961,
12.5216906929434));
#447641=CARTESIAN_POINT('Ctrl Pts',(2.71640231170236,0.428546891461126,
12.5161988840776));
#447642=CARTESIAN_POINT('Ctrl Pts',(2.69921122967856,0.446860480198498,
12.5369868989719));
#447643=CARTESIAN_POINT('Ctrl Pts',(2.71420610628378,0.443673129085926,
12.5369868989719));
#447644=CARTESIAN_POINT('Ctrl Pts',(2.7164087662027,0.428502307723778,12.5369868989719));
#447645=CARTESIAN_POINT('Origin',(5.06527468391092E-31,-4.21128796913916E-31,
12.5));
#447646=CARTESIAN_POINT('Origin',(2.59782442414821,0.672680104343423,12.5));
#447647=CARTESIAN_POINT('',(2.59782442414821,0.672680104343423,12.5893111709658));
#447648=CARTESIAN_POINT('',(2.59782442414821,0.672680104343423,13.8235269408515));
#447649=CARTESIAN_POINT('',(2.59782442414821,0.672680104343423,12.5));
#447650=CARTESIAN_POINT('',(2.63329143090732,0.668057969474058,13.7902182540695));
#447651=CARTESIAN_POINT('',(2.59782442414821,0.672680104343423,13.8235269408515));
#447652=CARTESIAN_POINT('',(2.65384464771224,0.665379431058994,13.7435492065112));
#447653=CARTESIAN_POINT('Origin',(2.58622487819144,0.674192110063431,13.7445212918691));
#447654=CARTESIAN_POINT('',(2.65384464771224,0.665379431058994,12.5369868989719));
#447655=CARTESIAN_POINT('',(2.65384464771224,0.665379431058994,12.5));
#447656=CARTESIAN_POINT('Ctrl Pts',(2.65384464771224,0.665379431058994,
12.5369868989719));
#447657=CARTESIAN_POINT('Ctrl Pts',(2.63518485910551,0.667811213931451,
12.5544431401645));
#447658=CARTESIAN_POINT('Ctrl Pts',(2.61651172452202,0.670244736079652,
12.5718848856037));
#447659=CARTESIAN_POINT('Ctrl Pts',(2.59782442414821,0.672680104343423,
12.5893111709658));
#447660=CARTESIAN_POINT('Origin',(2.79844051361145,0.90252811439659,12.5));
#447661=CARTESIAN_POINT('',(2.62582115106376,0.768560006826695,13.7435492065112));
#447662=CARTESIAN_POINT('',(2.60944684686499,0.755852078156887,13.7902182540695));
#447663=CARTESIAN_POINT('Origin',(2.56641800548108,0.722457837985626,13.7418732680453));
#447664=CARTESIAN_POINT('',(2.58119104811553,0.733923044064349,13.8235269408515));
#447665=CARTESIAN_POINT('',(2.60944684686499,0.755852078156887,13.7902182540695));
#447666=CARTESIAN_POINT('',(2.58119104811553,0.733923044064349,12.5893111709658));
#447667=CARTESIAN_POINT('',(2.58119104811553,0.733923044064349,12.5));
#447668=CARTESIAN_POINT('',(2.62582115106376,0.768560006826695,12.5369868989719));
#447669=CARTESIAN_POINT('Ctrl Pts',(2.58119104811553,0.733923044064349,
12.5893111709658));
#447670=CARTESIAN_POINT('Ctrl Pts',(2.59607881696841,0.745477287978364,
12.5718848856037));
#447671=CARTESIAN_POINT('Ctrl Pts',(2.61095530024189,0.75702277327057,12.5544431401645));
#447672=CARTESIAN_POINT('Ctrl Pts',(2.62582115106376,0.768560006826695,
12.5369868989719));
#447673=CARTESIAN_POINT('',(2.62582115106376,0.768560006826695,12.5));
#447674=CARTESIAN_POINT('Origin',(2.60226668190706,0.70676686087736,12.5));
#447675=CARTESIAN_POINT('',(2.56940516467475,0.69668168079129,13.8587068136939));
#447676=CARTESIAN_POINT('Ctrl Pts',(2.58119104811137,0.733923044069481,
13.8235269408542));
#447677=CARTESIAN_POINT('Ctrl Pts',(2.57980673583883,0.732848693586994,
13.8262006681044));
#447678=CARTESIAN_POINT('Ctrl Pts',(2.57849661569527,0.731611999105121,
13.8288634856214));
#447679=CARTESIAN_POINT('Ctrl Pts',(2.57725650689879,0.73022562265809,13.8314912288862));
#447680=CARTESIAN_POINT('Ctrl Pts',(2.5759780826409,0.728796411539299,13.8342001611531));
#447681=CARTESIAN_POINT('Ctrl Pts',(2.57477227246862,0.727206869931805,
13.8368750301949));
#447682=CARTESIAN_POINT('Ctrl Pts',(2.573651705902,0.725429073630892,13.8394886372969));
#447683=CARTESIAN_POINT('Ctrl Pts',(2.57356516182794,0.725291770110243,
13.8396904925131));
#447684=CARTESIAN_POINT('Ctrl Pts',(2.57347914264093,0.725153328817326,
13.8398919674349));
#447685=CARTESIAN_POINT('Ctrl Pts',(2.57339366328585,0.725013729983829,
13.8400930404591));
#447686=CARTESIAN_POINT('Ctrl Pts',(2.57206183742609,0.722838686240423,
13.8432258934518));
#447687=CARTESIAN_POINT('Ctrl Pts',(2.57086689571031,0.720394327187652,
13.8462331177034));
#447688=CARTESIAN_POINT('Ctrl Pts',(2.56993447561436,0.717718007930113,
13.8489036603661));
#447689=CARTESIAN_POINT('Ctrl Pts',(2.56962937690785,0.716842285123152,
13.849777493004));
#447690=CARTESIAN_POINT('Ctrl Pts',(2.56935258380642,0.715941879350438,
13.85061494757));
#447691=CARTESIAN_POINT('Ctrl Pts',(2.56910905624937,0.71501854406218,13.8514076489583));
#447692=CARTESIAN_POINT('Ctrl Pts',(2.56859396034427,0.713065556762635,
13.8530843267192));
#447693=CARTESIAN_POINT('Ctrl Pts',(2.56817995315849,0.710817397480646,
13.8546805203176));
#447694=CARTESIAN_POINT('Ctrl Pts',(2.56802525284017,0.708379837091844,
13.8559412814273));
#447695=CARTESIAN_POINT('Ctrl Pts',(2.56800454892053,0.708053612459863,
13.8561100121513));
#447696=CARTESIAN_POINT('Ctrl Pts',(2.56798843423225,0.707724048824368,
13.8562727473908));
#447697=CARTESIAN_POINT('Ctrl Pts',(2.5679772273273,0.707391445193895,13.8564289040185));
#447698=CARTESIAN_POINT('Ctrl Pts',(2.5679264041412,0.705883091524182,13.8571370725437));
#447699=CARTESIAN_POINT('Ctrl Pts',(2.5679778968314,0.704285627645851,13.8577210840553));
#447700=CARTESIAN_POINT('Ctrl Pts',(2.56815903667544,0.702662092778626,
13.8581177131616));
#447701=CARTESIAN_POINT('Ctrl Pts',(2.56821005189016,0.702204849479646,
13.8582294175695));
#447702=CARTESIAN_POINT('Ctrl Pts',(2.5682711734966,0.701745553554236,13.8583265086086));
#447703=CARTESIAN_POINT('Ctrl Pts',(2.56834257260757,0.701285624802972,
13.8584082369006));
#447704=CARTESIAN_POINT('Ctrl Pts',(2.56844515398361,0.700624830522173,
13.8585256585398));
#447705=CARTESIAN_POINT('Ctrl Pts',(2.56857054501354,0.699954564335941,
13.8586122832068));
#447706=CARTESIAN_POINT('Ctrl Pts',(2.5687162646227,0.699292383029854,13.8586682984299));
#447707=CARTESIAN_POINT('Ctrl Pts',(2.56883282586531,0.698762703624906,
13.8587131050557));
#447708=CARTESIAN_POINT('Ctrl Pts',(2.56896345259151,0.698232296553719,
13.8587357943552));
#447709=CARTESIAN_POINT('Ctrl Pts',(2.56910865207591,0.69770121989644,13.8587355499465));
#447710=CARTESIAN_POINT('Ctrl Pts',(2.56920249796439,0.697357972391407,
13.8587353919793));
#447711=CARTESIAN_POINT('Ctrl Pts',(2.56930137925673,0.697018146810693,
13.8587257282814));
#447712=CARTESIAN_POINT('Ctrl Pts',(2.56940516467475,0.69668168079129,13.8587068136939));
#447713=CARTESIAN_POINT('Ctrl Pts',(2.56940516467475,0.69668168079129,13.8587068136939));
#447714=CARTESIAN_POINT('Ctrl Pts',(2.56974650925671,0.695575062396045,
13.8586446046466));
#447715=CARTESIAN_POINT('Ctrl Pts',(2.57014083738664,0.694504739382945,
13.858482427929));
#447716=CARTESIAN_POINT('Ctrl Pts',(2.57058406984971,0.693468882554442,
13.8582284286032));
#447717=CARTESIAN_POINT('Ctrl Pts',(2.5710387747979,0.692406213944235,13.8579678548414));
#447718=CARTESIAN_POINT('Ctrl Pts',(2.5715474673676,0.691377825557677,13.857615680862));
#447719=CARTESIAN_POINT('Ctrl Pts',(2.57208140752236,0.690419964702098,
13.8571944833187));
#447720=CARTESIAN_POINT('Ctrl Pts',(2.57341390978546,0.688029524975056,
13.8561433417727));
#447721=CARTESIAN_POINT('Ctrl Pts',(2.57496179646164,0.685964180731319,
13.8546163505475));
#447722=CARTESIAN_POINT('Ctrl Pts',(2.57651885142229,0.684239188934588,
13.8528973491087));
#447723=CARTESIAN_POINT('Ctrl Pts',(2.57680330239142,0.683924058383181,
13.8525833129073));
#447724=CARTESIAN_POINT('Ctrl Pts',(2.57708801004023,0.683620154271979,
13.8522628768812));
#447725=CARTESIAN_POINT('Ctrl Pts',(2.5773716816524,0.683327394353899,13.851937733538));
#447726=CARTESIAN_POINT('Ctrl Pts',(2.57910402483015,0.681539550152906,
13.8499521282529));
#447727=CARTESIAN_POINT('Ctrl Pts',(2.58097282149759,0.679992474613509,
13.847639871647));
#447728=CARTESIAN_POINT('Ctrl Pts',(2.58282862244085,0.678705590183642,
13.8452109780794));
#447729=CARTESIAN_POINT('Ctrl Pts',(2.58366358569838,0.678126594241463,
13.8441181685877));
#447730=CARTESIAN_POINT('Ctrl Pts',(2.58449573846324,0.67759957354068,13.8430021611332));
#447731=CARTESIAN_POINT('Ctrl Pts',(2.58531167264054,0.677122994520366,
13.8418824960098));
#447732=CARTESIAN_POINT('Ctrl Pts',(2.58723444236496,0.675999923889115,
13.8392439765549));
#447733=CARTESIAN_POINT('Ctrl Pts',(2.58915715575003,0.675100013115308,
13.8364981347964));
#447734=CARTESIAN_POINT('Ctrl Pts',(2.59107039127242,0.674389888570763,
13.8336931113419));
#447735=CARTESIAN_POINT('Ctrl Pts',(2.59293376116954,0.673698272361454,
13.8309611966328));
#447736=CARTESIAN_POINT('Ctrl Pts',(2.59479020447205,0.673186514409347,
13.8281701127186));
#447737=CARTESIAN_POINT('Ctrl Pts',(2.59663035114141,0.672863077529967,
13.8253580685121));
#447738=CARTESIAN_POINT('Ctrl Pts',(2.59702929692528,0.672792956065454,
13.8247484142933));
#447739=CARTESIAN_POINT('Ctrl Pts',(2.59742740652207,0.672731844514956,
13.8241378483365));
#447740=CARTESIAN_POINT('Ctrl Pts',(2.59782442414821,0.672680104343423,
13.8235269408515));
#447741=CARTESIAN_POINT('',(2.56906221652971,0.697875482880214,12.5969504640361));
#447742=CARTESIAN_POINT('Origin',(2.60229866198257,0.706775343658747,12.584524458991));
#447743=CARTESIAN_POINT('Origin',(2.60229866198257,0.706775343658747,12.584524458991));
#447744=CARTESIAN_POINT('Ctrl Pts',(2.58119104811553,0.733923044064349,
12.5893111709658));
#447745=CARTESIAN_POINT('Ctrl Pts',(2.57223724225787,0.726974087651837,
12.5770542771492));
#447746=CARTESIAN_POINT('Ctrl Pts',(2.579684388468,0.712402070352234,12.5737548217797));
#447747=CARTESIAN_POINT('Ctrl Pts',(2.60077001653969,0.749118079599428,
12.5663937883685));
#447748=CARTESIAN_POINT('Ctrl Pts',(2.59180478885918,0.742160258827957,
12.5540940315304));
#447749=CARTESIAN_POINT('Ctrl Pts',(2.59927787167869,0.727544547128353,
12.5508374392248));
#447750=CARTESIAN_POINT('Ctrl Pts',(2.62032923002471,0.76429778352992,12.5434499600945));
#447751=CARTESIAN_POINT('Ctrl Pts',(2.6113348531964,0.757317340405427,12.5311293540533));
#447752=CARTESIAN_POINT('Ctrl Pts',(2.61885149015097,0.742673162946224,
12.5278936106989));
#447753=CARTESIAN_POINT('Ctrl Pts',(2.63987023600205,0.779463356801421,
12.5204817579905));
#447754=CARTESIAN_POINT('Ctrl Pts',(2.63083134315524,0.772448365253878,
12.5081597038247));
#447755=CARTESIAN_POINT('Ctrl Pts',(2.6384067793781,0.757789006095711,12.5049254088044));
#447756=CARTESIAN_POINT('Ctrl Pts',(2.62582115106376,0.768560006826693,
12.5369868989719));
#447757=CARTESIAN_POINT('Ctrl Pts',(2.62655703813531,0.769131120990989,
12.5342545179733));
#447758=CARTESIAN_POINT('Ctrl Pts',(2.62733581815076,0.769577617128592,
12.5314872231885));
#447759=CARTESIAN_POINT('Ctrl Pts',(2.62814142522858,0.769825847558425,
12.5287124745063));
#447760=CARTESIAN_POINT('Ctrl Pts',(2.62886796167813,0.770049714081107,
12.5262100684184));
#447761=CARTESIAN_POINT('Ctrl Pts',(2.62961587403641,0.770111158706971,
12.5237004536639));
#447762=CARTESIAN_POINT('Ctrl Pts',(2.63040343216518,0.769945168450488,
12.5212220730815));
#447763=CARTESIAN_POINT('Ctrl Pts',(2.63100637604196,0.769818088549847,
12.5193246583486));
#447764=CARTESIAN_POINT('Ctrl Pts',(2.6316396323685,0.769555564173845,12.517417831369));
#447765=CARTESIAN_POINT('Ctrl Pts',(2.63228442007479,0.769062194619328,
12.5155812248347));
#447766=CARTESIAN_POINT('Ctrl Pts',(2.63255910310341,0.768852016537232,
12.5147988205793));
#447767=CARTESIAN_POINT('Ctrl Pts',(2.63283632603725,0.768599951185227,
12.5140295443047));
#447768=CARTESIAN_POINT('Ctrl Pts',(2.63311665696456,0.76829928970777,12.5132817086137));
#447769=CARTESIAN_POINT('Ctrl Pts',(2.63354089990074,0.767844279234201,
12.5121499604604));
#447770=CARTESIAN_POINT('Ctrl Pts',(2.63397619142954,0.767263267700918,
12.5110494206568));
#447771=CARTESIAN_POINT('Ctrl Pts',(2.63440149722945,0.766525523104014,
12.5100666561695));
#447772=CARTESIAN_POINT('Ctrl Pts',(2.63464570684037,0.766101911855346,
12.5095023550641));
#447773=CARTESIAN_POINT('Ctrl Pts',(2.63488888024053,0.765621404797231,
12.5089719619137));
#447774=CARTESIAN_POINT('Ctrl Pts',(2.63512076064498,0.765090124489872,
12.5085043804652));
#447775=CARTESIAN_POINT('Ctrl Pts',(2.63546008741233,0.76431266496418,12.5078201359221));
#447776=CARTESIAN_POINT('Ctrl Pts',(2.63578396543699,0.763403444948041,
12.5072563000949));
#447777=CARTESIAN_POINT('Ctrl Pts',(2.6360624654395,0.762421255284591,12.5068768744332));
#447778=CARTESIAN_POINT('Ctrl Pts',(2.63626328311331,0.761713028923076,
12.5066032824114));
#447779=CARTESIAN_POINT('Ctrl Pts',(2.63644409276933,0.760954436615598,
12.5064197834844));
#447780=CARTESIAN_POINT('Ctrl Pts',(2.63659731194885,0.760188439435245,
12.5063282718343));
#447781=CARTESIAN_POINT('Ctrl Pts',(2.63682096451549,0.759070320698664,
12.5061946931565));
#447782=CARTESIAN_POINT('Ctrl Pts',(2.63699165202955,0.757912734307713,
12.5062515701262));
#447783=CARTESIAN_POINT('Ctrl Pts',(2.63711408043292,0.756789777984089,
12.5064436508398));
#447784=CARTESIAN_POINT('',(2.579684388468,0.712402070352234,12.5737548217797));
#447785=CARTESIAN_POINT('Origin',(2.59467945374211,0.716543086824676,12.5893111709658));
#447786=CARTESIAN_POINT('Ctrl Pts',(2.63711408043292,0.75678977798409,12.5064436508398));
#447787=CARTESIAN_POINT('Ctrl Pts',(2.62861328777127,0.750218863901955,
12.5164271754438));
#447788=CARTESIAN_POINT('Ctrl Pts',(2.62010899761836,0.743645510418688,
12.5264061185523));
#447789=CARTESIAN_POINT('Ctrl Pts',(2.61160108737432,0.73706963087177,12.536380305637));
#447790=CARTESIAN_POINT('Ctrl Pts',(2.60096792515941,0.728851115170202,
12.5488460165097));
#447791=CARTESIAN_POINT('Ctrl Pts',(2.59032910523158,0.720628651366349,
12.5613043021964));
#447792=CARTESIAN_POINT('Ctrl Pts',(2.579684388468,0.712402070352235,12.5737548217797));
#447793=CARTESIAN_POINT('Ctrl Pts',(2.59782442414821,0.672680104343423,
12.5893111709658));
#447794=CARTESIAN_POINT('Ctrl Pts',(2.58658550304428,0.674144784164906,
12.5770542771492));
#447795=CARTESIAN_POINT('Ctrl Pts',(2.58563779814647,0.690482027821093,
12.5737548217797));
#447796=CARTESIAN_POINT('Ctrl Pts',(2.58733860850922,0.674046637877755,
12.5928319619712));
#447797=CARTESIAN_POINT('Ctrl Pts',(2.58020635512882,0.678261418784176,
12.5821634970842));
#447798=CARTESIAN_POINT('Ctrl Pts',(2.58181684954086,0.690970463203354,
12.5773203894503));
#447799=CARTESIAN_POINT('Ctrl Pts',(2.57314512645719,0.68294209551513,12.5969440695591));
#447800=CARTESIAN_POINT('Ctrl Pts',(2.57207391382378,0.686816504637298,
12.5878292599214));
#447801=CARTESIAN_POINT('Ctrl Pts',(2.57675908943053,0.694142719460964,
12.5813877129824));
#447802=CARTESIAN_POINT('Ctrl Pts',(2.56507357985403,0.712455234639498,
12.596957478804));
#447803=CARTESIAN_POINT('Ctrl Pts',(2.56613695319864,0.708609479800865,
12.5878468778671));
#447804=CARTESIAN_POINT('Ctrl Pts',(2.5738759248271,0.704707454676469,12.5814011370086));
#447805=CARTESIAN_POINT('Ctrl Pts',(2.57282509538981,0.727430314406849,
12.5928371701607));
#447806=CARTESIAN_POINT('Ctrl Pts',(2.56881311714011,0.720188830012911,
12.5821692192952));
#447807=CARTESIAN_POINT('Ctrl Pts',(2.57662560011115,0.710040483753784,
12.5773318885715));
#447808=CARTESIAN_POINT('Ctrl Pts',(2.58119104811549,0.73392304406439,12.5893111709658));
#447809=CARTESIAN_POINT('Ctrl Pts',(2.57223724225783,0.726974087651879,
12.5770542771492));
#447810=CARTESIAN_POINT('Ctrl Pts',(2.57968438846796,0.712402070352277,
12.5737548217797));
#447811=CARTESIAN_POINT('',(2.58563779814647,0.690482027821093,12.5737548217797));
#447812=CARTESIAN_POINT('Origin',(2.60066746911387,0.694495628525142,12.5893111709658));
#447813=CARTESIAN_POINT('Ctrl Pts',(2.57968438846796,0.712402070352277,
12.5737548217797));
#447814=CARTESIAN_POINT('Ctrl Pts',(2.57887306713315,0.71181378698289,12.5746934679442));
#447815=CARTESIAN_POINT('Ctrl Pts',(2.57808281832406,0.711014510899208,
12.5756680099006));
#447816=CARTESIAN_POINT('Ctrl Pts',(2.57740118190847,0.710097518279326,
12.5765688348656));
#447817=CARTESIAN_POINT('Ctrl Pts',(2.5772207262134,0.709854754634652,12.5768073183026));
#447818=CARTESIAN_POINT('Ctrl Pts',(2.57704772001294,0.709603939593634,
12.5770407398754));
#447819=CARTESIAN_POINT('Ctrl Pts',(2.5768833328898,0.709347136134447,12.5772674179684));
#447820=CARTESIAN_POINT('Ctrl Pts',(2.57620873258859,0.708293284180544,
12.5781976435658));
#447821=CARTESIAN_POINT('Ctrl Pts',(2.57565046725709,0.707072646108709,
12.5790594849312));
#447822=CARTESIAN_POINT('Ctrl Pts',(2.57529014610397,0.705747556907826,
12.5797571720116));
#447823=CARTESIAN_POINT('Ctrl Pts',(2.57505538391673,0.70488421364749,12.580211740231));
#447824=CARTESIAN_POINT('Ctrl Pts',(2.57491209519903,0.703932370528216,
12.5806009430798));
#447825=CARTESIAN_POINT('Ctrl Pts',(2.5748878861526,0.702956395842894,12.5808812374708));
#447826=CARTESIAN_POINT('Ctrl Pts',(2.57486708255046,0.702117709811969,
12.5811221033394));
#447827=CARTESIAN_POINT('Ctrl Pts',(2.57493390164797,0.701244030831503,
12.581287365893));
#447828=CARTESIAN_POINT('Ctrl Pts',(2.57509288576999,0.700385306584494,
12.581359338449));
#447829=CARTESIAN_POINT('Ctrl Pts',(2.57511498128005,0.700265961646139,
12.5813693411482));
#447830=CARTESIAN_POINT('Ctrl Pts',(2.57513880510371,0.700146875662145,
12.5813775999465));
#447831=CARTESIAN_POINT('Ctrl Pts',(2.57516431683881,0.700028151144637,
12.5813841266931));
#447832=CARTESIAN_POINT('Ctrl Pts',(2.57520760058298,0.699826720641251,
12.5813952001081));
#447833=CARTESIAN_POINT('Ctrl Pts',(2.57525662819535,0.69962510945769,12.5814007534795));
#447834=CARTESIAN_POINT('Ctrl Pts',(2.57531156994799,0.699423452001435,
12.5814005856065));
#447835=CARTESIAN_POINT('Ctrl Pts',(2.57556307181075,0.698500343009653,
12.5813998171494));
#447836=CARTESIAN_POINT('Ctrl Pts',(2.57592079907501,0.697639955419613,
12.58127954464));
#447837=CARTESIAN_POINT('Ctrl Pts',(2.57635539889883,0.696835814200509,
12.5810700125799));
#447838=CARTESIAN_POINT('Ctrl Pts',(2.57688034600285,0.69586450316664,12.5808169217085));
#447839=CARTESIAN_POINT('Ctrl Pts',(2.57753222009882,0.694983124404432,
12.5804173076348));
#447840=CARTESIAN_POINT('Ctrl Pts',(2.57823295416952,0.694253434655424,
12.5799304713245));
#447841=CARTESIAN_POINT('Ctrl Pts',(2.57910138443712,0.693349119180426,
12.5793271277669));
#447842=CARTESIAN_POINT('Ctrl Pts',(2.58007550391725,0.692599383195681,
12.5785808224116));
#447843=CARTESIAN_POINT('Ctrl Pts',(2.58109490679138,0.692010695126134,
12.5777485681082));
#447844=CARTESIAN_POINT('Ctrl Pts',(2.58261392875775,0.691133485406916,
12.576508418016));
#447845=CARTESIAN_POINT('Ctrl Pts',(2.58421727195989,0.690615305817478,
12.5750928681475));
#447846=CARTESIAN_POINT('Ctrl Pts',(2.58563779814647,0.690482027821093,
12.5737548217797));
#447847=CARTESIAN_POINT('Ctrl Pts',(2.58563779814647,0.690482027821093,
12.5737548217797));
#447848=CARTESIAN_POINT('Ctrl Pts',(2.58658550304428,0.674144784164906,
12.5770542771492));
#447849=CARTESIAN_POINT('Ctrl Pts',(2.59782442414821,0.672680104343423,
12.5893111709658));
#447850=CARTESIAN_POINT('Ctrl Pts',(2.61019578895115,0.687332418034614,
12.5508408821982));
#447851=CARTESIAN_POINT('Ctrl Pts',(2.61114322150309,0.670944370677193,
12.55409748406));
#447852=CARTESIAN_POINT('Ctrl Pts',(2.6223964805919,0.669477822299387,12.5663972313419));
#447853=CARTESIAN_POINT('Ctrl Pts',(2.63472963964692,0.68418471508971,12.52790050457));
#447854=CARTESIAN_POINT('Ctrl Pts',(2.63565390608582,0.667750086743115,
12.5311362602938));
#447855=CARTESIAN_POINT('Ctrl Pts',(2.64694374786836,0.66627877083173,12.5434568539655));
#447856=CARTESIAN_POINT('Ctrl Pts',(2.65924122446842,0.681038757064725,
12.5049357605811));
#447857=CARTESIAN_POINT('Ctrl Pts',(2.66012245983368,0.664561293387921,
12.5081700652078));
#447858=CARTESIAN_POINT('Ctrl Pts',(2.6714681674702,0.663082696921053,12.5204921097672));
#447859=CARTESIAN_POINT('Ctrl Pts',(2.65763169752453,0.681245331426205,
12.5064436508395));
#447860=CARTESIAN_POINT('Ctrl Pts',(2.65813124959428,0.680132094919352,
12.5062361689309));
#447861=CARTESIAN_POINT('Ctrl Pts',(2.65860327198979,0.678953118041469,
12.5061871075062));
#447862=CARTESIAN_POINT('Ctrl Pts',(2.65899529819047,0.6777880720771,12.5063648335164));
#447863=CARTESIAN_POINT('Ctrl Pts',(2.659173380672,0.677258836337068,12.5064455676329));
#447864=CARTESIAN_POINT('Ctrl Pts',(2.65933723071486,0.676725023291958,
12.506574497099));
#447865=CARTESIAN_POINT('Ctrl Pts',(2.65947881823401,0.676209212862752,
12.5067492519495));
#447866=CARTESIAN_POINT('Ctrl Pts',(2.65976334384976,0.675172671783016,
12.5071004286051));
#447867=CARTESIAN_POINT('Ctrl Pts',(2.65996764954846,0.674170505851928,
12.5076537929612));
#447868=CARTESIAN_POINT('Ctrl Pts',(2.66008566893586,0.673279822254663,
12.5083435010503));
#447869=CARTESIAN_POINT('Ctrl Pts',(2.66009309896159,0.673223748399357,
12.5083869222963));
#447870=CARTESIAN_POINT('Ctrl Pts',(2.66010017597423,0.673168108716542,
12.5084308732336));
#447871=CARTESIAN_POINT('Ctrl Pts',(2.66010689419839,0.673112918993485,
12.5084753333615));
#447872=CARTESIAN_POINT('Ctrl Pts',(2.66016078322331,0.672670224571504,
12.508831962269));
#447873=CARTESIAN_POINT('Ctrl Pts',(2.66019396189943,0.672247649732734,
12.509227847131));
#447874=CARTESIAN_POINT('Ctrl Pts',(2.66020823511389,0.671857979002731,
12.5096423454524));
#447875=CARTESIAN_POINT('Ctrl Pts',(2.66025296105096,0.67063692339594,12.5109411997424));
#447876=CARTESIAN_POINT('Ctrl Pts',(2.66012446388748,0.669664210401967,
12.5124831113042));
#447877=CARTESIAN_POINT('Ctrl Pts',(2.65990367814058,0.668890794518083,
12.5140723025008));
#447878=CARTESIAN_POINT('Ctrl Pts',(2.65988299027427,0.668818324602665,
12.5142212114565));
#447879=CARTESIAN_POINT('Ctrl Pts',(2.65986151043435,0.668747581228111,
12.5143705582413));
#447880=CARTESIAN_POINT('Ctrl Pts',(2.65983931687852,0.668678511711671,
12.5145201959299));
#447881=CARTESIAN_POINT('Ctrl Pts',(2.6595542076112,0.667791210939238,12.5164425148273));
#447882=CARTESIAN_POINT('Ctrl Pts',(2.65915176673183,0.667146463610461,
12.5184635205941));
#447883=CARTESIAN_POINT('Ctrl Pts',(2.65867357626237,0.666664214032228,
12.5205025929157));
#447884=CARTESIAN_POINT('Ctrl Pts',(2.65839620683639,0.666384490162265,
12.5216853356836));
#447885=CARTESIAN_POINT('Ctrl Pts',(2.6580941961743,0.666159602824852,12.5228750347131));
#447886=CARTESIAN_POINT('Ctrl Pts',(2.65778074882996,0.665976959426719,
12.5240609649613));
#447887=CARTESIAN_POINT('Ctrl Pts',(2.65701140913917,0.66552867100448,12.5269717671326));
#447888=CARTESIAN_POINT('Ctrl Pts',(2.65614628521843,0.665331238509816,
12.5299036066169));
#447889=CARTESIAN_POINT('Ctrl Pts',(2.65521799080379,0.665304375786692,
12.5328133004019));
#447890=CARTESIAN_POINT('Ctrl Pts',(2.6547723554318,0.665291480115423,12.5342101228451));
#447891=CARTESIAN_POINT('Ctrl Pts',(2.65431270291339,0.665318433204005,
12.5356023438238));
#447892=CARTESIAN_POINT('Ctrl Pts',(2.65384464771223,0.665379431058994,
12.5369868989719));
#447893=CARTESIAN_POINT('Origin',(15.291180332043,-0.98688563005775,-1.23957201933111));
#447894=CARTESIAN_POINT('Ctrl Pts',(2.62578810934736,0.76853441374342,12.5369868989719));
#447895=CARTESIAN_POINT('Ctrl Pts',(2.63792369202002,0.777915828182662,
12.5369868989719));
#447896=CARTESIAN_POINT('Ctrl Pts',(2.63331726935041,0.792546760274453,
12.5369868989719));
#447897=CARTESIAN_POINT('Ctrl Pts',(2.62989037041483,0.77170575111314,12.5218025310016));
#447898=CARTESIAN_POINT('Ctrl Pts',(2.63683581805028,0.781266955056582,
12.5216901060418));
#447899=CARTESIAN_POINT('Ctrl Pts',(2.63333132698383,0.792502165297268,
12.5161920673678));
#447900=CARTESIAN_POINT('Ctrl Pts',(2.63566681220354,0.769982732988681,
12.5042015548894));
#447901=CARTESIAN_POINT('Ctrl Pts',(2.63841449808402,0.775798880108503,
12.4980677368513));
#447902=CARTESIAN_POINT('Ctrl Pts',(2.63649140361122,0.782317506296004,
12.4907278922777));
#447903=CARTESIAN_POINT('Ctrl Pts',(2.63709485533895,0.756784260822992,
12.506463626192));
#447904=CARTESIAN_POINT('Ctrl Pts',(2.64338375481666,0.758589027205586,
12.4999376786891));
#447905=CARTESIAN_POINT('Ctrl Pts',(2.64330694505359,0.758566984608351,
12.4906970594712));
#447906=CARTESIAN_POINT('Origin',(2.61233274543718,0.785939964066368,12.5369868989719));
#447907=CARTESIAN_POINT('Origin',(2.61233274543718,0.785939964066368,14.));
#447908=CARTESIAN_POINT('Origin',(2.61233274543718,0.785939964066368,13.7435492065112));
#447909=CARTESIAN_POINT('Ctrl Pts',(2.606260700401,0.753379377104391,13.793642941384));
#447910=CARTESIAN_POINT('Ctrl Pts',(2.61481907347178,0.759986984037845,
13.8071662555867));
#447911=CARTESIAN_POINT('Ctrl Pts',(2.60650673469415,0.774850510122887,
13.8103758687955));
#447912=CARTESIAN_POINT('Ctrl Pts',(2.61939135650484,0.763569940165686,
13.7804579775006));
#447913=CARTESIAN_POINT('Ctrl Pts',(2.62994541808841,0.771731156730597,
13.7901904343351));
#447914=CARTESIAN_POINT('Ctrl Pts',(2.62458111199279,0.786546019007273,
13.7927914348263));
#447915=CARTESIAN_POINT('Ctrl Pts',(2.62712186789201,0.769569508183912,
13.7597120340895));
#447916=CARTESIAN_POINT('Ctrl Pts',(2.63933238396734,0.779018867270492,
13.7635825532445));
#447917=CARTESIAN_POINT('Ctrl Pts',(2.63522566452749,0.793464308474768,
13.7651073818884));
#447918=CARTESIAN_POINT('Ctrl Pts',(2.62560805675334,0.768394655392109,
13.7381884353898));
#447919=CARTESIAN_POINT('Ctrl Pts',(2.63753331304775,0.777622123784822,
13.7368803041982));
#447920=CARTESIAN_POINT('Ctrl Pts',(2.63314087550801,0.792109916217712,
13.7363986145813));
#447921=CARTESIAN_POINT('Origin',(2.59595844123841,0.77323203539656,13.7902182540695));
#447922=CARTESIAN_POINT('Ctrl Pts',(2.58118793806113,0.733920631343859,
13.8235227101244));
#447923=CARTESIAN_POINT('Ctrl Pts',(2.59027332090908,0.740966091359053,
13.8358800583119));
#447924=CARTESIAN_POINT('Ctrl Pts',(2.5826329971052,0.755671583572118,13.8390832900376));
#447925=CARTESIAN_POINT('Ctrl Pts',(2.59061070256867,0.741233541730976,
13.8124254819052));
#447926=CARTESIAN_POINT('Ctrl Pts',(2.59971372893087,0.748292684149464,
13.8247886449158));
#447927=CARTESIAN_POINT('Ctrl Pts',(2.59204862653025,0.76300889922979,13.8279860620657));
#447928=CARTESIAN_POINT('Ctrl Pts',(2.60002924409971,0.748543174709559,
13.8013225099955));
#447929=CARTESIAN_POINT('Ctrl Pts',(2.60914562003793,0.755612667165597,
13.8136962257787));
#447930=CARTESIAN_POINT('Ctrl Pts',(2.60146006359299,0.770342604267049,
13.8168830918626));
#447931=CARTESIAN_POINT('Ctrl Pts',(2.60944372696379,0.755849657798537,
13.7902140179785));
#447932=CARTESIAN_POINT('Ctrl Pts',(2.61856943917847,0.76292638572319,13.802602731458));
#447933=CARTESIAN_POINT('Ctrl Pts',(2.61086747415274,0.777672839102351,
13.8057746032558));
#447934=CARTESIAN_POINT('Origin',(2.56770264248895,0.751303001304022,13.8235269408515));
#447935=CARTESIAN_POINT('Ctrl Pts',(2.59782442414821,0.672680104343423,
13.8235269408515));
#447936=CARTESIAN_POINT('Ctrl Pts',(2.60953289676871,0.671154231581342,
13.8362179249168));
#447937=CARTESIAN_POINT('Ctrl Pts',(2.61009406336906,0.654085309643976,
13.8391868794938));
#447938=CARTESIAN_POINT('Ctrl Pts',(2.58711168133992,0.674076211503438,
13.8400110824519));
#447939=CARTESIAN_POINT('Ctrl Pts',(2.59605691881181,0.669460522017201,
13.8494522556837));
#447940=CARTESIAN_POINT('Ctrl Pts',(2.59247843281422,0.656494322674229,
13.85569149686));
#447941=CARTESIAN_POINT('Ctrl Pts',(2.57323467775334,0.682610055742881,
13.8586819406588));
#447942=CARTESIAN_POINT('Ctrl Pts',(2.57438924629646,0.678412078240054,
13.868010383617));
#447943=CARTESIAN_POINT('Ctrl Pts',(2.56951881116523,0.670785038943894,
13.8744918421245));
#447944=CARTESIAN_POINT('Ctrl Pts',(2.56498262170184,0.712792419283031,
13.8587686893867));
#447945=CARTESIAN_POINT('Ctrl Pts',(2.56383827451559,0.716953019893181,
13.8680909899357));
#447946=CARTESIAN_POINT('Ctrl Pts',(2.55578404302611,0.721030489282356,
13.8745789365163));
#447947=CARTESIAN_POINT('Ctrl Pts',(2.57264254930173,0.727288642278172,
13.8400379222776));
#447948=CARTESIAN_POINT('Ctrl Pts',(2.5780163648333,0.735797011131287,13.8494748685453));
#447949=CARTESIAN_POINT('Ctrl Pts',(2.56837546851325,0.745167935493955,
13.8557104837033));
#447950=CARTESIAN_POINT('Ctrl Pts',(2.58119104811137,0.733923044069481,
13.8235269408542));
#447951=CARTESIAN_POINT('Ctrl Pts',(2.59051893552723,0.741162321322599,
13.8362179249195));
#447952=CARTESIAN_POINT('Ctrl Pts',(2.5823682198157,0.756169947298957,13.8391868794965));
#447953=CARTESIAN_POINT('Origin',(2.59498137918254,0.650864580161703,13.8235269408515));
#447954=CARTESIAN_POINT('Ctrl Pts',(2.63328752098124,0.668058478257452,
13.7902140241682));
#447955=CARTESIAN_POINT('Ctrl Pts',(2.64473936075701,0.666570539702663,
13.8026027327198));
#447956=CARTESIAN_POINT('Ctrl Pts',(2.64555550050207,0.649953926082844,
13.8057746032556));
#447957=CARTESIAN_POINT('Ctrl Pts',(2.62147035274383,0.669598516461878,
13.8013225161808));
#447958=CARTESIAN_POINT('Ctrl Pts',(2.6329104787429,0.668112096261962,13.8136962270464));
#447959=CARTESIAN_POINT('Ctrl Pts',(2.63373241740558,0.651518030390442,
13.8168830918628));
#447960=CARTESIAN_POINT('Ctrl Pts',(2.6096480900189,0.671139218590636,13.8124254880875));
#447961=CARTESIAN_POINT('Ctrl Pts',(2.62107146476185,0.669654973151802,
13.8247886461868));
#447962=CARTESIAN_POINT('Ctrl Pts',(2.62190410553007,0.653083091196216,
13.8279860620656));
#447963=CARTESIAN_POINT('Ctrl Pts',(2.59782052656158,0.672680611521997,
13.8235227163065));
#447964=CARTESIAN_POINT('Ctrl Pts',(2.60922176031045,0.671199243154391,
13.8358800595847));
#447965=CARTESIAN_POINT('Ctrl Pts',(2.61007035076852,0.654649145721658,
13.8390832900376));
#447966=CARTESIAN_POINT('Origin',(2.63044838594165,0.646242445292339,13.7902182540695));
#447967=CARTESIAN_POINT('Ctrl Pts',(2.65357704709218,0.665414277516546,
13.7382347919292));
#447968=CARTESIAN_POINT('Ctrl Pts',(2.66854391703599,0.663487966841118,
13.7369371795943));
#447969=CARTESIAN_POINT('Ctrl Pts',(2.67207869907657,0.648755380749542,
13.7364597369711));
#447970=CARTESIAN_POINT('Ctrl Pts',(2.65545274453738,0.665169833088515,
13.7595490285574));
#447971=CARTESIAN_POINT('Ctrl Pts',(2.67077658282397,0.663196565092251,
13.7633824266925));
#447972=CARTESIAN_POINT('Ctrl Pts',(2.67453179815223,0.648643489192444,
13.7648920890506));
#447973=CARTESIAN_POINT('Ctrl Pts',(2.64588679032705,0.666416486287619,
13.7803806590111));
#447974=CARTESIAN_POINT('Ctrl Pts',(2.6591420514446,0.664715034345835,13.7901039518745));
#447975=CARTESIAN_POINT('Ctrl Pts',(2.66202580035423,0.649217633478212,
13.7926933640892));
#447976=CARTESIAN_POINT('Ctrl Pts',(2.62925902651006,0.66858344775921,13.7936647693663));
#447977=CARTESIAN_POINT('Ctrl Pts',(2.63998758966256,0.667215506010775,
13.8072068914932));
#447978=CARTESIAN_POINT('Ctrl Pts',(2.64032626442967,0.650170578048214,
13.8104111085397));
#447979=CARTESIAN_POINT('Origin',(2.65100160274657,0.643563906877274,13.7435492065112));
#447980=CARTESIAN_POINT('Origin',(2.65100160274657,0.643563906877274,14.));
#447981=CARTESIAN_POINT('Origin',(2.65100160274657,0.643563906877274,12.5369868989719));
#447982=CARTESIAN_POINT('Ctrl Pts',(2.65761389002454,0.681240766742555,
12.506462012331));
#447983=CARTESIAN_POINT('Ctrl Pts',(2.66394773156924,0.682864355137594,
12.4999388158272));
#447984=CARTESIAN_POINT('Ctrl Pts',(2.66387279391744,0.682845145957675,
12.4907030323752));
#447985=CARTESIAN_POINT('Ctrl Pts',(2.66305686697698,0.669132811297897,
12.5042014951932));
#447986=CARTESIAN_POINT('Ctrl Pts',(2.66836750394045,0.665508141360079,
12.4980716682127));
#447987=CARTESIAN_POINT('Ctrl Pts',(2.67000662320842,0.658917325534159,
12.4907355092743));
#447988=CARTESIAN_POINT('Ctrl Pts',(2.65894801738008,0.664723383190354,
12.5218047446509));
#447989=CARTESIAN_POINT('Ctrl Pts',(2.66977023209787,0.659990673655744,
12.5216906929434));
#447990=CARTESIAN_POINT('Ctrl Pts',(2.67243315700827,0.648532943284871,
12.5161988840776));
#447991=CARTESIAN_POINT('Ctrl Pts',(2.65380654939458,0.665384362287319,
12.5369868989719));
#447992=CARTESIAN_POINT('Ctrl Pts',(2.66901133049048,0.663429838471607,
12.5369868989719));
#447993=CARTESIAN_POINT('Ctrl Pts',(2.67244322402028,0.648489033997923,
12.5369868989719));
#447994=CARTESIAN_POINT('Origin',(4.97175483587121E-31,-3.80155074318086E-31,
12.5));
#447995=CARTESIAN_POINT('Origin',(2.53435070432089,0.882188624381805,12.5));
#447996=CARTESIAN_POINT('',(2.53435070432089,0.882188624381805,12.5893111709658));
#447997=CARTESIAN_POINT('',(2.53435070432089,0.882188624381805,13.8235269408515));
#447998=CARTESIAN_POINT('',(2.53435070432089,0.882188624381805,12.5));
#447999=CARTESIAN_POINT('',(2.57007644444249,0.880472759595413,13.7902182540695));
#448000=CARTESIAN_POINT('',(2.53435070432089,0.882188624381805,13.8235269408515));
#448001=CARTESIAN_POINT('',(2.59077959786117,0.879478411772317,13.7435492065112));
#448002=CARTESIAN_POINT('Origin',(2.52266651239525,0.882750128347015,13.7445212918698));
#448003=CARTESIAN_POINT('',(2.59077959786117,0.879478411772317,12.5369868989719));
#448004=CARTESIAN_POINT('',(2.59077959786117,0.879478411772317,12.5));
#448005=CARTESIAN_POINT('Ctrl Pts',(2.59077959786117,0.879478411772317,
12.5369868989719));
#448006=CARTESIAN_POINT('Ctrl Pts',(2.57198368528203,0.8803811570874,12.5544431401645));
#448007=CARTESIAN_POINT('Ctrl Pts',(2.55317432936665,0.881284548069926,
12.5718848856037));
#448008=CARTESIAN_POINT('Ctrl Pts',(2.53435070432089,0.882188624381805,
12.5893111709658));
#448009=CARTESIAN_POINT('Origin',(2.71556451367195,1.12762390786281,12.5));
#448010=CARTESIAN_POINT('',(2.55443917227923,0.980031487551649,13.7435492065112));
#448011=CARTESIAN_POINT('',(2.53915516638813,0.966031185662336,13.7902182540695));
#448012=CARTESIAN_POINT('Origin',(2.49899144051201,0.929240812034377,13.7418732680438));
#448013=CARTESIAN_POINT('',(2.51278080633584,0.941872008709604,13.8235269408515));
#448014=CARTESIAN_POINT('',(2.53915516638813,0.966031185662336,13.7902182540695));
#448015=CARTESIAN_POINT('',(2.51278080633584,0.941872008709604,12.5893111709658));
#448016=CARTESIAN_POINT('',(2.51278080633584,0.941872008709604,12.5));
#448017=CARTESIAN_POINT('',(2.55443917227923,0.980031487551649,12.5369868989719));
#448018=CARTESIAN_POINT('Ctrl Pts',(2.51278080633584,0.941872008709604,
12.5893111709658));
#448019=CARTESIAN_POINT('Ctrl Pts',(2.52667725922265,0.954601298202966,
12.5718848856037));
#448020=CARTESIAN_POINT('Ctrl Pts',(2.5405631779909,0.967320938338619,12.5544431401645));
#448021=CARTESIAN_POINT('Ctrl Pts',(2.55443917227923,0.980031487551649,
12.5369868989719));
#448022=CARTESIAN_POINT('',(2.55443917227923,0.980031487551649,12.5));
#448023=CARTESIAN_POINT('Origin',(2.53599979372999,0.91652404529259,12.5));
#448024=CARTESIAN_POINT('',(2.50406965628867,0.903793904085336,13.8587068136939));
#448025=CARTESIAN_POINT('Ctrl Pts',(2.51278080633127,0.94187200871438,13.8235269408542));
#448026=CARTESIAN_POINT('Ctrl Pts',(2.51148866978172,0.940688398742956,
13.8262006681044));
#448027=CARTESIAN_POINT('Ctrl Pts',(2.51028371103606,0.939349032305694,
13.8288634856214));
#448028=CARTESIAN_POINT('Ctrl Pts',(2.50916073115021,0.937866188532404,
13.8314912288862));
#448029=CARTESIAN_POINT('Ctrl Pts',(2.50800305471791,0.936337529550384,
13.834200161153));
#448030=CARTESIAN_POINT('Ctrl Pts',(2.5069308191771,0.934654992288229,13.8368750301949));
#448031=CARTESIAN_POINT('Ctrl Pts',(2.50595888810607,0.932791774879842,
13.8394886372968));
#448032=CARTESIAN_POINT('Ctrl Pts',(2.50588382351188,0.932647874079853,
13.839690492513));
#448033=CARTESIAN_POINT('Ctrl Pts',(2.5058093747972,0.932502882076606,13.8398919674349));
#448034=CARTESIAN_POINT('Ctrl Pts',(2.50573555846853,0.932356780385714,
13.8400930404591));
#448035=CARTESIAN_POINT('Ctrl Pts',(2.50458545040666,0.930080417749296,
13.8432258934518));
#448036=CARTESIAN_POINT('Ctrl Pts',(2.50359372271598,0.927546793256493,
13.8462331177034));
#448037=CARTESIAN_POINT('Ctrl Pts',(2.50288255003621,0.924803378336516,
13.8489036603661));
#448038=CARTESIAN_POINT('Ctrl Pts',(2.50264984605906,0.923905701047975,
13.8497774930041));
#448039=CARTESIAN_POINT('Ctrl Pts',(2.50244736539328,0.922985730093805,
13.85061494757));
#448040=CARTESIAN_POINT('Ctrl Pts',(2.5022799085519,0.922045617370849,13.8514076489583));
#448041=CARTESIAN_POINT('Ctrl Pts',(2.5019257131815,0.920057143377244,13.8530843267192));
#448042=CARTESIAN_POINT('Ctrl Pts',(2.50169632942285,0.917782719230699,
13.8546805203176));
#448043=CARTESIAN_POINT('Ctrl Pts',(2.50174082765797,0.915340660110883,
13.8559412814274));
#448044=CARTESIAN_POINT('Ctrl Pts',(2.50174678296495,0.915013833402807,
13.8561100121513));
#448045=CARTESIAN_POINT('Ctrl Pts',(2.50175758439277,0.914684052866435,
13.8562727473908));
#448046=CARTESIAN_POINT('Ctrl Pts',(2.5017735250615,0.914351642480321,13.8564289040185));
#448047=CARTESIAN_POINT('Ctrl Pts',(2.50184581581231,0.912844165171528,
13.8571370725437));
#448048=CARTESIAN_POINT('Ctrl Pts',(2.50202734530105,0.911256213854759,
13.8577210840554));
#448049=CARTESIAN_POINT('Ctrl Pts',(2.50234021558104,0.909652845744784,
13.8581177131616));
#448050=CARTESIAN_POINT('Ctrl Pts',(2.50242833062056,0.909201282098762,
13.8582294175695));
#448051=CARTESIAN_POINT('Ctrl Pts',(2.50252668573171,0.908748496421003,
13.8583265086086));
#448052=CARTESIAN_POINT('Ctrl Pts',(2.50263533573102,0.908295917735097,
13.8584082369006));
#448053=CARTESIAN_POINT('Ctrl Pts',(2.50279143664439,0.907645683527221,
13.8585256585398));
#448054=CARTESIAN_POINT('Ctrl Pts',(2.50297104336265,0.906987868129444,
13.8586122832068));
#448055=CARTESIAN_POINT('Ctrl Pts',(2.50317025202566,0.906339767677968,
13.8586682984299));
#448056=CARTESIAN_POINT('Ctrl Pts',(2.50332959920916,0.905821351560919,
13.8587131050557));
#448057=CARTESIAN_POINT('Ctrl Pts',(2.50350302438606,0.90530335666637,13.8587357943552));
#448058=CARTESIAN_POINT('Ctrl Pts',(2.503691028409,0.904785882228803,13.8587355499465));
#448059=CARTESIAN_POINT('Ctrl Pts',(2.50381253989126,0.904451426162635,
13.8587353919793));
#448060=CARTESIAN_POINT('Ctrl Pts',(2.50393879110388,0.904120791066776,
13.8587257282814));
#448061=CARTESIAN_POINT('Ctrl Pts',(2.50406965628867,0.903793904085336,
13.8587068136939));
#448062=CARTESIAN_POINT('Ctrl Pts',(2.50406965628867,0.903793904085336,
13.8587068136939));
#448063=CARTESIAN_POINT('Ctrl Pts',(2.50450006474724,0.902718790623857,
13.8586446046466));
#448064=CARTESIAN_POINT('Ctrl Pts',(2.5049803220448,0.901684170425667,13.858482427929));
#448065=CARTESIAN_POINT('Ctrl Pts',(2.50550651163635,0.900687887885843,
13.8582284286032));
#448066=CARTESIAN_POINT('Ctrl Pts',(2.5060463209484,0.899665817892324,13.8579678548414));
#448067=CARTESIAN_POINT('Ctrl Pts',(2.50663714408614,0.898682314550188,
13.857615680862));
#448068=CARTESIAN_POINT('Ctrl Pts',(2.50724738215115,0.89777116197706,13.8571944833187));
#448069=CARTESIAN_POINT('Ctrl Pts',(2.50877029365242,0.895497287545792,
13.8561433417727));
#448070=CARTESIAN_POINT('Ctrl Pts',(2.51048137459297,0.893564982698628,
13.8546163505475));
#448071=CARTESIAN_POINT('Ctrl Pts',(2.51217385142717,0.891972645104082,
13.8528973491086));
#448072=CARTESIAN_POINT('Ctrl Pts',(2.51248304197463,0.891681748518294,
13.8525833129073));
#448073=CARTESIAN_POINT('Ctrl Pts',(2.51279157328859,0.891402061939436,
13.8522628768812));
#448074=CARTESIAN_POINT('Ctrl Pts',(2.51309816365804,0.89113339802571,13.851937733538));
#448075=CARTESIAN_POINT('Ctrl Pts',(2.51497046850669,0.889492704780083,
13.8499521282529));
#448076=CARTESIAN_POINT('Ctrl Pts',(2.5169591479262,0.888103101284376,13.847639871647));
#448077=CARTESIAN_POINT('Ctrl Pts',(2.5189136668728,0.886971763861578,13.8452109780794));
#448078=CARTESIAN_POINT('Ctrl Pts',(2.51979304540339,0.886462751737545,
13.8441181685877));
#448079=CARTESIAN_POINT('Ctrl Pts',(2.5206653863283,0.886005312830334,13.8430021611332));
#448080=CARTESIAN_POINT('Ctrl Pts',(2.52151745116643,0.885596825797609,
13.8418824960098));
#448081=CARTESIAN_POINT('Ctrl Pts',(2.52352536371575,0.884634215673897,
13.8392439765549));
#448082=CARTESIAN_POINT('Ctrl Pts',(2.52551503051308,0.883894018269432,
13.8364981347963));
#448083=CARTESIAN_POINT('Ctrl Pts',(2.52747978164497,0.883342203062412,
13.8336931113419));
#448084=CARTESIAN_POINT('Ctrl Pts',(2.52939332447419,0.882804770094281,
13.8309611966327));
#448085=CARTESIAN_POINT('Ctrl Pts',(2.53128530363879,0.882446032338076,
13.8281701127185));
#448086=CARTESIAN_POINT('Ctrl Pts',(2.53314569048023,0.882273660704874,
13.825358068512));
#448087=CARTESIAN_POINT('Ctrl Pts',(2.53354902435522,0.882236290348769,
13.8247484142932));
#448088=CARTESIAN_POINT('Ctrl Pts',(2.53395079043386,0.882207831769924,
13.8241378483365));
#448089=CARTESIAN_POINT('Ctrl Pts',(2.53435070432089,0.882188624381805,
13.8235269408515));
#448090=CARTESIAN_POINT('',(2.50363054332231,0.90495578043872,12.5969504640361));
#448091=CARTESIAN_POINT('Origin',(2.53603097596901,0.916535106521272,12.584524458991));
#448092=CARTESIAN_POINT('Origin',(2.53603097596901,0.916535106521272,12.584524458991));
#448093=CARTESIAN_POINT('Ctrl Pts',(2.51278080633584,0.941872008709604,
12.5893111709658));
#448094=CARTESIAN_POINT('Ctrl Pts',(2.50442319798711,0.934216356075829,
12.5770542771492));
#448095=CARTESIAN_POINT('Ctrl Pts',(2.5130333191225,0.920299837513742,12.5737548217797));
#448096=CARTESIAN_POINT('Ctrl Pts',(2.53105609089778,0.958612351706294,
12.5663937883685));
#448097=CARTESIAN_POINT('Ctrl Pts',(2.52268782125892,0.950946933224371,
12.5540940315304));
#448098=CARTESIAN_POINT('Ctrl Pts',(2.531327354201,0.936988979726258,12.5508374392248));
#448099=CARTESIAN_POINT('Ctrl Pts',(2.54931293592164,0.975335803902121,
12.5434499600945));
#448100=CARTESIAN_POINT('Ctrl Pts',(2.54091745805819,0.967645462414973,
12.5311293540533));
#448101=CARTESIAN_POINT('Ctrl Pts',(2.54960272043615,0.95366268794112,12.5278936106989));
#448102=CARTESIAN_POINT('Ctrl Pts',(2.56755278580165,0.992043688376609,
12.5204817579905));
#448103=CARTESIAN_POINT('Ctrl Pts',(2.55911575606026,0.984315284954743,
12.5081597038247));
#448104=CARTESIAN_POINT('Ctrl Pts',(2.56786085950626,0.970322171983944,
12.5049254088044));
#448105=CARTESIAN_POINT('Ctrl Pts',(2.55443917227922,0.980031487551647,
12.5369868989719));
#448106=CARTESIAN_POINT('Ctrl Pts',(2.55512605964089,0.980660683008643,
12.5342545179733));
#448107=CARTESIAN_POINT('Ctrl Pts',(2.5558658547498,0.981169171268279,12.5314872231885));
#448108=CARTESIAN_POINT('Ctrl Pts',(2.55664854815204,0.981482240187567,
12.5287124745063));
#448109=CARTESIAN_POINT('Ctrl Pts',(2.55735441991161,0.981764581278338,
12.5262100684184));
#448110=CARTESIAN_POINT('Ctrl Pts',(2.5580948353458,0.98188678325276,12.5237004536639));
#448111=CARTESIAN_POINT('Ctrl Pts',(2.55889330268674,0.98178553861399,12.5212220730815));
#448112=CARTESIAN_POINT('Ctrl Pts',(2.55950459850916,0.981708027084652,
12.5193246583486));
#448113=CARTESIAN_POINT('Ctrl Pts',(2.56015714590132,0.981497992506336,
12.5174178313691));
#448114=CARTESIAN_POINT('Ctrl Pts',(2.56084000232861,0.981058820782296,
12.5155812248348));
#448115=CARTESIAN_POINT('Ctrl Pts',(2.56113090283701,0.980871731267295,
12.5147988205794));
#448116=CARTESIAN_POINT('Ctrl Pts',(2.56142774900065,0.980643100884673,
12.5140295443047));
#448117=CARTESIAN_POINT('Ctrl Pts',(2.56173165385155,0.980366289406517,
12.5132817086137));
#448118=CARTESIAN_POINT('Ctrl Pts',(2.56219157273206,0.979947372680541,
12.5121499604604));
#448119=CARTESIAN_POINT('Ctrl Pts',(2.56267277369802,0.979403774715852,
12.5110494206568));
#448120=CARTESIAN_POINT('Ctrl Pts',(2.5631567973615,0.978703151274273,12.5100666561695));
#448121=CARTESIAN_POINT('Ctrl Pts',(2.56343472263447,0.978300854907512,
12.5095023550641));
#448122=CARTESIAN_POINT('Ctrl Pts',(2.56371625268125,0.977841767586617,
12.5089719619137));
#448123=CARTESIAN_POINT('Ctrl Pts',(2.56399066579999,0.977331155476289,
12.5085043804652));
#448124=CARTESIAN_POINT('Ctrl Pts',(2.56439223365444,0.976583941164728,
12.5078201359221));
#448125=CARTESIAN_POINT('Ctrl Pts',(2.5647891438738,0.975704145568934,12.5072563000949));
#448126=CARTESIAN_POINT('Ctrl Pts',(2.56514677476629,0.974747924396236,
12.5068768744332));
#448127=CARTESIAN_POINT('Ctrl Pts',(2.56540465125918,0.97405842310423,12.5066032824114));
#448128=CARTESIAN_POINT('Ctrl Pts',(2.56564669160147,0.973317092615597,
12.5064197834844));
#448129=CARTESIAN_POINT('Ctrl Pts',(2.56586183683818,0.97256613301322,12.5063282718343));
#448130=CARTESIAN_POINT('Ctrl Pts',(2.5661758822765,0.971469964484967,12.5061946931565));
#448131=CARTESIAN_POINT('Ctrl Pts',(2.56644035587931,0.970330142484219,
12.5062515701262));
#448132=CARTESIAN_POINT('Ctrl Pts',(2.56665390827765,0.969220901756571,
12.5064436508398));
#448133=CARTESIAN_POINT('',(2.5130333191225,0.920299837513742,12.5737548217797));
#448134=CARTESIAN_POINT('Origin',(2.52764095826809,0.925649312122715,12.5893111709658));
#448135=CARTESIAN_POINT('Ctrl Pts',(2.56665390827765,0.96922090175657,12.5064436508398));
#448136=CARTESIAN_POINT('Ctrl Pts',(2.5587169918014,0.961978958329554,12.5164271754438));
#448137=CARTESIAN_POINT('Ctrl Pts',(2.55077678830534,0.954734298540301,
12.5264061185523));
#448138=CARTESIAN_POINT('Ctrl Pts',(2.54283318266135,0.94748682602163,12.536380305637));
#448139=CARTESIAN_POINT('Ctrl Pts',(2.53290528674318,0.938428955319102,
12.5488460165097));
#448140=CARTESIAN_POINT('Ctrl Pts',(2.52297207374467,0.929366688495138,
12.5613043021964));
#448141=CARTESIAN_POINT('Ctrl Pts',(2.5130333191225,0.920299837513742,12.5737548217797));
#448142=CARTESIAN_POINT('Ctrl Pts',(2.53435070432089,0.882188624381805,
12.5893111709658));
#448143=CARTESIAN_POINT('Ctrl Pts',(2.52302979479691,0.882732354194987,
12.5770542771492));
#448144=CARTESIAN_POINT('Ctrl Pts',(2.52075360628342,0.898937990273401,
12.5737548217797));
#448145=CARTESIAN_POINT('Ctrl Pts',(2.5237883941991,0.882695919568392,12.5928319619712));
#448146=CARTESIAN_POINT('Ctrl Pts',(2.51633632903146,0.886315331275931,
12.5821634970843));
#448147=CARTESIAN_POINT('Ctrl Pts',(2.51690555955102,0.899113357643908,
12.5773203894503));
#448148=CARTESIAN_POINT('Ctrl Pts',(2.50891707740886,0.890404877751204,
12.5969440695591));
#448149=CARTESIAN_POINT('Ctrl Pts',(2.50753362883541,0.894179081322358,
12.5878292599214));
#448150=CARTESIAN_POINT('Ctrl Pts',(2.51160606038543,0.901862804077567,
12.5813877129824));
#448151=CARTESIAN_POINT('Ctrl Pts',(2.49846679338592,0.919161908359058,
12.596957478804));
#448152=CARTESIAN_POINT('Ctrl Pts',(2.49984009316504,0.915415624751862,
12.5878468778671));
#448153=CARTESIAN_POINT('Ctrl Pts',(2.50787136527611,0.912157381326999,
12.5814011370086));
#448154=CARTESIAN_POINT('Ctrl Pts',(2.50497190837032,0.934718980261566,
12.5928371701607));
#448155=CARTESIAN_POINT('Ctrl Pts',(2.50156352785204,0.92717457783683,12.5821692192952));
#448156=CARTESIAN_POINT('Ctrl Pts',(2.51017719986325,0.917696789252394,
12.5773318885715));
#448157=CARTESIAN_POINT('Ctrl Pts',(2.5127808063358,0.941872008709643,12.5893111709658));
#448158=CARTESIAN_POINT('Ctrl Pts',(2.50442319798707,0.934216356075868,
12.5770542771492));
#448159=CARTESIAN_POINT('Ctrl Pts',(2.51303331912246,0.920299837513782,
12.5737548217797));
#448160=CARTESIAN_POINT('',(2.52075360628342,0.898937990273401,12.5737548217797));
#448161=CARTESIAN_POINT('Origin',(2.53540612154271,0.904163293764707,12.5893111709658));
#448162=CARTESIAN_POINT('Ctrl Pts',(2.51303331912246,0.920299837513782,
12.5737548217797));
#448163=CARTESIAN_POINT('Ctrl Pts',(2.51227264794842,0.919647381388047,
12.5746934679442));
#448164=CARTESIAN_POINT('Ctrl Pts',(2.51155017704798,0.91878635221534,12.5756680099006));
#448165=CARTESIAN_POINT('Ctrl Pts',(2.5109455521328,0.917816851116875,12.5765688348656));
#448166=CARTESIAN_POINT('Ctrl Pts',(2.51078548437992,0.917560186433789,
12.5768073183026));
#448167=CARTESIAN_POINT('Ctrl Pts',(2.51063349759762,0.917296104347685,
12.5770407398754));
#448168=CARTESIAN_POINT('Ctrl Pts',(2.51049058932504,0.917026756304196,
12.5772674179684));
#448169=CARTESIAN_POINT('Ctrl Pts',(2.50990413241841,0.9159214247685,12.5781976435658));
#448170=CARTESIAN_POINT('Ctrl Pts',(2.50944721800345,0.914659344461954,
12.5790594849312));
#448171=CARTESIAN_POINT('Ctrl Pts',(2.50919610286065,0.913309294867038,
12.5797571720116));
#448172=CARTESIAN_POINT('Ctrl Pts',(2.50903249231582,0.912429689012493,
12.580211740231));
#448173=CARTESIAN_POINT('Ctrl Pts',(2.50896726443021,0.911469333711957,
12.5806009430798));
#448174=CARTESIAN_POINT('Ctrl Pts',(2.50902268693475,0.910494633239858,
12.5808812374708));
#448175=CARTESIAN_POINT('Ctrl Pts',(2.50907031325237,0.909657042180811,
12.5811221033394));
#448176=CARTESIAN_POINT('Ctrl Pts',(2.5092081229626,0.908791716671847,12.581287365893));
#448177=CARTESIAN_POINT('Ctrl Pts',(2.5094365720762,0.907948808440815,12.581359338449));
#448178=CARTESIAN_POINT('Ctrl Pts',(2.5094683217857,0.907831661602089,12.5813693411482));
#448179=CARTESIAN_POINT('Ctrl Pts',(2.50950177295079,0.907714913729678,
12.5813775999465));
#448180=CARTESIAN_POINT('Ctrl Pts',(2.50953687694806,0.907598663701455,
12.5813841266931));
#448181=CARTESIAN_POINT('Ctrl Pts',(2.50959643512516,0.907401431468428,
12.5813952001081));
#448182=CARTESIAN_POINT('Ctrl Pts',(2.50966173278532,0.907204487335008,
12.5814007534795));
#448183=CARTESIAN_POINT('Ctrl Pts',(2.50973292867859,0.907007979140197,
12.5814005856065));
#448184=CARTESIAN_POINT('Ctrl Pts',(2.51005883564221,0.906108441454079,
12.5813998171494));
#448185=CARTESIAN_POINT('Ctrl Pts',(2.51048550217453,0.905280074825782,
12.58127954464));
#448186=CARTESIAN_POINT('Ctrl Pts',(2.51098420087793,0.904514033240517,
12.5810700125799));
#448187=CARTESIAN_POINT('Ctrl Pts',(2.51158657213025,0.903588742226335,
12.5808169217085));
#448188=CARTESIAN_POINT('Ctrl Pts',(2.51230811772037,0.902763429969774,
12.5804173076348));
#448189=CARTESIAN_POINT('Ctrl Pts',(2.51306599664491,0.902093284535271,
12.5799304713245));
#448190=CARTESIAN_POINT('Ctrl Pts',(2.51400524738891,0.901262763224338,
12.5793271277669));
#448191=CARTESIAN_POINT('Ctrl Pts',(2.51503723600979,0.900594921705148,
12.5785808224116));
#448192=CARTESIAN_POINT('Ctrl Pts',(2.51610123044773,0.900091283244504,
12.5777485681082));
#448193=CARTESIAN_POINT('Ctrl Pts',(2.51768669872955,0.899340806760433,
12.576508418016));
#448194=CARTESIAN_POINT('Ctrl Pts',(2.51932694338654,0.898955038726519,
12.5750928681475));
#448195=CARTESIAN_POINT('Ctrl Pts',(2.52075360628342,0.898937990273401,
12.5737548217797));
#448196=CARTESIAN_POINT('Ctrl Pts',(2.52075360628342,0.898937990273401,
12.5737548217797));
#448197=CARTESIAN_POINT('Ctrl Pts',(2.52302979479691,0.882732354194987,
12.5770542771492));
#448198=CARTESIAN_POINT('Ctrl Pts',(2.53435070432089,0.882188624381805,
12.5893111709658));
#448199=CARTESIAN_POINT('Ctrl Pts',(2.54548660483675,0.897800564789506,
12.5508408821982));
#448200=CARTESIAN_POINT('Ctrl Pts',(2.54776666288385,0.881544271856277,
12.55409748406));
#448201=CARTESIAN_POINT('Ctrl Pts',(2.55910201498895,0.880999848383104,
12.5663972313419));
#448202=CARTESIAN_POINT('Ctrl Pts',(2.57019538818008,0.896663072159344,
12.52790050457));
#448203=CARTESIAN_POINT('Ctrl Pts',(2.5724561539806,0.880358464978034,12.5311362602938));
#448204=CARTESIAN_POINT('Ctrl Pts',(2.58382835565171,0.879812271664045,
12.5434568539655));
#448205=CARTESIAN_POINT('Ctrl Pts',(2.59488183750983,0.895525503767571,
12.5049357605811));
#448206=CARTESIAN_POINT('Ctrl Pts',(2.59710320689608,0.879174696355115,
12.5081700652078));
#448207=CARTESIAN_POINT('Ctrl Pts',(2.60853168196507,0.878625800296802,
12.5204921097672));
#448208=CARTESIAN_POINT('Ctrl Pts',(2.59326082840587,0.895600199381859,
12.5064436508395));
#448209=CARTESIAN_POINT('Ctrl Pts',(2.59384945736741,0.894531385208946,
12.5062361689309));
#448210=CARTESIAN_POINT('Ctrl Pts',(2.59441600670797,0.893394805486641,
12.5061871075061));
#448211=CARTESIAN_POINT('Ctrl Pts',(2.59490169053566,0.892265589891358,
12.5063648335164));
#448212=CARTESIAN_POINT('Ctrl Pts',(2.59512231808842,0.891752630515074,
12.5064455676329));
#448213=CARTESIAN_POINT('Ctrl Pts',(2.59532913365264,0.891233948988439,
12.506574497099));
#448214=CARTESIAN_POINT('Ctrl Pts',(2.59551229338953,0.89073139557313,12.5067492519495));
#448215=CARTESIAN_POINT('Ctrl Pts',(2.59588035999054,0.88972149497742,12.5071004286051));
#448216=CARTESIAN_POINT('Ctrl Pts',(2.59616567170592,0.888739316481922,
12.5076537929612));
#448217=CARTESIAN_POINT('Ctrl Pts',(2.59635589737542,0.887861216236564,
12.5083435010503));
#448218=CARTESIAN_POINT('Ctrl Pts',(2.59636787321813,0.887805934578458,
12.5083869222963));
#448219=CARTESIAN_POINT('Ctrl Pts',(2.59637946183328,0.887751056874326,
12.5084308732336));
#448220=CARTESIAN_POINT('Ctrl Pts',(2.59639065617788,0.887696598388155,
12.5084753333615));
#448221=CARTESIAN_POINT('Ctrl Pts',(2.59648044959668,0.887259769451156,
12.508831962269));
#448222=CARTESIAN_POINT('Ctrl Pts',(2.59654796164586,0.886841305065423,
12.509227847131));
#448223=CARTESIAN_POINT('Ctrl Pts',(2.5965939491494,0.886454094332113,12.5096423454524));
#448224=CARTESIAN_POINT('Ctrl Pts',(2.59673805363227,0.88524074726621,12.5109411997424));
#448225=CARTESIAN_POINT('Ctrl Pts',(2.59668926917174,0.88426079718275,12.5124831113042));
#448226=CARTESIAN_POINT('Ctrl Pts',(2.59653225864578,0.88347195868837,12.5140723025008));
#448227=CARTESIAN_POINT('Ctrl Pts',(2.59651754658752,0.883398043657455,
12.5142212114565));
#448228=CARTESIAN_POINT('Ctrl Pts',(2.59650190446177,0.883325784869281,
12.5143705582413));
#448229=CARTESIAN_POINT('Ctrl Pts',(2.59648541455998,0.883255136195124,
12.5145201959299));
#448230=CARTESIAN_POINT('Ctrl Pts',(2.59627357722047,0.882347548790702,
12.5164425148273));
#448231=CARTESIAN_POINT('Ctrl Pts',(2.59592502832276,0.881672144137725,
12.5184635205941));
#448232=CARTESIAN_POINT('Ctrl Pts',(2.59548773681026,0.881152522242616,
12.5205025929158));
#448233=CARTESIAN_POINT('Ctrl Pts',(2.59523409040039,0.880851120947565,
12.5216853356836));
#448234=CARTESIAN_POINT('Ctrl Pts',(2.59495141505961,0.880602365231525,
12.5228750347131));
#448235=CARTESIAN_POINT('Ctrl Pts',(2.59465389781798,0.880394780695765,
12.5240609649613));
#448236=CARTESIAN_POINT('Ctrl Pts',(2.59392365770967,0.879885275589271,
12.5269717671326));
#448237=CARTESIAN_POINT('Ctrl Pts',(2.5930775049986,0.879617984403987,12.5299036066169));
#448238=CARTESIAN_POINT('Ctrl Pts',(2.59215448896836,0.879515546451699,
12.5328133004019));
#448239=CARTESIAN_POINT('Ctrl Pts',(2.59171138752823,0.879466370269818,
12.5342101228451));
#448240=CARTESIAN_POINT('Ctrl Pts',(2.59125106753872,0.879455767726765,
12.5356023438238));
#448241=CARTESIAN_POINT('Ctrl Pts',(2.59077959786117,0.879478411772317,
12.5369868989719));
#448242=CARTESIAN_POINT('Origin',(15.3207548595525,0.262770591828722,-1.23958748038645));
#448243=CARTESIAN_POINT('Ctrl Pts',(2.5544083265803,0.980003286420626,12.5369868989719));
#448244=CARTESIAN_POINT('Ctrl Pts',(2.56573885673312,0.990342647626308,
12.5369868989719));
#448245=CARTESIAN_POINT('Ctrl Pts',(2.55995520476251,1.00454943028701,12.5369868989719));
#448246=CARTESIAN_POINT('Ctrl Pts',(2.55823844427557,0.983498443787384,
12.5218025310016));
#448247=CARTESIAN_POINT('Ctrl Pts',(2.56438145462366,0.993593952074142,
12.5216901060417));
#448248=CARTESIAN_POINT('Ctrl Pts',(2.55997285052496,1.00450612952355,12.5161920673677));
#448249=CARTESIAN_POINT('Ctrl Pts',(2.5641361074036,0.982251992495257,12.5042015548895));
#448250=CARTESIAN_POINT('Ctrl Pts',(2.56640058060124,0.988272748772843,
12.4980677368514));
#448251=CARTESIAN_POINT('Ctrl Pts',(2.56395255651642,0.994612934716805,
12.4907278922778));
#448252=CARTESIAN_POINT('Ctrl Pts',(2.56663519685345,0.969213835929737,
12.506463626192));
#448253=CARTESIAN_POINT('Ctrl Pts',(2.57275606532212,0.971525200791801,
12.4999376786891));
#448254=CARTESIAN_POINT('Ctrl Pts',(2.57268130781351,0.971496970830732,
12.4906970594712));
#448255=CARTESIAN_POINT('Origin',(2.53957902034697,0.996254184138538,12.5369868989719));
#448256=CARTESIAN_POINT('Origin',(2.53957902034697,0.996254184138538,14.));
#448257=CARTESIAN_POINT('Origin',(2.53957902034697,0.996254184138538,13.7435492065112));
#448258=CARTESIAN_POINT('Ctrl Pts',(2.53618116965488,0.963307011803056,
13.793642941384));
#448259=CARTESIAN_POINT('Ctrl Pts',(2.54417248413818,0.970590219326861,
13.8071662555867));
#448260=CARTESIAN_POINT('Ctrl Pts',(2.53467628861993,0.984726755476637,
13.8103758687955));
#448261=CARTESIAN_POINT('Ctrl Pts',(2.54843750908966,0.974533936977943,
13.7804579775006));
#448262=CARTESIAN_POINT('Ctrl Pts',(2.55829123798887,0.983528251766164,
13.7901904343351));
#448263=CARTESIAN_POINT('Ctrl Pts',(2.55173723236927,0.997856578064193,
13.7927914348262));
#448264=CARTESIAN_POINT('Ctrl Pts',(2.55565327734718,0.981143650373165,
13.7597120340895));
#448265=CARTESIAN_POINT('Ctrl Pts',(2.56705295344843,0.991556837913933,
13.7635825532445));
#448266=CARTESIAN_POINT('Ctrl Pts',(2.56178246121564,1.00561947734499,13.7651073818884));
#448267=CARTESIAN_POINT('Ctrl Pts',(2.5542402646995,0.979849317145748,13.7381884353898));
#448268=CARTESIAN_POINT('Ctrl Pts',(2.56537371634972,0.990018100995272,
13.7368803041982));
#448269=CARTESIAN_POINT('Ctrl Pts',(2.55981500470216,1.00409966205711,13.7363986145813));
#448270=CARTESIAN_POINT('Origin',(2.52429501445587,0.982253882249225,13.7902182540695));
#448271=CARTESIAN_POINT('Ctrl Pts',(2.51277790328901,0.94186935051894,13.8235227101244));
#448272=CARTESIAN_POINT('Ctrl Pts',(2.52125878487692,0.949631910393832,
13.8358800583119));
#448273=CARTESIAN_POINT('Ctrl Pts',(2.51244524948572,0.963665713975349,
13.8390832900376));
#448274=CARTESIAN_POINT('Ctrl Pts',(2.52157324423867,0.94992597058406,13.8124254819052));
#448275=CARTESIAN_POINT('Ctrl Pts',(2.53007059539059,0.957703605445395,
13.8247886449157));
#448276=CARTESIAN_POINT('Ctrl Pts',(2.52123148983817,0.971746076529041,
13.8279860620657));
#448277=CARTESIAN_POINT('Ctrl Pts',(2.53036464340266,0.957978979934154,
13.8013225099955));
#448278=CARTESIAN_POINT('Ctrl Pts',(2.53887445608688,0.965768018508477,
13.8136962257787));
#448279=CARTESIAN_POINT('Ctrl Pts',(2.53001384607715,0.979822498759896,
13.8168830918626));
#448280=CARTESIAN_POINT('Ctrl Pts',(2.53915225414983,0.966028519056621,
13.7902140179785));
#448281=CARTESIAN_POINT('Ctrl Pts',(2.54767078228692,0.973825530017369,
13.802602731458));
#448282=CARTESIAN_POINT('Ctrl Pts',(2.53879247206465,0.987895134138251,
13.8057746032558));
#448283=CARTESIAN_POINT('Origin',(2.49792065440358,0.958094705296493,13.8235269408515));
#448284=CARTESIAN_POINT('Ctrl Pts',(2.53435070432089,0.882188624381805,
13.8235269408515));
#448285=CARTESIAN_POINT('Ctrl Pts',(2.54614459076024,0.881622178050192,
13.8362179249168));
#448286=CARTESIAN_POINT('Ctrl Pts',(2.54809516572306,0.864655791830034,
13.8391868794938));
#448287=CARTESIAN_POINT('Ctrl Pts',(2.52355981158623,0.882706898119287,
13.8400110824519));
#448288=CARTESIAN_POINT('Ctrl Pts',(2.53285150606145,0.878835686856507,
13.8494522556837));
#448289=CARTESIAN_POINT('Ctrl Pts',(2.53034179279955,0.86562095164239,13.85569149686));
#448290=CARTESIAN_POINT('Ctrl Pts',(2.50903339505441,0.890081242075895,
13.8586819406588));
#448291=CARTESIAN_POINT('Ctrl Pts',(2.51052629600454,0.885991341051656,
13.868010383617));
#448292=CARTESIAN_POINT('Ctrl Pts',(2.50629374135306,0.87799269442146,13.8744918421245));
#448293=CARTESIAN_POINT('Ctrl Pts',(2.49834865421076,0.919490557114688,
13.8587686893867));
#448294=CARTESIAN_POINT('Ctrl Pts',(2.49686898717052,0.923544038750251,
13.8680909899357));
#448295=CARTESIAN_POINT('Ctrl Pts',(2.48850920386329,0.926951446058171,
13.8745789365163));
#448296=CARTESIAN_POINT('Ctrl Pts',(2.50480151728297,0.93456290033434,13.8400379222776));
#448297=CARTESIAN_POINT('Ctrl Pts',(2.50946394083728,0.943480974145899,
13.8494748685453));
#448298=CARTESIAN_POINT('Ctrl Pts',(2.49909130647347,0.952034894978994,
13.8557104837033));
#448299=CARTESIAN_POINT('Ctrl Pts',(2.51278080633127,0.94187200871438,13.8235269408542));
#448300=CARTESIAN_POINT('Ctrl Pts',(2.52148758766895,0.94984750728991,13.8362179249195));
#448301=CARTESIAN_POINT('Ctrl Pts',(2.51214073195049,0.964140837630829,
13.8391868794965));
#448302=CARTESIAN_POINT('Origin',(2.53329528709906,0.860213954998902,13.8235269408515));
#448303=CARTESIAN_POINT('Ctrl Pts',(2.57007250605579,0.880472947990599,
13.7902140241682));
#448304=CARTESIAN_POINT('Ctrl Pts',(2.58160752158498,0.879923391684029,
13.8026027327198));
#448305=CARTESIAN_POINT('Ctrl Pts',(2.5837753539635,0.863428591441144,13.8057746032556));
#448306=CARTESIAN_POINT('Ctrl Pts',(2.55816913106018,0.881044652928356,
13.8013225161807));
#448307=CARTESIAN_POINT('Ctrl Pts',(2.56969234802928,0.880495655142914,
13.8136962270464));
#448308=CARTESIAN_POINT('Ctrl Pts',(2.57186412217919,0.864023800288172,
13.8168830918628));
#448309=CARTESIAN_POINT('Ctrl Pts',(2.54626062441251,0.881616604333268,
13.8124254880876));
#448310=CARTESIAN_POINT('Ctrl Pts',(2.5577669686007,0.881068408689682,13.8247886461868));
#448311=CARTESIAN_POINT('Ctrl Pts',(2.55994760105066,0.86461953625668,13.8279860620656));
#448312=CARTESIAN_POINT('Ctrl Pts',(2.53434677836339,0.882188812183291,
13.8235227163065));
#448313=CARTESIAN_POINT('Ctrl Pts',(2.54583082072181,0.881641679341152,
13.8358800595847));
#448314=CARTESIAN_POINT('Ctrl Pts',(2.54802557414951,0.865215818992596,
13.8390832900376));
#448315=CARTESIAN_POINT('Origin',(2.56902102722067,0.85849809021251,13.7902182540695));
#448316=CARTESIAN_POINT('Ctrl Pts',(2.59051004735031,0.879491330346339,
13.7382347919292));
#448317=CARTESIAN_POINT('Ctrl Pts',(2.60558412847211,0.878791368156842,
13.7369371795943));
#448318=CARTESIAN_POINT('Ctrl Pts',(2.61030799135417,0.864395921081753,
13.7364597369711));
#448319=CARTESIAN_POINT('Ctrl Pts',(2.59239942805721,0.879400586041886,
13.7595490285574));
#448320=CARTESIAN_POINT('Ctrl Pts',(2.60783311719664,0.878682919012028,
13.7633824266925));
#448321=CARTESIAN_POINT('Ctrl Pts',(2.61276204814568,0.864484352182699,
13.7648920890506));
#448322=CARTESIAN_POINT('Ctrl Pts',(2.58276368996126,0.879863377031185,
13.7803806590111));
#448323=CARTESIAN_POINT('Ctrl Pts',(2.5961135294197,0.879248013367294,13.7901039518745));
#448324=CARTESIAN_POINT('Ctrl Pts',(2.60025086493429,0.864037231130171,
13.7926933640892));
#448325=CARTESIAN_POINT('Ctrl Pts',(2.56601462617966,0.880667811001527,
13.7936647693663));
#448326=CARTESIAN_POINT('Ctrl Pts',(2.57681899087517,0.88017889846247,13.8072068914933));
#448327=CARTESIAN_POINT('Ctrl Pts',(2.57854585859628,0.863218291229214,
13.8104111085397));
#448328=CARTESIAN_POINT('Origin',(2.58972418063935,0.857503742389414,13.7435492065112));
#448329=CARTESIAN_POINT('Origin',(2.58972418063935,0.857503742389415,14.));
#448330=CARTESIAN_POINT('Origin',(2.58972418063935,0.857503742389415,12.5369868989719));
#448331=CARTESIAN_POINT('Ctrl Pts',(2.59324345222295,0.895594198410246,
12.506462012331));
#448332=CARTESIAN_POINT('Ctrl Pts',(2.59942388090557,0.89772865133525,12.4999388158272));
#448333=CARTESIAN_POINT('Ctrl Pts',(2.59935075832912,0.897703397957985,
12.4907030323752));
#448334=CARTESIAN_POINT('Ctrl Pts',(2.59965522889214,0.883970184340286,
12.5042014951932));
#448335=CARTESIAN_POINT('Ctrl Pts',(2.60524363939895,0.88079044140674,12.4980716682126));
#448336=CARTESIAN_POINT('Ctrl Pts',(2.6074145173087,0.874355159413935,12.4907355092743));
#448337=CARTESIAN_POINT('Ctrl Pts',(2.59591946047918,0.879240518854148,
12.521804744651));
#448338=CARTESIAN_POINT('Ctrl Pts',(2.60709142493367,0.875405667988131,
12.5216906929435));
#448339=CARTESIAN_POINT('Ctrl Pts',(2.61067940057473,0.864203115371447,
12.5161988840776));
#448340=CARTESIAN_POINT('Ctrl Pts',(2.59074122437161,0.879480221225811,
12.5369868989719));
#448341=CARTESIAN_POINT('Ctrl Pts',(2.60605472464864,0.878771531740491,
12.5369868989719));
#448342=CARTESIAN_POINT('Ctrl Pts',(2.6106930131041,0.864160172743973,12.5369868989719));
#448343=CARTESIAN_POINT('Origin',(4.84514877968059E-31,-3.40079961985215E-31,
12.5));
#448344=CARTESIAN_POINT('Origin',(2.45401129869475,1.0858263246758,12.5));
#448345=CARTESIAN_POINT('',(2.45401129869475,1.0858263246758,12.5893111709658));
#448346=CARTESIAN_POINT('',(2.45401129869475,1.0858263246758,13.8235269408515));
#448347=CARTESIAN_POINT('',(2.45401129869475,1.0858263246758,12.5));
#448348=CARTESIAN_POINT('',(2.48975802327266,1.08702814876944,13.7902182540695));
#448349=CARTESIAN_POINT('',(2.45401129869475,1.0858263246758,13.8235269408515));
#448350=CARTESIAN_POINT('',(2.51047333723489,1.08772460875902,13.7435492065112));
#448351=CARTESIAN_POINT('Origin',(2.4423202171704,1.08543359017029,13.7445212918704));
#448352=CARTESIAN_POINT('',(2.51047333723489,1.08772460875902,12.5369868989719));
#448353=CARTESIAN_POINT('',(2.51047333723489,1.08772460875902,12.5));
#448354=CARTESIAN_POINT('Ctrl Pts',(2.51047333723489,1.08772460875902,12.5369868989719));
#448355=CARTESIAN_POINT('Ctrl Pts',(2.49166638438045,1.0870923088956,12.5544431401645));
#448356=CARTESIAN_POINT('Ctrl Pts',(2.47284598029346,1.08645955679451,12.5718848856037));
#448357=CARTESIAN_POINT('Ctrl Pts',(2.45401129869475,1.0858263246758,12.5893111709658));
#448358=CARTESIAN_POINT('Origin',(2.61461687993057,1.34521555026705,12.5));
#448359=CARTESIAN_POINT('',(2.46605782225597,1.18498102042076,13.7435492065112));
#448360=CARTESIAN_POINT('',(2.45196582721007,1.16978151501113,13.7902182540695));
#448361=CARTESIAN_POINT('Origin',(2.41493449982007,1.12983984180181,13.7418732680468));
#448362=CARTESIAN_POINT('',(2.42764842286963,1.14355297053484,13.8235269408515));
#448363=CARTESIAN_POINT('',(2.45196582721007,1.16978151501113,13.7902182540695));
#448364=CARTESIAN_POINT('',(2.42764842286963,1.14355297053484,12.5893111709658));
#448365=CARTESIAN_POINT('',(2.42764842286963,1.14355297053484,12.5));
#448366=CARTESIAN_POINT('',(2.46605782225597,1.18498102042076,12.5369868989719));
#448367=CARTESIAN_POINT('Ctrl Pts',(2.42764842286963,1.14355297053484,12.5893111709658));
#448368=CARTESIAN_POINT('Ctrl Pts',(2.44046108118917,1.15737259428616,12.5718848856037));
#448369=CARTESIAN_POINT('Ctrl Pts',(2.45326402695379,1.17118174215875,12.5544431401645));
#448370=CARTESIAN_POINT('Ctrl Pts',(2.46605782225597,1.18498102042076,12.5369868989719));
#448371=CARTESIAN_POINT('',(2.46605782225597,1.18498102042076,12.5));
#448372=CARTESIAN_POINT('Origin',(2.45285624533615,1.12018191340222,12.5));
#448373=CARTESIAN_POINT('',(2.42206997748234,1.10489152806335,13.8587068136939));
#448374=CARTESIAN_POINT('Ctrl Pts',(2.42764842286468,1.14355297053923,13.8235269408542));
#448375=CARTESIAN_POINT('Ctrl Pts',(2.42645706099368,1.14226797780794,13.8262006681044));
#448376=CARTESIAN_POINT('Ctrl Pts',(2.42536528244755,1.14083485267795,13.8288634856214));
#448377=CARTESIAN_POINT('Ctrl Pts',(2.42436690471821,1.13926540965906,13.8314912288862));
#448378=CARTESIAN_POINT('Ctrl Pts',(2.42333768025715,1.13764747578712,13.834200161153));
#448379=CARTESIAN_POINT('Ctrl Pts',(2.42240615489842,1.13588313987818,13.8368750301949));
#448380=CARTESIAN_POINT('Ctrl Pts',(2.42158932736391,1.13394690076675,13.8394886372968));
#448381=CARTESIAN_POINT('Ctrl Pts',(2.42152624179207,1.13379736032351,13.8396904925131));
#448382=CARTESIAN_POINT('Ctrl Pts',(2.42146385899365,1.1336467825078,13.8398919674349));
#448383=CARTESIAN_POINT('Ctrl Pts',(2.42140219692688,1.13349515024217,13.8400930404591));
#448384=CARTESIAN_POINT('Ctrl Pts',(2.42044146044229,1.13113261753052,13.8432258934518));
#448385=CARTESIAN_POINT('Ctrl Pts',(2.41965954656088,1.12852658845066,13.8462331177034));
#448386=CARTESIAN_POINT('Ctrl Pts',(2.41917435403413,1.12573433484191,13.8489036603661));
#448387=CARTESIAN_POINT('Ctrl Pts',(2.41901559339291,1.12482067696604,13.8497774930041));
#448388=CARTESIAN_POINT('Ctrl Pts',(2.4188887726382,1.12388726308532,13.85061494757));
#448389=CARTESIAN_POINT('Ctrl Pts',(2.41879850091015,1.12293662922273,13.8514076489583));
#448390=CARTESIAN_POINT('Ctrl Pts',(2.41860756318619,1.12092590150143,13.8530843267192));
#448391=CARTESIAN_POINT('Ctrl Pts',(2.41856432936575,1.11864034840778,13.8546805203176));
#448392=CARTESIAN_POINT('Ctrl Pts',(2.4188077300259,1.11621004205749,13.8559412814274));
#448393=CARTESIAN_POINT('Ctrl Pts',(2.4188403049279,1.11588478825113,13.8561100121513));
#448394=CARTESIAN_POINT('Ctrl Pts',(2.41887795059011,1.11555698544893,13.8562727473908));
#448395=CARTESIAN_POINT('Ctrl Pts',(2.41892093274999,1.11522698044344,13.8564289040185));
#448396=CARTESIAN_POINT('Ctrl Pts',(2.4191158563547,1.11373041150834,13.8571370725437));
#448397=CARTESIAN_POINT('Ctrl Pts',(2.41942621459317,1.11216254030716,13.8577210840554));
#448398=CARTESIAN_POINT('Ctrl Pts',(2.41986873320903,1.11059000910466,13.8581177131616));
#448399=CARTESIAN_POINT('Ctrl Pts',(2.41999336168228,1.11014713019316,13.8582294175695));
#448400=CARTESIAN_POINT('Ctrl Pts',(2.42012829576111,1.10970386797704,13.8583265086086));
#448401=CARTESIAN_POINT('Ctrl Pts',(2.42027347360095,1.10926165119297,13.8584082369006));
#448402=CARTESIAN_POINT('Ctrl Pts',(2.42048205522583,1.10862630425939,13.8585256585398));
#448403=CARTESIAN_POINT('Ctrl Pts',(2.42071468237932,1.10798531730301,13.8586122832068));
#448404=CARTESIAN_POINT('Ctrl Pts',(2.42096605439541,1.10735561070772,13.8586682984299));
#448405=CARTESIAN_POINT('Ctrl Pts',(2.42116712709058,1.1068519078523,13.8587131050557));
#448406=CARTESIAN_POINT('Ctrl Pts',(2.42138219660225,1.10634977230495,13.8587357943552));
#448407=CARTESIAN_POINT('Ctrl Pts',(2.42161175402798,1.1058493437941,13.8587355499465));
#448408=CARTESIAN_POINT('Ctrl Pts',(2.42176012246511,1.10552590491679,13.8587353919793));
#448409=CARTESIAN_POINT('Ctrl Pts',(2.42191290341701,1.10520666062785,13.8587257282814));
#448410=CARTESIAN_POINT('Ctrl Pts',(2.42206997748234,1.10489152806335,13.8587068136939));
#448411=CARTESIAN_POINT('Ctrl Pts',(2.42206997748234,1.10489152806335,13.8587068136939));
#448412=CARTESIAN_POINT('Ctrl Pts',(2.42258658552026,1.10385507423829,13.8586446046466));
#448413=CARTESIAN_POINT('Ctrl Pts',(2.42314957595238,1.10286304208167,13.858482427929));
#448414=CARTESIAN_POINT('Ctrl Pts',(2.42375522096753,1.1019129639264,13.8582284286032));
#448415=CARTESIAN_POINT('Ctrl Pts',(2.42437654230153,1.10093829425675,13.8579678548414));
#448416=CARTESIAN_POINT('Ctrl Pts',(2.42504556417679,1.10000622101151,13.857615680862));
#448417=CARTESIAN_POINT('Ctrl Pts',(2.42572803911843,1.09914784029088,13.8571944833187));
#448418=CARTESIAN_POINT('Ctrl Pts',(2.42743122513308,1.09700566341456,13.8561433417727));
#448419=CARTESIAN_POINT('Ctrl Pts',(2.42929411337666,1.09521925713392,13.8546163505474));
#448420=CARTESIAN_POINT('Ctrl Pts',(2.43111074893032,1.09377017048553,13.8528973491086));
#448421=CARTESIAN_POINT('Ctrl Pts',(2.43144262144402,1.09350544373414,13.8525833129072));
#448422=CARTESIAN_POINT('Ctrl Pts',(2.43177292319813,1.09325183595566,13.8522628768812));
#448423=CARTESIAN_POINT('Ctrl Pts',(2.43210039201653,1.09300905596031,13.851937733538));
#448424=CARTESIAN_POINT('Ctrl Pts',(2.43410019865623,1.09152643221291,13.8499521282529));
#448425=CARTESIAN_POINT('Ctrl Pts',(2.43619552649437,1.09030354834289,13.847639871647));
#448426=CARTESIAN_POINT('Ctrl Pts',(2.43823575644318,1.08933528679105,13.8452109780794));
#448427=CARTESIAN_POINT('Ctrl Pts',(2.43915369812781,1.08889964587687,13.8441181685877));
#448428=CARTESIAN_POINT('Ctrl Pts',(2.44006042192786,1.08851483294368,13.8430021611332));
#448429=CARTESIAN_POINT('Ctrl Pts',(2.4409429470759,1.08817715631235,13.8418824960098));
#448430=CARTESIAN_POINT('Ctrl Pts',(2.44302264012336,1.08738141270774,13.8392439765549));
#448431=CARTESIAN_POINT('Ctrl Pts',(2.44506601942868,1.08680585456423,13.8364981347964));
#448432=CARTESIAN_POINT('Ctrl Pts',(2.44706921107542,1.0864160209339,13.8336931113419));
#448433=CARTESIAN_POINT('Ctrl Pts',(2.4490201925249,1.08603634773468,13.8309611966328));
#448434=CARTESIAN_POINT('Ctrl Pts',(2.4509351167424,1.08583301751496,13.8281701127186));
#448435=CARTESIAN_POINT('Ctrl Pts',(2.45280336318841,1.08581285823271,13.8253580685121));
#448436=CARTESIAN_POINT('Ctrl Pts',(2.45320840103418,1.08580848767856,13.8247484142933));
#448437=CARTESIAN_POINT('Ctrl Pts',(2.45361114990772,1.08581287145851,13.8241378483365));
#448438=CARTESIAN_POINT('Ctrl Pts',(2.45401129869475,1.0858263246758,13.8235269408515));
#448439=CARTESIAN_POINT('',(2.42153762191903,1.10601374658571,12.5969504640361));
#448440=CARTESIAN_POINT('Origin',(2.45288642222602,1.12019547946754,12.584524458991));
#448441=CARTESIAN_POINT('Origin',(2.45288642222602,1.12019547946754,12.584524458991));
#448442=CARTESIAN_POINT('Ctrl Pts',(2.42764842286963,1.14355297053484,12.5893111709658));
#448443=CARTESIAN_POINT('Ctrl Pts',(2.41994263053449,1.13524156878499,12.5770542771492));
#448444=CARTESIAN_POINT('Ctrl Pts',(2.42965842765955,1.12207316109538,12.5737548217797));
#448445=CARTESIAN_POINT('Ctrl Pts',(2.4444984045658,1.16172721677244,12.5663937883685));
#448446=CARTESIAN_POINT('Ctrl Pts',(2.43678278242238,1.1534052126754,12.5540940315304));
#448447=CARTESIAN_POINT('Ctrl Pts',(2.44653127082073,1.14019790525636,12.5508374392248));
#448448=CARTESIAN_POINT('Ctrl Pts',(2.46133138483701,1.1798831254184,12.5434499600945));
#448449=CARTESIAN_POINT('Ctrl Pts',(2.45359067645838,1.17153406352246,12.5311293540533));
#448450=CARTESIAN_POINT('Ctrl Pts',(2.46338676527167,1.15830574509102,12.5278936106989));
#448451=CARTESIAN_POINT('Ctrl Pts',(2.47814869542813,1.19802213288134,12.5204817579905));
#448452=CARTESIAN_POINT('Ctrl Pts',(2.47036967583308,1.18963174883482,12.5081597038247));
#448453=CARTESIAN_POINT('Ctrl Pts',(2.48022624928162,1.17639800390951,12.5049254088044));
#448454=CARTESIAN_POINT('Ctrl Pts',(2.46605782225597,1.18498102042076,12.5369868989719));
#448455=CARTESIAN_POINT('Ctrl Pts',(2.46669113878569,1.18566410997851,12.5342545179733));
#448456=CARTESIAN_POINT('Ctrl Pts',(2.46738702577367,1.18623120645471,12.5314872231885));
#448457=CARTESIAN_POINT('Ctrl Pts',(2.46814159680487,1.18660703044145,12.5287124745063));
#448458=CARTESIAN_POINT('Ctrl Pts',(2.46882210641437,1.18694596716693,12.5262100684184));
#448459=CARTESIAN_POINT('Ctrl Pts',(2.46955009758189,1.18712811325593,12.5237004536639));
#448460=CARTESIAN_POINT('Ctrl Pts',(2.47035416046659,1.18709228800123,12.5212220730815));
#448461=CARTESIAN_POINT('Ctrl Pts',(2.47096974016182,1.18706486066964,12.5193246583486));
#448462=CARTESIAN_POINT('Ctrl Pts',(2.47163723602436,1.18690871363447,12.517417831369));
#448463=CARTESIAN_POINT('Ctrl Pts',(2.47235361687581,1.18652666235626,12.5155812248347));
#448464=CARTESIAN_POINT('Ctrl Pts',(2.47265879896908,1.18636390645821,12.5147988205793));
#448465=CARTESIAN_POINT('Ctrl Pts',(2.47297329290029,1.18616023254245,12.5140295443047));
#448466=CARTESIAN_POINT('Ctrl Pts',(2.47329874923813,1.18590911319832,12.5132817086137));
#448467=CARTESIAN_POINT('Ctrl Pts',(2.4737912833787,1.18552907804163,12.5121499604604));
#448468=CARTESIAN_POINT('Ctrl Pts',(2.47431519146879,1.1850265112003,12.5110494206568));
#448469=CARTESIAN_POINT('Ctrl Pts',(2.47485471189822,1.18436767144746,12.5100666561695));
#448470=CARTESIAN_POINT('Ctrl Pts',(2.47516450328639,1.18398936717855,12.5095023550641));
#448471=CARTESIAN_POINT('Ctrl Pts',(2.47548251644376,1.18355475474528,12.5089719619137));
#448472=CARTESIAN_POINT('Ctrl Pts',(2.47579763610277,1.18306820887133,12.5085043804652));
#448473=CARTESIAN_POINT('Ctrl Pts',(2.47625877267651,1.18235621236187,12.5078201359221));
#448474=CARTESIAN_POINT('Ctrl Pts',(2.47672607371854,1.18151169608092,12.5072563000949));
#448475=CARTESIAN_POINT('Ctrl Pts',(2.47716045552645,1.18058780689311,12.5068768744332));
#448476=CARTESIAN_POINT('Ctrl Pts',(2.47747367471289,1.17992161918795,12.5066032824114));
#448477=CARTESIAN_POINT('Ctrl Pts',(2.47777533500291,1.17920248395026,12.5064197834844));
#448478=CARTESIAN_POINT('Ctrl Pts',(2.47805097454076,1.17847155943811,12.5063282718343));
#448479=CARTESIAN_POINT('Ctrl Pts',(2.47845332293017,1.17740463593888,12.5061946931565));
#448480=CARTESIAN_POINT('Ctrl Pts',(2.47880982259354,1.1762901636557,12.5062515701262));
#448481=CARTESIAN_POINT('Ctrl Pts',(2.47911307783089,1.17520202033805,12.5064436508398));
#448482=CARTESIAN_POINT('',(2.42965842765955,1.12207316109538,12.5737548217797));
#448483=CARTESIAN_POINT('Origin',(2.4437814292482,1.12859549396996,12.5893111709658));
#448484=CARTESIAN_POINT('Ctrl Pts',(2.47911307783089,1.17520202033805,12.5064436508398));
#448485=CARTESIAN_POINT('Ctrl Pts',(2.47179285640968,1.16733724150482,12.5164271754438));
#448486=CARTESIAN_POINT('Ctrl Pts',(2.4644695803147,1.15946948742519,12.5264061185523));
#448487=CARTESIAN_POINT('Ctrl Pts',(2.45714314265571,1.15159865266862,12.536380305637));
#448488=CARTESIAN_POINT('Ctrl Pts',(2.44798658154365,1.14176170560022,12.5488460165097));
#448489=CARTESIAN_POINT('Ctrl Pts',(2.43882507936809,1.1319199436467,12.5613043021964));
#448490=CARTESIAN_POINT('Ctrl Pts',(2.42965842765955,1.12207316109538,12.5737548217797));
#448491=CARTESIAN_POINT('Ctrl Pts',(2.45401129869475,1.0858263246758,12.5893111709658));
#448492=CARTESIAN_POINT('Ctrl Pts',(2.44268373953579,1.08544548604849,12.5770542771492));
#448493=CARTESIAN_POINT('Ctrl Pts',(2.43909421506563,1.10141166871477,12.5737548217797));
#448494=CARTESIAN_POINT('Ctrl Pts',(2.44344278452135,1.08547100554888,12.5928319619712));
#448495=CARTESIAN_POINT('Ctrl Pts',(2.43572049983066,1.08847096146978,12.5821634970843));
#448496=CARTESIAN_POINT('Ctrl Pts',(2.43524467832255,1.1012728010326,12.5773203894503));
#448497=CARTESIAN_POINT('Ctrl Pts',(2.42799259915257,1.09194216243231,12.5969440695591));
#448498=CARTESIAN_POINT('Ctrl Pts',(2.42630612126106,1.09559104375038,12.5878292599214));
#448499=CARTESIAN_POINT('Ctrl Pts',(2.42973870739431,1.10358114052992,12.5813877129824));
#448500=CARTESIAN_POINT('Ctrl Pts',(2.41523312262583,1.11975171122953,12.596957478804));
#448501=CARTESIAN_POINT('Ctrl Pts',(2.41690720975602,1.11612982975308,12.5878468778671));
#448502=CARTESIAN_POINT('Ctrl Pts',(2.42517733555884,1.11353705110017,12.5814011370086));
#448503=CARTESIAN_POINT('Ctrl Pts',(2.42044854659189,1.13578724552042,12.5928371701607));
#448504=CARTESIAN_POINT('Ctrl Pts',(2.41766644601505,1.12799013181828,12.5821692192952));
#448505=CARTESIAN_POINT('Ctrl Pts',(2.42702398450034,1.11924597402784,12.5773318885715));
#448506=CARTESIAN_POINT('Ctrl Pts',(2.42764842286958,1.14355297053488,12.5893111709658));
#448507=CARTESIAN_POINT('Ctrl Pts',(2.41994263053445,1.13524156878502,12.5770542771492));
#448508=CARTESIAN_POINT('Ctrl Pts',(2.42965842765951,1.12207316109542,12.5737548217797));
#448509=CARTESIAN_POINT('',(2.43909421506563,1.10141166871477,12.5737548217797));
#448510=CARTESIAN_POINT('Origin',(2.45327206454525,1.10781390146071,12.5893111709658));
#448511=CARTESIAN_POINT('Ctrl Pts',(2.42965842765951,1.12207316109542,12.5737548217797));
#448512=CARTESIAN_POINT('Ctrl Pts',(2.4289534687874,1.1213608742012,12.5746934679442));
#448513=CARTESIAN_POINT('Ctrl Pts',(2.42830358372026,1.12044382194655,12.5756680099006));
#448514=CARTESIAN_POINT('Ctrl Pts',(2.42777999398454,1.11942826423936,12.5765688348656));
#448515=CARTESIAN_POINT('Ctrl Pts',(2.42764137939834,1.11915940657898,12.5768073183026));
#448516=CARTESIAN_POINT('Ctrl Pts',(2.42751142348116,1.1188838148705,12.5770407398754));
#448517=CARTESIAN_POINT('Ctrl Pts',(2.42739094509012,1.11860371470951,12.5772674179684));
#448518=CARTESIAN_POINT('Ctrl Pts',(2.42689653435202,1.11745425939102,12.5781976435658));
#448519=CARTESIAN_POINT('Ctrl Pts',(2.42654401154365,1.11615913578597,12.5790594849312));
#448520=CARTESIAN_POINT('Ctrl Pts',(2.426403773541,1.11479311015434,12.5797571720116));
#448521=CARTESIAN_POINT('Ctrl Pts',(2.42631240343977,1.11390309533742,12.580211740231));
#448522=CARTESIAN_POINT('Ctrl Pts',(2.42632567046707,1.1129406188617,12.5806009430798));
#448523=CARTESIAN_POINT('Ctrl Pts',(2.42646035569495,1.11197367907365,12.5808812374708));
#448524=CARTESIAN_POINT('Ctrl Pts',(2.42657609498706,1.11114275701678,12.5811221033394));
#448525=CARTESIAN_POINT('Ctrl Pts',(2.42678397820911,1.11029154357781,12.581287365893));
#448526=CARTESIAN_POINT('Ctrl Pts',(2.42708037202315,1.10947006077796,12.581359338449));
#448527=CARTESIAN_POINT('Ctrl Pts',(2.427121564643,1.10935589163175,12.5813693411482));
#448528=CARTESIAN_POINT('Ctrl Pts',(2.42716442053753,1.10924225880875,12.5813775999465));
#448529=CARTESIAN_POINT('Ctrl Pts',(2.42720888318565,1.10912925689458,12.5813841266931));
#448530=CARTESIAN_POINT('Ctrl Pts',(2.42728431944584,1.10893753547988,12.5813952001081));
#448531=CARTESIAN_POINT('Ctrl Pts',(2.42736545260864,1.10874656902732,12.5814007534795));
#448532=CARTESIAN_POINT('Ctrl Pts',(2.42745242884562,1.10855651782356,12.5814005856065));
#448533=CARTESIAN_POINT('Ctrl Pts',(2.42785057205302,1.107686537718,12.5813998171494));
#448534=CARTESIAN_POINT('Ctrl Pts',(2.42834333845804,1.10689570469468,12.58127954464));
#448535=CARTESIAN_POINT('Ctrl Pts',(2.42890281728343,1.10617286062362,12.5810700125799));
#448536=CARTESIAN_POINT('Ctrl Pts',(2.42957860400273,1.10529974728816,12.5808169217085));
#448537=CARTESIAN_POINT('Ctrl Pts',(2.43036501932016,1.10453599385415,12.5804173076348));
#448538=CARTESIAN_POINT('Ctrl Pts',(2.43117499953934,1.10392985244145,12.5799304713245));
#448539=CARTESIAN_POINT('Ctrl Pts',(2.43217882020099,1.10317865227688,12.5793271277669));
#448540=CARTESIAN_POINT('Ctrl Pts',(2.43326181024863,1.10259714959837,12.5785808224116));
#448541=CARTESIAN_POINT('Ctrl Pts',(2.43436331554294,1.10218191237749,12.5777485681082));
#448542=CARTESIAN_POINT('Ctrl Pts',(2.43600467911038,1.10156316342575,12.576508418016));
#448543=CARTESIAN_POINT('Ctrl Pts',(2.43767090966464,1.10131237416998,12.5750928681475));
#448544=CARTESIAN_POINT('Ctrl Pts',(2.43909421506563,1.10141166871477,12.5737548217797));
#448545=CARTESIAN_POINT('Ctrl Pts',(2.43909421506563,1.10141166871477,12.5737548217797));
#448546=CARTESIAN_POINT('Ctrl Pts',(2.44268373953579,1.08544548604849,12.5770542771492));
#448547=CARTESIAN_POINT('Ctrl Pts',(2.45401129869475,1.0858263246758,12.5893111709658));
#448548=CARTESIAN_POINT('Ctrl Pts',(2.46383762734287,1.1022939969124,12.5508408821982));
#448549=CARTESIAN_POINT('Ctrl Pts',(2.46743513747504,1.08627764135071,12.55409748406));
#448550=CARTESIAN_POINT('Ctrl Pts',(2.47877714769835,1.08665896583058,12.5663972313419));
#448551=CARTESIAN_POINT('Ctrl Pts',(2.48855691045729,1.10317428442276,12.52790050457));
#448552=CARTESIAN_POINT('Ctrl Pts',(2.49213913059592,1.0871082028775,12.5311362602938));
#448553=CARTESIAN_POINT('Ctrl Pts',(2.50351801202985,1.08749076698724,12.5434568539655));
#448554=CARTESIAN_POINT('Ctrl Pts',(2.51325394004799,1.10405267599415,12.5049357605811));
#448555=CARTESIAN_POINT('Ctrl Pts',(2.51680066060845,1.08793733677168,12.5081700652078));
#448556=CARTESIAN_POINT('Ctrl Pts',(2.52823584849389,1.08832179393463,12.5204921097672));
#448557=CARTESIAN_POINT('Ctrl Pts',(2.51163223633209,1.10399499577426,12.5064436508395));
#448558=CARTESIAN_POINT('Ctrl Pts',(2.5123060249568,1.10297771671726,12.5062361689309));
#448559=CARTESIAN_POINT('Ctrl Pts',(2.51296333095002,1.10189109790107,12.5061871075061));
#448560=CARTESIAN_POINT('Ctrl Pts',(2.51353944025899,1.10080522741835,12.5063648335164));
#448561=CARTESIAN_POINT('Ctrl Pts',(2.51380114464302,1.10031195806583,12.5064455676329));
#448562=CARTESIAN_POINT('Ctrl Pts',(2.51404954940513,1.09981185979765,12.506574497099));
#448563=CARTESIAN_POINT('Ctrl Pts',(2.51427306246193,1.0993259078063,12.5067492519495));
#448564=CARTESIAN_POINT('Ctrl Pts',(2.5147222206257,1.09834936841645,12.5071004286051));
#448565=CARTESIAN_POINT('Ctrl Pts',(2.51508663965537,1.09739371359238,12.5076537929612));
#448566=CARTESIAN_POINT('Ctrl Pts',(2.51534780568653,1.09653404031118,12.5083435010503));
#448567=CARTESIAN_POINT('Ctrl Pts',(2.51536424764895,1.0964799187406,12.5083869222963));
#448568=CARTESIAN_POINT('Ctrl Pts',(2.51538027074628,1.09642616821722,12.5084308732336));
#448569=CARTESIAN_POINT('Ctrl Pts',(2.51539586671482,1.09637280338018,12.5084753333615));
#448570=CARTESIAN_POINT('Ctrl Pts',(2.51552096696711,1.09594474695267,12.508831962269));
#448571=CARTESIAN_POINT('Ctrl Pts',(2.51562236310778,1.09553317783142,12.509227847131));
#448572=CARTESIAN_POINT('Ctrl Pts',(2.51569975886115,1.09515100391834,12.5096423454524));
#448573=CARTESIAN_POINT('Ctrl Pts',(2.51594228289828,1.09395344001786,12.5109411997424));
#448574=CARTESIAN_POINT('Ctrl Pts',(2.51597353579324,1.09297277425104,12.5124831113042));
#448575=CARTESIAN_POINT('Ctrl Pts',(2.51588134536736,1.0921737627362,12.5140723025008));
#448576=CARTESIAN_POINT('Ctrl Pts',(2.51587270702348,1.09209889448212,12.5142212114565));
#448577=CARTESIAN_POINT('Ctrl Pts',(2.51586300670766,1.09202560115064,12.5143705582413));
#448578=CARTESIAN_POINT('Ctrl Pts',(2.51585233019747,1.09195384347404,12.5145201959299));
#448579=CARTESIAN_POINT('Ctrl Pts',(2.51571517452833,1.09103200928206,12.5164425148273));
#448580=CARTESIAN_POINT('Ctrl Pts',(2.51542283714769,1.09033044201141,12.5184635205941));
#448581=CARTESIAN_POINT('Ctrl Pts',(2.515029354695,1.08977690579741,12.5205025929158));
#448582=CARTESIAN_POINT('Ctrl Pts',(2.51480111927626,1.08945583285316,12.5216853356836));
#448583=CARTESIAN_POINT('Ctrl Pts',(2.51453966041455,1.08918486418674,12.5228750347131));
#448584=CARTESIAN_POINT('Ctrl Pts',(2.51426005320379,1.0889537199542,12.5240609649613));
#448585=CARTESIAN_POINT('Ctrl Pts',(2.51357377230539,1.08838638883587,12.5269717671326));
#448586=CARTESIAN_POINT('Ctrl Pts',(2.51275222181068,1.08805101773871,12.5299036066168));
#448587=CARTESIAN_POINT('Ctrl Pts',(2.51184062668424,1.08787368626492,12.5328133004019));
#448588=CARTESIAN_POINT('Ctrl Pts',(2.51140300794295,1.08778855683181,12.5342101228451));
#448589=CARTESIAN_POINT('Ctrl Pts',(2.51094508383591,1.08774046921529,12.5356023438238));
#448590=CARTESIAN_POINT('Ctrl Pts',(2.51047333723489,1.08772460875902,12.5369868989719));
#448591=CARTESIAN_POINT('Origin',(15.2493479500663,1.51071161473945,-1.2406553367009));
#448592=CARTESIAN_POINT('Ctrl Pts',(2.46602937784755,1.18495039891586,12.5369868989719));
#448593=CARTESIAN_POINT('Ctrl Pts',(2.47647945267177,1.19617890014503,12.5369868989719));
#448594=CARTESIAN_POINT('Ctrl Pts',(2.4695570606498,1.20986698957999,12.5369868989719));
#448595=CARTESIAN_POINT('Ctrl Pts',(2.46956186336931,1.18874611658407,12.5218025310016));
#448596=CARTESIAN_POINT('Ctrl Pts',(2.47486155570973,1.19930874527211,12.5216901060418));
#448597=CARTESIAN_POINT('Ctrl Pts',(2.46957817711163,1.20982527118971,12.5161920673678));
#448598=CARTESIAN_POINT('Ctrl Pts',(2.47554149986159,1.18798452705193,12.5042015548895));
#448599=CARTESIAN_POINT('Ctrl Pts',(2.47730769068085,1.19416982534763,12.4980677368514));
#448600=CARTESIAN_POINT('Ctrl Pts',(2.47435102818041,1.20028937815663,12.4907278922776));
#448601=CARTESIAN_POINT('Ctrl Pts',(2.47909500459789,1.17519345286739,12.506463626192));
#448602=CARTESIAN_POINT('Ctrl Pts',(2.48500710868774,1.17799603445712,12.4999376786891));
#448603=CARTESIAN_POINT('Ctrl Pts',(2.48493490093248,1.17796180499795,12.4906970594712));
#448604=CARTESIAN_POINT('Origin',(2.44992481587739,1.19993849698564,12.5369868989719));
#448605=CARTESIAN_POINT('Origin',(2.44992481587739,1.19993849698564,14.));
#448606=CARTESIAN_POINT('Origin',(2.44992481587739,1.19993849698564,13.7435492065112));
#448607=CARTESIAN_POINT('Ctrl Pts',(2.44922377166514,1.16682399727264,13.793642941384));
#448608=CARTESIAN_POINT('Ctrl Pts',(2.45659484668155,1.17473433684236,13.8071662555867));
#448609=CARTESIAN_POINT('Ctrl Pts',(2.4459779900371,1.18804980674117,13.8103758687955));
#448610=CARTESIAN_POINT('Ctrl Pts',(2.46052423051409,1.1790125712264,13.7804579775006));
#448611=CARTESIAN_POINT('Ctrl Pts',(2.46961205178888,1.18878012855701,13.7901904343351));
#448612=CARTESIAN_POINT('Ctrl Pts',(2.46191196247133,1.20252656622885,13.7927914348263));
#448613=CARTESIAN_POINT('Ctrl Pts',(2.46717723589469,1.18618844344647,13.7597120340895));
#448614=CARTESIAN_POINT('Ctrl Pts',(2.47769020905823,1.19749616139639,13.7635825532445));
#448615=CARTESIAN_POINT('Ctrl Pts',(2.47129101828876,1.211082414509,13.7651073818884));
#448616=CARTESIAN_POINT('Ctrl Pts',(2.46587442510408,1.18478324335754,13.7381884353898));
#448617=CARTESIAN_POINT('Ctrl Pts',(2.47614198082626,1.19582567108509,13.7368803041982));
#448618=CARTESIAN_POINT('Ctrl Pts',(2.46945398737976,1.2094072903103,13.7363986145813));
#448619=CARTESIAN_POINT('Origin',(2.4358328208315,1.184738991576,13.7902182540695));
#448620=CARTESIAN_POINT('Ctrl Pts',(2.42764574614966,1.14355008456382,13.8235227101244));
#448621=CARTESIAN_POINT('Ctrl Pts',(2.43546568760982,1.15197808574317,13.8358800583119));
#448622=CARTESIAN_POINT('Ctrl Pts',(2.4255375932552,1.16524680804573,13.8390832900376));
#448623=CARTESIAN_POINT('Ctrl Pts',(2.43575513199856,1.15229679882965,13.8124254819053));
#448624=CARTESIAN_POINT('Ctrl Pts',(2.44359025947028,1.16074116725703,13.8247886449157));
#448625=CARTESIAN_POINT('Ctrl Pts',(2.43363597355513,1.17401644401579,13.8279860620657));
#448626=CARTESIAN_POINT('Ctrl Pts',(2.44386088348455,1.1610395931027,13.8013225099955));
#448627=CARTESIAN_POINT('Ctrl Pts',(2.45170750151535,1.16949634302873,13.8136962257787));
#448628=CARTESIAN_POINT('Ctrl Pts',(2.44173080383857,1.18278183618285,13.8168830918626));
#448629=CARTESIAN_POINT('Ctrl Pts',(2.45196314201513,1.16977861990387,13.7902140179785));
#448630=CARTESIAN_POINT('Ctrl Pts',(2.45981779667535,1.17824402607918,13.802602731458));
#448631=CARTESIAN_POINT('Ctrl Pts',(2.44982222494626,1.19154315004769,13.8057746032558));
#448632=CARTESIAN_POINT('Origin',(2.41151541649105,1.15851044709972,13.8235269408515));
#448633=CARTESIAN_POINT('Ctrl Pts',(2.45401129869475,1.0858263246758,13.8235269408515));
#448634=CARTESIAN_POINT('Ctrl Pts',(2.46581211258456,1.08622307438154,13.8362179249168));
#448635=CARTESIAN_POINT('Ctrl Pts',(2.46913911515529,1.06947213237963,13.8391868794938));
#448636=CARTESIAN_POINT('Ctrl Pts',(2.4432140676444,1.08546331596454,13.8400110824519));
#448637=CARTESIAN_POINT('Ctrl Pts',(2.45279038442927,1.08236234519754,13.8494522556837));
#448638=CARTESIAN_POINT('Ctrl Pts',(2.45136614563081,1.0689870159948,13.85569149686));
#448639=CARTESIAN_POINT('Ctrl Pts',(2.42813490907277,1.09162908459596,13.8586819406588));
#448640=CARTESIAN_POINT('Ctrl Pts',(2.42995620742041,1.08767447766684,13.868010383617));
#448641=CARTESIAN_POINT('Ctrl Pts',(2.42638970020154,1.07935745337625,13.8744918421245));
#448642=CARTESIAN_POINT('Ctrl Pts',(2.41508858862442,1.12006963699401,13.8587686893867));
#448643=CARTESIAN_POINT('Ctrl Pts',(2.4132834486702,1.12398902440348,13.8680909899357));
#448644=CARTESIAN_POINT('Ctrl Pts',(2.40467374652388,1.1267036938967,13.8745789365163));
#448645=CARTESIAN_POINT('Ctrl Pts',(2.42029144442988,1.13561779648083,13.8400379222776));
#448646=CARTESIAN_POINT('Ctrl Pts',(2.42421144834743,1.14488622694096,13.8494748685453));
#448647=CARTESIAN_POINT('Ctrl Pts',(2.41317610411016,1.15256621931266,13.8557104837033));
#448648=CARTESIAN_POINT('Ctrl Pts',(2.42764842286468,1.14355297053923,13.8235269408542));
#448649=CARTESIAN_POINT('Ctrl Pts',(2.4356761559309,1.15221161481001,13.8362179249195));
#448650=CARTESIAN_POINT('Ctrl Pts',(2.4251953619882,1.16569552976031,13.8391868794965));
#448651=CARTESIAN_POINT('Origin',(2.45475053284425,1.0638387478909,13.8235269408515));
#448652=CARTESIAN_POINT('Ctrl Pts',(2.48975408263468,1.08702801552268,13.7902140241683));
#448653=CARTESIAN_POINT('Ctrl Pts',(2.50129551029208,1.08742049867086,13.8026027327198));
#448654=CARTESIAN_POINT('Ctrl Pts',(2.50480060873724,1.07115728197909,13.8057746032556));
#448655=CARTESIAN_POINT('Ctrl Pts',(2.47784371587751,1.08662758259173,13.8013225161808));
#448656=CARTESIAN_POINT('Ctrl Pts',(2.4893733387089,1.08701966071042,13.8136962270464));
#448657=CARTESIAN_POINT('Ctrl Pts',(2.49288049554738,1.07077963434889,13.8168830918628));
#448658=CARTESIAN_POINT('Ctrl Pts',(2.46592821445409,1.08622697703056,13.8124254880875));
#448659=CARTESIAN_POINT('Ctrl Pts',(2.47744095526533,1.08661847933377,13.8247886461868));
#448660=CARTESIAN_POINT('Ctrl Pts',(2.48095506764791,1.07040208095555,13.8279860620656));
#448661=CARTESIAN_POINT('Ctrl Pts',(2.454007370493,1.08582619185041,13.8235227163065));
#448662=CARTESIAN_POINT('Ctrl Pts',(2.4654977970538,1.08621693561251,13.8358800595847));
#448663=CARTESIAN_POINT('Ctrl Pts',(2.46902410772917,1.0700246237387,13.8390832900376));
#448664=CARTESIAN_POINT('Origin',(2.49049725742216,1.06504057198453,13.7902182540695));
#448665=CARTESIAN_POINT('Ctrl Pts',(2.5102036306474,1.08771551347853,13.7382347919292));
#448666=CARTESIAN_POINT('Ctrl Pts',(2.52528460742438,1.08824655790786,13.7369371795942));
#448667=CARTESIAN_POINT('Ctrl Pts',(2.53116611461982,1.07428404917444,13.7364597369712));
#448668=CARTESIAN_POINT('Ctrl Pts',(2.51209412109904,1.08777907318603,13.7595490285574));
#448669=CARTESIAN_POINT('Ctrl Pts',(2.52753495243651,1.08832178307826,13.7633824266926));
#448670=CARTESIAN_POINT('Ctrl Pts',(2.53360479778411,1.07457221443906,13.7648920890506));
#448671=CARTESIAN_POINT('Ctrl Pts',(2.50245272336482,1.08745492216785,13.780380659011));
#448672=CARTESIAN_POINT('Ctrl Pts',(2.51580830018509,1.08792974192552,13.7901039518743));
#448673=CARTESIAN_POINT('Ctrl Pts',(2.52117168901941,1.07310680356507,13.7926933640892));
#448674=CARTESIAN_POINT('Ctrl Pts',(2.48569382187465,1.08689147526159,13.7936647693663));
#448675=CARTESIAN_POINT('Ctrl Pts',(2.49650208684873,1.0872848455642,13.8072068914933));
#448676=CARTESIAN_POINT('Ctrl Pts',(2.49960565550404,1.07052142910306,13.8104111085397));
#448677=CARTESIAN_POINT('Origin',(2.51121257138439,1.06573703197411,13.7435492065112));
#448678=CARTESIAN_POINT('Origin',(2.51121257138439,1.06573703197411,14.));
#448679=CARTESIAN_POINT('Origin',(2.51121257138439,1.06573703197411,12.5369868989719));
#448680=CARTESIAN_POINT('Ctrl Pts',(2.51161540710188,1.10398759845017,12.506462012331));
#448681=CARTESIAN_POINT('Ctrl Pts',(2.51760129318922,1.10661871147307,12.4999388158272));
#448682=CARTESIAN_POINT('Ctrl Pts',(2.5175304723068,1.10658758195552,12.4907030323752));
#448683=CARTESIAN_POINT('Ctrl Pts',(2.5189533141719,1.09292488165065,12.5042014951932));
#448684=CARTESIAN_POINT('Ctrl Pts',(2.52478230827215,1.090211226386,12.4980716682127));
#448685=CARTESIAN_POINT('Ctrl Pts',(2.52747049798941,1.08397430396625,12.4907355092743));
#448686=CARTESIAN_POINT('Ctrl Pts',(2.5156154878654,1.08790645392943,12.5218047446509));
#448687=CARTESIAN_POINT('Ctrl Pts',(2.52706285447636,1.0849949820318,12.5216906929434));
#448688=CARTESIAN_POINT('Ctrl Pts',(2.53155200346214,1.07412215830871,12.5161988840776));
#448689=CARTESIAN_POINT('Ctrl Pts',(2.51043494394272,1.08772328439607,12.5369868989719));
#448690=CARTESIAN_POINT('Ctrl Pts',(2.52575525458304,1.08826514545271,12.5369868989719));
#448691=CARTESIAN_POINT('Ctrl Pts',(2.53156907091975,1.0740804681168,12.5369868989719));
#448692=CARTESIAN_POINT('Origin',(4.68629905775447E-31,-3.01170153175948E-31,
12.5));
#448693=CARTESIAN_POINT('Origin',(2.35734085275916,1.28223802992782,12.5));
#448694=CARTESIAN_POINT('',(2.35734085275916,1.28223802992782,12.5893111709658));
#448695=CARTESIAN_POINT('',(2.35734085275916,1.28223802992782,13.8235269408515));
#448696=CARTESIAN_POINT('',(2.35734085275916,1.28223802992782,12.5));
#448697=CARTESIAN_POINT('',(2.39287067323911,1.28634954496043,13.7902182540695));
#448698=CARTESIAN_POINT('',(2.35734085275916,1.28223802992782,13.8235269408515));
#448699=CARTESIAN_POINT('',(2.41346029074826,1.28873217793636,13.7435492065112));
#448700=CARTESIAN_POINT('Origin',(2.34572068385282,1.28089367053509,13.7445212918707));
#448701=CARTESIAN_POINT('',(2.41346029074826,1.28873217793636,12.5369868989719));
#448702=CARTESIAN_POINT('',(2.41346029074826,1.28873217793636,12.5));
#448703=CARTESIAN_POINT('Ctrl Pts',(2.41346029074826,1.28873217793636,12.5369868989719));
#448704=CARTESIAN_POINT('Ctrl Pts',(2.39476745478683,1.2865690407457,12.5544431401645));
#448705=CARTESIAN_POINT('Ctrl Pts',(2.37606124921229,1.28440435642184,12.5718848856037));
#448706=CARTESIAN_POINT('Ctrl Pts',(2.35734085275916,1.28223802992782,12.5893111709658));
#448707=CARTESIAN_POINT('Origin',(2.49626940223468,1.55385500512921,12.5));
#448708=CARTESIAN_POINT('',(2.3612652642965,1.38204470010708,13.7435492065112));
#448709=CARTESIAN_POINT('',(2.34845905999782,1.36574714137789,13.7902182540695));
#448710=CARTESIAN_POINT('Origin',(2.31480656845809,1.32291997382215,13.7418732680446));
#448711=CARTESIAN_POINT('',(2.32636043968301,1.33762377601413,13.8235269408515));
#448712=CARTESIAN_POINT('',(2.34845905999782,1.36574714137789,13.7902182540695));
#448713=CARTESIAN_POINT('',(2.32636043968301,1.33762377601413,12.5893111709658));
#448714=CARTESIAN_POINT('',(2.32636043968301,1.33762377601413,12.5));
#448715=CARTESIAN_POINT('',(2.3612652642965,1.38204470010708,12.5369868989719));
#448716=CARTESIAN_POINT('Ctrl Pts',(2.32636043968301,1.33762377601413,12.5893111709658));
#448717=CARTESIAN_POINT('Ctrl Pts',(2.33800403730811,1.35244176670741,12.5718848856037));
#448718=CARTESIAN_POINT('Ctrl Pts',(2.34963880857737,1.36724852471619,12.5544431401645));
#448719=CARTESIAN_POINT('Ctrl Pts',(2.3612652642965,1.38204470010708,12.5369868989719));
#448720=CARTESIAN_POINT('',(2.3612652642965,1.38204470010708,12.5));
#448721=CARTESIAN_POINT('Origin',(2.3533893433224,1.31638515569517,12.5));
#448722=CARTESIAN_POINT('',(2.3239518225894,1.29863628121615,13.8587068136939));
#448723=CARTESIAN_POINT('Ctrl Pts',(2.32636043967773,1.3376237760181,13.8235269408542));
#448724=CARTESIAN_POINT('Ctrl Pts',(2.32527778080196,1.33624595194157,13.8262006681044));
#448725=CARTESIAN_POINT('Ctrl Pts',(2.32430644806145,1.33472860533013,13.8288634856214));
#448726=CARTESIAN_POINT('Ctrl Pts',(2.32343931652769,1.33308300744998,13.8314912288862));
#448727=CARTESIAN_POINT('Ctrl Pts',(2.32254539335684,1.33138656577109,13.8342001611531));
#448728=CARTESIAN_POINT('Ctrl Pts',(2.32176077732778,1.32955217257974,13.8368750301949));
#448729=CARTESIAN_POINT('Ctrl Pts',(2.32110448918224,1.32755579711711,13.8394886372969));
#448730=CARTESIAN_POINT('Ctrl Pts',(2.32105380245683,1.3274016121976,13.8396904925131));
#448731=CARTESIAN_POINT('Ctrl Pts',(2.32100390072192,1.32724645063996,13.8398919674349));
#448732=CARTESIAN_POINT('Ctrl Pts',(2.32095480326791,1.3270902968873,13.8400930404591));
#448733=CARTESIAN_POINT('Ctrl Pts',(2.32018983190341,1.32465731636581,13.8432258934518));
#448734=CARTESIAN_POINT('Ctrl Pts',(2.31962293533913,1.32199622539247,13.8462331177034));
#448735=CARTESIAN_POINT('Ctrl Pts',(2.31936695184163,1.31917371508202,13.8489036603661));
#448736=CARTESIAN_POINT('Ctrl Pts',(2.31928319106221,1.31825015686123,13.8497774930041));
#448737=CARTESIAN_POINT('Ctrl Pts',(2.31923287418977,1.31730951176935,13.85061494757));
#448738=CARTESIAN_POINT('Ctrl Pts',(2.31922038831851,1.31635468307864,13.8514076489583));
#448739=CARTESIAN_POINT('Ctrl Pts',(2.31919397890005,1.31433508269089,13.8530843267192));
#448740=CARTESIAN_POINT('Ctrl Pts',(2.31933718273174,1.31205361062889,13.8546805203176));
#448741=CARTESIAN_POINT('Ctrl Pts',(2.31977786602568,1.30965123033594,13.8559412814273));
#448742=CARTESIAN_POINT('Ctrl Pts',(2.31983684374211,1.3093297139417,13.8561100121513));
#448743=CARTESIAN_POINT('Ctrl Pts',(2.31990108311304,1.30900607034723,13.8562727473908));
#448744=CARTESIAN_POINT('Ctrl Pts',(2.3199708207249,1.30868066685121,13.8564289040185));
#448745=CARTESIAN_POINT('Ctrl Pts',(2.32028707999907,1.30720496570915,13.8571370725437));
#448746=CARTESIAN_POINT('Ctrl Pts',(2.32072420160441,1.3056676085477,13.8577210840554));
#448747=CARTESIAN_POINT('Ctrl Pts',(2.32129342366775,1.30413637918839,13.8581177131616));
#448748=CARTESIAN_POINT('Ctrl Pts',(2.32145373619281,1.3037051322975,13.8582294175695));
#448749=CARTESIAN_POINT('Ctrl Pts',(2.32162435127528,1.30327434337993,13.8583265086086));
#448750=CARTESIAN_POINT('Ctrl Pts',(2.32180509082108,1.30284543137745,13.8584082369006));
#448751=CARTESIAN_POINT('Ctrl Pts',(2.32206476508117,1.30222919984718,13.8585256585398));
#448752=CARTESIAN_POINT('Ctrl Pts',(2.32234886457458,1.30160930699463,13.8586122832068));
#448753=CARTESIAN_POINT('Ctrl Pts',(2.32265072710445,1.30100218484903,13.8586682984299));
#448754=CARTESIAN_POINT('Ctrl Pts',(2.32289218720567,1.30051654731463,13.8587131050557));
#448755=CARTESIAN_POINT('Ctrl Pts',(2.3231474698,1.3000336127437,13.8587357943552));
#448756=CARTESIAN_POINT('Ctrl Pts',(2.32341705296171,1.29955356042874,13.8587355499465));
#448757=CARTESIAN_POINT('Ctrl Pts',(2.3235912909863,1.29924329117257,13.8587353919793));
#448758=CARTESIAN_POINT('Ctrl Pts',(2.32376958494548,1.29893756220855,13.8587257282814));
#448759=CARTESIAN_POINT('Ctrl Pts',(2.3239518225894,1.29863628121615,13.8587068136939));
#448760=CARTESIAN_POINT('Ctrl Pts',(2.3239518225894,1.29863628121615,13.8587068136939));
#448761=CARTESIAN_POINT('Ctrl Pts',(2.32455119226537,1.29764538445678,13.8586446046466));
#448762=CARTESIAN_POINT('Ctrl Pts',(2.32519316922359,1.29670254215215,13.858482427929));
#448763=CARTESIAN_POINT('Ctrl Pts',(2.32587423919463,1.29580499099488,13.8582284286032));
#448764=CARTESIAN_POINT('Ctrl Pts',(2.32657293775961,1.29488420791493,13.8579678548414));
#448765=CARTESIAN_POINT('Ctrl Pts',(2.32731570614221,1.29400976756026,13.857615680862));
#448766=CARTESIAN_POINT('Ctrl Pts',(2.32806587620233,1.29320987107419,13.8571944833187));
#448767=CARTESIAN_POINT('Ctrl Pts',(2.32993800230844,1.29121364758652,13.8561433417727));
#448768=CARTESIAN_POINT('Ctrl Pts',(2.33194030064112,1.28958502811147,13.8546163505475));
#448769=CARTESIAN_POINT('Ctrl Pts',(2.33386900550433,1.28828883584181,13.8528973491086));
#448770=CARTESIAN_POINT('Ctrl Pts',(2.33422135142747,1.28805204063767,13.8525833129072));
#448771=CARTESIAN_POINT('Ctrl Pts',(2.33457122551807,1.28782619937748,13.8522628768812));
#448772=CARTESIAN_POINT('Ctrl Pts',(2.33491739353448,1.2876109189613,13.851937733538));
#448773=CARTESIAN_POINT('Ctrl Pts',(2.33703139358197,1.28629623132855,13.8499521282529));
#448774=CARTESIAN_POINT('Ctrl Pts',(2.33921942577769,1.28524820517461,13.847639871647));
#448775=CARTESIAN_POINT('Ctrl Pts',(2.34133178933503,1.28444946311461,13.8452109780794));
#448776=CARTESIAN_POINT('Ctrl Pts',(2.34228218542323,1.28409009252868,13.8441181685877));
#448777=CARTESIAN_POINT('Ctrl Pts',(2.34321725800112,1.2837804664361,13.8430021611332));
#448778=CARTESIAN_POINT('Ctrl Pts',(2.34412437039983,1.28351584738843,13.8418824960098));
#448779=CARTESIAN_POINT('Ctrl Pts',(2.34626200393133,1.28289226584532,13.8392439765549));
#448780=CARTESIAN_POINT('Ctrl Pts',(2.34834549739249,1.28248517720724,13.8364981347964));
#448781=CARTESIAN_POINT('Ctrl Pts',(2.35037379864419,1.28225991943209,13.8336931113419));
#448782=CARTESIAN_POINT('Ctrl Pts',(2.3523492352543,1.28204053266428,13.8309611966328));
#448783=CARTESIAN_POINT('Ctrl Pts',(2.35427436101996,1.28199396311011,13.8281701127186));
#448784=CARTESIAN_POINT('Ctrl Pts',(2.3561380341987,1.28212615033551,13.8253580685121));
#448785=CARTESIAN_POINT('Ctrl Pts',(2.35654208055519,1.28215480866864,13.8247484142933));
#448786=CARTESIAN_POINT('Ctrl Pts',(2.35694313199631,1.28219200563405,13.8241378483365));
#448787=CARTESIAN_POINT('Ctrl Pts',(2.35734085275916,1.28223802992782,13.8235269408515));
#448788=CARTESIAN_POINT('',(2.32332976716748,1.29971137372854,12.5969504640361));
#448789=CARTESIAN_POINT('Origin',(2.35341831404089,1.31640113631719,12.584524458991));
#448790=CARTESIAN_POINT('Origin',(2.35341831404089,1.31640113631719,12.584524458991));
#448791=CARTESIAN_POINT('Ctrl Pts',(2.32636043968301,1.33762377601413,12.5893111709658));
#448792=CARTESIAN_POINT('Ctrl Pts',(2.31935774413809,1.32871193615555,12.5770542771492));
#448793=CARTESIAN_POINT('Ctrl Pts',(2.33011456022595,1.31637927291897,12.5737548217797));
#448794=CARTESIAN_POINT('Ctrl Pts',(2.34167298466528,1.35711097888248,12.5663937883685));
#448795=CARTESIAN_POINT('Ctrl Pts',(2.33466135620968,1.34818777073451,12.5540940315304));
#448796=CARTESIAN_POINT('Ctrl Pts',(2.34545392548238,1.33581900184643,12.5508374392248));
#448797=CARTESIAN_POINT('Ctrl Pts',(2.3569700794774,1.37657851940206,12.5434499600945));
#448798=CARTESIAN_POINT('Ctrl Pts',(2.34993565372079,1.36762629872672,12.5311293540533));
#448799=CARTESIAN_POINT('Ctrl Pts',(2.36077737761453,1.35524046861433,12.5278936106989));
#448800=CARTESIAN_POINT('Ctrl Pts',(2.37225293435228,1.39602793775148,12.5204817579905));
#448801=CARTESIAN_POINT('Ctrl Pts',(2.36518369299553,1.38703140970183,12.5081597038247));
#448802=CARTESIAN_POINT('Ctrl Pts',(2.37608614257654,1.37464510121107,12.5049254088044));
#448803=CARTESIAN_POINT('Ctrl Pts',(2.3612652642965,1.38204470010708,12.5369868989719));
#448804=CARTESIAN_POINT('Ctrl Pts',(2.36184079537726,1.38277713791727,12.5342545179733));
#448805=CARTESIAN_POINT('Ctrl Pts',(2.36248814323123,1.38339906867655,12.5314872231885));
#448806=CARTESIAN_POINT('Ctrl Pts',(2.36320957034566,1.38383514668411,12.5287124745063));
#448807=CARTESIAN_POINT('Ctrl Pts',(2.36386018912591,1.38422842347631,12.5262100684184));
#448808=CARTESIAN_POINT('Ctrl Pts',(2.36457091136567,1.38446930152772,12.5237004536639));
#448809=CARTESIAN_POINT('Ctrl Pts',(2.36537521888829,1.38449913406827,12.5212220730815));
#448810=CARTESIAN_POINT('Ctrl Pts',(2.36599098587501,1.38452197345878,12.5193246583486));
#448811=CARTESIAN_POINT('Ctrl Pts',(2.36666898813309,1.38442075309951,12.517417831369));
#448812=CARTESIAN_POINT('Ctrl Pts',(2.36741412601232,1.38409836475537,12.5155812248348));
#448813=CARTESIAN_POINT('Ctrl Pts',(2.367731558754,1.38396102558792,12.5147988205793));
#448814=CARTESIAN_POINT('Ctrl Pts',(2.36806160754755,1.38378366355532,12.5140295443047));
#448815=CARTESIAN_POINT('Ctrl Pts',(2.36840644951409,1.38355990750301,12.5132817086137));
#448816=CARTESIAN_POINT('Ctrl Pts',(2.36892832118129,1.38322128298688,12.5121499604604));
#448817=CARTESIAN_POINT('Ctrl Pts',(2.3694914498736,1.38276309176832,12.5110494206568));
#448818=CARTESIAN_POINT('Ctrl Pts',(2.37008287664953,1.38215042017407,12.5100666561695));
#448819=CARTESIAN_POINT('Ctrl Pts',(2.37042247254234,1.3817986255555,12.5095023550641));
#448820=CARTESIAN_POINT('Ctrl Pts',(2.37077485248524,1.38139138028384,12.5089719619137));
#448821=CARTESIAN_POINT('Ctrl Pts',(2.37112858161518,1.38093213852879,12.5085043804652));
#448822=CARTESIAN_POINT('Ctrl Pts',(2.37164621812038,1.38026009804072,12.5078201359221));
#448823=CARTESIAN_POINT('Ctrl Pts',(2.37218080017373,1.37945648119119,12.5072563000949));
#448824=CARTESIAN_POINT('Ctrl Pts',(2.37268904215778,1.37857107231839,12.5068768744332));
#448825=CARTESIAN_POINT('Ctrl Pts',(2.37305551961577,1.37793263156935,12.5066032824114));
#448826=CARTESIAN_POINT('Ctrl Pts',(2.37341479235406,1.37724047730894,12.5064197834844));
#448827=CARTESIAN_POINT('Ctrl Pts',(2.3737490918574,1.37653445206906,12.5063282718343));
#448828=CARTESIAN_POINT('Ctrl Pts',(2.37423706563576,1.37550387379872,12.5061946931565));
#448829=CARTESIAN_POINT('Ctrl Pts',(2.37468321891324,1.37442216786226,12.5062515701262));
#448830=CARTESIAN_POINT('Ctrl Pts',(2.37507415887602,1.37336236336887,12.5064436508398));
#448831=CARTESIAN_POINT('',(2.33011456022595,1.31637927291897,12.5737548217797));
#448832=CARTESIAN_POINT('Origin',(2.34365893801222,1.32403105900999,12.5893111709658));
#448833=CARTESIAN_POINT('Ctrl Pts',(2.37507415887602,1.37336236336887,12.5064436508398));
#448834=CARTESIAN_POINT('Ctrl Pts',(2.36841934737568,1.36492708793495,12.5164271754438));
#448835=CARTESIAN_POINT('Ctrl Pts',(2.36176173387593,1.35648859817026,12.5264061185523));
#448836=CARTESIAN_POINT('Ctrl Pts',(2.35510122043578,1.34804678028252,12.536380305637));
#448837=CARTESIAN_POINT('Ctrl Pts',(2.34677692953329,1.33749622010799,12.5488460165097));
#448838=CARTESIAN_POINT('Ctrl Pts',(2.33844810646613,1.32694045832694,12.5613043021964));
#448839=CARTESIAN_POINT('Ctrl Pts',(2.33011456022595,1.31637927291897,12.5737548217797));
#448840=CARTESIAN_POINT('Ctrl Pts',(2.35734085275916,1.28223802992782,12.5893111709658));
#448841=CARTESIAN_POINT('Ctrl Pts',(2.3460820270025,1.28093515727823,12.5770542771492));
#448842=CARTESIAN_POINT('Ctrl Pts',(2.34120305426879,1.29655563422097,12.5737548217797));
#448843=CARTESIAN_POINT('Ctrl Pts',(2.3468364662523,1.28102246107754,12.5928319619712));
#448844=CARTESIAN_POINT('Ctrl Pts',(2.33889535256909,1.28338299700011,12.5821634970843));
#448845=CARTESIAN_POINT('Ctrl Pts',(2.33737764554695,1.29610345562765,12.5773203894503));
#448846=CARTESIAN_POINT('Ctrl Pts',(2.33091023073949,1.2862127521802,12.5969440695591));
#448847=CARTESIAN_POINT('Ctrl Pts',(2.32893194676206,1.28971202854204,12.5878292599214));
#448848=CARTESIAN_POINT('Ctrl Pts',(2.33170184418414,1.29795532657012,12.5813877129824));
#448849=CARTESIAN_POINT('Ctrl Pts',(2.31592647392008,1.31288975120779,12.596957478804));
#448850=CARTESIAN_POINT('Ctrl Pts',(2.31789020762768,1.30941637488575,12.5878468778671));
#448851=CARTESIAN_POINT('Ctrl Pts',(2.32634415079954,1.30750631551895,12.5814011370086));
#448852=CARTESIAN_POINT('Ctrl Pts',(2.31981749908179,1.32929703405204,12.5928371701607));
#448853=CARTESIAN_POINT('Ctrl Pts',(2.3176801928667,1.32129909757775,12.5821692192952));
#448854=CARTESIAN_POINT('Ctrl Pts',(2.32771932495136,1.31334676150872,12.5773318885715));
#448855=CARTESIAN_POINT('Ctrl Pts',(2.32636043968297,1.33762377601416,12.5893111709658));
#448856=CARTESIAN_POINT('Ctrl Pts',(2.31935774413805,1.32871193615558,12.5770542771492));
#448857=CARTESIAN_POINT('Ctrl Pts',(2.33011456022591,1.316379272919,12.5737548217797));
#448858=CARTESIAN_POINT('',(2.34120305426879,1.29655563422097,12.5737548217797));
#448859=CARTESIAN_POINT('Origin',(2.35481188671963,1.30409219041892,12.5893111709658));
#448860=CARTESIAN_POINT('Ctrl Pts',(2.33011456022591,1.316379272919,12.5737548217797));
#448861=CARTESIAN_POINT('Ctrl Pts',(2.32947000504072,1.31561189540807,12.5746934679442));
#448862=CARTESIAN_POINT('Ctrl Pts',(2.32889703068478,1.31464492290294,12.5756680099006));
#448863=CARTESIAN_POINT('Ctrl Pts',(2.32845796053182,1.31359006695601,12.5765688348656));
#448864=CARTESIAN_POINT('Ctrl Pts',(2.3283417215695,1.3133108055217,12.5768073183026));
#448865=CARTESIAN_POINT('Ctrl Pts',(2.32823466135262,1.3130255382082,12.5770407398754));
#448866=CARTESIAN_POINT('Ctrl Pts',(2.32813741460693,1.31273654995004,12.5772674179684));
#448867=CARTESIAN_POINT('Ctrl Pts',(2.32773834025925,1.31155062028427,12.5781976435658));
#448868=CARTESIAN_POINT('Ctrl Pts',(2.3274925550386,1.31023107221463,12.5790594849312));
#448869=CARTESIAN_POINT('Ctrl Pts',(2.32746412743688,1.30885816122147,12.5797571720116));
#448870=CARTESIAN_POINT('Ctrl Pts',(2.3274456058322,1.30796366034395,12.580211740231));
#448871=CARTESIAN_POINT('Ctrl Pts',(2.32753727948252,1.30700546781519,12.5806009430798));
#448872=CARTESIAN_POINT('Ctrl Pts',(2.32775033112578,1.30605272353595,12.5808812374708));
#448873=CARTESIAN_POINT('Ctrl Pts',(2.32793341316648,1.30523400013046,12.5811221033394));
#448874=CARTESIAN_POINT('Ctrl Pts',(2.32820998647182,1.30440256344648,12.581287365893));
#448875=CARTESIAN_POINT('Ctrl Pts',(2.32857235253435,1.3036079729103,12.581359338449));
#448876=CARTESIAN_POINT('Ctrl Pts',(2.32862271393447,1.30349754123344,12.5813693411482));
#448877=CARTESIAN_POINT('Ctrl Pts',(2.32867468935954,1.30338777966755,12.5813775999465));
#448878=CARTESIAN_POINT('Ctrl Pts',(2.32872821476693,1.30327877787652,12.5813841266931));
#448879=CARTESIAN_POINT('Ctrl Pts',(2.32881902709433,1.30309384315453,12.5813952001081));
#448880=CARTESIAN_POINT('Ctrl Pts',(2.32891545583196,1.30291012523305,12.5814007534795));
#448881=CARTESIAN_POINT('Ctrl Pts',(2.32901763360014,1.30272779577977,12.5814005856065));
#448882=CARTESIAN_POINT('Ctrl Pts',(2.32948536347396,1.30189316282882,12.5813998171494));
#448883=CARTESIAN_POINT('Ctrl Pts',(2.33004095047256,1.30114512627378,12.58127954464));
#448884=CARTESIAN_POINT('Ctrl Pts',(2.33065748618066,1.30047029012495,12.5810700125799));
#448885=CARTESIAN_POINT('Ctrl Pts',(2.33140219111783,1.29965516489341,12.5808169217085));
#448886=CARTESIAN_POINT('Ctrl Pts',(2.33224824269838,1.29895805293504,12.5804173076348));
#448887=CARTESIAN_POINT('Ctrl Pts',(2.33310493392748,1.29841994931524,12.5799304713245));
#448888=CARTESIAN_POINT('Ctrl Pts',(2.3341666442459,1.29775306941019,12.5793271277669));
#448889=CARTESIAN_POINT('Ctrl Pts',(2.3352934286002,1.29726177537674,12.5785808224116));
#448890=CARTESIAN_POINT('Ctrl Pts',(2.33642511441489,1.29693770273082,12.5777485681082));
#448891=CARTESIAN_POINT('Ctrl Pts',(2.33811145026421,1.29645479898359,12.576508418016));
#448892=CARTESIAN_POINT('Ctrl Pts',(2.33979257822632,1.29634065746709,12.5750928681475));
#448893=CARTESIAN_POINT('Ctrl Pts',(2.34120305426879,1.29655563422097,12.5737548217797));
#448894=CARTESIAN_POINT('Ctrl Pts',(2.34120305426879,1.29655563422097,12.5737548217797));
#448895=CARTESIAN_POINT('Ctrl Pts',(2.3460820270025,1.28093515727823,12.5770542771492));
#448896=CARTESIAN_POINT('Ctrl Pts',(2.35734085275916,1.28223802992782,12.5893111709658));
#448897=CARTESIAN_POINT('Ctrl Pts',(2.36579221694363,1.29945184435155,12.5508408821982));
#448898=CARTESIAN_POINT('Ctrl Pts',(2.37068323832445,1.28378201236515,12.55409748406));
#448899=CARTESIAN_POINT('Ctrl Pts',(2.38195642745925,1.28508654714655,12.5663972313419));
#448900=CARTESIAN_POINT('Ctrl Pts',(2.39035749707839,1.30234405383429,12.52790050457));
#448901=CARTESIAN_POINT('Ctrl Pts',(2.39523733247122,1.28662341504699,12.5311362602938));
#448902=CARTESIAN_POINT('Ctrl Pts',(2.40654716908935,1.28793219067949,12.5434568539655));
#448903=CARTESIAN_POINT('Ctrl Pts',(2.41490075227283,1.30523255981786,12.5049357605811));
#448904=CARTESIAN_POINT('Ctrl Pts',(2.41974922116736,1.28945993370906,12.5081700652078));
#448905=CARTESIAN_POINT('Ctrl Pts',(2.43111502258053,1.29077518559428,12.5204921097672));
#448906=CARTESIAN_POINT('Ctrl Pts',(2.41328914611567,1.30504288761613,12.5064436508395));
#448907=CARTESIAN_POINT('Ctrl Pts',(2.41404361045141,1.30408391349934,12.5062361689309));
#448908=CARTESIAN_POINT('Ctrl Pts',(2.41478729883436,1.3030544868582,12.5061871075061));
#448909=CARTESIAN_POINT('Ctrl Pts',(2.4154499997122,1.30201918777695,12.5063648335164));
#448910=CARTESIAN_POINT('Ctrl Pts',(2.415751039328,1.30154889107435,12.5064455676329));
#448911=CARTESIAN_POINT('Ctrl Pts',(2.4160393801953,1.3010707041361,12.506574497099));
#448912=CARTESIAN_POINT('Ctrl Pts',(2.4163017591295,1.30060458749904,12.5067492519495));
#448913=CARTESIAN_POINT('Ctrl Pts',(2.41682901978261,1.29966790802348,12.5071004286051));
#448914=CARTESIAN_POINT('Ctrl Pts',(2.41727012097808,1.29874513659593,12.5076537929613));
#448915=CARTESIAN_POINT('Ctrl Pts',(2.41760048935406,1.29790961126267,12.5083435010505));
#448916=CARTESIAN_POINT('Ctrl Pts',(2.41762128801762,1.29785700994982,12.5083869222964));
#448917=CARTESIAN_POINT('Ctrl Pts',(2.41764163896602,1.29780474430814,12.5084308732337));
#448918=CARTESIAN_POINT('Ctrl Pts',(2.41766153276987,1.29775282825451,12.5084753333615));
#448919=CARTESIAN_POINT('Ctrl Pts',(2.41782110733411,1.29733639298138,12.5088319622689));
#448920=CARTESIAN_POINT('Ctrl Pts',(2.4179557127917,1.29693445804919,12.509227847131));
#448921=CARTESIAN_POINT('Ctrl Pts',(2.41806400173893,1.2965598642607,12.5096423454524));
#448922=CARTESIAN_POINT('Ctrl Pts',(2.41840333137287,1.29538605311581,12.5109411997424));
#448923=CARTESIAN_POINT('Ctrl Pts',(2.41851441364044,1.29441119783451,12.5124831113042));
#448924=CARTESIAN_POINT('Ctrl Pts',(2.41848765682672,1.293607330589,12.5140723025008));
#448925=CARTESIAN_POINT('Ctrl Pts',(2.41848514968397,1.29353200734764,12.5142212114565));
#448926=CARTESIAN_POINT('Ctrl Pts',(2.41848145573209,1.29345816722788,12.5143705582413));
#448927=CARTESIAN_POINT('Ctrl Pts',(2.41847666366391,1.29338577808433,12.5145201959299));
#448928=CARTESIAN_POINT('Ctrl Pts',(2.41841510241349,1.29245583175926,12.5164425148273));
#448929=CARTESIAN_POINT('Ctrl Pts',(2.41818092200696,1.29173277068538,12.5184635205941));
#448930=CARTESIAN_POINT('Ctrl Pts',(2.41783386717489,1.29114900384466,12.5205025929158));
#448931=CARTESIAN_POINT('Ctrl Pts',(2.41763256161632,1.29081039593868,12.5216853356836));
#448932=CARTESIAN_POINT('Ctrl Pts',(2.41739405919928,1.29051901757365,12.5228750347131));
#448933=CARTESIAN_POINT('Ctrl Pts',(2.41713422275923,1.29026585187105,12.5240609649613));
#448934=CARTESIAN_POINT('Ctrl Pts',(2.41649646815689,1.28964447023587,12.5269717671326));
#448935=CARTESIAN_POINT('Ctrl Pts',(2.41570498716153,1.28924325106614,12.5299036066169));
#448936=CARTESIAN_POINT('Ctrl Pts',(2.41481087945404,1.28899220618257,12.5328133004019));
#448937=CARTESIAN_POINT('Ctrl Pts',(2.41438165569212,1.28887169002055,12.5342101228451));
#448938=CARTESIAN_POINT('Ctrl Pts',(2.41392917487694,1.28878643734573,12.5356023438238));
#448939=CARTESIAN_POINT('Ctrl Pts',(2.41346029074826,1.28873217793636,12.5369868989719));
#448940=CARTESIAN_POINT('Origin',(15.0752513500072,2.74862334284653,-1.24041811817541));
#448941=CARTESIAN_POINT('Ctrl Pts',(2.36123941047144,1.38201186200937,12.5369868989719));
#448942=CARTESIAN_POINT('Ctrl Pts',(2.37073948644324,1.39405477943892,12.5369868989719));
#448943=CARTESIAN_POINT('Ctrl Pts',(2.3627244217467,1.40713308367132,12.5369868989719));
#448944=CARTESIAN_POINT('Ctrl Pts',(2.36445075571135,1.38608288010418,12.5218025310016));
#448945=CARTESIAN_POINT('Ctrl Pts',(2.36887186146598,1.39704233664229,12.5216901060418));
#448946=CARTESIAN_POINT('Ctrl Pts',(2.36274886838135,1.40709322528321,12.5161920673677));
#448947=CARTESIAN_POINT('Ctrl Pts',(2.37047257207358,1.38581122058474,12.5042015548895));
#448948=CARTESIAN_POINT('Ctrl Pts',(2.37172872680604,1.39211989875893,12.4980677368513));
#448949=CARTESIAN_POINT('Ctrl Pts',(2.36828310199102,1.39797809381866,12.4907278922778));
#448950=CARTESIAN_POINT('Ctrl Pts',(2.37505684410862,1.3733523512695,12.506463626192));
#448951=CARTESIAN_POINT('Ctrl Pts',(2.38072083974236,1.3766274988688,12.4999376786891));
#448952=CARTESIAN_POINT('Ctrl Pts',(2.38065166227114,1.37658749770293,12.4906970594712));
#448953=CARTESIAN_POINT('Origin',(2.34396676596729,1.39563741711121,12.5369868989719));
#448954=CARTESIAN_POINT('Origin',(2.34396676596729,1.39563741711121,14.));
#448955=CARTESIAN_POINT('Origin',(2.34396676596729,1.39563741711121,13.7435492065112));
#448956=CARTESIAN_POINT('Ctrl Pts',(2.34596719356845,1.36257596155278,13.793642941384));
#448957=CARTESIAN_POINT('Ctrl Pts',(2.35266897582987,1.3710607911637,13.8071662555867));
#448958=CARTESIAN_POINT('Ctrl Pts',(2.34100211148853,1.38346658255626,13.8103758687955));
#448959=CARTESIAN_POINT('Ctrl Pts',(2.35623656914238,1.37564507133673,13.7804579775006));
#448960=CARTESIAN_POINT('Ctrl Pts',(2.36449800484156,1.38612086972719,13.7901904343351));
#448961=CARTESIAN_POINT('Ctrl Pts',(2.35570307465003,1.39919393849814,13.7927914348262));
#448962=CARTESIAN_POINT('Ctrl Pts',(2.36228253699291,1.38333934813595,13.7597120340895));
#448963=CARTESIAN_POINT('Ctrl Pts',(2.37183884511689,1.3954663454977,13.7635825532445));
#448964=CARTESIAN_POINT('Ctrl Pts',(2.36435354136949,1.40848579801899,13.7651073818884));
#448965=CARTESIAN_POINT('Ctrl Pts',(2.36109859805022,1.38183263256027,13.7381884353898));
#448966=CARTESIAN_POINT('Ctrl Pts',(2.37043192895505,1.39367521863119,13.7368803041982));
#448967=CARTESIAN_POINT('Ctrl Pts',(2.36265916120258,1.40666651258464,13.7363986145813));
#448968=CARTESIAN_POINT('Origin',(2.33116056166861,1.37933985838202,13.7902182540695));
#448969=CARTESIAN_POINT('Ctrl Pts',(2.32635800710304,1.33762068146841,13.8235227101244));
#448970=CARTESIAN_POINT('Ctrl Pts',(2.33346496801523,1.34665803699489,13.8358800583119));
#448971=CARTESIAN_POINT('Ctrl Pts',(2.3224883845271,1.35907337686075,13.8390832900376));
#448972=CARTESIAN_POINT('Ctrl Pts',(2.33372747122631,1.34699928199462,13.8124254819053));
#448973=CARTESIAN_POINT('Ctrl Pts',(2.34084823353721,1.35605418810938,13.8247886449157));
#448974=CARTESIAN_POINT('Ctrl Pts',(2.32984501138978,1.36847392576671,13.8279860620657));
#448975=CARTESIAN_POINT('Ctrl Pts',(2.34109363259552,1.35637367933719,13.8013225099955));
#448976=CARTESIAN_POINT('Ctrl Pts',(2.34822483802452,1.36544186233943,13.8136962257787));
#448977=CARTESIAN_POINT('Ctrl Pts',(2.33719844595767,1.37786995563124,13.8168830918626));
#448978=CARTESIAN_POINT('Ctrl Pts',(2.34845661971575,1.36574403703554,13.7902140179785));
#448979=CARTESIAN_POINT('Ctrl Pts',(2.35559512946828,1.37482150254402,13.802602731458));
#448980=CARTESIAN_POINT('Ctrl Pts',(2.34454881511306,1.38726164288434,13.8057746032558));
#448981=CARTESIAN_POINT('Origin',(2.30906194135381,1.35121649301826,13.8235269408515));
#448982=CARTESIAN_POINT('Ctrl Pts',(2.35734085275916,1.28223802992782,13.8235269408515));
#448983=CARTESIAN_POINT('Ctrl Pts',(2.36907006162998,1.28359533536707,13.8362179249168));
#448984=CARTESIAN_POINT('Ctrl Pts',(2.37375135115543,1.26717131233872,13.8391868794938));
#448985=CARTESIAN_POINT('Ctrl Pts',(2.34660913718441,1.28099615453089,13.8400110824519));
#448986=CARTESIAN_POINT('Ctrl Pts',(2.35640634747062,1.27868606070842,13.8494522556836));
#448987=CARTESIAN_POINT('Ctrl Pts',(2.35607706120985,1.26523914812621,13.85569149686));
#448988=CARTESIAN_POINT('Ctrl Pts',(2.33107758588531,1.28591231566416,13.8586819406588));
#448989=CARTESIAN_POINT('Ctrl Pts',(2.33321516119045,1.28211932008681,13.868010383617));
#448990=CARTESIAN_POINT('Ctrl Pts',(2.33033843592131,1.27353926656026,13.8744918421245));
#448991=CARTESIAN_POINT('Ctrl Pts',(2.31575650694236,1.31319483823762,13.8587686893867));
#448992=CARTESIAN_POINT('Ctrl Pts',(2.31363790698273,1.31695404854444,13.8680909899357));
#448993=CARTESIAN_POINT('Ctrl Pts',(2.3048355821446,1.31895791454536,13.8745789365162));
#448994=CARTESIAN_POINT('Ctrl Pts',(2.31967473133409,1.32911534355549,13.8400379222776));
#448995=CARTESIAN_POINT('Ctrl Pts',(2.32282622863558,1.33867245078868,13.8494748685453));
#448996=CARTESIAN_POINT('Ctrl Pts',(2.31120161292003,1.34542740561683,13.8557104837033));
#448997=CARTESIAN_POINT('Ctrl Pts',(2.32636043967773,1.3376237760181,13.8235269408542));
#448998=CARTESIAN_POINT('Ctrl Pts',(2.33365570123341,1.34690794413509,13.8362179249195));
#448999=CARTESIAN_POINT('Ctrl Pts',(2.32211071702094,1.35949271046546,13.8391868794964));
#449000=CARTESIAN_POINT('Origin',(2.35986981879868,1.26038386943671,13.8235269408515));
#449001=CARTESIAN_POINT('Ctrl Pts',(2.39286675657413,1.28634909095845,13.7902140241682));
#449002=CARTESIAN_POINT('Ctrl Pts',(2.40433779006288,1.2876810016508,13.8026027327198));
#449003=CARTESIAN_POINT('Ctrl Pts',(2.40915682872283,1.27175759753398,13.8057746032556));
#449004=CARTESIAN_POINT('Ctrl Pts',(2.38102865958112,1.28497918497389,13.8013225161808));
#449005=CARTESIAN_POINT('Ctrl Pts',(2.39248796053712,1.28630972978154,13.8136962270464));
#449006=CARTESIAN_POINT('Ctrl Pts',(2.39730716051404,1.27040960660921,13.8168830918628));
#449007=CARTESIAN_POINT('Ctrl Pts',(2.369185459078,1.28360868841055,13.8124254880875));
#449008=CARTESIAN_POINT('Ctrl Pts',(2.38062798112169,1.28493728327733,13.8247886461867));
#449009=CARTESIAN_POINT('Ctrl Pts',(2.38545218759873,1.26906127640957,13.8279860620656));
#449010=CARTESIAN_POINT('Ctrl Pts',(2.35733694845468,1.28223757735948,13.8235227163065));
#449011=CARTESIAN_POINT('Ctrl Pts',(2.36875729232489,1.28356359739057,13.8358800595847));
#449012=CARTESIAN_POINT('Ctrl Pts',(2.3735916932322,1.26771259115546,13.8390832900376));
#449013=CARTESIAN_POINT('Origin',(2.39539963927864,1.26449538446932,13.7902182540695));
#449014=CARTESIAN_POINT('Ctrl Pts',(2.41319222293699,1.28870112932895,13.7382347919292));
#449015=CARTESIAN_POINT('Ctrl Pts',(2.42817973395686,1.29045964636402,13.7369371795942));
#449016=CARTESIAN_POINT('Ctrl Pts',(2.43517974500568,1.27702299416428,13.7364597369712));
#449017=CARTESIAN_POINT('Ctrl Pts',(2.4150712422314,1.28891857006904,13.7595490285574));
#449018=CARTESIAN_POINT('Ctrl Pts',(2.43041645958188,1.29071804523856,13.7633824266926));
#449019=CARTESIAN_POINT('Ctrl Pts',(2.43758682550866,1.27750897590027,13.7648920890506));
#449020=CARTESIAN_POINT('Ctrl Pts',(2.40548834677001,1.28780963421491,13.780380659011));
#449021=CARTESIAN_POINT('Ctrl Pts',(2.4187607817919,1.28937147754697,13.7901039518744));
#449022=CARTESIAN_POINT('Ctrl Pts',(2.42531453147815,1.2750350272724,13.7926933640892));
#449023=CARTESIAN_POINT('Ctrl Pts',(2.38883113529569,1.28588205607826,13.7936647693663));
#449024=CARTESIAN_POINT('Ctrl Pts',(2.39957137332815,1.28715509140806,13.8072068914933));
#449025=CARTESIAN_POINT('Ctrl Pts',(2.40403098918034,1.27070042348985,13.8104111085397));
#449026=CARTESIAN_POINT('Origin',(2.41598925678778,1.26687801744526,13.7435492065112));
#449027=CARTESIAN_POINT('Origin',(2.41598925678778,1.26687801744526,14.));
#449028=CARTESIAN_POINT('Origin',(2.41598925678778,1.26687801744526,12.5369868989719));
#449029=CARTESIAN_POINT('Ctrl Pts',(2.41327297583393,1.30503414316753,12.506462012331));
#449030=CARTESIAN_POINT('Ctrl Pts',(2.41902448424168,1.30814440666528,12.4999388158272));
#449031=CARTESIAN_POINT('Ctrl Pts',(2.41895643635458,1.30810760816924,12.4907030323752));
#449032=CARTESIAN_POINT('Ctrl Pts',(2.4214881807439,1.29460634419357,12.5042014951932));
#449033=CARTESIAN_POINT('Ctrl Pts',(2.42751896744353,1.29237683552585,12.4980716682127));
#449034=CARTESIAN_POINT('Ctrl Pts',(2.43070657950927,1.28637977836885,12.4907355092743));
#449035=CARTESIAN_POINT('Ctrl Pts',(2.41857050922723,1.28933255104575,12.5218047446509));
#449036=CARTESIAN_POINT('Ctrl Pts',(2.43021709765855,1.28736383348164,12.5216906929434));
#449037=CARTESIAN_POINT('Ctrl Pts',(2.43557754544319,1.27689309550011,12.5161988840776));
#449038=CARTESIAN_POINT('Ctrl Pts',(2.41342213315448,1.28872772857038,12.5369868989719));
#449039=CARTESIAN_POINT('Ctrl Pts',(2.42864730001847,1.29051653417306,12.5369868989719));
#449040=CARTESIAN_POINT('Ctrl Pts',(2.43559795424792,1.27685293518512,12.5369868989719));
#449041=CARTESIAN_POINT('Origin',(4.49626278878391E-31,-2.63684586248246E-31,
12.5));
#449042=CARTESIAN_POINT('Origin',(2.24498269238232,1.47011665264505,12.5));
#449043=CARTESIAN_POINT('',(2.24498269238232,1.47011665264505,12.5893111709658));
#449044=CARTESIAN_POINT('',(2.24498269238232,1.47011665264505,13.8235269408515));
#449045=CARTESIAN_POINT('',(2.24498269238232,1.47011665264505,12.5));
#449046=CARTESIAN_POINT('',(2.28005916367103,1.47711049716244,13.7902182540695));
#449047=CARTESIAN_POINT('',(2.24498269238232,1.47011665264505,13.8235269408515));
#449048=CARTESIAN_POINT('',(2.30038606421962,1.48116344709537,13.7435492065112));
#449049=CARTESIAN_POINT('Origin',(2.23351076640297,1.46782961485557,13.7445212918716));
#449050=CARTESIAN_POINT('',(2.30038606421962,1.48116344709537,12.5369868989719));
#449051=CARTESIAN_POINT('',(2.30038606421962,1.48116344709537,12.5));
#449052=CARTESIAN_POINT('Ctrl Pts',(2.30038606421962,1.48116344709537,12.5369868989719));
#449053=CARTESIAN_POINT('Ctrl Pts',(2.28193174289042,1.4774838678986,12.5544431401645));
#449054=CARTESIAN_POINT('Ctrl Pts',(2.26346422254012,1.47380165696898,12.5718848856037));
#449055=CARTESIAN_POINT('Ctrl Pts',(2.24498269238232,1.47011665264505,12.5893111709658));
#449056=CARTESIAN_POINT('Origin',(2.36130966352237,1.75215381130026,12.5));
#449057=CARTESIAN_POINT('',(2.24075887558448,1.56991110033551,13.7435492065112));
#449058=CARTESIAN_POINT('',(2.22932368520975,1.55262394585119,13.7902182540695));
#449059=CARTESIAN_POINT('Origin',(2.19927398130261,1.50719629168648,13.7418732680442));
#449060=CARTESIAN_POINT('',(2.20959091159277,1.52279291595643,13.8235269408515));
#449061=CARTESIAN_POINT('',(2.22932368520975,1.55262394585119,13.7902182540695));
#449062=CARTESIAN_POINT('',(2.20959091159277,1.52279291595643,12.5893111709658));
#449063=CARTESIAN_POINT('',(2.20959091159277,1.52279291595643,12.5));
#449064=CARTESIAN_POINT('',(2.24075887558448,1.56991110033551,12.5369868989719));
#449065=CARTESIAN_POINT('Ctrl Pts',(2.20959091159277,1.52279291595643,12.5893111709658));
#449066=CARTESIAN_POINT('Ctrl Pts',(2.21998796230228,1.53851066230841,12.5718848856037));
#449067=CARTESIAN_POINT('Ctrl Pts',(2.23037713159299,1.55421649392178,12.5544431401645));
#449068=CARTESIAN_POINT('Ctrl Pts',(2.24075887558448,1.56991110033551,12.5369868989719));
#449069=CARTESIAN_POINT('',(2.24075887558448,1.56991110033551,12.5));
#449070=CARTESIAN_POINT('Origin',(2.23826102351075,1.50382807196523,12.5));
#449071=CARTESIAN_POINT('',(2.21036815174207,1.48373882417756,13.8587068136939));
#449072=CARTESIAN_POINT('Ctrl Pts',(2.20959091158718,1.52279291595995,13.8235269408542));
#449073=CARTESIAN_POINT('Ctrl Pts',(2.20862416062284,1.52133142973009,13.8262006681044));
#449074=CARTESIAN_POINT('Ctrl Pts',(2.20777973774708,1.51973995932856,13.8288634856214));
#449075=CARTESIAN_POINT('Ctrl Pts',(2.20704962302618,1.51802915776954,13.8314912288862));
#449076=CARTESIAN_POINT('Ctrl Pts',(2.20629695005677,1.51626549782319,13.8342001611531));
#449077=CARTESIAN_POINT('Ctrl Pts',(2.20566446484758,1.51437325493347,13.8368750301949));
#449078=CARTESIAN_POINT('Ctrl Pts',(2.20517308358036,1.51233002866895,13.8394886372969));
#449079=CARTESIAN_POINT('Ctrl Pts',(2.20513513301317,1.51217222534838,13.8396904925131));
#449080=CARTESIAN_POINT('Ctrl Pts',(2.20509804442956,1.51201351262336,13.8398919674349));
#449081=CARTESIAN_POINT('Ctrl Pts',(2.20506183832379,1.51185387656114,13.8400930404591));
#449082=CARTESIAN_POINT('Ctrl Pts',(2.20449772283759,1.50936663931377,13.8432258934518));
#449083=CARTESIAN_POINT('Ctrl Pts',(2.20414961619355,1.50666819556832,13.8462331177034));
#449084=CARTESIAN_POINT('Ctrl Pts',(2.20412454525322,1.50383421189661,13.8489036603661));
#449085=CARTESIAN_POINT('Ctrl Pts',(2.20411634174978,1.50290689945849,13.849777493004));
#449086=CARTESIAN_POINT('Ctrl Pts',(2.2041428636101,1.50196528299333,13.85061494757));
#449087=CARTESIAN_POINT('Ctrl Pts',(2.20420824668703,1.5010126137019,13.8514076489583));
#449088=CARTESIAN_POINT('Ctrl Pts',(2.20434654132439,1.49899758075505,13.8530843267192));
#449089=CARTESIAN_POINT('Ctrl Pts',(2.20467522981035,1.49673537254486,13.8546805203176));
#449090=CARTESIAN_POINT('Ctrl Pts',(2.20531026306347,1.49437690575371,13.8559412814273));
#449091=CARTESIAN_POINT('Ctrl Pts',(2.20539525110736,1.49406126641016,13.8561100121513));
#449092=CARTESIAN_POINT('Ctrl Pts',(2.20548565668459,1.49374393581815,13.8562727473908));
#449093=CARTESIAN_POINT('Ctrl Pts',(2.20558168565612,1.4934252993382,13.8564289040185));
#449094=CARTESIAN_POINT('Ctrl Pts',(2.20601717594647,1.49198028653681,13.8571370725437));
#449095=CARTESIAN_POINT('Ctrl Pts',(2.20657815194651,1.49048367427338,13.8577210840554));
#449096=CARTESIAN_POINT('Ctrl Pts',(2.20727028937841,1.48900393683601,13.8581177131616));
#449097=CARTESIAN_POINT('Ctrl Pts',(2.20746521910188,1.48858719184263,13.8582294175695));
#449098=CARTESIAN_POINT('Ctrl Pts',(2.20767037977277,1.48817174305277,13.8583265086086));
#449099=CARTESIAN_POINT('Ctrl Pts',(2.20788547823267,1.48775899017047,13.8584082369006));
#449100=CARTESIAN_POINT('Ctrl Pts',(2.20819451703861,1.48716597496268,13.8585256585398));
#449101=CARTESIAN_POINT('Ctrl Pts',(2.20852819823668,1.48657130149863,13.8586122832068));
#449102=CARTESIAN_POINT('Ctrl Pts',(2.208878542435,1.48599080410042,13.8586682984299));
#449103=CARTESIAN_POINT('Ctrl Pts',(2.20915878306515,1.48552646372471,13.8587131050557));
#449104=CARTESIAN_POINT('Ctrl Pts',(2.20945257987857,1.48506594398009,13.8587357943552));
#449105=CARTESIAN_POINT('Ctrl Pts',(2.20976039474481,1.48460946252997,13.8587355499465));
#449106=CARTESIAN_POINT('Ctrl Pts',(2.20995934283152,1.48431442768573,13.8587353919793));
#449107=CARTESIAN_POINT('Ctrl Pts',(2.21016196328106,1.48402424862251,13.8587257282814));
#449108=CARTESIAN_POINT('Ctrl Pts',(2.21036815174207,1.48373882417756,13.8587068136939));
#449109=CARTESIAN_POINT('Ctrl Pts',(2.21036815174207,1.48373882417756,13.8587068136939));
#449110=CARTESIAN_POINT('Ctrl Pts',(2.21104629434983,1.48280007873827,13.8586446046466));
#449111=CARTESIAN_POINT('Ctrl Pts',(2.21176298558344,1.48191270074552,13.858482427929));
#449112=CARTESIAN_POINT('Ctrl Pts',(2.21251494810213,1.48107364964105,13.8582284286032));
#449113=CARTESIAN_POINT('Ctrl Pts',(2.21328637417442,1.48021288081029,13.8579678548414));
#449114=CARTESIAN_POINT('Ctrl Pts',(2.21409794606332,1.47940189260247,13.857615680862));
#449115=CARTESIAN_POINT('Ctrl Pts',(2.21491081898393,1.47866580353012,13.8571944833187));
#449116=CARTESIAN_POINT('Ctrl Pts',(2.21693942649115,1.47682881796904,13.8561433417727));
#449117=CARTESIAN_POINT('Ctrl Pts',(2.21906780994789,1.47536882349349,13.8546163505475));
#449118=CARTESIAN_POINT('Ctrl Pts',(2.22109574890803,1.47423415154825,13.8528973491086));
#449119=CARTESIAN_POINT('Ctrl Pts',(2.2214662234366,1.47402686372437,13.8525833129072));
#449120=CARTESIAN_POINT('Ctrl Pts',(2.22183334150934,1.47383029191881,13.8522628768812));
#449121=CARTESIAN_POINT('Ctrl Pts',(2.22219590503271,1.47364394373746,13.851937733538));
#449122=CARTESIAN_POINT('Ctrl Pts',(2.22441003016648,1.47250594124864,13.8499521282529));
#449123=CARTESIAN_POINT('Ctrl Pts',(2.22667620572651,1.47163974725192,13.847639871647));
#449124=CARTESIAN_POINT('Ctrl Pts',(2.22884664546143,1.47101584018038,13.8452109780794));
#449125=CARTESIAN_POINT('Ctrl Pts',(2.22982317122403,1.47073513147467,13.8441181685877));
#449126=CARTESIAN_POINT('Ctrl Pts',(2.23078036982602,1.47050275273326,13.8430021611332));
#449127=CARTESIAN_POINT('Ctrl Pts',(2.23170603279204,1.47031295226536,13.8418824960098));
#449128=CARTESIAN_POINT('Ctrl Pts',(2.23388738120913,1.46986568261602,13.8392439765549));
#449129=CARTESIAN_POINT('Ctrl Pts',(2.23599712352092,1.4696297725911,13.8364981347964));
#449130=CARTESIAN_POINT('Ctrl Pts',(2.23803703636739,1.46957058972445,13.8336931113419));
#449131=CARTESIAN_POINT('Ctrl Pts',(2.24002378193342,1.4695129493708,13.8309611966328));
#449132=CARTESIAN_POINT('Ctrl Pts',(2.24194629785291,1.46962345039488,13.8281701127185));
#449133=CARTESIAN_POINT('Ctrl Pts',(2.24379299532685,1.46990710444376,13.825358068512));
#449134=CARTESIAN_POINT('Ctrl Pts',(2.2441933613322,1.46996860094768,13.8247484142932));
#449135=CARTESIAN_POINT('Ctrl Pts',(2.24459004640973,1.4700383635589,13.8241378483365));
#449136=CARTESIAN_POINT('Ctrl Pts',(2.24498269238232,1.47011665264505,13.8235269408515));
#449137=CARTESIAN_POINT('',(2.20966053613784,1.48475963611651,12.5969504640361));
#449138=CARTESIAN_POINT('Origin',(2.23828859526251,1.50384636079555,12.584524458991));
#449139=CARTESIAN_POINT('Origin',(2.23828859526251,1.50384636079555,12.584524458991));
#449140=CARTESIAN_POINT('Ctrl Pts',(2.20959091159277,1.52279291595643,12.5893111709658));
#449141=CARTESIAN_POINT('Ctrl Pts',(2.20333791462155,1.51333994481304,12.5770542771492));
#449142=CARTESIAN_POINT('Ctrl Pts',(2.21506416483589,1.50192509786858,12.5737548217797));
#449143=CARTESIAN_POINT('Ctrl Pts',(2.22326411740067,1.54346339133561,12.5663937883685));
#449144=CARTESIAN_POINT('Ctrl Pts',(2.21700314386343,1.53399836161473,12.5540940315304));
#449145=CARTESIAN_POINT('Ctrl Pts',(2.22876797124263,1.52255044337381,12.5508374392248));
#449146=CARTESIAN_POINT('Ctrl Pts',(2.23692352711152,1.56411301045852,12.5434499600945));
#449147=CARTESIAN_POINT('Ctrl Pts',(2.23064219691974,1.55461720655537,12.5311293540532));
#449148=CARTESIAN_POINT('Ctrl Pts',(2.24245740601019,1.54315629041795,12.5278936106989));
#449149=CARTESIAN_POINT('Ctrl Pts',(2.25057022139251,1.58474340702428,12.5204817579905));
#449150=CARTESIAN_POINT('Ctrl Pts',(2.24425780290893,1.57520060538135,12.5081597038247));
#449151=CARTESIAN_POINT('Ctrl Pts',(2.25613357461923,1.56374416216455,12.5049254088044));
#449152=CARTESIAN_POINT('Ctrl Pts',(2.24075887558448,1.56991110033551,12.5369868989719));
#449153=CARTESIAN_POINT('Ctrl Pts',(2.2412727911519,1.57068801214536,12.5342545179733));
#449154=CARTESIAN_POINT('Ctrl Pts',(2.24186729187868,1.57136063834112,12.5314872231885));
#449155=CARTESIAN_POINT('Ctrl Pts',(2.24255077409794,1.57185406834232,12.5287124745063));
#449156=CARTESIAN_POINT('Ctrl Pts',(2.2431671722883,1.57229906800908,12.5262100684184));
#449157=CARTESIAN_POINT('Ctrl Pts',(2.24385589586104,1.57259707501921,12.5237004536639));
#449158=CARTESIAN_POINT('Ctrl Pts',(2.24465509548773,1.57269236682436,12.5212220730815));
#449159=CARTESIAN_POINT('Ctrl Pts',(2.24526695193824,1.5727653209446,12.5193246583486));
#449160=CARTESIAN_POINT('Ctrl Pts',(2.2459509485987,1.57271970086603,12.517417831369));
#449161=CARTESIAN_POINT('Ctrl Pts',(2.24671988473605,1.57245912089718,12.5155812248348));
#449162=CARTESIAN_POINT('Ctrl Pts',(2.24704745566362,1.57234811242983,12.5147988205793));
#449163=CARTESIAN_POINT('Ctrl Pts',(2.24739086289924,1.57219824259547,12.5140295443047));
#449164=CARTESIAN_POINT('Ctrl Pts',(2.2477527956281,1.57200333889459,12.5132817086137));
#449165=CARTESIAN_POINT('Ctrl Pts',(2.24830053185208,1.5717083785093,12.5121499604604));
#449166=CARTESIAN_POINT('Ctrl Pts',(2.24889913361807,1.57129761210048,12.5110494206568));
#449167=CARTESIAN_POINT('Ctrl Pts',(2.2495385308929,1.57073518589319,12.5100666561695));
#449168=CARTESIAN_POINT('Ctrl Pts',(2.2499056713357,1.57041224206012,12.5095023550641));
#449169=CARTESIAN_POINT('Ctrl Pts',(2.25029007303371,1.57003507410021,12.5089719619137));
#449170=CARTESIAN_POINT('Ctrl Pts',(2.25068005762558,1.56960619264217,12.5085043804652));
#449171=CARTESIAN_POINT('Ctrl Pts',(2.25125074927671,1.56897858049405,12.5078201359221));
#449172=CARTESIAN_POINT('Ctrl Pts',(2.25184905478605,1.56822121101344,12.5072563000949));
#449173=CARTESIAN_POINT('Ctrl Pts',(2.25242777467969,1.56738017470561,12.5068768744332));
#449174=CARTESIAN_POINT('Ctrl Pts',(2.25284507156222,1.56677372963052,12.5066032824114));
#449175=CARTESIAN_POINT('Ctrl Pts',(2.25325956584798,1.56611316251982,12.5064197834844));
#449176=CARTESIAN_POINT('Ctrl Pts',(2.25365030060876,1.56543673503369,12.5063282718343));
#449177=CARTESIAN_POINT('Ctrl Pts',(2.25422065239109,1.56444936032059,12.5061946931565));
#449178=CARTESIAN_POINT('Ctrl Pts',(2.25475349020623,1.5634076193054,12.5062515701262));
#449179=CARTESIAN_POINT('Ctrl Pts',(2.25522951325349,1.56238320646031,12.5064436508398));
#449180=CARTESIAN_POINT('',(2.21506416483589,1.50192509786858,12.5737548217797));
#449181=CARTESIAN_POINT('Origin',(2.22793978322027,1.51065541580206,12.5893111709658));
#449182=CARTESIAN_POINT('Ctrl Pts',(2.25522951325349,1.56238320646031,12.5064436508398));
#449183=CARTESIAN_POINT('Ctrl Pts',(2.24928439834657,1.553433569792,12.5164271754438));
#449184=CARTESIAN_POINT('Ctrl Pts',(2.24333675276147,1.54448050109937,12.5264061185523));
#449185=CARTESIAN_POINT('Ctrl Pts',(2.23738648815821,1.53552387898569,12.536380305637));
#449186=CARTESIAN_POINT('Ctrl Pts',(2.22994986424784,1.52432991794228,12.5488460165097));
#449187=CARTESIAN_POINT('Ctrl Pts',(2.22250914723241,1.51313040318678,12.5613043021964));
#449188=CARTESIAN_POINT('Ctrl Pts',(2.21506416483589,1.50192509786858,12.5737548217797));
#449189=CARTESIAN_POINT('Ctrl Pts',(2.24498269238232,1.47011665264505,12.5893111709658));
#449190=CARTESIAN_POINT('Ctrl Pts',(2.2338675256558,1.46790041637572,12.5770542771492));
#449191=CARTESIAN_POINT('Ctrl Pts',(2.22773157341711,1.48307123589806,12.5737548217797));
#449192=CARTESIAN_POINT('Ctrl Pts',(2.2346123385011,1.46804892348157,12.5928319619712));
#449193=CARTESIAN_POINT('Ctrl Pts',(2.22650524262674,1.4697543304287,12.5821634970843));
#449194=CARTESIAN_POINT('Ctrl Pts',(2.22395575018039,1.48230875556751,12.5773203894503));
#449195=CARTESIAN_POINT('Ctrl Pts',(2.21831603931396,1.4719238082725,12.5969440695591));
#449196=CARTESIAN_POINT('Ctrl Pts',(2.21605911440408,1.47525019257127,12.5878292599214));
#449197=CARTESIAN_POINT('Ctrl Pts',(2.21814788990466,1.48369183405955,12.5813877129824));
#449198=CARTESIAN_POINT('Ctrl Pts',(2.20120771663137,1.49729072650333,12.596957478804));
#449199=CARTESIAN_POINT('Ctrl Pts',(2.20344802859256,1.49398897008205,12.5878468778671));
#449200=CARTESIAN_POINT('Ctrl Pts',(2.21202952953643,1.49277434113131,12.5814011370086));
#449201=CARTESIAN_POINT('Ctrl Pts',(2.20374844885825,1.51396057014061,12.5928371701607));
#449202=CARTESIAN_POINT('Ctrl Pts',(2.20227016042516,1.50581503584185,12.5821692192952));
#449203=CARTESIAN_POINT('Ctrl Pts',(2.21292407734148,1.49870744297872,12.5773318885715));
#449204=CARTESIAN_POINT('Ctrl Pts',(2.20959091159272,1.52279291595645,12.5893111709658));
#449205=CARTESIAN_POINT('Ctrl Pts',(2.2033379146215,1.51333994481307,12.5770542771492));
#449206=CARTESIAN_POINT('Ctrl Pts',(2.21506416483584,1.5019250978686,12.5737548217797));
#449207=CARTESIAN_POINT('',(2.22773157341711,1.48307123589806,12.5737548217797));
#449208=CARTESIAN_POINT('Origin',(2.24068082430451,1.49169196100996,12.5893111709658));
#449209=CARTESIAN_POINT('Ctrl Pts',(2.21506416483584,1.5019250978686,12.5737548217797));
#449210=CARTESIAN_POINT('Ctrl Pts',(2.21448430274599,1.50110773651169,12.5746934679442));
#449211=CARTESIAN_POINT('Ctrl Pts',(2.21399205215106,1.50009727879856,12.5756680099006));
#449212=CARTESIAN_POINT('Ctrl Pts',(2.2136404235203,1.49901014450419,12.5765688348656));
#449213=CARTESIAN_POINT('Ctrl Pts',(2.21354733373296,1.49872233773472,12.5768073183026));
#449214=CARTESIAN_POINT('Ctrl Pts',(2.21346388168446,1.49842929322309,12.5770407398754));
#449215=CARTESIAN_POINT('Ctrl Pts',(2.21339051374517,1.49813334003695,12.5772674179684));
#449216=CARTESIAN_POINT('Ctrl Pts',(2.21308943156186,1.49691882819014,12.5781976435658));
#449217=CARTESIAN_POINT('Ctrl Pts',(2.21295201958902,1.49558363703061,12.5790594849312));
#449218=CARTESIAN_POINT('Ctrl Pts',(2.21303559156923,1.49421297717208,12.5797571720116));
#449219=CARTESIAN_POINT('Ctrl Pts',(2.21309004171931,1.49331994298971,12.580211740231));
#449220=CARTESIAN_POINT('Ctrl Pts',(2.21325951191965,1.4923724110211,12.5806009430798));
#449221=CARTESIAN_POINT('Ctrl Pts',(2.21354951215474,1.49144020260665,12.5808812374708));
#449222=CARTESIAN_POINT('Ctrl Pts',(2.21379871856325,1.49063912632172,12.5811221033394));
#449223=CARTESIAN_POINT('Ctrl Pts',(2.21414214140216,1.48983299946668,12.581287365893));
#449224=CARTESIAN_POINT('Ctrl Pts',(2.21456806822683,1.48907058906311,12.581359338449));
#449225=CARTESIAN_POINT('Ctrl Pts',(2.21462726326041,1.48896462976018,12.5813693411482));
#449226=CARTESIAN_POINT('Ctrl Pts',(2.21468801232813,1.48885946989651,12.5813775999465));
#449227=CARTESIAN_POINT('Ctrl Pts',(2.21475024429204,1.48875519361755,12.5813841266931));
#449228=CARTESIAN_POINT('Ctrl Pts',(2.21485582834561,1.48857827629834,12.5813952001081));
#449229=CARTESIAN_POINT('Ctrl Pts',(2.21496691094072,1.48840302952041,12.5814007534795));
#449230=CARTESIAN_POINT('Ctrl Pts',(2.21508361026391,1.48822963519001,12.5814005856065));
#449231=CARTESIAN_POINT('Ctrl Pts',(2.21561781413902,1.48743590373826,12.5813998171494));
#449232=CARTESIAN_POINT('Ctrl Pts',(2.21623252439138,1.48673564171136,12.58127954464));
#449233=CARTESIAN_POINT('Ctrl Pts',(2.21690201403878,1.48611330440799,12.5810700125799));
#449234=CARTESIAN_POINT('Ctrl Pts',(2.21771068130532,1.4853615918043,12.5808169217085));
#449235=CARTESIAN_POINT('Ctrl Pts',(2.21861073881532,1.48473576048663,12.5804173076348));
#449236=CARTESIAN_POINT('Ctrl Pts',(2.21950843991555,1.48426927565054,12.5799304713245));
#449237=CARTESIAN_POINT('Ctrl Pts',(2.22062097438374,1.48369115398075,12.5793271277669));
#449238=CARTESIAN_POINT('Ctrl Pts',(2.22178405448073,1.4832933380731,12.5785808224116));
#449239=CARTESIAN_POINT('Ctrl Pts',(2.22293838963342,1.48306258665214,12.5777485681082));
#449240=CARTESIAN_POINT('Ctrl Pts',(2.22465847547777,1.48271874175419,12.576508418016));
#449241=CARTESIAN_POINT('Ctrl Pts',(2.2263433132185,1.4827420075699,12.5750928681475));
#449242=CARTESIAN_POINT('Ctrl Pts',(2.22773157341711,1.48307123589806,12.5737548217797));
#449243=CARTESIAN_POINT('Ctrl Pts',(2.22773157341711,1.48307123589806,12.5737548217797));
#449244=CARTESIAN_POINT('Ctrl Pts',(2.2338675256558,1.46790041637572,12.5770542771492));
#449245=CARTESIAN_POINT('Ctrl Pts',(2.24498269238232,1.47011665264505,12.5893111709658));
#449246=CARTESIAN_POINT('Ctrl Pts',(2.25200284966887,1.48796205416098,12.5508408821982));
#449247=CARTESIAN_POINT('Ctrl Pts',(2.25815483335804,1.47274302589642,12.55409748406));
#449248=CARTESIAN_POINT('Ctrl Pts',(2.26928418019057,1.47496208951563,12.5663972313419));
#449249=CARTESIAN_POINT('Ctrl Pts',(2.27625064893766,1.49284693843918,12.52790050457));
#449250=CARTESIAN_POINT('Ctrl Pts',(2.28239562508524,1.47757636066729,12.5311362602938));
#449251=CARTESIAN_POINT('Ctrl Pts',(2.29356115179089,1.47980263813662,12.5434568539655));
#449252=CARTESIAN_POINT('Ctrl Pts',(2.30047679842188,1.4977263363042,12.5049357605811));
#449253=CARTESIAN_POINT('Ctrl Pts',(2.30659474988991,1.48240138753351,12.5081700652078));
#449254=CARTESIAN_POINT('Ctrl Pts',(2.31781552729765,1.48463868135671,12.5204921097672));
#449255=CARTESIAN_POINT('Ctrl Pts',(2.29888601479652,1.49740593435784,12.5064436508395));
#449256=CARTESIAN_POINT('Ctrl Pts',(2.29971613400763,1.49651164699579,12.5062361689309));
#449257=CARTESIAN_POINT('Ctrl Pts',(2.30054125565682,1.49554626319414,12.5061871075061));
#449258=CARTESIAN_POINT('Ctrl Pts',(2.30128613793853,1.49456842525894,12.5063648335164));
#449259=CARTESIAN_POINT('Ctrl Pts',(2.30162450941712,1.49412423095323,12.5064455676329));
#449260=CARTESIAN_POINT('Ctrl Pts',(2.30195086752871,1.49367113760007,12.506574497099));
#449261=CARTESIAN_POINT('Ctrl Pts',(2.30225036625179,1.49322795824661,12.5067492519495));
#449262=CARTESIAN_POINT('Ctrl Pts',(2.30285222056147,1.49233737213291,12.5071004286051));
#449263=CARTESIAN_POINT('Ctrl Pts',(2.303367068467,1.49145362499365,12.5076537929612));
#449264=CARTESIAN_POINT('Ctrl Pts',(2.30376444064075,1.49064780789172,12.5083435010503));
#449265=CARTESIAN_POINT('Ctrl Pts',(2.30378945759384,1.49059707688947,12.5083869222963));
#449266=CARTESIAN_POINT('Ctrl Pts',(2.3038140009612,1.49054664394855,12.5084308732336));
#449267=CARTESIAN_POINT('Ctrl Pts',(2.30383806021042,1.49049652217092,12.5084753333615));
#449268=CARTESIAN_POINT('Ctrl Pts',(2.30403104714423,1.49009447936021,12.508831962269));
#449269=CARTESIAN_POINT('Ctrl Pts',(2.30419796614161,1.48970485342778,12.509227847131));
#449270=CARTESIAN_POINT('Ctrl Pts',(2.30433642763762,1.48934033262371,12.5096423454524));
#449271=CARTESIAN_POINT('Ctrl Pts',(2.30477030468563,1.48819808575393,12.5109411997424));
#449272=CARTESIAN_POINT('Ctrl Pts',(2.30496047709166,1.4872355284592,12.5124831113042));
#449273=CARTESIAN_POINT('Ctrl Pts',(2.30499933195228,1.48643215508692,12.5140723025007));
#449274=CARTESIAN_POINT('Ctrl Pts',(2.30500297269527,1.48635687812203,12.5142212114565));
#449275=CARTESIAN_POINT('Ctrl Pts',(2.30500530968998,1.48628298260781,12.5143705582413));
#449276=CARTESIAN_POINT('Ctrl Pts',(2.30500643395424,1.48621044373511,12.5145201959299));
#449277=CARTESIAN_POINT('Ctrl Pts',(2.30502087680249,1.4852785739163,12.5164425148273));
#449278=CARTESIAN_POINT('Ctrl Pts',(2.30484641180203,1.48453883089135,12.5184635205941));
#449279=CARTESIAN_POINT('Ctrl Pts',(2.30454809418324,1.48392871829592,12.5205025929157));
#449280=CARTESIAN_POINT('Ctrl Pts',(2.30437505814013,1.48357482880796,12.5216853356836));
#449281=CARTESIAN_POINT('Ctrl Pts',(2.30416109936197,1.48326497981927,12.5228750347131));
#449282=CARTESIAN_POINT('Ctrl Pts',(2.30392276286129,1.48299147742258,12.5240609649613));
#449283=CARTESIAN_POINT('Ctrl Pts',(2.30333777870667,1.48232018046282,12.5269717671326));
#449284=CARTESIAN_POINT('Ctrl Pts',(2.3025816343861,1.48185578326791,12.5299036066169));
#449285=CARTESIAN_POINT('Ctrl Pts',(2.30171096423685,1.48153269563683,12.5328133004019));
#449286=CARTESIAN_POINT('Ctrl Pts',(2.3012929918676,1.48137759476108,12.5342101228451));
#449287=CARTESIAN_POINT('Ctrl Pts',(2.30084896552946,1.48125574437044,12.5356023438238));
#449288=CARTESIAN_POINT('Ctrl Pts',(2.30038606421962,1.48116344709537,12.5369868989719));
#449289=CARTESIAN_POINT('Origin',(14.8001517004723,3.96807264688619,-1.2394292610445));
#449290=CARTESIAN_POINT('Ctrl Pts',(2.24073578439569,1.56987626417708,12.5369868989719));
#449291=CARTESIAN_POINT('Ctrl Pts',(2.24922264007692,1.58265345417846,12.5369868989719));
#449292=CARTESIAN_POINT('Ctrl Pts',(2.24016824163897,1.59503493925143,12.5369868989719));
#449293=CARTESIAN_POINT('Ctrl Pts',(2.24360461838103,1.57419549074474,12.5218025310016));
#449294=CARTESIAN_POINT('Ctrl Pts',(2.24711771582048,1.58547884175789,12.5216901060417));
#449295=CARTESIAN_POINT('Ctrl Pts',(2.2401958557581,1.59499720611652,12.5161920673677));
#449296=CARTESIAN_POINT('Ctrl Pts',(2.2496285404189,1.5744155690873,12.5042015548895));
#449297=CARTESIAN_POINT('Ctrl Pts',(2.25036629956198,1.58080564392752,12.4980677368514));
#449298=CARTESIAN_POINT('Ctrl Pts',(2.24645464249712,1.58636349591643,12.4907278922778));
#449299=CARTESIAN_POINT('Ctrl Pts',(2.25521307217858,1.56237181636108,12.506463626192));
#449300=CARTESIAN_POINT('Ctrl Pts',(2.26059126639978,1.56609773440305,12.4999376786891));
#449301=CARTESIAN_POINT('Ctrl Pts',(2.26052557957726,1.56605222773164,12.4906970594712));
#449302=CARTESIAN_POINT('Origin',(2.22241000395697,1.58204860048988,12.5369868989719));
#449303=CARTESIAN_POINT('Origin',(2.22241000395697,1.58204860048988,14.));
#449304=CARTESIAN_POINT('Origin',(2.22241000395697,1.58204860048988,13.7435492065112));
#449305=CARTESIAN_POINT('Ctrl Pts',(2.22709859085591,1.549260207618,13.793642941384));
#449306=CARTESIAN_POINT('Ctrl Pts',(2.23308648110711,1.55826306212895,13.8071662555867));
#449307=CARTESIAN_POINT('Ctrl Pts',(2.22044725012617,1.56967661652036,13.8103758687955));
#449308=CARTESIAN_POINT('Ctrl Pts',(2.23626854215468,1.56312288046277,13.7804579775006));
#449309=CARTESIAN_POINT('Ctrl Pts',(2.24364861378668,1.57423720520318,13.7901904343351));
#449310=CARTESIAN_POINT('Ctrl Pts',(2.23381737153057,1.58654990595751,13.7927914348263));
#449311=CARTESIAN_POINT('Ctrl Pts',(2.24166723755664,1.57128435769853,13.7597120340895));
#449312=CARTESIAN_POINT('Ctrl Pts',(2.25020328498712,1.58414993130553,13.7635825532445));
#449313=CARTESIAN_POINT('Ctrl Pts',(2.24168168172328,1.59651594092699,13.7651073818884));
#449314=CARTESIAN_POINT('Ctrl Pts',(2.24061004938019,1.56968615357964,13.7381884353898));
#449315=CARTESIAN_POINT('Ctrl Pts',(2.24894704369041,1.58225008753751,13.7368803041982));
#449316=CARTESIAN_POINT('Ctrl Pts',(2.24014122811892,1.59456460130136,13.7363986145813));
#449317=CARTESIAN_POINT('Origin',(2.21097481358224,1.56476144600556,13.7902182540695));
#449318=CARTESIAN_POINT('Ctrl Pts',(2.20958873934121,1.5227896334297,13.8235227101244));
#449319=CARTESIAN_POINT('Ctrl Pts',(2.21593542405313,1.53237620119335,13.8358800583119));
#449320=CARTESIAN_POINT('Ctrl Pts',(2.20398339878359,1.54385553658409,13.8390832900376));
#449321=CARTESIAN_POINT('Ctrl Pts',(2.21616923917098,1.53273770717716,13.8124254819052));
#449322=CARTESIAN_POINT('Ctrl Pts',(2.22252824882269,1.54234289207307,13.8247886449158));
#449323=CARTESIAN_POINT('Ctrl Pts',(2.21054931507098,1.55382443932396,13.8279860620657));
#449324=CARTESIAN_POINT('Ctrl Pts',(2.22274678983482,1.54268132252161,13.8013225099955));
#449325=CARTESIAN_POINT('Ctrl Pts',(2.22911512566644,1.55230059133835,13.8136962257787));
#449326=CARTESIAN_POINT('Ctrl Pts',(2.21711241802951,1.56378857785748,13.8168830918626));
#449327=CARTESIAN_POINT('Ctrl Pts',(2.22932150608024,1.55262065293264,13.7902140179785));
#449328=CARTESIAN_POINT('Ctrl Pts',(2.23569636532044,1.562249768739,13.802602731458));
#449329=CARTESIAN_POINT('Ctrl Pts',(2.22367281973861,1.57374813836965,13.8057746032558));
#449330=CARTESIAN_POINT('Origin',(2.19124203996526,1.5349304161108,13.8235269408515));
#449331=CARTESIAN_POINT('Ctrl Pts',(2.24498269238232,1.47011665264505,13.8235269408515));
#449332=CARTESIAN_POINT('Ctrl Pts',(2.25656224028431,1.47242548117405,13.8362179249168));
#449333=CARTESIAN_POINT('Ctrl Pts',(2.26256666355505,1.45643767628273,13.8391868794938));
#449334=CARTESIAN_POINT('Ctrl Pts',(2.23438791007974,1.46800417503834,13.8400110824519));
#449335=CARTESIAN_POINT('Ctrl Pts',(2.24434081504938,1.46650033145368,13.8494522556837));
#449336=CARTESIAN_POINT('Ctrl Pts',(2.24510867267189,1.45307132247656,13.85569149686));
#449337=CARTESIAN_POINT('Ctrl Pts',(2.21850732596451,1.47163801243222,13.8586819406588));
#449338=CARTESIAN_POINT('Ctrl Pts',(2.22094695301616,1.4680318699664,13.868010383617));
#449339=CARTESIAN_POINT('Ctrl Pts',(2.21877915382878,1.45924588604451,13.8744918421245));
#449340=CARTESIAN_POINT('Ctrl Pts',(2.20101344777952,1.49758094449465,13.8587686893867));
#449341=CARTESIAN_POINT('Ctrl Pts',(2.19859548674768,1.50115496077446,13.8680909899357));
#449342=CARTESIAN_POINT('Ctrl Pts',(2.18965911723724,1.50243468788547,13.8745789365163));
#449343=CARTESIAN_POINT('Ctrl Pts',(2.20362096562065,1.51376784730737,13.8400379222776));
#449344=CARTESIAN_POINT('Ctrl Pts',(2.2059829836115,1.52355003034179,13.8494748685453));
#449345=CARTESIAN_POINT('Ctrl Pts',(2.19384645631734,1.52933499451651,13.8557104837033));
#449346=CARTESIAN_POINT('Ctrl Pts',(2.20959091158718,1.52279291595995,13.8235269408542));
#449347=CARTESIAN_POINT('Ctrl Pts',(2.2161051528703,1.53264082331612,13.8362179249195));
#449348=CARTESIAN_POINT('Ctrl Pts',(2.20357280835321,1.54424269148298,13.8391868794964));
#449349=CARTESIAN_POINT('Origin',(2.24928456046012,1.44854134428013,13.8235269408515));
#449350=CARTESIAN_POINT('Ctrl Pts',(2.28005529704379,1.47710972542656,13.7902140241682));
#449351=CARTESIAN_POINT('Ctrl Pts',(2.29137959852863,1.47937220001718,13.8026027327198));
#449352=CARTESIAN_POINT('Ctrl Pts',(2.29748050749618,1.46389457610252,13.8057746032556));
#449353=CARTESIAN_POINT('Ctrl Pts',(2.2683682503973,1.4747794628867,13.8013225161807));
#449354=CARTESIAN_POINT('Ctrl Pts',(2.27968096972068,1.47703961982715,13.8136962270464));
#449355=CARTESIAN_POINT('Ctrl Pts',(2.28578014185534,1.46158521254037,13.8168830918628));
#449356=CARTESIAN_POINT('Ctrl Pts',(2.25667616535983,1.4724481957497,13.8124254880876));
#449357=CARTESIAN_POINT('Ctrl Pts',(2.26797232053967,1.47470504160042,13.8247886461868));
#449358=CARTESIAN_POINT('Ctrl Pts',(2.27407451681297,1.45927507844944,13.8279860620656));
#449359=CARTESIAN_POINT('Ctrl Pts',(2.2449788379576,1.47011588334553,13.8235227163065));
#449360=CARTESIAN_POINT('Ctrl Pts',(2.256253098633,1.47236835520109,13.8358800595847));
#449361=CARTESIAN_POINT('Ctrl Pts',(2.26236341763183,1.45696414043593,13.8390832900376));
#449362=CARTESIAN_POINT('Origin',(2.28436103174884,1.45553518879752,13.7902182540695));
#449363=CARTESIAN_POINT('Ctrl Pts',(2.30012141913163,1.48111065178441,13.7382347919292));
#449364=CARTESIAN_POINT('Ctrl Pts',(2.31491572498132,1.48408493878449,13.7369371795943));
#449365=CARTESIAN_POINT('Ctrl Pts',(2.3229876559649,1.47126356182191,13.7364597369711));
#449366=CARTESIAN_POINT('Ctrl Pts',(2.30197646270541,1.48148052652483,13.7595490285573));
#449367=CARTESIAN_POINT('Ctrl Pts',(2.3171239461792,1.48452479176127,13.7633824266926));
#449368=CARTESIAN_POINT('Ctrl Pts',(2.32534711508297,1.47194412590101,13.7648920890506));
#449369=CARTESIAN_POINT('Ctrl Pts',(2.29251584210512,1.47959418561992,13.7803806590111));
#449370=CARTESIAN_POINT('Ctrl Pts',(2.30561680946336,1.4822326587167,13.7901039518744));
#449371=CARTESIAN_POINT('Ctrl Pts',(2.31331730587864,1.4684781032392,13.7926933640892));
#449372=CARTESIAN_POINT('Ctrl Pts',(2.27607117164073,1.47631530396733,13.7936647693663));
#449373=CARTESIAN_POINT('Ctrl Pts',(2.28667190821947,1.47845953248422,13.8072068914933));
#449374=CARTESIAN_POINT('Ctrl Pts',(2.29245789326083,1.46242311620913,13.8104111085397));
#449375=CARTESIAN_POINT('Origin',(2.30468793229742,1.45958813873046,13.7435492065112));
#449376=CARTESIAN_POINT('Origin',(2.30468793229742,1.45958813873046,14.));
#449377=CARTESIAN_POINT('Origin',(2.30468793229742,1.45958813873046,12.5369868989719));
#449378=CARTESIAN_POINT('Ctrl Pts',(2.2988706110738,1.49739590097759,12.506462012331));
#449379=CARTESIAN_POINT('Ctrl Pts',(2.30434946646245,1.50096461665976,12.4999388158272));
#449380=CARTESIAN_POINT('Ctrl Pts',(2.30428464441813,1.50092239407316,12.4907030323752));
#449381=CARTESIAN_POINT('Ctrl Pts',(2.3079084429905,1.4876724151109,12.5042014951932));
#449382=CARTESIAN_POINT('Ctrl Pts',(2.31410088839908,1.48594189005247,12.4980716682127));
#449383=CARTESIAN_POINT('Ctrl Pts',(2.31776670978086,1.48022460758411,12.4907355092744));
#449384=CARTESIAN_POINT('Ctrl Pts',(2.30543034288613,1.48217835275976,12.5218047446509));
#449385=CARTESIAN_POINT('Ctrl Pts',(2.31719864701337,1.48116549101972,12.5216906929434));
#449386=CARTESIAN_POINT('Ctrl Pts',(2.32339472070133,1.47116651981349,12.5161988840775));
#449387=CARTESIAN_POINT('Ctrl Pts',(2.30034839625671,1.48115590233616,12.5369868989719));
#449388=CARTESIAN_POINT('Ctrl Pts',(2.31537709837087,1.48417974827874,12.5369868989719));
#449389=CARTESIAN_POINT('Ctrl Pts',(2.32341833503594,1.47112815663568,12.5369868989719));
#449390=CARTESIAN_POINT('Origin',(4.27630463278515E-31,-2.27872721465328E-31,
12.5));
#449391=CARTESIAN_POINT('',(0.,0.,0.));
#449392=CARTESIAN_POINT('',(0.,0.,0.));
#449393=CARTESIAN_POINT('Origin',(5.65685387860011,26.,-5.65685387860012));
#449394=CARTESIAN_POINT('',(4.9222125558517,22.573038475773,-6.39190072013885));
#449395=CARTESIAN_POINT('',(4.92305381642377,22.5,-6.39065394077646));
#449396=CARTESIAN_POINT('',(4.92305381642377,26.,-6.39065394077646));
#449397=CARTESIAN_POINT('',(5.8978925564917,22.5,-6.66622270032004));
#449398=CARTESIAN_POINT('Origin',(5.65685387860011,22.5,-5.65685387860012));
#449399=CARTESIAN_POINT('Ctrl Pts',(5.89851203167784,22.5,-6.66798006829997));
#449400=CARTESIAN_POINT('Ctrl Pts',(5.5764199513446,22.5229375355598,-6.7439998684947));
#449401=CARTESIAN_POINT('Ctrl Pts',(5.21379162224851,22.5458750711197,-6.65366449057419));
#449402=CARTESIAN_POINT('Ctrl Pts',(4.96646199655034,22.5688126066795,-6.43383171727969));
#449403=CARTESIAN_POINT('Ctrl Pts',(4.95127317183385,22.5702212297106,-6.42033150900063));
#449404=CARTESIAN_POINT('Ctrl Pts',(4.93651917810251,22.5716298527418,-6.40634292159547));
#449405=CARTESIAN_POINT('Ctrl Pts',(4.9222125558517,22.573038475773,-6.39190072013885));
#449406=CARTESIAN_POINT('Origin',(5.65685387860011,26.,-5.65685387860012));
#449407=CARTESIAN_POINT('',(4.92436540268704,23.0230384757729,-6.39037461032892));
#449408=CARTESIAN_POINT('',(4.92349966353597,22.9019615242271,-6.38930388760559));
#449409=CARTESIAN_POINT('',(4.92305381642377,26.,-6.39065394077646));
#449410=CARTESIAN_POINT('',(4.62591736201901,22.5,-5.77557608073439));
#449411=CARTESIAN_POINT('Ctrl Pts',(4.92349966353597,22.9019615242271,-6.38930388760559));
#449412=CARTESIAN_POINT('Ctrl Pts',(5.07692511110986,22.8871128006417,-6.54102880287524));
#449413=CARTESIAN_POINT('Ctrl Pts',(5.27640120658105,22.8722640770563,-6.64766299899898));
#449414=CARTESIAN_POINT('Ctrl Pts',(5.48772889025785,22.8574153534709,-6.68249361011691));
#449415=CARTESIAN_POINT('Ctrl Pts',(5.82684562005693,22.8335876632395,-6.73838615923167));
#449416=CARTESIAN_POINT('Ctrl Pts',(6.19648078060475,22.8097599730081,-6.60938089562333));
#449417=CARTESIAN_POINT('Ctrl Pts',(6.42720821100081,22.7859322827767,-6.35472685290066));
#449418=CARTESIAN_POINT('Ctrl Pts',(6.65793564139688,22.7621045925453,-6.10007281017799));
#449419=CARTESIAN_POINT('Ctrl Pts',(6.74975534164119,22.7382769023139,-5.71976998834099));
#449420=CARTESIAN_POINT('Ctrl Pts',(6.66080060824128,22.7144492120825,-5.38773213421059));
#449421=CARTESIAN_POINT('Ctrl Pts',(6.57184587484137,22.6906215218511,-5.05569428008018));
#449422=CARTESIAN_POINT('Ctrl Pts',(6.30211670779724,22.6667938316197,-4.77192139365638));
#449423=CARTESIAN_POINT('Ctrl Pts',(5.97477550103877,22.6429661413884,-4.66700870222797));
#449424=CARTESIAN_POINT('Ctrl Pts',(5.6474342942803,22.619138451157,-4.56209601079956));
#449425=CARTESIAN_POINT('Ctrl Pts',(5.26248104780748,22.5953107609256,-4.63604351436656));
#449426=CARTESIAN_POINT('Ctrl Pts',(4.99722717517853,22.5714830706942,-4.85366607828882));
#449427=CARTESIAN_POINT('Ctrl Pts',(4.73197330254959,22.5476553804628,-5.07128864221107));
#449428=CARTESIAN_POINT('Ctrl Pts',(4.58641880376449,22.5238276902314,-5.43258626648858));
#449429=CARTESIAN_POINT('Ctrl Pts',(4.625917362019,22.5,-5.77557608073438));
#449430=CARTESIAN_POINT('Origin',(5.65685387860011,22.5,-5.65685387860012));
#449431=CARTESIAN_POINT('Ctrl Pts',(4.9222125558517,22.573038475773,-6.39190072013885));
#449432=CARTESIAN_POINT('Ctrl Pts',(4.69451421601594,22.5954575429732,-6.16204455719575));
#449433=CARTESIAN_POINT('Ctrl Pts',(4.58013776446742,22.6178766101734,-5.81728522517979));
#449434=CARTESIAN_POINT('Ctrl Pts',(4.62964039434809,22.6402956773736,-5.49777863793003));
#449435=CARTESIAN_POINT('Ctrl Pts',(4.68225334741615,22.664123367605,-5.15819698094666));
#449436=CARTESIAN_POINT('Ctrl Pts',(4.91998587117151,22.6879510578364,-4.8471410957032));
#449437=CARTESIAN_POINT('Ctrl Pts',(5.23393572436938,22.7117787480678,-4.70728537400252));
#449438=CARTESIAN_POINT('Ctrl Pts',(5.54788557756724,22.7356064382992,-4.56742965230184));
#449439=CARTESIAN_POINT('Ctrl Pts',(5.93805276020761,22.7594341285306,-4.59877409414395));
#449440=CARTESIAN_POINT('Ctrl Pts',(6.22570363532513,22.783261818762,-4.78686738296995));
#449441=CARTESIAN_POINT('Ctrl Pts',(6.51335451044265,22.8070895089934,-4.97496067179595));
#449442=CARTESIAN_POINT('Ctrl Pts',(6.69848907803731,22.8309171992248,-5.31980280760584));
#449443=CARTESIAN_POINT('Ctrl Pts',(6.69629884619592,22.8547448894562,-5.66347121722023));
#449444=CARTESIAN_POINT('Ctrl Pts',(6.69410861435453,22.8785725796876,-6.00713962683461));
#449445=CARTESIAN_POINT('Ctrl Pts',(6.5045935830771,22.902400269919,-6.34963431025348));
#449446=CARTESIAN_POINT('Ctrl Pts',(6.21456908983246,22.9262279601503,-6.53403672593788));
#449447=CARTESIAN_POINT('Ctrl Pts',(5.92454459658782,22.9500556503817,-6.71843914162228));
#449448=CARTESIAN_POINT('Ctrl Pts',(5.53401064137597,22.9738833406131,-6.7447492895722));
#449449=CARTESIAN_POINT('Ctrl Pts',(5.22186823831326,22.9977110308445,-6.60092695407667));
#449450=CARTESIAN_POINT('Ctrl Pts',(5.11127184889382,23.0061535124873,-6.54996870275417));
#449451=CARTESIAN_POINT('Ctrl Pts',(5.0105166042882,23.0145959941301,-6.47765230299322));
#449452=CARTESIAN_POINT('Ctrl Pts',(4.92436540268704,23.0230384757729,-6.39037461032892));
#449453=CARTESIAN_POINT('Origin',(5.65685387860011,26.,-5.65685387860012));
#449454=CARTESIAN_POINT('',(4.92330089590042,23.4730384757729,-6.38935290488262));
#449455=CARTESIAN_POINT('',(4.92169609601798,23.3519615242271,-6.3913110357232));
#449456=CARTESIAN_POINT('',(4.92305381642377,26.,-6.39065394077646));
#449457=CARTESIAN_POINT('Ctrl Pts',(4.92169609601798,23.3519615242271,-6.3913110357232));
#449458=CARTESIAN_POINT('Ctrl Pts',(5.14636061012976,23.33007894203,-6.61334324490838));
#449459=CARTESIAN_POINT('Ctrl Pts',(5.47994522249351,23.308196359833,-6.72868171719176));
#449460=CARTESIAN_POINT('Ctrl Pts',(5.79285848911253,23.286313777636,-6.68738448495221));
#449461=CARTESIAN_POINT('Ctrl Pts',(6.1335861198444,23.2624860874046,-6.64241640721999));
#449462=CARTESIAN_POINT('Ctrl Pts',(6.44980419113038,23.2386583971732,-6.41172882390928));
#449463=CARTESIAN_POINT('Ctrl Pts',(6.59665364733223,23.2148307069418,-6.10100080909856));
#449464=CARTESIAN_POINT('Ctrl Pts',(6.74350310353408,23.1910030167104,-5.79027279428784));
#449465=CARTESIAN_POINT('Ctrl Pts',(6.7209839446518,23.167175326479,-5.39950434797711));
#449466=CARTESIAN_POINT('Ctrl Pts',(6.539415444341,23.1433476362476,-5.1076985472349));
#449467=CARTESIAN_POINT('Ctrl Pts',(6.3578469440302,23.1195199460162,-4.8158927464927));
#449468=CARTESIAN_POINT('Ctrl Pts',(6.01722910229088,23.0956922557848,-4.62304959131903));
#449469=CARTESIAN_POINT('Ctrl Pts',(5.67358993507176,23.0718645655534,-4.61751951301592));
#449470=CARTESIAN_POINT('Ctrl Pts',(5.32995076785264,23.048036875322,-4.61198943471281));
#449471=CARTESIAN_POINT('Ctrl Pts',(4.98329027515371,23.0242091850907,-4.79377243328026));
#449472=CARTESIAN_POINT('Ctrl Pts',(4.7924243254548,23.0003814948593,-5.07957475014376));
#449473=CARTESIAN_POINT('Ctrl Pts',(4.60155837575589,22.9765538046279,-5.36537706700727));
#449474=CARTESIAN_POINT('Ctrl Pts',(4.56648696905699,22.9527261143965,-5.75519870216683));
#449475=CARTESIAN_POINT('Ctrl Pts',(4.70325041523271,22.9288984241651,-6.07050470066555));
#449476=CARTESIAN_POINT('Ctrl Pts',(4.75478685916323,22.9199194575191,-6.18932117076026));
#449477=CARTESIAN_POINT('Ctrl Pts',(4.830723879241,22.9109404908731,-6.29755640872372));
#449478=CARTESIAN_POINT('Ctrl Pts',(4.92349966353597,22.9019615242271,-6.38930388760559));
#449479=CARTESIAN_POINT('Ctrl Pts',(4.92436540268704,23.0230384757729,-6.39037461032892));
#449480=CARTESIAN_POINT('Ctrl Pts',(4.76736722811336,23.0384236843615,-6.23132356780567));
#449481=CARTESIAN_POINT('Ctrl Pts',(4.65886881811934,23.0538088929501,-6.02258634020352));
#449482=CARTESIAN_POINT('Ctrl Pts',(4.62769529041208,23.0691941015387,-5.80287677492702));
#449483=CARTESIAN_POINT('Ctrl Pts',(4.57941559648716,23.0930217917701,-5.46260375021388));
#449484=CARTESIAN_POINT('Ctrl Pts',(4.71660705955086,23.1168494820015,-5.09601251972857));
#449485=CARTESIAN_POINT('Ctrl Pts',(4.97642324075838,23.1406771722329,-4.87103919530453));
#449486=CARTESIAN_POINT('Ctrl Pts',(5.23623942196589,23.1645048624643,-4.64606587088049));
#449487=CARTESIAN_POINT('Ctrl Pts',(5.61868032131722,23.1883325526957,-4.56271045251773));
#449488=CARTESIAN_POINT('Ctrl Pts',(5.94855238336812,23.2121602429271,-4.65915585483332));
#449489=CARTESIAN_POINT('Ctrl Pts',(6.27842444541901,23.2359879331585,-4.75560125714891));
#449490=CARTESIAN_POINT('Ctrl Pts',(6.55572767016945,23.2598156233899,-5.03184748014285));
#449491=CARTESIAN_POINT('Ctrl Pts',(6.65343136663416,23.2836433136212,-5.36134886181892));
#449492=CARTESIAN_POINT('Ctrl Pts',(6.75113506309887,23.3074710038526,-5.690850243495));
#449493=CARTESIAN_POINT('Ctrl Pts',(6.66923923127783,23.331298694084,-6.07360678385322));
#449494=CARTESIAN_POINT('Ctrl Pts',(6.4452597843657,23.3551263843154,-6.33427992409048));
#449495=CARTESIAN_POINT('Ctrl Pts',(6.22128033745358,23.3789540745468,-6.59495306432775));
#449496=CARTESIAN_POINT('Ctrl Pts',(5.85521727545038,23.4027817647782,-6.73354280444407));
#449497=CARTESIAN_POINT('Ctrl Pts',(5.51476156795534,23.4266094550096,-6.6865623548039));
#449498=CARTESIAN_POINT('Ctrl Pts',(5.29363193601897,23.442085795264,-6.65604804910002));
#449499=CARTESIAN_POINT('Ctrl Pts',(5.08330512959901,23.4575621355185,-6.54724832815155));
#449500=CARTESIAN_POINT('Ctrl Pts',(4.92330089590042,23.4730384757729,-6.38935290488262));
#449501=CARTESIAN_POINT('Origin',(5.65685387860011,26.,-5.65685387860012));
#449502=CARTESIAN_POINT('',(4.9216948349357,23.9230384757729,-6.39152331859132));
#449503=CARTESIAN_POINT('',(4.92356615355223,23.8019615242271,-6.39146732321148));
#449504=CARTESIAN_POINT('',(4.92305381642377,26.,-6.39065394077646));
#449505=CARTESIAN_POINT('Ctrl Pts',(4.92356615355223,23.8019615242271,-6.39146732321148));
#449506=CARTESIAN_POINT('Ctrl Pts',(4.97518123721477,23.7968727736498,-6.44404636753914));
#449507=CARTESIAN_POINT('Ctrl Pts',(5.03225965778749,23.7917840230725,-6.49097569651667));
#449508=CARTESIAN_POINT('Ctrl Pts',(5.09396482100832,23.7866952724952,-6.53072214720976));
#449509=CARTESIAN_POINT('Ctrl Pts',(5.38289458727869,23.7628675822638,-6.71683190058211));
#449510=CARTESIAN_POINT('Ctrl Pts',(5.77326614382955,23.7390398920324,-6.74545633697037));
#449511=CARTESIAN_POINT('Ctrl Pts',(6.08625298439034,23.715212201801,-6.60348277515141));
#449512=CARTESIAN_POINT('Ctrl Pts',(6.39923982495114,23.6913845115696,-6.46150921333244));
#449513=CARTESIAN_POINT('Ctrl Pts',(6.63484194952187,23.6675568213382,-6.14893765330626));
#449514=CARTESIAN_POINT('Ctrl Pts',(6.68513161677842,23.6437291311068,-5.80895502137128));
#449515=CARTESIAN_POINT('Ctrl Pts',(6.73542128403497,23.6199014408755,-5.4689723894363));
#449516=CARTESIAN_POINT('Ctrl Pts',(6.60039849397735,23.5960737506441,-5.10157868559252));
#449517=CARTESIAN_POINT('Ctrl Pts',(6.34191631672375,23.5722460604127,-4.87507434314934));
#449518=CARTESIAN_POINT('Ctrl Pts',(6.08343413947014,23.5484183701813,-4.64857000070616));
#449519=CARTESIAN_POINT('Ctrl Pts',(5.70149257502055,23.5245906799499,-4.56295501966359));
#449520=CARTESIAN_POINT('Ctrl Pts',(5.37105630657982,23.5007629897185,-4.65744921450722));
#449521=CARTESIAN_POINT('Ctrl Pts',(5.04062003813909,23.4769352994871,-4.75194340935084));
#449522=CARTESIAN_POINT('Ctrl Pts',(4.76168906570723,23.4531076092557,-5.02654678008065));
#449523=CARTESIAN_POINT('Ctrl Pts',(4.66203997694959,23.4292799190243,-5.35546505814245));
#449524=CARTESIAN_POINT('Ctrl Pts',(4.56239088819195,23.4054522287929,-5.68438333620426));
#449525=CARTESIAN_POINT('Ctrl Pts',(4.64202368310855,23.3816245385615,-6.06761652159808));
#449526=CARTESIAN_POINT('Ctrl Pts',(4.86445867565572,23.3577968483301,-6.32960882821811));
#449527=CARTESIAN_POINT('Ctrl Pts',(4.88261654521522,23.3558517402958,-6.350995850443));
#449528=CARTESIAN_POINT('Ctrl Pts',(4.90172602358781,23.3539066322614,-6.37157494470416));
#449529=CARTESIAN_POINT('Ctrl Pts',(4.92169609601798,23.3519615242271,-6.3913110357232));
#449530=CARTESIAN_POINT('Ctrl Pts',(4.92330089590042,23.4730384757729,-6.38935290488262));
#449531=CARTESIAN_POINT('Ctrl Pts',(4.83695933636888,23.4813898257499,-6.30414930262286));
#449532=CARTESIAN_POINT('Ctrl Pts',(4.76527121936352,23.4897411757268,-6.20464951053553));
#449533=CARTESIAN_POINT('Ctrl Pts',(4.71444637045848,23.4980925257038,-6.09544017298549));
#449534=CARTESIAN_POINT('Ctrl Pts',(4.56943523344352,23.5219202159352,-5.78384908020389));
#449535=CARTESIAN_POINT('Ctrl Pts',(4.59426131240048,23.5457479061666,-5.39321753403732));
#449536=CARTESIAN_POINT('Ctrl Pts',(4.77755195197114,23.569575596398,-5.10249121190879));
#449537=CARTESIAN_POINT('Ctrl Pts',(4.9608425915418,23.5934032866293,-4.81176488978025));
#449538=CARTESIAN_POINT('Ctrl Pts',(5.30259779172617,23.6172309768607,-4.62094379168974));
#449539=CARTESIAN_POINT('Ctrl Pts',(5.64626184853499,23.6410586670921,-4.61744171997954));
#449540=CARTESIAN_POINT('Ctrl Pts',(5.98992590534381,23.6648863573235,-4.61393964826935));
#449541=CARTESIAN_POINT('Ctrl Pts',(6.33549881877709,23.6887140475549,-4.79775660293947));
#449542=CARTESIAN_POINT('Ctrl Pts',(6.52467601704459,23.7125417377863,-5.08468731748426));
#449543=CARTESIAN_POINT('Ctrl Pts',(6.71385321531209,23.7363694280177,-5.37161803202905));
#449544=CARTESIAN_POINT('Ctrl Pts',(6.74663469841383,23.7601971182491,-5.76166250644852));
#449545=CARTESIAN_POINT('Ctrl Pts',(6.60800349462427,23.7840248084805,-6.07614404554655));
#449546=CARTESIAN_POINT('Ctrl Pts',(6.46937229083472,23.8078524987119,-6.39062558464459));
#449547=CARTESIAN_POINT('Ctrl Pts',(6.15932840015388,23.8316801889433,-6.6295441884212));
#449548=CARTESIAN_POINT('Ctrl Pts',(5.81990079386588,23.8555078791747,-6.6834528935629));
#449549=CARTESIAN_POINT('Ctrl Pts',(5.49924097144978,23.8780180780408,-6.73438085433327));
#449550=CARTESIAN_POINT('Ctrl Pts',(5.15235699515365,23.9005282769068,-6.62019259508593));
#449551=CARTESIAN_POINT('Ctrl Pts',(4.9216948349357,23.9230384757729,-6.39152331859132));
#449552=CARTESIAN_POINT('Origin',(5.65685387860011,26.,-5.65685387860012));
#449553=CARTESIAN_POINT('',(4.92377157353715,24.3730384757729,-6.39128196913613));
#449554=CARTESIAN_POINT('',(4.92421628016771,24.2519615242271,-6.38942086037359));
#449555=CARTESIAN_POINT('',(4.92305381642377,26.,-6.39065394077646));
#449556=CARTESIAN_POINT('Ctrl Pts',(4.92421628016771,24.2519615242271,-6.38942086037359));
#449557=CARTESIAN_POINT('Ctrl Pts',(5.04895543667044,24.2398389150381,-6.51405309196749));
#449558=CARTESIAN_POINT('Ctrl Pts',(5.20382475542584,24.2277163058492,-6.60860369693141));
#449559=CARTESIAN_POINT('Ctrl Pts',(5.37198243345446,24.2155936966603,-6.65652287894995));
#449560=CARTESIAN_POINT('Ctrl Pts',(5.70250608555364,24.1917660064289,-6.75071080561528));
#449561=CARTESIAN_POINT('Ctrl Pts',(6.08436822205294,24.1679383161975,-6.66474206054895));
#449562=CARTESIAN_POINT('Ctrl Pts',(6.34264042812557,24.1441106259661,-6.4379983333991));
#449563=CARTESIAN_POINT('Ctrl Pts',(6.60091263419821,24.1202829357347,-6.21125460624925));
#449564=CARTESIAN_POINT('Ctrl Pts',(6.73559490984418,24.0964552455033,-5.84373589701587));
#449565=CARTESIAN_POINT('Ctrl Pts',(6.68499023152592,24.0726275552719,-5.5037999963824));
#449566=CARTESIAN_POINT('Ctrl Pts',(6.63438555320766,24.0487998650405,-5.16386409574893));
#449567=CARTESIAN_POINT('Ctrl Pts',(6.39849392092517,24.0249721748091,-4.85151100371537));
#449568=CARTESIAN_POINT('Ctrl Pts',(6.08537566804496,24.0011444845777,-4.70982751913656));
#449569=CARTESIAN_POINT('Ctrl Pts',(5.77225741516475,23.9773167943464,-4.56814403455775));
#449570=CARTESIAN_POINT('Ctrl Pts',(5.38191254168682,23.9534891041149,-4.59713015743369));
#449571=CARTESIAN_POINT('Ctrl Pts',(5.09315534403941,23.9296614138835,-4.78350754767415));
#449572=CARTESIAN_POINT('Ctrl Pts',(4.804398146392,23.9058337236522,-4.96988493791459));
#449573=CARTESIAN_POINT('Ctrl Pts',(4.61722862457511,23.8820060334208,-5.31365359551954));
#449574=CARTESIAN_POINT('Ctrl Pts',(4.6173878516616,23.8581783431894,-5.65733545950024));
#449575=CARTESIAN_POINT('Ctrl Pts',(4.61751307348277,23.8394394035353,-5.92761905169082));
#449576=CARTESIAN_POINT('Ctrl Pts',(4.73349750638545,23.8207004638812,-6.19784896370209));
#449577=CARTESIAN_POINT('Ctrl Pts',(4.92356615355223,23.8019615242271,-6.39146732321148));
#449578=CARTESIAN_POINT('Ctrl Pts',(4.9216948349357,23.9230384757729,-6.39152331859132));
#449579=CARTESIAN_POINT('Ctrl Pts',(4.90819449199352,23.9243559671382,-6.37813961642664));
#449580=CARTESIAN_POINT('Ctrl Pts',(4.895092278726,23.9256734585035,-6.3643637478711));
#449581=CARTESIAN_POINT('Ctrl Pts',(4.88241675495565,23.9269909498688,-6.35020586507153));
#449582=CARTESIAN_POINT('Ctrl Pts',(4.65317164422858,23.9508186401002,-6.0941513249317));
#449583=CARTESIAN_POINT('Ctrl Pts',(4.56349274466962,23.9746463303316,-5.71314343814525));
#449584=CARTESIAN_POINT('Ctrl Pts',(4.6544613426263,23.998474020563,-5.38171929489582));
#449585=CARTESIAN_POINT('Ctrl Pts',(4.74542994058297,24.0223017107944,-5.0502951516464));
#449586=CARTESIAN_POINT('Ctrl Pts',(5.01704603605528,24.0461294010258,-4.76845475193401));
#449587=CARTESIAN_POINT('Ctrl Pts',(5.34488416612327,24.0699570912572,-4.6653072414873));
#449588=CARTESIAN_POINT('Ctrl Pts',(5.67272229619127,24.0937847814886,-4.56215973104059));
#449589=CARTESIAN_POINT('Ctrl Pts',(6.05678246085496,24.11761247172,-4.63770510985959));
#449590=CARTESIAN_POINT('Ctrl Pts',(6.32112934350159,24.1414401619514,-4.8573365604447));
#449591=CARTESIAN_POINT('Ctrl Pts',(6.58547622614821,24.1652678521828,-5.07696801102981));
#449592=CARTESIAN_POINT('Ctrl Pts',(6.73010982677778,24.1890955424141,-5.44068553338104));
#449593=CARTESIAN_POINT('Ctrl Pts',(6.68877448884911,24.2129232326455,-5.78187263496817));
#449594=CARTESIAN_POINT('Ctrl Pts',(6.64743915092045,24.2367509228769,-6.12305973655531));
#449595=CARTESIAN_POINT('Ctrl Pts',(6.42013487443355,24.2605786131083,-6.44171641737836));
#449596=CARTESIAN_POINT('Ctrl Pts',(6.11098818332588,24.2844063033397,-6.59186824658804));
#449597=CARTESIAN_POINT('Ctrl Pts',(5.80184149221821,24.3082339935711,-6.74202007579772));
#449598=CARTESIAN_POINT('Ctrl Pts',(5.41085238648977,24.3320616838025,-6.72366705339403));
#449599=CARTESIAN_POINT('Ctrl Pts',(5.11713028264445,24.3558893740339,-6.54521657215205));
#449600=CARTESIAN_POINT('Ctrl Pts',(5.04666506349635,24.3616057412803,-6.50240552012982));
#449601=CARTESIAN_POINT('Ctrl Pts',(4.98179796021342,24.3673221085266,-6.45038020112141));
#449602=CARTESIAN_POINT('Ctrl Pts',(4.92377157353715,24.3730384757729,-6.39128196913613));
#449603=CARTESIAN_POINT('Origin',(5.65685387860011,26.,-5.65685387860012));
#449604=CARTESIAN_POINT('',(4.92408802232565,24.8230384757729,-6.38933869113556));
#449605=CARTESIAN_POINT('',(4.92212745780798,24.7019615242271,-6.39028821611916));
#449606=CARTESIAN_POINT('',(4.92305381642377,26.,-6.39065394077646));
#449607=CARTESIAN_POINT('Ctrl Pts',(4.92212745780798,24.7019615242271,-6.39028821611916));
#449608=CARTESIAN_POINT('Ctrl Pts',(5.11995795053563,24.6828050564265,-6.5845155347103));
#449609=CARTESIAN_POINT('Ctrl Pts',(5.39828521249021,24.6636485886259,-6.70087353526984));
#449610=CARTESIAN_POINT('Ctrl Pts',(5.67455106061111,24.6444921208254,-6.69616935490973));
#449611=CARTESIAN_POINT('Ctrl Pts',(6.01818314973456,24.620664430594,-6.69031808036474));
#449612=CARTESIAN_POINT('Ctrl Pts',(6.35862591802897,24.5968367403626,-6.49716519325234));
#449613=CARTESIAN_POINT('Ctrl Pts',(6.53992487743045,24.5730090501312,-6.20519269912468));
#449614=CARTESIAN_POINT('Ctrl Pts',(6.72122383683193,24.5491813598998,-5.91322020499702));
#449615=CARTESIAN_POINT('Ctrl Pts',(6.74337898734047,24.5253536696684,-5.52242810385412));
#449616=CARTESIAN_POINT('Ctrl Pts',(6.59624120723028,24.501525979437,-5.21183556708661));
#449617=CARTESIAN_POINT('Ctrl Pts',(6.44910342712008,24.4776982892056,-4.9012430303191));
#449618=CARTESIAN_POINT('Ctrl Pts',(6.13267271639114,24.4538705989742,-4.670850057927));
#449619=CARTESIAN_POINT('Ctrl Pts',(5.7919038045113,24.4300429087428,-4.62619808347199));
#449620=CARTESIAN_POINT('Ctrl Pts',(5.45113489263147,24.4062152185114,-4.58154610901698));
#449621=CARTESIAN_POINT('Ctrl Pts',(5.08602777960075,24.38238752828,-4.72263513249906));
#449622=CARTESIAN_POINT('Ctrl Pts',(4.86383551964991,24.3585598380486,-4.98483324415836));
#449623=CARTESIAN_POINT('Ctrl Pts',(4.64164325969907,24.3347321478172,-5.24703135581765));
#449624=CARTESIAN_POINT('Ctrl Pts',(4.56236585282811,24.3109044575858,-5.63033855565415));
#449625=CARTESIAN_POINT('Ctrl Pts',(4.66231973324216,24.2870767673545,-5.9591644547709));
#449626=CARTESIAN_POINT('Ctrl Pts',(4.71142093690032,24.275371686312,-6.12069642705377));
#449627=CARTESIAN_POINT('Ctrl Pts',(4.80377340246064,24.2636666052695,-6.26908122485669));
#449628=CARTESIAN_POINT('Ctrl Pts',(4.92421628016771,24.2519615242271,-6.38942086037359));
#449629=CARTESIAN_POINT('Ctrl Pts',(4.92377157353715,24.3730384757729,-6.39128196913613));
#449630=CARTESIAN_POINT('Ctrl Pts',(4.7399249826062,24.391149798758,-6.20403942134221));
#449631=CARTESIAN_POINT('Ctrl Pts',(4.62474754709557,24.4092611217431,-5.94579686164739));
#449632=CARTESIAN_POINT('Ctrl Pts',(4.61775970678069,24.4273724447281,-5.68465923264326));
#449633=CARTESIAN_POINT('Ctrl Pts',(4.60856633672445,24.4512001349595,-5.34110031445674));
#449634=CARTESIAN_POINT('Ctrl Pts',(4.78663469857419,24.4750278251909,-4.99253041816396));
#449635=CARTESIAN_POINT('Ctrl Pts',(5.07039290068915,24.4988555154223,-4.79862701145602));
#449636=CARTESIAN_POINT('Ctrl Pts',(5.35415110280411,24.5226832056536,-4.60472360474809));
#449637=CARTESIAN_POINT('Ctrl Pts',(5.7435991451843,24.546510895885,-4.565486687625));
#449638=CARTESIAN_POINT('Ctrl Pts',(6.06033356407531,24.5703385861164,-4.69889042440694));
#449639=CARTESIAN_POINT('Ctrl Pts',(6.37706798296632,24.5941662763478,-4.83229416118888));
#449640=CARTESIAN_POINT('Ctrl Pts',(6.62108877836816,24.6179939665792,-5.13833855187585));
#449641=CARTESIAN_POINT('Ctrl Pts',(6.68061169925027,24.6418216568106,-5.47682676316715));
#449642=CARTESIAN_POINT('Ctrl Pts',(6.74013462013239,24.665649347042,-5.81531497445846));
#449643=CARTESIAN_POINT('Ctrl Pts',(6.61515966649478,24.6894770372734,-6.18624700635411));
#449644=CARTESIAN_POINT('Ctrl Pts',(6.36293701391879,24.7133047275048,-6.41970146010492));
#449645=CARTESIAN_POINT('Ctrl Pts',(6.1107143613428,24.7371324177362,-6.65315591385573));
#449646=CARTESIAN_POINT('Ctrl Pts',(5.73124400982843,24.7609601079676,-6.74913278946171));
#449647=CARTESIAN_POINT('Ctrl Pts',(5.39835869474429,24.784787798199,-6.6636657201663));
#449648=CARTESIAN_POINT('Ctrl Pts',(5.22023136007979,24.797538024057,-6.61793218802978));
#449649=CARTESIAN_POINT('Ctrl Pts',(5.05544287282308,24.8102882499149,-6.5202452116208));
#449650=CARTESIAN_POINT('Ctrl Pts',(4.92408802232565,24.8230384757729,-6.38933869113556));
#449651=CARTESIAN_POINT('Origin',(5.65685387860011,26.,-5.65685387860012));
#449652=CARTESIAN_POINT('',(4.92197603118329,25.2730384757729,-6.39051881327128));
#449653=CARTESIAN_POINT('',(4.92254817630007,25.1519615242271,-6.39198798715976));
#449654=CARTESIAN_POINT('',(4.92305381642377,26.,-6.39065394077646));
#449655=CARTESIAN_POINT('Ctrl Pts',(4.92254817630007,25.1519615242271,-6.39198798715976));
#449656=CARTESIAN_POINT('Ctrl Pts',(4.94650751599249,25.1495988880462,-6.41627314991444));
#449657=CARTESIAN_POINT('Ctrl Pts',(4.97169983154625,25.1472362518654,-6.43929566708609));
#449658=CARTESIAN_POINT('Ctrl Pts',(4.99805942366946,25.1448736156846,-6.46089355482011));
#449659=CARTESIAN_POINT('Ctrl Pts',(5.26390153716753,25.1210459254532,-6.67871286308055));
#449660=CARTESIAN_POINT('Ctrl Pts',(5.64846913729549,25.0972182352218,-6.75163093056004));
#449661=CARTESIAN_POINT('Ctrl Pts',(5.97559449046916,25.0733905449904,-6.64624470558553));
#449662=CARTESIAN_POINT('Ctrl Pts',(6.30271984364283,25.049562854759,-6.54085848061101));
#449663=CARTESIAN_POINT('Ctrl Pts',(6.57240294986222,25.0257351645276,-6.25716796318249));
#449664=CARTESIAN_POINT('Ctrl Pts',(6.66110381706144,25.0019074742962,-5.92512971718013));
#449665=CARTESIAN_POINT('Ctrl Pts',(6.74980468426065,24.9780797840648,-5.59309147117778));
#449666=CARTESIAN_POINT('Ctrl Pts',(6.65752331243968,24.9542520938335,-5.21270549660159));
#449667=CARTESIAN_POINT('Ctrl Pts',(6.42653317184816,24.9304244036021,-4.95822404429259));
#449668=CARTESIAN_POINT('Ctrl Pts',(6.19554303125664,24.9065967133707,-4.70374259198359));
#449669=CARTESIAN_POINT('Ctrl Pts',(5.82584412189456,24.8827690231393,-4.57516566194178));
#449670=CARTESIAN_POINT('Ctrl Pts',(5.48679296352304,24.8589413329079,-4.63139343216518));
#449671=CARTESIAN_POINT('Ctrl Pts',(5.14774180515151,24.8351136426765,-4.68762120238858));
#449672=CARTESIAN_POINT('Ctrl Pts',(4.83933839777055,24.8112859524451,-4.9286536728772));
#449673=CARTESIAN_POINT('Ctrl Pts',(4.70286022094558,24.7874582622137,-5.24407554312886));
#449674=CARTESIAN_POINT('Ctrl Pts',(4.56638204412062,24.7636305719823,-5.55949741338051));
#449675=CARTESIAN_POINT('Ctrl Pts',(4.60182909785165,24.7398028817509,-5.94930868339519));
#449676=CARTESIAN_POINT('Ctrl Pts',(4.79296332969341,24.7159751915195,-6.23493948741374));
#449677=CARTESIAN_POINT('Ctrl Pts',(4.83043362171106,24.7113039690887,-6.29093505415592));
#449678=CARTESIAN_POINT('Ctrl Pts',(4.87388734148021,24.7066327466579,-6.34292671833547));
#449679=CARTESIAN_POINT('Ctrl Pts',(4.92212745780798,24.7019615242271,-6.39028821611916));
#449680=CARTESIAN_POINT('Ctrl Pts',(4.92408802232565,24.8230384757729,-6.38933869113556));
#449681=CARTESIAN_POINT('Ctrl Pts',(4.80996622614209,24.8341159401463,-6.27560640646284));
#449682=CARTESIAN_POINT('Ctrl Pts',(4.72108089883846,24.8451934045197,-6.13679925493306));
#449683=CARTESIAN_POINT('Ctrl Pts',(4.67061008310121,24.8562708688931,-5.98520281626299));
#449684=CARTESIAN_POINT('Ctrl Pts',(4.56204706519615,24.8800985591245,-5.65911799585187));
#449685=CARTESIAN_POINT('Ctrl Pts',(4.63122130803993,24.9039262493559,-5.27385936922642));
#449686=CARTESIAN_POINT('Ctrl Pts',(4.84644449237099,24.9277539395873,-5.00591117956891));
#449687=CARTESIAN_POINT('Ctrl Pts',(5.06166767670205,24.9515816298187,-4.7379629899114));
#449688=CARTESIAN_POINT('Ctrl Pts',(5.42293980252039,24.9754093200501,-4.58732523722183));
#449689=CARTESIAN_POINT('Ctrl Pts',(5.76476474386039,24.9992370102815,-4.62300419682159));
#449690=CARTESIAN_POINT('Ctrl Pts',(6.10658968520039,25.0230647005129,-4.65868315642135));
#449691=CARTESIAN_POINT('Ctrl Pts',(6.42896744206204,25.0468923907443,-4.88067882831045));
#449692=CARTESIAN_POINT('Ctrl Pts',(6.58421869570625,25.0707200809757,-5.18729621377842));
#449693=CARTESIAN_POINT('Ctrl Pts',(6.73946994935045,25.0945477712071,-5.4939135992464));
#449694=CARTESIAN_POINT('Ctrl Pts',(6.72759469977719,25.1183754614385,-5.88515269829325));
#449695=CARTESIAN_POINT('Ctrl Pts',(6.5540334824637,25.1422031516699,-6.18179018209155));
#449696=CARTESIAN_POINT('Ctrl Pts',(6.38047226515022,25.1660308419013,-6.47842766588984));
#449697=CARTESIAN_POINT('Ctrl Pts',(6.0452250800965,25.1898585321326,-6.68046353443956));
#449698=CARTESIAN_POINT('Ctrl Pts',(5.70186524531576,25.213686222364,-6.69534535485933));
#449699=CARTESIAN_POINT('Ctrl Pts',(5.41677424787487,25.2334703068337,-6.70770170116849));
#449700=CARTESIAN_POINT('Ctrl Pts',(5.12609043162756,25.2532543913033,-6.59103501365993));
#449701=CARTESIAN_POINT('Ctrl Pts',(4.92197603118329,25.2730384757729,-6.39051881327128));
#449702=CARTESIAN_POINT('Origin',(5.65685387860011,26.,-5.65685387860012));
#449703=CARTESIAN_POINT('',(4.92276701974739,25.7230384757729,-6.39190058798136));
#449704=CARTESIAN_POINT('',(4.92443355077908,25.6019615242271,-6.39006796800885));
#449705=CARTESIAN_POINT('',(4.92305381642377,26.,-6.39065394077646));
#449706=CARTESIAN_POINT('',(6.69274404704181,26.,-5.59475217632209));
#449707=CARTESIAN_POINT('Ctrl Pts',(4.92276701974739,25.7230384757729,-6.39190058798136));
#449708=CARTESIAN_POINT('Ctrl Pts',(4.71160994855805,25.7438759131544,-6.17742942344334));
#449709=CARTESIAN_POINT('Ctrl Pts',(4.59523934827088,25.764713350536,-5.86562000134797));
#449710=CARTESIAN_POINT('Ctrl Pts',(4.62142687258513,25.7855507879175,-5.56615422141077));
#449711=CARTESIAN_POINT('Ctrl Pts',(4.65137240791476,25.8093784781489,-5.22371394391399));
#449712=CARTESIAN_POINT('Ctrl Pts',(4.86772710302321,25.8332061683802,-4.8974142264151));
#449713=CARTESIAN_POINT('Ctrl Pts',(5.17187737628347,25.8570338586116,-4.7372531902219));
#449714=CARTESIAN_POINT('Ctrl Pts',(5.47602764954372,25.880861548843,-4.57709215402869));
#449715=CARTESIAN_POINT('Ctrl Pts',(5.86797350095578,25.9046892390744,-4.58306979914119));
#449716=CARTESIAN_POINT('Ctrl Pts',(6.16698733288025,25.9285169293058,-4.75132533448083));
#449717=CARTESIAN_POINT('Ctrl Pts',(6.46600116480472,25.9523446195372,-4.91958086982048));
#449718=CARTESIAN_POINT('Ctrl Pts',(6.67208297724159,25.9761723097686,-5.25011429538726));
#449719=CARTESIAN_POINT('Ctrl Pts',(6.69274404704181,26.,-5.59475217632212));
#449720=CARTESIAN_POINT('',(5.59444809180803,26.,-6.69457727933146));
#449721=CARTESIAN_POINT('Origin',(5.65685387860011,26.,-5.65685387860012));
#449722=CARTESIAN_POINT('Ctrl Pts',(5.59444726164187,26.,-6.69458228414866));
#449723=CARTESIAN_POINT('Ctrl Pts',(5.92484673178863,25.9770624644402,-6.71351646533255));
#449724=CARTESIAN_POINT('Ctrl Pts',(6.26627937525033,25.9541249288804,-6.56158375468957));
#449725=CARTESIAN_POINT('Ctrl Pts',(6.47167795527827,25.9311873933205,-6.30214239804398));
#449726=CARTESIAN_POINT('Ctrl Pts',(6.68504759676004,25.9073597030892,-6.03263270014108));
#449727=CARTESIAN_POINT('Ctrl Pts',(6.75161994353754,25.8835320128578,-5.64710810132191));
#449728=CARTESIAN_POINT('Ctrl Pts',(6.64083855948586,25.8597043226264,-5.32182159136528));
#449729=CARTESIAN_POINT('Ctrl Pts',(6.53005717543418,25.835876632395,-4.99653508140864));
#449730=CARTESIAN_POINT('Ctrl Pts',(6.24192206055332,25.8120489421636,-4.73148666031454));
#449731=CARTESIAN_POINT('Ctrl Pts',(5.90845611919746,25.7882212519322,-4.64827248224482));
#449732=CARTESIAN_POINT('Ctrl Pts',(5.5749901778416,25.7643935617008,-4.56505830417509));
#449733=CARTESIAN_POINT('Ctrl Pts',(5.19619341001074,25.7405658714694,-4.66367836912974));
#449734=CARTESIAN_POINT('Ctrl Pts',(4.94557465216384,25.716738181238,-4.89886414913017));
#449735=CARTESIAN_POINT('Ctrl Pts',(4.69495589431694,25.6929104910066,-5.13404992913059));
#449736=CARTESIAN_POINT('Ctrl Pts',(4.572515146454,25.6690828007752,-5.50580142417678));
#449737=CARTESIAN_POINT('Ctrl Pts',(4.63434949773116,25.6452551105439,-5.84386841174159));
#449738=CARTESIAN_POINT('Ctrl Pts',(4.67179935541582,25.6308239151049,-6.04861804217652));
#449739=CARTESIAN_POINT('Ctrl Pts',(4.7768430935332,25.616392719666,-6.24101187097706));
#449740=CARTESIAN_POINT('Ctrl Pts',(4.92443355077908,25.6019615242271,-6.39006796800885));
#449741=CARTESIAN_POINT('Origin',(5.65685387860011,26.993675081176,-5.65685387860012));
#449742=CARTESIAN_POINT('',(4.74524035180399,22.756324918824,-6.5673434103921));
#449743=CARTESIAN_POINT('',(4.74364038176038,22.718675081176,-6.57057146528766));
#449744=CARTESIAN_POINT('',(4.74468613086949,26.993675081176,-6.56902162633079));
#449745=CARTESIAN_POINT('',(6.64591806159944,22.5,-4.8286920333622));
#449746=CARTESIAN_POINT('Ctrl Pts',(4.74364038176038,22.718675081176,-6.57057146528766));
#449747=CARTESIAN_POINT('Ctrl Pts',(4.76142457130848,22.7172664581449,-6.58852418981576));
#449748=CARTESIAN_POINT('Ctrl Pts',(5.09000197050781,22.6920301448823,-6.9000556810006));
#449749=CARTESIAN_POINT('Ctrl Pts',(6.06611679986992,22.6429661413884,-7.12689194633153));
#449750=CARTESIAN_POINT('Ctrl Pts',(7.11331947438321,22.5714830706942,-6.10694434613243));
#449751=CARTESIAN_POINT('Ctrl Pts',(6.92144528650133,22.5238276902314,-5.15775103452081));
#449752=CARTESIAN_POINT('Ctrl Pts',(6.64591806159944,22.5,-4.8286920333622));
#449753=CARTESIAN_POINT('',(6.09734856608926,22.5,-4.44194770692244));
#449754=CARTESIAN_POINT('Origin',(5.65685387860011,22.5,-5.65685387860012));
#449755=CARTESIAN_POINT('Ctrl Pts',(4.74524035180399,22.756324918824,-6.5673434103921));
#449756=CARTESIAN_POINT('Ctrl Pts',(4.93595953019022,22.7414761952386,-6.75594870135602));
#449757=CARTESIAN_POINT('Ctrl Pts',(5.58182921801751,22.7027997814218,-7.1012121014615));
#449758=CARTESIAN_POINT('Ctrl Pts',(6.78713386963136,22.6402956773736,-6.68055232418451));
#449759=CARTESIAN_POINT('Ctrl Pts',(7.12528591239125,22.5697027613511,-5.27997950888059));
#449760=CARTESIAN_POINT('Ctrl Pts',(6.48370144903282,22.5229375355598,-4.58325719964658));
#449761=CARTESIAN_POINT('Ctrl Pts',(6.09735008669021,22.5,-4.44194158662797));
#449762=CARTESIAN_POINT('Origin',(5.65685387860011,26.993675081176,-5.65685387860012));
#449763=CARTESIAN_POINT('',(4.74299838399068,23.206324918824,-6.56983844394705));
#449764=CARTESIAN_POINT('',(4.74631652959707,23.168675081176,-6.56867439792569));
#449765=CARTESIAN_POINT('',(4.74468613086949,26.993675081176,-6.56902162633079));
#449766=CARTESIAN_POINT('Ctrl Pts',(4.74631652959707,23.168675081176,-6.56867439792569));
#449767=CARTESIAN_POINT('Ctrl Pts',(4.853408844765,23.1602325995332,-6.67716702479821));
#449768=CARTESIAN_POINT('Ctrl Pts',(5.33214451040115,23.127962427659,-7.02077633180239));
#449769=CARTESIAN_POINT('Ctrl Pts',(6.47507582842176,23.0718645655535,-6.94377741359719));
#449770=CARTESIAN_POINT('Ctrl Pts',(7.18181942856023,23.0003814948592,-5.66653874837813));
#449771=CARTESIAN_POINT('Ctrl Pts',(6.49141154940691,22.9288984241651,-4.38054591235379));
#449772=CARTESIAN_POINT('Ctrl Pts',(5.03639155729104,22.8574153534709,-4.26365553420012));
#449773=CARTESIAN_POINT('Ctrl Pts',(4.16730445086878,22.7873409058079,-5.40079341912851));
#449774=CARTESIAN_POINT('Ctrl Pts',(4.46059450521194,22.7410941483762,-6.28484325502835));
#449775=CARTESIAN_POINT('Ctrl Pts',(4.74364038176038,22.718675081176,-6.57057146528766));
#449776=CARTESIAN_POINT('Ctrl Pts',(4.74299838399068,23.206324918824,-6.56983844394705));
#449777=CARTESIAN_POINT('Ctrl Pts',(5.02227299078827,23.184442336627,-6.84584090104065));
#449778=CARTESIAN_POINT('Ctrl Pts',(5.8884730690954,23.1387320641985,-7.14533371342118));
#449779=CARTESIAN_POINT('Ctrl Pts',(7.03563221165043,23.0691941015387,-6.3084575374563));
#449780=CARTESIAN_POINT('Ctrl Pts',(6.95165327175697,22.9977110308445,-4.85119529970874));
#449781=CARTESIAN_POINT('Ctrl Pts',(5.68141376558385,22.9262279601503,-4.13204038713624));
#449782=CARTESIAN_POINT('Ctrl Pts',(4.38863987327371,22.8547448894562,-4.80994952176022));
#449783=CARTESIAN_POINT('Ctrl Pts',(4.28501879514302,22.7981105423474,-5.9617065202947));
#449784=CARTESIAN_POINT('Ctrl Pts',(4.62991319040622,22.76530388547,-6.45329450867432));
#449785=CARTESIAN_POINT('Ctrl Pts',(4.74524035180399,22.756324918824,-6.5673434103921));
#449786=CARTESIAN_POINT('Origin',(5.65685387860011,26.993675081176,-5.65685387860012));
#449787=CARTESIAN_POINT('',(4.74532300381163,23.656324918824,-6.57003272085371));
#449788=CARTESIAN_POINT('',(4.74499326893249,23.618675081176,-6.56740434249263));
#449789=CARTESIAN_POINT('',(4.74468613086949,26.993675081176,-6.56902162633079));
#449790=CARTESIAN_POINT('Ctrl Pts',(4.74499326893249,23.618675081176,-6.56740434249264));
#449791=CARTESIAN_POINT('Ctrl Pts',(4.94389036502613,23.6031987409216,-6.76368003125862));
#449792=CARTESIAN_POINT('Ctrl Pts',(5.60787864620878,23.5638947104357,-7.10715379447204));
#449793=CARTESIAN_POINT('Ctrl Pts',(6.81352117024561,23.5007629897185,-6.65070324968042));
#449794=CARTESIAN_POINT('Ctrl Pts',(7.11892889768229,23.4292799190243,-5.22331918686542));
#449795=CARTESIAN_POINT('Ctrl Pts',(6.08480364614364,23.3577968483302,-4.19313572939824));
#449796=CARTESIAN_POINT('Ctrl Pts',(4.65859667867589,23.2863137776359,-4.50398657889369));
#449797=CARTESIAN_POINT('Ctrl Pts',(4.20740365817457,23.2232731885846,-5.70962577012502));
#449798=CARTESIAN_POINT('Ctrl Pts',(4.55115618731809,23.1840602897646,-6.37096218895919));
#449799=CARTESIAN_POINT('Ctrl Pts',(4.74631652959707,23.168675081176,-6.56867439792569));
#449800=CARTESIAN_POINT('Ctrl Pts',(4.74532300381163,23.656324918824,-6.57003272085371));
#449801=CARTESIAN_POINT('Ctrl Pts',(4.80948437015677,23.6512361682467,-6.63539236159828));
#449802=CARTESIAN_POINT('Ctrl Pts',(5.21266771861286,23.622319727438,-6.9668858368575));
#449803=CARTESIAN_POINT('Ctrl Pts',(6.28682364983267,23.569575596398,-7.04564953674368));
#449804=CARTESIAN_POINT('Ctrl Pts',(7.16543624640093,23.4980925257038,-5.88000083782647));
#449805=CARTESIAN_POINT('Ctrl Pts',(6.66190630419616,23.4266094550096,-4.50990820099157));
#449806=CARTESIAN_POINT('Ctrl Pts',(5.23756146736659,23.3551263843154,-4.19063094092434));
#449807=CARTESIAN_POINT('Ctrl Pts',(4.19736598356861,23.2836433136212,-5.21468783779197));
#449808=CARTESIAN_POINT('Ctrl Pts',(4.40342562281452,23.2340428251241,-6.20635078283889));
#449809=CARTESIAN_POINT('Ctrl Pts',(4.71817410701172,23.2082700268584,-6.54530502316694));
#449810=CARTESIAN_POINT('Ctrl Pts',(4.74299838399068,23.206324918824,-6.56983844394705));
#449811=CARTESIAN_POINT('Origin',(5.65685387860011,26.993675081176,-5.65685387860012));
#449812=CARTESIAN_POINT('',(4.74613115927677,24.106324918824,-6.56748881619374));
#449813=CARTESIAN_POINT('',(4.74299681637215,24.068675081176,-6.57010232725217));
#449814=CARTESIAN_POINT('',(4.74468613086949,26.993675081176,-6.56902162633079));
#449815=CARTESIAN_POINT('Ctrl Pts',(4.74299681637215,24.068675081176,-6.57010232725218));
#449816=CARTESIAN_POINT('Ctrl Pts',(5.02972694085412,24.0461648823099,-6.85435514987614));
#449817=CARTESIAN_POINT('Ctrl Pts',(5.91736950865738,23.9998269932124,-7.14655186859909));
#449818=CARTESIAN_POINT('Ctrl Pts',(7.0522818436793,23.9296614138836,-6.27199288310558));
#449819=CARTESIAN_POINT('Ctrl Pts',(6.93003241982605,23.8581783431894,-4.81743049717126));
#449820=CARTESIAN_POINT('Ctrl Pts',(5.64131435190337,23.7866952724952,-4.13193628895796));
#449821=CARTESIAN_POINT('Ctrl Pts',(4.3668333837381,23.715212201801,-4.84355050202496));
#449822=CARTESIAN_POINT('Ctrl Pts',(4.29429575151248,23.6592054713613,-5.98491025846012));
#449823=CARTESIAN_POINT('Ctrl Pts',(4.63766432477859,23.627026431153,-6.4614899633887));
#449824=CARTESIAN_POINT('Ctrl Pts',(4.74499326893249,23.618675081176,-6.56740434249264));
#449825=CARTESIAN_POINT('Ctrl Pts',(4.74613115927677,24.106324918824,-6.56748881619374));
#449826=CARTESIAN_POINT('Ctrl Pts',(4.90119115627847,24.0942023096351,-6.72241589762581));
#449827=CARTESIAN_POINT('Ctrl Pts',(5.47210261995127,24.0582520102147,-7.07096798466868));
#449828=CARTESIAN_POINT('Ctrl Pts',(6.662968703113,23.998474020563,-6.80286792203874));
#449829=CARTESIAN_POINT('Ctrl Pts',(7.16522879152533,23.9269909498688,-5.43230911237055));
#449830=CARTESIAN_POINT('Ctrl Pts',(6.2855365564656,23.8555078791747,-4.26747512907024));
#449831=CARTESIAN_POINT('Ctrl Pts',(4.82985391579145,23.7840248084805,-4.37557081254884));
#449832=CARTESIAN_POINT('Ctrl Pts',(4.18154636230721,23.7176304883636,-5.56629788826614));
#449833=CARTESIAN_POINT('Ctrl Pts',(4.50905361827065,23.6750638584781,-6.32935078034096));
#449834=CARTESIAN_POINT('Ctrl Pts',(4.74532300381163,23.656324918824,-6.57003272085371));
#449835=CARTESIAN_POINT('Origin',(5.65685387860011,26.993675081176,-5.65685387860012));
#449836=CARTESIAN_POINT('',(4.74353459859835,24.556324918824,-6.56856700353347));
#449837=CARTESIAN_POINT('',(4.74557835604531,24.518675081176,-6.56980231202958));
#449838=CARTESIAN_POINT('',(4.74468613086949,26.993675081176,-6.56902162633079));
#449839=CARTESIAN_POINT('Ctrl Pts',(4.74557835604531,24.518675081176,-6.56980231202958));
#449840=CARTESIAN_POINT('Ctrl Pts',(4.81770944620421,24.5129587139297,-6.64326578517921));
#449841=CARTESIAN_POINT('Ctrl Pts',(5.23445549419879,24.4834146564519,-6.97750833641272));
#449842=CARTESIAN_POINT('Ctrl Pts',(6.32311258055821,24.4300429087428,-7.02860988272989));
#449843=CARTESIAN_POINT('Ctrl Pts',(7.17078066054311,24.3585598380486,-5.84026841822957));
#449844=CARTESIAN_POINT('Ctrl Pts',(6.63140987332417,24.2870767673545,-4.4838850778304));
#449845=CARTESIAN_POINT('Ctrl Pts',(5.19916430623342,24.2155936966603,-4.2021595986403));
#449846=CARTESIAN_POINT('Ctrl Pts',(4.18624762160045,24.1441106259661,-5.25320498229437));
#449847=CARTESIAN_POINT('Ctrl Pts',(4.41536649518845,24.095137754138,-6.22663461042285));
#449848=CARTESIAN_POINT('Ctrl Pts',(4.72621489163553,24.0699925725413,-6.55346539562853));
#449849=CARTESIAN_POINT('Ctrl Pts',(4.74299681637215,24.068675081176,-6.57010232725218));
#449850=CARTESIAN_POINT('Ctrl Pts',(4.74353459859835,24.556324918824,-6.56856700353346));
#449851=CARTESIAN_POINT('Ctrl Pts',(4.98945253222269,24.5371684510234,-6.81000592522228));
#449852=CARTESIAN_POINT('Ctrl Pts',(5.76578134653658,24.4941842929915,-7.13455935910424));
#449853=CARTESIAN_POINT('Ctrl Pts',(6.95240396480877,24.4273724447281,-6.46131966662841));
#449854=CARTESIAN_POINT('Ctrl Pts',(7.03502543671246,24.3558893740339,-5.00396921476326));
#449855=CARTESIAN_POINT('Ctrl Pts',(5.85498510857852,24.2844063033397,-4.14478270244581));
#449856=CARTESIAN_POINT('Ctrl Pts',(4.49341967622111,24.2129232326456,-4.67093497503137));
#449857=CARTESIAN_POINT('Ctrl Pts',(4.24791389261248,24.1535627711403,-5.85795834238072));
#449858=CARTESIAN_POINT('Ctrl Pts',(4.5964117545626,24.1180299998665,-6.41789774915756));
#449859=CARTESIAN_POINT('Ctrl Pts',(4.74613115927677,24.106324918824,-6.56748881619374));
#449860=CARTESIAN_POINT('Origin',(5.65685387860011,26.993675081176,-5.65685387860012));
#449861=CARTESIAN_POINT('',(4.74405758279953,25.006324918824,-6.57067994464874));
#449862=CARTESIAN_POINT('',(4.74597172529335,24.968675081176,-6.56738667375376));
#449863=CARTESIAN_POINT('',(4.74468613086949,26.993675081176,-6.56902162633079));
#449864=CARTESIAN_POINT('Ctrl Pts',(4.74597172529335,24.968675081176,-6.56738667375376));
#449865=CARTESIAN_POINT('Ctrl Pts',(4.90925551921452,24.955924855318,-6.73011316031215));
#449866=CARTESIAN_POINT('Ctrl Pts',(5.49691387622178,24.9193469392286,-7.0784783223036));
#449867=CARTESIAN_POINT('Ctrl Pts',(6.69274573713214,24.8589413329079,-6.77602463836695));
#449868=CARTESIAN_POINT('Ctrl Pts',(7.15880506797054,24.7874582622137,-5.39273679116275));
#449869=CARTESIAN_POINT('Ctrl Pts',(6.24879737998679,24.7159751915195,-4.25142935492228));
#449870=CARTESIAN_POINT('Ctrl Pts',(4.79645922145989,24.6444921208253,-4.39775252453571));
#449871=CARTESIAN_POINT('Ctrl Pts',(4.18550614000559,24.5787254173775,-5.59369688000734));
#449872=CARTESIAN_POINT('Ctrl Pts',(4.51704344657683,24.5367864041611,-6.33704597702196));
#449873=CARTESIAN_POINT('Ctrl Pts',(4.74557835604531,24.518675081176,-6.56980231202958));
#449874=CARTESIAN_POINT('Ctrl Pts',(4.74405758279953,25.006324918824,-6.57067994464874));
#449875=CARTESIAN_POINT('Ctrl Pts',(4.77384081402403,25.0039622826432,-6.60086819803687));
#449876=CARTESIAN_POINT('Ctrl Pts',(5.12098437694123,24.9777719562309,-6.91811250300101));
#449877=CARTESIAN_POINT('Ctrl Pts',(6.12447699388038,24.9277539395874,-7.10838527255516));
#449878=CARTESIAN_POINT('Ctrl Pts',(7.13018513270865,24.8562708688931,-6.05044038944422));
#449879=CARTESIAN_POINT('Ctrl Pts',(6.78604742232836,24.784787798199,-4.63189669239788));
#449880=CARTESIAN_POINT('Ctrl Pts',(5.40735816264999,24.7133047275048,-4.15240479236239));
#449881=CARTESIAN_POINT('Ctrl Pts',(4.25725342975252,24.6418216568106,-5.0512683537124));
#449882=CARTESIAN_POINT('Ctrl Pts',(4.35401829743014,24.589495053917,-6.11539165852711));
#449883=CARTESIAN_POINT('Ctrl Pts',(4.68356856625642,24.5609961412548,-6.50969315902277));
#449884=CARTESIAN_POINT('Ctrl Pts',(4.74353459859835,24.556324918824,-6.56856700353346));
#449885=CARTESIAN_POINT('Origin',(5.65685387860011,26.993675081176,-5.65685387860012));
#449886=CARTESIAN_POINT('',(4.74640124271564,25.456324918824,-6.56829321884323));
#449887=CARTESIAN_POINT('',(4.74334636410459,25.418675081176,-6.56885365284802));
#449888=CARTESIAN_POINT('',(4.74468613086949,26.993675081176,-6.56902162633079));
#449889=CARTESIAN_POINT('Ctrl Pts',(4.74334636410459,25.418675081176,-6.56885365284802));
#449890=CARTESIAN_POINT('Ctrl Pts',(4.99707565976646,25.3988909967064,-6.81811011972481));
#449891=CARTESIAN_POINT('Ctrl Pts',(5.79361205385018,25.3552792220053,-7.13780202337966));
#449892=CARTESIAN_POINT('Ctrl Pts',(6.97310209577086,25.287839757073,-6.42698533143036));
#449893=CARTESIAN_POINT('Ctrl Pts',(7.01738753624157,25.2163566863788,-4.96796792520408));
#449894=CARTESIAN_POINT('Ctrl Pts',(5.81516935358236,25.1448736156846,-4.14009680960707));
#449895=CARTESIAN_POINT('Ctrl Pts',(4.46790543942481,25.0733905449904,-4.70185841202445));
#449896=CARTESIAN_POINT('Ctrl Pts',(4.25595199715398,25.0146577001542,-5.88231068328694));
#449897=CARTESIAN_POINT('Ctrl Pts',(4.604109892408,24.9797525455494,-6.4260090324839));
#449898=CARTESIAN_POINT('Ctrl Pts',(4.74597172529335,24.968675081176,-6.56738667375376));
#449899=CARTESIAN_POINT('Ctrl Pts',(4.74640124271564,25.456324918824,-6.56829321884323));
#449900=CARTESIAN_POINT('Ctrl Pts',(4.86586022639608,25.4469284240315,-6.68893848409318));
#449901=CARTESIAN_POINT('Ctrl Pts',(5.36752678600608,25.4137042390077,-7.03476003379299));
#449902=CARTESIAN_POINT('Ctrl Pts',(6.5258341885166,25.3566523637524,-6.9100356033464));
#449903=CARTESIAN_POINT('Ctrl Pts',(7.18099123031483,25.2851692930582,-5.60564496305001));
#449904=CARTESIAN_POINT('Ctrl Pts',(6.43975200870338,25.213686222364,-4.34815567114858));
#449905=CARTESIAN_POINT('Ctrl Pts',(4.98123363545819,25.1422031516699,-4.2896855842815));
#449906=CARTESIAN_POINT('Ctrl Pts',(4.16945626611646,25.0730827171565,-5.44432497425889));
#449907=CARTESIAN_POINT('Ctrl Pts',(4.47347056935133,25.0277899728745,-6.29641321838457));
#449908=CARTESIAN_POINT('Ctrl Pts',(4.74405758279953,25.006324918824,-6.57067994464874));
#449909=CARTESIAN_POINT('Origin',(5.65685387860011,26.993675081176,-5.65685387860012));
#449910=CARTESIAN_POINT('',(4.74450601134849,25.906324918824,-6.56704169373441));
#449911=CARTESIAN_POINT('',(4.74432962138981,25.868675081176,-6.57057130100612));
#449912=CARTESIAN_POINT('',(4.74468613086949,26.993675081176,-6.56902162633079));
#449913=CARTESIAN_POINT('',(4.53900700771687,26.,-5.01302286563433));
#449914=CARTESIAN_POINT('Ctrl Pts',(4.53900700771688,26.,-5.01302286563431));
#449915=CARTESIAN_POINT('Ctrl Pts',(4.32480615636363,25.9761723097686,-5.38492752167559));
#449916=CARTESIAN_POINT('Ctrl Pts',(4.30899334914827,25.9449472827099,-6.01924597306242));
#449917=CARTESIAN_POINT('Ctrl Pts',(4.64940368207851,25.9137222556513,-6.47338425157137));
#449918=CARTESIAN_POINT('Ctrl Pts',(4.74450601134849,25.906324918824,-6.56704169373441));
#449919=CARTESIAN_POINT('',(5.01208503488091,26.,-4.53689596693371));
#449920=CARTESIAN_POINT('Origin',(5.65685387860011,26.,-5.65685387860012));
#449921=CARTESIAN_POINT('Ctrl Pts',(5.01208247494518,26.,-4.5368902045627));
#449922=CARTESIAN_POINT('Ctrl Pts',(4.65613984562121,25.9770624644402,-4.74314812622022));
#449923=CARTESIAN_POINT('Ctrl Pts',(4.17795197796789,25.9332874914989,-5.48969900651177));
#449924=CARTESIAN_POINT('Ctrl Pts',(4.48184576512937,25.8895125185575,-6.3039677816093));
#449925=CARTESIAN_POINT('Ctrl Pts',(4.74432962138981,25.868675081176,-6.57057130100612));
#449926=CARTESIAN_POINT('Origin',(-5.65685387860012,26.,-5.65685387860011));
#449927=CARTESIAN_POINT('',(-6.39190072013885,22.573038475773,-4.9222125558517));
#449928=CARTESIAN_POINT('',(-6.39065394077646,22.5,-4.92305381642377));
#449929=CARTESIAN_POINT('',(-6.39065394077646,26.,-4.92305381642377));
#449930=CARTESIAN_POINT('',(-6.66622270032004,22.5,-5.8978925564917));
#449931=CARTESIAN_POINT('Origin',(-5.65685387860012,22.5,-5.65685387860011));
#449932=CARTESIAN_POINT('Ctrl Pts',(-6.66798006829997,22.5,-5.89851203167784));
#449933=CARTESIAN_POINT('Ctrl Pts',(-6.7439998684947,22.5229375355598,-5.5764199513446));
#449934=CARTESIAN_POINT('Ctrl Pts',(-6.65366449057419,22.5458750711197,
-5.21379162224851));
#449935=CARTESIAN_POINT('Ctrl Pts',(-6.43383171727969,22.5688126066795,
-4.96646199655034));
#449936=CARTESIAN_POINT('Ctrl Pts',(-6.42033150900063,22.5702212297106,
-4.95127317183385));
#449937=CARTESIAN_POINT('Ctrl Pts',(-6.40634292159547,22.5716298527418,
-4.93651917810251));
#449938=CARTESIAN_POINT('Ctrl Pts',(-6.39190072013885,22.573038475773,-4.9222125558517));
#449939=CARTESIAN_POINT('Origin',(-5.65685387860012,26.,-5.65685387860011));
#449940=CARTESIAN_POINT('',(-6.39037461032892,23.0230384757729,-4.92436540268704));
#449941=CARTESIAN_POINT('',(-6.38930388760559,22.9019615242271,-4.92349966353597));
#449942=CARTESIAN_POINT('',(-6.39065394077646,26.,-4.92305381642377));
#449943=CARTESIAN_POINT('',(-5.77557608073439,22.5,-4.62591736201901));
#449944=CARTESIAN_POINT('Ctrl Pts',(-6.38930388760559,22.9019615242271,
-4.92349966353597));
#449945=CARTESIAN_POINT('Ctrl Pts',(-6.54102880287524,22.8871128006417,
-5.07692511110986));
#449946=CARTESIAN_POINT('Ctrl Pts',(-6.64766299899898,22.8722640770563,
-5.27640120658105));
#449947=CARTESIAN_POINT('Ctrl Pts',(-6.68249361011691,22.8574153534709,
-5.48772889025785));
#449948=CARTESIAN_POINT('Ctrl Pts',(-6.73838615923167,22.8335876632395,
-5.82684562005693));
#449949=CARTESIAN_POINT('Ctrl Pts',(-6.60938089562333,22.8097599730081,
-6.19648078060475));
#449950=CARTESIAN_POINT('Ctrl Pts',(-6.35472685290066,22.7859322827767,
-6.42720821100081));
#449951=CARTESIAN_POINT('Ctrl Pts',(-6.10007281017799,22.7621045925453,
-6.65793564139688));
#449952=CARTESIAN_POINT('Ctrl Pts',(-5.71976998834099,22.7382769023139,
-6.74975534164119));
#449953=CARTESIAN_POINT('Ctrl Pts',(-5.38773213421059,22.7144492120825,
-6.66080060824128));
#449954=CARTESIAN_POINT('Ctrl Pts',(-5.05569428008018,22.6906215218511,
-6.57184587484137));
#449955=CARTESIAN_POINT('Ctrl Pts',(-4.77192139365638,22.6667938316197,
-6.30211670779724));
#449956=CARTESIAN_POINT('Ctrl Pts',(-4.66700870222797,22.6429661413884,
-5.97477550103877));
#449957=CARTESIAN_POINT('Ctrl Pts',(-4.56209601079956,22.619138451157,-5.6474342942803));
#449958=CARTESIAN_POINT('Ctrl Pts',(-4.63604351436656,22.5953107609256,
-5.26248104780748));
#449959=CARTESIAN_POINT('Ctrl Pts',(-4.85366607828882,22.5714830706942,
-4.99722717517853));
#449960=CARTESIAN_POINT('Ctrl Pts',(-5.07128864221107,22.5476553804628,
-4.73197330254959));
#449961=CARTESIAN_POINT('Ctrl Pts',(-5.43258626648858,22.5238276902314,
-4.58641880376449));
#449962=CARTESIAN_POINT('Ctrl Pts',(-5.77557608073438,22.5,-4.625917362019));
#449963=CARTESIAN_POINT('Origin',(-5.65685387860012,22.5,-5.65685387860011));
#449964=CARTESIAN_POINT('Ctrl Pts',(-6.39190072013885,22.573038475773,-4.9222125558517));
#449965=CARTESIAN_POINT('Ctrl Pts',(-6.16204455719575,22.5954575429732,
-4.69451421601594));
#449966=CARTESIAN_POINT('Ctrl Pts',(-5.81728522517979,22.6178766101734,
-4.58013776446743));
#449967=CARTESIAN_POINT('Ctrl Pts',(-5.49777863793003,22.6402956773736,
-4.62964039434809));
#449968=CARTESIAN_POINT('Ctrl Pts',(-5.15819698094666,22.664123367605,-4.68225334741615));
#449969=CARTESIAN_POINT('Ctrl Pts',(-4.8471410957032,22.6879510578364,-4.91998587117151));
#449970=CARTESIAN_POINT('Ctrl Pts',(-4.70728537400252,22.7117787480678,
-5.23393572436937));
#449971=CARTESIAN_POINT('Ctrl Pts',(-4.56742965230184,22.7356064382992,
-5.54788557756724));
#449972=CARTESIAN_POINT('Ctrl Pts',(-4.59877409414395,22.7594341285306,
-5.93805276020761));
#449973=CARTESIAN_POINT('Ctrl Pts',(-4.78686738296995,22.783261818762,-6.22570363532513));
#449974=CARTESIAN_POINT('Ctrl Pts',(-4.97496067179595,22.8070895089934,
-6.51335451044265));
#449975=CARTESIAN_POINT('Ctrl Pts',(-5.31980280760584,22.8309171992248,
-6.69848907803731));
#449976=CARTESIAN_POINT('Ctrl Pts',(-5.66347121722023,22.8547448894562,
-6.69629884619592));
#449977=CARTESIAN_POINT('Ctrl Pts',(-6.00713962683461,22.8785725796876,
-6.69410861435453));
#449978=CARTESIAN_POINT('Ctrl Pts',(-6.34963431025348,22.902400269919,-6.5045935830771));
#449979=CARTESIAN_POINT('Ctrl Pts',(-6.53403672593788,22.9262279601503,
-6.21456908983246));
#449980=CARTESIAN_POINT('Ctrl Pts',(-6.71843914162228,22.9500556503817,
-5.92454459658782));
#449981=CARTESIAN_POINT('Ctrl Pts',(-6.7447492895722,22.9738833406131,-5.53401064137597));
#449982=CARTESIAN_POINT('Ctrl Pts',(-6.60092695407667,22.9977110308445,
-5.22186823831326));
#449983=CARTESIAN_POINT('Ctrl Pts',(-6.54996870275417,23.0061535124873,
-5.11127184889382));
#449984=CARTESIAN_POINT('Ctrl Pts',(-6.47765230299322,23.0145959941301,
-5.0105166042882));
#449985=CARTESIAN_POINT('Ctrl Pts',(-6.39037461032892,23.0230384757729,
-4.92436540268704));
#449986=CARTESIAN_POINT('Origin',(-5.65685387860012,26.,-5.65685387860011));
#449987=CARTESIAN_POINT('',(-6.38935290488262,23.4730384757729,-4.92330089590042));
#449988=CARTESIAN_POINT('',(-6.3913110357232,23.3519615242271,-4.92169609601798));
#449989=CARTESIAN_POINT('',(-6.39065394077646,26.,-4.92305381642377));
#449990=CARTESIAN_POINT('Ctrl Pts',(-6.3913110357232,23.3519615242271,-4.92169609601798));
#449991=CARTESIAN_POINT('Ctrl Pts',(-6.61334324490838,23.33007894203,-5.14636061012976));
#449992=CARTESIAN_POINT('Ctrl Pts',(-6.72868171719176,23.308196359833,-5.47994522249351));
#449993=CARTESIAN_POINT('Ctrl Pts',(-6.68738448495221,23.286313777636,-5.79285848911253));
#449994=CARTESIAN_POINT('Ctrl Pts',(-6.64241640721999,23.2624860874046,
-6.1335861198444));
#449995=CARTESIAN_POINT('Ctrl Pts',(-6.41172882390928,23.2386583971732,
-6.44980419113038));
#449996=CARTESIAN_POINT('Ctrl Pts',(-6.10100080909856,23.2148307069418,
-6.59665364733223));
#449997=CARTESIAN_POINT('Ctrl Pts',(-5.79027279428784,23.1910030167104,
-6.74350310353408));
#449998=CARTESIAN_POINT('Ctrl Pts',(-5.39950434797711,23.167175326479,-6.7209839446518));
#449999=CARTESIAN_POINT('Ctrl Pts',(-5.1076985472349,23.1433476362476,-6.539415444341));
#450000=CARTESIAN_POINT('Ctrl Pts',(-4.8158927464927,23.1195199460162,-6.3578469440302));
#450001=CARTESIAN_POINT('Ctrl Pts',(-4.62304959131903,23.0956922557848,
-6.01722910229088));
#450002=CARTESIAN_POINT('Ctrl Pts',(-4.61751951301592,23.0718645655534,
-5.67358993507176));
#450003=CARTESIAN_POINT('Ctrl Pts',(-4.61198943471281,23.048036875322,-5.32995076785264));
#450004=CARTESIAN_POINT('Ctrl Pts',(-4.79377243328026,23.0242091850907,
-4.98329027515371));
#450005=CARTESIAN_POINT('Ctrl Pts',(-5.07957475014376,23.0003814948593,
-4.7924243254548));
#450006=CARTESIAN_POINT('Ctrl Pts',(-5.36537706700727,22.9765538046279,
-4.60155837575589));
#450007=CARTESIAN_POINT('Ctrl Pts',(-5.75519870216683,22.9527261143965,
-4.56648696905699));
#450008=CARTESIAN_POINT('Ctrl Pts',(-6.07050470066555,22.9288984241651,
-4.70325041523271));
#450009=CARTESIAN_POINT('Ctrl Pts',(-6.18932117076026,22.9199194575191,
-4.75478685916323));
#450010=CARTESIAN_POINT('Ctrl Pts',(-6.29755640872372,22.9109404908731,
-4.830723879241));
#450011=CARTESIAN_POINT('Ctrl Pts',(-6.38930388760559,22.9019615242271,
-4.92349966353597));
#450012=CARTESIAN_POINT('Ctrl Pts',(-6.39037461032892,23.0230384757729,
-4.92436540268704));
#450013=CARTESIAN_POINT('Ctrl Pts',(-6.23132356780567,23.0384236843615,
-4.76736722811336));
#450014=CARTESIAN_POINT('Ctrl Pts',(-6.02258634020352,23.0538088929501,
-4.65886881811934));
#450015=CARTESIAN_POINT('Ctrl Pts',(-5.80287677492702,23.0691941015387,
-4.62769529041208));
#450016=CARTESIAN_POINT('Ctrl Pts',(-5.46260375021388,23.0930217917701,
-4.57941559648716));
#450017=CARTESIAN_POINT('Ctrl Pts',(-5.09601251972857,23.1168494820015,
-4.71660705955086));
#450018=CARTESIAN_POINT('Ctrl Pts',(-4.87103919530453,23.1406771722329,
-4.97642324075838));
#450019=CARTESIAN_POINT('Ctrl Pts',(-4.64606587088049,23.1645048624643,
-5.23623942196589));
#450020=CARTESIAN_POINT('Ctrl Pts',(-4.56271045251773,23.1883325526957,
-5.61868032131723));
#450021=CARTESIAN_POINT('Ctrl Pts',(-4.65915585483332,23.2121602429271,
-5.94855238336812));
#450022=CARTESIAN_POINT('Ctrl Pts',(-4.75560125714891,23.2359879331585,
-6.27842444541901));
#450023=CARTESIAN_POINT('Ctrl Pts',(-5.03184748014285,23.2598156233899,
-6.55572767016945));
#450024=CARTESIAN_POINT('Ctrl Pts',(-5.36134886181892,23.2836433136212,
-6.65343136663416));
#450025=CARTESIAN_POINT('Ctrl Pts',(-5.690850243495,23.3074710038526,-6.75113506309887));
#450026=CARTESIAN_POINT('Ctrl Pts',(-6.07360678385322,23.331298694084,-6.66923923127783));
#450027=CARTESIAN_POINT('Ctrl Pts',(-6.33427992409048,23.3551263843154,
-6.4452597843657));
#450028=CARTESIAN_POINT('Ctrl Pts',(-6.59495306432775,23.3789540745468,
-6.22128033745358));
#450029=CARTESIAN_POINT('Ctrl Pts',(-6.73354280444407,23.4027817647782,
-5.85521727545038));
#450030=CARTESIAN_POINT('Ctrl Pts',(-6.6865623548039,23.4266094550096,-5.51476156795534));
#450031=CARTESIAN_POINT('Ctrl Pts',(-6.65604804910002,23.442085795264,-5.29363193601897));
#450032=CARTESIAN_POINT('Ctrl Pts',(-6.54724832815155,23.4575621355185,
-5.08330512959901));
#450033=CARTESIAN_POINT('Ctrl Pts',(-6.38935290488262,23.4730384757729,
-4.92330089590042));
#450034=CARTESIAN_POINT('Origin',(-5.65685387860012,26.,-5.65685387860011));
#450035=CARTESIAN_POINT('',(-6.39152331859132,23.9230384757729,-4.9216948349357));
#450036=CARTESIAN_POINT('',(-6.39146732321148,23.8019615242271,-4.92356615355223));
#450037=CARTESIAN_POINT('',(-6.39065394077646,26.,-4.92305381642377));
#450038=CARTESIAN_POINT('Ctrl Pts',(-6.39146732321148,23.8019615242271,
-4.92356615355223));
#450039=CARTESIAN_POINT('Ctrl Pts',(-6.44404636753914,23.7968727736498,
-4.97518123721477));
#450040=CARTESIAN_POINT('Ctrl Pts',(-6.49097569651667,23.7917840230725,
-5.03225965778749));
#450041=CARTESIAN_POINT('Ctrl Pts',(-6.53072214720976,23.7866952724952,
-5.09396482100832));
#450042=CARTESIAN_POINT('Ctrl Pts',(-6.71683190058211,23.7628675822638,
-5.38289458727869));
#450043=CARTESIAN_POINT('Ctrl Pts',(-6.74545633697037,23.7390398920324,
-5.77326614382955));
#450044=CARTESIAN_POINT('Ctrl Pts',(-6.60348277515141,23.715212201801,-6.08625298439034));
#450045=CARTESIAN_POINT('Ctrl Pts',(-6.46150921333244,23.6913845115696,
-6.39923982495114));
#450046=CARTESIAN_POINT('Ctrl Pts',(-6.14893765330626,23.6675568213382,
-6.63484194952187));
#450047=CARTESIAN_POINT('Ctrl Pts',(-5.80895502137128,23.6437291311068,
-6.68513161677842));
#450048=CARTESIAN_POINT('Ctrl Pts',(-5.4689723894363,23.6199014408755,-6.73542128403497));
#450049=CARTESIAN_POINT('Ctrl Pts',(-5.10157868559252,23.5960737506441,
-6.60039849397735));
#450050=CARTESIAN_POINT('Ctrl Pts',(-4.87507434314934,23.5722460604127,
-6.34191631672375));
#450051=CARTESIAN_POINT('Ctrl Pts',(-4.64857000070616,23.5484183701813,
-6.08343413947014));
#450052=CARTESIAN_POINT('Ctrl Pts',(-4.56295501966359,23.5245906799499,
-5.70149257502055));
#450053=CARTESIAN_POINT('Ctrl Pts',(-4.65744921450722,23.5007629897185,
-5.37105630657982));
#450054=CARTESIAN_POINT('Ctrl Pts',(-4.75194340935084,23.4769352994871,
-5.04062003813909));
#450055=CARTESIAN_POINT('Ctrl Pts',(-5.02654678008065,23.4531076092557,
-4.76168906570723));
#450056=CARTESIAN_POINT('Ctrl Pts',(-5.35546505814245,23.4292799190243,
-4.66203997694959));
#450057=CARTESIAN_POINT('Ctrl Pts',(-5.68438333620426,23.4054522287929,
-4.56239088819195));
#450058=CARTESIAN_POINT('Ctrl Pts',(-6.06761652159808,23.3816245385615,
-4.64202368310855));
#450059=CARTESIAN_POINT('Ctrl Pts',(-6.32960882821811,23.3577968483301,
-4.86445867565572));
#450060=CARTESIAN_POINT('Ctrl Pts',(-6.350995850443,23.3558517402958,-4.88261654521522));
#450061=CARTESIAN_POINT('Ctrl Pts',(-6.37157494470416,23.3539066322614,
-4.90172602358781));
#450062=CARTESIAN_POINT('Ctrl Pts',(-6.3913110357232,23.3519615242271,-4.92169609601798));
#450063=CARTESIAN_POINT('Ctrl Pts',(-6.38935290488262,23.4730384757729,
-4.92330089590042));
#450064=CARTESIAN_POINT('Ctrl Pts',(-6.30414930262286,23.4813898257499,
-4.83695933636888));
#450065=CARTESIAN_POINT('Ctrl Pts',(-6.20464951053553,23.4897411757268,
-4.76527121936352));
#450066=CARTESIAN_POINT('Ctrl Pts',(-6.09544017298549,23.4980925257038,
-4.71444637045848));
#450067=CARTESIAN_POINT('Ctrl Pts',(-5.78384908020389,23.5219202159352,
-4.56943523344352));
#450068=CARTESIAN_POINT('Ctrl Pts',(-5.39321753403732,23.5457479061666,
-4.59426131240047));
#450069=CARTESIAN_POINT('Ctrl Pts',(-5.10249121190879,23.569575596398,-4.77755195197114));
#450070=CARTESIAN_POINT('Ctrl Pts',(-4.81176488978025,23.5934032866293,
-4.9608425915418));
#450071=CARTESIAN_POINT('Ctrl Pts',(-4.62094379168974,23.6172309768607,
-5.30259779172617));
#450072=CARTESIAN_POINT('Ctrl Pts',(-4.61744171997954,23.6410586670921,
-5.64626184853499));
#450073=CARTESIAN_POINT('Ctrl Pts',(-4.61393964826935,23.6648863573235,
-5.98992590534381));
#450074=CARTESIAN_POINT('Ctrl Pts',(-4.79775660293947,23.6887140475549,
-6.33549881877709));
#450075=CARTESIAN_POINT('Ctrl Pts',(-5.08468731748426,23.7125417377863,
-6.52467601704459));
#450076=CARTESIAN_POINT('Ctrl Pts',(-5.37161803202905,23.7363694280177,
-6.71385321531209));
#450077=CARTESIAN_POINT('Ctrl Pts',(-5.76166250644852,23.7601971182491,
-6.74663469841383));
#450078=CARTESIAN_POINT('Ctrl Pts',(-6.07614404554655,23.7840248084805,
-6.60800349462427));
#450079=CARTESIAN_POINT('Ctrl Pts',(-6.39062558464459,23.8078524987119,
-6.46937229083472));
#450080=CARTESIAN_POINT('Ctrl Pts',(-6.6295441884212,23.8316801889433,-6.15932840015388));
#450081=CARTESIAN_POINT('Ctrl Pts',(-6.6834528935629,23.8555078791747,-5.81990079386588));
#450082=CARTESIAN_POINT('Ctrl Pts',(-6.73438085433327,23.8780180780408,
-5.49924097144978));
#450083=CARTESIAN_POINT('Ctrl Pts',(-6.62019259508593,23.9005282769068,
-5.15235699515365));
#450084=CARTESIAN_POINT('Ctrl Pts',(-6.39152331859132,23.9230384757729,
-4.9216948349357));
#450085=CARTESIAN_POINT('Origin',(-5.65685387860012,26.,-5.65685387860011));
#450086=CARTESIAN_POINT('',(-6.39128196913613,24.3730384757729,-4.92377157353715));
#450087=CARTESIAN_POINT('',(-6.38942086037359,24.2519615242271,-4.92421628016771));
#450088=CARTESIAN_POINT('',(-6.39065394077646,26.,-4.92305381642377));
#450089=CARTESIAN_POINT('Ctrl Pts',(-6.38942086037359,24.2519615242271,
-4.92421628016771));
#450090=CARTESIAN_POINT('Ctrl Pts',(-6.51405309196749,24.2398389150381,
-5.04895543667044));
#450091=CARTESIAN_POINT('Ctrl Pts',(-6.60860369693141,24.2277163058492,
-5.20382475542584));
#450092=CARTESIAN_POINT('Ctrl Pts',(-6.65652287894995,24.2155936966603,
-5.37198243345446));
#450093=CARTESIAN_POINT('Ctrl Pts',(-6.75071080561528,24.1917660064289,
-5.70250608555364));
#450094=CARTESIAN_POINT('Ctrl Pts',(-6.66474206054895,24.1679383161975,
-6.08436822205294));
#450095=CARTESIAN_POINT('Ctrl Pts',(-6.4379983333991,24.1441106259661,-6.34264042812557));
#450096=CARTESIAN_POINT('Ctrl Pts',(-6.21125460624925,24.1202829357347,
-6.60091263419821));
#450097=CARTESIAN_POINT('Ctrl Pts',(-5.84373589701587,24.0964552455033,
-6.73559490984418));
#450098=CARTESIAN_POINT('Ctrl Pts',(-5.5037999963824,24.0726275552719,-6.68499023152592));
#450099=CARTESIAN_POINT('Ctrl Pts',(-5.16386409574893,24.0487998650405,
-6.63438555320766));
#450100=CARTESIAN_POINT('Ctrl Pts',(-4.85151100371537,24.0249721748091,
-6.39849392092517));
#450101=CARTESIAN_POINT('Ctrl Pts',(-4.70982751913656,24.0011444845777,
-6.08537566804496));
#450102=CARTESIAN_POINT('Ctrl Pts',(-4.56814403455775,23.9773167943464,
-5.77225741516475));
#450103=CARTESIAN_POINT('Ctrl Pts',(-4.59713015743369,23.9534891041149,
-5.38191254168682));
#450104=CARTESIAN_POINT('Ctrl Pts',(-4.78350754767415,23.9296614138835,
-5.09315534403941));
#450105=CARTESIAN_POINT('Ctrl Pts',(-4.96988493791459,23.9058337236522,
-4.804398146392));
#450106=CARTESIAN_POINT('Ctrl Pts',(-5.31365359551954,23.8820060334208,
-4.61722862457511));
#450107=CARTESIAN_POINT('Ctrl Pts',(-5.65733545950024,23.8581783431894,
-4.6173878516616));
#450108=CARTESIAN_POINT('Ctrl Pts',(-5.92761905169082,23.8394394035353,
-4.61751307348277));
#450109=CARTESIAN_POINT('Ctrl Pts',(-6.19784896370209,23.8207004638812,
-4.73349750638545));
#450110=CARTESIAN_POINT('Ctrl Pts',(-6.39146732321148,23.8019615242271,
-4.92356615355223));
#450111=CARTESIAN_POINT('Ctrl Pts',(-6.39152331859132,23.9230384757729,
-4.9216948349357));
#450112=CARTESIAN_POINT('Ctrl Pts',(-6.37813961642664,23.9243559671382,
-4.90819449199352));
#450113=CARTESIAN_POINT('Ctrl Pts',(-6.3643637478711,23.9256734585035,-4.895092278726));
#450114=CARTESIAN_POINT('Ctrl Pts',(-6.35020586507153,23.9269909498688,
-4.88241675495565));
#450115=CARTESIAN_POINT('Ctrl Pts',(-6.0941513249317,23.9508186401002,-4.65317164422858));
#450116=CARTESIAN_POINT('Ctrl Pts',(-5.71314343814525,23.9746463303316,
-4.56349274466962));
#450117=CARTESIAN_POINT('Ctrl Pts',(-5.38171929489582,23.998474020563,-4.6544613426263));
#450118=CARTESIAN_POINT('Ctrl Pts',(-5.0502951516464,24.0223017107944,-4.74542994058297));
#450119=CARTESIAN_POINT('Ctrl Pts',(-4.76845475193401,24.0461294010258,
-5.01704603605528));
#450120=CARTESIAN_POINT('Ctrl Pts',(-4.6653072414873,24.0699570912572,-5.34488416612327));
#450121=CARTESIAN_POINT('Ctrl Pts',(-4.56215973104059,24.0937847814886,
-5.67272229619127));
#450122=CARTESIAN_POINT('Ctrl Pts',(-4.63770510985959,24.11761247172,-6.05678246085496));
#450123=CARTESIAN_POINT('Ctrl Pts',(-4.8573365604447,24.1414401619514,-6.32112934350159));
#450124=CARTESIAN_POINT('Ctrl Pts',(-5.07696801102981,24.1652678521828,
-6.58547622614821));
#450125=CARTESIAN_POINT('Ctrl Pts',(-5.44068553338104,24.1890955424141,
-6.73010982677778));
#450126=CARTESIAN_POINT('Ctrl Pts',(-5.78187263496817,24.2129232326455,
-6.68877448884911));
#450127=CARTESIAN_POINT('Ctrl Pts',(-6.12305973655531,24.2367509228769,
-6.64743915092045));
#450128=CARTESIAN_POINT('Ctrl Pts',(-6.44171641737836,24.2605786131083,
-6.42013487443355));
#450129=CARTESIAN_POINT('Ctrl Pts',(-6.59186824658804,24.2844063033397,
-6.11098818332588));
#450130=CARTESIAN_POINT('Ctrl Pts',(-6.74202007579772,24.3082339935711,
-5.80184149221821));
#450131=CARTESIAN_POINT('Ctrl Pts',(-6.72366705339403,24.3320616838025,
-5.41085238648977));
#450132=CARTESIAN_POINT('Ctrl Pts',(-6.54521657215205,24.3558893740339,
-5.11713028264445));
#450133=CARTESIAN_POINT('Ctrl Pts',(-6.50240552012982,24.3616057412803,
-5.04666506349635));
#450134=CARTESIAN_POINT('Ctrl Pts',(-6.45038020112141,24.3673221085266,
-4.98179796021342));
#450135=CARTESIAN_POINT('Ctrl Pts',(-6.39128196913613,24.3730384757729,
-4.92377157353715));
#450136=CARTESIAN_POINT('Origin',(-5.65685387860012,26.,-5.65685387860011));
#450137=CARTESIAN_POINT('',(-6.38933869113556,24.8230384757729,-4.92408802232565));
#450138=CARTESIAN_POINT('',(-6.39028821611916,24.7019615242271,-4.92212745780798));
#450139=CARTESIAN_POINT('',(-6.39065394077646,26.,-4.92305381642377));
#450140=CARTESIAN_POINT('Ctrl Pts',(-6.39028821611916,24.7019615242271,
-4.92212745780798));
#450141=CARTESIAN_POINT('Ctrl Pts',(-6.5845155347103,24.6828050564265,-5.11995795053563));
#450142=CARTESIAN_POINT('Ctrl Pts',(-6.70087353526984,24.6636485886259,
-5.39828521249021));
#450143=CARTESIAN_POINT('Ctrl Pts',(-6.69616935490973,24.6444921208254,
-5.67455106061111));
#450144=CARTESIAN_POINT('Ctrl Pts',(-6.69031808036474,24.620664430594,-6.01818314973456));
#450145=CARTESIAN_POINT('Ctrl Pts',(-6.49716519325234,24.5968367403626,
-6.35862591802897));
#450146=CARTESIAN_POINT('Ctrl Pts',(-6.20519269912468,24.5730090501312,
-6.53992487743045));
#450147=CARTESIAN_POINT('Ctrl Pts',(-5.91322020499702,24.5491813598998,
-6.72122383683193));
#450148=CARTESIAN_POINT('Ctrl Pts',(-5.52242810385412,24.5253536696684,
-6.74337898734047));
#450149=CARTESIAN_POINT('Ctrl Pts',(-5.21183556708661,24.501525979437,-6.59624120723028));
#450150=CARTESIAN_POINT('Ctrl Pts',(-4.9012430303191,24.4776982892056,-6.44910342712008));
#450151=CARTESIAN_POINT('Ctrl Pts',(-4.670850057927,24.4538705989742,-6.13267271639114));
#450152=CARTESIAN_POINT('Ctrl Pts',(-4.62619808347199,24.4300429087428,
-5.7919038045113));
#450153=CARTESIAN_POINT('Ctrl Pts',(-4.58154610901698,24.4062152185114,
-5.45113489263147));
#450154=CARTESIAN_POINT('Ctrl Pts',(-4.72263513249906,24.38238752828,-5.08602777960075));
#450155=CARTESIAN_POINT('Ctrl Pts',(-4.98483324415836,24.3585598380486,
-4.86383551964991));
#450156=CARTESIAN_POINT('Ctrl Pts',(-5.24703135581765,24.3347321478172,
-4.64164325969907));
#450157=CARTESIAN_POINT('Ctrl Pts',(-5.63033855565415,24.3109044575858,
-4.56236585282811));
#450158=CARTESIAN_POINT('Ctrl Pts',(-5.9591644547709,24.2870767673545,-4.66231973324216));
#450159=CARTESIAN_POINT('Ctrl Pts',(-6.12069642705377,24.275371686312,-4.71142093690032));
#450160=CARTESIAN_POINT('Ctrl Pts',(-6.26908122485669,24.2636666052695,
-4.80377340246064));
#450161=CARTESIAN_POINT('Ctrl Pts',(-6.38942086037359,24.2519615242271,
-4.92421628016771));
#450162=CARTESIAN_POINT('Ctrl Pts',(-6.39128196913613,24.3730384757729,
-4.92377157353715));
#450163=CARTESIAN_POINT('Ctrl Pts',(-6.20403942134221,24.391149798758,-4.7399249826062));
#450164=CARTESIAN_POINT('Ctrl Pts',(-5.94579686164739,24.4092611217431,
-4.62474754709557));
#450165=CARTESIAN_POINT('Ctrl Pts',(-5.68465923264326,24.4273724447281,
-4.61775970678069));
#450166=CARTESIAN_POINT('Ctrl Pts',(-5.34110031445674,24.4512001349595,
-4.60856633672445));
#450167=CARTESIAN_POINT('Ctrl Pts',(-4.99253041816396,24.4750278251909,
-4.78663469857419));
#450168=CARTESIAN_POINT('Ctrl Pts',(-4.79862701145602,24.4988555154223,
-5.07039290068915));
#450169=CARTESIAN_POINT('Ctrl Pts',(-4.60472360474809,24.5226832056536,
-5.35415110280411));
#450170=CARTESIAN_POINT('Ctrl Pts',(-4.565486687625,24.546510895885,-5.7435991451843));
#450171=CARTESIAN_POINT('Ctrl Pts',(-4.69889042440694,24.5703385861164,
-6.06033356407531));
#450172=CARTESIAN_POINT('Ctrl Pts',(-4.83229416118888,24.5941662763478,
-6.37706798296632));
#450173=CARTESIAN_POINT('Ctrl Pts',(-5.13833855187585,24.6179939665792,
-6.62108877836816));
#450174=CARTESIAN_POINT('Ctrl Pts',(-5.47682676316715,24.6418216568106,
-6.68061169925027));
#450175=CARTESIAN_POINT('Ctrl Pts',(-5.81531497445846,24.665649347042,-6.74013462013239));
#450176=CARTESIAN_POINT('Ctrl Pts',(-6.18624700635411,24.6894770372734,
-6.61515966649478));
#450177=CARTESIAN_POINT('Ctrl Pts',(-6.41970146010492,24.7133047275048,
-6.36293701391879));
#450178=CARTESIAN_POINT('Ctrl Pts',(-6.65315591385573,24.7371324177362,
-6.1107143613428));
#450179=CARTESIAN_POINT('Ctrl Pts',(-6.74913278946171,24.7609601079676,
-5.73124400982843));
#450180=CARTESIAN_POINT('Ctrl Pts',(-6.6636657201663,24.784787798199,-5.39835869474429));
#450181=CARTESIAN_POINT('Ctrl Pts',(-6.61793218802978,24.797538024057,-5.22023136007979));
#450182=CARTESIAN_POINT('Ctrl Pts',(-6.5202452116208,24.8102882499149,-5.05544287282308));
#450183=CARTESIAN_POINT('Ctrl Pts',(-6.38933869113556,24.8230384757729,
-4.92408802232565));
#450184=CARTESIAN_POINT('Origin',(-5.65685387860012,26.,-5.65685387860011));
#450185=CARTESIAN_POINT('',(-6.39051881327128,25.2730384757729,-4.92197603118329));
#450186=CARTESIAN_POINT('',(-6.39198798715976,25.1519615242271,-4.92254817630007));
#450187=CARTESIAN_POINT('',(-6.39065394077646,26.,-4.92305381642377));
#450188=CARTESIAN_POINT('Ctrl Pts',(-6.39198798715976,25.1519615242271,
-4.92254817630007));
#450189=CARTESIAN_POINT('Ctrl Pts',(-6.41627314991444,25.1495988880462,
-4.94650751599249));
#450190=CARTESIAN_POINT('Ctrl Pts',(-6.43929566708609,25.1472362518654,
-4.97169983154625));
#450191=CARTESIAN_POINT('Ctrl Pts',(-6.46089355482011,25.1448736156846,
-4.99805942366946));
#450192=CARTESIAN_POINT('Ctrl Pts',(-6.67871286308055,25.1210459254532,
-5.26390153716753));
#450193=CARTESIAN_POINT('Ctrl Pts',(-6.75163093056004,25.0972182352218,
-5.64846913729549));
#450194=CARTESIAN_POINT('Ctrl Pts',(-6.64624470558553,25.0733905449904,
-5.97559449046916));
#450195=CARTESIAN_POINT('Ctrl Pts',(-6.54085848061101,25.049562854759,-6.30271984364283));
#450196=CARTESIAN_POINT('Ctrl Pts',(-6.25716796318249,25.0257351645276,
-6.57240294986222));
#450197=CARTESIAN_POINT('Ctrl Pts',(-5.92512971718013,25.0019074742962,
-6.66110381706144));
#450198=CARTESIAN_POINT('Ctrl Pts',(-5.59309147117778,24.9780797840648,
-6.74980468426065));
#450199=CARTESIAN_POINT('Ctrl Pts',(-5.21270549660159,24.9542520938335,
-6.65752331243968));
#450200=CARTESIAN_POINT('Ctrl Pts',(-4.95822404429259,24.9304244036021,
-6.42653317184816));
#450201=CARTESIAN_POINT('Ctrl Pts',(-4.70374259198359,24.9065967133707,
-6.19554303125664));
#450202=CARTESIAN_POINT('Ctrl Pts',(-4.57516566194178,24.8827690231393,
-5.82584412189456));
#450203=CARTESIAN_POINT('Ctrl Pts',(-4.63139343216518,24.8589413329079,
-5.48679296352304));
#450204=CARTESIAN_POINT('Ctrl Pts',(-4.68762120238858,24.8351136426765,
-5.14774180515151));
#450205=CARTESIAN_POINT('Ctrl Pts',(-4.9286536728772,24.8112859524451,-4.83933839777055));
#450206=CARTESIAN_POINT('Ctrl Pts',(-5.24407554312886,24.7874582622137,
-4.70286022094558));
#450207=CARTESIAN_POINT('Ctrl Pts',(-5.55949741338051,24.7636305719823,
-4.56638204412062));
#450208=CARTESIAN_POINT('Ctrl Pts',(-5.94930868339519,24.7398028817509,
-4.60182909785165));
#450209=CARTESIAN_POINT('Ctrl Pts',(-6.23493948741374,24.7159751915195,
-4.79296332969341));
#450210=CARTESIAN_POINT('Ctrl Pts',(-6.29093505415592,24.7113039690887,
-4.83043362171106));
#450211=CARTESIAN_POINT('Ctrl Pts',(-6.34292671833547,24.7066327466579,
-4.87388734148021));
#450212=CARTESIAN_POINT('Ctrl Pts',(-6.39028821611916,24.7019615242271,
-4.92212745780798));
#450213=CARTESIAN_POINT('Ctrl Pts',(-6.38933869113556,24.8230384757729,
-4.92408802232565));
#450214=CARTESIAN_POINT('Ctrl Pts',(-6.27560640646284,24.8341159401463,
-4.80996622614209));
#450215=CARTESIAN_POINT('Ctrl Pts',(-6.13679925493306,24.8451934045197,
-4.72108089883846));
#450216=CARTESIAN_POINT('Ctrl Pts',(-5.98520281626299,24.8562708688931,
-4.67061008310121));
#450217=CARTESIAN_POINT('Ctrl Pts',(-5.65911799585187,24.8800985591245,
-4.56204706519615));
#450218=CARTESIAN_POINT('Ctrl Pts',(-5.27385936922642,24.9039262493559,
-4.63122130803993));
#450219=CARTESIAN_POINT('Ctrl Pts',(-5.00591117956891,24.9277539395873,
-4.84644449237099));
#450220=CARTESIAN_POINT('Ctrl Pts',(-4.7379629899114,24.9515816298187,-5.06166767670205));
#450221=CARTESIAN_POINT('Ctrl Pts',(-4.58732523722183,24.9754093200501,
-5.42293980252039));
#450222=CARTESIAN_POINT('Ctrl Pts',(-4.62300419682159,24.9992370102815,
-5.76476474386039));
#450223=CARTESIAN_POINT('Ctrl Pts',(-4.65868315642135,25.0230647005129,
-6.10658968520039));
#450224=CARTESIAN_POINT('Ctrl Pts',(-4.88067882831045,25.0468923907443,
-6.42896744206204));
#450225=CARTESIAN_POINT('Ctrl Pts',(-5.18729621377842,25.0707200809757,
-6.58421869570625));
#450226=CARTESIAN_POINT('Ctrl Pts',(-5.4939135992464,25.0945477712071,-6.73946994935045));
#450227=CARTESIAN_POINT('Ctrl Pts',(-5.88515269829325,25.1183754614385,
-6.72759469977719));
#450228=CARTESIAN_POINT('Ctrl Pts',(-6.18179018209155,25.1422031516699,
-6.5540334824637));
#450229=CARTESIAN_POINT('Ctrl Pts',(-6.47842766588984,25.1660308419013,
-6.38047226515022));
#450230=CARTESIAN_POINT('Ctrl Pts',(-6.68046353443956,25.1898585321326,
-6.04522508009649));
#450231=CARTESIAN_POINT('Ctrl Pts',(-6.69534535485933,25.213686222364,-5.70186524531576));
#450232=CARTESIAN_POINT('Ctrl Pts',(-6.70770170116849,25.2334703068337,
-5.41677424787487));
#450233=CARTESIAN_POINT('Ctrl Pts',(-6.59103501365993,25.2532543913033,
-5.12609043162756));
#450234=CARTESIAN_POINT('Ctrl Pts',(-6.39051881327128,25.2730384757729,
-4.92197603118329));
#450235=CARTESIAN_POINT('Origin',(-5.65685387860012,26.,-5.65685387860011));
#450236=CARTESIAN_POINT('',(-6.39190058798136,25.7230384757729,-4.92276701974739));
#450237=CARTESIAN_POINT('',(-6.39006796800885,25.6019615242271,-4.92443355077908));
#450238=CARTESIAN_POINT('',(-6.39065394077646,26.,-4.92305381642377));
#450239=CARTESIAN_POINT('',(-5.59475217632209,26.,-6.69274404704181));
#450240=CARTESIAN_POINT('Ctrl Pts',(-6.39190058798136,25.7230384757729,
-4.92276701974739));
#450241=CARTESIAN_POINT('Ctrl Pts',(-6.17742942344334,25.7438759131544,
-4.71160994855805));
#450242=CARTESIAN_POINT('Ctrl Pts',(-5.86562000134797,25.764713350536,-4.59523934827088));
#450243=CARTESIAN_POINT('Ctrl Pts',(-5.56615422141077,25.7855507879175,
-4.62142687258513));
#450244=CARTESIAN_POINT('Ctrl Pts',(-5.22371394391399,25.8093784781489,
-4.65137240791476));
#450245=CARTESIAN_POINT('Ctrl Pts',(-4.8974142264151,25.8332061683802,-4.86772710302321));
#450246=CARTESIAN_POINT('Ctrl Pts',(-4.7372531902219,25.8570338586116,-5.17187737628347));
#450247=CARTESIAN_POINT('Ctrl Pts',(-4.57709215402869,25.880861548843,-5.47602764954372));
#450248=CARTESIAN_POINT('Ctrl Pts',(-4.58306979914119,25.9046892390744,
-5.86797350095578));
#450249=CARTESIAN_POINT('Ctrl Pts',(-4.75132533448083,25.9285169293058,
-6.16698733288025));
#450250=CARTESIAN_POINT('Ctrl Pts',(-4.91958086982048,25.9523446195372,
-6.46600116480472));
#450251=CARTESIAN_POINT('Ctrl Pts',(-5.25011429538726,25.9761723097686,
-6.67208297724159));
#450252=CARTESIAN_POINT('Ctrl Pts',(-5.59475217632212,26.,-6.69274404704181));
#450253=CARTESIAN_POINT('',(-6.69457727933146,26.,-5.59444809180803));
#450254=CARTESIAN_POINT('Origin',(-5.65685387860012,26.,-5.65685387860011));
#450255=CARTESIAN_POINT('Ctrl Pts',(-6.69458228414866,26.,-5.59444726164187));
#450256=CARTESIAN_POINT('Ctrl Pts',(-6.71351646533255,25.9770624644402,
-5.92484673178863));
#450257=CARTESIAN_POINT('Ctrl Pts',(-6.56158375468957,25.9541249288804,
-6.26627937525033));
#450258=CARTESIAN_POINT('Ctrl Pts',(-6.30214239804398,25.9311873933205,
-6.47167795527827));
#450259=CARTESIAN_POINT('Ctrl Pts',(-6.03263270014108,25.9073597030892,
-6.68504759676004));
#450260=CARTESIAN_POINT('Ctrl Pts',(-5.64710810132191,25.8835320128578,
-6.75161994353754));
#450261=CARTESIAN_POINT('Ctrl Pts',(-5.32182159136528,25.8597043226264,
-6.64083855948586));
#450262=CARTESIAN_POINT('Ctrl Pts',(-4.99653508140864,25.835876632395,-6.53005717543418));
#450263=CARTESIAN_POINT('Ctrl Pts',(-4.73148666031454,25.8120489421636,
-6.24192206055332));
#450264=CARTESIAN_POINT('Ctrl Pts',(-4.64827248224482,25.7882212519322,
-5.90845611919746));
#450265=CARTESIAN_POINT('Ctrl Pts',(-4.56505830417509,25.7643935617008,
-5.5749901778416));
#450266=CARTESIAN_POINT('Ctrl Pts',(-4.66367836912974,25.7405658714694,
-5.19619341001074));
#450267=CARTESIAN_POINT('Ctrl Pts',(-4.89886414913017,25.716738181238,-4.94557465216384));
#450268=CARTESIAN_POINT('Ctrl Pts',(-5.13404992913059,25.6929104910066,
-4.69495589431694));
#450269=CARTESIAN_POINT('Ctrl Pts',(-5.50580142417678,25.6690828007752,
-4.572515146454));
#450270=CARTESIAN_POINT('Ctrl Pts',(-5.84386841174159,25.6452551105439,
-4.63434949773116));
#450271=CARTESIAN_POINT('Ctrl Pts',(-6.04861804217652,25.6308239151049,
-4.67179935541582));
#450272=CARTESIAN_POINT('Ctrl Pts',(-6.24101187097706,25.616392719666,-4.7768430935332));
#450273=CARTESIAN_POINT('Ctrl Pts',(-6.39006796800885,25.6019615242271,
-4.92443355077908));
#450274=CARTESIAN_POINT('Origin',(-5.65685387860012,26.993675081176,-5.65685387860011));
#450275=CARTESIAN_POINT('',(-6.5673434103921,22.756324918824,-4.74524035180399));
#450276=CARTESIAN_POINT('',(-6.57057146528766,22.718675081176,-4.74364038176038));
#450277=CARTESIAN_POINT('',(-6.56902162633079,26.993675081176,-4.74468613086949));
#450278=CARTESIAN_POINT('',(-4.8286920333622,22.5,-6.64591806159944));
#450279=CARTESIAN_POINT('Ctrl Pts',(-6.57057146528766,22.718675081176,-4.74364038176038));
#450280=CARTESIAN_POINT('Ctrl Pts',(-6.58852418981576,22.7172664581449,
-4.76142457130848));
#450281=CARTESIAN_POINT('Ctrl Pts',(-6.9000556810006,22.6920301448823,-5.09000197050781));
#450282=CARTESIAN_POINT('Ctrl Pts',(-7.12689194633153,22.6429661413884,
-6.06611679986992));
#450283=CARTESIAN_POINT('Ctrl Pts',(-6.10694434613243,22.5714830706942,
-7.11331947438321));
#450284=CARTESIAN_POINT('Ctrl Pts',(-5.15775103452081,22.5238276902314,
-6.92144528650133));
#450285=CARTESIAN_POINT('Ctrl Pts',(-4.8286920333622,22.5,-6.64591806159944));
#450286=CARTESIAN_POINT('',(-4.44194770692244,22.5,-6.09734856608926));
#450287=CARTESIAN_POINT('Origin',(-5.65685387860012,22.5,-5.65685387860011));
#450288=CARTESIAN_POINT('Ctrl Pts',(-6.5673434103921,22.756324918824,-4.74524035180399));
#450289=CARTESIAN_POINT('Ctrl Pts',(-6.75594870135602,22.7414761952386,
-4.93595953019022));
#450290=CARTESIAN_POINT('Ctrl Pts',(-7.1012121014615,22.7027997814218,-5.58182921801751));
#450291=CARTESIAN_POINT('Ctrl Pts',(-6.68055232418451,22.6402956773736,
-6.78713386963136));
#450292=CARTESIAN_POINT('Ctrl Pts',(-5.27997950888059,22.5697027613511,
-7.12528591239125));
#450293=CARTESIAN_POINT('Ctrl Pts',(-4.58325719964658,22.5229375355598,
-6.48370144903282));
#450294=CARTESIAN_POINT('Ctrl Pts',(-4.44194158662797,22.5,-6.09735008669021));
#450295=CARTESIAN_POINT('Origin',(-5.65685387860012,26.993675081176,-5.65685387860011));
#450296=CARTESIAN_POINT('',(-6.56983844394705,23.206324918824,-4.74299838399068));
#450297=CARTESIAN_POINT('',(-6.56867439792569,23.168675081176,-4.74631652959707));
#450298=CARTESIAN_POINT('',(-6.56902162633079,26.993675081176,-4.74468613086949));
#450299=CARTESIAN_POINT('Ctrl Pts',(-6.56867439792569,23.168675081176,-4.74631652959707));
#450300=CARTESIAN_POINT('Ctrl Pts',(-6.67716702479821,23.1602325995332,
-4.853408844765));
#450301=CARTESIAN_POINT('Ctrl Pts',(-7.02077633180239,23.127962427659,-5.33214451040114));
#450302=CARTESIAN_POINT('Ctrl Pts',(-6.94377741359719,23.0718645655535,
-6.47507582842176));
#450303=CARTESIAN_POINT('Ctrl Pts',(-5.66653874837813,23.0003814948592,
-7.18181942856023));
#450304=CARTESIAN_POINT('Ctrl Pts',(-4.38054591235379,22.9288984241651,
-6.49141154940691));
#450305=CARTESIAN_POINT('Ctrl Pts',(-4.26365553420012,22.8574153534709,
-5.03639155729104));
#450306=CARTESIAN_POINT('Ctrl Pts',(-5.40079341912851,22.7873409058079,
-4.16730445086878));
#450307=CARTESIAN_POINT('Ctrl Pts',(-6.28484325502835,22.7410941483762,
-4.46059450521194));
#450308=CARTESIAN_POINT('Ctrl Pts',(-6.57057146528766,22.718675081176,-4.74364038176038));
#450309=CARTESIAN_POINT('Ctrl Pts',(-6.56983844394705,23.206324918824,-4.74299838399068));
#450310=CARTESIAN_POINT('Ctrl Pts',(-6.84584090104065,23.184442336627,-5.02227299078827));
#450311=CARTESIAN_POINT('Ctrl Pts',(-7.14533371342118,23.1387320641985,
-5.8884730690954));
#450312=CARTESIAN_POINT('Ctrl Pts',(-6.3084575374563,23.0691941015387,-7.03563221165043));
#450313=CARTESIAN_POINT('Ctrl Pts',(-4.85119529970874,22.9977110308445,
-6.95165327175697));
#450314=CARTESIAN_POINT('Ctrl Pts',(-4.13204038713624,22.9262279601503,
-5.68141376558385));
#450315=CARTESIAN_POINT('Ctrl Pts',(-4.80994952176022,22.8547448894562,
-4.38863987327371));
#450316=CARTESIAN_POINT('Ctrl Pts',(-5.9617065202947,22.7981105423474,-4.28501879514302));
#450317=CARTESIAN_POINT('Ctrl Pts',(-6.45329450867432,22.76530388547,-4.62991319040622));
#450318=CARTESIAN_POINT('Ctrl Pts',(-6.5673434103921,22.756324918824,-4.74524035180399));
#450319=CARTESIAN_POINT('Origin',(-5.65685387860012,26.993675081176,-5.65685387860011));
#450320=CARTESIAN_POINT('',(-6.57003272085371,23.656324918824,-4.74532300381163));
#450321=CARTESIAN_POINT('',(-6.56740434249263,23.618675081176,-4.74499326893249));
#450322=CARTESIAN_POINT('',(-6.56902162633079,26.993675081176,-4.74468613086949));
#450323=CARTESIAN_POINT('Ctrl Pts',(-6.56740434249263,23.618675081176,-4.74499326893249));
#450324=CARTESIAN_POINT('Ctrl Pts',(-6.76368003125862,23.6031987409216,
-4.94389036502613));
#450325=CARTESIAN_POINT('Ctrl Pts',(-7.10715379447205,23.5638947104357,
-5.60787864620878));
#450326=CARTESIAN_POINT('Ctrl Pts',(-6.65070324968042,23.5007629897185,
-6.81352117024561));
#450327=CARTESIAN_POINT('Ctrl Pts',(-5.22331918686542,23.4292799190243,
-7.11892889768229));
#450328=CARTESIAN_POINT('Ctrl Pts',(-4.19313572939823,23.3577968483302,
-6.08480364614364));
#450329=CARTESIAN_POINT('Ctrl Pts',(-4.50398657889369,23.2863137776359,
-4.65859667867589));
#450330=CARTESIAN_POINT('Ctrl Pts',(-5.70962577012502,23.2232731885846,
-4.20740365817457));
#450331=CARTESIAN_POINT('Ctrl Pts',(-6.37096218895919,23.1840602897646,
-4.55115618731808));
#450332=CARTESIAN_POINT('Ctrl Pts',(-6.56867439792569,23.168675081176,-4.74631652959707));
#450333=CARTESIAN_POINT('Ctrl Pts',(-6.57003272085371,23.656324918824,-4.74532300381163));
#450334=CARTESIAN_POINT('Ctrl Pts',(-6.63539236159828,23.6512361682467,
-4.80948437015677));
#450335=CARTESIAN_POINT('Ctrl Pts',(-6.9668858368575,23.622319727438,-5.21266771861286));
#450336=CARTESIAN_POINT('Ctrl Pts',(-7.04564953674368,23.569575596398,-6.28682364983267));
#450337=CARTESIAN_POINT('Ctrl Pts',(-5.88000083782647,23.4980925257038,
-7.16543624640093));
#450338=CARTESIAN_POINT('Ctrl Pts',(-4.50990820099157,23.4266094550096,
-6.66190630419616));
#450339=CARTESIAN_POINT('Ctrl Pts',(-4.19063094092434,23.3551263843154,
-5.23756146736659));
#450340=CARTESIAN_POINT('Ctrl Pts',(-5.21468783779197,23.2836433136212,
-4.19736598356861));
#450341=CARTESIAN_POINT('Ctrl Pts',(-6.20635078283889,23.2340428251241,
-4.40342562281452));
#450342=CARTESIAN_POINT('Ctrl Pts',(-6.54530502316694,23.2082700268584,
-4.71817410701172));
#450343=CARTESIAN_POINT('Ctrl Pts',(-6.56983844394705,23.206324918824,-4.74299838399068));
#450344=CARTESIAN_POINT('Origin',(-5.65685387860012,26.993675081176,-5.65685387860011));
#450345=CARTESIAN_POINT('',(-6.56748881619374,24.106324918824,-4.74613115927677));
#450346=CARTESIAN_POINT('',(-6.57010232725217,24.068675081176,-4.74299681637215));
#450347=CARTESIAN_POINT('',(-6.56902162633079,26.993675081176,-4.74468613086949));
#450348=CARTESIAN_POINT('Ctrl Pts',(-6.57010232725218,24.068675081176,-4.74299681637215));
#450349=CARTESIAN_POINT('Ctrl Pts',(-6.85435514987614,24.0461648823099,
-5.02972694085412));
#450350=CARTESIAN_POINT('Ctrl Pts',(-7.14655186859909,23.9998269932124,
-5.91736950865738));
#450351=CARTESIAN_POINT('Ctrl Pts',(-6.27199288310558,23.9296614138836,
-7.0522818436793));
#450352=CARTESIAN_POINT('Ctrl Pts',(-4.81743049717126,23.8581783431894,
-6.93003241982605));
#450353=CARTESIAN_POINT('Ctrl Pts',(-4.13193628895796,23.7866952724952,
-5.64131435190337));
#450354=CARTESIAN_POINT('Ctrl Pts',(-4.84355050202496,23.715212201801,-4.3668333837381));
#450355=CARTESIAN_POINT('Ctrl Pts',(-5.98491025846012,23.6592054713613,
-4.29429575151248));
#450356=CARTESIAN_POINT('Ctrl Pts',(-6.4614899633887,23.627026431153,-4.63766432477859));
#450357=CARTESIAN_POINT('Ctrl Pts',(-6.56740434249263,23.618675081176,-4.74499326893249));
#450358=CARTESIAN_POINT('Ctrl Pts',(-6.56748881619374,24.106324918824,-4.74613115927677));
#450359=CARTESIAN_POINT('Ctrl Pts',(-6.72241589762581,24.0942023096351,
-4.90119115627847));
#450360=CARTESIAN_POINT('Ctrl Pts',(-7.07096798466868,24.0582520102147,
-5.47210261995127));
#450361=CARTESIAN_POINT('Ctrl Pts',(-6.80286792203874,23.998474020563,-6.662968703113));
#450362=CARTESIAN_POINT('Ctrl Pts',(-5.43230911237055,23.9269909498688,
-7.16522879152533));
#450363=CARTESIAN_POINT('Ctrl Pts',(-4.26747512907024,23.8555078791747,
-6.2855365564656));
#450364=CARTESIAN_POINT('Ctrl Pts',(-4.37557081254884,23.7840248084805,
-4.82985391579145));
#450365=CARTESIAN_POINT('Ctrl Pts',(-5.56629788826614,23.7176304883636,
-4.18154636230721));
#450366=CARTESIAN_POINT('Ctrl Pts',(-6.32935078034096,23.6750638584781,
-4.50905361827065));
#450367=CARTESIAN_POINT('Ctrl Pts',(-6.57003272085371,23.656324918824,-4.74532300381163));
#450368=CARTESIAN_POINT('Origin',(-5.65685387860012,26.993675081176,-5.65685387860011));
#450369=CARTESIAN_POINT('',(-6.56856700353347,24.556324918824,-4.74353459859835));
#450370=CARTESIAN_POINT('',(-6.56980231202958,24.518675081176,-4.74557835604531));
#450371=CARTESIAN_POINT('',(-6.56902162633079,26.993675081176,-4.74468613086949));
#450372=CARTESIAN_POINT('Ctrl Pts',(-6.56980231202958,24.518675081176,-4.74557835604531));
#450373=CARTESIAN_POINT('Ctrl Pts',(-6.64326578517921,24.5129587139297,
-4.81770944620421));
#450374=CARTESIAN_POINT('Ctrl Pts',(-6.97750833641272,24.4834146564519,
-5.23445549419879));
#450375=CARTESIAN_POINT('Ctrl Pts',(-7.02860988272989,24.4300429087428,
-6.32311258055821));
#450376=CARTESIAN_POINT('Ctrl Pts',(-5.84026841822957,24.3585598380486,
-7.17078066054311));
#450377=CARTESIAN_POINT('Ctrl Pts',(-4.4838850778304,24.2870767673545,-6.63140987332417));
#450378=CARTESIAN_POINT('Ctrl Pts',(-4.2021595986403,24.2155936966603,-5.19916430623342));
#450379=CARTESIAN_POINT('Ctrl Pts',(-5.25320498229437,24.1441106259661,
-4.18624762160045));
#450380=CARTESIAN_POINT('Ctrl Pts',(-6.22663461042285,24.095137754138,-4.41536649518845));
#450381=CARTESIAN_POINT('Ctrl Pts',(-6.55346539562853,24.0699925725413,
-4.72621489163553));
#450382=CARTESIAN_POINT('Ctrl Pts',(-6.57010232725218,24.068675081176,-4.74299681637215));
#450383=CARTESIAN_POINT('Ctrl Pts',(-6.56856700353346,24.556324918824,-4.74353459859835));
#450384=CARTESIAN_POINT('Ctrl Pts',(-6.81000592522228,24.5371684510234,
-4.98945253222269));
#450385=CARTESIAN_POINT('Ctrl Pts',(-7.13455935910424,24.4941842929915,
-5.76578134653658));
#450386=CARTESIAN_POINT('Ctrl Pts',(-6.46131966662841,24.4273724447281,
-6.95240396480877));
#450387=CARTESIAN_POINT('Ctrl Pts',(-5.00396921476326,24.3558893740339,
-7.03502543671246));
#450388=CARTESIAN_POINT('Ctrl Pts',(-4.14478270244581,24.2844063033397,
-5.85498510857852));
#450389=CARTESIAN_POINT('Ctrl Pts',(-4.67093497503137,24.2129232326456,
-4.49341967622111));
#450390=CARTESIAN_POINT('Ctrl Pts',(-5.85795834238072,24.1535627711403,
-4.24791389261248));
#450391=CARTESIAN_POINT('Ctrl Pts',(-6.41789774915756,24.1180299998665,
-4.5964117545626));
#450392=CARTESIAN_POINT('Ctrl Pts',(-6.56748881619374,24.106324918824,-4.74613115927677));
#450393=CARTESIAN_POINT('Origin',(-5.65685387860012,26.993675081176,-5.65685387860011));
#450394=CARTESIAN_POINT('',(-6.57067994464874,25.006324918824,-4.74405758279953));
#450395=CARTESIAN_POINT('',(-6.56738667375376,24.968675081176,-4.74597172529335));
#450396=CARTESIAN_POINT('',(-6.56902162633079,26.993675081176,-4.74468613086949));
#450397=CARTESIAN_POINT('Ctrl Pts',(-6.56738667375376,24.968675081176,-4.74597172529335));
#450398=CARTESIAN_POINT('Ctrl Pts',(-6.73011316031215,24.955924855318,-4.90925551921452));
#450399=CARTESIAN_POINT('Ctrl Pts',(-7.0784783223036,24.9193469392286,-5.49691387622178));
#450400=CARTESIAN_POINT('Ctrl Pts',(-6.77602463836695,24.8589413329079,
-6.69274573713214));
#450401=CARTESIAN_POINT('Ctrl Pts',(-5.39273679116276,24.7874582622137,
-7.15880506797054));
#450402=CARTESIAN_POINT('Ctrl Pts',(-4.25142935492228,24.7159751915195,
-6.24879737998679));
#450403=CARTESIAN_POINT('Ctrl Pts',(-4.39775252453572,24.6444921208253,
-4.79645922145989));
#450404=CARTESIAN_POINT('Ctrl Pts',(-5.59369688000734,24.5787254173775,
-4.18550614000559));
#450405=CARTESIAN_POINT('Ctrl Pts',(-6.33704597702196,24.5367864041611,
-4.51704344657683));
#450406=CARTESIAN_POINT('Ctrl Pts',(-6.56980231202958,24.518675081176,-4.74557835604531));
#450407=CARTESIAN_POINT('Ctrl Pts',(-6.57067994464874,25.006324918824,-4.74405758279953));
#450408=CARTESIAN_POINT('Ctrl Pts',(-6.60086819803687,25.0039622826432,
-4.77384081402403));
#450409=CARTESIAN_POINT('Ctrl Pts',(-6.91811250300101,24.9777719562309,
-5.12098437694123));
#450410=CARTESIAN_POINT('Ctrl Pts',(-7.10838527255516,24.9277539395874,
-6.12447699388038));
#450411=CARTESIAN_POINT('Ctrl Pts',(-6.05044038944422,24.8562708688931,
-7.13018513270865));
#450412=CARTESIAN_POINT('Ctrl Pts',(-4.63189669239788,24.784787798199,-6.78604742232836));
#450413=CARTESIAN_POINT('Ctrl Pts',(-4.15240479236239,24.7133047275048,
-5.40735816264999));
#450414=CARTESIAN_POINT('Ctrl Pts',(-5.0512683537124,24.6418216568106,-4.25725342975252));
#450415=CARTESIAN_POINT('Ctrl Pts',(-6.11539165852711,24.589495053917,-4.35401829743014));
#450416=CARTESIAN_POINT('Ctrl Pts',(-6.50969315902277,24.5609961412548,
-4.68356856625642));
#450417=CARTESIAN_POINT('Ctrl Pts',(-6.56856700353346,24.556324918824,-4.74353459859835));
#450418=CARTESIAN_POINT('Origin',(-5.65685387860012,26.993675081176,-5.65685387860011));
#450419=CARTESIAN_POINT('',(-6.56829321884323,25.456324918824,-4.74640124271564));
#450420=CARTESIAN_POINT('',(-6.56885365284802,25.418675081176,-4.74334636410459));
#450421=CARTESIAN_POINT('',(-6.56902162633079,26.993675081176,-4.74468613086949));
#450422=CARTESIAN_POINT('Ctrl Pts',(-6.56885365284802,25.418675081176,-4.74334636410459));
#450423=CARTESIAN_POINT('Ctrl Pts',(-6.81811011972481,25.3988909967064,
-4.99707565976646));
#450424=CARTESIAN_POINT('Ctrl Pts',(-7.13780202337966,25.3552792220053,
-5.79361205385018));
#450425=CARTESIAN_POINT('Ctrl Pts',(-6.42698533143036,25.287839757073,-6.97310209577086));
#450426=CARTESIAN_POINT('Ctrl Pts',(-4.96796792520408,25.2163566863788,
-7.01738753624157));
#450427=CARTESIAN_POINT('Ctrl Pts',(-4.14009680960707,25.1448736156846,
-5.81516935358236));
#450428=CARTESIAN_POINT('Ctrl Pts',(-4.70185841202445,25.0733905449904,
-4.46790543942481));
#450429=CARTESIAN_POINT('Ctrl Pts',(-5.88231068328694,25.0146577001542,
-4.25595199715398));
#450430=CARTESIAN_POINT('Ctrl Pts',(-6.4260090324839,24.9797525455494,-4.604109892408));
#450431=CARTESIAN_POINT('Ctrl Pts',(-6.56738667375376,24.968675081176,-4.74597172529335));
#450432=CARTESIAN_POINT('Ctrl Pts',(-6.56829321884323,25.456324918824,-4.74640124271564));
#450433=CARTESIAN_POINT('Ctrl Pts',(-6.68893848409318,25.4469284240315,
-4.86586022639608));
#450434=CARTESIAN_POINT('Ctrl Pts',(-7.03476003379299,25.4137042390077,
-5.36752678600608));
#450435=CARTESIAN_POINT('Ctrl Pts',(-6.9100356033464,25.3566523637524,-6.5258341885166));
#450436=CARTESIAN_POINT('Ctrl Pts',(-5.60564496305001,25.2851692930582,
-7.18099123031483));
#450437=CARTESIAN_POINT('Ctrl Pts',(-4.34815567114858,25.213686222364,-6.43975200870338));
#450438=CARTESIAN_POINT('Ctrl Pts',(-4.2896855842815,25.1422031516699,-4.98123363545819));
#450439=CARTESIAN_POINT('Ctrl Pts',(-5.44432497425889,25.0730827171565,
-4.16945626611646));
#450440=CARTESIAN_POINT('Ctrl Pts',(-6.29641321838457,25.0277899728745,
-4.47347056935133));
#450441=CARTESIAN_POINT('Ctrl Pts',(-6.57067994464874,25.006324918824,-4.74405758279953));
#450442=CARTESIAN_POINT('Origin',(-5.65685387860012,26.993675081176,-5.65685387860011));
#450443=CARTESIAN_POINT('',(-6.56704169373441,25.906324918824,-4.74450601134849));
#450444=CARTESIAN_POINT('',(-6.57057130100612,25.868675081176,-4.74432962138981));
#450445=CARTESIAN_POINT('',(-6.56902162633079,26.993675081176,-4.74468613086949));
#450446=CARTESIAN_POINT('',(-5.01302286563433,26.,-4.53900700771688));
#450447=CARTESIAN_POINT('Ctrl Pts',(-5.01302286563431,26.,-4.53900700771688));
#450448=CARTESIAN_POINT('Ctrl Pts',(-5.38492752167559,25.9761723097686,
-4.32480615636363));
#450449=CARTESIAN_POINT('Ctrl Pts',(-6.01924597306242,25.9449472827099,
-4.30899334914827));
#450450=CARTESIAN_POINT('Ctrl Pts',(-6.47338425157137,25.9137222556513,
-4.64940368207851));
#450451=CARTESIAN_POINT('Ctrl Pts',(-6.56704169373441,25.906324918824,-4.74450601134849));
#450452=CARTESIAN_POINT('',(-4.53689596693371,26.,-5.01208503488091));
#450453=CARTESIAN_POINT('Origin',(-5.65685387860012,26.,-5.65685387860011));
#450454=CARTESIAN_POINT('Ctrl Pts',(-4.5368902045627,26.,-5.01208247494518));
#450455=CARTESIAN_POINT('Ctrl Pts',(-4.74314812622022,25.9770624644402,
-4.65613984562121));
#450456=CARTESIAN_POINT('Ctrl Pts',(-5.48969900651177,25.9332874914989,
-4.17795197796789));
#450457=CARTESIAN_POINT('Ctrl Pts',(-6.3039677816093,25.8895125185575,-4.48184576512937));
#450458=CARTESIAN_POINT('Ctrl Pts',(-6.57057130100612,25.868675081176,-4.74432962138981));
#450459=CARTESIAN_POINT('Origin',(-5.65685387860011,26.,5.65685387860011));
#450460=CARTESIAN_POINT('',(-4.9222125558517,22.573038475773,6.39190072013885));
#450461=CARTESIAN_POINT('',(-4.92305381642377,22.5,6.39065394077645));
#450462=CARTESIAN_POINT('',(-4.92305381642377,26.,6.39065394077645));
#450463=CARTESIAN_POINT('',(-5.8978925564917,22.5,6.66622270032004));
#450464=CARTESIAN_POINT('Origin',(-5.65685387860011,22.5,5.65685387860011));
#450465=CARTESIAN_POINT('Ctrl Pts',(-5.89851203167784,22.5,6.66798006829997));
#450466=CARTESIAN_POINT('Ctrl Pts',(-5.57641995134461,22.5229375355598,
6.7439998684947));
#450467=CARTESIAN_POINT('Ctrl Pts',(-5.21379162224851,22.5458750711197,
6.65366449057419));
#450468=CARTESIAN_POINT('Ctrl Pts',(-4.96646199655034,22.5688126066795,
6.43383171727969));
#450469=CARTESIAN_POINT('Ctrl Pts',(-4.95127317183385,22.5702212297106,
6.42033150900062));
#450470=CARTESIAN_POINT('Ctrl Pts',(-4.93651917810251,22.5716298527418,
6.40634292159547));
#450471=CARTESIAN_POINT('Ctrl Pts',(-4.9222125558517,22.573038475773,6.39190072013885));
#450472=CARTESIAN_POINT('Origin',(-5.65685387860011,26.,5.65685387860011));
#450473=CARTESIAN_POINT('',(-4.92436540268704,23.0230384757729,6.39037461032892));
#450474=CARTESIAN_POINT('',(-4.92349966353597,22.9019615242271,6.38930388760559));
#450475=CARTESIAN_POINT('',(-4.92305381642377,26.,6.39065394077645));
#450476=CARTESIAN_POINT('',(-4.62591736201901,22.5,5.77557608073439));
#450477=CARTESIAN_POINT('Ctrl Pts',(-4.92349966353597,22.9019615242271,
6.38930388760559));
#450478=CARTESIAN_POINT('Ctrl Pts',(-5.07692511110986,22.8871128006417,
6.54102880287524));
#450479=CARTESIAN_POINT('Ctrl Pts',(-5.27640120658105,22.8722640770563,
6.64766299899898));
#450480=CARTESIAN_POINT('Ctrl Pts',(-5.48772889025785,22.8574153534709,
6.68249361011691));
#450481=CARTESIAN_POINT('Ctrl Pts',(-5.82684562005692,22.8335876632395,
6.73838615923167));
#450482=CARTESIAN_POINT('Ctrl Pts',(-6.19648078060475,22.8097599730081,
6.60938089562333));
#450483=CARTESIAN_POINT('Ctrl Pts',(-6.42720821100082,22.7859322827767,
6.35472685290066));
#450484=CARTESIAN_POINT('Ctrl Pts',(-6.65793564139689,22.7621045925453,
6.10007281017799));
#450485=CARTESIAN_POINT('Ctrl Pts',(-6.74975534164119,22.7382769023139,
5.71976998834099));
#450486=CARTESIAN_POINT('Ctrl Pts',(-6.66080060824128,22.7144492120825,
5.38773213421059));
#450487=CARTESIAN_POINT('Ctrl Pts',(-6.57184587484137,22.6906215218511,
5.05569428008018));
#450488=CARTESIAN_POINT('Ctrl Pts',(-6.30211670779724,22.6667938316197,
4.77192139365638));
#450489=CARTESIAN_POINT('Ctrl Pts',(-5.97477550103877,22.6429661413884,
4.66700870222797));
#450490=CARTESIAN_POINT('Ctrl Pts',(-5.6474342942803,22.619138451157,4.56209601079956));
#450491=CARTESIAN_POINT('Ctrl Pts',(-5.26248104780748,22.5953107609256,
4.63604351436656));
#450492=CARTESIAN_POINT('Ctrl Pts',(-4.99722717517853,22.5714830706942,
4.85366607828882));
#450493=CARTESIAN_POINT('Ctrl Pts',(-4.73197330254959,22.5476553804628,
5.07128864221107));
#450494=CARTESIAN_POINT('Ctrl Pts',(-4.58641880376449,22.5238276902314,
5.43258626648858));
#450495=CARTESIAN_POINT('Ctrl Pts',(-4.625917362019,22.5,5.77557608073438));
#450496=CARTESIAN_POINT('Origin',(-5.65685387860011,22.5,5.65685387860011));
#450497=CARTESIAN_POINT('Ctrl Pts',(-4.9222125558517,22.573038475773,6.39190072013885));
#450498=CARTESIAN_POINT('Ctrl Pts',(-4.69451421601594,22.5954575429732,
6.16204455719575));
#450499=CARTESIAN_POINT('Ctrl Pts',(-4.58013776446743,22.6178766101734,
5.81728522517979));
#450500=CARTESIAN_POINT('Ctrl Pts',(-4.62964039434809,22.6402956773736,
5.49777863793003));
#450501=CARTESIAN_POINT('Ctrl Pts',(-4.68225334741615,22.664123367605,5.15819698094666));
#450502=CARTESIAN_POINT('Ctrl Pts',(-4.91998587117151,22.6879510578364,
4.84714109570319));
#450503=CARTESIAN_POINT('Ctrl Pts',(-5.23393572436938,22.7117787480678,
4.70728537400252));
#450504=CARTESIAN_POINT('Ctrl Pts',(-5.54788557756724,22.7356064382992,
4.56742965230184));
#450505=CARTESIAN_POINT('Ctrl Pts',(-5.93805276020761,22.7594341285306,
4.59877409414395));
#450506=CARTESIAN_POINT('Ctrl Pts',(-6.22570363532513,22.783261818762,4.78686738296995));
#450507=CARTESIAN_POINT('Ctrl Pts',(-6.51335451044265,22.8070895089934,
4.97496067179595));
#450508=CARTESIAN_POINT('Ctrl Pts',(-6.69848907803731,22.8309171992248,
5.31980280760584));
#450509=CARTESIAN_POINT('Ctrl Pts',(-6.69629884619592,22.8547448894562,
5.66347121722023));
#450510=CARTESIAN_POINT('Ctrl Pts',(-6.69410861435454,22.8785725796876,
6.00713962683461));
#450511=CARTESIAN_POINT('Ctrl Pts',(-6.5045935830771,22.902400269919,6.34963431025349));
#450512=CARTESIAN_POINT('Ctrl Pts',(-6.21456908983246,22.9262279601503,
6.53403672593788));
#450513=CARTESIAN_POINT('Ctrl Pts',(-5.92454459658782,22.9500556503817,
6.71843914162228));
#450514=CARTESIAN_POINT('Ctrl Pts',(-5.53401064137597,22.9738833406131,
6.7447492895722));
#450515=CARTESIAN_POINT('Ctrl Pts',(-5.22186823831327,22.9977110308445,
6.60092695407667));
#450516=CARTESIAN_POINT('Ctrl Pts',(-5.11127184889382,23.0061535124873,
6.54996870275417));
#450517=CARTESIAN_POINT('Ctrl Pts',(-5.01051660428821,23.0145959941301,
6.47765230299322));
#450518=CARTESIAN_POINT('Ctrl Pts',(-4.92436540268704,23.0230384757729,
6.39037461032892));
#450519=CARTESIAN_POINT('Origin',(-5.65685387860011,26.,5.65685387860011));
#450520=CARTESIAN_POINT('',(-4.92330089590042,23.4730384757729,6.38935290488262));
#450521=CARTESIAN_POINT('',(-4.92169609601798,23.3519615242271,6.39131103572319));
#450522=CARTESIAN_POINT('',(-4.92305381642377,26.,6.39065394077645));
#450523=CARTESIAN_POINT('Ctrl Pts',(-4.92169609601798,23.3519615242271,
6.39131103572319));
#450524=CARTESIAN_POINT('Ctrl Pts',(-5.14636061012976,23.33007894203,6.61334324490838));
#450525=CARTESIAN_POINT('Ctrl Pts',(-5.47994522249351,23.308196359833,6.72868171719176));
#450526=CARTESIAN_POINT('Ctrl Pts',(-5.79285848911254,23.286313777636,6.68738448495221));
#450527=CARTESIAN_POINT('Ctrl Pts',(-6.13358611984441,23.2624860874046,
6.64241640721998));
#450528=CARTESIAN_POINT('Ctrl Pts',(-6.44980419113038,23.2386583971732,
6.41172882390928));
#450529=CARTESIAN_POINT('Ctrl Pts',(-6.59665364733223,23.2148307069418,
6.10100080909856));
#450530=CARTESIAN_POINT('Ctrl Pts',(-6.74350310353408,23.1910030167104,
5.79027279428784));
#450531=CARTESIAN_POINT('Ctrl Pts',(-6.7209839446518,23.167175326479,5.39950434797711));
#450532=CARTESIAN_POINT('Ctrl Pts',(-6.539415444341,23.1433476362476,5.1076985472349));
#450533=CARTESIAN_POINT('Ctrl Pts',(-6.3578469440302,23.1195199460162,4.8158927464927));
#450534=CARTESIAN_POINT('Ctrl Pts',(-6.01722910229088,23.0956922557848,
4.62304959131903));
#450535=CARTESIAN_POINT('Ctrl Pts',(-5.67358993507176,23.0718645655534,
4.61751951301592));
#450536=CARTESIAN_POINT('Ctrl Pts',(-5.32995076785264,23.048036875322,4.61198943471281));
#450537=CARTESIAN_POINT('Ctrl Pts',(-4.98329027515371,23.0242091850907,
4.79377243328025));
#450538=CARTESIAN_POINT('Ctrl Pts',(-4.7924243254548,23.0003814948593,5.07957475014376));
#450539=CARTESIAN_POINT('Ctrl Pts',(-4.60155837575589,22.9765538046279,
5.36537706700727));
#450540=CARTESIAN_POINT('Ctrl Pts',(-4.566486969057,22.9527261143965,5.75519870216683));
#450541=CARTESIAN_POINT('Ctrl Pts',(-4.70325041523272,22.9288984241651,
6.07050470066555));
#450542=CARTESIAN_POINT('Ctrl Pts',(-4.75478685916324,22.9199194575191,
6.18932117076025));
#450543=CARTESIAN_POINT('Ctrl Pts',(-4.83072387924101,22.9109404908731,
6.29755640872372));
#450544=CARTESIAN_POINT('Ctrl Pts',(-4.92349966353597,22.9019615242271,
6.38930388760559));
#450545=CARTESIAN_POINT('Ctrl Pts',(-4.92436540268704,23.0230384757729,
6.39037461032892));
#450546=CARTESIAN_POINT('Ctrl Pts',(-4.76736722811336,23.0384236843615,
6.23132356780567));
#450547=CARTESIAN_POINT('Ctrl Pts',(-4.65886881811934,23.0538088929501,
6.02258634020352));
#450548=CARTESIAN_POINT('Ctrl Pts',(-4.62769529041208,23.0691941015387,
5.80287677492702));
#450549=CARTESIAN_POINT('Ctrl Pts',(-4.57941559648715,23.0930217917701,
5.46260375021388));
#450550=CARTESIAN_POINT('Ctrl Pts',(-4.71660705955086,23.1168494820015,
5.09601251972856));
#450551=CARTESIAN_POINT('Ctrl Pts',(-4.97642324075838,23.1406771722329,
4.87103919530453));
#450552=CARTESIAN_POINT('Ctrl Pts',(-5.2362394219659,23.1645048624643,4.64606587088049));
#450553=CARTESIAN_POINT('Ctrl Pts',(-5.61868032131723,23.1883325526957,
4.56271045251773));
#450554=CARTESIAN_POINT('Ctrl Pts',(-5.94855238336812,23.2121602429271,
4.65915585483332));
#450555=CARTESIAN_POINT('Ctrl Pts',(-6.278424445419,23.2359879331585,4.75560125714891));
#450556=CARTESIAN_POINT('Ctrl Pts',(-6.55572767016945,23.2598156233899,
5.03184748014285));
#450557=CARTESIAN_POINT('Ctrl Pts',(-6.65343136663416,23.2836433136212,
5.36134886181892));
#450558=CARTESIAN_POINT('Ctrl Pts',(-6.75113506309886,23.3074710038526,
5.690850243495));
#450559=CARTESIAN_POINT('Ctrl Pts',(-6.66923923127783,23.331298694084,6.07360678385322));
#450560=CARTESIAN_POINT('Ctrl Pts',(-6.44525978436571,23.3551263843154,
6.33427992409048));
#450561=CARTESIAN_POINT('Ctrl Pts',(-6.22128033745359,23.3789540745468,
6.59495306432775));
#450562=CARTESIAN_POINT('Ctrl Pts',(-5.85521727545038,23.4027817647782,
6.73354280444407));
#450563=CARTESIAN_POINT('Ctrl Pts',(-5.51476156795534,23.4266094550096,
6.6865623548039));
#450564=CARTESIAN_POINT('Ctrl Pts',(-5.29363193601897,23.442085795264,6.65604804910002));
#450565=CARTESIAN_POINT('Ctrl Pts',(-5.08330512959901,23.4575621355185,
6.54724832815155));
#450566=CARTESIAN_POINT('Ctrl Pts',(-4.92330089590042,23.4730384757729,
6.38935290488262));
#450567=CARTESIAN_POINT('Origin',(-5.65685387860011,26.,5.65685387860011));
#450568=CARTESIAN_POINT('',(-4.92169483493571,23.9230384757729,6.39152331859132));
#450569=CARTESIAN_POINT('',(-4.92356615355223,23.8019615242271,6.39146732321148));
#450570=CARTESIAN_POINT('',(-4.92305381642377,26.,6.39065394077645));
#450571=CARTESIAN_POINT('Ctrl Pts',(-4.92356615355223,23.8019615242271,
6.39146732321148));
#450572=CARTESIAN_POINT('Ctrl Pts',(-4.97518123721477,23.7968727736498,
6.44404636753914));
#450573=CARTESIAN_POINT('Ctrl Pts',(-5.03225965778749,23.7917840230725,
6.49097569651667));
#450574=CARTESIAN_POINT('Ctrl Pts',(-5.09396482100832,23.7866952724952,
6.53072214720976));
#450575=CARTESIAN_POINT('Ctrl Pts',(-5.38289458727869,23.7628675822638,
6.71683190058211));
#450576=CARTESIAN_POINT('Ctrl Pts',(-5.77326614382955,23.7390398920324,
6.74545633697037));
#450577=CARTESIAN_POINT('Ctrl Pts',(-6.08625298439034,23.715212201801,6.60348277515141));
#450578=CARTESIAN_POINT('Ctrl Pts',(-6.39923982495114,23.6913845115696,
6.46150921333244));
#450579=CARTESIAN_POINT('Ctrl Pts',(-6.63484194952187,23.6675568213382,
6.14893765330626));
#450580=CARTESIAN_POINT('Ctrl Pts',(-6.68513161677842,23.6437291311068,
5.80895502137128));
#450581=CARTESIAN_POINT('Ctrl Pts',(-6.73542128403497,23.6199014408755,
5.4689723894363));
#450582=CARTESIAN_POINT('Ctrl Pts',(-6.60039849397735,23.5960737506441,
5.10157868559252));
#450583=CARTESIAN_POINT('Ctrl Pts',(-6.34191631672375,23.5722460604127,
4.87507434314934));
#450584=CARTESIAN_POINT('Ctrl Pts',(-6.08343413947014,23.5484183701813,
4.64857000070617));
#450585=CARTESIAN_POINT('Ctrl Pts',(-5.70149257502055,23.5245906799499,
4.56295501966359));
#450586=CARTESIAN_POINT('Ctrl Pts',(-5.37105630657982,23.5007629897185,
4.65744921450721));
#450587=CARTESIAN_POINT('Ctrl Pts',(-5.04062003813909,23.4769352994871,
4.75194340935083));
#450588=CARTESIAN_POINT('Ctrl Pts',(-4.76168906570723,23.4531076092557,
5.02654678008064));
#450589=CARTESIAN_POINT('Ctrl Pts',(-4.66203997694959,23.4292799190243,
5.35546505814245));
#450590=CARTESIAN_POINT('Ctrl Pts',(-4.56239088819196,23.4054522287929,
5.68438333620426));
#450591=CARTESIAN_POINT('Ctrl Pts',(-4.64202368310855,23.3816245385615,
6.06761652159808));
#450592=CARTESIAN_POINT('Ctrl Pts',(-4.86445867565572,23.3577968483301,
6.32960882821811));
#450593=CARTESIAN_POINT('Ctrl Pts',(-4.88261654521522,23.3558517402958,
6.350995850443));
#450594=CARTESIAN_POINT('Ctrl Pts',(-4.90172602358781,23.3539066322614,
6.37157494470415));
#450595=CARTESIAN_POINT('Ctrl Pts',(-4.92169609601798,23.3519615242271,
6.39131103572319));
#450596=CARTESIAN_POINT('Ctrl Pts',(-4.92330089590042,23.4730384757729,
6.38935290488262));
#450597=CARTESIAN_POINT('Ctrl Pts',(-4.83695933636888,23.4813898257499,
6.30414930262285));
#450598=CARTESIAN_POINT('Ctrl Pts',(-4.76527121936352,23.4897411757268,
6.20464951053553));
#450599=CARTESIAN_POINT('Ctrl Pts',(-4.71444637045848,23.4980925257038,
6.09544017298549));
#450600=CARTESIAN_POINT('Ctrl Pts',(-4.56943523344352,23.5219202159352,
5.78384908020389));
#450601=CARTESIAN_POINT('Ctrl Pts',(-4.59426131240048,23.5457479061666,
5.39321753403733));
#450602=CARTESIAN_POINT('Ctrl Pts',(-4.77755195197114,23.569575596398,5.10249121190879));
#450603=CARTESIAN_POINT('Ctrl Pts',(-4.9608425915418,23.5934032866293,4.81176488978025));
#450604=CARTESIAN_POINT('Ctrl Pts',(-5.30259779172617,23.6172309768607,
4.62094379168974));
#450605=CARTESIAN_POINT('Ctrl Pts',(-5.64626184853499,23.6410586670921,
4.61744171997954));
#450606=CARTESIAN_POINT('Ctrl Pts',(-5.98992590534381,23.6648863573235,
4.61393964826934));
#450607=CARTESIAN_POINT('Ctrl Pts',(-6.33549881877709,23.6887140475549,
4.79775660293946));
#450608=CARTESIAN_POINT('Ctrl Pts',(-6.52467601704459,23.7125417377863,
5.08468731748426));
#450609=CARTESIAN_POINT('Ctrl Pts',(-6.71385321531209,23.7363694280177,
5.37161803202905));
#450610=CARTESIAN_POINT('Ctrl Pts',(-6.74663469841383,23.7601971182491,
5.76166250644851));
#450611=CARTESIAN_POINT('Ctrl Pts',(-6.60800349462427,23.7840248084805,
6.07614404554655));
#450612=CARTESIAN_POINT('Ctrl Pts',(-6.46937229083472,23.8078524987119,
6.39062558464459));
#450613=CARTESIAN_POINT('Ctrl Pts',(-6.15932840015388,23.8316801889433,
6.6295441884212));
#450614=CARTESIAN_POINT('Ctrl Pts',(-5.81990079386588,23.8555078791747,
6.6834528935629));
#450615=CARTESIAN_POINT('Ctrl Pts',(-5.49924097144978,23.8780180780408,
6.73438085433327));
#450616=CARTESIAN_POINT('Ctrl Pts',(-5.15235699515366,23.9005282769068,
6.62019259508592));
#450617=CARTESIAN_POINT('Ctrl Pts',(-4.92169483493571,23.9230384757729,
6.39152331859132));
#450618=CARTESIAN_POINT('Origin',(-5.65685387860011,26.,5.65685387860011));
#450619=CARTESIAN_POINT('',(-4.92377157353716,24.3730384757729,6.39128196913613));
#450620=CARTESIAN_POINT('',(-4.92421628016771,24.2519615242271,6.38942086037359));
#450621=CARTESIAN_POINT('',(-4.92305381642377,26.,6.39065394077645));
#450622=CARTESIAN_POINT('Ctrl Pts',(-4.92421628016771,24.2519615242271,
6.38942086037359));
#450623=CARTESIAN_POINT('Ctrl Pts',(-5.04895543667043,24.2398389150381,
6.51405309196749));
#450624=CARTESIAN_POINT('Ctrl Pts',(-5.20382475542584,24.2277163058492,
6.60860369693141));
#450625=CARTESIAN_POINT('Ctrl Pts',(-5.37198243345446,24.2155936966603,
6.65652287894995));
#450626=CARTESIAN_POINT('Ctrl Pts',(-5.70250608555364,24.1917660064289,
6.75071080561528));
#450627=CARTESIAN_POINT('Ctrl Pts',(-6.08436822205294,24.1679383161975,
6.66474206054895));
#450628=CARTESIAN_POINT('Ctrl Pts',(-6.34264042812557,24.1441106259661,
6.4379983333991));
#450629=CARTESIAN_POINT('Ctrl Pts',(-6.60091263419821,24.1202829357347,
6.21125460624925));
#450630=CARTESIAN_POINT('Ctrl Pts',(-6.73559490984418,24.0964552455033,
5.84373589701588));
#450631=CARTESIAN_POINT('Ctrl Pts',(-6.68499023152592,24.0726275552719,
5.50379999638241));
#450632=CARTESIAN_POINT('Ctrl Pts',(-6.63438555320766,24.0487998650405,
5.16386409574894));
#450633=CARTESIAN_POINT('Ctrl Pts',(-6.39849392092517,24.0249721748091,
4.85151100371537));
#450634=CARTESIAN_POINT('Ctrl Pts',(-6.08537566804496,24.0011444845777,
4.70982751913656));
#450635=CARTESIAN_POINT('Ctrl Pts',(-5.77225741516475,23.9773167943463,
4.56814403455774));
#450636=CARTESIAN_POINT('Ctrl Pts',(-5.38191254168682,23.953489104115,4.59713015743369));
#450637=CARTESIAN_POINT('Ctrl Pts',(-5.09315534403941,23.9296614138836,
4.78350754767415));
#450638=CARTESIAN_POINT('Ctrl Pts',(-4.804398146392,23.9058337236522,4.96988493791459));
#450639=CARTESIAN_POINT('Ctrl Pts',(-4.61722862457511,23.8820060334208,
5.31365359551954));
#450640=CARTESIAN_POINT('Ctrl Pts',(-4.6173878516616,23.8581783431894,5.65733545950024));
#450641=CARTESIAN_POINT('Ctrl Pts',(-4.61751307348277,23.8394394035353,
5.92761905169082));
#450642=CARTESIAN_POINT('Ctrl Pts',(-4.73349750638545,23.8207004638812,
6.19784896370208));
#450643=CARTESIAN_POINT('Ctrl Pts',(-4.92356615355223,23.8019615242271,
6.39146732321148));
#450644=CARTESIAN_POINT('Ctrl Pts',(-4.92169483493571,23.9230384757729,
6.39152331859132));
#450645=CARTESIAN_POINT('Ctrl Pts',(-4.90819449199352,23.9243559671382,
6.37813961642664));
#450646=CARTESIAN_POINT('Ctrl Pts',(-4.895092278726,23.9256734585035,6.3643637478711));
#450647=CARTESIAN_POINT('Ctrl Pts',(-4.88241675495565,23.9269909498688,
6.35020586507153));
#450648=CARTESIAN_POINT('Ctrl Pts',(-4.65317164422858,23.9508186401002,
6.09415132493169));
#450649=CARTESIAN_POINT('Ctrl Pts',(-4.56349274466962,23.9746463303316,
5.71314343814525));
#450650=CARTESIAN_POINT('Ctrl Pts',(-4.6544613426263,23.998474020563,5.38171929489583));
#450651=CARTESIAN_POINT('Ctrl Pts',(-4.74542994058297,24.0223017107944,
5.05029515164641));
#450652=CARTESIAN_POINT('Ctrl Pts',(-5.01704603605528,24.0461294010258,
4.768454751934));
#450653=CARTESIAN_POINT('Ctrl Pts',(-5.34488416612327,24.0699570912572,
4.6653072414873));
#450654=CARTESIAN_POINT('Ctrl Pts',(-5.67272229619127,24.0937847814886,
4.56215973104059));
#450655=CARTESIAN_POINT('Ctrl Pts',(-6.05678246085496,24.11761247172,4.63770510985958));
#450656=CARTESIAN_POINT('Ctrl Pts',(-6.32112934350159,24.1414401619514,
4.8573365604447));
#450657=CARTESIAN_POINT('Ctrl Pts',(-6.58547622614821,24.1652678521828,
5.07696801102981));
#450658=CARTESIAN_POINT('Ctrl Pts',(-6.73010982677778,24.1890955424141,
5.44068553338104));
#450659=CARTESIAN_POINT('Ctrl Pts',(-6.68877448884912,24.2129232326455,
5.78187263496817));
#450660=CARTESIAN_POINT('Ctrl Pts',(-6.64743915092045,24.2367509228769,
6.12305973655531));
#450661=CARTESIAN_POINT('Ctrl Pts',(-6.42013487443355,24.2605786131083,
6.44171641737836));
#450662=CARTESIAN_POINT('Ctrl Pts',(-6.11098818332588,24.2844063033397,
6.59186824658804));
#450663=CARTESIAN_POINT('Ctrl Pts',(-5.80184149221821,24.3082339935711,
6.74202007579772));
#450664=CARTESIAN_POINT('Ctrl Pts',(-5.41085238648978,24.3320616838025,
6.72366705339403));
#450665=CARTESIAN_POINT('Ctrl Pts',(-5.11713028264445,24.3558893740339,
6.54521657215205));
#450666=CARTESIAN_POINT('Ctrl Pts',(-5.04666506349635,24.3616057412803,
6.50240552012982));
#450667=CARTESIAN_POINT('Ctrl Pts',(-4.98179796021343,24.3673221085266,
6.45038020112141));
#450668=CARTESIAN_POINT('Ctrl Pts',(-4.92377157353716,24.3730384757729,
6.39128196913613));
#450669=CARTESIAN_POINT('Origin',(-5.65685387860011,26.,5.65685387860011));
#450670=CARTESIAN_POINT('',(-4.92408802232565,24.8230384757729,6.38933869113556));
#450671=CARTESIAN_POINT('',(-4.92212745780799,24.7019615242271,6.39028821611916));
#450672=CARTESIAN_POINT('',(-4.92305381642377,26.,6.39065394077645));
#450673=CARTESIAN_POINT('Ctrl Pts',(-4.92212745780799,24.7019615242271,
6.39028821611916));
#450674=CARTESIAN_POINT('Ctrl Pts',(-5.11995795053564,24.6828050564265,
6.5845155347103));
#450675=CARTESIAN_POINT('Ctrl Pts',(-5.39828521249021,24.6636485886259,
6.70087353526984));
#450676=CARTESIAN_POINT('Ctrl Pts',(-5.67455106061111,24.6444921208253,
6.69616935490973));
#450677=CARTESIAN_POINT('Ctrl Pts',(-6.01818314973456,24.620664430594,6.69031808036474));
#450678=CARTESIAN_POINT('Ctrl Pts',(-6.35862591802898,24.5968367403626,
6.49716519325233));
#450679=CARTESIAN_POINT('Ctrl Pts',(-6.53992487743046,24.5730090501312,
6.20519269912468));
#450680=CARTESIAN_POINT('Ctrl Pts',(-6.72122383683194,24.5491813598998,
5.91322020499702));
#450681=CARTESIAN_POINT('Ctrl Pts',(-6.74337898734048,24.5253536696684,
5.52242810385412));
#450682=CARTESIAN_POINT('Ctrl Pts',(-6.59624120723028,24.501525979437,5.21183556708661));
#450683=CARTESIAN_POINT('Ctrl Pts',(-6.44910342712008,24.4776982892056,
4.9012430303191));
#450684=CARTESIAN_POINT('Ctrl Pts',(-6.13267271639113,24.4538705989742,
4.670850057927));
#450685=CARTESIAN_POINT('Ctrl Pts',(-5.7919038045113,24.4300429087428,4.62619808347199));
#450686=CARTESIAN_POINT('Ctrl Pts',(-5.45113489263147,24.4062152185114,
4.58154610901698));
#450687=CARTESIAN_POINT('Ctrl Pts',(-5.08602777960075,24.38238752828,4.72263513249907));
#450688=CARTESIAN_POINT('Ctrl Pts',(-4.86383551964991,24.3585598380486,
4.98483324415836));
#450689=CARTESIAN_POINT('Ctrl Pts',(-4.64164325969907,24.3347321478172,
5.24703135581765));
#450690=CARTESIAN_POINT('Ctrl Pts',(-4.56236585282811,24.3109044575858,
5.63033855565415));
#450691=CARTESIAN_POINT('Ctrl Pts',(-4.66231973324216,24.2870767673544,
5.9591644547709));
#450692=CARTESIAN_POINT('Ctrl Pts',(-4.71142093690032,24.275371686312,6.12069642705376));
#450693=CARTESIAN_POINT('Ctrl Pts',(-4.80377340246064,24.2636666052695,
6.26908122485669));
#450694=CARTESIAN_POINT('Ctrl Pts',(-4.92421628016771,24.2519615242271,
6.38942086037359));
#450695=CARTESIAN_POINT('Ctrl Pts',(-4.92377157353716,24.3730384757729,
6.39128196913613));
#450696=CARTESIAN_POINT('Ctrl Pts',(-4.7399249826062,24.391149798758,6.20403942134221));
#450697=CARTESIAN_POINT('Ctrl Pts',(-4.62474754709557,24.4092611217431,
5.94579686164739));
#450698=CARTESIAN_POINT('Ctrl Pts',(-4.61775970678068,24.4273724447281,
5.68465923264326));
#450699=CARTESIAN_POINT('Ctrl Pts',(-4.60856633672445,24.4512001349595,
5.34110031445673));
#450700=CARTESIAN_POINT('Ctrl Pts',(-4.7866346985742,24.4750278251909,4.99253041816395));
#450701=CARTESIAN_POINT('Ctrl Pts',(-5.07039290068915,24.4988555154223,
4.79862701145602));
#450702=CARTESIAN_POINT('Ctrl Pts',(-5.35415110280411,24.5226832056536,
4.60472360474809));
#450703=CARTESIAN_POINT('Ctrl Pts',(-5.7435991451843,24.546510895885,4.565486687625));
#450704=CARTESIAN_POINT('Ctrl Pts',(-6.06033356407531,24.5703385861164,
4.69889042440694));
#450705=CARTESIAN_POINT('Ctrl Pts',(-6.37706798296632,24.5941662763478,
4.83229416118888));
#450706=CARTESIAN_POINT('Ctrl Pts',(-6.62108877836816,24.6179939665792,
5.13833855187584));
#450707=CARTESIAN_POINT('Ctrl Pts',(-6.68061169925028,24.6418216568106,
5.47682676316715));
#450708=CARTESIAN_POINT('Ctrl Pts',(-6.74013462013239,24.665649347042,5.81531497445846));
#450709=CARTESIAN_POINT('Ctrl Pts',(-6.61515966649478,24.6894770372734,
6.18624700635411));
#450710=CARTESIAN_POINT('Ctrl Pts',(-6.36293701391879,24.7133047275048,
6.41970146010492));
#450711=CARTESIAN_POINT('Ctrl Pts',(-6.1107143613428,24.7371324177362,6.65315591385573));
#450712=CARTESIAN_POINT('Ctrl Pts',(-5.73124400982843,24.7609601079676,
6.7491327894617));
#450713=CARTESIAN_POINT('Ctrl Pts',(-5.3983586947443,24.784787798199,6.6636657201663));
#450714=CARTESIAN_POINT('Ctrl Pts',(-5.22023136007979,24.797538024057,6.61793218802977));
#450715=CARTESIAN_POINT('Ctrl Pts',(-5.05544287282308,24.8102882499149,
6.5202452116208));
#450716=CARTESIAN_POINT('Ctrl Pts',(-4.92408802232565,24.8230384757729,
6.38933869113556));
#450717=CARTESIAN_POINT('Origin',(-5.65685387860011,26.,5.65685387860011));
#450718=CARTESIAN_POINT('',(-4.92197603118329,25.2730384757729,6.39051881327128));
#450719=CARTESIAN_POINT('',(-4.92254817630007,25.1519615242271,6.39198798715976));
#450720=CARTESIAN_POINT('',(-4.92305381642377,26.,6.39065394077645));
#450721=CARTESIAN_POINT('Ctrl Pts',(-4.92254817630007,25.1519615242271,
6.39198798715976));
#450722=CARTESIAN_POINT('Ctrl Pts',(-4.94650751599249,25.1495988880462,
6.41627314991443));
#450723=CARTESIAN_POINT('Ctrl Pts',(-4.97169983154625,25.1472362518654,
6.43929566708609));
#450724=CARTESIAN_POINT('Ctrl Pts',(-4.99805942366946,25.1448736156846,
6.46089355482011));
#450725=CARTESIAN_POINT('Ctrl Pts',(-5.26390153716754,25.1210459254532,
6.67871286308055));
#450726=CARTESIAN_POINT('Ctrl Pts',(-5.64846913729549,25.0972182352218,
6.75163093056004));
#450727=CARTESIAN_POINT('Ctrl Pts',(-5.97559449046916,25.0733905449904,
6.64624470558553));
#450728=CARTESIAN_POINT('Ctrl Pts',(-6.30271984364283,25.049562854759,6.54085848061101));
#450729=CARTESIAN_POINT('Ctrl Pts',(-6.57240294986222,25.0257351645276,
6.25716796318249));
#450730=CARTESIAN_POINT('Ctrl Pts',(-6.66110381706144,25.0019074742962,
5.92512971718013));
#450731=CARTESIAN_POINT('Ctrl Pts',(-6.74980468426065,24.9780797840648,
5.59309147117778));
#450732=CARTESIAN_POINT('Ctrl Pts',(-6.65752331243968,24.9542520938335,
5.2127054966016));
#450733=CARTESIAN_POINT('Ctrl Pts',(-6.42653317184816,24.9304244036021,
4.95822404429259));
#450734=CARTESIAN_POINT('Ctrl Pts',(-6.19554303125664,24.9065967133707,
4.70374259198359));
#450735=CARTESIAN_POINT('Ctrl Pts',(-5.82584412189456,24.8827690231393,
4.57516566194178));
#450736=CARTESIAN_POINT('Ctrl Pts',(-5.48679296352304,24.8589413329079,
4.63139343216518));
#450737=CARTESIAN_POINT('Ctrl Pts',(-5.14774180515151,24.8351136426765,
4.68762120238858));
#450738=CARTESIAN_POINT('Ctrl Pts',(-4.83933839777055,24.8112859524451,
4.9286536728772));
#450739=CARTESIAN_POINT('Ctrl Pts',(-4.70286022094558,24.7874582622137,
5.24407554312885));
#450740=CARTESIAN_POINT('Ctrl Pts',(-4.56638204412061,24.7636305719823,
5.55949741338051));
#450741=CARTESIAN_POINT('Ctrl Pts',(-4.60182909785165,24.7398028817509,
5.94930868339519));
#450742=CARTESIAN_POINT('Ctrl Pts',(-4.79296332969342,24.7159751915195,
6.23493948741375));
#450743=CARTESIAN_POINT('Ctrl Pts',(-4.83043362171106,24.7113039690887,
6.29093505415592));
#450744=CARTESIAN_POINT('Ctrl Pts',(-4.87388734148021,24.7066327466579,
6.34292671833547));
#450745=CARTESIAN_POINT('Ctrl Pts',(-4.92212745780799,24.7019615242271,
6.39028821611916));
#450746=CARTESIAN_POINT('Ctrl Pts',(-4.92408802232565,24.8230384757729,
6.38933869113556));
#450747=CARTESIAN_POINT('Ctrl Pts',(-4.80996622614209,24.8341159401463,
6.27560640646284));
#450748=CARTESIAN_POINT('Ctrl Pts',(-4.72108089883846,24.8451934045197,
6.13679925493306));
#450749=CARTESIAN_POINT('Ctrl Pts',(-4.67061008310121,24.8562708688931,
5.98520281626299));
#450750=CARTESIAN_POINT('Ctrl Pts',(-4.56204706519615,24.8800985591245,
5.65911799585187));
#450751=CARTESIAN_POINT('Ctrl Pts',(-4.63122130803993,24.9039262493559,
5.27385936922642));
#450752=CARTESIAN_POINT('Ctrl Pts',(-4.84644449237099,24.9277539395873,
5.00591117956891));
#450753=CARTESIAN_POINT('Ctrl Pts',(-5.06166767670205,24.9515816298187,
4.7379629899114));
#450754=CARTESIAN_POINT('Ctrl Pts',(-5.42293980252039,24.9754093200501,
4.58732523722183));
#450755=CARTESIAN_POINT('Ctrl Pts',(-5.7647647438604,24.9992370102815,4.62300419682159));
#450756=CARTESIAN_POINT('Ctrl Pts',(-6.10658968520039,25.0230647005129,
4.65868315642135));
#450757=CARTESIAN_POINT('Ctrl Pts',(-6.42896744206205,25.0468923907443,
4.88067882831044));
#450758=CARTESIAN_POINT('Ctrl Pts',(-6.58421869570625,25.0707200809757,
5.18729621377842));
#450759=CARTESIAN_POINT('Ctrl Pts',(-6.73946994935045,25.0945477712071,
5.49391359924639));
#450760=CARTESIAN_POINT('Ctrl Pts',(-6.72759469977719,25.1183754614385,
5.88515269829325));
#450761=CARTESIAN_POINT('Ctrl Pts',(-6.5540334824637,25.1422031516699,6.18179018209155));
#450762=CARTESIAN_POINT('Ctrl Pts',(-6.38047226515022,25.1660308419013,
6.47842766588984));
#450763=CARTESIAN_POINT('Ctrl Pts',(-6.0452250800965,25.1898585321326,6.68046353443956));
#450764=CARTESIAN_POINT('Ctrl Pts',(-5.70186524531576,25.213686222364,6.69534535485932));
#450765=CARTESIAN_POINT('Ctrl Pts',(-5.41677424787487,25.2334703068337,
6.70770170116848));
#450766=CARTESIAN_POINT('Ctrl Pts',(-5.12609043162756,25.2532543913033,
6.59103501365993));
#450767=CARTESIAN_POINT('Ctrl Pts',(-4.92197603118329,25.2730384757729,
6.39051881327128));
#450768=CARTESIAN_POINT('Origin',(-5.65685387860011,26.,5.65685387860011));
#450769=CARTESIAN_POINT('',(-4.92276701974739,25.7230384757729,6.39190058798136));
#450770=CARTESIAN_POINT('',(-4.92443355077908,25.6019615242271,6.39006796800886));
#450771=CARTESIAN_POINT('',(-4.92305381642377,26.,6.39065394077645));
#450772=CARTESIAN_POINT('',(-6.69274404704181,26.,5.59475217632209));
#450773=CARTESIAN_POINT('Ctrl Pts',(-4.92276701974739,25.7230384757729,
6.39190058798136));
#450774=CARTESIAN_POINT('Ctrl Pts',(-4.71160994855805,25.7438759131544,
6.17742942344334));
#450775=CARTESIAN_POINT('Ctrl Pts',(-4.59523934827088,25.764713350536,5.86562000134797));
#450776=CARTESIAN_POINT('Ctrl Pts',(-4.62142687258513,25.7855507879175,
5.56615422141076));
#450777=CARTESIAN_POINT('Ctrl Pts',(-4.65137240791476,25.8093784781489,
5.22371394391399));
#450778=CARTESIAN_POINT('Ctrl Pts',(-4.86772710302321,25.8332061683802,
4.89741422641509));
#450779=CARTESIAN_POINT('Ctrl Pts',(-5.17187737628347,25.8570338586116,
4.73725319022189));
#450780=CARTESIAN_POINT('Ctrl Pts',(-5.47602764954372,25.880861548843,4.57709215402869));
#450781=CARTESIAN_POINT('Ctrl Pts',(-5.86797350095578,25.9046892390744,
4.58306979914119));
#450782=CARTESIAN_POINT('Ctrl Pts',(-6.16698733288025,25.9285169293058,
4.75132533448083));
#450783=CARTESIAN_POINT('Ctrl Pts',(-6.46600116480472,25.9523446195372,
4.91958086982048));
#450784=CARTESIAN_POINT('Ctrl Pts',(-6.67208297724159,25.9761723097686,
5.25011429538726));
#450785=CARTESIAN_POINT('Ctrl Pts',(-6.69274404704181,26.,5.59475217632212));
#450786=CARTESIAN_POINT('',(-5.59444809180803,26.,6.69457727933146));
#450787=CARTESIAN_POINT('Origin',(-5.65685387860011,26.,5.65685387860011));
#450788=CARTESIAN_POINT('Ctrl Pts',(-5.59444726164187,26.,6.69458228414866));
#450789=CARTESIAN_POINT('Ctrl Pts',(-5.92484673178863,25.9770624644402,
6.71351646533254));
#450790=CARTESIAN_POINT('Ctrl Pts',(-6.26627937525033,25.9541249288804,
6.56158375468957));
#450791=CARTESIAN_POINT('Ctrl Pts',(-6.47167795527827,25.9311873933205,
6.30214239804397));
#450792=CARTESIAN_POINT('Ctrl Pts',(-6.68504759676004,25.9073597030892,
6.03263270014108));
#450793=CARTESIAN_POINT('Ctrl Pts',(-6.75161994353754,25.8835320128578,
5.64710810132191));
#450794=CARTESIAN_POINT('Ctrl Pts',(-6.64083855948586,25.8597043226264,
5.32182159136527));
#450795=CARTESIAN_POINT('Ctrl Pts',(-6.53005717543418,25.835876632395,4.99653508140864));
#450796=CARTESIAN_POINT('Ctrl Pts',(-6.24192206055333,25.8120489421636,
4.73148666031454));
#450797=CARTESIAN_POINT('Ctrl Pts',(-5.90845611919747,25.7882212519322,
4.64827248224482));
#450798=CARTESIAN_POINT('Ctrl Pts',(-5.57499017784161,25.7643935617008,
4.56505830417509));
#450799=CARTESIAN_POINT('Ctrl Pts',(-5.19619341001074,25.7405658714694,
4.66367836912974));
#450800=CARTESIAN_POINT('Ctrl Pts',(-4.94557465216384,25.716738181238,4.89886414913016));
#450801=CARTESIAN_POINT('Ctrl Pts',(-4.69495589431694,25.6929104910066,
5.13404992913058));
#450802=CARTESIAN_POINT('Ctrl Pts',(-4.572515146454,25.6690828007752,5.50580142417677));
#450803=CARTESIAN_POINT('Ctrl Pts',(-4.63434949773116,25.6452551105439,
5.84386841174159));
#450804=CARTESIAN_POINT('Ctrl Pts',(-4.67179935541582,25.6308239151049,
6.04861804217652));
#450805=CARTESIAN_POINT('Ctrl Pts',(-4.7768430935332,25.616392719666,6.24101187097706));
#450806=CARTESIAN_POINT('Ctrl Pts',(-4.92443355077908,25.6019615242271,
6.39006796800886));
#450807=CARTESIAN_POINT('Origin',(-5.65685387860011,26.993675081176,5.65685387860011));
#450808=CARTESIAN_POINT('',(-4.74524035180399,22.756324918824,6.5673434103921));
#450809=CARTESIAN_POINT('',(-4.74364038176039,22.718675081176,6.57057146528765));
#450810=CARTESIAN_POINT('',(-4.74468613086949,26.993675081176,6.56902162633079));
#450811=CARTESIAN_POINT('',(-6.64591806159944,22.5,4.8286920333622));
#450812=CARTESIAN_POINT('Ctrl Pts',(-4.74364038176039,22.718675081176,6.57057146528766));
#450813=CARTESIAN_POINT('Ctrl Pts',(-4.76142457130848,22.7172664581449,
6.58852418981576));
#450814=CARTESIAN_POINT('Ctrl Pts',(-5.09000197050781,22.6920301448823,
6.9000556810006));
#450815=CARTESIAN_POINT('Ctrl Pts',(-6.06611679986992,22.6429661413884,
7.12689194633153));
#450816=CARTESIAN_POINT('Ctrl Pts',(-7.11331947438321,22.5714830706942,
6.10694434613243));
#450817=CARTESIAN_POINT('Ctrl Pts',(-6.92144528650133,22.5238276902314,
5.15775103452081));
#450818=CARTESIAN_POINT('Ctrl Pts',(-6.64591806159944,22.5,4.8286920333622));
#450819=CARTESIAN_POINT('',(-6.09734856608926,22.5,4.44194770692244));
#450820=CARTESIAN_POINT('Origin',(-5.65685387860011,22.5,5.65685387860011));
#450821=CARTESIAN_POINT('Ctrl Pts',(-4.74524035180399,22.756324918824,6.5673434103921));
#450822=CARTESIAN_POINT('Ctrl Pts',(-4.93595953019022,22.7414761952386,
6.75594870135602));
#450823=CARTESIAN_POINT('Ctrl Pts',(-5.58182921801751,22.7027997814218,
7.10121210146151));
#450824=CARTESIAN_POINT('Ctrl Pts',(-6.78713386963137,22.6402956773736,
6.6805523241845));
#450825=CARTESIAN_POINT('Ctrl Pts',(-7.12528591239125,22.569702761351,5.27997950888059));
#450826=CARTESIAN_POINT('Ctrl Pts',(-6.48370144903283,22.5229375355598,
4.58325719964657));
#450827=CARTESIAN_POINT('Ctrl Pts',(-6.09735008669021,22.5,4.44194158662797));
#450828=CARTESIAN_POINT('Origin',(-5.65685387860011,26.993675081176,5.65685387860011));
#450829=CARTESIAN_POINT('',(-4.74299838399068,23.206324918824,6.56983844394705));
#450830=CARTESIAN_POINT('',(-4.74631652959707,23.168675081176,6.56867439792569));
#450831=CARTESIAN_POINT('',(-4.74468613086949,26.993675081176,6.56902162633079));
#450832=CARTESIAN_POINT('Ctrl Pts',(-4.74631652959707,23.168675081176,6.56867439792569));
#450833=CARTESIAN_POINT('Ctrl Pts',(-4.853408844765,23.1602325995332,6.67716702479821));
#450834=CARTESIAN_POINT('Ctrl Pts',(-5.33214451040115,23.127962427659,7.02077633180239));
#450835=CARTESIAN_POINT('Ctrl Pts',(-6.47507582842176,23.0718645655535,
6.94377741359718));
#450836=CARTESIAN_POINT('Ctrl Pts',(-7.18181942856023,23.0003814948592,
5.66653874837814));
#450837=CARTESIAN_POINT('Ctrl Pts',(-6.49141154940691,22.9288984241651,
4.38054591235378));
#450838=CARTESIAN_POINT('Ctrl Pts',(-5.03639155729104,22.8574153534709,
4.26365553420012));
#450839=CARTESIAN_POINT('Ctrl Pts',(-4.16730445086878,22.7873409058079,
5.40079341912851));
#450840=CARTESIAN_POINT('Ctrl Pts',(-4.46059450521194,22.7410941483762,
6.28484325502835));
#450841=CARTESIAN_POINT('Ctrl Pts',(-4.74364038176039,22.718675081176,6.57057146528766));
#450842=CARTESIAN_POINT('Ctrl Pts',(-4.74299838399068,23.206324918824,6.56983844394705));
#450843=CARTESIAN_POINT('Ctrl Pts',(-5.02227299078827,23.184442336627,6.84584090104065));
#450844=CARTESIAN_POINT('Ctrl Pts',(-5.88847306909541,23.1387320641985,
7.14533371342118));
#450845=CARTESIAN_POINT('Ctrl Pts',(-7.03563221165043,23.0691941015387,
6.3084575374563));
#450846=CARTESIAN_POINT('Ctrl Pts',(-6.95165327175697,22.9977110308445,
4.85119529970875));
#450847=CARTESIAN_POINT('Ctrl Pts',(-5.68141376558384,22.9262279601503,
4.13204038713623));
#450848=CARTESIAN_POINT('Ctrl Pts',(-4.38863987327371,22.8547448894562,
4.80994952176022));
#450849=CARTESIAN_POINT('Ctrl Pts',(-4.28501879514303,22.7981105423474,
5.9617065202947));
#450850=CARTESIAN_POINT('Ctrl Pts',(-4.62991319040622,22.76530388547,6.45329450867431));
#450851=CARTESIAN_POINT('Ctrl Pts',(-4.74524035180399,22.756324918824,6.5673434103921));
#450852=CARTESIAN_POINT('Origin',(-5.65685387860011,26.993675081176,5.65685387860011));
#450853=CARTESIAN_POINT('',(-4.74532300381163,23.656324918824,6.57003272085371));
#450854=CARTESIAN_POINT('',(-4.74499326893249,23.618675081176,6.56740434249263));
#450855=CARTESIAN_POINT('',(-4.74468613086949,26.993675081176,6.56902162633079));
#450856=CARTESIAN_POINT('Ctrl Pts',(-4.74499326893249,23.618675081176,6.56740434249263));
#450857=CARTESIAN_POINT('Ctrl Pts',(-4.94389036502613,23.6031987409216,
6.76368003125862));
#450858=CARTESIAN_POINT('Ctrl Pts',(-5.60787864620878,23.5638947104357,
7.10715379447204));
#450859=CARTESIAN_POINT('Ctrl Pts',(-6.81352117024561,23.5007629897185,
6.65070324968042));
#450860=CARTESIAN_POINT('Ctrl Pts',(-7.11892889768229,23.4292799190243,
5.22331918686542));
#450861=CARTESIAN_POINT('Ctrl Pts',(-6.08480364614363,23.3577968483302,
4.19313572939823));
#450862=CARTESIAN_POINT('Ctrl Pts',(-4.65859667867589,23.2863137776359,
4.50398657889369));
#450863=CARTESIAN_POINT('Ctrl Pts',(-4.20740365817457,23.2232731885846,
5.70962577012502));
#450864=CARTESIAN_POINT('Ctrl Pts',(-4.55115618731809,23.1840602897646,
6.37096218895919));
#450865=CARTESIAN_POINT('Ctrl Pts',(-4.74631652959707,23.168675081176,6.56867439792569));
#450866=CARTESIAN_POINT('Ctrl Pts',(-4.74532300381163,23.656324918824,6.57003272085371));
#450867=CARTESIAN_POINT('Ctrl Pts',(-4.80948437015677,23.6512361682467,
6.63539236159828));
#450868=CARTESIAN_POINT('Ctrl Pts',(-5.21266771861287,23.622319727438,6.9668858368575));
#450869=CARTESIAN_POINT('Ctrl Pts',(-6.28682364983266,23.569575596398,7.04564953674368));
#450870=CARTESIAN_POINT('Ctrl Pts',(-7.16543624640093,23.4980925257038,
5.88000083782648));
#450871=CARTESIAN_POINT('Ctrl Pts',(-6.66190630419616,23.4266094550096,
4.50990820099156));
#450872=CARTESIAN_POINT('Ctrl Pts',(-5.23756146736659,23.3551263843154,
4.19063094092434));
#450873=CARTESIAN_POINT('Ctrl Pts',(-4.19736598356862,23.2836433136212,
5.21468783779196));
#450874=CARTESIAN_POINT('Ctrl Pts',(-4.40342562281452,23.2340428251241,
6.20635078283889));
#450875=CARTESIAN_POINT('Ctrl Pts',(-4.71817410701172,23.2082700268584,
6.54530502316694));
#450876=CARTESIAN_POINT('Ctrl Pts',(-4.74299838399068,23.206324918824,6.56983844394705));
#450877=CARTESIAN_POINT('Origin',(-5.65685387860011,26.993675081176,5.65685387860011));
#450878=CARTESIAN_POINT('',(-4.74613115927677,24.106324918824,6.56748881619374));
#450879=CARTESIAN_POINT('',(-4.74299681637215,24.068675081176,6.57010232725217));
#450880=CARTESIAN_POINT('',(-4.74468613086949,26.993675081176,6.56902162633079));
#450881=CARTESIAN_POINT('Ctrl Pts',(-4.74299681637215,24.068675081176,6.57010232725217));
#450882=CARTESIAN_POINT('Ctrl Pts',(-5.02972694085412,24.0461648823099,
6.85435514987614));
#450883=CARTESIAN_POINT('Ctrl Pts',(-5.91736950865738,23.9998269932124,
7.14655186859909));
#450884=CARTESIAN_POINT('Ctrl Pts',(-7.0522818436793,23.9296614138836,6.27199288310558));
#450885=CARTESIAN_POINT('Ctrl Pts',(-6.93003241982605,23.8581783431894,
4.81743049717126));
#450886=CARTESIAN_POINT('Ctrl Pts',(-5.64131435190337,23.7866952724952,
4.13193628895796));
#450887=CARTESIAN_POINT('Ctrl Pts',(-4.3668333837381,23.715212201801,4.84355050202496));
#450888=CARTESIAN_POINT('Ctrl Pts',(-4.29429575151249,23.6592054713613,
5.98491025846011));
#450889=CARTESIAN_POINT('Ctrl Pts',(-4.63766432477859,23.627026431153,6.4614899633887));
#450890=CARTESIAN_POINT('Ctrl Pts',(-4.74499326893249,23.618675081176,6.56740434249263));
#450891=CARTESIAN_POINT('Ctrl Pts',(-4.74613115927677,24.106324918824,6.56748881619374));
#450892=CARTESIAN_POINT('Ctrl Pts',(-4.90119115627847,24.0942023096351,
6.72241589762581));
#450893=CARTESIAN_POINT('Ctrl Pts',(-5.47210261995128,24.0582520102147,
7.07096798466868));
#450894=CARTESIAN_POINT('Ctrl Pts',(-6.662968703113,23.998474020563,6.80286792203874));
#450895=CARTESIAN_POINT('Ctrl Pts',(-7.16522879152533,23.9269909498688,
5.43230911237055));
#450896=CARTESIAN_POINT('Ctrl Pts',(-6.2855365564656,23.8555078791747,4.26747512907024));
#450897=CARTESIAN_POINT('Ctrl Pts',(-4.82985391579145,23.7840248084805,
4.37557081254884));
#450898=CARTESIAN_POINT('Ctrl Pts',(-4.18154636230721,23.7176304883636,
5.56629788826614));
#450899=CARTESIAN_POINT('Ctrl Pts',(-4.50905361827065,23.6750638584781,
6.32935078034095));
#450900=CARTESIAN_POINT('Ctrl Pts',(-4.74532300381163,23.656324918824,6.57003272085371));
#450901=CARTESIAN_POINT('Origin',(-5.65685387860011,26.993675081176,5.65685387860011));
#450902=CARTESIAN_POINT('',(-4.74353459859835,24.556324918824,6.56856700353347));
#450903=CARTESIAN_POINT('',(-4.74557835604531,24.518675081176,6.56980231202958));
#450904=CARTESIAN_POINT('',(-4.74468613086949,26.993675081176,6.56902162633079));
#450905=CARTESIAN_POINT('Ctrl Pts',(-4.74557835604531,24.518675081176,6.56980231202958));
#450906=CARTESIAN_POINT('Ctrl Pts',(-4.81770944620421,24.5129587139297,
6.64326578517921));
#450907=CARTESIAN_POINT('Ctrl Pts',(-5.23445549419879,24.4834146564519,
6.97750833641272));
#450908=CARTESIAN_POINT('Ctrl Pts',(-6.32311258055822,24.4300429087428,
7.0286098827299));
#450909=CARTESIAN_POINT('Ctrl Pts',(-7.17078066054311,24.3585598380486,
5.84026841822956));
#450910=CARTESIAN_POINT('Ctrl Pts',(-6.63140987332417,24.2870767673545,
4.4838850778304));
#450911=CARTESIAN_POINT('Ctrl Pts',(-5.19916430623342,24.2155936966603,
4.2021595986403));
#450912=CARTESIAN_POINT('Ctrl Pts',(-4.18624762160046,24.1441106259661,
5.25320498229437));
#450913=CARTESIAN_POINT('Ctrl Pts',(-4.41536649518845,24.095137754138,6.22663461042285));
#450914=CARTESIAN_POINT('Ctrl Pts',(-4.72621489163553,24.0699925725413,
6.55346539562852));
#450915=CARTESIAN_POINT('Ctrl Pts',(-4.74299681637215,24.068675081176,6.57010232725217));
#450916=CARTESIAN_POINT('Ctrl Pts',(-4.74353459859835,24.556324918824,6.56856700353347));
#450917=CARTESIAN_POINT('Ctrl Pts',(-4.9894525322227,24.5371684510234,6.81000592522228));
#450918=CARTESIAN_POINT('Ctrl Pts',(-5.76578134653658,24.4941842929915,
7.13455935910424));
#450919=CARTESIAN_POINT('Ctrl Pts',(-6.95240396480877,24.4273724447281,
6.4613196666284));
#450920=CARTESIAN_POINT('Ctrl Pts',(-7.03502543671246,24.3558893740339,
5.00396921476326));
#450921=CARTESIAN_POINT('Ctrl Pts',(-5.85498510857851,24.2844063033397,
4.14478270244581));
#450922=CARTESIAN_POINT('Ctrl Pts',(-4.49341967622111,24.2129232326456,
4.67093497503136));
#450923=CARTESIAN_POINT('Ctrl Pts',(-4.24791389261248,24.1535627711403,
5.85795834238072));
#450924=CARTESIAN_POINT('Ctrl Pts',(-4.59641175456261,24.1180299998664,
6.41789774915756));
#450925=CARTESIAN_POINT('Ctrl Pts',(-4.74613115927677,24.106324918824,6.56748881619374));
#450926=CARTESIAN_POINT('Origin',(-5.65685387860011,26.993675081176,5.65685387860011));
#450927=CARTESIAN_POINT('',(-4.74405758279954,25.006324918824,6.57067994464873));
#450928=CARTESIAN_POINT('',(-4.74597172529335,24.968675081176,6.56738667375376));
#450929=CARTESIAN_POINT('',(-4.74468613086949,26.993675081176,6.56902162633079));
#450930=CARTESIAN_POINT('Ctrl Pts',(-4.74597172529336,24.968675081176,6.56738667375376));
#450931=CARTESIAN_POINT('Ctrl Pts',(-4.90925551921452,24.955924855318,6.73011316031215));
#450932=CARTESIAN_POINT('Ctrl Pts',(-5.49691387622178,24.9193469392286,
7.07847832230359));
#450933=CARTESIAN_POINT('Ctrl Pts',(-6.69274573713214,24.8589413329079,
6.77602463836695));
#450934=CARTESIAN_POINT('Ctrl Pts',(-7.15880506797054,24.7874582622137,
5.39273679116275));
#450935=CARTESIAN_POINT('Ctrl Pts',(-6.24879737998678,24.7159751915195,
4.25142935492228));
#450936=CARTESIAN_POINT('Ctrl Pts',(-4.79645922145989,24.6444921208253,
4.39775252453571));
#450937=CARTESIAN_POINT('Ctrl Pts',(-4.18550614000559,24.5787254173775,
5.59369688000734));
#450938=CARTESIAN_POINT('Ctrl Pts',(-4.51704344657683,24.5367864041611,
6.33704597702196));
#450939=CARTESIAN_POINT('Ctrl Pts',(-4.74557835604531,24.518675081176,6.56980231202958));
#450940=CARTESIAN_POINT('Ctrl Pts',(-4.74405758279954,25.006324918824,6.57067994464873));
#450941=CARTESIAN_POINT('Ctrl Pts',(-4.77384081402403,25.0039622826432,
6.60086819803686));
#450942=CARTESIAN_POINT('Ctrl Pts',(-5.12098437694123,24.9777719562309,
6.91811250300101));
#450943=CARTESIAN_POINT('Ctrl Pts',(-6.12447699388038,24.9277539395873,
7.10838527255516));
#450944=CARTESIAN_POINT('Ctrl Pts',(-7.13018513270865,24.8562708688931,
6.05044038944422));
#450945=CARTESIAN_POINT('Ctrl Pts',(-6.78604742232836,24.784787798199,4.63189669239788));
#450946=CARTESIAN_POINT('Ctrl Pts',(-5.40735816264999,24.7133047275048,
4.15240479236238));
#450947=CARTESIAN_POINT('Ctrl Pts',(-4.25725342975252,24.6418216568106,
5.05126835371239));
#450948=CARTESIAN_POINT('Ctrl Pts',(-4.35401829743014,24.589495053917,6.11539165852711));
#450949=CARTESIAN_POINT('Ctrl Pts',(-4.68356856625642,24.5609961412548,
6.50969315902277));
#450950=CARTESIAN_POINT('Ctrl Pts',(-4.74353459859835,24.556324918824,6.56856700353347));
#450951=CARTESIAN_POINT('Origin',(-5.65685387860011,26.993675081176,5.65685387860011));
#450952=CARTESIAN_POINT('',(-4.74640124271564,25.456324918824,6.56829321884323));
#450953=CARTESIAN_POINT('',(-4.74334636410459,25.418675081176,6.56885365284802));
#450954=CARTESIAN_POINT('',(-4.74468613086949,26.993675081176,6.56902162633079));
#450955=CARTESIAN_POINT('Ctrl Pts',(-4.74334636410459,25.418675081176,6.56885365284802));
#450956=CARTESIAN_POINT('Ctrl Pts',(-4.99707565976646,25.3988909967064,
6.81811011972481));
#450957=CARTESIAN_POINT('Ctrl Pts',(-5.79361205385018,25.3552792220053,
7.13780202337966));
#450958=CARTESIAN_POINT('Ctrl Pts',(-6.97310209577086,25.287839757073,6.42698533143036));
#450959=CARTESIAN_POINT('Ctrl Pts',(-7.01738753624157,25.2163566863788,
4.96796792520407));
#450960=CARTESIAN_POINT('Ctrl Pts',(-5.81516935358237,25.1448736156846,
4.14009680960707));
#450961=CARTESIAN_POINT('Ctrl Pts',(-4.4679054394248,25.0733905449904,4.70185841202445));
#450962=CARTESIAN_POINT('Ctrl Pts',(-4.25595199715398,25.0146577001542,
5.88231068328695));
#450963=CARTESIAN_POINT('Ctrl Pts',(-4.604109892408,24.9797525455494,6.4260090324839));
#450964=CARTESIAN_POINT('Ctrl Pts',(-4.74597172529336,24.968675081176,6.56738667375376));
#450965=CARTESIAN_POINT('Ctrl Pts',(-4.74640124271564,25.456324918824,6.56829321884323));
#450966=CARTESIAN_POINT('Ctrl Pts',(-4.86586022639608,25.4469284240315,
6.68893848409317));
#450967=CARTESIAN_POINT('Ctrl Pts',(-5.36752678600608,25.4137042390077,
7.03476003379299));
#450968=CARTESIAN_POINT('Ctrl Pts',(-6.5258341885166,25.3566523637524,6.91003560334641));
#450969=CARTESIAN_POINT('Ctrl Pts',(-7.18099123031483,25.2851692930582,
5.60564496305));
#450970=CARTESIAN_POINT('Ctrl Pts',(-6.43975200870338,25.213686222364,4.34815567114859));
#450971=CARTESIAN_POINT('Ctrl Pts',(-4.98123363545819,25.1422031516699,
4.28968558428151));
#450972=CARTESIAN_POINT('Ctrl Pts',(-4.16945626611646,25.0730827171565,
5.44432497425889));
#450973=CARTESIAN_POINT('Ctrl Pts',(-4.47347056935133,25.0277899728746,
6.29641321838457));
#450974=CARTESIAN_POINT('Ctrl Pts',(-4.74405758279954,25.006324918824,6.57067994464873));
#450975=CARTESIAN_POINT('Origin',(-5.65685387860011,26.993675081176,5.65685387860011));
#450976=CARTESIAN_POINT('',(-4.7445060113485,25.906324918824,6.56704169373441));
#450977=CARTESIAN_POINT('',(-4.74432962138981,25.868675081176,6.57057130100612));
#450978=CARTESIAN_POINT('',(-4.74468613086949,26.993675081176,6.56902162633079));
#450979=CARTESIAN_POINT('',(-4.53900700771688,26.,5.01302286563433));
#450980=CARTESIAN_POINT('Ctrl Pts',(-4.53900700771688,26.,5.01302286563431));
#450981=CARTESIAN_POINT('Ctrl Pts',(-4.32480615636363,25.9761723097686,
5.38492752167559));
#450982=CARTESIAN_POINT('Ctrl Pts',(-4.30899334914827,25.9449472827099,
6.01924597306242));
#450983=CARTESIAN_POINT('Ctrl Pts',(-4.64940368207851,25.9137222556513,
6.47338425157138));
#450984=CARTESIAN_POINT('Ctrl Pts',(-4.7445060113485,25.906324918824,6.56704169373441));
#450985=CARTESIAN_POINT('',(-5.01208503488091,26.,4.53689596693371));
#450986=CARTESIAN_POINT('Origin',(-5.65685387860011,26.,5.65685387860011));
#450987=CARTESIAN_POINT('Ctrl Pts',(-5.01208247494518,26.,4.5368902045627));
#450988=CARTESIAN_POINT('Ctrl Pts',(-4.65613984562121,25.9770624644402,
4.74314812622022));
#450989=CARTESIAN_POINT('Ctrl Pts',(-4.17795197796788,25.9332874914989,
5.48969900651177));
#450990=CARTESIAN_POINT('Ctrl Pts',(-4.48184576512937,25.8895125185575,
6.3039677816093));
#450991=CARTESIAN_POINT('Ctrl Pts',(-4.74432962138981,25.868675081176,6.57057130100612));
#450992=CARTESIAN_POINT('Origin',(5.65685387860011,26.,5.65685387860011));
#450993=CARTESIAN_POINT('',(6.39190072013885,22.573038475773,4.9222125558517));
#450994=CARTESIAN_POINT('',(6.39065394077645,22.5,4.92305381642377));
#450995=CARTESIAN_POINT('',(6.39065394077645,26.,4.92305381642377));
#450996=CARTESIAN_POINT('',(6.66622270032004,22.5,5.8978925564917));
#450997=CARTESIAN_POINT('Origin',(5.65685387860011,22.5,5.65685387860011));
#450998=CARTESIAN_POINT('Ctrl Pts',(6.66798006829997,22.5,5.89851203167784));
#450999=CARTESIAN_POINT('Ctrl Pts',(6.7439998684947,22.5229375355598,5.57641995134461));
#451000=CARTESIAN_POINT('Ctrl Pts',(6.65366449057419,22.5458750711197,5.21379162224851));
#451001=CARTESIAN_POINT('Ctrl Pts',(6.43383171727969,22.5688126066795,4.96646199655034));
#451002=CARTESIAN_POINT('Ctrl Pts',(6.42033150900062,22.5702212297106,4.95127317183385));
#451003=CARTESIAN_POINT('Ctrl Pts',(6.40634292159547,22.5716298527418,4.93651917810251));
#451004=CARTESIAN_POINT('Ctrl Pts',(6.39190072013885,22.573038475773,4.9222125558517));
#451005=CARTESIAN_POINT('Origin',(5.65685387860011,26.,5.65685387860011));
#451006=CARTESIAN_POINT('',(6.39037461032892,23.0230384757729,4.92436540268704));
#451007=CARTESIAN_POINT('',(6.38930388760559,22.9019615242271,4.92349966353597));
#451008=CARTESIAN_POINT('',(6.39065394077645,26.,4.92305381642377));
#451009=CARTESIAN_POINT('',(5.77557608073439,22.5,4.62591736201901));
#451010=CARTESIAN_POINT('Ctrl Pts',(6.38930388760559,22.9019615242271,4.92349966353597));
#451011=CARTESIAN_POINT('Ctrl Pts',(6.54102880287524,22.8871128006417,5.07692511110986));
#451012=CARTESIAN_POINT('Ctrl Pts',(6.64766299899898,22.8722640770563,5.27640120658105));
#451013=CARTESIAN_POINT('Ctrl Pts',(6.68249361011691,22.8574153534709,5.48772889025785));
#451014=CARTESIAN_POINT('Ctrl Pts',(6.73838615923167,22.8335876632395,5.82684562005692));
#451015=CARTESIAN_POINT('Ctrl Pts',(6.60938089562333,22.8097599730081,6.19648078060475));
#451016=CARTESIAN_POINT('Ctrl Pts',(6.35472685290066,22.7859322827767,6.42720821100082));
#451017=CARTESIAN_POINT('Ctrl Pts',(6.10007281017799,22.7621045925453,6.65793564139689));
#451018=CARTESIAN_POINT('Ctrl Pts',(5.71976998834099,22.7382769023139,6.74975534164119));
#451019=CARTESIAN_POINT('Ctrl Pts',(5.38773213421059,22.7144492120825,6.66080060824128));
#451020=CARTESIAN_POINT('Ctrl Pts',(5.05569428008018,22.6906215218511,6.57184587484137));
#451021=CARTESIAN_POINT('Ctrl Pts',(4.77192139365638,22.6667938316197,6.30211670779724));
#451022=CARTESIAN_POINT('Ctrl Pts',(4.66700870222797,22.6429661413884,5.97477550103877));
#451023=CARTESIAN_POINT('Ctrl Pts',(4.56209601079956,22.619138451157,5.6474342942803));
#451024=CARTESIAN_POINT('Ctrl Pts',(4.63604351436656,22.5953107609256,5.26248104780748));
#451025=CARTESIAN_POINT('Ctrl Pts',(4.85366607828882,22.5714830706942,4.99722717517853));
#451026=CARTESIAN_POINT('Ctrl Pts',(5.07128864221107,22.5476553804628,4.73197330254958));
#451027=CARTESIAN_POINT('Ctrl Pts',(5.43258626648858,22.5238276902314,4.58641880376449));
#451028=CARTESIAN_POINT('Ctrl Pts',(5.77557608073438,22.5,4.625917362019));
#451029=CARTESIAN_POINT('Origin',(5.65685387860011,22.5,5.65685387860011));
#451030=CARTESIAN_POINT('Ctrl Pts',(6.39190072013885,22.573038475773,4.9222125558517));
#451031=CARTESIAN_POINT('Ctrl Pts',(6.16204455719575,22.5954575429732,4.69451421601594));
#451032=CARTESIAN_POINT('Ctrl Pts',(5.81728522517979,22.6178766101734,4.58013776446743));
#451033=CARTESIAN_POINT('Ctrl Pts',(5.49777863793003,22.6402956773736,4.62964039434809));
#451034=CARTESIAN_POINT('Ctrl Pts',(5.15819698094666,22.664123367605,4.68225334741615));
#451035=CARTESIAN_POINT('Ctrl Pts',(4.84714109570319,22.6879510578364,4.91998587117151));
#451036=CARTESIAN_POINT('Ctrl Pts',(4.70728537400252,22.7117787480678,5.23393572436938));
#451037=CARTESIAN_POINT('Ctrl Pts',(4.56742965230184,22.7356064382992,5.54788557756724));
#451038=CARTESIAN_POINT('Ctrl Pts',(4.59877409414395,22.7594341285306,5.93805276020761));
#451039=CARTESIAN_POINT('Ctrl Pts',(4.78686738296995,22.783261818762,6.22570363532513));
#451040=CARTESIAN_POINT('Ctrl Pts',(4.97496067179595,22.8070895089934,6.51335451044265));
#451041=CARTESIAN_POINT('Ctrl Pts',(5.31980280760584,22.8309171992248,6.69848907803731));
#451042=CARTESIAN_POINT('Ctrl Pts',(5.66347121722023,22.8547448894562,6.69629884619592));
#451043=CARTESIAN_POINT('Ctrl Pts',(6.00713962683461,22.8785725796876,6.69410861435454));
#451044=CARTESIAN_POINT('Ctrl Pts',(6.34963431025349,22.902400269919,6.5045935830771));
#451045=CARTESIAN_POINT('Ctrl Pts',(6.53403672593788,22.9262279601503,6.21456908983246));
#451046=CARTESIAN_POINT('Ctrl Pts',(6.71843914162228,22.9500556503817,5.92454459658782));
#451047=CARTESIAN_POINT('Ctrl Pts',(6.7447492895722,22.9738833406131,5.53401064137597));
#451048=CARTESIAN_POINT('Ctrl Pts',(6.60092695407667,22.9977110308445,5.22186823831327));
#451049=CARTESIAN_POINT('Ctrl Pts',(6.54996870275417,23.0061535124873,5.11127184889382));
#451050=CARTESIAN_POINT('Ctrl Pts',(6.47765230299322,23.0145959941301,5.01051660428821));
#451051=CARTESIAN_POINT('Ctrl Pts',(6.39037461032892,23.0230384757729,4.92436540268704));
#451052=CARTESIAN_POINT('Origin',(5.65685387860011,26.,5.65685387860011));
#451053=CARTESIAN_POINT('',(6.38935290488262,23.4730384757729,4.92330089590042));
#451054=CARTESIAN_POINT('',(6.39131103572319,23.3519615242271,4.92169609601798));
#451055=CARTESIAN_POINT('',(6.39065394077645,26.,4.92305381642377));
#451056=CARTESIAN_POINT('Ctrl Pts',(6.39131103572319,23.3519615242271,4.92169609601798));
#451057=CARTESIAN_POINT('Ctrl Pts',(6.61334324490838,23.33007894203,5.14636061012976));
#451058=CARTESIAN_POINT('Ctrl Pts',(6.72868171719176,23.308196359833,5.47994522249351));
#451059=CARTESIAN_POINT('Ctrl Pts',(6.6873844849522,23.286313777636,5.79285848911253));
#451060=CARTESIAN_POINT('Ctrl Pts',(6.64241640721998,23.2624860874046,6.1335861198444));
#451061=CARTESIAN_POINT('Ctrl Pts',(6.41172882390928,23.2386583971732,6.44980419113038));
#451062=CARTESIAN_POINT('Ctrl Pts',(6.10100080909856,23.2148307069418,6.59665364733223));
#451063=CARTESIAN_POINT('Ctrl Pts',(5.79027279428784,23.1910030167104,6.74350310353408));
#451064=CARTESIAN_POINT('Ctrl Pts',(5.39950434797711,23.167175326479,6.7209839446518));
#451065=CARTESIAN_POINT('Ctrl Pts',(5.10769854723491,23.1433476362476,6.539415444341));
#451066=CARTESIAN_POINT('Ctrl Pts',(4.8158927464927,23.1195199460162,6.3578469440302));
#451067=CARTESIAN_POINT('Ctrl Pts',(4.62304959131903,23.0956922557848,6.01722910229088));
#451068=CARTESIAN_POINT('Ctrl Pts',(4.61751951301592,23.0718645655534,5.67358993507176));
#451069=CARTESIAN_POINT('Ctrl Pts',(4.61198943471281,23.048036875322,5.32995076785264));
#451070=CARTESIAN_POINT('Ctrl Pts',(4.79377243328026,23.0242091850907,4.98329027515371));
#451071=CARTESIAN_POINT('Ctrl Pts',(5.07957475014376,23.0003814948593,4.7924243254548));
#451072=CARTESIAN_POINT('Ctrl Pts',(5.36537706700727,22.9765538046279,4.60155837575589));
#451073=CARTESIAN_POINT('Ctrl Pts',(5.75519870216683,22.9527261143965,4.566486969057));
#451074=CARTESIAN_POINT('Ctrl Pts',(6.07050470066555,22.9288984241651,4.70325041523272));
#451075=CARTESIAN_POINT('Ctrl Pts',(6.18932117076025,22.9199194575191,4.75478685916323));
#451076=CARTESIAN_POINT('Ctrl Pts',(6.29755640872372,22.9109404908731,4.83072387924101));
#451077=CARTESIAN_POINT('Ctrl Pts',(6.38930388760559,22.9019615242271,4.92349966353597));
#451078=CARTESIAN_POINT('Ctrl Pts',(6.39037461032892,23.0230384757729,4.92436540268704));
#451079=CARTESIAN_POINT('Ctrl Pts',(6.23132356780567,23.0384236843615,4.76736722811336));
#451080=CARTESIAN_POINT('Ctrl Pts',(6.02258634020352,23.0538088929501,4.65886881811934));
#451081=CARTESIAN_POINT('Ctrl Pts',(5.80287677492702,23.0691941015387,4.62769529041208));
#451082=CARTESIAN_POINT('Ctrl Pts',(5.46260375021388,23.0930217917701,4.57941559648715));
#451083=CARTESIAN_POINT('Ctrl Pts',(5.09601251972856,23.1168494820015,4.71660705955086));
#451084=CARTESIAN_POINT('Ctrl Pts',(4.87103919530453,23.1406771722329,4.97642324075838));
#451085=CARTESIAN_POINT('Ctrl Pts',(4.64606587088049,23.1645048624643,5.2362394219659));
#451086=CARTESIAN_POINT('Ctrl Pts',(4.56271045251773,23.1883325526957,5.61868032131723));
#451087=CARTESIAN_POINT('Ctrl Pts',(4.65915585483332,23.2121602429271,5.94855238336812));
#451088=CARTESIAN_POINT('Ctrl Pts',(4.75560125714891,23.2359879331585,6.278424445419));
#451089=CARTESIAN_POINT('Ctrl Pts',(5.03184748014285,23.2598156233899,6.55572767016945));
#451090=CARTESIAN_POINT('Ctrl Pts',(5.36134886181892,23.2836433136212,6.65343136663416));
#451091=CARTESIAN_POINT('Ctrl Pts',(5.690850243495,23.3074710038526,6.75113506309886));
#451092=CARTESIAN_POINT('Ctrl Pts',(6.07360678385322,23.331298694084,6.66923923127783));
#451093=CARTESIAN_POINT('Ctrl Pts',(6.33427992409048,23.3551263843154,6.44525978436571));
#451094=CARTESIAN_POINT('Ctrl Pts',(6.59495306432775,23.3789540745468,6.22128033745359));
#451095=CARTESIAN_POINT('Ctrl Pts',(6.73354280444407,23.4027817647782,5.85521727545038));
#451096=CARTESIAN_POINT('Ctrl Pts',(6.6865623548039,23.4266094550096,5.51476156795534));
#451097=CARTESIAN_POINT('Ctrl Pts',(6.65604804910002,23.442085795264,5.29363193601897));
#451098=CARTESIAN_POINT('Ctrl Pts',(6.54724832815155,23.4575621355185,5.08330512959901));
#451099=CARTESIAN_POINT('Ctrl Pts',(6.38935290488262,23.4730384757729,4.92330089590042));
#451100=CARTESIAN_POINT('Origin',(5.65685387860011,26.,5.65685387860011));
#451101=CARTESIAN_POINT('',(6.39152331859132,23.9230384757729,4.92169483493571));
#451102=CARTESIAN_POINT('',(6.39146732321148,23.8019615242271,4.92356615355223));
#451103=CARTESIAN_POINT('',(6.39065394077645,26.,4.92305381642377));
#451104=CARTESIAN_POINT('Ctrl Pts',(6.39146732321148,23.8019615242271,4.92356615355223));
#451105=CARTESIAN_POINT('Ctrl Pts',(6.44404636753914,23.7968727736498,4.97518123721477));
#451106=CARTESIAN_POINT('Ctrl Pts',(6.49097569651667,23.7917840230725,5.03225965778749));
#451107=CARTESIAN_POINT('Ctrl Pts',(6.53072214720976,23.7866952724952,5.09396482100832));
#451108=CARTESIAN_POINT('Ctrl Pts',(6.71683190058211,23.7628675822638,5.38289458727869));
#451109=CARTESIAN_POINT('Ctrl Pts',(6.74545633697037,23.7390398920324,5.77326614382955));
#451110=CARTESIAN_POINT('Ctrl Pts',(6.60348277515141,23.715212201801,6.08625298439034));
#451111=CARTESIAN_POINT('Ctrl Pts',(6.46150921333244,23.6913845115696,6.39923982495114));
#451112=CARTESIAN_POINT('Ctrl Pts',(6.14893765330626,23.6675568213382,6.63484194952187));
#451113=CARTESIAN_POINT('Ctrl Pts',(5.80895502137127,23.6437291311068,6.68513161677842));
#451114=CARTESIAN_POINT('Ctrl Pts',(5.4689723894363,23.6199014408755,6.73542128403497));
#451115=CARTESIAN_POINT('Ctrl Pts',(5.10157868559252,23.5960737506441,6.60039849397735));
#451116=CARTESIAN_POINT('Ctrl Pts',(4.87507434314934,23.5722460604127,6.34191631672375));
#451117=CARTESIAN_POINT('Ctrl Pts',(4.64857000070616,23.5484183701813,6.08343413947014));
#451118=CARTESIAN_POINT('Ctrl Pts',(4.56295501966359,23.5245906799499,5.70149257502055));
#451119=CARTESIAN_POINT('Ctrl Pts',(4.65744921450722,23.5007629897185,5.37105630657982));
#451120=CARTESIAN_POINT('Ctrl Pts',(4.75194340935084,23.4769352994871,5.0406200381391));
#451121=CARTESIAN_POINT('Ctrl Pts',(5.02654678008064,23.4531076092557,4.76168906570723));
#451122=CARTESIAN_POINT('Ctrl Pts',(5.35546505814245,23.4292799190243,4.66203997694959));
#451123=CARTESIAN_POINT('Ctrl Pts',(5.68438333620426,23.4054522287929,4.56239088819196));
#451124=CARTESIAN_POINT('Ctrl Pts',(6.06761652159808,23.3816245385615,4.64202368310855));
#451125=CARTESIAN_POINT('Ctrl Pts',(6.32960882821811,23.3577968483301,4.86445867565572));
#451126=CARTESIAN_POINT('Ctrl Pts',(6.350995850443,23.3558517402958,4.88261654521522));
#451127=CARTESIAN_POINT('Ctrl Pts',(6.37157494470415,23.3539066322614,4.90172602358781));
#451128=CARTESIAN_POINT('Ctrl Pts',(6.39131103572319,23.3519615242271,4.92169609601798));
#451129=CARTESIAN_POINT('Ctrl Pts',(6.38935290488262,23.4730384757729,4.92330089590042));
#451130=CARTESIAN_POINT('Ctrl Pts',(6.30414930262285,23.4813898257499,4.83695933636888));
#451131=CARTESIAN_POINT('Ctrl Pts',(6.20464951053553,23.4897411757268,4.76527121936352));
#451132=CARTESIAN_POINT('Ctrl Pts',(6.09544017298549,23.4980925257038,4.71444637045848));
#451133=CARTESIAN_POINT('Ctrl Pts',(5.78384908020389,23.5219202159352,4.56943523344352));
#451134=CARTESIAN_POINT('Ctrl Pts',(5.39321753403733,23.5457479061666,4.59426131240048));
#451135=CARTESIAN_POINT('Ctrl Pts',(5.10249121190879,23.569575596398,4.77755195197114));
#451136=CARTESIAN_POINT('Ctrl Pts',(4.81176488978025,23.5934032866293,4.9608425915418));
#451137=CARTESIAN_POINT('Ctrl Pts',(4.62094379168974,23.6172309768607,5.30259779172617));
#451138=CARTESIAN_POINT('Ctrl Pts',(4.61744171997954,23.6410586670921,5.64626184853499));
#451139=CARTESIAN_POINT('Ctrl Pts',(4.61393964826934,23.6648863573235,5.98992590534381));
#451140=CARTESIAN_POINT('Ctrl Pts',(4.79775660293946,23.6887140475549,6.33549881877709));
#451141=CARTESIAN_POINT('Ctrl Pts',(5.08468731748426,23.7125417377863,6.52467601704459));
#451142=CARTESIAN_POINT('Ctrl Pts',(5.37161803202905,23.7363694280177,6.71385321531209));
#451143=CARTESIAN_POINT('Ctrl Pts',(5.76166250644851,23.7601971182491,6.74663469841383));
#451144=CARTESIAN_POINT('Ctrl Pts',(6.07614404554655,23.7840248084805,6.60800349462427));
#451145=CARTESIAN_POINT('Ctrl Pts',(6.39062558464459,23.8078524987119,6.46937229083472));
#451146=CARTESIAN_POINT('Ctrl Pts',(6.6295441884212,23.8316801889433,6.15932840015388));
#451147=CARTESIAN_POINT('Ctrl Pts',(6.6834528935629,23.8555078791747,5.81990079386588));
#451148=CARTESIAN_POINT('Ctrl Pts',(6.73438085433327,23.8780180780408,5.49924097144978));
#451149=CARTESIAN_POINT('Ctrl Pts',(6.62019259508592,23.9005282769068,5.15235699515366));
#451150=CARTESIAN_POINT('Ctrl Pts',(6.39152331859132,23.9230384757729,4.92169483493571));
#451151=CARTESIAN_POINT('Origin',(5.65685387860011,26.,5.65685387860011));
#451152=CARTESIAN_POINT('',(6.39128196913613,24.3730384757729,4.92377157353716));
#451153=CARTESIAN_POINT('',(6.38942086037359,24.2519615242271,4.92421628016771));
#451154=CARTESIAN_POINT('',(6.39065394077645,26.,4.92305381642377));
#451155=CARTESIAN_POINT('Ctrl Pts',(6.38942086037359,24.2519615242271,4.92421628016771));
#451156=CARTESIAN_POINT('Ctrl Pts',(6.51405309196749,24.2398389150381,5.04895543667044));
#451157=CARTESIAN_POINT('Ctrl Pts',(6.60860369693141,24.2277163058492,5.20382475542584));
#451158=CARTESIAN_POINT('Ctrl Pts',(6.65652287894995,24.2155936966603,5.37198243345446));
#451159=CARTESIAN_POINT('Ctrl Pts',(6.75071080561528,24.1917660064289,5.70250608555364));
#451160=CARTESIAN_POINT('Ctrl Pts',(6.66474206054895,24.1679383161975,6.08436822205294));
#451161=CARTESIAN_POINT('Ctrl Pts',(6.4379983333991,24.1441106259661,6.34264042812557));
#451162=CARTESIAN_POINT('Ctrl Pts',(6.21125460624925,24.1202829357347,6.60091263419821));
#451163=CARTESIAN_POINT('Ctrl Pts',(5.84373589701588,24.0964552455033,6.73559490984418));
#451164=CARTESIAN_POINT('Ctrl Pts',(5.50379999638241,24.0726275552719,6.68499023152592));
#451165=CARTESIAN_POINT('Ctrl Pts',(5.16386409574894,24.0487998650405,6.63438555320766));
#451166=CARTESIAN_POINT('Ctrl Pts',(4.85151100371537,24.0249721748091,6.39849392092517));
#451167=CARTESIAN_POINT('Ctrl Pts',(4.70982751913656,24.0011444845777,6.08537566804496));
#451168=CARTESIAN_POINT('Ctrl Pts',(4.56814403455774,23.9773167943464,5.77225741516475));
#451169=CARTESIAN_POINT('Ctrl Pts',(4.59713015743369,23.9534891041149,5.38191254168682));
#451170=CARTESIAN_POINT('Ctrl Pts',(4.78350754767415,23.9296614138835,5.09315534403941));
#451171=CARTESIAN_POINT('Ctrl Pts',(4.96988493791459,23.9058337236522,4.804398146392));
#451172=CARTESIAN_POINT('Ctrl Pts',(5.31365359551954,23.8820060334208,4.61722862457511));
#451173=CARTESIAN_POINT('Ctrl Pts',(5.65733545950024,23.8581783431894,4.6173878516616));
#451174=CARTESIAN_POINT('Ctrl Pts',(5.92761905169082,23.8394394035353,4.61751307348277));
#451175=CARTESIAN_POINT('Ctrl Pts',(6.19784896370209,23.8207004638812,4.73349750638545));
#451176=CARTESIAN_POINT('Ctrl Pts',(6.39146732321148,23.8019615242271,4.92356615355223));
#451177=CARTESIAN_POINT('Ctrl Pts',(6.39152331859132,23.9230384757729,4.92169483493571));
#451178=CARTESIAN_POINT('Ctrl Pts',(6.37813961642664,23.9243559671382,4.90819449199352));
#451179=CARTESIAN_POINT('Ctrl Pts',(6.3643637478711,23.9256734585035,4.895092278726));
#451180=CARTESIAN_POINT('Ctrl Pts',(6.35020586507153,23.9269909498688,4.88241675495565));
#451181=CARTESIAN_POINT('Ctrl Pts',(6.09415132493169,23.9508186401002,4.65317164422858));
#451182=CARTESIAN_POINT('Ctrl Pts',(5.71314343814525,23.9746463303316,4.56349274466962));
#451183=CARTESIAN_POINT('Ctrl Pts',(5.38171929489583,23.998474020563,4.6544613426263));
#451184=CARTESIAN_POINT('Ctrl Pts',(5.05029515164641,24.0223017107944,4.74542994058297));
#451185=CARTESIAN_POINT('Ctrl Pts',(4.768454751934,24.0461294010258,5.01704603605528));
#451186=CARTESIAN_POINT('Ctrl Pts',(4.6653072414873,24.0699570912572,5.34488416612327));
#451187=CARTESIAN_POINT('Ctrl Pts',(4.56215973104059,24.0937847814886,5.67272229619127));
#451188=CARTESIAN_POINT('Ctrl Pts',(4.63770510985958,24.11761247172,6.05678246085496));
#451189=CARTESIAN_POINT('Ctrl Pts',(4.8573365604447,24.1414401619514,6.32112934350159));
#451190=CARTESIAN_POINT('Ctrl Pts',(5.07696801102981,24.1652678521828,6.58547622614821));
#451191=CARTESIAN_POINT('Ctrl Pts',(5.44068553338104,24.1890955424141,6.73010982677778));
#451192=CARTESIAN_POINT('Ctrl Pts',(5.78187263496817,24.2129232326455,6.68877448884912));
#451193=CARTESIAN_POINT('Ctrl Pts',(6.12305973655531,24.2367509228769,6.64743915092045));
#451194=CARTESIAN_POINT('Ctrl Pts',(6.44171641737836,24.2605786131083,6.42013487443355));
#451195=CARTESIAN_POINT('Ctrl Pts',(6.59186824658804,24.2844063033397,6.11098818332588));
#451196=CARTESIAN_POINT('Ctrl Pts',(6.74202007579772,24.3082339935711,5.80184149221821));
#451197=CARTESIAN_POINT('Ctrl Pts',(6.72366705339403,24.3320616838025,5.41085238648978));
#451198=CARTESIAN_POINT('Ctrl Pts',(6.54521657215205,24.3558893740339,5.11713028264445));
#451199=CARTESIAN_POINT('Ctrl Pts',(6.50240552012982,24.3616057412803,5.04666506349635));
#451200=CARTESIAN_POINT('Ctrl Pts',(6.45038020112141,24.3673221085266,4.98179796021343));
#451201=CARTESIAN_POINT('Ctrl Pts',(6.39128196913613,24.3730384757729,4.92377157353716));
#451202=CARTESIAN_POINT('Origin',(5.65685387860011,26.,5.65685387860011));
#451203=CARTESIAN_POINT('',(6.38933869113556,24.8230384757729,4.92408802232565));
#451204=CARTESIAN_POINT('',(6.39028821611916,24.7019615242271,4.92212745780798));
#451205=CARTESIAN_POINT('',(6.39065394077645,26.,4.92305381642377));
#451206=CARTESIAN_POINT('Ctrl Pts',(6.39028821611916,24.7019615242271,4.92212745780798));
#451207=CARTESIAN_POINT('Ctrl Pts',(6.5845155347103,24.6828050564265,5.11995795053563));
#451208=CARTESIAN_POINT('Ctrl Pts',(6.70087353526984,24.6636485886259,5.39828521249021));
#451209=CARTESIAN_POINT('Ctrl Pts',(6.69616935490973,24.6444921208254,5.67455106061111));
#451210=CARTESIAN_POINT('Ctrl Pts',(6.69031808036474,24.620664430594,6.01818314973456));
#451211=CARTESIAN_POINT('Ctrl Pts',(6.49716519325233,24.5968367403626,6.35862591802898));
#451212=CARTESIAN_POINT('Ctrl Pts',(6.20519269912468,24.5730090501312,6.53992487743046));
#451213=CARTESIAN_POINT('Ctrl Pts',(5.91322020499702,24.5491813598998,6.72122383683194));
#451214=CARTESIAN_POINT('Ctrl Pts',(5.52242810385412,24.5253536696684,6.74337898734048));
#451215=CARTESIAN_POINT('Ctrl Pts',(5.21183556708661,24.501525979437,6.59624120723028));
#451216=CARTESIAN_POINT('Ctrl Pts',(4.90124303031911,24.4776982892056,6.44910342712008));
#451217=CARTESIAN_POINT('Ctrl Pts',(4.670850057927,24.4538705989742,6.13267271639114));
#451218=CARTESIAN_POINT('Ctrl Pts',(4.62619808347199,24.4300429087428,5.79190380451131));
#451219=CARTESIAN_POINT('Ctrl Pts',(4.58154610901698,24.4062152185114,5.45113489263147));
#451220=CARTESIAN_POINT('Ctrl Pts',(4.72263513249906,24.38238752828,5.08602777960075));
#451221=CARTESIAN_POINT('Ctrl Pts',(4.98483324415836,24.3585598380486,4.86383551964991));
#451222=CARTESIAN_POINT('Ctrl Pts',(5.24703135581765,24.3347321478172,4.64164325969907));
#451223=CARTESIAN_POINT('Ctrl Pts',(5.63033855565415,24.3109044575858,4.56236585282811));
#451224=CARTESIAN_POINT('Ctrl Pts',(5.9591644547709,24.2870767673545,4.66231973324217));
#451225=CARTESIAN_POINT('Ctrl Pts',(6.12069642705376,24.275371686312,4.71142093690032));
#451226=CARTESIAN_POINT('Ctrl Pts',(6.26908122485669,24.2636666052695,4.80377340246064));
#451227=CARTESIAN_POINT('Ctrl Pts',(6.38942086037359,24.2519615242271,4.92421628016771));
#451228=CARTESIAN_POINT('Ctrl Pts',(6.39128196913613,24.3730384757729,4.92377157353716));
#451229=CARTESIAN_POINT('Ctrl Pts',(6.20403942134221,24.391149798758,4.7399249826062));
#451230=CARTESIAN_POINT('Ctrl Pts',(5.94579686164739,24.4092611217431,4.62474754709557));
#451231=CARTESIAN_POINT('Ctrl Pts',(5.68465923264326,24.4273724447281,4.61775970678068));
#451232=CARTESIAN_POINT('Ctrl Pts',(5.34110031445673,24.4512001349595,4.60856633672445));
#451233=CARTESIAN_POINT('Ctrl Pts',(4.99253041816395,24.4750278251909,4.7866346985742));
#451234=CARTESIAN_POINT('Ctrl Pts',(4.79862701145602,24.4988555154223,5.07039290068915));
#451235=CARTESIAN_POINT('Ctrl Pts',(4.60472360474809,24.5226832056536,5.35415110280411));
#451236=CARTESIAN_POINT('Ctrl Pts',(4.565486687625,24.546510895885,5.7435991451843));
#451237=CARTESIAN_POINT('Ctrl Pts',(4.69889042440694,24.5703385861164,6.06033356407531));
#451238=CARTESIAN_POINT('Ctrl Pts',(4.83229416118888,24.5941662763478,6.37706798296632));
#451239=CARTESIAN_POINT('Ctrl Pts',(5.13833855187584,24.6179939665792,6.62108877836816));
#451240=CARTESIAN_POINT('Ctrl Pts',(5.47682676316715,24.6418216568106,6.68061169925028));
#451241=CARTESIAN_POINT('Ctrl Pts',(5.81531497445846,24.665649347042,6.74013462013239));
#451242=CARTESIAN_POINT('Ctrl Pts',(6.18624700635411,24.6894770372734,6.61515966649478));
#451243=CARTESIAN_POINT('Ctrl Pts',(6.41970146010492,24.7133047275048,6.36293701391879));
#451244=CARTESIAN_POINT('Ctrl Pts',(6.65315591385573,24.7371324177362,6.1107143613428));
#451245=CARTESIAN_POINT('Ctrl Pts',(6.7491327894617,24.7609601079676,5.73124400982843));
#451246=CARTESIAN_POINT('Ctrl Pts',(6.6636657201663,24.784787798199,5.3983586947443));
#451247=CARTESIAN_POINT('Ctrl Pts',(6.61793218802977,24.797538024057,5.22023136007979));
#451248=CARTESIAN_POINT('Ctrl Pts',(6.5202452116208,24.8102882499149,5.05544287282308));
#451249=CARTESIAN_POINT('Ctrl Pts',(6.38933869113556,24.8230384757729,4.92408802232565));
#451250=CARTESIAN_POINT('Origin',(5.65685387860011,26.,5.65685387860011));
#451251=CARTESIAN_POINT('',(6.39051881327128,25.2730384757729,4.92197603118329));
#451252=CARTESIAN_POINT('',(6.39198798715975,25.151961524227,4.92254817630007));
#451253=CARTESIAN_POINT('',(6.39065394077645,26.,4.92305381642377));
#451254=CARTESIAN_POINT('Ctrl Pts',(6.39198798715975,25.151961524227,4.92254817630007));
#451255=CARTESIAN_POINT('Ctrl Pts',(6.41627314991443,25.1495988880462,4.94650751599249));
#451256=CARTESIAN_POINT('Ctrl Pts',(6.43929566708608,25.1472362518654,4.97169983154625));
#451257=CARTESIAN_POINT('Ctrl Pts',(6.46089355482011,25.1448736156846,4.99805942366946));
#451258=CARTESIAN_POINT('Ctrl Pts',(6.67871286308055,25.1210459254532,5.26390153716753));
#451259=CARTESIAN_POINT('Ctrl Pts',(6.75163093056004,25.0972182352218,5.64846913729549));
#451260=CARTESIAN_POINT('Ctrl Pts',(6.64624470558553,25.0733905449904,5.97559449046916));
#451261=CARTESIAN_POINT('Ctrl Pts',(6.54085848061101,25.049562854759,6.30271984364283));
#451262=CARTESIAN_POINT('Ctrl Pts',(6.25716796318248,25.0257351645276,6.57240294986222));
#451263=CARTESIAN_POINT('Ctrl Pts',(5.92512971718013,25.0019074742962,6.66110381706143));
#451264=CARTESIAN_POINT('Ctrl Pts',(5.59309147117778,24.9780797840648,6.74980468426065));
#451265=CARTESIAN_POINT('Ctrl Pts',(5.2127054966016,24.9542520938335,6.65752331243968));
#451266=CARTESIAN_POINT('Ctrl Pts',(4.9582240442926,24.9304244036021,6.42653317184816));
#451267=CARTESIAN_POINT('Ctrl Pts',(4.7037425919836,24.9065967133707,6.19554303125664));
#451268=CARTESIAN_POINT('Ctrl Pts',(4.57516566194178,24.8827690231393,5.82584412189456));
#451269=CARTESIAN_POINT('Ctrl Pts',(4.63139343216518,24.8589413329079,5.48679296352304));
#451270=CARTESIAN_POINT('Ctrl Pts',(4.68762120238858,24.8351136426765,5.14774180515151));
#451271=CARTESIAN_POINT('Ctrl Pts',(4.9286536728772,24.8112859524451,4.83933839777055));
#451272=CARTESIAN_POINT('Ctrl Pts',(5.24407554312886,24.7874582622137,4.70286022094558));
#451273=CARTESIAN_POINT('Ctrl Pts',(5.55949741338051,24.7636305719823,4.56638204412062));
#451274=CARTESIAN_POINT('Ctrl Pts',(5.94930868339519,24.7398028817509,4.60182909785165));
#451275=CARTESIAN_POINT('Ctrl Pts',(6.23493948741374,24.7159751915195,4.79296332969341));
#451276=CARTESIAN_POINT('Ctrl Pts',(6.29093505415592,24.7113039690887,4.83043362171106));
#451277=CARTESIAN_POINT('Ctrl Pts',(6.34292671833546,24.7066327466579,4.87388734148021));
#451278=CARTESIAN_POINT('Ctrl Pts',(6.39028821611916,24.7019615242271,4.92212745780798));
#451279=CARTESIAN_POINT('Ctrl Pts',(6.38933869113556,24.8230384757729,4.92408802232565));
#451280=CARTESIAN_POINT('Ctrl Pts',(6.27560640646284,24.8341159401463,4.80996622614209));
#451281=CARTESIAN_POINT('Ctrl Pts',(6.13679925493306,24.8451934045197,4.72108089883846));
#451282=CARTESIAN_POINT('Ctrl Pts',(5.98520281626299,24.8562708688931,4.67061008310121));
#451283=CARTESIAN_POINT('Ctrl Pts',(5.65911799585187,24.8800985591245,4.56204706519615));
#451284=CARTESIAN_POINT('Ctrl Pts',(5.27385936922642,24.9039262493559,4.63122130803993));
#451285=CARTESIAN_POINT('Ctrl Pts',(5.00591117956891,24.9277539395873,4.84644449237099));
#451286=CARTESIAN_POINT('Ctrl Pts',(4.7379629899114,24.9515816298187,5.06166767670205));
#451287=CARTESIAN_POINT('Ctrl Pts',(4.58732523722183,24.9754093200501,5.42293980252039));
#451288=CARTESIAN_POINT('Ctrl Pts',(4.62300419682159,24.9992370102815,5.7647647438604));
#451289=CARTESIAN_POINT('Ctrl Pts',(4.65868315642135,25.0230647005129,6.10658968520039));
#451290=CARTESIAN_POINT('Ctrl Pts',(4.88067882831044,25.0468923907443,6.42896744206205));
#451291=CARTESIAN_POINT('Ctrl Pts',(5.18729621377842,25.0707200809757,6.58421869570625));
#451292=CARTESIAN_POINT('Ctrl Pts',(5.49391359924639,25.0945477712071,6.73946994935045));
#451293=CARTESIAN_POINT('Ctrl Pts',(5.88515269829325,25.1183754614385,6.72759469977719));
#451294=CARTESIAN_POINT('Ctrl Pts',(6.18179018209155,25.1422031516699,6.5540334824637));
#451295=CARTESIAN_POINT('Ctrl Pts',(6.47842766588984,25.1660308419013,6.38047226515022));
#451296=CARTESIAN_POINT('Ctrl Pts',(6.68046353443956,25.1898585321326,6.0452250800965));
#451297=CARTESIAN_POINT('Ctrl Pts',(6.69534535485932,25.213686222364,5.70186524531576));
#451298=CARTESIAN_POINT('Ctrl Pts',(6.70770170116848,25.2334703068337,5.41677424787487));
#451299=CARTESIAN_POINT('Ctrl Pts',(6.59103501365993,25.2532543913033,5.12609043162756));
#451300=CARTESIAN_POINT('Ctrl Pts',(6.39051881327128,25.2730384757729,4.92197603118329));
#451301=CARTESIAN_POINT('Origin',(5.65685387860011,26.,5.65685387860011));
#451302=CARTESIAN_POINT('',(6.39190058798136,25.7230384757729,4.92276701974739));
#451303=CARTESIAN_POINT('',(6.39006796800885,25.6019615242271,4.92443355077908));
#451304=CARTESIAN_POINT('',(6.39065394077645,26.,4.92305381642377));
#451305=CARTESIAN_POINT('',(5.59475217632209,26.,6.69274404704181));
#451306=CARTESIAN_POINT('Ctrl Pts',(6.39190058798136,25.7230384757729,4.92276701974739));
#451307=CARTESIAN_POINT('Ctrl Pts',(6.17742942344334,25.7438759131544,4.71160994855805));
#451308=CARTESIAN_POINT('Ctrl Pts',(5.86562000134797,25.764713350536,4.59523934827088));
#451309=CARTESIAN_POINT('Ctrl Pts',(5.56615422141076,25.7855507879175,4.62142687258513));
#451310=CARTESIAN_POINT('Ctrl Pts',(5.22371394391399,25.8093784781489,4.65137240791476));
#451311=CARTESIAN_POINT('Ctrl Pts',(4.89741422641509,25.8332061683802,4.86772710302321));
#451312=CARTESIAN_POINT('Ctrl Pts',(4.73725319022189,25.8570338586116,5.17187737628347));
#451313=CARTESIAN_POINT('Ctrl Pts',(4.57709215402869,25.880861548843,5.47602764954372));
#451314=CARTESIAN_POINT('Ctrl Pts',(4.58306979914119,25.9046892390744,5.86797350095578));
#451315=CARTESIAN_POINT('Ctrl Pts',(4.75132533448083,25.9285169293058,6.16698733288025));
#451316=CARTESIAN_POINT('Ctrl Pts',(4.91958086982048,25.9523446195372,6.46600116480472));
#451317=CARTESIAN_POINT('Ctrl Pts',(5.25011429538726,25.9761723097686,6.67208297724159));
#451318=CARTESIAN_POINT('Ctrl Pts',(5.59475217632212,26.,6.69274404704181));
#451319=CARTESIAN_POINT('',(6.69457727933146,26.,5.59444809180803));
#451320=CARTESIAN_POINT('Origin',(5.65685387860011,26.,5.65685387860011));
#451321=CARTESIAN_POINT('Ctrl Pts',(6.69458228414866,26.,5.59444726164187));
#451322=CARTESIAN_POINT('Ctrl Pts',(6.71351646533254,25.9770624644402,5.92484673178863));
#451323=CARTESIAN_POINT('Ctrl Pts',(6.56158375468957,25.9541249288804,6.26627937525033));
#451324=CARTESIAN_POINT('Ctrl Pts',(6.30214239804398,25.9311873933205,6.47167795527827));
#451325=CARTESIAN_POINT('Ctrl Pts',(6.03263270014108,25.9073597030892,6.68504759676004));
#451326=CARTESIAN_POINT('Ctrl Pts',(5.64710810132191,25.8835320128578,6.75161994353754));
#451327=CARTESIAN_POINT('Ctrl Pts',(5.32182159136527,25.8597043226264,6.64083855948586));
#451328=CARTESIAN_POINT('Ctrl Pts',(4.99653508140864,25.835876632395,6.53005717543419));
#451329=CARTESIAN_POINT('Ctrl Pts',(4.73148666031454,25.8120489421636,6.24192206055333));
#451330=CARTESIAN_POINT('Ctrl Pts',(4.64827248224482,25.7882212519322,5.90845611919747));
#451331=CARTESIAN_POINT('Ctrl Pts',(4.56505830417509,25.7643935617008,5.57499017784161));
#451332=CARTESIAN_POINT('Ctrl Pts',(4.66367836912974,25.7405658714694,5.19619341001074));
#451333=CARTESIAN_POINT('Ctrl Pts',(4.89886414913016,25.716738181238,4.94557465216384));
#451334=CARTESIAN_POINT('Ctrl Pts',(5.13404992913058,25.6929104910066,4.69495589431694));
#451335=CARTESIAN_POINT('Ctrl Pts',(5.50580142417677,25.6690828007752,4.572515146454));
#451336=CARTESIAN_POINT('Ctrl Pts',(5.84386841174159,25.6452551105438,4.63434949773116));
#451337=CARTESIAN_POINT('Ctrl Pts',(6.04861804217652,25.6308239151049,4.67179935541582));
#451338=CARTESIAN_POINT('Ctrl Pts',(6.24101187097706,25.616392719666,4.7768430935332));
#451339=CARTESIAN_POINT('Ctrl Pts',(6.39006796800885,25.6019615242271,4.92443355077908));
#451340=CARTESIAN_POINT('Origin',(5.65685387860011,26.993675081176,5.65685387860011));
#451341=CARTESIAN_POINT('',(6.5673434103921,22.756324918824,4.74524035180398));
#451342=CARTESIAN_POINT('',(6.57057146528765,22.718675081176,4.74364038176039));
#451343=CARTESIAN_POINT('',(6.56902162633079,26.993675081176,4.74468613086949));
#451344=CARTESIAN_POINT('',(4.8286920333622,22.5,6.64591806159944));
#451345=CARTESIAN_POINT('Ctrl Pts',(6.57057146528766,22.718675081176,4.74364038176039));
#451346=CARTESIAN_POINT('Ctrl Pts',(6.58852418981576,22.7172664581449,4.76142457130848));
#451347=CARTESIAN_POINT('Ctrl Pts',(6.9000556810006,22.6920301448823,5.09000197050781));
#451348=CARTESIAN_POINT('Ctrl Pts',(7.12689194633153,22.6429661413884,6.06611679986992));
#451349=CARTESIAN_POINT('Ctrl Pts',(6.10694434613243,22.5714830706942,7.11331947438321));
#451350=CARTESIAN_POINT('Ctrl Pts',(5.15775103452081,22.5238276902314,6.92144528650133));
#451351=CARTESIAN_POINT('Ctrl Pts',(4.8286920333622,22.5,6.64591806159944));
#451352=CARTESIAN_POINT('',(4.44194770692244,22.5,6.09734856608929));
#451353=CARTESIAN_POINT('Origin',(5.65685387860011,22.5,5.65685387860011));
#451354=CARTESIAN_POINT('Ctrl Pts',(6.5673434103921,22.756324918824,4.74524035180399));
#451355=CARTESIAN_POINT('Ctrl Pts',(6.75594870135602,22.7414761952386,4.93595953019022));
#451356=CARTESIAN_POINT('Ctrl Pts',(7.10121210146151,22.7027997814218,5.58182921801751));
#451357=CARTESIAN_POINT('Ctrl Pts',(6.68055232418451,22.6402956773736,6.78713386963137));
#451358=CARTESIAN_POINT('Ctrl Pts',(5.27997950888059,22.5697027613511,7.12528591239124));
#451359=CARTESIAN_POINT('Ctrl Pts',(4.58325719964657,22.5229375355598,6.48370144903283));
#451360=CARTESIAN_POINT('Ctrl Pts',(4.44194158662797,22.5,6.09735008669022));
#451361=CARTESIAN_POINT('Origin',(5.65685387860011,26.993675081176,5.65685387860011));
#451362=CARTESIAN_POINT('',(6.56983844394705,23.206324918824,4.74299838399068));
#451363=CARTESIAN_POINT('',(6.56867439792569,23.168675081176,4.74631652959707));
#451364=CARTESIAN_POINT('',(6.56902162633079,26.993675081176,4.74468613086949));
#451365=CARTESIAN_POINT('Ctrl Pts',(6.56867439792569,23.168675081176,4.74631652959707));
#451366=CARTESIAN_POINT('Ctrl Pts',(6.67716702479821,23.1602325995332,4.853408844765));
#451367=CARTESIAN_POINT('Ctrl Pts',(7.02077633180239,23.127962427659,5.33214451040115));
#451368=CARTESIAN_POINT('Ctrl Pts',(6.94377741359718,23.0718645655535,6.47507582842176));
#451369=CARTESIAN_POINT('Ctrl Pts',(5.66653874837814,23.0003814948592,7.18181942856023));
#451370=CARTESIAN_POINT('Ctrl Pts',(4.38054591235378,22.9288984241651,6.49141154940691));
#451371=CARTESIAN_POINT('Ctrl Pts',(4.26365553420012,22.8574153534709,5.03639155729104));
#451372=CARTESIAN_POINT('Ctrl Pts',(5.40079341912851,22.7873409058079,4.16730445086878));
#451373=CARTESIAN_POINT('Ctrl Pts',(6.28484325502835,22.7410941483762,4.46059450521194));
#451374=CARTESIAN_POINT('Ctrl Pts',(6.57057146528766,22.718675081176,4.74364038176039));
#451375=CARTESIAN_POINT('Ctrl Pts',(6.56983844394705,23.206324918824,4.74299838399068));
#451376=CARTESIAN_POINT('Ctrl Pts',(6.84584090104065,23.184442336627,5.02227299078826));
#451377=CARTESIAN_POINT('Ctrl Pts',(7.14533371342118,23.1387320641985,5.88847306909541));
#451378=CARTESIAN_POINT('Ctrl Pts',(6.30845753745629,23.0691941015387,7.03563221165043));
#451379=CARTESIAN_POINT('Ctrl Pts',(4.85119529970875,22.9977110308445,6.95165327175697));
#451380=CARTESIAN_POINT('Ctrl Pts',(4.13204038713623,22.9262279601503,5.68141376558384));
#451381=CARTESIAN_POINT('Ctrl Pts',(4.80994952176022,22.8547448894562,4.38863987327371));
#451382=CARTESIAN_POINT('Ctrl Pts',(5.9617065202947,22.7981105423474,4.28501879514303));
#451383=CARTESIAN_POINT('Ctrl Pts',(6.45329450867431,22.76530388547,4.62991319040622));
#451384=CARTESIAN_POINT('Ctrl Pts',(6.5673434103921,22.756324918824,4.74524035180399));
#451385=CARTESIAN_POINT('Origin',(5.65685387860011,26.993675081176,5.65685387860011));
#451386=CARTESIAN_POINT('',(6.57003272085371,23.656324918824,4.74532300381163));
#451387=CARTESIAN_POINT('',(6.56740434249263,23.618675081176,4.74499326893249));
#451388=CARTESIAN_POINT('',(6.56902162633079,26.993675081176,4.74468613086949));
#451389=CARTESIAN_POINT('Ctrl Pts',(6.56740434249263,23.618675081176,4.74499326893249));
#451390=CARTESIAN_POINT('Ctrl Pts',(6.76368003125862,23.6031987409216,4.94389036502613));
#451391=CARTESIAN_POINT('Ctrl Pts',(7.10715379447204,23.5638947104357,5.60787864620878));
#451392=CARTESIAN_POINT('Ctrl Pts',(6.65070324968042,23.5007629897185,6.81352117024561));
#451393=CARTESIAN_POINT('Ctrl Pts',(5.22331918686542,23.4292799190243,7.11892889768229));
#451394=CARTESIAN_POINT('Ctrl Pts',(4.19313572939823,23.3577968483302,6.08480364614363));
#451395=CARTESIAN_POINT('Ctrl Pts',(4.50398657889369,23.2863137776359,4.65859667867589));
#451396=CARTESIAN_POINT('Ctrl Pts',(5.70962577012502,23.2232731885846,4.20740365817457));
#451397=CARTESIAN_POINT('Ctrl Pts',(6.37096218895919,23.1840602897646,4.55115618731809));
#451398=CARTESIAN_POINT('Ctrl Pts',(6.56867439792569,23.168675081176,4.74631652959707));
#451399=CARTESIAN_POINT('Ctrl Pts',(6.57003272085371,23.656324918824,4.74532300381163));
#451400=CARTESIAN_POINT('Ctrl Pts',(6.63539236159828,23.6512361682467,4.80948437015677));
#451401=CARTESIAN_POINT('Ctrl Pts',(6.9668858368575,23.622319727438,5.21266771861287));
#451402=CARTESIAN_POINT('Ctrl Pts',(7.04564953674368,23.569575596398,6.28682364983267));
#451403=CARTESIAN_POINT('Ctrl Pts',(5.88000083782648,23.4980925257038,7.16543624640093));
#451404=CARTESIAN_POINT('Ctrl Pts',(4.50990820099156,23.4266094550096,6.66190630419616));
#451405=CARTESIAN_POINT('Ctrl Pts',(4.19063094092434,23.3551263843154,5.23756146736659));
#451406=CARTESIAN_POINT('Ctrl Pts',(5.21468783779196,23.2836433136212,4.19736598356862));
#451407=CARTESIAN_POINT('Ctrl Pts',(6.20635078283888,23.2340428251241,4.40342562281452));
#451408=CARTESIAN_POINT('Ctrl Pts',(6.54530502316694,23.2082700268584,4.71817410701172));
#451409=CARTESIAN_POINT('Ctrl Pts',(6.56983844394705,23.206324918824,4.74299838399068));
#451410=CARTESIAN_POINT('Origin',(5.65685387860011,26.993675081176,5.65685387860011));
#451411=CARTESIAN_POINT('',(6.56748881619374,24.106324918824,4.74613115927677));
#451412=CARTESIAN_POINT('',(6.57010232725217,24.068675081176,4.74299681637215));
#451413=CARTESIAN_POINT('',(6.56902162633079,26.993675081176,4.74468613086949));
#451414=CARTESIAN_POINT('Ctrl Pts',(6.57010232725217,24.068675081176,4.74299681637215));
#451415=CARTESIAN_POINT('Ctrl Pts',(6.85435514987614,24.0461648823099,5.02972694085412));
#451416=CARTESIAN_POINT('Ctrl Pts',(7.14655186859909,23.9998269932124,5.91736950865738));
#451417=CARTESIAN_POINT('Ctrl Pts',(6.27199288310558,23.9296614138836,7.0522818436793));
#451418=CARTESIAN_POINT('Ctrl Pts',(4.81743049717126,23.8581783431894,6.93003241982605));
#451419=CARTESIAN_POINT('Ctrl Pts',(4.13193628895796,23.7866952724952,5.64131435190337));
#451420=CARTESIAN_POINT('Ctrl Pts',(4.84355050202496,23.715212201801,4.3668333837381));
#451421=CARTESIAN_POINT('Ctrl Pts',(5.98491025846011,23.6592054713613,4.29429575151249));
#451422=CARTESIAN_POINT('Ctrl Pts',(6.4614899633887,23.627026431153,4.63766432477859));
#451423=CARTESIAN_POINT('Ctrl Pts',(6.56740434249263,23.618675081176,4.74499326893249));
#451424=CARTESIAN_POINT('Ctrl Pts',(6.56748881619374,24.106324918824,4.74613115927677));
#451425=CARTESIAN_POINT('Ctrl Pts',(6.72241589762581,24.0942023096351,4.90119115627847));
#451426=CARTESIAN_POINT('Ctrl Pts',(7.07096798466868,24.0582520102147,5.47210261995128));
#451427=CARTESIAN_POINT('Ctrl Pts',(6.80286792203874,23.998474020563,6.662968703113));
#451428=CARTESIAN_POINT('Ctrl Pts',(5.43230911237055,23.9269909498688,7.16522879152533));
#451429=CARTESIAN_POINT('Ctrl Pts',(4.26747512907024,23.8555078791747,6.2855365564656));
#451430=CARTESIAN_POINT('Ctrl Pts',(4.37557081254884,23.7840248084805,4.82985391579145));
#451431=CARTESIAN_POINT('Ctrl Pts',(5.56629788826614,23.7176304883636,4.18154636230721));
#451432=CARTESIAN_POINT('Ctrl Pts',(6.32935078034095,23.6750638584781,4.50905361827065));
#451433=CARTESIAN_POINT('Ctrl Pts',(6.57003272085371,23.656324918824,4.74532300381163));
#451434=CARTESIAN_POINT('Origin',(5.65685387860011,26.993675081176,5.65685387860011));
#451435=CARTESIAN_POINT('',(6.56856700353347,24.556324918824,4.74353459859835));
#451436=CARTESIAN_POINT('',(6.56980231202958,24.518675081176,4.74557835604531));
#451437=CARTESIAN_POINT('',(6.56902162633079,26.993675081176,4.74468613086949));
#451438=CARTESIAN_POINT('Ctrl Pts',(6.56980231202958,24.518675081176,4.74557835604531));
#451439=CARTESIAN_POINT('Ctrl Pts',(6.64326578517921,24.5129587139297,4.81770944620421));
#451440=CARTESIAN_POINT('Ctrl Pts',(6.97750833641272,24.4834146564519,5.23445549419879));
#451441=CARTESIAN_POINT('Ctrl Pts',(7.0286098827299,24.4300429087428,6.32311258055822));
#451442=CARTESIAN_POINT('Ctrl Pts',(5.84026841822956,24.3585598380486,7.17078066054311));
#451443=CARTESIAN_POINT('Ctrl Pts',(4.4838850778304,24.2870767673545,6.63140987332417));
#451444=CARTESIAN_POINT('Ctrl Pts',(4.2021595986403,24.2155936966603,5.19916430623342));
#451445=CARTESIAN_POINT('Ctrl Pts',(5.25320498229437,24.1441106259661,4.18624762160046));
#451446=CARTESIAN_POINT('Ctrl Pts',(6.22663461042285,24.095137754138,4.41536649518845));
#451447=CARTESIAN_POINT('Ctrl Pts',(6.55346539562852,24.0699925725413,4.72621489163553));
#451448=CARTESIAN_POINT('Ctrl Pts',(6.57010232725217,24.068675081176,4.74299681637215));
#451449=CARTESIAN_POINT('Ctrl Pts',(6.56856700353347,24.556324918824,4.74353459859835));
#451450=CARTESIAN_POINT('Ctrl Pts',(6.81000592522228,24.5371684510234,4.9894525322227));
#451451=CARTESIAN_POINT('Ctrl Pts',(7.13455935910424,24.4941842929914,5.76578134653658));
#451452=CARTESIAN_POINT('Ctrl Pts',(6.46131966662841,24.4273724447281,6.95240396480877));
#451453=CARTESIAN_POINT('Ctrl Pts',(5.00396921476326,24.3558893740339,7.03502543671246));
#451454=CARTESIAN_POINT('Ctrl Pts',(4.14478270244581,24.2844063033397,5.85498510857851));
#451455=CARTESIAN_POINT('Ctrl Pts',(4.67093497503136,24.2129232326456,4.49341967622111));
#451456=CARTESIAN_POINT('Ctrl Pts',(5.85795834238072,24.1535627711403,4.24791389261248));
#451457=CARTESIAN_POINT('Ctrl Pts',(6.41789774915756,24.1180299998665,4.59641175456261));
#451458=CARTESIAN_POINT('Ctrl Pts',(6.56748881619374,24.106324918824,4.74613115927677));
#451459=CARTESIAN_POINT('Origin',(5.65685387860011,26.993675081176,5.65685387860011));
#451460=CARTESIAN_POINT('',(6.57067994464873,25.006324918824,4.74405758279954));
#451461=CARTESIAN_POINT('',(6.56738667375376,24.968675081176,4.74597172529336));
#451462=CARTESIAN_POINT('',(6.56902162633079,26.993675081176,4.74468613086949));
#451463=CARTESIAN_POINT('Ctrl Pts',(6.56738667375376,24.968675081176,4.74597172529336));
#451464=CARTESIAN_POINT('Ctrl Pts',(6.73011316031215,24.955924855318,4.90925551921452));
#451465=CARTESIAN_POINT('Ctrl Pts',(7.07847832230359,24.9193469392286,5.49691387622178));
#451466=CARTESIAN_POINT('Ctrl Pts',(6.77602463836695,24.8589413329079,6.69274573713214));
#451467=CARTESIAN_POINT('Ctrl Pts',(5.39273679116275,24.7874582622137,7.15880506797054));
#451468=CARTESIAN_POINT('Ctrl Pts',(4.25142935492228,24.7159751915195,6.24879737998678));
#451469=CARTESIAN_POINT('Ctrl Pts',(4.39775252453571,24.6444921208253,4.79645922145989));
#451470=CARTESIAN_POINT('Ctrl Pts',(5.59369688000734,24.5787254173775,4.18550614000559));
#451471=CARTESIAN_POINT('Ctrl Pts',(6.33704597702196,24.5367864041611,4.51704344657683));
#451472=CARTESIAN_POINT('Ctrl Pts',(6.56980231202958,24.518675081176,4.74557835604531));
#451473=CARTESIAN_POINT('Ctrl Pts',(6.57067994464873,25.006324918824,4.74405758279954));
#451474=CARTESIAN_POINT('Ctrl Pts',(6.60086819803686,25.0039622826432,4.77384081402403));
#451475=CARTESIAN_POINT('Ctrl Pts',(6.918112503001,24.9777719562309,5.12098437694123));
#451476=CARTESIAN_POINT('Ctrl Pts',(7.10838527255517,24.9277539395874,6.12447699388039));
#451477=CARTESIAN_POINT('Ctrl Pts',(6.05044038944422,24.8562708688931,7.13018513270865));
#451478=CARTESIAN_POINT('Ctrl Pts',(4.63189669239788,24.784787798199,6.78604742232837));
#451479=CARTESIAN_POINT('Ctrl Pts',(4.15240479236238,24.7133047275048,5.40735816264999));
#451480=CARTESIAN_POINT('Ctrl Pts',(5.0512683537124,24.6418216568106,4.25725342975252));
#451481=CARTESIAN_POINT('Ctrl Pts',(6.11539165852711,24.589495053917,4.35401829743014));
#451482=CARTESIAN_POINT('Ctrl Pts',(6.50969315902277,24.5609961412548,4.68356856625642));
#451483=CARTESIAN_POINT('Ctrl Pts',(6.56856700353347,24.556324918824,4.74353459859835));
#451484=CARTESIAN_POINT('Origin',(5.65685387860011,26.993675081176,5.65685387860011));
#451485=CARTESIAN_POINT('',(6.56829321884323,25.456324918824,4.74640124271564));
#451486=CARTESIAN_POINT('',(6.56885365284802,25.418675081176,4.74334636410459));
#451487=CARTESIAN_POINT('',(6.56902162633079,26.993675081176,4.74468613086949));
#451488=CARTESIAN_POINT('Ctrl Pts',(6.56885365284802,25.418675081176,4.74334636410459));
#451489=CARTESIAN_POINT('Ctrl Pts',(6.81811011972481,25.3988909967064,4.99707565976646));
#451490=CARTESIAN_POINT('Ctrl Pts',(7.13780202337966,25.3552792220053,5.79361205385018));
#451491=CARTESIAN_POINT('Ctrl Pts',(6.42698533143036,25.287839757073,6.97310209577086));
#451492=CARTESIAN_POINT('Ctrl Pts',(4.96796792520407,25.2163566863788,7.01738753624157));
#451493=CARTESIAN_POINT('Ctrl Pts',(4.14009680960707,25.1448736156846,5.81516935358237));
#451494=CARTESIAN_POINT('Ctrl Pts',(4.70185841202445,25.0733905449904,4.4679054394248));
#451495=CARTESIAN_POINT('Ctrl Pts',(5.88231068328695,25.0146577001542,4.25595199715398));
#451496=CARTESIAN_POINT('Ctrl Pts',(6.4260090324839,24.9797525455494,4.604109892408));
#451497=CARTESIAN_POINT('Ctrl Pts',(6.56738667375376,24.968675081176,4.74597172529336));
#451498=CARTESIAN_POINT('Ctrl Pts',(6.56829321884323,25.456324918824,4.74640124271564));
#451499=CARTESIAN_POINT('Ctrl Pts',(6.68893848409317,25.4469284240315,4.86586022639608));
#451500=CARTESIAN_POINT('Ctrl Pts',(7.03476003379299,25.4137042390077,5.36752678600608));
#451501=CARTESIAN_POINT('Ctrl Pts',(6.91003560334641,25.3566523637524,6.5258341885166));
#451502=CARTESIAN_POINT('Ctrl Pts',(5.60564496305,25.2851692930582,7.18099123031483));
#451503=CARTESIAN_POINT('Ctrl Pts',(4.34815567114858,25.213686222364,6.43975200870338));
#451504=CARTESIAN_POINT('Ctrl Pts',(4.28968558428151,25.1422031516699,4.98123363545819));
#451505=CARTESIAN_POINT('Ctrl Pts',(5.44432497425889,25.0730827171565,4.16945626611646));
#451506=CARTESIAN_POINT('Ctrl Pts',(6.29641321838457,25.0277899728745,4.47347056935133));
#451507=CARTESIAN_POINT('Ctrl Pts',(6.57067994464873,25.006324918824,4.74405758279954));
#451508=CARTESIAN_POINT('Origin',(5.65685387860011,26.993675081176,5.65685387860011));
#451509=CARTESIAN_POINT('',(6.56704169373441,25.906324918824,4.7445060113485));
#451510=CARTESIAN_POINT('',(6.57057130100612,25.868675081176,4.74432962138981));
#451511=CARTESIAN_POINT('',(6.56902162633079,26.993675081176,4.74468613086949));
#451512=CARTESIAN_POINT('',(5.01302286563433,26.,4.53900700771688));
#451513=CARTESIAN_POINT('Ctrl Pts',(5.01302286563431,26.,4.53900700771688));
#451514=CARTESIAN_POINT('Ctrl Pts',(5.38492752167559,25.9761723097686,4.32480615636363));
#451515=CARTESIAN_POINT('Ctrl Pts',(6.01924597306242,25.9449472827099,4.30899334914827));
#451516=CARTESIAN_POINT('Ctrl Pts',(6.47338425157137,25.9137222556513,4.64940368207851));
#451517=CARTESIAN_POINT('Ctrl Pts',(6.56704169373441,25.906324918824,4.74450601134849));
#451518=CARTESIAN_POINT('',(4.5368959669337,26.,5.01208503488093));
#451519=CARTESIAN_POINT('Origin',(5.65685387860011,26.,5.65685387860011));
#451520=CARTESIAN_POINT('Ctrl Pts',(4.5368902045627,26.,5.01208247494518));
#451521=CARTESIAN_POINT('Ctrl Pts',(4.74314812622022,25.9770624644402,4.65613984562121));
#451522=CARTESIAN_POINT('Ctrl Pts',(5.48969900651177,25.9332874914989,4.17795197796788));
#451523=CARTESIAN_POINT('Ctrl Pts',(6.3039677816093,25.8895125185575,4.48184576512937));
#451524=CARTESIAN_POINT('Ctrl Pts',(6.57057130100612,25.868675081176,4.74432962138981));
#451525=CARTESIAN_POINT('Origin',(0.,25.85,0.));
#451526=CARTESIAN_POINT('',(-1.69705627484771,26.,-1.69705627484771));
#451527=CARTESIAN_POINT('Origin',(0.,26.,0.));
#451528=CARTESIAN_POINT('',(-1.48492424049175,25.7,-1.48492424049175));
#451529=CARTESIAN_POINT('',(-1.59099025766973,25.85,-1.59099025766973));
#451530=CARTESIAN_POINT('Origin',(0.,25.7,0.));
#451531=CARTESIAN_POINT('Origin',(0.,0.,0.));
#451532=CARTESIAN_POINT('',(-1.48492424049175,14.7,-1.48492424049175));
#451533=CARTESIAN_POINT('',(1.48492424049174,14.7,1.48492424049174));
#451534=CARTESIAN_POINT('Origin',(0.,14.7,0.));
#451535=CARTESIAN_POINT('Origin',(0.,14.7,0.));
#451536=CARTESIAN_POINT('',(-1.48492424049175,0.,-1.48492424049175));
#451537=CARTESIAN_POINT('Origin',(7.88424061023,26.,-7.88424061023001));
#451538=CARTESIAN_POINT('',(7.42462120245875,26.,7.42462120245875));
#451539=CARTESIAN_POINT('Origin',(0.,26.,0.));
#451540=CARTESIAN_POINT('Ctrl Pts',(5.01302286563431,26.,4.53900700771688));
#451541=CARTESIAN_POINT('Ctrl Pts',(5.06076150603835,26.,4.51730428611638));
#451542=CARTESIAN_POINT('Ctrl Pts',(5.10974961966388,26.,4.49883681289365));
#451543=CARTESIAN_POINT('Ctrl Pts',(5.15967019073111,26.,4.48353831525793));
#451544=CARTESIAN_POINT('Ctrl Pts',(5.21017178076232,26.,4.46806176041941));
#451545=CARTESIAN_POINT('Ctrl Pts',(5.26162887990441,26.,4.45582849042794));
#451546=CARTESIAN_POINT('Ctrl Pts',(5.31372001428672,26.,4.44682362697332));
#451547=CARTESIAN_POINT('Ctrl Pts',(5.3513943575585,26.,4.44031095795722));
#451548=CARTESIAN_POINT('Ctrl Pts',(5.38940054503647,26.,4.43548811807628));
#451549=CARTESIAN_POINT('Ctrl Pts',(5.42761365593421,26.,4.43236615256964));
#451550=CARTESIAN_POINT('Ctrl Pts',(5.44398133170966,26.,4.43102893301346));
#451551=CARTESIAN_POINT('Ctrl Pts',(5.46038690933068,26.,4.43000393185805));
#451552=CARTESIAN_POINT('Ctrl Pts',(5.47682022646822,26.,4.42929277127865));
#451553=CARTESIAN_POINT('Ctrl Pts',(5.48697840403902,26.,4.4288531707168));
#451554=CARTESIAN_POINT('Ctrl Pts',(5.49714835620506,26.,4.42853358462936));
#451555=CARTESIAN_POINT('Ctrl Pts',(5.50731025736073,26.,4.42833449334039));
#451556=CARTESIAN_POINT('Ctrl Pts',(5.55884880603531,26.,4.42732475353579));
#451557=CARTESIAN_POINT('Ctrl Pts',(5.610283939002,26.,4.42940473009374));
#451558=CARTESIAN_POINT('Ctrl Pts',(5.66131493500104,26.,4.43455229706354));
#451559=CARTESIAN_POINT('Ctrl Pts',(5.7111818931385,26.,4.43958244592831));
#451560=CARTESIAN_POINT('Ctrl Pts',(5.7606639397111,26.,4.44754223428516));
#451561=CARTESIAN_POINT('Ctrl Pts',(5.8094641568765,26.,4.45845673165193));
#451562=CARTESIAN_POINT('Ctrl Pts',(5.84341695883143,26.,4.46605050457051));
#451563=CARTESIAN_POINT('Ctrl Pts',(5.87703937804619,26.,4.47507550289033));
#451564=CARTESIAN_POINT('Ctrl Pts',(5.91022284171251,26.,4.48555225878239));
#451565=CARTESIAN_POINT('Ctrl Pts',(5.92194029467554,26.,4.48925171871836));
#451566=CARTESIAN_POINT('Ctrl Pts',(5.93360293686827,26.,4.49313228200365));
#451567=CARTESIAN_POINT('Ctrl Pts',(5.94520571051292,26.,4.49719513441307));
#451568=CARTESIAN_POINT('Ctrl Pts',(5.95377453080572,26.,4.50019561112999));
#451569=CARTESIAN_POINT('Ctrl Pts',(5.96230961480298,26.,4.50329523558675));
#451570=CARTESIAN_POINT('Ctrl Pts',(5.97079740732734,26.,4.50648983134838));
#451571=CARTESIAN_POINT('Ctrl Pts',(6.01606106262497,26.,4.52352595481099));
#451572=CARTESIAN_POINT('Ctrl Pts',(6.06007213708863,26.,4.54329052845224));
#451573=CARTESIAN_POINT('Ctrl Pts',(6.10256102519025,26.,4.56579698909369));
#451574=CARTESIAN_POINT('Ctrl Pts',(6.13297429945773,26.,4.58190696962887));
#451575=CARTESIAN_POINT('Ctrl Pts',(6.16260727981828,26.,4.59942271299404));
#451576=CARTESIAN_POINT('Ctrl Pts',(6.1913507700685,26.,4.61836202894701));
#451577=CARTESIAN_POINT('Ctrl Pts',(6.22965595338923,26.,4.64360162105055));
#451578=CARTESIAN_POINT('Ctrl Pts',(6.26638275459849,26.,4.67136946042345));
#451579=CARTESIAN_POINT('Ctrl Pts',(6.30137698491027,26.,4.70144469586272));
#451580=CARTESIAN_POINT('Ctrl Pts',(6.31060442836129,26.,4.70937507558016));
#451581=CARTESIAN_POINT('Ctrl Pts',(6.31971121578836,26.,4.71746597339334));
#451582=CARTESIAN_POINT('Ctrl Pts',(6.32869409556115,26.,4.72571349227114));
#451583=CARTESIAN_POINT('Ctrl Pts',(6.33546837134763,26.,4.73193320898177));
#451584=CARTESIAN_POINT('Ctrl Pts',(6.34217214625841,26.,4.73824213429014));
#451585=CARTESIAN_POINT('Ctrl Pts',(6.34879370706907,26.,4.74462823868481));
#451586=CARTESIAN_POINT('Ctrl Pts',(6.38351694987569,26.,4.77811675594305));
#451587=CARTESIAN_POINT('Ctrl Pts',(6.41605753628304,26.,4.81379250852091));
#451588=CARTESIAN_POINT('Ctrl Pts',(6.4462758017894,26.,4.85136909773308));
#451589=CARTESIAN_POINT('Ctrl Pts',(6.47641151646928,26.,4.88884303451155));
#451590=CARTESIAN_POINT('Ctrl Pts',(6.50423803830034,26.,4.92820865020386));
#451591=CARTESIAN_POINT('Ctrl Pts',(6.52957020070414,26.,4.96920312732197));
#451592=CARTESIAN_POINT('Ctrl Pts',(6.54313464053154,26.,4.9911541597392));
#451593=CARTESIAN_POINT('Ctrl Pts',(6.55598305842118,26.,5.0135724729987));
#451594=CARTESIAN_POINT('Ctrl Pts',(6.56808081878415,26.,5.03641841923856));
#451595=CARTESIAN_POINT('Ctrl Pts',(6.57436456839788,26.,5.04828493019204));
#451596=CARTESIAN_POINT('Ctrl Pts',(6.58044572293647,26.,5.06026681279699));
#451597=CARTESIAN_POINT('Ctrl Pts',(6.58631893168823,26.,5.07235847248556));
#451598=CARTESIAN_POINT('Ctrl Pts',(6.59081778530665,26.,5.0816206338086));
#451599=CARTESIAN_POINT('Ctrl Pts',(6.5951946526525,26.,5.09094758402314));
#451600=CARTESIAN_POINT('Ctrl Pts',(6.59944110229676,26.,5.10032287212331));
#451601=CARTESIAN_POINT('Ctrl Pts',(6.6185486795277,26.,5.14250847573184));
#451602=CARTESIAN_POINT('Ctrl Pts',(6.63505331111242,26.,5.18574009205373));
#451603=CARTESIAN_POINT('Ctrl Pts',(6.64877678422558,26.,5.22977562437019));
#451604=CARTESIAN_POINT('Ctrl Pts',(6.65803415466685,26.,5.25948043975257));
#451605=CARTESIAN_POINT('Ctrl Pts',(6.66602500922953,26.,5.28955126506286));
#451606=CARTESIAN_POINT('Ctrl Pts',(6.67268119205899,26.,5.3199128379813));
#451607=CARTESIAN_POINT('Ctrl Pts',(6.67555458049447,26.,5.33301953813398));
#451608=CARTESIAN_POINT('Ctrl Pts',(6.67817927295671,26.,5.34618251321162));
#451609=CARTESIAN_POINT('Ctrl Pts',(6.68054575323313,26.,5.35937322817315));
#451610=CARTESIAN_POINT('Ctrl Pts',(6.68833148242524,26.,5.4027707310232));
#451611=CARTESIAN_POINT('Ctrl Pts',(6.69333871127853,26.,5.44652175704576));
#451612=CARTESIAN_POINT('Ctrl Pts',(6.69538344663679,26.,5.49040691017122));
#451613=CARTESIAN_POINT('Ctrl Pts',(6.69639471249186,26.,5.51211121372355));
#451614=CARTESIAN_POINT('Ctrl Pts',(6.69668059243935,26.,5.53384821037826));
#451615=CARTESIAN_POINT('Ctrl Pts',(6.69621420261903,26.,5.55559016156262));
#451616=CARTESIAN_POINT('Ctrl Pts',(6.69593634735414,26.,5.56854309351446));
#451617=CARTESIAN_POINT('Ctrl Pts',(6.69539142062067,26.,5.58149776570054));
#451618=CARTESIAN_POINT('Ctrl Pts',(6.69458228414866,26.,5.59444726164187));
#451619=CARTESIAN_POINT('Ctrl Pts',(5.59475217632212,26.,6.69274404704181));
#451620=CARTESIAN_POINT('Ctrl Pts',(5.55137724984311,26.,6.69531021368757));
#451621=CARTESIAN_POINT('Ctrl Pts',(5.50802061877154,26.,6.69492058849835));
#451622=CARTESIAN_POINT('Ctrl Pts',(5.4649019749424,26.,6.69178524360462));
#451623=CARTESIAN_POINT('Ctrl Pts',(5.41981030827847,26.,6.6885064316043));
#451624=CARTESIAN_POINT('Ctrl Pts',(5.3749781156863,26.,6.6822250250606));
#451625=CARTESIAN_POINT('Ctrl Pts',(5.33063916085636,26.,6.67312701402814));
#451626=CARTESIAN_POINT('Ctrl Pts',(5.29648485405826,26.,6.66611881409995));
#451627=CARTESIAN_POINT('Ctrl Pts',(5.26262271564401,26.,6.657438192268));
#451628=CARTESIAN_POINT('Ctrl Pts',(5.22915790417526,26.,6.64714921184179));
#451629=CARTESIAN_POINT('Ctrl Pts',(5.2180438660871,26.,6.64373212639213));
#451630=CARTESIAN_POINT('Ctrl Pts',(5.20697366141539,26.,6.64013749916696));
#451631=CARTESIAN_POINT('Ctrl Pts',(5.19595119703594,26.,6.63636725687979));
#451632=CARTESIAN_POINT('Ctrl Pts',(5.18836217076809,26.,6.63377142469848));
#451633=CARTESIAN_POINT('Ctrl Pts',(5.18079825567733,26.,6.63109312202817));
#451634=CARTESIAN_POINT('Ctrl Pts',(5.17326885643069,26.,6.62833627003802));
#451635=CARTESIAN_POINT('Ctrl Pts',(5.1291279008345,26.,6.61217427924751));
#451636=CARTESIAN_POINT('Ctrl Pts',(5.08609247696685,26.,6.59328941999762));
#451637=CARTESIAN_POINT('Ctrl Pts',(5.04440658587507,26.,6.57188267750787));
#451638=CARTESIAN_POINT('Ctrl Pts',(5.00189276334404,26.,6.55005077161978));
#451639=CARTESIAN_POINT('Ctrl Pts',(4.96078147197193,26.,6.52559561372727));
#451640=CARTESIAN_POINT('Ctrl Pts',(4.92133403622236,26.,6.49867698438676));
#451641=CARTESIAN_POINT('Ctrl Pts',(4.89441638666335,26.,6.48030858559407));
#451642=CARTESIAN_POINT('Ctrl Pts',(4.86827351967756,26.,6.46079201260925));
#451643=CARTESIAN_POINT('Ctrl Pts',(4.84299340446309,26.,6.4401650142142));
#451644=CARTESIAN_POINT('Ctrl Pts',(4.83579340555386,26.,6.43429026385467));
#451645=CARTESIAN_POINT('Ctrl Pts',(4.82866342617017,26.,6.42832537837765));
#451646=CARTESIAN_POINT('Ctrl Pts',(4.82160559536045,26.,6.42227108527737));
#451647=CARTESIAN_POINT('Ctrl Pts',(4.81488692701488,26.,6.41650772986347));
#451648=CARTESIAN_POINT('Ctrl Pts',(4.80824066086902,26.,6.41066935775182));
#451649=CARTESIAN_POINT('Ctrl Pts',(4.80166944006503,26.,6.40475816436008));
#451650=CARTESIAN_POINT('Ctrl Pts',(4.76504957872374,26.,6.37181647988102));
#451651=CARTESIAN_POINT('Ctrl Pts',(4.73074760271325,26.,6.3366074009898));
#451652=CARTESIAN_POINT('Ctrl Pts',(4.69903040790721,26.,6.29931177973046));
#451653=CARTESIAN_POINT('Ctrl Pts',(4.67944112167677,26.,6.27627712598951));
#451654=CARTESIAN_POINT('Ctrl Pts',(4.66083800978401,26.,6.25244551905118));
#451655=CARTESIAN_POINT('Ctrl Pts',(4.64328815682614,26.,6.22785054805505));
#451656=CARTESIAN_POINT('Ctrl Pts',(4.61561379199964,26.,6.18906673591271));
#451657=CARTESIAN_POINT('Ctrl Pts',(4.59055615782454,26.,6.14838638392197));
#451658=CARTESIAN_POINT('Ctrl Pts',(4.56810357334095,26.,6.10609561292347));
#451659=CARTESIAN_POINT('Ctrl Pts',(4.56308085571068,26.,6.0966350271612));
#451660=CARTESIAN_POINT('Ctrl Pts',(4.55818866062255,26.,6.08709371894873));
#451661=CARTESIAN_POINT('Ctrl Pts',(4.55342713549933,26.,6.0774746818157));
#451662=CARTESIAN_POINT('Ctrl Pts',(4.54941744651794,26.,6.06937447312086));
#451663=CARTESIAN_POINT('Ctrl Pts',(4.54550147490651,26.,6.06122106951547));
#451664=CARTESIAN_POINT('Ctrl Pts',(4.54168378413803,26.,6.05302670560527));
#451665=CARTESIAN_POINT('Ctrl Pts',(4.52091202527781,26.,6.00844180822155));
#451666=CARTESIAN_POINT('Ctrl Pts',(4.5030051530968,26.,5.9625645247388));
#451667=CARTESIAN_POINT('Ctrl Pts',(4.48791424199878,26.,5.91572767775388));
#451668=CARTESIAN_POINT('Ctrl Pts',(4.4724457898949,26.,5.86771907710826));
#451669=CARTESIAN_POINT('Ctrl Pts',(4.45993552318701,26.,5.81870139486952));
#451670=CARTESIAN_POINT('Ctrl Pts',(4.45037293016505,26.,5.76899658983648));
#451671=CARTESIAN_POINT('Ctrl Pts',(4.44466425311952,26.,5.73932381395939));
#451672=CARTESIAN_POINT('Ctrl Pts',(4.4400069173499,26.,5.70940552486093));
#451673=CARTESIAN_POINT('Ctrl Pts',(4.43640656180746,26.,5.67930640361674));
#451674=CARTESIAN_POINT('Ctrl Pts',(4.4344238827759,26.,5.66273112491008));
#451675=CARTESIAN_POINT('Ctrl Pts',(4.4327618494722,26.,5.6461009688343));
#451676=CARTESIAN_POINT('Ctrl Pts',(4.4314222120057,26.,5.62942654610506));
#451677=CARTESIAN_POINT('Ctrl Pts',(4.4306913632861,26.,5.62032969654203));
#451678=CARTESIAN_POINT('Ctrl Pts',(4.43005669150461,26.,5.61122148290957));
#451679=CARTESIAN_POINT('Ctrl Pts',(4.42951879017363,26.,5.60211289272811));
#451680=CARTESIAN_POINT('Ctrl Pts',(4.4264158896556,26.,5.54956970763969));
#451681=CARTESIAN_POINT('Ctrl Pts',(4.42652201105729,26.,5.4969304712558));
#451682=CARTESIAN_POINT('Ctrl Pts',(4.42983270797829,26.,5.44453981443333));
#451683=CARTESIAN_POINT('Ctrl Pts',(4.43208820455334,26.,5.40884734549178));
#451684=CARTESIAN_POINT('Ctrl Pts',(4.43583203037196,26.,5.37326963814493));
#451685=CARTESIAN_POINT('Ctrl Pts',(4.44107619046014,26.,5.33791219834493));
#451686=CARTESIAN_POINT('Ctrl Pts',(4.44350332623801,26.,5.32154784147763));
#451687=CARTESIAN_POINT('Ctrl Pts',(4.44625314527356,26.,5.3052257211536));
#451688=CARTESIAN_POINT('Ctrl Pts',(4.44932134384721,26.,5.2889864307097));
#451689=CARTESIAN_POINT('Ctrl Pts',(4.45918506317858,26.,5.23677996517828));
#451690=CARTESIAN_POINT('Ctrl Pts',(4.47234120944802,26.,5.18537728352641));
#451691=CARTESIAN_POINT('Ctrl Pts',(4.48880818879318,26.,5.13511946191399));
#451692=CARTESIAN_POINT('Ctrl Pts',(4.49754364477499,26.,5.10845853162224));
#451693=CARTESIAN_POINT('Ctrl Pts',(4.50721166236008,26.,5.08211963725754));
#451694=CARTESIAN_POINT('Ctrl Pts',(4.51782098438608,26.,5.05615381819268));
#451695=CARTESIAN_POINT('Ctrl Pts',(4.52387352626206,26.,5.04134050525441));
#451696=CARTESIAN_POINT('Ctrl Pts',(4.53023250440261,26.,5.02664862375098));
#451697=CARTESIAN_POINT('Ctrl Pts',(4.53689020456271,26.,5.01208247494515));
#451698=CARTESIAN_POINT('Ctrl Pts',(-4.53900700771688,26.,5.01302286563431));
#451699=CARTESIAN_POINT('Ctrl Pts',(-4.51730428611638,26.,5.06076150603835));
#451700=CARTESIAN_POINT('Ctrl Pts',(-4.49883681289365,26.,5.10974961966389));
#451701=CARTESIAN_POINT('Ctrl Pts',(-4.48353831525793,26.,5.15967019073111));
#451702=CARTESIAN_POINT('Ctrl Pts',(-4.46806176041944,26.,5.21017178076222));
#451703=CARTESIAN_POINT('Ctrl Pts',(-4.45582849042799,26.,5.26162887990419));
#451704=CARTESIAN_POINT('Ctrl Pts',(-4.44682362697337,26.,5.3137200142864));
#451705=CARTESIAN_POINT('Ctrl Pts',(-4.44031095795727,26.,5.35139435755819));
#451706=CARTESIAN_POINT('Ctrl Pts',(-4.43548811807631,26.,5.38940054503618));
#451707=CARTESIAN_POINT('Ctrl Pts',(-4.43236615256966,26.,5.42761365593392));
#451708=CARTESIAN_POINT('Ctrl Pts',(-4.43102893301347,26.,5.4439813317094));
#451709=CARTESIAN_POINT('Ctrl Pts',(-4.43000393185806,26.,5.46038690933045));
#451710=CARTESIAN_POINT('Ctrl Pts',(-4.42929277127866,26.,5.47682022646802));
#451711=CARTESIAN_POINT('Ctrl Pts',(-4.42885317071679,26.,5.48697840403927));
#451712=CARTESIAN_POINT('Ctrl Pts',(-4.42853358462933,26.,5.49714835620576));
#451713=CARTESIAN_POINT('Ctrl Pts',(-4.42833449334036,26.,5.50731025736187));
#451714=CARTESIAN_POINT('Ctrl Pts',(-4.42732475353582,26.,5.55884880603616));
#451715=CARTESIAN_POINT('Ctrl Pts',(-4.42940473009378,26.,5.61028393900257));
#451716=CARTESIAN_POINT('Ctrl Pts',(-4.43455229706356,26.,5.66131493500133));
#451717=CARTESIAN_POINT('Ctrl Pts',(-4.43958244592836,26.,5.71118189313887));
#451718=CARTESIAN_POINT('Ctrl Pts',(-4.44754223428524,26.,5.76066393971155));
#451719=CARTESIAN_POINT('Ctrl Pts',(-4.45845673165205,26.,5.80946415687703));
#451720=CARTESIAN_POINT('Ctrl Pts',(-4.46605050457064,26.,5.84341695883192));
#451721=CARTESIAN_POINT('Ctrl Pts',(-4.47507550289046,26.,5.87703937804663));
#451722=CARTESIAN_POINT('Ctrl Pts',(-4.48555225878251,26.,5.9102228417129));
#451723=CARTESIAN_POINT('Ctrl Pts',(-4.48925171871859,26.,5.92194029467625));
#451724=CARTESIAN_POINT('Ctrl Pts',(-4.493132282004,26.,5.9336029368693));
#451725=CARTESIAN_POINT('Ctrl Pts',(-4.49719513441354,26.,5.94520571051427));
#451726=CARTESIAN_POINT('Ctrl Pts',(-4.50019561112957,26.,5.95377453080449));
#451727=CARTESIAN_POINT('Ctrl Pts',(-4.50329523558538,26.,5.96230961479921));
#451728=CARTESIAN_POINT('Ctrl Pts',(-4.50648983134602,26.,5.97079740732105));
#451729=CARTESIAN_POINT('Ctrl Pts',(-4.52352595480839,26.,6.01606106261884));
#451730=CARTESIAN_POINT('Ctrl Pts',(-4.54329052844941,26.,6.06007213708267));
#451731=CARTESIAN_POINT('Ctrl Pts',(-4.56579698909062,26.,6.10256102518446));
#451732=CARTESIAN_POINT('Ctrl Pts',(-4.58190696962665,26.,6.13297429945397));
#451733=CARTESIAN_POINT('Ctrl Pts',(-4.59942271299284,26.,6.16260727981646));
#451734=CARTESIAN_POINT('Ctrl Pts',(-4.61836202894701,26.,6.1913507700685));
#451735=CARTESIAN_POINT('Ctrl Pts',(-4.64360162105055,26.,6.22965595338923));
#451736=CARTESIAN_POINT('Ctrl Pts',(-4.67136946042345,26.,6.2663827545985));
#451737=CARTESIAN_POINT('Ctrl Pts',(-4.70144469586272,26.,6.30137698491027));
#451738=CARTESIAN_POINT('Ctrl Pts',(-4.70937507558004,26.,6.31060442836116));
#451739=CARTESIAN_POINT('Ctrl Pts',(-4.71746597339309,26.,6.31971121578808));
#451740=CARTESIAN_POINT('Ctrl Pts',(-4.72571349227076,26.,6.32869409556074));
#451741=CARTESIAN_POINT('Ctrl Pts',(-4.7319332089771,26.,6.33546837134255));
#451742=CARTESIAN_POINT('Ctrl Pts',(-4.73824213428106,26.,6.34217214624876));
#451743=CARTESIAN_POINT('Ctrl Pts',(-4.74462823867121,26.,6.34879370705498));
#451744=CARTESIAN_POINT('Ctrl Pts',(-4.77811675592868,26.,6.383516949862));
#451745=CARTESIAN_POINT('Ctrl Pts',(-4.81379250850578,26.,6.41605753626979));
#451746=CARTESIAN_POINT('Ctrl Pts',(-4.85136909771721,26.,6.44627580177665));
#451747=CARTESIAN_POINT('Ctrl Pts',(-4.88884303449548,26.,6.47641151645744));
#451748=CARTESIAN_POINT('Ctrl Pts',(-4.92820865018765,26.,6.5042380382894));
#451749=CARTESIAN_POINT('Ctrl Pts',(-4.96920312730568,26.,6.52957020069408));
#451750=CARTESIAN_POINT('Ctrl Pts',(-4.99115415972337,26.,6.54313464052225));
#451751=CARTESIAN_POINT('Ctrl Pts',(-5.01357247298336,26.,6.55598305841263));
#451752=CARTESIAN_POINT('Ctrl Pts',(-5.03641841922373,26.,6.5680808187763));
#451753=CARTESIAN_POINT('Ctrl Pts',(-5.04828493017013,26.,6.57436456838649));
#451754=CARTESIAN_POINT('Ctrl Pts',(-5.06026681276785,26.,6.58044572292179));
#451755=CARTESIAN_POINT('Ctrl Pts',(-5.07235847244907,26.,6.5863189316705));
#451756=CARTESIAN_POINT('Ctrl Pts',(-5.08162063377995,26.,6.59081778529314));
#451757=CARTESIAN_POINT('Ctrl Pts',(-5.09094758400247,26.,6.595194652643));
#451758=CARTESIAN_POINT('Ctrl Pts',(-5.1003228721107,26.,6.59944110229105));
#451759=CARTESIAN_POINT('Ctrl Pts',(-5.14250847571933,26.,6.61854867952265));
#451760=CARTESIAN_POINT('Ctrl Pts',(-5.18574009204136,26.,6.63505331110801));
#451761=CARTESIAN_POINT('Ctrl Pts',(-5.22977562435799,26.,6.64877678422178));
#451762=CARTESIAN_POINT('Ctrl Pts',(-5.2594804397383,26.,6.65803415466278));
#451763=CARTESIAN_POINT('Ctrl Pts',(-5.28955126504646,26.,6.66602500922537));
#451764=CARTESIAN_POINT('Ctrl Pts',(-5.31991283796277,26.,6.67268119205492));
#451765=CARTESIAN_POINT('Ctrl Pts',(-5.33301953811817,26.,6.67555458049125));
#451766=CARTESIAN_POINT('Ctrl Pts',(-5.34618251319858,26.,6.67817927295424));
#451767=CARTESIAN_POINT('Ctrl Pts',(-5.35937322816289,26.,6.68054575323129));
#451768=CARTESIAN_POINT('Ctrl Pts',(-5.40277073101277,26.,6.68833148242381));
#451769=CARTESIAN_POINT('Ctrl Pts',(-5.44652175703517,26.,6.69333871127755));
#451770=CARTESIAN_POINT('Ctrl Pts',(-5.4904069101605,26.,6.6953834466363));
#451771=CARTESIAN_POINT('Ctrl Pts',(-5.51211121371639,26.,6.69639471249176));
#451772=CARTESIAN_POINT('Ctrl Pts',(-5.53384821037469,26.,6.69668059243942));
#451773=CARTESIAN_POINT('Ctrl Pts',(-5.55559016156262,26.,6.69621420261903));
#451774=CARTESIAN_POINT('Ctrl Pts',(-5.56854309351446,26.,6.69593634735414));
#451775=CARTESIAN_POINT('Ctrl Pts',(-5.58149776570054,26.,6.69539142062068));
#451776=CARTESIAN_POINT('Ctrl Pts',(-5.59444726164187,26.,6.69458228414866));
#451777=CARTESIAN_POINT('Ctrl Pts',(-6.69274404704181,26.,5.59475217632212));
#451778=CARTESIAN_POINT('Ctrl Pts',(-6.69531021368757,26.,5.55137724984311));
#451779=CARTESIAN_POINT('Ctrl Pts',(-6.69492058849835,26.,5.50802061877154));
#451780=CARTESIAN_POINT('Ctrl Pts',(-6.69178524360462,26.,5.4649019749424));
#451781=CARTESIAN_POINT('Ctrl Pts',(-6.6885064316043,26.,5.41981030827847));
#451782=CARTESIAN_POINT('Ctrl Pts',(-6.6822250250606,26.,5.3749781156863));
#451783=CARTESIAN_POINT('Ctrl Pts',(-6.67312701402814,26.,5.33063916085636));
#451784=CARTESIAN_POINT('Ctrl Pts',(-6.66611881409995,26.,5.29648485405826));
#451785=CARTESIAN_POINT('Ctrl Pts',(-6.657438192268,26.,5.26262271564401));
#451786=CARTESIAN_POINT('Ctrl Pts',(-6.64714921184179,26.,5.22915790417526));
#451787=CARTESIAN_POINT('Ctrl Pts',(-6.64373212639213,26.,5.2180438660871));
#451788=CARTESIAN_POINT('Ctrl Pts',(-6.64013749916696,26.,5.20697366141539));
#451789=CARTESIAN_POINT('Ctrl Pts',(-6.63636725687979,26.,5.19595119703594));
#451790=CARTESIAN_POINT('Ctrl Pts',(-6.63377142469848,26.,5.18836217076809));
#451791=CARTESIAN_POINT('Ctrl Pts',(-6.63109312202817,26.,5.18079825567733));
#451792=CARTESIAN_POINT('Ctrl Pts',(-6.62833627003802,26.,5.17326885643069));
#451793=CARTESIAN_POINT('Ctrl Pts',(-6.61217427924751,26.,5.1291279008345));
#451794=CARTESIAN_POINT('Ctrl Pts',(-6.59328941999762,26.,5.08609247696685));
#451795=CARTESIAN_POINT('Ctrl Pts',(-6.57188267750787,26.,5.04440658587507));
#451796=CARTESIAN_POINT('Ctrl Pts',(-6.55005077161978,26.,5.00189276334404));
#451797=CARTESIAN_POINT('Ctrl Pts',(-6.52559561372727,26.,4.96078147197193));
#451798=CARTESIAN_POINT('Ctrl Pts',(-6.49867698438676,26.,4.92133403622236));
#451799=CARTESIAN_POINT('Ctrl Pts',(-6.48030858559407,26.,4.89441638666335));
#451800=CARTESIAN_POINT('Ctrl Pts',(-6.46079201260925,26.,4.86827351967756));
#451801=CARTESIAN_POINT('Ctrl Pts',(-6.4401650142142,26.,4.84299340446309));
#451802=CARTESIAN_POINT('Ctrl Pts',(-6.43429026385467,26.,4.83579340555386));
#451803=CARTESIAN_POINT('Ctrl Pts',(-6.42832537837765,26.,4.82866342617017));
#451804=CARTESIAN_POINT('Ctrl Pts',(-6.42227108527737,26.,4.82160559536045));
#451805=CARTESIAN_POINT('Ctrl Pts',(-6.41650772986347,26.,4.81488692701488));
#451806=CARTESIAN_POINT('Ctrl Pts',(-6.41066935775182,26.,4.80824066086902));
#451807=CARTESIAN_POINT('Ctrl Pts',(-6.40475816436008,26.,4.80166944006503));
#451808=CARTESIAN_POINT('Ctrl Pts',(-6.37181647988102,26.,4.76504957872374));
#451809=CARTESIAN_POINT('Ctrl Pts',(-6.3366074009898,26.,4.73074760271325));
#451810=CARTESIAN_POINT('Ctrl Pts',(-6.29931177973046,26.,4.69903040790721));
#451811=CARTESIAN_POINT('Ctrl Pts',(-6.27627712598951,26.,4.67944112167677));
#451812=CARTESIAN_POINT('Ctrl Pts',(-6.25244551905118,26.,4.66083800978401));
#451813=CARTESIAN_POINT('Ctrl Pts',(-6.22785054805505,26.,4.64328815682614));
#451814=CARTESIAN_POINT('Ctrl Pts',(-6.18906673591271,26.,4.61561379199964));
#451815=CARTESIAN_POINT('Ctrl Pts',(-6.14838638392197,26.,4.59055615782454));
#451816=CARTESIAN_POINT('Ctrl Pts',(-6.10609561292347,26.,4.56810357334095));
#451817=CARTESIAN_POINT('Ctrl Pts',(-6.0966350271612,26.,4.56308085571068));
#451818=CARTESIAN_POINT('Ctrl Pts',(-6.08709371894873,26.,4.55818866062255));
#451819=CARTESIAN_POINT('Ctrl Pts',(-6.0774746818157,26.,4.55342713549933));
#451820=CARTESIAN_POINT('Ctrl Pts',(-6.06937447312086,26.,4.54941744651794));
#451821=CARTESIAN_POINT('Ctrl Pts',(-6.06122106951547,26.,4.54550147490651));
#451822=CARTESIAN_POINT('Ctrl Pts',(-6.05302670560527,26.,4.54168378413803));
#451823=CARTESIAN_POINT('Ctrl Pts',(-6.00844180822155,26.,4.52091202527781));
#451824=CARTESIAN_POINT('Ctrl Pts',(-5.9625645247388,26.,4.5030051530968));
#451825=CARTESIAN_POINT('Ctrl Pts',(-5.91572767775388,26.,4.48791424199878));
#451826=CARTESIAN_POINT('Ctrl Pts',(-5.86771907710826,26.,4.4724457898949));
#451827=CARTESIAN_POINT('Ctrl Pts',(-5.81870139486952,26.,4.45993552318701));
#451828=CARTESIAN_POINT('Ctrl Pts',(-5.76899658983648,26.,4.45037293016505));
#451829=CARTESIAN_POINT('Ctrl Pts',(-5.73932381395939,26.,4.44466425311952));
#451830=CARTESIAN_POINT('Ctrl Pts',(-5.70940552486093,26.,4.4400069173499));
#451831=CARTESIAN_POINT('Ctrl Pts',(-5.67930640361674,26.,4.43640656180746));
#451832=CARTESIAN_POINT('Ctrl Pts',(-5.66273112491008,26.,4.4344238827759));
#451833=CARTESIAN_POINT('Ctrl Pts',(-5.6461009688343,26.,4.4327618494722));
#451834=CARTESIAN_POINT('Ctrl Pts',(-5.62942654610506,26.,4.4314222120057));
#451835=CARTESIAN_POINT('Ctrl Pts',(-5.62032969654203,26.,4.4306913632861));
#451836=CARTESIAN_POINT('Ctrl Pts',(-5.61122148290957,26.,4.43005669150461));
#451837=CARTESIAN_POINT('Ctrl Pts',(-5.60211289272811,26.,4.42951879017363));
#451838=CARTESIAN_POINT('Ctrl Pts',(-5.54956970763969,26.,4.4264158896556));
#451839=CARTESIAN_POINT('Ctrl Pts',(-5.4969304712558,26.,4.42652201105729));
#451840=CARTESIAN_POINT('Ctrl Pts',(-5.44453981443333,26.,4.42983270797829));
#451841=CARTESIAN_POINT('Ctrl Pts',(-5.40884734549178,26.,4.43208820455334));
#451842=CARTESIAN_POINT('Ctrl Pts',(-5.37326963814493,26.,4.43583203037196));
#451843=CARTESIAN_POINT('Ctrl Pts',(-5.33791219834493,26.,4.44107619046014));
#451844=CARTESIAN_POINT('Ctrl Pts',(-5.32154784147763,26.,4.44350332623801));
#451845=CARTESIAN_POINT('Ctrl Pts',(-5.3052257211536,26.,4.44625314527356));
#451846=CARTESIAN_POINT('Ctrl Pts',(-5.2889864307097,26.,4.44932134384721));
#451847=CARTESIAN_POINT('Ctrl Pts',(-5.23677996517828,26.,4.45918506317858));
#451848=CARTESIAN_POINT('Ctrl Pts',(-5.18537728352641,26.,4.47234120944802));
#451849=CARTESIAN_POINT('Ctrl Pts',(-5.13511946191399,26.,4.48880818879318));
#451850=CARTESIAN_POINT('Ctrl Pts',(-5.10845853162224,26.,4.49754364477499));
#451851=CARTESIAN_POINT('Ctrl Pts',(-5.08211963725754,26.,4.50721166236008));
#451852=CARTESIAN_POINT('Ctrl Pts',(-5.05615381819268,26.,4.51782098438608));
#451853=CARTESIAN_POINT('Ctrl Pts',(-5.04134050525441,26.,4.52387352626206));
#451854=CARTESIAN_POINT('Ctrl Pts',(-5.02664862375098,26.,4.53023250440261));
#451855=CARTESIAN_POINT('Ctrl Pts',(-5.01208247494515,26.,4.53689020456271));
#451856=CARTESIAN_POINT('Ctrl Pts',(-5.01302286563431,26.,-4.53900700771688));
#451857=CARTESIAN_POINT('Ctrl Pts',(-5.06076150603835,26.,-4.51730428611638));
#451858=CARTESIAN_POINT('Ctrl Pts',(-5.10974961966388,26.,-4.49883681289365));
#451859=CARTESIAN_POINT('Ctrl Pts',(-5.1596701907311,26.,-4.48353831525793));
#451860=CARTESIAN_POINT('Ctrl Pts',(-5.21017178076207,26.,-4.46806176041948));
#451861=CARTESIAN_POINT('Ctrl Pts',(-5.26162887990392,26.,-4.45582849042805));
#451862=CARTESIAN_POINT('Ctrl Pts',(-5.31372001428598,26.,-4.44682362697344));
#451863=CARTESIAN_POINT('Ctrl Pts',(-5.35139435755779,26.,-4.44031095795732));
#451864=CARTESIAN_POINT('Ctrl Pts',(-5.38940054503579,26.,-4.43548811807635));
#451865=CARTESIAN_POINT('Ctrl Pts',(-5.42761365593355,26.,-4.43236615256969));
#451866=CARTESIAN_POINT('Ctrl Pts',(-5.44398133170877,26.,-4.43102893301352));
#451867=CARTESIAN_POINT('Ctrl Pts',(-5.46038690932955,26.,-4.43000393185811));
#451868=CARTESIAN_POINT('Ctrl Pts',(-5.47682022646686,26.,-4.42929277127871));
#451869=CARTESIAN_POINT('Ctrl Pts',(-5.48697840405261,26.,-4.4288531707162));
#451870=CARTESIAN_POINT('Ctrl Pts',(-5.49714835623362,26.,-4.42853358462845));
#451871=CARTESIAN_POINT('Ctrl Pts',(-5.50731025740424,26.,-4.42833449333953));
#451872=CARTESIAN_POINT('Ctrl Pts',(-5.5588488060778,26.,-4.42732475353669));
#451873=CARTESIAN_POINT('Ctrl Pts',(-5.61028393904341,26.,-4.42940473009627));
#451874=CARTESIAN_POINT('Ctrl Pts',(-5.66131493504129,26.,-4.43455229706759));
#451875=CARTESIAN_POINT('Ctrl Pts',(-5.71118189317826,26.,-4.43958244593392));
#451876=CARTESIAN_POINT('Ctrl Pts',(-5.76066393975029,26.,-4.44754223429228));
#451877=CARTESIAN_POINT('Ctrl Pts',(-5.80946415691505,26.,-4.45845673166055));
#451878=CARTESIAN_POINT('Ctrl Pts',(-5.84341695886652,26.,-4.4660505045795));
#451879=CARTESIAN_POINT('Ctrl Pts',(-5.87703937807783,26.,-4.47507550289942));
#451880=CARTESIAN_POINT('Ctrl Pts',(-5.91022284174077,26.,-4.48555225879131));
#451881=CARTESIAN_POINT('Ctrl Pts',(-5.92194029476516,26.,-4.48925171874697));
#451882=CARTESIAN_POINT('Ctrl Pts',(-5.93360293701868,26.,-4.49313228205386));
#451883=CARTESIAN_POINT('Ctrl Pts',(-5.94520571072346,26.,-4.49719513448679));
#451884=CARTESIAN_POINT('Ctrl Pts',(-5.95377453098711,26.,-4.50019561119532));
#451885=CARTESIAN_POINT('Ctrl Pts',(-5.9623096149553,26.,-4.50329523564298));
#451886=CARTESIAN_POINT('Ctrl Pts',(-5.9707974074509,26.,-4.50648983139489));
#451887=CARTESIAN_POINT('Ctrl Pts',(-6.01606106274569,26.,-4.52352595486226));
#451888=CARTESIAN_POINT('Ctrl Pts',(-6.06007213720631,26.,-4.5432905285082));
#451889=CARTESIAN_POINT('Ctrl Pts',(-6.10256102530468,26.,-4.5657969891543));
#451890=CARTESIAN_POINT('Ctrl Pts',(-6.13297429953205,26.,-4.5819069696728));
#451891=CARTESIAN_POINT('Ctrl Pts',(-6.16260727985433,26.,-4.59942271301779));
#451892=CARTESIAN_POINT('Ctrl Pts',(-6.1913507700685,26.,-4.61836202894701));
#451893=CARTESIAN_POINT('Ctrl Pts',(-6.22965595338923,26.,-4.64360162105055));
#451894=CARTESIAN_POINT('Ctrl Pts',(-6.26638275459849,26.,-4.67136946042345));
#451895=CARTESIAN_POINT('Ctrl Pts',(-6.30137698491027,26.,-4.70144469586272));
#451896=CARTESIAN_POINT('Ctrl Pts',(-6.31060442836122,26.,-4.7093750755801));
#451897=CARTESIAN_POINT('Ctrl Pts',(-6.31971121578822,26.,-4.71746597339321));
#451898=CARTESIAN_POINT('Ctrl Pts',(-6.32869409556094,26.,-4.72571349227094));
#451899=CARTESIAN_POINT('Ctrl Pts',(-6.33546837134828,26.,-4.73193320898236));
#451900=CARTESIAN_POINT('Ctrl Pts',(-6.34217214625989,26.,-4.73824213429154));
#451901=CARTESIAN_POINT('Ctrl Pts',(-6.34879370707138,26.,-4.74462823868703));
#451902=CARTESIAN_POINT('Ctrl Pts',(-6.38351694987776,26.,-4.77811675594523));
#451903=CARTESIAN_POINT('Ctrl Pts',(-6.41605753628488,26.,-4.81379250852302));
#451904=CARTESIAN_POINT('Ctrl Pts',(-6.44627580179103,26.,-4.85136909773509));
#451905=CARTESIAN_POINT('Ctrl Pts',(-6.47641151647102,26.,-4.88884303451388));
#451906=CARTESIAN_POINT('Ctrl Pts',(-6.50423803830216,26.,-4.92820865020652));
#451907=CARTESIAN_POINT('Ctrl Pts',(-6.529570200706,26.,-4.96920312732498));
#451908=CARTESIAN_POINT('Ctrl Pts',(-6.54313464053326,26.,-4.99115415974213));
#451909=CARTESIAN_POINT('Ctrl Pts',(-6.55598305842276,26.,-5.01357247300154));
#451910=CARTESIAN_POINT('Ctrl Pts',(-6.5680808187856,26.,-5.0364184192413));
#451911=CARTESIAN_POINT('Ctrl Pts',(-6.57436456839916,26.,-5.04828493019454));
#451912=CARTESIAN_POINT('Ctrl Pts',(-6.58044572293759,26.,-5.06026681279923));
#451913=CARTESIAN_POINT('Ctrl Pts',(-6.58631893168919,26.,-5.07235847248755));
#451914=CARTESIAN_POINT('Ctrl Pts',(-6.59081778529731,26.,-5.08162063378941));
#451915=CARTESIAN_POINT('Ctrl Pts',(-6.59519465263342,26.,-5.09094758398249));
#451916=CARTESIAN_POINT('Ctrl Pts',(-6.59944110226853,26.,-5.10032287206098));
#451917=CARTESIAN_POINT('Ctrl Pts',(-6.61854867950197,26.,-5.14250847566835));
#451918=CARTESIAN_POINT('Ctrl Pts',(-6.63505331108929,26.,-5.18574009198917));
#451919=CARTESIAN_POINT('Ctrl Pts',(-6.64877678420517,26.,-5.22977562430468));
#451920=CARTESIAN_POINT('Ctrl Pts',(-6.65803415464525,26.,-5.25948043967676));
#451921=CARTESIAN_POINT('Ctrl Pts',(-6.66602500920764,26.,-5.28955126497656));
#451922=CARTESIAN_POINT('Ctrl Pts',(-6.67268119203775,26.,-5.31991283788441));
#451923=CARTESIAN_POINT('Ctrl Pts',(-6.6755545804784,26.,-5.33301953805478));
#451924=CARTESIAN_POINT('Ctrl Pts',(-6.67817927294514,26.,-5.34618251315033));
#451925=CARTESIAN_POINT('Ctrl Pts',(-6.68054575322537,26.,-5.35937322812986));
#451926=CARTESIAN_POINT('Ctrl Pts',(-6.68833148241942,26.,-5.40277073098025));
#451927=CARTESIAN_POINT('Ctrl Pts',(-6.69333871127465,26.,-5.44652175700321));
#451928=CARTESIAN_POINT('Ctrl Pts',(-6.69538344663484,26.,-5.49040691012916));
#451929=CARTESIAN_POINT('Ctrl Pts',(-6.69639471249149,26.,-5.51211121369546));
#451930=CARTESIAN_POINT('Ctrl Pts',(-6.69668059243965,26.,-5.53384821036422));
#451931=CARTESIAN_POINT('Ctrl Pts',(-6.69621420261903,26.,-5.55559016156262));
#451932=CARTESIAN_POINT('Ctrl Pts',(-6.69593634735414,26.,-5.56854309351446));
#451933=CARTESIAN_POINT('Ctrl Pts',(-6.69539142062068,26.,-5.58149776570054));
#451934=CARTESIAN_POINT('Ctrl Pts',(-6.69458228414866,26.,-5.59444726164187));
#451935=CARTESIAN_POINT('Ctrl Pts',(-5.59475217632212,26.,-6.69274404704181));
#451936=CARTESIAN_POINT('Ctrl Pts',(-5.55137724984312,26.,-6.69531021368757));
#451937=CARTESIAN_POINT('Ctrl Pts',(-5.50802061877154,26.,-6.69492058849835));
#451938=CARTESIAN_POINT('Ctrl Pts',(-5.46490197494241,26.,-6.69178524360462));
#451939=CARTESIAN_POINT('Ctrl Pts',(-5.4198103082784,26.,-6.68850643160429));
#451940=CARTESIAN_POINT('Ctrl Pts',(-5.37497811568615,26.,-6.68222502506058));
#451941=CARTESIAN_POINT('Ctrl Pts',(-5.33063916085613,26.,-6.67312701402809));
#451942=CARTESIAN_POINT('Ctrl Pts',(-5.29648485405804,26.,-6.6661188140999));
#451943=CARTESIAN_POINT('Ctrl Pts',(-5.2626227156438,26.,-6.65743819226794));
#451944=CARTESIAN_POINT('Ctrl Pts',(-5.22915790417506,26.,-6.64714921184172));
#451945=CARTESIAN_POINT('Ctrl Pts',(-5.21804386616628,26.,-6.64373212641647));
#451946=CARTESIAN_POINT('Ctrl Pts',(-5.20697366157331,26.,-6.64013749921824));
#451947=CARTESIAN_POINT('Ctrl Pts',(-5.19595119727191,26.,-6.6363672569605));
#451948=CARTESIAN_POINT('Ctrl Pts',(-5.1883621710592,26.,-6.63377142479994));
#451949=CARTESIAN_POINT('Ctrl Pts',(-5.18079825602294,26.,-6.63109312215148));
#451950=CARTESIAN_POINT('Ctrl Pts',(-5.17326885683034,26.,-6.62833627018435));
#451951=CARTESIAN_POINT('Ctrl Pts',(-5.1291279012311,26.,-6.61217427941162));
#451952=CARTESIAN_POINT('Ctrl Pts',(-5.08609247735947,26.,-6.59328942017928));
#451953=CARTESIAN_POINT('Ctrl Pts',(-5.04440658626274,26.,-6.57188267770694));
#451954=CARTESIAN_POINT('Ctrl Pts',(-5.00189276372273,26.,-6.5500507718346));
#451955=CARTESIAN_POINT('Ctrl Pts',(-4.9607814723409,26.,-6.52559561395722));
#451956=CARTESIAN_POINT('Ctrl Pts',(-4.92133403658083,26.,-6.49867698463137));
#451957=CARTESIAN_POINT('Ctrl Pts',(-4.89441638698506,26.,-6.4803085858285));
#451958=CARTESIAN_POINT('Ctrl Pts',(-4.86827351996386,26.,-6.46079201283075));
#451959=CARTESIAN_POINT('Ctrl Pts',(-4.84299340471559,26.,-6.44016501442022));
#451960=CARTESIAN_POINT('Ctrl Pts',(-4.83579340611366,26.,-6.43429026431488));
#451961=CARTESIAN_POINT('Ctrl Pts',(-4.82866342703126,26.,-6.42832537909978));
#451962=CARTESIAN_POINT('Ctrl Pts',(-4.8216055965165,26.,-6.42227108626905));
#451963=CARTESIAN_POINT('Ctrl Pts',(-4.81488692784565,26.,-6.41650773059184));
#451964=CARTESIAN_POINT('Ctrl Pts',(-4.80824066137958,26.,-6.41066935820828));
#451965=CARTESIAN_POINT('Ctrl Pts',(-4.80166944026328,26.,-6.40475816453841));
#451966=CARTESIAN_POINT('Ctrl Pts',(-4.76504957891336,26.,-6.37181648006733));
#451967=CARTESIAN_POINT('Ctrl Pts',(-4.73074760289381,26.,-6.33660740118367));
#451968=CARTESIAN_POINT('Ctrl Pts',(-4.69903040807827,26.,-6.2993117799316));
#451969=CARTESIAN_POINT('Ctrl Pts',(-4.67944112178507,26.,-6.27627712612825));
#451970=CARTESIAN_POINT('Ctrl Pts',(-4.6608380098351,26.,-6.25244551912277));
#451971=CARTESIAN_POINT('Ctrl Pts',(-4.64328815682614,26.,-6.22785054805505));
#451972=CARTESIAN_POINT('Ctrl Pts',(-4.61561379199964,26.,-6.1890667359127));
#451973=CARTESIAN_POINT('Ctrl Pts',(-4.59055615782454,26.,-6.14838638392196));
#451974=CARTESIAN_POINT('Ctrl Pts',(-4.56810357334094,26.,-6.10609561292346));
#451975=CARTESIAN_POINT('Ctrl Pts',(-4.56308085570443,26.,-6.09663502714943));
#451976=CARTESIAN_POINT('Ctrl Pts',(-4.55818866061037,26.,-6.08709371892498));
#451977=CARTESIAN_POINT('Ctrl Pts',(-4.55342713548155,26.,-6.07747468177979));
#451978=CARTESIAN_POINT('Ctrl Pts',(-4.54941744650604,26.,-6.0693744730961));
#451979=CARTESIAN_POINT('Ctrl Pts',(-4.54550147490024,26.,-6.06122106950204));
#451980=CARTESIAN_POINT('Ctrl Pts',(-4.54168378413711,26.,-6.05302670560328));
#451981=CARTESIAN_POINT('Ctrl Pts',(-4.52091202527692,26.,-6.00844180821941));
#451982=CARTESIAN_POINT('Ctrl Pts',(-4.50300515309595,26.,-5.96256452473651));
#451983=CARTESIAN_POINT('Ctrl Pts',(-4.487914241998,26.,-5.91572767775144));
#451984=CARTESIAN_POINT('Ctrl Pts',(-4.47244578989431,26.,-5.86771907710606));
#451985=CARTESIAN_POINT('Ctrl Pts',(-4.45993552318657,26.,-5.81870139486759));
#451986=CARTESIAN_POINT('Ctrl Pts',(-4.45037293016473,26.,-5.76899658983482));
#451987=CARTESIAN_POINT('Ctrl Pts',(-4.44466425311925,26.,-5.73932381395779));
#451988=CARTESIAN_POINT('Ctrl Pts',(-4.44000691734968,26.,-5.70940552485939));
#451989=CARTESIAN_POINT('Ctrl Pts',(-4.43640656180728,26.,-5.67930640361527));
#451990=CARTESIAN_POINT('Ctrl Pts',(-4.43442388277574,26.,-5.66273112490856));
#451991=CARTESIAN_POINT('Ctrl Pts',(-4.43276184947206,26.,-5.64610096883273));
#451992=CARTESIAN_POINT('Ctrl Pts',(-4.43142221200557,26.,-5.62942654610346));
#451993=CARTESIAN_POINT('Ctrl Pts',(-4.43069136328561,26.,-5.62032969653584));
#451994=CARTESIAN_POINT('Ctrl Pts',(-4.43005669150386,26.,-5.61122148289879));
#451995=CARTESIAN_POINT('Ctrl Pts',(-4.42951879017273,26.,-5.60211289271274));
#451996=CARTESIAN_POINT('Ctrl Pts',(-4.42641588965533,26.,-5.54956970762436));
#451997=CARTESIAN_POINT('Ctrl Pts',(-4.42652201105763,26.,-5.49693047124056));
#451998=CARTESIAN_POINT('Ctrl Pts',(-4.42983270797924,26.,-5.44453981441821));
#451999=CARTESIAN_POINT('Ctrl Pts',(-4.43208820455486,26.,-5.40884734547433));
#452000=CARTESIAN_POINT('Ctrl Pts',(-4.43583203037426,26.,-5.3732696381252));
#452001=CARTESIAN_POINT('Ctrl Pts',(-4.4410761904634,26.,-5.33791219832296));
#452002=CARTESIAN_POINT('Ctrl Pts',(-4.44350332624102,26.,-5.32154784145933));
#452003=CARTESIAN_POINT('Ctrl Pts',(-4.44625314527617,26.,-5.30522572113897));
#452004=CARTESIAN_POINT('Ctrl Pts',(-4.44932134384929,26.,-5.28898643069871));
#452005=CARTESIAN_POINT('Ctrl Pts',(-4.45918506318114,26.,-5.23677996516729));
#452006=CARTESIAN_POINT('Ctrl Pts',(-4.47234120945108,26.,-5.18537728351545));
#452007=CARTESIAN_POINT('Ctrl Pts',(-4.48880818879675,26.,-5.1351194619031));
#452008=CARTESIAN_POINT('Ctrl Pts',(-4.49754364477762,26.,-5.10845853161507));
#452009=CARTESIAN_POINT('Ctrl Pts',(-4.50721166236153,26.,-5.08211963725401));
#452010=CARTESIAN_POINT('Ctrl Pts',(-4.51782098438609,26.,-5.05615381819268));
#452011=CARTESIAN_POINT('Ctrl Pts',(-4.52387352626206,26.,-5.0413405052544));
#452012=CARTESIAN_POINT('Ctrl Pts',(-4.53023250440261,26.,-5.02664862375098));
#452013=CARTESIAN_POINT('Ctrl Pts',(-4.53689020456271,26.,-5.01208247494515));
#452014=CARTESIAN_POINT('Ctrl Pts',(4.53900700771688,26.,-5.01302286563431));
#452015=CARTESIAN_POINT('Ctrl Pts',(4.51730428611638,26.,-5.06076150603835));
#452016=CARTESIAN_POINT('Ctrl Pts',(4.49883681289365,26.,-5.10974961966388));
#452017=CARTESIAN_POINT('Ctrl Pts',(4.48353831525793,26.,-5.1596701907311));
#452018=CARTESIAN_POINT('Ctrl Pts',(4.46806176041948,26.,-5.21017178076207));
#452019=CARTESIAN_POINT('Ctrl Pts',(4.45582849042805,26.,-5.26162887990392));
#452020=CARTESIAN_POINT('Ctrl Pts',(4.44682362697344,26.,-5.31372001428598));
#452021=CARTESIAN_POINT('Ctrl Pts',(4.44031095795732,26.,-5.35139435755779));
#452022=CARTESIAN_POINT('Ctrl Pts',(4.43548811807635,26.,-5.38940054503579));
#452023=CARTESIAN_POINT('Ctrl Pts',(4.43236615256969,26.,-5.42761365593355));
#452024=CARTESIAN_POINT('Ctrl Pts',(4.43102893301352,26.,-5.44398133170877));
#452025=CARTESIAN_POINT('Ctrl Pts',(4.43000393185811,26.,-5.46038690932955));
#452026=CARTESIAN_POINT('Ctrl Pts',(4.42929277127871,26.,-5.47682022646686));
#452027=CARTESIAN_POINT('Ctrl Pts',(4.4288531707162,26.,-5.48697840405261));
#452028=CARTESIAN_POINT('Ctrl Pts',(4.42853358462845,26.,-5.49714835623362));
#452029=CARTESIAN_POINT('Ctrl Pts',(4.42833449333953,26.,-5.50731025740424));
#452030=CARTESIAN_POINT('Ctrl Pts',(4.42732475353669,26.,-5.5588488060778));
#452031=CARTESIAN_POINT('Ctrl Pts',(4.42940473009627,26.,-5.61028393904341));
#452032=CARTESIAN_POINT('Ctrl Pts',(4.43455229706759,26.,-5.66131493504129));
#452033=CARTESIAN_POINT('Ctrl Pts',(4.43958244593392,26.,-5.71118189317826));
#452034=CARTESIAN_POINT('Ctrl Pts',(4.44754223429228,26.,-5.76066393975029));
#452035=CARTESIAN_POINT('Ctrl Pts',(4.45845673166055,26.,-5.80946415691505));
#452036=CARTESIAN_POINT('Ctrl Pts',(4.4660505045795,26.,-5.84341695886652));
#452037=CARTESIAN_POINT('Ctrl Pts',(4.47507550289942,26.,-5.87703937807783));
#452038=CARTESIAN_POINT('Ctrl Pts',(4.48555225879131,26.,-5.91022284174077));
#452039=CARTESIAN_POINT('Ctrl Pts',(4.48925171874697,26.,-5.92194029476516));
#452040=CARTESIAN_POINT('Ctrl Pts',(4.49313228205386,26.,-5.93360293701868));
#452041=CARTESIAN_POINT('Ctrl Pts',(4.49719513448679,26.,-5.94520571072346));
#452042=CARTESIAN_POINT('Ctrl Pts',(4.50019561119532,26.,-5.95377453098711));
#452043=CARTESIAN_POINT('Ctrl Pts',(4.50329523564298,26.,-5.9623096149553));
#452044=CARTESIAN_POINT('Ctrl Pts',(4.50648983139489,26.,-5.9707974074509));
#452045=CARTESIAN_POINT('Ctrl Pts',(4.52352595486226,26.,-6.01606106274569));
#452046=CARTESIAN_POINT('Ctrl Pts',(4.5432905285082,26.,-6.06007213720631));
#452047=CARTESIAN_POINT('Ctrl Pts',(4.5657969891543,26.,-6.10256102530468));
#452048=CARTESIAN_POINT('Ctrl Pts',(4.5819069696728,26.,-6.13297429953205));
#452049=CARTESIAN_POINT('Ctrl Pts',(4.59942271301779,26.,-6.16260727985433));
#452050=CARTESIAN_POINT('Ctrl Pts',(4.61836202894701,26.,-6.1913507700685));
#452051=CARTESIAN_POINT('Ctrl Pts',(4.64360162105055,26.,-6.22965595338923));
#452052=CARTESIAN_POINT('Ctrl Pts',(4.67136946042345,26.,-6.26638275459849));
#452053=CARTESIAN_POINT('Ctrl Pts',(4.70144469586272,26.,-6.30137698491027));
#452054=CARTESIAN_POINT('Ctrl Pts',(4.7093750755801,26.,-6.31060442836122));
#452055=CARTESIAN_POINT('Ctrl Pts',(4.71746597339321,26.,-6.31971121578822));
#452056=CARTESIAN_POINT('Ctrl Pts',(4.72571349227094,26.,-6.32869409556094));
#452057=CARTESIAN_POINT('Ctrl Pts',(4.73193320898236,26.,-6.33546837134828));
#452058=CARTESIAN_POINT('Ctrl Pts',(4.73824213429154,26.,-6.34217214625989));
#452059=CARTESIAN_POINT('Ctrl Pts',(4.74462823868703,26.,-6.34879370707138));
#452060=CARTESIAN_POINT('Ctrl Pts',(4.77811675594523,26.,-6.38351694987776));
#452061=CARTESIAN_POINT('Ctrl Pts',(4.81379250852302,26.,-6.41605753628488));
#452062=CARTESIAN_POINT('Ctrl Pts',(4.85136909773509,26.,-6.44627580179103));
#452063=CARTESIAN_POINT('Ctrl Pts',(4.88884303451388,26.,-6.47641151647102));
#452064=CARTESIAN_POINT('Ctrl Pts',(4.92820865020652,26.,-6.50423803830216));
#452065=CARTESIAN_POINT('Ctrl Pts',(4.96920312732498,26.,-6.529570200706));
#452066=CARTESIAN_POINT('Ctrl Pts',(4.99115415974213,26.,-6.54313464053326));
#452067=CARTESIAN_POINT('Ctrl Pts',(5.01357247300154,26.,-6.55598305842276));
#452068=CARTESIAN_POINT('Ctrl Pts',(5.0364184192413,26.,-6.5680808187856));
#452069=CARTESIAN_POINT('Ctrl Pts',(5.04828493019454,26.,-6.57436456839916));
#452070=CARTESIAN_POINT('Ctrl Pts',(5.06026681279923,26.,-6.58044572293759));
#452071=CARTESIAN_POINT('Ctrl Pts',(5.07235847248755,26.,-6.58631893168919));
#452072=CARTESIAN_POINT('Ctrl Pts',(5.08162063378941,26.,-6.59081778529731));
#452073=CARTESIAN_POINT('Ctrl Pts',(5.09094758398249,26.,-6.59519465263342));
#452074=CARTESIAN_POINT('Ctrl Pts',(5.10032287206098,26.,-6.59944110226853));
#452075=CARTESIAN_POINT('Ctrl Pts',(5.14250847566835,26.,-6.61854867950197));
#452076=CARTESIAN_POINT('Ctrl Pts',(5.18574009198917,26.,-6.63505331108929));
#452077=CARTESIAN_POINT('Ctrl Pts',(5.22977562430468,26.,-6.64877678420517));
#452078=CARTESIAN_POINT('Ctrl Pts',(5.25948043967676,26.,-6.65803415464525));
#452079=CARTESIAN_POINT('Ctrl Pts',(5.28955126497656,26.,-6.66602500920764));
#452080=CARTESIAN_POINT('Ctrl Pts',(5.31991283788441,26.,-6.67268119203775));
#452081=CARTESIAN_POINT('Ctrl Pts',(5.33301953805478,26.,-6.6755545804784));
#452082=CARTESIAN_POINT('Ctrl Pts',(5.34618251315033,26.,-6.67817927294514));
#452083=CARTESIAN_POINT('Ctrl Pts',(5.35937322812986,26.,-6.68054575322537));
#452084=CARTESIAN_POINT('Ctrl Pts',(5.40277073098025,26.,-6.68833148241942));
#452085=CARTESIAN_POINT('Ctrl Pts',(5.44652175700321,26.,-6.69333871127465));
#452086=CARTESIAN_POINT('Ctrl Pts',(5.49040691012916,26.,-6.69538344663484));
#452087=CARTESIAN_POINT('Ctrl Pts',(5.51211121369546,26.,-6.69639471249149));
#452088=CARTESIAN_POINT('Ctrl Pts',(5.53384821036422,26.,-6.69668059243965));
#452089=CARTESIAN_POINT('Ctrl Pts',(5.55559016156262,26.,-6.69621420261903));
#452090=CARTESIAN_POINT('Ctrl Pts',(5.56854309351446,26.,-6.69593634735414));
#452091=CARTESIAN_POINT('Ctrl Pts',(5.58149776570054,26.,-6.69539142062068));
#452092=CARTESIAN_POINT('Ctrl Pts',(5.59444726164187,26.,-6.69458228414866));
#452093=CARTESIAN_POINT('Ctrl Pts',(6.69274404704181,26.,-5.59475217632212));
#452094=CARTESIAN_POINT('Ctrl Pts',(6.69531021368757,26.,-5.55137724984312));
#452095=CARTESIAN_POINT('Ctrl Pts',(6.69492058849835,26.,-5.50802061877154));
#452096=CARTESIAN_POINT('Ctrl Pts',(6.69178524360462,26.,-5.46490197494242));
#452097=CARTESIAN_POINT('Ctrl Pts',(6.6885064316043,26.,-5.41981030827848));
#452098=CARTESIAN_POINT('Ctrl Pts',(6.6822250250606,26.,-5.37497811568631));
#452099=CARTESIAN_POINT('Ctrl Pts',(6.67312701402814,26.,-5.33063916085636));
#452100=CARTESIAN_POINT('Ctrl Pts',(6.66611881409995,26.,-5.29648485405827));
#452101=CARTESIAN_POINT('Ctrl Pts',(6.657438192268,26.,-5.26262271564402));
#452102=CARTESIAN_POINT('Ctrl Pts',(6.64714921184178,26.,-5.22915790417526));
#452103=CARTESIAN_POINT('Ctrl Pts',(6.64373212641031,26.,-5.21804386614623));
#452104=CARTESIAN_POINT('Ctrl Pts',(6.6401374992052,26.,-5.20697366153317));
#452105=CARTESIAN_POINT('Ctrl Pts',(6.63636725693996,26.,-5.19595119721186));
#452106=CARTESIAN_POINT('Ctrl Pts',(6.63377142477236,26.,-5.18836217097996));
#452107=CARTESIAN_POINT('Ctrl Pts',(6.63109312211646,26.,-5.18079825592472));
#452108=CARTESIAN_POINT('Ctrl Pts',(6.62833627014149,26.,-5.17326885671329));
#452109=CARTESIAN_POINT('Ctrl Pts',(6.61217427936374,26.,-5.12912790111545));
#452110=CARTESIAN_POINT('Ctrl Pts',(6.59328942012651,26.,-5.08609247724548));
#452111=CARTESIAN_POINT('Ctrl Pts',(6.57188267764938,26.,-5.04440658615065));
#452112=CARTESIAN_POINT('Ctrl Pts',(6.55005077177248,26.,-5.00189276361322));
#452113=CARTESIAN_POINT('Ctrl Pts',(6.52559561389071,26.,-4.96078147223418));
#452114=CARTESIAN_POINT('Ctrl Pts',(6.49867698456061,26.,-4.92133403647713));
#452115=CARTESIAN_POINT('Ctrl Pts',(6.48030858576068,26.,-4.89441638689199));
#452116=CARTESIAN_POINT('Ctrl Pts',(6.46079201276668,26.,-4.86827351988104));
#452117=CARTESIAN_POINT('Ctrl Pts',(6.44016501436062,26.,-4.84299340464255));
#452118=CARTESIAN_POINT('Ctrl Pts',(6.43429026416939,26.,-4.83579340593657));
#452119=CARTESIAN_POINT('Ctrl Pts',(6.42832537886577,26.,-4.82866342675214));
#452120=CARTESIAN_POINT('Ctrl Pts',(6.42227108594394,26.,-4.82160559613751));
#452121=CARTESIAN_POINT('Ctrl Pts',(6.41650773035309,26.,-4.81488692757334));
#452122=CARTESIAN_POINT('Ctrl Pts',(6.41066935805872,26.,-4.80824066121229));
#452123=CARTESIAN_POINT('Ctrl Pts',(6.40475816448007,26.,-4.80166944019842));
#452124=CARTESIAN_POINT('Ctrl Pts',(6.37181648000639,26.,-4.76504957885134));
#452125=CARTESIAN_POINT('Ctrl Pts',(6.33660740112027,26.,-4.73074760283477));
#452126=CARTESIAN_POINT('Ctrl Pts',(6.29931177986584,26.,-4.69903040802235));
#452127=CARTESIAN_POINT('Ctrl Pts',(6.27627712608289,26.,-4.67944112174966));
#452128=CARTESIAN_POINT('Ctrl Pts',(6.25244551909937,26.,-4.6608380098184));
#452129=CARTESIAN_POINT('Ctrl Pts',(6.22785054805505,26.,-4.64328815682614));
#452130=CARTESIAN_POINT('Ctrl Pts',(6.18906673591271,26.,-4.61561379199964));
#452131=CARTESIAN_POINT('Ctrl Pts',(6.14838638392197,26.,-4.59055615782454));
#452132=CARTESIAN_POINT('Ctrl Pts',(6.10609561292348,26.,-4.56810357334095));
#452133=CARTESIAN_POINT('Ctrl Pts',(6.0966350271458,26.,-4.5630808557025));
#452134=CARTESIAN_POINT('Ctrl Pts',(6.08709371891765,26.,-4.55818866060661));
#452135=CARTESIAN_POINT('Ctrl Pts',(6.0774746817687,26.,-4.55342713547606));
#452136=CARTESIAN_POINT('Ctrl Pts',(6.06937447308074,26.,-4.54941744649855));
#452137=CARTESIAN_POINT('Ctrl Pts',(6.06122106948236,26.,-4.54550147489084));
#452138=CARTESIAN_POINT('Ctrl Pts',(6.05302670557925,26.,-4.54168378412591));
#452139=CARTESIAN_POINT('Ctrl Pts',(6.00844180819483,26.,-4.52091202526671));
#452140=CARTESIAN_POINT('Ctrl Pts',(5.96256452471144,26.,-4.50300515308674));
#452141=CARTESIAN_POINT('Ctrl Pts',(5.91572767772593,26.,-4.48791424198978));
#452142=CARTESIAN_POINT('Ctrl Pts',(5.86771907707987,26.,-4.47244578988703));
#452143=CARTESIAN_POINT('Ctrl Pts',(5.81870139484075,26.,-4.45993552318027));
#452144=CARTESIAN_POINT('Ctrl Pts',(5.76899658980738,26.,-4.45037293015945));
#452145=CARTESIAN_POINT('Ctrl Pts',(5.73932381393135,26.,-4.44466425311484));
#452146=CARTESIAN_POINT('Ctrl Pts',(5.70940552483398,26.,-4.44000691734606));
#452147=CARTESIAN_POINT('Ctrl Pts',(5.67930640359092,26.,-4.43640656180437));
#452148=CARTESIAN_POINT('Ctrl Pts',(5.66273112487801,26.,-4.43442388277241));
#452149=CARTESIAN_POINT('Ctrl Pts',(5.64610096879595,26.,-4.43276184946854));
#452150=CARTESIAN_POINT('Ctrl Pts',(5.62942654606042,26.,-4.43142221200212));
#452151=CARTESIAN_POINT('Ctrl Pts',(5.62032969647973,26.,-4.43069136328141));
#452152=CARTESIAN_POINT('Ctrl Pts',(5.61122148282963,26.,-4.4300566914992));
#452153=CARTESIAN_POINT('Ctrl Pts',(5.60211289263051,26.,-4.42951879016787));
#452154=CARTESIAN_POINT('Ctrl Pts',(5.54956970754168,26.,-4.4264158896538));
#452155=CARTESIAN_POINT('Ctrl Pts',(5.49693047115761,26.,-4.42652201105946));
#452156=CARTESIAN_POINT('Ctrl Pts',(5.44453981433516,26.,-4.42983270798449));
#452157=CARTESIAN_POINT('Ctrl Pts',(5.40884734538101,26.,-4.43208820456308));
#452158=CARTESIAN_POINT('Ctrl Pts',(5.37326963802174,26.,-4.43583203038632));
#452159=CARTESIAN_POINT('Ctrl Pts',(5.3379121982096,26.,-4.44107619048022));
#452160=CARTESIAN_POINT('Ctrl Pts',(5.32154784137259,26.,-4.4435033262554));
#452161=CARTESIAN_POINT('Ctrl Pts',(5.30522572107876,26.,-4.44625314528708));
#452162=CARTESIAN_POINT('Ctrl Pts',(5.2889864306648,26.,-4.4493213438557));
#452163=CARTESIAN_POINT('Ctrl Pts',(5.23677996513386,26.,-4.45918506318895));
#452164=CARTESIAN_POINT('Ctrl Pts',(5.18537728348257,26.,-4.47234120946028));
#452165=CARTESIAN_POINT('Ctrl Pts',(5.13511946187084,26.,-4.48880818880732));
#452166=CARTESIAN_POINT('Ctrl Pts',(5.10845853159382,26.,-4.49754364478542));
#452167=CARTESIAN_POINT('Ctrl Pts',(5.08211963724353,26.,-4.50721166236581));
#452168=CARTESIAN_POINT('Ctrl Pts',(5.05615381819268,26.,-4.51782098438608));
#452169=CARTESIAN_POINT('Ctrl Pts',(5.0413405052544,26.,-4.52387352626206));
#452170=CARTESIAN_POINT('Ctrl Pts',(5.02664862375098,26.,-4.53023250440261));
#452171=CARTESIAN_POINT('Ctrl Pts',(5.01208247494515,26.,-4.53689020456271));
#452172=CARTESIAN_POINT('Origin',(5.65685387860011,26.993675081176,5.65685387860011));
#452173=CARTESIAN_POINT('Ctrl Pts',(6.57057130100612,25.868675081176,4.74432962138981));
#452174=CARTESIAN_POINT('Ctrl Pts',(6.60882993708831,25.8656848283261,4.78199706987976));
#452175=CARTESIAN_POINT('Ctrl Pts',(6.92960341635462,25.8388668852448,5.14157728587623));
#452176=CARTESIAN_POINT('Ctrl Pts',(7.09568592881682,25.7882212519322,6.16255878293893));
#452177=CARTESIAN_POINT('Ctrl Pts',(6.01152748645437,25.716738181238,7.13997732676548));
#452178=CARTESIAN_POINT('Ctrl Pts',(4.60259286076204,25.6452551105438,6.75873746207651));
#452179=CARTESIAN_POINT('Ctrl Pts',(4.15947051927595,25.5737720398497,5.36788602689621));
#452180=CARTESIAN_POINT('Ctrl Pts',(5.0882746237623,25.5022889691555,4.24182426511434));
#452181=CARTESIAN_POINT('Ctrl Pts',(6.13675122222029,25.450589982931,4.36502559631504));
#452182=CARTESIAN_POINT('Ctrl Pts',(6.51790892062316,25.4227186869378,4.69148744470697));
#452183=CARTESIAN_POINT('Ctrl Pts',(6.56885365284802,25.418675081176,4.74334636410459));
#452184=CARTESIAN_POINT('Ctrl Pts',(6.56704169373441,25.906324918824,4.74450601134849));
#452185=CARTESIAN_POINT('Ctrl Pts',(6.7750658664325,25.8898945654199,4.9557394479142));
#452186=CARTESIAN_POINT('Ctrl Pts',(7.11639071403833,25.8496365217844,5.64807137163849));
#452187=CARTESIAN_POINT('Ctrl Pts',(6.60321033464885,25.7855507879174,6.8522203629011));
#452188=CARTESIAN_POINT('Ctrl Pts',(5.16550356767203,25.7140677172233,7.1004834147237));
#452189=CARTESIAN_POINT('Ctrl Pts',(4.17707919799325,25.6425846465291,6.0259636415713));
#452190=CARTESIAN_POINT('Ctrl Pts',(4.5448553014618,25.5711015758349,4.61334644908231));
#452191=CARTESIAN_POINT('Ctrl Pts',(5.74896333949311,25.5090149999332,4.21675923787012));
#452192=CARTESIAN_POINT('Ctrl Pts',(6.3830054663296,25.4707561142629,4.5629353888518));
#452193=CARTESIAN_POINT('Ctrl Pts',(6.56829321884323,25.456324918824,4.74640124271564));
#452194=CARTESIAN_POINT('Ctrl Pts',(5.59475217632212,26.,6.69274404704181));
#452195=CARTESIAN_POINT('Ctrl Pts',(5.25011429538726,25.9761723097686,6.67208297724159));
#452196=CARTESIAN_POINT('Ctrl Pts',(4.58904744425369,25.9285169293058,6.25991935236784));
#452197=CARTESIAN_POINT('Ctrl Pts',(4.57111450891619,25.8570338586116,5.08408179813166));
#452198=CARTESIAN_POINT('Ctrl Pts',(5.55001366141289,25.7855507879175,4.43501771280631));
#452199=CARTESIAN_POINT('Ctrl Pts',(6.62575617389683,25.7140677172233,4.90440858615388));
#452200=CARTESIAN_POINT('Ctrl Pts',(6.81433291744693,25.6425846465291,6.06367191307887));
#452201=CARTESIAN_POINT('Ctrl Pts',(5.94217367437589,25.5711015758349,6.8499634587037));
#452202=CARTESIAN_POINT('Ctrl Pts',(4.80874583886255,25.4996185051408,6.54327224197424));
#452203=CARTESIAN_POINT('Ctrl Pts',(4.45227280794999,25.4281354344466,5.42439156223909));
#452204=CARTESIAN_POINT('Ctrl Pts',(5.19945610983427,25.3566523637524,4.51852288527076));
#452205=CARTESIAN_POINT('Ctrl Pts',(6.36568271985868,25.2851692930583,4.65556044151952));
#452206=CARTESIAN_POINT('Ctrl Pts',(6.88249940298929,25.213686222364,5.70997789504277));
#452207=CARTESIAN_POINT('Ctrl Pts',(6.27639179734011,25.1422031516699,6.71571945020394));
#452208=CARTESIAN_POINT('Ctrl Pts',(5.10267450019953,25.0707200809757,6.7513451989237));
#452209=CARTESIAN_POINT('Ctrl Pts',(4.43668748453226,24.9992370102815,5.78421192833874));
#452210=CARTESIAN_POINT('Ctrl Pts',(4.88860074260097,24.9277539395873,4.7003955508837));
#452211=CARTESIAN_POINT('Ctrl Pts',(6.04437662247732,24.8562708688931,4.49287282235237));
#452212=CARTESIAN_POINT('Ctrl Pts',(6.84510966506768,24.784787798199,5.35177365831406));
#452213=CARTESIAN_POINT('Ctrl Pts',(6.55717903824976,24.7133047275048,6.49018471285717));
#452214=CARTESIAN_POINT('Ctrl Pts',(5.44438294256281,24.6418216568106,6.86510957377001));
#452215=CARTESIAN_POINT('Ctrl Pts',(4.52624977050191,24.5703385861164,6.13304718756447));
#452216=CARTESIAN_POINT('Ctrl Pts',(4.64396052187117,24.4988555154223,4.96470306042394));
#452217=CARTESIAN_POINT('Ctrl Pts',(5.68967021074952,24.4273724447281,4.43049797487471));
#452218=CARTESIAN_POINT('Ctrl Pts',(6.70531403099034,24.3558893740339,5.01986328076134));
#452219=CARTESIAN_POINT('Ctrl Pts',(6.76037309820141,24.2844063033397,6.19283059794665));
#452220=CARTESIAN_POINT('Ctrl Pts',(5.80440305573226,24.2129232326455,6.87474342740735));
#452221=CARTESIAN_POINT('Ctrl Pts',(4.71325048867858,24.1414401619514,6.44084262551864));
#452222=CARTESIAN_POINT('Ctrl Pts',(4.48661435222159,24.0699570912572,5.28866213152759));
#452223=CARTESIAN_POINT('Ctrl Pts',(5.33213555135881,23.9984740205631,4.47381384511066));
#452224=CARTESIAN_POINT('Ctrl Pts',(6.47515921171813,23.9269909498688,4.74285054378755));
#452225=CARTESIAN_POINT('Ctrl Pts',(6.86846279219781,23.8555078791747,5.84928450947304));
#452226=CARTESIAN_POINT('Ctrl Pts',(6.15170698086798,23.7840248084805,6.77941618151556));
#452227=CARTESIAN_POINT('Ctrl Pts',(4.98157355760958,23.7125417377863,6.68107173221035));
#452228=CARTESIAN_POINT('Ctrl Pts',(4.43012269359922,23.6410586670921,5.64435299191054));
#452229=CARTESIAN_POINT('Ctrl Pts',(5.00258598787076,23.569575596398,4.61908739135743));
#452230=CARTESIAN_POINT('Ctrl Pts',(6.17448062637044,23.4980925257038,4.54460915448657));
#452231=CARTESIAN_POINT('Ctrl Pts',(6.87213254456038,23.4266094550096,5.48915421344717));
#452232=CARTESIAN_POINT('Ctrl Pts',(6.45636332421143,23.3551263843154,6.5873433994568));
#452233=CARTESIAN_POINT('Ctrl Pts',(5.30809370313679,23.2836433136213,6.8330308949199));
#452234=CARTESIAN_POINT('Ctrl Pts',(4.47935503415496,23.212160242927,6.00112122066856));
#452235=CARTESIAN_POINT('Ctrl Pts',(4.72942128924326,23.1406771722329,4.85379852261456));
#452236=CARTESIAN_POINT('Ctrl Pts',(5.82919498069919,23.0691941015387,4.44222413342345));
#452237=CARTESIAN_POINT('Ctrl Pts',(6.77105943752211,22.9977110308445,5.14347668616413));
#452238=CARTESIAN_POINT('Ctrl Pts',(6.69212899367236,22.9262279601504,6.31507855179966));
#452239=CARTESIAN_POINT('Ctrl Pts',(5.66464494341573,22.8547448894562,6.88362364563197));
#452240=CARTESIAN_POINT('Ctrl Pts',(4.63011853598606,22.783261818762,6.32821994284799));
#452241=CARTESIAN_POINT('Ctrl Pts',(4.53608521045973,22.7117787480678,5.15771839492687));
#452242=CARTESIAN_POINT('Ctrl Pts',(5.46925286619012,22.6402956773736,4.4445208236608));
#452243=CARTESIAN_POINT('Ctrl Pts',(6.57357515235991,22.5688126066795,4.84204067651847));
#452244=CARTESIAN_POINT('Ctrl Pts',(6.8394368280484,22.4973295359852,5.98608844956735));
#452245=CARTESIAN_POINT('Ctrl Pts',(6.01893246982621,22.4258464652911,6.82851835303725));
#452246=CARTESIAN_POINT('Ctrl Pts',(5.25534692011694,22.3781910848283,6.67416374956871));
#452247=CARTESIAN_POINT('Ctrl Pts',(4.99063298333217,22.3543633945969,6.45251384441992));
#452248=CARTESIAN_POINT('Ctrl Pts',(5.58972040746333,26.0485455351344,6.77667668816907));
#452249=CARTESIAN_POINT('Ctrl Pts',(5.21715836192049,26.024717844903,6.75434156236399));
#452250=CARTESIAN_POINT('Ctrl Pts',(4.50252879876621,25.9770624644402,6.30878252293169));
#452251=CARTESIAN_POINT('Ctrl Pts',(4.4831428535712,25.905579393746,5.03767313923882));
#452252=CARTESIAN_POINT('Ctrl Pts',(5.54135696992154,25.8340963230518,4.33601886182374));
#452253=CARTESIAN_POINT('Ctrl Pts',(6.70426114586778,25.7626132523576,4.84344196766209));
#452254=CARTESIAN_POINT('Ctrl Pts',(6.90811725457023,25.6911301816635,6.09663420303223));
#452255=CARTESIAN_POINT('Ctrl Pts',(5.96529161173539,25.6196471109693,6.94663474805762));
#452256=CARTESIAN_POINT('Ctrl Pts',(4.7400281794957,25.5481640402751,6.61509398200833));
#452257=CARTESIAN_POINT('Ctrl Pts',(4.35467204505866,25.4766809695809,5.40555638379146));
#452258=CARTESIAN_POINT('Ctrl Pts',(5.16239561447694,25.4051978988867,4.42629001188529));
#452259=CARTESIAN_POINT('Ctrl Pts',(6.42311533054124,25.3337148281926,4.57443098853515));
#452260=CARTESIAN_POINT('Ctrl Pts',(6.98180690592903,25.2622317574984,5.71428225002475));
#452261=CARTESIAN_POINT('Ctrl Pts',(6.32658964203686,25.1907486868042,6.80151366539291));
#452262=CARTESIAN_POINT('Ctrl Pts',(5.05777230853438,25.11926561611,6.84002597802966));
#452263=CARTESIAN_POINT('Ctrl Pts',(4.33782392622387,25.0477825454159,5.79453107008661));
#452264=CARTESIAN_POINT('Ctrl Pts',(4.82635329907546,24.9762994747217,4.62289884706407));
#452265=CARTESIAN_POINT('Ctrl Pts',(6.07577551821105,24.9048164040275,4.39856166152736));
#452266=CARTESIAN_POINT('Ctrl Pts',(6.94138767747801,24.8333333333333,5.32705463942152));
#452267=CARTESIAN_POINT('Ctrl Pts',(6.63012757162215,24.7618502626391,6.55770505428216));
#452268=CARTESIAN_POINT('Ctrl Pts',(5.42716755876279,24.690367191945,6.96300807183686));
#452269=CARTESIAN_POINT('Ctrl Pts',(4.4346429653087,24.6188841212508,6.17163058503857));
#452270=CARTESIAN_POINT('Ctrl Pts',(4.56189118942602,24.5474010505566,4.90862178076926));
#452271=CARTESIAN_POINT('Ctrl Pts',(5.69232914266462,24.4759179798625,4.33113291369596));
#452272=CARTESIAN_POINT('Ctrl Pts',(6.79026515070139,24.4044349091683,4.96825133880203));
#452273=CARTESIAN_POINT('Ctrl Pts',(6.84978535971091,24.3329518384741,6.23625792548383));
#452274=CARTESIAN_POINT('Ctrl Pts',(5.81635817656469,24.2614687677799,6.97342250511928));
#452275=CARTESIAN_POINT('Ctrl Pts',(4.63679535172919,24.1899856970857,6.50436504145382));
#452276=CARTESIAN_POINT('Ctrl Pts',(4.39179610102783,24.1185026263916,5.2588295230962));
#452277=CARTESIAN_POINT('Ctrl Pts',(5.30582536167067,24.0470195556974,4.37795843727393));
#452278=CARTESIAN_POINT('Ctrl Pts',(6.54146211713177,23.9755364850032,4.66879374102307));
#452279=CARTESIAN_POINT('Ctrl Pts',(6.96663298362319,23.904053414309,5.86487613450725));
#452280=CARTESIAN_POINT('Ctrl Pts',(6.19180228161384,23.8325703436148,6.8703714022368));
#452281=CARTESIAN_POINT('Ctrl Pts',(4.92685920413015,23.7610872729207,6.76405862808226));
#452282=CARTESIAN_POINT('Ctrl Pts',(4.33072722538547,23.6896042022265,5.64334011190815));
#452283=CARTESIAN_POINT('Ctrl Pts',(4.94957415925549,23.6181211315323,4.53500272215098));
#452284=CARTESIAN_POINT('Ctrl Pts',(6.21642115383373,23.5466380608381,4.45448991200439));
#452285=CARTESIAN_POINT('Ctrl Pts',(6.97060007639641,23.475154990144,5.47556640632123));
#452286=CARTESIAN_POINT('Ctrl Pts',(6.52114329936776,23.4036719194498,6.66273598971974));
#452287=CARTESIAN_POINT('Ctrl Pts',(5.27983553104633,23.3321888487556,6.92833022917403));
#452288=CARTESIAN_POINT('Ctrl Pts',(4.38394859923605,23.2607057780614,6.02901536249358));
#452289=CARTESIAN_POINT('Ctrl Pts',(4.6542763857934,23.1892227073672,4.78873124130167));
#452290=CARTESIAN_POINT('Ctrl Pts',(5.84315885864169,23.1177396366731,4.34380918016856));
#452291=CARTESIAN_POINT('Ctrl Pts',(6.86133755596364,23.0462565659789,5.1018804774459));
#452292=CARTESIAN_POINT('Ctrl Pts',(6.77601180031397,22.9747734952847,6.36841097734037));
#452293=CARTESIAN_POINT('Ctrl Pts',(5.66527621173653,22.9032904245905,6.98302223994139));
#452294=CARTESIAN_POINT('Ctrl Pts',(4.54692766144197,22.8318073538963,6.3826171450343));
#452295=CARTESIAN_POINT('Ctrl Pts',(4.4452753183732,22.7603242832022,5.11727611571493));
#452296=CARTESIAN_POINT('Ctrl Pts',(5.45405255931453,22.688841212508,4.34629195893472));
#452297=CARTESIAN_POINT('Ctrl Pts',(6.64785217518362,22.6173581418138,4.77602071980922));
#452298=CARTESIAN_POINT('Ctrl Pts',(6.93525520080945,22.5458750711197,6.01276456633487));
#452299=CARTESIAN_POINT('Ctrl Pts',(6.04826976192828,22.4743920004254,6.92345206015257));
#452300=CARTESIAN_POINT('Ctrl Pts',(5.22281495825156,22.4267366199627,6.75659092854625));
#452301=CARTESIAN_POINT('Ctrl Pts',(4.93665266667552,22.4029089297313,6.5169819168131));
#452302=CARTESIAN_POINT('Ctrl Pts',(5.58468863860454,26.0970910702687,6.86060932929632));
#452303=CARTESIAN_POINT('Ctrl Pts',(5.18420242845371,26.0732633800373,6.83660014748639));
#452304=CARTESIAN_POINT('Ctrl Pts',(4.41601015327873,26.0256079995746,6.35764569349554));
#452305=CARTESIAN_POINT('Ctrl Pts',(4.39517119822623,25.9541249288803,4.99126448034597));
#452306=CARTESIAN_POINT('Ctrl Pts',(5.53270027843017,25.8826418581862,4.23702001084117));
#452307=CARTESIAN_POINT('Ctrl Pts',(6.78276611783875,25.811158787492,4.7824753491703));
#452308=CARTESIAN_POINT('Ctrl Pts',(7.00190159169352,25.7396757167979,6.12959649298558));
#452309=CARTESIAN_POINT('Ctrl Pts',(5.98840954909488,25.6681926461036,7.04330603741155));
#452310=CARTESIAN_POINT('Ctrl Pts',(4.67131052012887,25.5967095754095,6.68691572204241));
#452311=CARTESIAN_POINT('Ctrl Pts',(4.2570712821673,25.5252265047153,5.38672120534384));
#452312=CARTESIAN_POINT('Ctrl Pts',(5.12533511911963,25.4537434340211,4.33405713849982));
#452313=CARTESIAN_POINT('Ctrl Pts',(6.48054794122378,25.382260363327,4.49330153555078));
#452314=CARTESIAN_POINT('Ctrl Pts',(7.0811144088688,25.3107772926328,5.71858660500674));
#452315=CARTESIAN_POINT('Ctrl Pts',(6.37678748673361,25.2392942219386,6.88730788058188));
#452316=CARTESIAN_POINT('Ctrl Pts',(5.01287011686923,25.1678111512444,6.92870675713562));
#452317=CARTESIAN_POINT('Ctrl Pts',(4.23896036791547,25.0963280805502,5.80485021183448));
#452318=CARTESIAN_POINT('Ctrl Pts',(4.76410585554996,25.0248450098561,4.54540214324445));
#452319=CARTESIAN_POINT('Ctrl Pts',(6.10717441394477,24.9533619391619,4.30425050070234));
#452320=CARTESIAN_POINT('Ctrl Pts',(7.03766568988833,24.8818788684677,5.302335620529));
#452321=CARTESIAN_POINT('Ctrl Pts',(6.70307610499455,24.8103957977735,6.62522539570715));
#452322=CARTESIAN_POINT('Ctrl Pts',(5.40995217496278,24.7389127270793,7.06090656990369));
#452323=CARTESIAN_POINT('Ctrl Pts',(4.34303616011548,24.6674296563851,6.21021398251268));
#452324=CARTESIAN_POINT('Ctrl Pts',(4.47982185698087,24.595946585691,4.85254050111457));
#452325=CARTESIAN_POINT('Ctrl Pts',(5.69498807457971,24.5244635149968,4.23176785251722));
#452326=CARTESIAN_POINT('Ctrl Pts',(6.87521627041245,24.4529804443027,4.91663939684271));
#452327=CARTESIAN_POINT('Ctrl Pts',(6.93919762122039,24.3814973736084,6.27968525302103));
#452328=CARTESIAN_POINT('Ctrl Pts',(5.82831329739714,24.3100143029143,7.07210158283119));
#452329=CARTESIAN_POINT('Ctrl Pts',(4.56034021477979,24.2385312322201,6.567887457389));
#452330=CARTESIAN_POINT('Ctrl Pts',(4.29697784983407,24.1670481615259,5.2289969146648));
#452331=CARTESIAN_POINT('Ctrl Pts',(5.27951517198252,24.0955650908318,4.28210302943719));
#452332=CARTESIAN_POINT('Ctrl Pts',(6.60776502254541,24.0240820201375,4.59473693825861));
#452333=CARTESIAN_POINT('Ctrl Pts',(7.06480317504856,23.9525989494434,5.88046775954144));
#452334=CARTESIAN_POINT('Ctrl Pts',(6.2318975823597,23.8811158787492,6.96132662295805));
#452335=CARTESIAN_POINT('Ctrl Pts',(4.87214485065071,23.809632808055,6.84704552395415));
#452336=CARTESIAN_POINT('Ctrl Pts',(4.23133175717171,23.7381497373609,5.64232723190575));
#452337=CARTESIAN_POINT('Ctrl Pts',(4.89656233064023,23.6666666666667,4.45091805294455));
#452338=CARTESIAN_POINT('Ctrl Pts',(6.258361681297,23.5951835959725,4.3643706695222));
#452339=CARTESIAN_POINT('Ctrl Pts',(7.06906760823243,23.5237005252783,5.46197859919531));
#452340=CARTESIAN_POINT('Ctrl Pts',(6.58592327452408,23.4522174545842,6.73812857998267));
#452341=CARTESIAN_POINT('Ctrl Pts',(5.25157735895588,23.3807343838899,7.02362956342815));
#452342=CARTESIAN_POINT('Ctrl Pts',(4.28854216431713,23.3092513131958,6.05690950431861));
#452343=CARTESIAN_POINT('Ctrl Pts',(4.57913148234355,23.2377682425016,4.72366395998878));
#452344=CARTESIAN_POINT('Ctrl Pts',(5.85712273658419,23.1662851718074,4.24539422691366));
#452345=CARTESIAN_POINT('Ctrl Pts',(6.95161567440517,23.0948021011132,5.06028426872769));
#452346=CARTESIAN_POINT('Ctrl Pts',(6.85989460695557,23.0233190304191,6.42174340288107));
#452347=CARTESIAN_POINT('Ctrl Pts',(5.66590748005734,22.9518359597249,7.0824208342508));
#452348=CARTESIAN_POINT('Ctrl Pts',(4.46373678689787,22.8803528890307,6.43701434722061));
#452349=CARTESIAN_POINT('Ctrl Pts',(4.35446542628666,22.8088698183366,5.07683383650298));
#452350=CARTESIAN_POINT('Ctrl Pts',(5.43885225243895,22.7373867476423,4.24806309420865));
#452351=CARTESIAN_POINT('Ctrl Pts',(6.72212919800732,22.6659036769482,4.71000076309996));
#452352=CARTESIAN_POINT('Ctrl Pts',(7.03107357357049,22.594420606254,6.0394406831024));
#452353=CARTESIAN_POINT('Ctrl Pts',(6.07760705403035,22.5229375355598,7.01838576726789));
#452354=CARTESIAN_POINT('Ctrl Pts',(5.19028299638618,22.475282155097,6.83901810752379));
#452355=CARTESIAN_POINT('Ctrl Pts',(4.88267235001886,22.4514544648656,6.58144998920627));
#452356=CARTESIAN_POINT('Ctrl Pts',(5.57965686974575,26.1456366054031,6.94454197042357));
#452357=CARTESIAN_POINT('Ctrl Pts',(5.15124649498693,26.1218089151717,6.91885873260879));
#452358=CARTESIAN_POINT('Ctrl Pts',(4.32949150779126,26.0741535347089,6.40650886405939));
#452359=CARTESIAN_POINT('Ctrl Pts',(4.30719954288124,26.0026704640147,4.94485582145312));
#452360=CARTESIAN_POINT('Ctrl Pts',(5.52404358693882,25.9311873933206,4.1380211598586));
#452361=CARTESIAN_POINT('Ctrl Pts',(6.86127108980971,25.8597043226263,4.7215087306785));
#452362=CARTESIAN_POINT('Ctrl Pts',(7.09568592881682,25.7882212519322,6.16255878293893));
#452363=CARTESIAN_POINT('Ctrl Pts',(6.01152748645437,25.716738181238,7.13997732676548));
#452364=CARTESIAN_POINT('Ctrl Pts',(4.60259286076204,25.6452551105438,6.75873746207651));
#452365=CARTESIAN_POINT('Ctrl Pts',(4.15947051927595,25.5737720398497,5.36788602689621));
#452366=CARTESIAN_POINT('Ctrl Pts',(5.0882746237623,25.5022889691555,4.24182426511434));
#452367=CARTESIAN_POINT('Ctrl Pts',(6.53798055190634,25.4308058984613,4.41217208256641));
#452368=CARTESIAN_POINT('Ctrl Pts',(7.18042191180854,25.3593228277671,5.72289095998872));
#452369=CARTESIAN_POINT('Ctrl Pts',(6.42698533143036,25.287839757073,6.97310209577086));
#452370=CARTESIAN_POINT('Ctrl Pts',(4.96796792520407,25.2163566863788,7.01738753624157));
#452371=CARTESIAN_POINT('Ctrl Pts',(4.14009680960707,25.1448736156846,5.81516935358237));
#452372=CARTESIAN_POINT('Ctrl Pts',(4.70185841202445,25.0733905449904,4.4679054394248));
#452373=CARTESIAN_POINT('Ctrl Pts',(6.13857330967851,25.0019074742962,4.20993933987732));
#452374=CARTESIAN_POINT('Ctrl Pts',(7.13394370229865,24.930424403602,5.27761660163647));
#452375=CARTESIAN_POINT('Ctrl Pts',(6.77602463836695,24.8589413329079,6.69274573713214));
#452376=CARTESIAN_POINT('Ctrl Pts',(5.39273679116275,24.7874582622137,7.15880506797054));
#452377=CARTESIAN_POINT('Ctrl Pts',(4.25142935492228,24.7159751915195,6.24879737998678));
#452378=CARTESIAN_POINT('Ctrl Pts',(4.39775252453571,24.6444921208253,4.79645922145989));
#452379=CARTESIAN_POINT('Ctrl Pts',(5.69764700649482,24.5730090501312,4.13240279133847));
#452380=CARTESIAN_POINT('Ctrl Pts',(6.9601673901235,24.501525979437,4.86502745488341));
#452381=CARTESIAN_POINT('Ctrl Pts',(7.0286098827299,24.4300429087428,6.32311258055822));
#452382=CARTESIAN_POINT('Ctrl Pts',(5.84026841822956,24.3585598380486,7.17078066054311));
#452383=CARTESIAN_POINT('Ctrl Pts',(4.4838850778304,24.2870767673545,6.63140987332417));
#452384=CARTESIAN_POINT('Ctrl Pts',(4.2021595986403,24.2155936966603,5.19916430623342));
#452385=CARTESIAN_POINT('Ctrl Pts',(5.25320498229437,24.1441106259661,4.18624762160046));
#452386=CARTESIAN_POINT('Ctrl Pts',(6.67406792795905,24.0726275552719,4.52068013549415));
#452387=CARTESIAN_POINT('Ctrl Pts',(7.16297336647392,24.0011444845777,5.89605938457563));
#452388=CARTESIAN_POINT('Ctrl Pts',(6.27199288310558,23.9296614138836,7.0522818436793));
#452389=CARTESIAN_POINT('Ctrl Pts',(4.81743049717126,23.8581783431894,6.93003241982605));
#452390=CARTESIAN_POINT('Ctrl Pts',(4.13193628895796,23.7866952724952,5.64131435190337));
#452391=CARTESIAN_POINT('Ctrl Pts',(4.84355050202496,23.715212201801,4.3668333837381));
#452392=CARTESIAN_POINT('Ctrl Pts',(6.30030220876029,23.6437291311069,4.27425142704003));
#452393=CARTESIAN_POINT('Ctrl Pts',(7.16753514006844,23.5722460604127,5.44839079206937));
#452394=CARTESIAN_POINT('Ctrl Pts',(6.65070324968042,23.5007629897185,6.81352117024561));
#452395=CARTESIAN_POINT('Ctrl Pts',(5.22331918686542,23.4292799190243,7.11892889768229));
#452396=CARTESIAN_POINT('Ctrl Pts',(4.19313572939823,23.3577968483302,6.08480364614363));
#452397=CARTESIAN_POINT('Ctrl Pts',(4.50398657889369,23.2863137776359,4.65859667867589));
#452398=CARTESIAN_POINT('Ctrl Pts',(5.8710866145267,23.2148307069418,4.14697927365876));
#452399=CARTESIAN_POINT('Ctrl Pts',(7.04189379284668,23.1433476362476,5.01868806000948));
#452400=CARTESIAN_POINT('Ctrl Pts',(6.94377741359718,23.0718645655535,6.47507582842176));
#452401=CARTESIAN_POINT('Ctrl Pts',(5.66653874837814,23.0003814948592,7.18181942856023));
#452402=CARTESIAN_POINT('Ctrl Pts',(4.38054591235378,22.9288984241651,6.49141154940691));
#452403=CARTESIAN_POINT('Ctrl Pts',(4.26365553420012,22.8574153534709,5.03639155729104));
#452404=CARTESIAN_POINT('Ctrl Pts',(5.42365194556336,22.7859322827767,4.14983422948258));
#452405=CARTESIAN_POINT('Ctrl Pts',(6.79640622083105,22.7144492120825,4.6439808063907));
#452406=CARTESIAN_POINT('Ctrl Pts',(7.12689194633153,22.6429661413884,6.06611679986992));
#452407=CARTESIAN_POINT('Ctrl Pts',(6.10694434613243,22.5714830706942,7.11331947438321));
#452408=CARTESIAN_POINT('Ctrl Pts',(5.15775103452081,22.5238276902314,6.92144528650133));
#452409=CARTESIAN_POINT('Ctrl Pts',(4.8286920333622,22.5,6.64591806159944));
#452410=CARTESIAN_POINT('Ctrl Pts',(4.8286920333622,22.5,6.64591806159944));
#452411=CARTESIAN_POINT('Ctrl Pts',(4.8719367804586,22.5,6.6755807993511));
#452412=CARTESIAN_POINT('Ctrl Pts',(4.91697381282208,22.5,6.7022744086721));
#452413=CARTESIAN_POINT('Ctrl Pts',(4.96347942286292,22.5,6.72600910610866));
#452414=CARTESIAN_POINT('Ctrl Pts',(5.01052630347802,22.5,6.750020047493));
#452415=CARTESIAN_POINT('Ctrl Pts',(5.05907736675444,22.5,6.77100289981649));
#452416=CARTESIAN_POINT('Ctrl Pts',(5.10881343934042,22.5,6.78891649180094));
#452417=CARTESIAN_POINT('Ctrl Pts',(5.14478450961691,22.5,6.80187230118985));
#452418=CARTESIAN_POINT('Ctrl Pts',(5.18137581815852,22.5,6.81322157811539));
#452419=CARTESIAN_POINT('Ctrl Pts',(5.21846626007043,22.5,6.82293175279788));
#452420=CARTESIAN_POINT('Ctrl Pts',(5.23435307151024,22.5,6.82709087591091));
#452421=CARTESIAN_POINT('Ctrl Pts',(5.25033142515782,22.5,6.83094910537833));
#452422=CARTESIAN_POINT('Ctrl Pts',(5.26639159475908,22.5,6.83450307899072));
#452423=CARTESIAN_POINT('Ctrl Pts',(5.27631910355995,22.5,6.83669994896103));
#452424=CARTESIAN_POINT('Ctrl Pts',(5.28627904830748,22.5,6.83878067254843));
#452425=CARTESIAN_POINT('Ctrl Pts',(5.29625198803563,22.5,6.8407413340506));
#452426=CARTESIAN_POINT('Ctrl Pts',(5.34683220766748,22.5,6.8506853116647));
#452427=CARTESIAN_POINT('Ctrl Pts',(5.39784710619139,22.5,6.85756855483867));
#452428=CARTESIAN_POINT('Ctrl Pts',(5.44899668904261,22.5,6.86136063349203));
#452429=CARTESIAN_POINT('Ctrl Pts',(5.4989795280052,22.5,6.86506621320742));
#452430=CARTESIAN_POINT('Ctrl Pts',(5.5490920296864,22.5,6.86581982211597));
#452431=CARTESIAN_POINT('Ctrl Pts',(5.59904614057211,22.5,6.86354521214504));
#452432=CARTESIAN_POINT('Ctrl Pts',(5.63380176660143,22.5,6.86196264982713));
#452433=CARTESIAN_POINT('Ctrl Pts',(5.66848055894767,22.5,6.8589132351154));
#452434=CARTESIAN_POINT('Ctrl Pts',(5.70297915970175,22.5,6.85435789423314));
#452435=CARTESIAN_POINT('Ctrl Pts',(5.71516099278645,22.5,6.85274935356602));
#452436=CARTESIAN_POINT('Ctrl Pts',(5.72732029612368,22.5,6.85095294339145));
#452437=CARTESIAN_POINT('Ctrl Pts',(5.73945229469627,22.5,6.84896661767721));
#452438=CARTESIAN_POINT('Ctrl Pts',(5.74841196470285,22.5,6.84749968518305));
#452439=CARTESIAN_POINT('Ctrl Pts',(5.75735562780225,22.5,6.84592925290685));
#452440=CARTESIAN_POINT('Ctrl Pts',(5.76626920948405,22.5,6.84425708000572));
#452441=CARTESIAN_POINT('Ctrl Pts',(5.81380349733577,22.5,6.83533972771596));
#452442=CARTESIAN_POINT('Ctrl Pts',(5.86057802478339,22.5,6.82351786783565));
#452443=CARTESIAN_POINT('Ctrl Pts',(5.90632961568247,22.5,6.80873145101255));
#452444=CARTESIAN_POINT('Ctrl Pts',(5.93907832139669,22.5,6.79814742532969));
#452445=CARTESIAN_POINT('Ctrl Pts',(5.97130269582608,22.5,6.78604349575646));
#452446=CARTESIAN_POINT('Ctrl Pts',(6.00289829431615,22.5,6.77238316128915));
#452447=CARTESIAN_POINT('Ctrl Pts',(6.0450043450931,22.5,6.75417864027363));
#452448=CARTESIAN_POINT('Ctrl Pts',(6.08599501913005,22.5,6.73321019789003));
#452449=CARTESIAN_POINT('Ctrl Pts',(6.12568011956913,22.5,6.70966855565445));
#452450=CARTESIAN_POINT('Ctrl Pts',(6.13614447303852,22.5,6.7034609849824));
#452451=CARTESIAN_POINT('Ctrl Pts',(6.14651787724421,22.5,6.69707438313333));
#452452=CARTESIAN_POINT('Ctrl Pts',(6.1567964532414,22.5,6.69051202329594));
#452453=CARTESIAN_POINT('Ctrl Pts',(6.1645478556042,22.5,6.68556313820106));
#452454=CARTESIAN_POINT('Ctrl Pts',(6.17224531908615,22.5,6.68051415741144));
#452455=CARTESIAN_POINT('Ctrl Pts',(6.17987521950616,22.5,6.67537489370653));
#452456=CARTESIAN_POINT('Ctrl Pts',(6.21988616021516,22.5,6.64842476800822));
#452457=CARTESIAN_POINT('Ctrl Pts',(6.25812741389502,22.5,6.61894162118579));
#452458=CARTESIAN_POINT('Ctrl Pts',(6.29441170508163,22.5,6.58718324857477));
#452459=CARTESIAN_POINT('Ctrl Pts',(6.33059687379256,22.5,6.55551163440422));
#452460=CARTESIAN_POINT('Ctrl Pts',(6.36483641843439,22.5,6.52157609274862));
#452461=CARTESIAN_POINT('Ctrl Pts',(6.39690234758754,22.5,6.48560329463389));
#452462=CARTESIAN_POINT('Ctrl Pts',(6.41407247164262,22.5,6.46634118614209));
#452463=CARTESIAN_POINT('Ctrl Pts',(6.4306185942519,22.5,6.44649455990001));
#452464=CARTESIAN_POINT('Ctrl Pts',(6.44649972121378,22.5,6.42609644704949));
#452465=CARTESIAN_POINT('Ctrl Pts',(6.45474860376629,22.5,6.41550137797154));
#452466=CARTESIAN_POINT('Ctrl Pts',(6.4628180032753,22.5,6.40475750978787));
#452467=CARTESIAN_POINT('Ctrl Pts',(6.47070167883221,22.5,6.39386942293182));
#452468=CARTESIAN_POINT('Ctrl Pts',(6.47674054415646,22.5,6.38552919004326));
#452469=CARTESIAN_POINT('Ctrl Pts',(6.48267052688883,22.5,6.37710396981869));
#452470=CARTESIAN_POINT('Ctrl Pts',(6.48848046699456,22.5,6.3686084992472));
#452471=CARTESIAN_POINT('Ctrl Pts',(6.51462321287319,22.5,6.33038178361366));
#452472=CARTESIAN_POINT('Ctrl Pts',(6.53838419602365,22.5,6.29067294990532));
#452473=CARTESIAN_POINT('Ctrl Pts',(6.55954587128772,22.5,6.24968947065537));
#452474=CARTESIAN_POINT('Ctrl Pts',(6.57382078988697,22.5,6.22204346329034));
#452475=CARTESIAN_POINT('Ctrl Pts',(6.58691199084907,22.5,6.19381707848861));
#452476=CARTESIAN_POINT('Ctrl Pts',(6.59873928456135,22.5,6.16507260006602));
#452477=CARTESIAN_POINT('Ctrl Pts',(6.60384497627704,22.5,6.15266397566519));
#452478=CARTESIAN_POINT('Ctrl Pts',(6.6087155221976,22.5,6.14015674565985));
#452479=CARTESIAN_POINT('Ctrl Pts',(6.61333659561112,22.5,6.12757735912736));
#452480=CARTESIAN_POINT('Ctrl Pts',(6.6285399411254,22.5,6.08619113936898));
#452481=CARTESIAN_POINT('Ctrl Pts',(6.64106838659551,22.5,6.04397428614735));
#452482=CARTESIAN_POINT('Ctrl Pts',(6.65070263630215,22.5,6.00111091245467));
#452483=CARTESIAN_POINT('Ctrl Pts',(6.65546745351706,22.5,5.9799119455316));
#452484=CARTESIAN_POINT('Ctrl Pts',(6.65952358177373,22.5,5.9585548202981));
#452485=CARTESIAN_POINT('Ctrl Pts',(6.66283972884874,22.5,5.93706218561481));
#452486=CARTESIAN_POINT('Ctrl Pts',(6.66481534816931,22.5,5.92425778841234));
#452487=CARTESIAN_POINT('Ctrl Pts',(6.6665282555788,22.5,5.91140530098883));
#452488=CARTESIAN_POINT('Ctrl Pts',(6.66798006829994,22.5,5.89851203167795));
#452489=CARTESIAN_POINT('Ctrl Pts',(6.39051881327128,25.2730384757729,4.92197603118329));
#452490=CARTESIAN_POINT('Ctrl Pts',(6.34953594825859,25.2770820815347,4.8802577415671));
#452491=CARTESIAN_POINT('Ctrl Pts',(6.3050503566324,25.2811256872965,4.84215579969383));
#452492=CARTESIAN_POINT('Ctrl Pts',(6.25744773204304,25.2851692930582,4.80845709106527));
#452493=CARTESIAN_POINT('Ctrl Pts',(5.97694051651721,25.3089969832896,4.60988125610327));
#452494=CARTESIAN_POINT('Ctrl Pts',(5.58819831317574,25.332824673521,4.56420207068701));
#452495=CARTESIAN_POINT('Ctrl Pts',(5.26929666119096,25.3566523637524,4.69234059080694));
#452496=CARTESIAN_POINT('Ctrl Pts',(4.95039500920618,25.3804800539838,4.82047911092687));
#452497=CARTESIAN_POINT('Ctrl Pts',(4.70133390857808,25.4043077442152,5.12243533658298));
#452498=CARTESIAN_POINT('Ctrl Pts',(4.6362155300828,25.4281354344466,5.45989356270023));
#452499=CARTESIAN_POINT('Ctrl Pts',(4.57109715158751,25.451963124678,5.79735178881747));
#452500=CARTESIAN_POINT('Ctrl Pts',(4.68992149522503,25.4757908149094,6.17031201539585));
#452501=CARTESIAN_POINT('Ctrl Pts',(4.93823830629601,25.4996185051408,6.40790733147329));
#452502=CARTESIAN_POINT('Ctrl Pts',(5.186555117367,25.5234461953722,6.64550264755072));
#452503=CARTESIAN_POINT('Ctrl Pts',(5.56436439587144,25.5472738856035,6.74773305312721));
#452504=CARTESIAN_POINT('Ctrl Pts',(5.89862890896884,25.5711015758349,6.66779966497798));
#452505=CARTESIAN_POINT('Ctrl Pts',(6.23289342206624,25.5949292660663,6.58786627682875));
#452506=CARTESIAN_POINT('Ctrl Pts',(6.52361316975658,25.6187569562977,6.32576909495381));
#452507=CARTESIAN_POINT('Ctrl Pts',(6.63754358634341,25.6425846465291,6.00150994952884));
#452508=CARTESIAN_POINT('Ctrl Pts',(6.75147400293023,25.6664123367605,5.67725080410387));
#452509=CARTESIAN_POINT('Ctrl Pts',(6.68861508841353,25.6902400269919,5.29082969512888));
#452510=CARTESIAN_POINT('Ctrl Pts',(6.47789521240786,25.7140677172233,5.01938732841678));
#452511=CARTESIAN_POINT('Ctrl Pts',(6.45145094929911,25.7170579700732,4.98532270432787));
#452512=CARTESIAN_POINT('Ctrl Pts',(6.42267802952733,25.720048222923,4.95306887608107));
#452513=CARTESIAN_POINT('Ctrl Pts',(6.39190058798136,25.7230384757729,4.92276701974739));
#452514=CARTESIAN_POINT('Ctrl Pts',(5.01302286563431,26.,4.53900700771688));
#452515=CARTESIAN_POINT('Ctrl Pts',(5.38492752167559,25.9761723097686,4.32480615636363));
#452516=CARTESIAN_POINT('Ctrl Pts',(6.35301914505848,25.9285169293058,4.30067277954968));
#452517=CARTESIAN_POINT('Ctrl Pts',(7.17562648915451,25.8570338586117,5.50907794609548));
#452518=CARTESIAN_POINT('Ctrl Pts',(6.60321033464885,25.7855507879174,6.8522203629011));
#452519=CARTESIAN_POINT('Ctrl Pts',(5.16550356767203,25.7140677172233,7.1004834147237));
#452520=CARTESIAN_POINT('Ctrl Pts',(4.17707919799325,25.6425846465291,6.0259636415713));
#452521=CARTESIAN_POINT('Ctrl Pts',(4.5448553014618,25.5711015758349,4.61334644908231));
#452522=CARTESIAN_POINT('Ctrl Pts',(5.93119910857215,25.4996185051408,4.15673773385264));
#452523=CARTESIAN_POINT('Ctrl Pts',(7.06630891143689,25.4281354344466,5.07453447980768));
#452524=CARTESIAN_POINT('Ctrl Pts',(6.91003560334641,25.3566523637524,6.5258341885166));
#452525=CARTESIAN_POINT('Ctrl Pts',(5.60564496305,25.2851692930582,7.18099123031483));
#452526=CARTESIAN_POINT('Ctrl Pts',(4.34815567114858,25.213686222364,6.43975200870338));
#452527=CARTESIAN_POINT('Ctrl Pts',(4.28968558428151,25.1422031516699,4.98123363545819));
#452528=CARTESIAN_POINT('Ctrl Pts',(5.48379221455872,25.0707200809757,4.14170854437417));
#452529=CARTESIAN_POINT('Ctrl Pts',(6.8364576202828,24.9992370102815,4.69033908735646));
#452530=CARTESIAN_POINT('Ctrl Pts',(7.10838527255517,24.9277539395874,6.12447699388039));
#452531=CARTESIAN_POINT('Ctrl Pts',(6.05044038944422,24.8562708688931,7.13018513270865));
#452532=CARTESIAN_POINT('Ctrl Pts',(4.63189669239788,24.784787798199,6.78604742232837));
#452533=CARTESIAN_POINT('Ctrl Pts',(4.15240479236238,24.7133047275048,5.40735816264999));
#452534=CARTESIAN_POINT('Ctrl Pts',(5.0512683537124,24.6418216568106,4.25725342975252));
#452535=CARTESIAN_POINT('Ctrl Pts',(6.50496106867921,24.5703385861164,4.38944335790392));
#452536=CARTESIAN_POINT('Ctrl Pts',(7.18162963832199,24.4988555154223,5.68281734635597));
#452537=CARTESIAN_POINT('Ctrl Pts',(6.46131966662841,24.4273724447281,6.95240396480877));
#452538=CARTESIAN_POINT('Ctrl Pts',(5.00396921476326,24.3558893740339,7.03502543671246));
#452539=CARTESIAN_POINT('Ctrl Pts',(4.14478270244581,24.2844063033397,5.85498510857851));
#452540=CARTESIAN_POINT('Ctrl Pts',(4.67093497503136,24.2129232326456,4.49341967622111));
#452541=CARTESIAN_POINT('Ctrl Pts',(6.10037256921808,24.1414401619514,4.19777663638434));
#452542=CARTESIAN_POINT('Ctrl Pts',(7.12346444664167,24.0699570912572,5.23892007073304));
#452543=CARTESIAN_POINT('Ctrl Pts',(6.80286792203874,23.998474020563,6.662968703113));
#452544=CARTESIAN_POINT('Ctrl Pts',(5.43230911237055,23.9269909498688,7.16522879152533));
#452545=CARTESIAN_POINT('Ctrl Pts',(4.26747512907024,23.8555078791747,6.2855365564656));
#452546=CARTESIAN_POINT('Ctrl Pts',(4.37557081254884,23.7840248084805,4.82985391579145));
#452547=CARTESIAN_POINT('Ctrl Pts',(5.6575604101698,23.7125417377863,4.13185724083954));
#452548=CARTESIAN_POINT('Ctrl Pts',(6.93890266242659,23.6410586670921,4.83104150205929));
#452549=CARTESIAN_POINT('Ctrl Pts',(7.04564953674368,23.569575596398,6.28682364983267));
#452550=CARTESIAN_POINT('Ctrl Pts',(5.88000083782648,23.4980925257038,7.16543624640093));
#452551=CARTESIAN_POINT('Ctrl Pts',(4.50990820099156,23.4266094550096,6.66190630419616));
#452552=CARTESIAN_POINT('Ctrl Pts',(4.19063094092434,23.3551263843154,5.23756146736659));
#452553=CARTESIAN_POINT('Ctrl Pts',(5.21468783779196,23.2836433136212,4.19736598356862));
#452554=CARTESIAN_POINT('Ctrl Pts',(6.64384941569999,23.2121602429271,4.49433434427902));
#452555=CARTESIAN_POINT('Ctrl Pts',(7.16874271925581,23.1406771722329,5.85638486317849));
#452556=CARTESIAN_POINT('Ctrl Pts',(6.30845753745629,23.0691941015387,7.03563221165043));
#452557=CARTESIAN_POINT('Ctrl Pts',(4.85119529970875,22.9977110308445,6.95165327175697));
#452558=CARTESIAN_POINT('Ctrl Pts',(4.13204038713623,22.9262279601503,5.68141376558384));
#452559=CARTESIAN_POINT('Ctrl Pts',(4.80994952176022,22.8547448894562,4.38863987327371));
#452560=CARTESIAN_POINT('Ctrl Pts',(6.26368089065206,22.783261818762,4.25785081625158));
#452561=CARTESIAN_POINT('Ctrl Pts',(7.16164157512573,22.7117787480678,5.40868234342553));
#452562=CARTESIAN_POINT('Ctrl Pts',(6.68055232418451,22.6402956773736,6.78713386963137));
#452563=CARTESIAN_POINT('Ctrl Pts',(5.26231872215201,22.5688126066795,7.12954990426925));
#452564=CARTESIAN_POINT('Ctrl Pts',(4.20406666678212,22.4973295359853,6.12366999440581));
#452565=CARTESIAN_POINT('Ctrl Pts',(4.47983331463011,22.4258464652911,4.68809392709694));
#452566=CARTESIAN_POINT('Ctrl Pts',(5.37807265034296,22.3781910848283,4.32622391325397));
#452567=CARTESIAN_POINT('Ctrl Pts',(5.80443435631943,22.3543633945969,4.37532354240196));
#452568=CARTESIAN_POINT('Ctrl Pts',(5.05498833669907,26.0485455351344,4.61186924884874));
#452569=CARTESIAN_POINT('Ctrl Pts',(5.40265192052163,26.024717844903,4.41163019717349));
#452570=CARTESIAN_POINT('Ctrl Pts',(6.30764248137266,25.9770624644402,4.38906985506272));
#452571=CARTESIAN_POINT('Ctrl Pts',(7.07663155607638,25.905579393746,5.51871011120511));
#452572=CARTESIAN_POINT('Ctrl Pts',(6.54152598941931,25.8340963230518,6.77430532526158));
#452573=CARTESIAN_POINT('Ctrl Pts',(5.1975302126156,25.7626132523576,7.00638637325414));
#452574=CARTESIAN_POINT('Ctrl Pts',(4.27353221173564,25.6911301816635,6.00190474293836));
#452575=CARTESIAN_POINT('Ctrl Pts',(4.61733634566934,25.6196471109693,4.68136318011483));
#452576=CARTESIAN_POINT('Ctrl Pts',(5.91331704545575,25.5481640402751,4.25451662209878));
#452577=CARTESIAN_POINT('Ctrl Pts',(6.97443939411569,25.4766809695809,5.11249056981941));
#452578=CARTESIAN_POINT('Ctrl Pts',(6.82835211754091,25.4051978988868,6.46919328847101));
#452579=CARTESIAN_POINT('Ctrl Pts',(5.60898280515531,25.3337148281926,7.08164661869467));
#452580=CARTESIAN_POINT('Ctrl Pts',(4.43345777007097,25.2622317574984,6.38872202076577));
#452581=CARTESIAN_POINT('Ctrl Pts',(4.37879881483496,25.1907486868042,5.02527115647435));
#452582=CARTESIAN_POINT('Ctrl Pts',(5.49507252586478,25.1192656161101,4.24046704839446));
#452583=CARTESIAN_POINT('Ctrl Pts',(6.75957001205555,25.0477825454158,4.75333737058416));
#452584=CARTESIAN_POINT('Ctrl Pts',(7.01377318104996,24.9762994747217,6.09399690839474));
#452585=CARTESIAN_POINT('Ctrl Pts',(6.0247860748808,24.9048164040275,7.03415210716631));
#452586=CARTESIAN_POINT('Ctrl Pts',(4.69870430227373,24.8333333333333,6.71244559509181));
#452587=CARTESIAN_POINT('Ctrl Pts',(4.25046610554157,24.7618502626392,5.42362051261082));
#452588=CARTESIAN_POINT('Ctrl Pts',(5.09074095026354,24.6903671919449,4.34848061663154));
#452589=CARTESIAN_POINT('Ctrl Pts',(6.44968069692276,24.6188841212508,4.47205428913018));
#452590=CARTESIAN_POINT('Ctrl Pts',(7.08224341470704,24.5474010505566,5.68112502471735));
#452591=CARTESIAN_POINT('Ctrl Pts',(6.40888387979891,24.4759179798625,6.86795887198032));
#452592=CARTESIAN_POINT('Ctrl Pts',(5.04652481074591,24.4044349091682,6.94519500375797));
#452593=CARTESIAN_POINT('Ctrl Pts',(4.24334083014217,24.3329518384741,5.84207074093976));
#452594=CARTESIAN_POINT('Ctrl Pts',(4.73519803534796,24.2614687677799,4.56925333967074));
#452595=CARTESIAN_POINT('Ctrl Pts',(6.07146363130893,24.1899856970857,4.29288057290862));
#452596=CARTESIAN_POINT('Ctrl Pts',(7.02786948132165,24.1185026263916,5.2661613635068));
#452597=CARTESIAN_POINT('Ctrl Pts',(6.72816971985337,24.0470195556973,6.59738925492609));
#452598=CARTESIAN_POINT('Ctrl Pts',(5.44694513750786,23.9755364850032,7.0669115895136));
#452599=CARTESIAN_POINT('Ctrl Pts',(4.35803605660743,23.904053414309,6.2445584671913));
#452600=CARTESIAN_POINT('Ctrl Pts',(4.45908596846911,23.8325703436148,4.88375849993059));
#452601=CARTESIAN_POINT('Ctrl Pts',(5.65751435782136,23.7610872729207,4.2312578614791));
#452602=CARTESIAN_POINT('Ctrl Pts',(6.85533759634902,23.6896042022265,4.88486867828213));
#452603=CARTESIAN_POINT('Ctrl Pts',(6.95512661561532,23.6181211315323,6.24576166668191));
#452604=CARTESIAN_POINT('Ctrl Pts',(5.86545592297768,23.5466380608381,7.06710552229816));
#452605=CARTESIAN_POINT('Ctrl Pts',(4.58466712791062,23.475154990144,6.59639610410402));
#452606=CARTESIAN_POINT('Ctrl Pts',(4.28620064015657,23.4036719194498,5.26489131510138));
#452607=CARTESIAN_POINT('Ctrl Pts',(5.24350860879812,23.3321888487556,4.2924966868042));
#452608=CARTESIAN_POINT('Ctrl Pts',(6.57951617946397,23.2607057780614,4.57010838886106));
#452609=CARTESIAN_POINT('Ctrl Pts',(7.07019647634743,23.1892227073672,5.84337925830513));
#452610=CARTESIAN_POINT('Ctrl Pts',(6.26598543850372,23.1177396366731,6.94576222857241));
#452611=CARTESIAN_POINT('Ctrl Pts',(4.90370883369462,23.0462565659789,6.86725710976116));
#452612=CARTESIAN_POINT('Ctrl Pts',(4.23142907013928,22.9747734952847,5.67981293057308));
#452613=CARTESIAN_POINT('Ctrl Pts',(4.86515149178938,22.9032904245905,4.47130317633407));
#452614=CARTESIAN_POINT('Ctrl Pts',(6.22412737287685,22.8318073538963,4.34903906495375));
#452615=CARTESIAN_POINT('Ctrl Pts',(7.06355819103049,22.7603242832022,5.42485838212006));
#452616=CARTESIAN_POINT('Ctrl Pts',(6.613826760128,22.688841212508,6.7134612268051));
#452617=CARTESIAN_POINT('Ctrl Pts',(5.28803487026933,22.6173581418138,7.03355828347467));
#452618=CARTESIAN_POINT('Ctrl Pts',(4.29876061359894,22.5458750711196,6.0932425098549));
#452619=CARTESIAN_POINT('Ctrl Pts',(4.55655254906459,22.4743920004255,4.75123855184286));
#452620=CARTESIAN_POINT('Ctrl Pts',(5.39624385572484,22.4267366199627,4.41295554342414));
#452621=CARTESIAN_POINT('Ctrl Pts',(5.79481493112442,22.4029089297313,4.45885481560765));
#452622=CARTESIAN_POINT('Ctrl Pts',(5.09695380776383,26.0970910702687,4.6847314899806));
#452623=CARTESIAN_POINT('Ctrl Pts',(5.42037631936769,26.0732633800373,4.49845423798335));
#452624=CARTESIAN_POINT('Ctrl Pts',(6.26226581768684,26.0256079995745,4.47746693057576));
#452625=CARTESIAN_POINT('Ctrl Pts',(6.97763662299825,25.9541249288804,5.52834227631475));
#452626=CARTESIAN_POINT('Ctrl Pts',(6.47984164418979,25.8826418581862,6.69639028762206));
#452627=CARTESIAN_POINT('Ctrl Pts',(5.22955685755916,25.811158787492,6.91228933178459));
#452628=CARTESIAN_POINT('Ctrl Pts',(4.36998522547805,25.7396757167978,5.97784584430541));
#452629=CARTESIAN_POINT('Ctrl Pts',(4.68981738987686,25.6681926461037,4.74937991114736));
#452630=CARTESIAN_POINT('Ctrl Pts',(5.89543498233936,25.5967095754095,4.35229551034491));
#452631=CARTESIAN_POINT('Ctrl Pts',(6.88256987679448,25.5252265047153,5.15044665983115));
#452632=CARTESIAN_POINT('Ctrl Pts',(6.74666863173542,25.4537434340211,6.41255238842542));
#452633=CARTESIAN_POINT('Ctrl Pts',(5.61232064726061,25.3822603633269,6.9823020070745));
#452634=CARTESIAN_POINT('Ctrl Pts',(4.51875986899336,25.3107772926328,6.33769203282816));
#452635=CARTESIAN_POINT('Ctrl Pts',(4.46791204538842,25.2392942219386,5.06930867749052));
#452636=CARTESIAN_POINT('Ctrl Pts',(5.50635283717083,25.1678111512444,4.33922555241474));
#452637=CARTESIAN_POINT('Ctrl Pts',(6.68268240382831,25.0963280805502,4.81633565381187));
#452638=CARTESIAN_POINT('Ctrl Pts',(6.91916108954474,25.0248450098561,6.06351682290909));
#452639=CARTESIAN_POINT('Ctrl Pts',(5.99913176031738,24.9533619391618,6.93811908162396));
#452640=CARTESIAN_POINT('Ctrl Pts',(4.76551191214957,24.8818788684677,6.63884376785527));
#452641=CARTESIAN_POINT('Ctrl Pts',(4.34852741872076,24.8103957977735,5.43988286257165));
#452642=CARTESIAN_POINT('Ctrl Pts',(5.13021354681469,24.7389127270793,4.43970780351056));
#452643=CARTESIAN_POINT('Ctrl Pts',(6.39440032516631,24.6674296563851,4.55466522035643));
#452644=CARTESIAN_POINT('Ctrl Pts',(6.9828571910921,24.595946585691,5.67943270307875));
#452645=CARTESIAN_POINT('Ctrl Pts',(6.35644809296942,24.5244635149968,6.78351377915185));
#452646=CARTESIAN_POINT('Ctrl Pts',(5.08908040672856,24.4529804443026,6.8553645708035));
#452647=CARTESIAN_POINT('Ctrl Pts',(4.34189895783853,24.3814973736085,5.82915637330097));
#452648=CARTESIAN_POINT('Ctrl Pts',(4.79946109566455,24.3100143029142,4.64508700312038));
#452649=CARTESIAN_POINT('Ctrl Pts',(6.0425546933998,24.2385312322201,4.38798450943289));
#452650=CARTESIAN_POINT('Ctrl Pts',(6.93227451600162,24.1670481615259,5.29340265628057));
#452651=CARTESIAN_POINT('Ctrl Pts',(6.65347151766801,24.0955650908317,6.53180980673917));
#452652=CARTESIAN_POINT('Ctrl Pts',(5.46158116264517,24.0240820201376,6.96859438750187));
#452653=CARTESIAN_POINT('Ctrl Pts',(4.44859698414461,23.9525989494434,6.20358037791699));
#452654=CARTESIAN_POINT('Ctrl Pts',(4.54260112438938,23.8811158787492,4.93766308406974));
#452655=CARTESIAN_POINT('Ctrl Pts',(5.65746830547292,23.809632808055,4.33065848211867));
#452656=CARTESIAN_POINT('Ctrl Pts',(6.77177253027144,23.7381497373608,4.93869585450498));
#452657=CARTESIAN_POINT('Ctrl Pts',(6.86460369448697,23.6666666666667,6.20469968353116));
#452658=CARTESIAN_POINT('Ctrl Pts',(5.85091100812889,23.5951835959725,6.96877479819537));
#452659=CARTESIAN_POINT('Ctrl Pts',(4.65942605482967,23.5237005252783,6.53088590401187));
#452660=CARTESIAN_POINT('Ctrl Pts',(4.3817703393888,23.4522174545841,5.29222116283617));
#452661=CARTESIAN_POINT('Ctrl Pts',(5.27232937980428,23.38073438389,4.38762739003978));
#452662=CARTESIAN_POINT('Ctrl Pts',(6.51518294322793,23.3092513131958,4.6458824334431));
#452663=CARTESIAN_POINT('Ctrl Pts',(6.97165023343906,23.2377682425016,5.83037365343178));
#452664=CARTESIAN_POINT('Ctrl Pts',(6.22351333955115,23.1662851718074,6.85589224549438));
#452665=CARTESIAN_POINT('Ctrl Pts',(4.9562223676805,23.0948021011132,6.78286094776533));
#452666=CARTESIAN_POINT('Ctrl Pts',(4.33081775314232,23.0233190304191,5.67821209556232));
#452667=CARTESIAN_POINT('Ctrl Pts',(4.92035346181854,22.9518359597249,4.55396647939443));
#452668=CARTESIAN_POINT('Ctrl Pts',(6.18457385510162,22.8803528890307,4.44022731365593));
#452669=CARTESIAN_POINT('Ctrl Pts',(6.96547480693525,22.8088698183366,5.44103442081457));
#452670=CARTESIAN_POINT('Ctrl Pts',(6.5471011960715,22.7373867476423,6.63978858397884));
#452671=CARTESIAN_POINT('Ctrl Pts',(5.31375101838666,22.6659036769482,6.93756666268008));
#452672=CARTESIAN_POINT('Ctrl Pts',(4.39345456041576,22.594420606254,6.06281502530401));
#452673=CARTESIAN_POINT('Ctrl Pts',(4.63327178349907,22.5229375355598,4.81438317658877));
#452674=CARTESIAN_POINT('Ctrl Pts',(5.41441506110672,22.475282155097,4.49968717359432));
#452675=CARTESIAN_POINT('Ctrl Pts',(5.78519550592941,22.4514544648656,4.54238608881333));
#452676=CARTESIAN_POINT('Ctrl Pts',(5.13891927882859,26.1456366054031,4.75759373111246));
#452677=CARTESIAN_POINT('Ctrl Pts',(5.43810071821374,26.1218089151717,4.58527827879321));
#452678=CARTESIAN_POINT('Ctrl Pts',(6.21688915400102,26.0741535347089,4.5658640060888));
#452679=CARTESIAN_POINT('Ctrl Pts',(6.87864168992013,26.0026704640147,5.53797444142439));
#452680=CARTESIAN_POINT('Ctrl Pts',(6.41815729896025,25.9311873933205,6.61847524998255));
#452681=CARTESIAN_POINT('Ctrl Pts',(5.26158350250274,25.8597043226264,6.81819229031504));
#452682=CARTESIAN_POINT('Ctrl Pts',(4.46643823922045,25.7882212519322,5.95378694567247));
#452683=CARTESIAN_POINT('Ctrl Pts',(4.76229843408439,25.716738181238,4.81739664217988));
#452684=CARTESIAN_POINT('Ctrl Pts',(5.87755291922296,25.6452551105439,4.45007439859106));
#452685=CARTESIAN_POINT('Ctrl Pts',(6.79070035947327,25.5737720398496,5.18840274984287));
#452686=CARTESIAN_POINT('Ctrl Pts',(6.66498514592993,25.5022889691555,6.35591148837983));
#452687=CARTESIAN_POINT('Ctrl Pts',(5.61565848936591,25.4308058984613,6.88295739545434));
#452688=CARTESIAN_POINT('Ctrl Pts',(4.60406196791575,25.3593228277671,6.28666204489054));
#452689=CARTESIAN_POINT('Ctrl Pts',(4.55702527594187,25.2878397570729,5.11334619850669));
#452690=CARTESIAN_POINT('Ctrl Pts',(5.5176331484769,25.2163566863788,4.43798405643501));
#452691=CARTESIAN_POINT('Ctrl Pts',(6.60579479560105,25.1448736156845,4.87933393703958));
#452692=CARTESIAN_POINT('Ctrl Pts',(6.82454899803954,25.0733905449905,6.03303673742345));
#452693=CARTESIAN_POINT('Ctrl Pts',(5.97347744575396,25.0019074742962,6.84208605608161));
#452694=CARTESIAN_POINT('Ctrl Pts',(4.83231952202542,24.9304244036021,6.56524194061872));
#452695=CARTESIAN_POINT('Ctrl Pts',(4.44658873189995,24.8589413329078,5.45614521253248));
#452696=CARTESIAN_POINT('Ctrl Pts',(5.16968614336583,24.7874582622137,4.53093499038958));
#452697=CARTESIAN_POINT('Ctrl Pts',(6.33911995340987,24.7159751915195,4.63727615158269));
#452698=CARTESIAN_POINT('Ctrl Pts',(6.88347096747714,24.6444921208254,5.67774038144014));
#452699=CARTESIAN_POINT('Ctrl Pts',(6.30401230613993,24.5730090501312,6.69906868632339));
#452700=CARTESIAN_POINT('Ctrl Pts',(5.13163600271121,24.501525979437,6.76553413784902));
#452701=CARTESIAN_POINT('Ctrl Pts',(4.44045708553489,24.4300429087428,5.8162420056622));
#452702=CARTESIAN_POINT('Ctrl Pts',(4.86372415598115,24.3585598380486,4.72092066657002));
#452703=CARTESIAN_POINT('Ctrl Pts',(6.01364575549064,24.2870767673545,4.48308844595715));
#452704=CARTESIAN_POINT('Ctrl Pts',(6.83667955068161,24.2155936966602,5.32064394905434));
#452705=CARTESIAN_POINT('Ctrl Pts',(6.57877331548261,24.1441106259661,6.46623035855224));
#452706=CARTESIAN_POINT('Ctrl Pts',(5.4762171877825,24.0726275552719,6.87027718549015));
#452707=CARTESIAN_POINT('Ctrl Pts',(4.53915791168179,24.0011444845778,6.16260228864268));
#452708=CARTESIAN_POINT('Ctrl Pts',(4.62611628030965,23.9296614138835,4.99156766820889));
#452709=CARTESIAN_POINT('Ctrl Pts',(5.65742225312448,23.8581783431894,4.43005910275823));
#452710=CARTESIAN_POINT('Ctrl Pts',(6.68820746419386,23.7866952724952,4.99252303072782));
#452711=CARTESIAN_POINT('Ctrl Pts',(6.77408077335862,23.715212201801,6.16363770038041));
#452712=CARTESIAN_POINT('Ctrl Pts',(5.83636609328008,23.6437291311068,6.87044407409259));
#452713=CARTESIAN_POINT('Ctrl Pts',(4.73418498174874,23.5722460604127,6.46537570391973));
#452714=CARTESIAN_POINT('Ctrl Pts',(4.47734003862102,23.5007629897185,5.31955101057097));
#452715=CARTESIAN_POINT('Ctrl Pts',(5.30115015081045,23.4292799190243,4.48275809327536));
#452716=CARTESIAN_POINT('Ctrl Pts',(6.4508497069919,23.3577968483301,4.72165647802514));
#452717=CARTESIAN_POINT('Ctrl Pts',(6.87310399053069,23.286313777636,5.81736804855842));
#452718=CARTESIAN_POINT('Ctrl Pts',(6.18104124059857,23.2148307069418,6.76602226241636));
#452719=CARTESIAN_POINT('Ctrl Pts',(5.00873590166638,23.1433476362476,6.69846478576952));
#452720=CARTESIAN_POINT('Ctrl Pts',(4.43020643614535,23.0718645655534,5.67661126055156));
#452721=CARTESIAN_POINT('Ctrl Pts',(4.97555543184771,23.0003814948593,4.63662978245478));
#452722=CARTESIAN_POINT('Ctrl Pts',(6.1450203373264,22.9288984241651,4.5314155623581));
#452723=CARTESIAN_POINT('Ctrl Pts',(6.86739142284002,22.8574153534709,5.4572104595091));
#452724=CARTESIAN_POINT('Ctrl Pts',(6.48037563201499,22.7859322827767,6.56611594115258));
#452725=CARTESIAN_POINT('Ctrl Pts',(5.33946716650399,22.7144492120825,6.8415750418855));
#452726=CARTESIAN_POINT('Ctrl Pts',(4.48814850723257,22.6429661413884,6.03238754075311));
#452727=CARTESIAN_POINT('Ctrl Pts',(4.70999101793355,22.5714830706942,4.87752780133467));
#452728=CARTESIAN_POINT('Ctrl Pts',(5.4325862664886,22.5238276902314,4.58641880376449));
#452729=CARTESIAN_POINT('Ctrl Pts',(5.7755760807344,22.5,4.62591736201901));
#452730=CARTESIAN_POINT('Ctrl Pts',(5.7755760807344,22.5,4.62591736201901));
#452731=CARTESIAN_POINT('Ctrl Pts',(5.73330573132647,22.5,4.61585820529768));
#452732=CARTESIAN_POINT('Ctrl Pts',(5.69054013141041,22.5,4.60871311258362));
#452733=CARTESIAN_POINT('Ctrl Pts',(5.64753211382414,22.5,4.60431335211636));
#452734=CARTESIAN_POINT('Ctrl Pts',(5.60255613397391,22.5,4.59971226726691));
#452735=CARTESIAN_POINT('Ctrl Pts',(5.557314290973,22.5,4.59811321835507));
#452736=CARTESIAN_POINT('Ctrl Pts',(5.51206909394922,22.5,4.59937363334921));
#452737=CARTESIAN_POINT('Ctrl Pts',(5.47721670522078,22.5,4.60034453139419));
#452738=CARTESIAN_POINT('Ctrl Pts',(5.4423616330716,22.5,4.60301317840862));
#452739=CARTESIAN_POINT('Ctrl Pts',(5.40761856297735,22.5,4.60733474482711));
#452740=CARTESIAN_POINT('Ctrl Pts',(5.39607992713772,22.5,4.60876999453373));
#452741=CARTESIAN_POINT('Ctrl Pts',(5.38455362913149,22.5,4.61038770271512));
#452742=CARTESIAN_POINT('Ctrl Pts',(5.37304385113196,22.5,4.61218665032394));
#452743=CARTESIAN_POINT('Ctrl Pts',(5.36511930671851,22.5,4.6134252354838));
#452744=CARTESIAN_POINT('Ctrl Pts',(5.35720517151447,22.5,4.61474939979765));
#452745=CARTESIAN_POINT('Ctrl Pts',(5.34931138805236,22.5,4.61615691477762));
#452746=CARTESIAN_POINT('Ctrl Pts',(5.30303453466167,22.5,4.62440839072526));
#452747=CARTESIAN_POINT('Ctrl Pts',(5.25737359700834,22.5,4.63553334197763));
#452748=CARTESIAN_POINT('Ctrl Pts',(5.2126037699498,22.5,4.64937620694302));
#452749=CARTESIAN_POINT('Ctrl Pts',(5.16694476107272,22.5,4.66349400761069));
#452750=CARTESIAN_POINT('Ctrl Pts',(5.12221145352414,22.5,4.6804387537632));
#452751=CARTESIAN_POINT('Ctrl Pts',(5.07868894732045,22.5,4.70009847065797));
#452752=CARTESIAN_POINT('Ctrl Pts',(5.04899062899618,22.5,4.71351361104013));
#452753=CARTESIAN_POINT('Ctrl Pts',(5.01985594352847,22.5,4.72819401930014));
#452754=CARTESIAN_POINT('Ctrl Pts',(4.99137807844692,22.5,4.74411779584756));
#452755=CARTESIAN_POINT('Ctrl Pts',(4.98326707951891,22.5,4.74865316864099));
#452756=CARTESIAN_POINT('Ctrl Pts',(4.97520938781291,22.5,4.75328947204393));
#452757=CARTESIAN_POINT('Ctrl Pts',(4.96720722656343,22.5,4.75802635928808));
#452758=CARTESIAN_POINT('Ctrl Pts',(4.95959010108946,22.5,4.76253532422516));
#452759=CARTESIAN_POINT('Ctrl Pts',(4.95203124878916,22.5,4.76713073184038));
#452760=CARTESIAN_POINT('Ctrl Pts',(4.94453365155277,22.5,4.77181088041349));
#452761=CARTESIAN_POINT('Ctrl Pts',(4.90274986858405,22.5,4.79789314464756));
#452762=CARTESIAN_POINT('Ctrl Pts',(4.86285502868317,22.5,4.826610852241));
#452763=CARTESIAN_POINT('Ctrl Pts',(4.82514337767408,22.5,4.85783224447811));
#452764=CARTESIAN_POINT('Ctrl Pts',(4.80185182418205,22.5,4.87711526996037));
#452765=CARTESIAN_POINT('Ctrl Pts',(4.77939307000758,22.5,4.89735438402041));
#452766=CARTESIAN_POINT('Ctrl Pts',(4.75783901282981,22.5,4.9185281570127));
#452767=CARTESIAN_POINT('Ctrl Pts',(4.72385034361533,22.5,4.95191715474625));
#452768=CARTESIAN_POINT('Ctrl Pts',(4.69210932076019,22.5,4.98762826934671));
#452769=CARTESIAN_POINT('Ctrl Pts',(4.66265412509277,22.5,5.02537769858569));
#452770=CARTESIAN_POINT('Ctrl Pts',(4.65606489345436,22.5,5.03382237966274));
#452771=CARTESIAN_POINT('Ctrl Pts',(4.64959018437146,22.5,5.04236922201164));
#452772=CARTESIAN_POINT('Ctrl Pts',(4.64323066284989,22.5,5.05101530317395));
#452773=CARTESIAN_POINT('Ctrl Pts',(4.63787530249446,22.5,5.05829617802112));
#452774=CARTESIAN_POINT('Ctrl Pts',(4.63260299860475,22.5,5.06564571345099));
#452775=CARTESIAN_POINT('Ctrl Pts',(4.62742036981385,22.5,5.07305265320345));
#452776=CARTESIAN_POINT('Ctrl Pts',(4.59922209460147,22.5,5.11335322923306));
#452777=CARTESIAN_POINT('Ctrl Pts',(4.57362076198805,22.5,5.15542403883563));
#452778=CARTESIAN_POINT('Ctrl Pts',(4.55062598367203,22.5,5.19892882008167));
#452779=CARTESIAN_POINT('Ctrl Pts',(4.52705592798244,22.5,5.24352199261156));
#452780=CARTESIAN_POINT('Ctrl Pts',(4.50622389130747,22.5,5.28962259945306));
#452781=CARTESIAN_POINT('Ctrl Pts',(4.48817542916681,22.5,5.33691174796499));
#452782=CARTESIAN_POINT('Ctrl Pts',(4.47740085898595,22.5,5.36514242188412));
#452783=CARTESIAN_POINT('Ctrl Pts',(4.46761902478338,22.5,5.39379744240128));
#452784=CARTESIAN_POINT('Ctrl Pts',(4.45884671158303,22.5,5.42281409035157));
#452785=CARTESIAN_POINT('Ctrl Pts',(4.45401588346689,22.5,5.43879327800172));
#452786=CARTESIAN_POINT('Ctrl Pts',(4.44949130096016,22.5,5.4548821890281));
#452787=CARTESIAN_POINT('Ctrl Pts',(4.4452765301246,22.5,5.47107067779953));
#452788=CARTESIAN_POINT('Ctrl Pts',(4.44297713124816,22.5,5.47990242556109));
#452789=CARTESIAN_POINT('Ctrl Pts',(4.44077047507025,22.5,5.48876206567358));
#452790=CARTESIAN_POINT('Ctrl Pts',(4.4386590540276,22.5,5.49763888067812));
#452791=CARTESIAN_POINT('Ctrl Pts',(4.42647927127823,22.5,5.54884500019556));
#452792=CARTESIAN_POINT('Ctrl Pts',(4.41744307914003,22.5,5.60070295226456));
#452793=CARTESIAN_POINT('Ctrl Pts',(4.411605943275,22.5,5.6528725699024));
#452794=CARTESIAN_POINT('Ctrl Pts',(4.4076292437891,22.5,5.68841446860706));
#452795=CARTESIAN_POINT('Ctrl Pts',(4.40513819218715,22.5,5.72410179499005));
#452796=CARTESIAN_POINT('Ctrl Pts',(4.40416293207702,22.5,5.75983273054518));
#452797=CARTESIAN_POINT('Ctrl Pts',(4.40371155802895,22.5,5.77636987469309));
#452798=CARTESIAN_POINT('Ctrl Pts',(4.4035852965956,22.5,5.79292145716924));
#452799=CARTESIAN_POINT('Ctrl Pts',(4.40378695835843,22.5,5.80944675439426));
#452800=CARTESIAN_POINT('Ctrl Pts',(4.40443526815155,22.5,5.86257289925538));
#452801=CARTESIAN_POINT('Ctrl Pts',(4.40846556103476,22.5,5.91547919598232));
#452802=CARTESIAN_POINT('Ctrl Pts',(4.41595519071752,22.5,5.96783294656611));
#452803=CARTESIAN_POINT('Ctrl Pts',(4.41992831406983,22.5,5.99560573612131));
#452804=CARTESIAN_POINT('Ctrl Pts',(4.42487575252187,22.5,6.023223319992));
#452805=CARTESIAN_POINT('Ctrl Pts',(4.43081497898236,22.5,6.05063695240159));
#452806=CARTESIAN_POINT('Ctrl Pts',(4.43420326443596,22.5,6.06627623009907));
#452807=CARTESIAN_POINT('Ctrl Pts',(4.43791441703144,22.5,6.0818491333573));
#452808=CARTESIAN_POINT('Ctrl Pts',(4.44194158662795,22.5,6.09735008669016));
#452809=CARTESIAN_POINT('Ctrl Pts',(6.39006796800885,25.6019615242271,4.92443355077908));
#452810=CARTESIAN_POINT('Ctrl Pts',(6.48712194011206,25.5925650294346,5.02053320993752));
#452811=CARTESIAN_POINT('Ctrl Pts',(6.56580235206401,25.5831685346421,5.13467106978717));
#452812=CARTESIAN_POINT('Ctrl Pts',(6.617556583841,25.5737720398497,5.25993281439039));
#452813=CARTESIAN_POINT('Ctrl Pts',(6.74879528829216,25.5499443496183,5.57757232935519));
#452814=CARTESIAN_POINT('Ctrl Pts',(6.70689021711104,25.5261166593869,5.96674190886751));
#452815=CARTESIAN_POINT('Ctrl Pts',(6.51104990542648,25.5022889691555,6.24916768313609));
#452816=CARTESIAN_POINT('Ctrl Pts',(6.31520959374192,25.4784612789241,6.53159345740467));
#452817=CARTESIAN_POINT('Ctrl Pts',(5.96543404155392,25.4546335886927,6.7072754264295));
#452818=CARTESIAN_POINT('Ctrl Pts',(5.62194684521822,25.4308058984613,6.69573385251462));
#452819=CARTESIAN_POINT('Ctrl Pts',(5.27845964888252,25.4069782082299,6.68419227859974));
#452820=CARTESIAN_POINT('Ctrl Pts',(4.94126080839914,25.3831505179985,6.48542716174514));
#452821=CARTESIAN_POINT('Ctrl Pts',(4.76482193949513,25.3593228277671,6.19049196225386));
#452822=CARTESIAN_POINT('Ctrl Pts',(4.58838307059113,25.3354951375357,5.89555676276259));
#452823=CARTESIAN_POINT('Ctrl Pts',(4.57270417326649,25.3116674473043,5.50445148063464));
#452824=CARTESIAN_POINT('Ctrl Pts',(4.72496603669335,25.2878397570729,5.19633848255872));
#452825=CARTESIAN_POINT('Ctrl Pts',(4.87722790012021,25.2640120668416,4.8882254844828));
#452826=CARTESIAN_POINT('Ctrl Pts',(5.19743052429855,25.2401843766102,4.66310477045891));
#452827=CARTESIAN_POINT('Ctrl Pts',(5.53889211090842,25.2163566863788,4.62410272688105));
#452828=CARTESIAN_POINT('Ctrl Pts',(5.84649605160076,25.1948916323282,4.58896793348097));
#452829=CARTESIAN_POINT('Ctrl Pts',(6.17135209942283,25.1734265782776,4.70487246063661));
#452830=CARTESIAN_POINT('Ctrl Pts',(6.39198798715975,25.151961524227,4.92254817630007));
#452831=CARTESIAN_POINT('Origin',(3.50148276475995,22.5,-3.50148276475995));
#452832=CARTESIAN_POINT('',(7.42462120245875,22.5,7.42462120245875));
#452833=CARTESIAN_POINT('Origin',(0.,22.5,0.));
#452834=CARTESIAN_POINT('Ctrl Pts',(6.64591806159944,22.5,-4.8286920333622));
#452835=CARTESIAN_POINT('Ctrl Pts',(6.6755807993511,22.5,-4.8719367804586));
#452836=CARTESIAN_POINT('Ctrl Pts',(6.70227440867208,22.5,-4.91697381282205));
#452837=CARTESIAN_POINT('Ctrl Pts',(6.72600910610864,22.5,-4.96347942286289));
#452838=CARTESIAN_POINT('Ctrl Pts',(6.75002004749321,22.5,-5.01052630347844));
#452839=CARTESIAN_POINT('Ctrl Pts',(6.77100289981689,22.5,-5.05907736675537));
#452840=CARTESIAN_POINT('Ctrl Pts',(6.78891649180145,22.5,-5.10881343934184));
#452841=CARTESIAN_POINT('Ctrl Pts',(6.8018723011903,22.5,-5.14478450961828));
#452842=CARTESIAN_POINT('Ctrl Pts',(6.81322157811577,22.5,-5.18137581815984));
#452843=CARTESIAN_POINT('Ctrl Pts',(6.82293175279821,22.5,-5.21846626007171));
#452844=CARTESIAN_POINT('Ctrl Pts',(6.82709087591144,22.5,-5.23435307151234));
#452845=CARTESIAN_POINT('Ctrl Pts',(6.83094910537903,22.5,-5.25033142516077));
#452846=CARTESIAN_POINT('Ctrl Pts',(6.83450307899155,22.5,-5.26639159476287));
#452847=CARTESIAN_POINT('Ctrl Pts',(6.83669994897119,22.5,-5.27631910360604));
#452848=CARTESIAN_POINT('Ctrl Pts',(6.83878067256692,22.5,-5.28627904839608));
#452849=CARTESIAN_POINT('Ctrl Pts',(6.84074133407639,22.5,-5.29625198816685));
#452850=CARTESIAN_POINT('Ctrl Pts',(6.85068531168518,22.5,-5.34683220779938));
#452851=CARTESIAN_POINT('Ctrl Pts',(6.85756855485384,22.5,-5.39784710632373));
#452852=CARTESIAN_POINT('Ctrl Pts',(6.86136063350185,22.5,-5.44899668917511));
#452853=CARTESIAN_POINT('Ctrl Pts',(6.86506621321198,22.5,-5.49897952813742));
#452854=CARTESIAN_POINT('Ctrl Pts',(6.86581982211528,22.5,-5.54909202981808));
#452855=CARTESIAN_POINT('Ctrl Pts',(6.86354521213908,22.5,-5.59904614070299));
#452856=CARTESIAN_POINT('Ctrl Pts',(6.86196264981798,22.5,-5.63380176672122));
#452857=CARTESIAN_POINT('Ctrl Pts',(6.85891323510394,22.5,-5.66848055905629));
#452858=CARTESIAN_POINT('Ctrl Pts',(6.85435789422027,22.5,-5.7029791597992));
#452859=CARTESIAN_POINT('Ctrl Pts',(6.85274935352435,22.5,-5.71516099309431));
#452860=CARTESIAN_POINT('Ctrl Pts',(6.85095294331449,22.5,-5.72732029664114));
#452861=CARTESIAN_POINT('Ctrl Pts',(6.84896661755834,22.5,-5.73945229542231));
#452862=CARTESIAN_POINT('Ctrl Pts',(6.8474996850627,22.5,-5.74841196540296));
#452863=CARTESIAN_POINT('Ctrl Pts',(6.84592925278567,22.5,-5.75735562847588));
#452864=CARTESIAN_POINT('Ctrl Pts',(6.84425707988428,22.5,-5.7662692101314));
#452865=CARTESIAN_POINT('Ctrl Pts',(6.83533972756861,22.5,-5.81380349797354));
#452866=CARTESIAN_POINT('Ctrl Pts',(6.82351786766256,22.5,-5.86057802541052));
#452867=CARTESIAN_POINT('Ctrl Pts',(6.80873145081366,22.5,-5.90632961629785));
#452868=CARTESIAN_POINT('Ctrl Pts',(6.79814742517805,22.5,-5.93907832180037));
#452869=CARTESIAN_POINT('Ctrl Pts',(6.78604349567089,22.5,-5.97130269602399));
#452870=CARTESIAN_POINT('Ctrl Pts',(6.77238316128915,22.5,-6.00289829431615));
#452871=CARTESIAN_POINT('Ctrl Pts',(6.75417864027363,22.5,-6.0450043450931));
#452872=CARTESIAN_POINT('Ctrl Pts',(6.73321019789003,22.5,-6.08599501913005));
#452873=CARTESIAN_POINT('Ctrl Pts',(6.70966855565445,22.5,-6.12568011956913));
#452874=CARTESIAN_POINT('Ctrl Pts',(6.70346098498274,22.5,-6.13614447303795));
#452875=CARTESIAN_POINT('Ctrl Pts',(6.69707438313402,22.5,-6.1465178772431));
#452876=CARTESIAN_POINT('Ctrl Pts',(6.690512023297,22.5,-6.15679645323974));
#452877=CARTESIAN_POINT('Ctrl Pts',(6.68556313817567,22.5,-6.16454785564401));
#452878=CARTESIAN_POINT('Ctrl Pts',(6.68051415735856,22.5,-6.17224531916678));
#452879=CARTESIAN_POINT('Ctrl Pts',(6.67537489362519,22.5,-6.17987521962693));
#452880=CARTESIAN_POINT('Ctrl Pts',(6.6484247679217,22.5,-6.21988616033247));
#452881=CARTESIAN_POINT('Ctrl Pts',(6.61894162109436,22.5,-6.25812741400869));
#452882=CARTESIAN_POINT('Ctrl Pts',(6.58718324847867,22.5,-6.29441170519143));
#452883=CARTESIAN_POINT('Ctrl Pts',(6.55551163430383,22.5,-6.33059687389808));
#452884=CARTESIAN_POINT('Ctrl Pts',(6.52157609264422,22.5,-6.36483641853547));
#452885=CARTESIAN_POINT('Ctrl Pts',(6.48560329452573,22.5,-6.39690234768395));
#452886=CARTESIAN_POINT('Ctrl Pts',(6.46634118603625,22.5,-6.41407247173267));
#452887=CARTESIAN_POINT('Ctrl Pts',(6.44649455979684,22.5,-6.4306185943358));
#452888=CARTESIAN_POINT('Ctrl Pts',(6.42609644694928,22.5,-6.44649972129179));
#452889=CARTESIAN_POINT('Ctrl Pts',(6.41550137782644,22.5,-6.45474860387739));
#452890=CARTESIAN_POINT('Ctrl Pts',(6.40475750959663,22.5,-6.46281800341801));
#452891=CARTESIAN_POINT('Ctrl Pts',(6.3938694226933,22.5,-6.47070167900491));
#452892=CARTESIAN_POINT('Ctrl Pts',(6.3855291898448,22.5,-6.47674054429691));
#452893=CARTESIAN_POINT('Ctrl Pts',(6.37710396966129,22.5,-6.48267052699799));
#452894=CARTESIAN_POINT('Ctrl Pts',(6.36860849913158,22.5,-6.48848046707363));
#452895=CARTESIAN_POINT('Ctrl Pts',(6.33038178349398,22.5,-6.51462321294818));
#452896=CARTESIAN_POINT('Ctrl Pts',(6.29067294978169,22.5,-6.53838419609424));
#452897=CARTESIAN_POINT('Ctrl Pts',(6.24968947052795,22.5,-6.55954587135352));
#452898=CARTESIAN_POINT('Ctrl Pts',(6.2220434631434,22.5,-6.57382078995829));
#452899=CARTESIAN_POINT('Ctrl Pts',(6.1938170783215,22.5,-6.58691199092427));
#452900=CARTESIAN_POINT('Ctrl Pts',(6.16507259987822,22.5,-6.59873928463863));
#452901=CARTESIAN_POINT('Ctrl Pts',(6.15266397552728,22.5,-6.60384497633101));
#452902=CARTESIAN_POINT('Ctrl Pts',(6.14015674557275,22.5,-6.60871552223012));
#452903=CARTESIAN_POINT('Ctrl Pts',(6.12757735909169,22.5,-6.61333659562422));
#452904=CARTESIAN_POINT('Ctrl Pts',(6.08619113933328,22.5,-6.6285399411368));
#452905=CARTESIAN_POINT('Ctrl Pts',(6.04397428611167,22.5,-6.64106838660522));
#452906=CARTESIAN_POINT('Ctrl Pts',(6.00111091241908,22.5,-6.65070263631015));
#452907=CARTESIAN_POINT('Ctrl Pts',(5.97991194550769,22.5,-6.6554674535216));
#452908=CARTESIAN_POINT('Ctrl Pts',(5.95855482028607,22.5,-6.65952358177559));
#452909=CARTESIAN_POINT('Ctrl Pts',(5.93706218561481,22.5,-6.66283972884874));
#452910=CARTESIAN_POINT('Ctrl Pts',(5.92425778841234,22.5,-6.66481534816932));
#452911=CARTESIAN_POINT('Ctrl Pts',(5.91140530098883,22.5,-6.66652825557881));
#452912=CARTESIAN_POINT('Ctrl Pts',(5.89851203167795,22.5,-6.66798006829994));
#452913=CARTESIAN_POINT('Ctrl Pts',(4.62591736201901,22.5,-5.7755760807344));
#452914=CARTESIAN_POINT('Ctrl Pts',(4.61585820529768,22.5,-5.73330573132648));
#452915=CARTESIAN_POINT('Ctrl Pts',(4.60871311258362,22.5,-5.69054013141041));
#452916=CARTESIAN_POINT('Ctrl Pts',(4.60431335211636,22.5,-5.64753211382415));
#452917=CARTESIAN_POINT('Ctrl Pts',(4.59971226726699,22.5,-5.60255613397477));
#452918=CARTESIAN_POINT('Ctrl Pts',(4.59811321835513,22.5,-5.5573142909747));
#452919=CARTESIAN_POINT('Ctrl Pts',(4.59937363334914,22.5,-5.51206909395177));
#452920=CARTESIAN_POINT('Ctrl Pts',(4.60034453139403,22.5,-5.47721670522323));
#452921=CARTESIAN_POINT('Ctrl Pts',(4.6030131784084,22.5,-5.4423616330739));
#452922=CARTESIAN_POINT('Ctrl Pts',(4.60733474482684,22.5,-5.40761856297955));
#452923=CARTESIAN_POINT('Ctrl Pts',(4.6087699944925,22.5,-5.39607992746903));
#452924=CARTESIAN_POINT('Ctrl Pts',(4.61038770262252,22.5,-5.38455362979122));
#452925=CARTESIAN_POINT('Ctrl Pts',(4.61218665016966,22.5,-5.37304385211902));
#452926=CARTESIAN_POINT('Ctrl Pts',(4.61342523528797,22.5,-5.36511930792512));
#452927=CARTESIAN_POINT('Ctrl Pts',(4.61474939955571,22.5,-5.35720517293886));
#452928=CARTESIAN_POINT('Ctrl Pts',(4.61615691448497,22.5,-5.3493113896936));
#452929=CARTESIAN_POINT('Ctrl Pts',(4.62440839035928,22.5,-5.30303453631806));
#452930=CARTESIAN_POINT('Ctrl Pts',(4.63553334153678,22.5,-5.25737359867573));
#452931=CARTESIAN_POINT('Ctrl Pts',(4.64937620642544,22.5,-5.21260377162372));
#452932=CARTESIAN_POINT('Ctrl Pts',(4.66349400702439,22.5,-5.16694476272245));
#452933=CARTESIAN_POINT('Ctrl Pts',(4.68043875311008,22.5,-5.12221145514625));
#452934=CARTESIAN_POINT('Ctrl Pts',(4.70009846993925,22.5,-5.07868894891155));
#452935=CARTESIAN_POINT('Ctrl Pts',(4.71351361033608,22.5,-5.04899063043454));
#452936=CARTESIAN_POINT('Ctrl Pts',(4.72819401862254,22.5,-5.01985594481751));
#452937=CARTESIAN_POINT('Ctrl Pts',(4.74411779520772,22.5,-4.99137807959121));
#452938=CARTESIAN_POINT('Ctrl Pts',(4.7486531673282,22.5,-4.98326708184471));
#452939=CARTESIAN_POINT('Ctrl Pts',(4.75328947002864,22.5,-4.97520939130455));
#452940=CARTESIAN_POINT('Ctrl Pts',(4.75802635654096,22.5,-4.96720723120421));
#452941=CARTESIAN_POINT('Ctrl Pts',(4.76253532219619,22.5,-4.95959010443409));
#452942=CARTESIAN_POINT('Ctrl Pts',(4.7671307305627,22.5,-4.95203125085003));
#452943=CARTESIAN_POINT('Ctrl Pts',(4.7718108799136,22.5,-4.9445336523536));
#452944=CARTESIAN_POINT('Ctrl Pts',(4.79789314411416,22.5,-4.90274986936038));
#452945=CARTESIAN_POINT('Ctrl Pts',(4.82661085167514,22.5,-4.86285502943318));
#452946=CARTESIAN_POINT('Ctrl Pts',(4.85783224388052,22.5,-4.8251433783959));
#452947=CARTESIAN_POINT('Ctrl Pts',(4.87711526954221,22.5,-4.80185182464605));
#452948=CARTESIAN_POINT('Ctrl Pts',(4.89735438380168,22.5,-4.77939307023024));
#452949=CARTESIAN_POINT('Ctrl Pts',(4.9185281570127,22.5,-4.75783901282981));
#452950=CARTESIAN_POINT('Ctrl Pts',(4.95191715474625,22.5,-4.72385034361532));
#452951=CARTESIAN_POINT('Ctrl Pts',(4.98762826934674,22.5,-4.69210932076016));
#452952=CARTESIAN_POINT('Ctrl Pts',(5.02537769858573,22.5,-4.66265412509274));
#452953=CARTESIAN_POINT('Ctrl Pts',(5.03382237964628,22.5,-4.6560648934672));
#452954=CARTESIAN_POINT('Ctrl Pts',(5.04236922197827,22.5,-4.64959018439674));
#452955=CARTESIAN_POINT('Ctrl Pts',(5.0510153031233,22.5,-4.64323066288715));
#452956=CARTESIAN_POINT('Ctrl Pts',(5.05829617800763,22.5,-4.63787530250376));
#452957=CARTESIAN_POINT('Ctrl Pts',(5.06564571347538,22.5,-4.63260299858695));
#452958=CARTESIAN_POINT('Ctrl Pts',(5.07305265326631,22.5,-4.62742036976986));
#452959=CARTESIAN_POINT('Ctrl Pts',(5.1133532292971,22.5,-4.59922209456066));
#452960=CARTESIAN_POINT('Ctrl Pts',(5.15542403890062,22.5,-4.57362076195032));
#452961=CARTESIAN_POINT('Ctrl Pts',(5.19892882014737,22.5,-4.55062598363731));
#452962=CARTESIAN_POINT('Ctrl Pts',(5.24352199267827,22.5,-4.52705592795066));
#452963=CARTESIAN_POINT('Ctrl Pts',(5.28962259952057,22.5,-4.50622389127859));
#452964=CARTESIAN_POINT('Ctrl Pts',(5.33691174803316,22.5,-4.48817542914079));
#452965=CARTESIAN_POINT('Ctrl Pts',(5.36514242195013,22.5,-4.47740085896262));
#452966=CARTESIAN_POINT('Ctrl Pts',(5.39379744246496,22.5,-4.46761902476255));
#452967=CARTESIAN_POINT('Ctrl Pts',(5.42281409041283,22.5,-4.45884671156451));
#452968=CARTESIAN_POINT('Ctrl Pts',(5.4387932780761,22.5,-4.45401588344527));
#452969=CARTESIAN_POINT('Ctrl Pts',(5.4548821891158,22.5,-4.44949130093593));
#452970=CARTESIAN_POINT('Ctrl Pts',(5.47107067790065,22.5,-4.44527653009828));
#452971=CARTESIAN_POINT('Ctrl Pts',(5.47990242565713,22.5,-4.44297713122391));
#452972=CARTESIAN_POINT('Ctrl Pts',(5.48876206576444,22.5,-4.440770475048));
#452973=CARTESIAN_POINT('Ctrl Pts',(5.49763888076378,22.5,-4.43865905400722));
#452974=CARTESIAN_POINT('Ctrl Pts',(5.54884500028241,22.5,-4.42647927126125));
#452975=CARTESIAN_POINT('Ctrl Pts',(5.60070295235243,22.5,-4.41744307912653));
#452976=CARTESIAN_POINT('Ctrl Pts',(5.6528725699911,22.5,-4.41160594326508));
#452977=CARTESIAN_POINT('Ctrl Pts',(5.68841446871037,22.5,-4.40762924378005));
#452978=CARTESIAN_POINT('Ctrl Pts',(5.72410179510797,22.5,-4.40513819218018));
#452979=CARTESIAN_POINT('Ctrl Pts',(5.75983273067766,22.5,-4.4041629320734));
#452980=CARTESIAN_POINT('Ctrl Pts',(5.77636987481073,22.5,-4.40371155802747));
#452981=CARTESIAN_POINT('Ctrl Pts',(5.79292145727197,22.5,-4.4035852965957));
#452982=CARTESIAN_POINT('Ctrl Pts',(5.80944675448204,22.5,-4.40378695835951));
#452983=CARTESIAN_POINT('Ctrl Pts',(5.86257289934304,22.5,-4.40443526815635));
#452984=CARTESIAN_POINT('Ctrl Pts',(5.91547919606967,22.5,-4.40846556104334));
#452985=CARTESIAN_POINT('Ctrl Pts',(5.96783294665298,22.5,-4.41595519072995));
#452986=CARTESIAN_POINT('Ctrl Pts',(5.99560573617887,22.5,-4.41992831408015));
#452987=CARTESIAN_POINT('Ctrl Pts',(6.02322332002059,22.5,-4.42487575252807));
#452988=CARTESIAN_POINT('Ctrl Pts',(6.05063695240159,22.5,-4.43081497898236));
#452989=CARTESIAN_POINT('Ctrl Pts',(6.06627623009907,22.5,-4.43420326443596));
#452990=CARTESIAN_POINT('Ctrl Pts',(6.0818491333573,22.5,-4.43791441703144));
#452991=CARTESIAN_POINT('Ctrl Pts',(6.09735008669015,22.5,-4.44194158662795));
#452992=CARTESIAN_POINT('Ctrl Pts',(-4.8286920333622,22.5,-6.64591806159944));
#452993=CARTESIAN_POINT('Ctrl Pts',(-4.8719367804586,22.5,-6.6755807993511));
#452994=CARTESIAN_POINT('Ctrl Pts',(-4.91697381282206,22.5,-6.70227440867209));
#452995=CARTESIAN_POINT('Ctrl Pts',(-4.9634794228629,22.5,-6.72600910610865));
#452996=CARTESIAN_POINT('Ctrl Pts',(-5.01052630347777,22.5,-6.75002004749286));
#452997=CARTESIAN_POINT('Ctrl Pts',(-5.05907736675395,22.5,-6.77100289981628));
#452998=CARTESIAN_POINT('Ctrl Pts',(-5.10881343933966,22.5,-6.78891649180067));
#452999=CARTESIAN_POINT('Ctrl Pts',(-5.14478450961618,22.5,-6.80187230118961));
#453000=CARTESIAN_POINT('Ctrl Pts',(-5.18137581815778,22.5,-6.81322157811517));
#453001=CARTESIAN_POINT('Ctrl Pts',(-5.21846626006973,22.5,-6.82293175279769));
#453002=CARTESIAN_POINT('Ctrl Pts',(-5.23435307150809,22.5,-6.82709087591036));
#453003=CARTESIAN_POINT('Ctrl Pts',(-5.25033142515424,22.5,-6.83094910537747));
#453004=CARTESIAN_POINT('Ctrl Pts',(-5.26639159475403,22.5,-6.8345030789896));
#453005=CARTESIAN_POINT('Ctrl Pts',(-5.27631910353288,22.5,-6.83669994895507));
#453006=CARTESIAN_POINT('Ctrl Pts',(-5.28627904825824,22.5,-6.83878067253816));
#453007=CARTESIAN_POINT('Ctrl Pts',(-5.29625198796418,22.5,-6.84074133403655));
#453008=CARTESIAN_POINT('Ctrl Pts',(-5.34683220759866,22.5,-6.85068531165414));
#453009=CARTESIAN_POINT('Ctrl Pts',(-5.39784710612543,22.5,-6.85756855483123));
#453010=CARTESIAN_POINT('Ctrl Pts',(-5.44899668897961,22.5,-6.86136063348736));
#453011=CARTESIAN_POINT('Ctrl Pts',(-5.49897952794281,22.5,-6.86506621320529));
#453012=CARTESIAN_POINT('Ctrl Pts',(-5.54909202962473,22.5,-6.86581982211631));
#453013=CARTESIAN_POINT('Ctrl Pts',(-5.59904614051128,22.5,-6.8635452121478));
#453014=CARTESIAN_POINT('Ctrl Pts',(-5.63380176654577,22.5,-6.86196264983138));
#453015=CARTESIAN_POINT('Ctrl Pts',(-5.66848055889722,22.5,-6.85891323512072));
#453016=CARTESIAN_POINT('Ctrl Pts',(-5.70297915965648,22.5,-6.85435789423911));
#453017=CARTESIAN_POINT('Ctrl Pts',(-5.71516099264261,22.5,-6.85274935358548));
#453018=CARTESIAN_POINT('Ctrl Pts',(-5.72732029588166,22.5,-6.85095294342745));
#453019=CARTESIAN_POINT('Ctrl Pts',(-5.73945229435654,22.5,-6.84896661773283));
#453020=CARTESIAN_POINT('Ctrl Pts',(-5.74841196443544,22.5,-6.84749968522951));
#453021=CARTESIAN_POINT('Ctrl Pts',(-5.75735562760714,22.5,-6.84592925294246));
#453022=CARTESIAN_POINT('Ctrl Pts',(-5.76626920936078,22.5,-6.84425708002884));
#453023=CARTESIAN_POINT('Ctrl Pts',(-5.81380349721498,22.5,-6.83533972774389));
#453024=CARTESIAN_POINT('Ctrl Pts',(-5.86057802466526,22.5,-6.82351786786828));
#453025=CARTESIAN_POINT('Ctrl Pts',(-5.9063296155672,22.5,-6.8087314510498));
#453026=CARTESIAN_POINT('Ctrl Pts',(-5.93907832132107,22.5,-6.79814742535809));
#453027=CARTESIAN_POINT('Ctrl Pts',(-5.97130269578902,22.5,-6.78604349577248));
#453028=CARTESIAN_POINT('Ctrl Pts',(-6.00289829431615,22.5,-6.77238316128915));
#453029=CARTESIAN_POINT('Ctrl Pts',(-6.0450043450931,22.5,-6.75417864027363));
#453030=CARTESIAN_POINT('Ctrl Pts',(-6.08599501913005,22.5,-6.73321019789003));
#453031=CARTESIAN_POINT('Ctrl Pts',(-6.12568011956913,22.5,-6.70966855565445));
#453032=CARTESIAN_POINT('Ctrl Pts',(-6.13614447303768,22.5,-6.7034609849829));
#453033=CARTESIAN_POINT('Ctrl Pts',(-6.14651787724254,22.5,-6.69707438313436));
#453034=CARTESIAN_POINT('Ctrl Pts',(-6.15679645323891,22.5,-6.69051202329753));
#453035=CARTESIAN_POINT('Ctrl Pts',(-6.164547855591,22.5,-6.68556313820952));
#453036=CARTESIAN_POINT('Ctrl Pts',(-6.17224531906237,22.5,-6.68051415742705));
#453037=CARTESIAN_POINT('Ctrl Pts',(-6.17987521947202,22.5,-6.67537489372953));
#453038=CARTESIAN_POINT('Ctrl Pts',(-6.21988616018154,22.5,-6.64842476803299));
#453039=CARTESIAN_POINT('Ctrl Pts',(-6.25812741386204,22.5,-6.61894162121229));
#453040=CARTESIAN_POINT('Ctrl Pts',(-6.29441170504936,22.5,-6.58718324860302));
#453041=CARTESIAN_POINT('Ctrl Pts',(-6.33059687376143,22.5,-6.55551163443383));
#453042=CARTESIAN_POINT('Ctrl Pts',(-6.36483641840449,22.5,-6.52157609277951));
#453043=CARTESIAN_POINT('Ctrl Pts',(-6.39690234755893,22.5,-6.48560329466599));
#453044=CARTESIAN_POINT('Ctrl Pts',(-6.41407247161589,22.5,-6.4663411861735));
#453045=CARTESIAN_POINT('Ctrl Pts',(-6.43061859422698,22.5,-6.44649455993064));
#453046=CARTESIAN_POINT('Ctrl Pts',(-6.44649972119062,22.5,-6.42609644707924));
#453047=CARTESIAN_POINT('Ctrl Pts',(-6.4547486037322,22.5,-6.41550137801605));
#453048=CARTESIAN_POINT('Ctrl Pts',(-6.46281800323078,22.5,-6.40475750984752));
#453049=CARTESIAN_POINT('Ctrl Pts',(-6.47070167877777,22.5,-6.39386942300701));
#453050=CARTESIAN_POINT('Ctrl Pts',(-6.47674054409838,22.5,-6.38552919012489));
#453051=CARTESIAN_POINT('Ctrl Pts',(-6.48267052682731,22.5,-6.37710396990682));
#453052=CARTESIAN_POINT('Ctrl Pts',(-6.48848046692978,22.5,-6.36860849934192));
#453053=CARTESIAN_POINT('Ctrl Pts',(-6.51462321281365,22.5,-6.33038178370894));
#453054=CARTESIAN_POINT('Ctrl Pts',(-6.53838419596926,22.5,-6.29067295000084));
#453055=CARTESIAN_POINT('Ctrl Pts',(-6.55954587123842,22.5,-6.24968947075085));
#453056=CARTESIAN_POINT('Ctrl Pts',(-6.5738207898325,22.5,-6.22204346340245));
#453057=CARTESIAN_POINT('Ctrl Pts',(-6.58691199079083,22.5,-6.1938170786179));
#453058=CARTESIAN_POINT('Ctrl Pts',(-6.59873928450088,22.5,-6.16507260021298));
#453059=CARTESIAN_POINT('Ctrl Pts',(-6.60384497623248,22.5,-6.15266397577878));
#453060=CARTESIAN_POINT('Ctrl Pts',(-6.60871552216769,22.5,-6.14015674573947));
#453061=CARTESIAN_POINT('Ctrl Pts',(-6.61333659559451,22.5,-6.12757735917257));
#453062=CARTESIAN_POINT('Ctrl Pts',(-6.62853994111127,22.5,-6.08619113941338));
#453063=CARTESIAN_POINT('Ctrl Pts',(-6.64106838658374,22.5,-6.04397428619079));
#453064=CARTESIAN_POINT('Ctrl Pts',(-6.65070263629263,22.5,-6.00111091249705));
#453065=CARTESIAN_POINT('Ctrl Pts',(-6.65546745351165,22.5,-5.97991194556006));
#453066=CARTESIAN_POINT('Ctrl Pts',(-6.65952358177152,22.5,-5.95855482031242));
#453067=CARTESIAN_POINT('Ctrl Pts',(-6.66283972884874,22.5,-5.93706218561481));
#453068=CARTESIAN_POINT('Ctrl Pts',(-6.66481534816932,22.5,-5.92425778841234));
#453069=CARTESIAN_POINT('Ctrl Pts',(-6.66652825557881,22.5,-5.91140530098883));
#453070=CARTESIAN_POINT('Ctrl Pts',(-6.66798006829994,22.5,-5.89851203167795));
#453071=CARTESIAN_POINT('Ctrl Pts',(-5.7755760807344,22.5,-4.62591736201901));
#453072=CARTESIAN_POINT('Ctrl Pts',(-5.73330573132648,22.5,-4.61585820529768));
#453073=CARTESIAN_POINT('Ctrl Pts',(-5.69054013141041,22.5,-4.60871311258362));
#453074=CARTESIAN_POINT('Ctrl Pts',(-5.64753211382415,22.5,-4.60431335211636));
#453075=CARTESIAN_POINT('Ctrl Pts',(-5.60255613397477,22.5,-4.59971226726699));
#453076=CARTESIAN_POINT('Ctrl Pts',(-5.5573142909747,22.5,-4.59811321835513));
#453077=CARTESIAN_POINT('Ctrl Pts',(-5.51206909395177,22.5,-4.59937363334914));
#453078=CARTESIAN_POINT('Ctrl Pts',(-5.47721670522323,22.5,-4.60034453139403));
#453079=CARTESIAN_POINT('Ctrl Pts',(-5.4423616330739,22.5,-4.6030131784084));
#453080=CARTESIAN_POINT('Ctrl Pts',(-5.40761856297955,22.5,-4.60733474482684));
#453081=CARTESIAN_POINT('Ctrl Pts',(-5.39607992746903,22.5,-4.6087699944925));
#453082=CARTESIAN_POINT('Ctrl Pts',(-5.38455362979122,22.5,-4.61038770262252));
#453083=CARTESIAN_POINT('Ctrl Pts',(-5.37304385211902,22.5,-4.61218665016966));
#453084=CARTESIAN_POINT('Ctrl Pts',(-5.36511930792512,22.5,-4.61342523528797));
#453085=CARTESIAN_POINT('Ctrl Pts',(-5.35720517293886,22.5,-4.61474939955571));
#453086=CARTESIAN_POINT('Ctrl Pts',(-5.3493113896936,22.5,-4.61615691448497));
#453087=CARTESIAN_POINT('Ctrl Pts',(-5.30303453631806,22.5,-4.62440839035928));
#453088=CARTESIAN_POINT('Ctrl Pts',(-5.25737359867573,22.5,-4.63553334153678));
#453089=CARTESIAN_POINT('Ctrl Pts',(-5.21260377162372,22.5,-4.64937620642544));
#453090=CARTESIAN_POINT('Ctrl Pts',(-5.16694476272245,22.5,-4.66349400702439));
#453091=CARTESIAN_POINT('Ctrl Pts',(-5.12221145514625,22.5,-4.68043875311008));
#453092=CARTESIAN_POINT('Ctrl Pts',(-5.07868894891155,22.5,-4.70009846993925));
#453093=CARTESIAN_POINT('Ctrl Pts',(-5.04899063043454,22.5,-4.71351361033608));
#453094=CARTESIAN_POINT('Ctrl Pts',(-5.01985594481751,22.5,-4.72819401862254));
#453095=CARTESIAN_POINT('Ctrl Pts',(-4.99137807959121,22.5,-4.74411779520772));
#453096=CARTESIAN_POINT('Ctrl Pts',(-4.98326708184471,22.5,-4.7486531673282));
#453097=CARTESIAN_POINT('Ctrl Pts',(-4.97520939130455,22.5,-4.75328947002864));
#453098=CARTESIAN_POINT('Ctrl Pts',(-4.96720723120421,22.5,-4.75802635654096));
#453099=CARTESIAN_POINT('Ctrl Pts',(-4.95959010443409,22.5,-4.76253532219619));
#453100=CARTESIAN_POINT('Ctrl Pts',(-4.95203125085003,22.5,-4.7671307305627));
#453101=CARTESIAN_POINT('Ctrl Pts',(-4.9445336523536,22.5,-4.7718108799136));
#453102=CARTESIAN_POINT('Ctrl Pts',(-4.90274986936038,22.5,-4.79789314411416));
#453103=CARTESIAN_POINT('Ctrl Pts',(-4.86285502943318,22.5,-4.82661085167514));
#453104=CARTESIAN_POINT('Ctrl Pts',(-4.8251433783959,22.5,-4.85783224388052));
#453105=CARTESIAN_POINT('Ctrl Pts',(-4.80185182464605,22.5,-4.87711526954221));
#453106=CARTESIAN_POINT('Ctrl Pts',(-4.77939307023024,22.5,-4.89735438380168));
#453107=CARTESIAN_POINT('Ctrl Pts',(-4.75783901282981,22.5,-4.9185281570127));
#453108=CARTESIAN_POINT('Ctrl Pts',(-4.72385034361532,22.5,-4.95191715474625));
#453109=CARTESIAN_POINT('Ctrl Pts',(-4.69210932076016,22.5,-4.98762826934674));
#453110=CARTESIAN_POINT('Ctrl Pts',(-4.66265412509274,22.5,-5.02537769858573));
#453111=CARTESIAN_POINT('Ctrl Pts',(-4.6560648934672,22.5,-5.03382237964628));
#453112=CARTESIAN_POINT('Ctrl Pts',(-4.64959018439674,22.5,-5.04236922197827));
#453113=CARTESIAN_POINT('Ctrl Pts',(-4.64323066288715,22.5,-5.0510153031233));
#453114=CARTESIAN_POINT('Ctrl Pts',(-4.63787530250376,22.5,-5.05829617800763));
#453115=CARTESIAN_POINT('Ctrl Pts',(-4.63260299858695,22.5,-5.06564571347538));
#453116=CARTESIAN_POINT('Ctrl Pts',(-4.62742036976986,22.5,-5.07305265326631));
#453117=CARTESIAN_POINT('Ctrl Pts',(-4.59922209456066,22.5,-5.1133532292971));
#453118=CARTESIAN_POINT('Ctrl Pts',(-4.57362076195032,22.5,-5.15542403890062));
#453119=CARTESIAN_POINT('Ctrl Pts',(-4.55062598363731,22.5,-5.19892882014737));
#453120=CARTESIAN_POINT('Ctrl Pts',(-4.52705592795066,22.5,-5.24352199267827));
#453121=CARTESIAN_POINT('Ctrl Pts',(-4.50622389127859,22.5,-5.28962259952057));
#453122=CARTESIAN_POINT('Ctrl Pts',(-4.48817542914079,22.5,-5.33691174803316));
#453123=CARTESIAN_POINT('Ctrl Pts',(-4.47740085896262,22.5,-5.36514242195013));
#453124=CARTESIAN_POINT('Ctrl Pts',(-4.46761902476255,22.5,-5.39379744246496));
#453125=CARTESIAN_POINT('Ctrl Pts',(-4.45884671156451,22.5,-5.42281409041283));
#453126=CARTESIAN_POINT('Ctrl Pts',(-4.45401588344527,22.5,-5.4387932780761));
#453127=CARTESIAN_POINT('Ctrl Pts',(-4.44949130093593,22.5,-5.4548821891158));
#453128=CARTESIAN_POINT('Ctrl Pts',(-4.44527653009828,22.5,-5.47107067790065));
#453129=CARTESIAN_POINT('Ctrl Pts',(-4.44297713122391,22.5,-5.47990242565713));
#453130=CARTESIAN_POINT('Ctrl Pts',(-4.440770475048,22.5,-5.48876206576444));
#453131=CARTESIAN_POINT('Ctrl Pts',(-4.43865905400722,22.5,-5.49763888076378));
#453132=CARTESIAN_POINT('Ctrl Pts',(-4.42647927126125,22.5,-5.54884500028241));
#453133=CARTESIAN_POINT('Ctrl Pts',(-4.41744307912653,22.5,-5.60070295235243));
#453134=CARTESIAN_POINT('Ctrl Pts',(-4.41160594326508,22.5,-5.6528725699911));
#453135=CARTESIAN_POINT('Ctrl Pts',(-4.40762924378005,22.5,-5.68841446871037));
#453136=CARTESIAN_POINT('Ctrl Pts',(-4.40513819218018,22.5,-5.72410179510797));
#453137=CARTESIAN_POINT('Ctrl Pts',(-4.4041629320734,22.5,-5.75983273067766));
#453138=CARTESIAN_POINT('Ctrl Pts',(-4.40371155802747,22.5,-5.77636987481073));
#453139=CARTESIAN_POINT('Ctrl Pts',(-4.4035852965957,22.5,-5.79292145727197));
#453140=CARTESIAN_POINT('Ctrl Pts',(-4.40378695835951,22.5,-5.80944675448204));
#453141=CARTESIAN_POINT('Ctrl Pts',(-4.40443526815635,22.5,-5.86257289934304));
#453142=CARTESIAN_POINT('Ctrl Pts',(-4.40846556104334,22.5,-5.91547919606967));
#453143=CARTESIAN_POINT('Ctrl Pts',(-4.41595519072995,22.5,-5.96783294665298));
#453144=CARTESIAN_POINT('Ctrl Pts',(-4.41992831408015,22.5,-5.99560573617887));
#453145=CARTESIAN_POINT('Ctrl Pts',(-4.42487575252807,22.5,-6.02322332002059));
#453146=CARTESIAN_POINT('Ctrl Pts',(-4.43081497898236,22.5,-6.05063695240159));
#453147=CARTESIAN_POINT('Ctrl Pts',(-4.43420326443596,22.5,-6.06627623009907));
#453148=CARTESIAN_POINT('Ctrl Pts',(-4.43791441703144,22.5,-6.0818491333573));
#453149=CARTESIAN_POINT('Ctrl Pts',(-4.44194158662795,22.5,-6.09735008669015));
#453150=CARTESIAN_POINT('Ctrl Pts',(-6.64591806159944,22.5,4.8286920333622));
#453151=CARTESIAN_POINT('Ctrl Pts',(-6.6755807993511,22.5,4.8719367804586));
#453152=CARTESIAN_POINT('Ctrl Pts',(-6.7022744086721,22.5,4.91697381282208));
#453153=CARTESIAN_POINT('Ctrl Pts',(-6.72600910610866,22.5,4.96347942286292));
#453154=CARTESIAN_POINT('Ctrl Pts',(-6.750020047493,22.5,5.01052630347802));
#453155=CARTESIAN_POINT('Ctrl Pts',(-6.77100289981649,22.5,5.05907736675444));
#453156=CARTESIAN_POINT('Ctrl Pts',(-6.78891649180094,22.5,5.10881343934042));
#453157=CARTESIAN_POINT('Ctrl Pts',(-6.80187230118985,22.5,5.14478450961691));
#453158=CARTESIAN_POINT('Ctrl Pts',(-6.81322157811539,22.5,5.18137581815852));
#453159=CARTESIAN_POINT('Ctrl Pts',(-6.82293175279788,22.5,5.21846626007043));
#453160=CARTESIAN_POINT('Ctrl Pts',(-6.82709087591091,22.5,5.23435307151024));
#453161=CARTESIAN_POINT('Ctrl Pts',(-6.83094910537833,22.5,5.25033142515782));
#453162=CARTESIAN_POINT('Ctrl Pts',(-6.83450307899072,22.5,5.26639159475908));
#453163=CARTESIAN_POINT('Ctrl Pts',(-6.83669994896103,22.5,5.27631910355995));
#453164=CARTESIAN_POINT('Ctrl Pts',(-6.83878067254843,22.5,5.28627904830748));
#453165=CARTESIAN_POINT('Ctrl Pts',(-6.8407413340506,22.5,5.29625198803563));
#453166=CARTESIAN_POINT('Ctrl Pts',(-6.8506853116647,22.5,5.34683220766748));
#453167=CARTESIAN_POINT('Ctrl Pts',(-6.85756855483867,22.5,5.39784710619139));
#453168=CARTESIAN_POINT('Ctrl Pts',(-6.86136063349203,22.5,5.44899668904261));
#453169=CARTESIAN_POINT('Ctrl Pts',(-6.86506621320742,22.5,5.4989795280052));
#453170=CARTESIAN_POINT('Ctrl Pts',(-6.86581982211597,22.5,5.5490920296864));
#453171=CARTESIAN_POINT('Ctrl Pts',(-6.86354521214504,22.5,5.59904614057211));
#453172=CARTESIAN_POINT('Ctrl Pts',(-6.86196264982713,22.5,5.63380176660143));
#453173=CARTESIAN_POINT('Ctrl Pts',(-6.8589132351154,22.5,5.66848055894767));
#453174=CARTESIAN_POINT('Ctrl Pts',(-6.85435789423314,22.5,5.70297915970175));
#453175=CARTESIAN_POINT('Ctrl Pts',(-6.85274935356602,22.5,5.71516099278645));
#453176=CARTESIAN_POINT('Ctrl Pts',(-6.85095294339145,22.5,5.72732029612368));
#453177=CARTESIAN_POINT('Ctrl Pts',(-6.84896661767721,22.5,5.73945229469627));
#453178=CARTESIAN_POINT('Ctrl Pts',(-6.84749968518305,22.5,5.74841196470285));
#453179=CARTESIAN_POINT('Ctrl Pts',(-6.84592925290685,22.5,5.75735562780225));
#453180=CARTESIAN_POINT('Ctrl Pts',(-6.84425708000572,22.5,5.76626920948405));
#453181=CARTESIAN_POINT('Ctrl Pts',(-6.83533972771596,22.5,5.81380349733577));
#453182=CARTESIAN_POINT('Ctrl Pts',(-6.82351786783565,22.5,5.86057802478339));
#453183=CARTESIAN_POINT('Ctrl Pts',(-6.80873145101255,22.5,5.90632961568247));
#453184=CARTESIAN_POINT('Ctrl Pts',(-6.79814742532969,22.5,5.93907832139669));
#453185=CARTESIAN_POINT('Ctrl Pts',(-6.78604349575646,22.5,5.97130269582608));
#453186=CARTESIAN_POINT('Ctrl Pts',(-6.77238316128915,22.5,6.00289829431615));
#453187=CARTESIAN_POINT('Ctrl Pts',(-6.75417864027363,22.5,6.0450043450931));
#453188=CARTESIAN_POINT('Ctrl Pts',(-6.73321019789003,22.5,6.08599501913005));
#453189=CARTESIAN_POINT('Ctrl Pts',(-6.70966855565445,22.5,6.12568011956913));
#453190=CARTESIAN_POINT('Ctrl Pts',(-6.7034609849824,22.5,6.13614447303852));
#453191=CARTESIAN_POINT('Ctrl Pts',(-6.69707438313333,22.5,6.14651787724421));
#453192=CARTESIAN_POINT('Ctrl Pts',(-6.69051202329594,22.5,6.1567964532414));
#453193=CARTESIAN_POINT('Ctrl Pts',(-6.68556313820106,22.5,6.1645478556042));
#453194=CARTESIAN_POINT('Ctrl Pts',(-6.68051415741144,22.5,6.17224531908615));
#453195=CARTESIAN_POINT('Ctrl Pts',(-6.67537489370653,22.5,6.17987521950616));
#453196=CARTESIAN_POINT('Ctrl Pts',(-6.64842476800822,22.5,6.21988616021516));
#453197=CARTESIAN_POINT('Ctrl Pts',(-6.61894162118579,22.5,6.25812741389502));
#453198=CARTESIAN_POINT('Ctrl Pts',(-6.58718324857477,22.5,6.29441170508163));
#453199=CARTESIAN_POINT('Ctrl Pts',(-6.55551163440422,22.5,6.33059687379256));
#453200=CARTESIAN_POINT('Ctrl Pts',(-6.52157609274862,22.5,6.36483641843439));
#453201=CARTESIAN_POINT('Ctrl Pts',(-6.48560329463389,22.5,6.39690234758754));
#453202=CARTESIAN_POINT('Ctrl Pts',(-6.46634118614209,22.5,6.41407247164262));
#453203=CARTESIAN_POINT('Ctrl Pts',(-6.44649455990001,22.5,6.4306185942519));
#453204=CARTESIAN_POINT('Ctrl Pts',(-6.42609644704949,22.5,6.44649972121378));
#453205=CARTESIAN_POINT('Ctrl Pts',(-6.41550137797154,22.5,6.45474860376629));
#453206=CARTESIAN_POINT('Ctrl Pts',(-6.40475750978787,22.5,6.4628180032753));
#453207=CARTESIAN_POINT('Ctrl Pts',(-6.39386942293182,22.5,6.47070167883221));
#453208=CARTESIAN_POINT('Ctrl Pts',(-6.38552919004326,22.5,6.47674054415646));
#453209=CARTESIAN_POINT('Ctrl Pts',(-6.37710396981869,22.5,6.48267052688883));
#453210=CARTESIAN_POINT('Ctrl Pts',(-6.3686084992472,22.5,6.48848046699456));
#453211=CARTESIAN_POINT('Ctrl Pts',(-6.33038178361366,22.5,6.51462321287319));
#453212=CARTESIAN_POINT('Ctrl Pts',(-6.29067294990532,22.5,6.53838419602365));
#453213=CARTESIAN_POINT('Ctrl Pts',(-6.24968947065537,22.5,6.55954587128772));
#453214=CARTESIAN_POINT('Ctrl Pts',(-6.22204346329034,22.5,6.57382078988697));
#453215=CARTESIAN_POINT('Ctrl Pts',(-6.19381707848861,22.5,6.58691199084907));
#453216=CARTESIAN_POINT('Ctrl Pts',(-6.16507260006602,22.5,6.59873928456135));
#453217=CARTESIAN_POINT('Ctrl Pts',(-6.15266397566519,22.5,6.60384497627704));
#453218=CARTESIAN_POINT('Ctrl Pts',(-6.14015674565985,22.5,6.6087155221976));
#453219=CARTESIAN_POINT('Ctrl Pts',(-6.12757735912736,22.5,6.61333659561112));
#453220=CARTESIAN_POINT('Ctrl Pts',(-6.08619113936898,22.5,6.6285399411254));
#453221=CARTESIAN_POINT('Ctrl Pts',(-6.04397428614735,22.5,6.64106838659551));
#453222=CARTESIAN_POINT('Ctrl Pts',(-6.00111091245467,22.5,6.65070263630215));
#453223=CARTESIAN_POINT('Ctrl Pts',(-5.9799119455316,22.5,6.65546745351706));
#453224=CARTESIAN_POINT('Ctrl Pts',(-5.9585548202981,22.5,6.65952358177373));
#453225=CARTESIAN_POINT('Ctrl Pts',(-5.93706218561481,22.5,6.66283972884874));
#453226=CARTESIAN_POINT('Ctrl Pts',(-5.92425778841234,22.5,6.66481534816931));
#453227=CARTESIAN_POINT('Ctrl Pts',(-5.91140530098883,22.5,6.6665282555788));
#453228=CARTESIAN_POINT('Ctrl Pts',(-5.89851203167795,22.5,6.66798006829994));
#453229=CARTESIAN_POINT('Ctrl Pts',(-4.62591736201901,22.5,5.7755760807344));
#453230=CARTESIAN_POINT('Ctrl Pts',(-4.61585820529768,22.5,5.73330573132647));
#453231=CARTESIAN_POINT('Ctrl Pts',(-4.60871311258362,22.5,5.69054013141041));
#453232=CARTESIAN_POINT('Ctrl Pts',(-4.60431335211636,22.5,5.64753211382414));
#453233=CARTESIAN_POINT('Ctrl Pts',(-4.59971226726699,22.5,5.60255613397471));
#453234=CARTESIAN_POINT('Ctrl Pts',(-4.59811321835512,22.5,5.55731429097459));
#453235=CARTESIAN_POINT('Ctrl Pts',(-4.59937363334914,22.5,5.51206909395162));
#453236=CARTESIAN_POINT('Ctrl Pts',(-4.60034453139405,22.5,5.47721670522309));
#453237=CARTESIAN_POINT('Ctrl Pts',(-4.60301317840841,22.5,5.4423616330738));
#453238=CARTESIAN_POINT('Ctrl Pts',(-4.60733474482685,22.5,5.40761856297945));
#453239=CARTESIAN_POINT('Ctrl Pts',(-4.60876999454272,22.5,5.39607992706529));
#453240=CARTESIAN_POINT('Ctrl Pts',(-4.61038770273571,22.5,5.38455362898469));
#453241=CARTESIAN_POINT('Ctrl Pts',(-4.61218665035847,22.5,5.37304385091102));
#453242=CARTESIAN_POINT('Ctrl Pts',(-4.61342523552785,22.5,5.365119306447));
#453243=CARTESIAN_POINT('Ctrl Pts',(-4.61474939985228,22.5,5.35720517119277));
#453244=CARTESIAN_POINT('Ctrl Pts',(-4.61615691484389,22.5,5.3493113876807));
#453245=CARTESIAN_POINT('Ctrl Pts',(-4.6244083908066,22.5,5.30303453429517));
#453246=CARTESIAN_POINT('Ctrl Pts',(-4.63553334207333,22.5,5.25737359664772));
#453247=CARTESIAN_POINT('Ctrl Pts',(-4.64937620705251,22.5,5.21260376959567));
#453248=CARTESIAN_POINT('Ctrl Pts',(-4.6634940077344,22.5,5.16694476072476));
#453249=CARTESIAN_POINT('Ctrl Pts',(-4.6804387539006,22.5,5.12221145318303));
#453250=CARTESIAN_POINT('Ctrl Pts',(-4.70009847080866,22.5,5.07868894698685));
#453251=CARTESIAN_POINT('Ctrl Pts',(-4.71351361118775,22.5,5.0489906286946));
#453252=CARTESIAN_POINT('Ctrl Pts',(-4.72819401944222,22.5,5.0198559432582));
#453253=CARTESIAN_POINT('Ctrl Pts',(-4.74411779598172,22.5,4.991378078207));
#453254=CARTESIAN_POINT('Ctrl Pts',(-4.7486531689218,22.5,4.98326707902134));
#453255=CARTESIAN_POINT('Ctrl Pts',(-4.75328947247782,22.5,4.9752093870611));
#453256=CARTESIAN_POINT('Ctrl Pts',(-4.75802635988146,22.5,4.96720722556103));
#453257=CARTESIAN_POINT('Ctrl Pts',(-4.76253532466324,22.5,4.95959010036734));
#453258=CARTESIAN_POINT('Ctrl Pts',(-4.76713073211599,22.5,4.95203124834462));
#453259=CARTESIAN_POINT('Ctrl Pts',(-4.77181088052091,22.5,4.94453365138069));
#453260=CARTESIAN_POINT('Ctrl Pts',(-4.79789314476199,22.5,4.90274986841753));
#453261=CARTESIAN_POINT('Ctrl Pts',(-4.82661085236217,22.5,4.86285502852259));
#453262=CARTESIAN_POINT('Ctrl Pts',(-4.85783224460585,22.5,4.82514337751978));
#453263=CARTESIAN_POINT('Ctrl Pts',(-4.87711527004975,22.5,4.80185182408287));
#453264=CARTESIAN_POINT('Ctrl Pts',(-4.89735438406717,22.5,4.77939306995998));
#453265=CARTESIAN_POINT('Ctrl Pts',(-4.9185281570127,22.5,4.75783901282981));
#453266=CARTESIAN_POINT('Ctrl Pts',(-4.95191715474625,22.5,4.72385034361533));
#453267=CARTESIAN_POINT('Ctrl Pts',(-4.98762826934672,22.5,4.69210932076018));
#453268=CARTESIAN_POINT('Ctrl Pts',(-5.02537769858569,22.5,4.66265412509277));
#453269=CARTESIAN_POINT('Ctrl Pts',(-5.03382237968492,22.5,4.65606489343705));
#453270=CARTESIAN_POINT('Ctrl Pts',(-5.04236922205654,22.5,4.64959018433745));
#453271=CARTESIAN_POINT('Ctrl Pts',(-5.05101530324207,22.5,4.64323066279978));
#453272=CARTESIAN_POINT('Ctrl Pts',(-5.05829617806584,22.5,4.6378753024624));
#453273=CARTESIAN_POINT('Ctrl Pts',(-5.06564571347179,22.5,4.63260299859024));
#453274=CARTESIAN_POINT('Ctrl Pts',(-5.07305265319997,22.5,4.62742036981628));
#453275=CARTESIAN_POINT('Ctrl Pts',(-5.11335322922775,22.5,4.59922209460497));
#453276=CARTESIAN_POINT('Ctrl Pts',(-5.15542403882833,22.5,4.5736207619924));
#453277=CARTESIAN_POINT('Ctrl Pts',(-5.19892882007228,22.5,4.550625983677));
#453278=CARTESIAN_POINT('Ctrl Pts',(-5.24352199260122,22.5,4.5270559279874));
#453279=CARTESIAN_POINT('Ctrl Pts',(-5.28962259944175,22.5,4.50622389131235));
#453280=CARTESIAN_POINT('Ctrl Pts',(-5.33691174795269,22.5,4.4881754291715));
#453281=CARTESIAN_POINT('Ctrl Pts',(-5.3651424218722,22.5,4.47740085899016));
#453282=CARTESIAN_POINT('Ctrl Pts',(-5.39379744238978,22.5,4.46761902478714));
#453283=CARTESIAN_POINT('Ctrl Pts',(-5.4228140903405,22.5,4.45884671158638));
#453284=CARTESIAN_POINT('Ctrl Pts',(-5.43879327798787,22.5,4.45401588347092));
#453285=CARTESIAN_POINT('Ctrl Pts',(-5.45488218901142,22.5,4.44949130096477));
#453286=CARTESIAN_POINT('Ctrl Pts',(-5.47107067778001,22.5,4.44527653012968));
#453287=CARTESIAN_POINT('Ctrl Pts',(-5.47990242551106,22.5,4.44297713126103));
#453288=CARTESIAN_POINT('Ctrl Pts',(-5.48876206559289,22.5,4.44077047509027));
#453289=CARTESIAN_POINT('Ctrl Pts',(-5.49763888056664,22.5,4.43865905405411));
#453290=CARTESIAN_POINT('Ctrl Pts',(-5.54884500008372,22.5,4.42647927130003));
#453291=CARTESIAN_POINT('Ctrl Pts',(-5.60070295215265,22.5,4.41744307915717));
#453292=CARTESIAN_POINT('Ctrl Pts',(-5.65287256979064,22.5,4.41160594328751));
#453293=CARTESIAN_POINT('Ctrl Pts',(-5.68841446847963,22.5,4.40762924380021));
#453294=CARTESIAN_POINT('Ctrl Pts',(-5.72410179484693,22.5,4.40513819219555));
#453295=CARTESIAN_POINT('Ctrl Pts',(-5.7598327303865,22.5,4.40416293208135));
#453296=CARTESIAN_POINT('Ctrl Pts',(-5.77636987462536,22.5,4.40371155802871));
#453297=CARTESIAN_POINT('Ctrl Pts',(-5.79292145719268,22.5,4.40358529659437));
#453298=CARTESIAN_POINT('Ctrl Pts',(-5.80944675450856,22.5,4.40378695835983));
#453299=CARTESIAN_POINT('Ctrl Pts',(-5.86257289936903,22.5,4.40443526815779));
#453300=CARTESIAN_POINT('Ctrl Pts',(-5.9154791960951,22.5,4.40846556104586));
#453301=CARTESIAN_POINT('Ctrl Pts',(-5.96783294667778,22.5,4.41595519073349));
#453302=CARTESIAN_POINT('Ctrl Pts',(-5.99560573619532,22.5,4.41992831408309));
#453303=CARTESIAN_POINT('Ctrl Pts',(-6.02322332002874,22.5,4.42487575252983));
#453304=CARTESIAN_POINT('Ctrl Pts',(-6.05063695240159,22.5,4.43081497898236));
#453305=CARTESIAN_POINT('Ctrl Pts',(-6.06627623009907,22.5,4.43420326443596));
#453306=CARTESIAN_POINT('Ctrl Pts',(-6.0818491333573,22.5,4.43791441703144));
#453307=CARTESIAN_POINT('Ctrl Pts',(-6.09735008669016,22.5,4.44194158662795));
#453308=CARTESIAN_POINT('',(3.50148276475995,22.5,3.50148276475995));
#453309=CARTESIAN_POINT('Origin',(0.,22.5,0.));
#453310=CARTESIAN_POINT('Origin',(5.65685387860011,26.,5.65685387860011));
#453311=CARTESIAN_POINT('Origin',(0.,25.,0.));
#453312=CARTESIAN_POINT('',(6.92964645562817,23.5,6.92964645562816));
#453313=CARTESIAN_POINT('Origin',(0.,23.5,0.));
#453314=CARTESIAN_POINT('',(6.92964645562817,25.,6.92964645562816));
#453315=CARTESIAN_POINT('',(6.92964645562816,25.,6.92964645562817));
#453316=CARTESIAN_POINT('Origin',(0.,25.,0.));
#453317=CARTESIAN_POINT('Origin',(0.,14.8,0.));
#453318=CARTESIAN_POINT('',(2.47487373415291,13.3,2.47487373415291));
#453319=CARTESIAN_POINT('',(1.41421356237307,14.8,1.41421356237307));
#453320=CARTESIAN_POINT('Origin',(0.,13.3,0.));
#453321=CARTESIAN_POINT('Origin',(0.,14.8,0.));
#453322=CARTESIAN_POINT('',(2.47487373415292,0.,2.47487373415292));
#453323=CARTESIAN_POINT('',(2.47487373415292,14.8,2.47487373415292));
#453324=CARTESIAN_POINT('Origin',(0.,0.,0.));
#453325=CARTESIAN_POINT('Origin',(0.,0.,0.));
#453326=CARTESIAN_POINT('',(7.42462120245875,25.,7.42462120245875));
#453327=CARTESIAN_POINT('Origin',(0.,25.,0.));
#453328=CARTESIAN_POINT('',(7.42462120245875,0.,7.42462120245875));
#453329=CARTESIAN_POINT('Origin',(0.,0.,0.));
#453330=CARTESIAN_POINT('',(7.42462120245875,23.5,7.42462120245875));
#453331=CARTESIAN_POINT('',(7.42462120245875,0.,7.42462120245875));
#453332=CARTESIAN_POINT('Origin',(0.,23.5,0.));
#453333=CARTESIAN_POINT('Origin',(0.,0.,0.));
#453334=CARTESIAN_POINT('',(3.50148276475995,21.,3.50148276475995));
#453335=CARTESIAN_POINT('Origin',(0.,21.,0.));
#453336=CARTESIAN_POINT('',(3.50148276475995,0.,3.50148276475995));
#453337=CARTESIAN_POINT('Origin',(0.,0.,0.));
#453338=CARTESIAN_POINT('',(7.42462120245875,20.,7.42462120245875));
#453339=CARTESIAN_POINT('Origin',(0.,20.,0.));
#453340=CARTESIAN_POINT('',(7.42462120245875,21.,7.42462120245875));
#453341=CARTESIAN_POINT('',(7.42462120245875,0.,7.42462120245875));
#453342=CARTESIAN_POINT('Origin',(0.,21.,0.));
#453343=CARTESIAN_POINT('Origin',(0.,0.,0.));
#453344=CARTESIAN_POINT('',(3.59412750505487,18.5,3.59412750505487));
#453345=CARTESIAN_POINT('Origin',(0.,18.5,0.));
#453346=CARTESIAN_POINT('',(3.59412750505487,20.,3.59412750505487));
#453347=CARTESIAN_POINT('',(3.59412750505487,0.,3.59412750505487));
#453348=CARTESIAN_POINT('Origin',(0.,20.,0.));
#453349=CARTESIAN_POINT('Origin',(0.,0.,0.));
#453350=CARTESIAN_POINT('',(7.42462120245875,17.5,7.42462120245875));
#453351=CARTESIAN_POINT('Origin',(0.,17.5,0.));
#453352=CARTESIAN_POINT('',(7.42462120245875,18.5,7.42462120245875));
#453353=CARTESIAN_POINT('',(7.42462120245875,0.,7.42462120245875));
#453354=CARTESIAN_POINT('Origin',(0.,18.5,0.));
#453355=CARTESIAN_POINT('Origin',(0.,0.,0.));
#453356=CARTESIAN_POINT('',(3.68677224534978,16.,3.68677224534978));
#453357=CARTESIAN_POINT('Origin',(0.,16.,0.));
#453358=CARTESIAN_POINT('',(3.68677224534978,17.5,3.68677224534978));
#453359=CARTESIAN_POINT('',(3.68677224534978,0.,3.68677224534978));
#453360=CARTESIAN_POINT('Origin',(0.,17.5,0.));
#453361=CARTESIAN_POINT('Origin',(0.,0.,0.));
#453362=CARTESIAN_POINT('',(7.42462120245875,15.,7.42462120245875));
#453363=CARTESIAN_POINT('Origin',(0.,15.,0.));
#453364=CARTESIAN_POINT('',(7.42462120245875,16.,7.42462120245875));
#453365=CARTESIAN_POINT('',(7.42462120245875,0.,7.42462120245875));
#453366=CARTESIAN_POINT('Origin',(0.,16.,0.));
#453367=CARTESIAN_POINT('Origin',(0.,0.,0.));
#453368=CARTESIAN_POINT('',(3.7794169856447,13.5,3.7794169856447));
#453369=CARTESIAN_POINT('Origin',(0.,13.5,0.));
#453370=CARTESIAN_POINT('',(3.7794169856447,15.,3.7794169856447));
#453371=CARTESIAN_POINT('',(3.7794169856447,0.,3.7794169856447));
#453372=CARTESIAN_POINT('Origin',(0.,15.,0.));
#453373=CARTESIAN_POINT('Origin',(0.,0.,0.));
#453374=CARTESIAN_POINT('',(7.42462120245875,12.5,7.42462120245875));
#453375=CARTESIAN_POINT('Origin',(0.,12.5,0.));
#453376=CARTESIAN_POINT('',(7.42462120245875,13.5,7.42462120245875));
#453377=CARTESIAN_POINT('',(7.42462120245875,0.,7.42462120245875));
#453378=CARTESIAN_POINT('Origin',(0.,13.5,0.));
#453379=CARTESIAN_POINT('Origin',(0.,0.,0.));
#453380=CARTESIAN_POINT('',(3.87206172593962,11.,3.87206172593962));
#453381=CARTESIAN_POINT('Origin',(0.,11.,0.));
#453382=CARTESIAN_POINT('',(3.87206172593962,12.5,3.87206172593962));
#453383=CARTESIAN_POINT('',(3.87206172593962,0.,3.87206172593962));
#453384=CARTESIAN_POINT('Origin',(0.,12.5,0.));
#453385=CARTESIAN_POINT('Origin',(0.,0.,0.));
#453386=CARTESIAN_POINT('',(7.42462120245875,10.,7.42462120245875));
#453387=CARTESIAN_POINT('Origin',(0.,10.,0.));
#453388=CARTESIAN_POINT('',(7.42462120245875,11.,7.42462120245875));
#453389=CARTESIAN_POINT('',(7.42462120245875,0.,7.42462120245875));
#453390=CARTESIAN_POINT('Origin',(0.,11.,0.));
#453391=CARTESIAN_POINT('Origin',(0.,0.,0.));
#453392=CARTESIAN_POINT('',(3.96470646623454,8.5,3.96470646623454));
#453393=CARTESIAN_POINT('Origin',(0.,8.5,0.));
#453394=CARTESIAN_POINT('',(3.96470646623454,10.,3.96470646623454));
#453395=CARTESIAN_POINT('',(3.96470646623454,0.,3.96470646623454));
#453396=CARTESIAN_POINT('Origin',(0.,10.,0.));
#453397=CARTESIAN_POINT('Origin',(0.,0.,0.));
#453398=CARTESIAN_POINT('',(7.42462120245875,7.5,7.42462120245875));
#453399=CARTESIAN_POINT('Origin',(0.,7.5,0.));
#453400=CARTESIAN_POINT('',(7.42462120245875,8.5,7.42462120245875));
#453401=CARTESIAN_POINT('',(7.42462120245875,0.,7.42462120245875));
#453402=CARTESIAN_POINT('Origin',(0.,8.5,0.));
#453403=CARTESIAN_POINT('Origin',(0.,0.,0.));
#453404=CARTESIAN_POINT('',(4.05735120652945,6.,4.05735120652945));
#453405=CARTESIAN_POINT('Origin',(0.,6.,0.));
#453406=CARTESIAN_POINT('',(4.05735120652945,7.5,4.05735120652945));
#453407=CARTESIAN_POINT('',(4.05735120652945,0.,4.05735120652945));
#453408=CARTESIAN_POINT('Origin',(0.,7.5,0.));
#453409=CARTESIAN_POINT('Origin',(0.,0.,0.));
#453410=CARTESIAN_POINT('',(7.42462120245875,5.,7.42462120245875));
#453411=CARTESIAN_POINT('Origin',(0.,5.,0.));
#453412=CARTESIAN_POINT('',(7.42462120245875,6.,7.42462120245875));
#453413=CARTESIAN_POINT('',(7.42462120245875,0.,7.42462120245875));
#453414=CARTESIAN_POINT('Origin',(0.,6.,0.));
#453415=CARTESIAN_POINT('Origin',(0.,0.,0.));
#453416=CARTESIAN_POINT('',(4.14999594682437,3.5,4.14999594682437));
#453417=CARTESIAN_POINT('Origin',(0.,3.5,0.));
#453418=CARTESIAN_POINT('',(4.14999594682437,5.,4.14999594682437));
#453419=CARTESIAN_POINT('',(4.14999594682437,0.,4.14999594682437));
#453420=CARTESIAN_POINT('Origin',(0.,5.,0.));
#453421=CARTESIAN_POINT('Origin',(0.,0.,0.));
#453422=CARTESIAN_POINT('',(7.42462120245875,2.5,7.42462120245875));
#453423=CARTESIAN_POINT('Origin',(0.,2.5,0.));
#453424=CARTESIAN_POINT('',(7.42462120245875,3.5,7.42462120245875));
#453425=CARTESIAN_POINT('',(7.42462120245875,0.,7.42462120245875));
#453426=CARTESIAN_POINT('Origin',(0.,3.5,0.));
#453427=CARTESIAN_POINT('Origin',(0.,0.,0.));
#453428=CARTESIAN_POINT('',(4.24264068711929,0.999999999999999,4.24264068711929));
#453429=CARTESIAN_POINT('Origin',(0.,0.999999999999999,0.));
#453430=CARTESIAN_POINT('',(4.24264068711929,2.5,4.24264068711929));
#453431=CARTESIAN_POINT('',(4.24264068711929,0.,4.24264068711929));
#453432=CARTESIAN_POINT('Origin',(0.,2.5,0.));
#453433=CARTESIAN_POINT('Origin',(0.,0.,0.));
#453434=CARTESIAN_POINT('',(7.42462120245875,0.,7.42462120245875));
#453435=CARTESIAN_POINT('Origin',(0.,0.,0.));
#453436=CARTESIAN_POINT('',(7.42462120245875,1.,7.42462120245875));
#453437=CARTESIAN_POINT('',(7.42462120245875,0.,7.42462120245875));
#453438=CARTESIAN_POINT('Origin',(0.,1.,0.));
#453439=CARTESIAN_POINT('Origin',(0.,0.,0.));
#453440=CARTESIAN_POINT('Origin',(7.88424061023,1.,-7.88424061023001));
#453441=CARTESIAN_POINT('Origin',(4.24264068711929,2.5,-4.24264068711929));
#453442=CARTESIAN_POINT('Origin',(7.88424061023,3.5,-7.88424061023001));
#453443=CARTESIAN_POINT('Origin',(4.14999594682437,5.,-4.14999594682437));
#453444=CARTESIAN_POINT('Origin',(7.88424061023,6.,-7.88424061023001));
#453445=CARTESIAN_POINT('Origin',(4.05735120652945,7.5,-4.05735120652945));
#453446=CARTESIAN_POINT('Origin',(7.88424061023,8.5,-7.88424061023001));
#453447=CARTESIAN_POINT('Origin',(3.96470646623454,10.,-3.96470646623454));
#453448=CARTESIAN_POINT('Origin',(7.88424061023,11.,-7.88424061023001));
#453449=CARTESIAN_POINT('Origin',(3.87206172593962,12.5,-3.87206172593962));
#453450=CARTESIAN_POINT('Origin',(7.88424061023,13.5,-7.88424061023001));
#453451=CARTESIAN_POINT('Origin',(3.7794169856447,15.,-3.7794169856447));
#453452=CARTESIAN_POINT('Origin',(7.88424061023,16.,-7.88424061023001));
#453453=CARTESIAN_POINT('Origin',(3.68677224534978,17.5,-3.68677224534978));
#453454=CARTESIAN_POINT('Origin',(7.88424061023,18.5,-7.88424061023001));
#453455=CARTESIAN_POINT('Origin',(3.59412750505487,20.,-3.59412750505487));
#453456=CARTESIAN_POINT('Origin',(7.88424061023,21.,-7.88424061023001));
#453457=CARTESIAN_POINT('Origin',(7.88424061023,23.5,-7.88424061023001));
#453458=CARTESIAN_POINT('Origin',(3.40883802446503,25.,-3.40883802446503));
#453459=CARTESIAN_POINT('Origin',(-5.65685387860011,26.993675081176,5.65685387860011));
#453460=CARTESIAN_POINT('Ctrl Pts',(-4.74432962138981,25.868675081176,6.57057130100612));
#453461=CARTESIAN_POINT('Ctrl Pts',(-4.78199706987976,25.8656848283261,
6.60882993708831));
#453462=CARTESIAN_POINT('Ctrl Pts',(-5.14157728587623,25.8388668852448,
6.92960341635462));
#453463=CARTESIAN_POINT('Ctrl Pts',(-6.16255878293893,25.7882212519322,
7.09568592881682));
#453464=CARTESIAN_POINT('Ctrl Pts',(-7.13997732676548,25.716738181238,6.01152748645437));
#453465=CARTESIAN_POINT('Ctrl Pts',(-6.75873746207651,25.6452551105438,
4.60259286076204));
#453466=CARTESIAN_POINT('Ctrl Pts',(-5.36788602689621,25.5737720398497,
4.15947051927595));
#453467=CARTESIAN_POINT('Ctrl Pts',(-4.24182426511434,25.5022889691555,
5.0882746237623));
#453468=CARTESIAN_POINT('Ctrl Pts',(-4.36502559631504,25.450589982931,6.13675122222029));
#453469=CARTESIAN_POINT('Ctrl Pts',(-4.69148744470697,25.4227186869378,
6.51790892062316));
#453470=CARTESIAN_POINT('Ctrl Pts',(-4.74334636410459,25.418675081176,6.56885365284802));
#453471=CARTESIAN_POINT('Ctrl Pts',(-4.7445060113485,25.906324918824,6.56704169373441));
#453472=CARTESIAN_POINT('Ctrl Pts',(-4.9557394479142,25.8898945654199,6.77506586643251));
#453473=CARTESIAN_POINT('Ctrl Pts',(-5.64807137163849,25.8496365217844,
7.11639071403833));
#453474=CARTESIAN_POINT('Ctrl Pts',(-6.8522203629011,25.7855507879174,6.60321033464885));
#453475=CARTESIAN_POINT('Ctrl Pts',(-7.1004834147237,25.7140677172233,5.16550356767203));
#453476=CARTESIAN_POINT('Ctrl Pts',(-6.02596364157129,25.6425846465291,
4.17707919799326));
#453477=CARTESIAN_POINT('Ctrl Pts',(-4.61334644908231,25.5711015758349,
4.5448553014618));
#453478=CARTESIAN_POINT('Ctrl Pts',(-4.21675923787011,25.5090149999332,
5.74896333949311));
#453479=CARTESIAN_POINT('Ctrl Pts',(-4.5629353888518,25.4707561142629,6.3830054663296));
#453480=CARTESIAN_POINT('Ctrl Pts',(-4.74640124271564,25.456324918824,6.56829321884323));
#453481=CARTESIAN_POINT('Ctrl Pts',(-6.69274404704181,26.,5.59475217632212));
#453482=CARTESIAN_POINT('Ctrl Pts',(-6.67208297724159,25.9761723097686,
5.25011429538726));
#453483=CARTESIAN_POINT('Ctrl Pts',(-6.25991935236784,25.9285169293058,
4.58904744425369));
#453484=CARTESIAN_POINT('Ctrl Pts',(-5.08408179813166,25.8570338586116,
4.57111450891619));
#453485=CARTESIAN_POINT('Ctrl Pts',(-4.43501771280631,25.7855507879175,
5.55001366141289));
#453486=CARTESIAN_POINT('Ctrl Pts',(-4.90440858615388,25.7140677172233,
6.62575617389683));
#453487=CARTESIAN_POINT('Ctrl Pts',(-6.06367191307887,25.6425846465291,
6.81433291744693));
#453488=CARTESIAN_POINT('Ctrl Pts',(-6.8499634587037,25.5711015758349,5.94217367437589));
#453489=CARTESIAN_POINT('Ctrl Pts',(-6.54327224197424,25.4996185051408,
4.80874583886255));
#453490=CARTESIAN_POINT('Ctrl Pts',(-5.42439156223909,25.4281354344466,
4.45227280794999));
#453491=CARTESIAN_POINT('Ctrl Pts',(-4.51852288527076,25.3566523637524,
5.19945610983427));
#453492=CARTESIAN_POINT('Ctrl Pts',(-4.65556044151952,25.2851692930583,
6.36568271985868));
#453493=CARTESIAN_POINT('Ctrl Pts',(-5.70997789504277,25.213686222364,6.88249940298929));
#453494=CARTESIAN_POINT('Ctrl Pts',(-6.71571945020394,25.1422031516699,
6.27639179734011));
#453495=CARTESIAN_POINT('Ctrl Pts',(-6.7513451989237,25.0707200809757,5.10267450019953));
#453496=CARTESIAN_POINT('Ctrl Pts',(-5.78421192833874,24.9992370102815,
4.43668748453226));
#453497=CARTESIAN_POINT('Ctrl Pts',(-4.7003955508837,24.9277539395873,4.88860074260097));
#453498=CARTESIAN_POINT('Ctrl Pts',(-4.49287282235237,24.8562708688931,
6.04437662247732));
#453499=CARTESIAN_POINT('Ctrl Pts',(-5.35177365831406,24.784787798199,6.84510966506768));
#453500=CARTESIAN_POINT('Ctrl Pts',(-6.49018471285717,24.7133047275048,
6.55717903824976));
#453501=CARTESIAN_POINT('Ctrl Pts',(-6.86510957377001,24.6418216568106,
5.44438294256281));
#453502=CARTESIAN_POINT('Ctrl Pts',(-6.13304718756447,24.5703385861164,
4.52624977050191));
#453503=CARTESIAN_POINT('Ctrl Pts',(-4.96470306042394,24.4988555154223,
4.64396052187117));
#453504=CARTESIAN_POINT('Ctrl Pts',(-4.43049797487471,24.4273724447281,
5.68967021074952));
#453505=CARTESIAN_POINT('Ctrl Pts',(-5.01986328076134,24.3558893740339,
6.70531403099034));
#453506=CARTESIAN_POINT('Ctrl Pts',(-6.19283059794665,24.2844063033397,
6.76037309820141));
#453507=CARTESIAN_POINT('Ctrl Pts',(-6.87474342740735,24.2129232326455,
5.80440305573226));
#453508=CARTESIAN_POINT('Ctrl Pts',(-6.44084262551864,24.1414401619514,
4.71325048867858));
#453509=CARTESIAN_POINT('Ctrl Pts',(-5.28866213152759,24.0699570912572,
4.48661435222159));
#453510=CARTESIAN_POINT('Ctrl Pts',(-4.47381384511066,23.9984740205631,
5.33213555135881));
#453511=CARTESIAN_POINT('Ctrl Pts',(-4.74285054378755,23.9269909498688,
6.47515921171813));
#453512=CARTESIAN_POINT('Ctrl Pts',(-5.84928450947304,23.8555078791747,
6.86846279219781));
#453513=CARTESIAN_POINT('Ctrl Pts',(-6.77941618151556,23.7840248084805,
6.15170698086798));
#453514=CARTESIAN_POINT('Ctrl Pts',(-6.68107173221035,23.7125417377863,
4.98157355760958));
#453515=CARTESIAN_POINT('Ctrl Pts',(-5.64435299191054,23.6410586670921,
4.43012269359922));
#453516=CARTESIAN_POINT('Ctrl Pts',(-4.61908739135743,23.569575596398,5.00258598787076));
#453517=CARTESIAN_POINT('Ctrl Pts',(-4.54460915448657,23.4980925257038,
6.17448062637044));
#453518=CARTESIAN_POINT('Ctrl Pts',(-5.48915421344717,23.4266094550096,
6.87213254456038));
#453519=CARTESIAN_POINT('Ctrl Pts',(-6.5873433994568,23.3551263843154,6.45636332421143));
#453520=CARTESIAN_POINT('Ctrl Pts',(-6.8330308949199,23.2836433136213,5.30809370313679));
#453521=CARTESIAN_POINT('Ctrl Pts',(-6.00112122066856,23.212160242927,4.47935503415496));
#453522=CARTESIAN_POINT('Ctrl Pts',(-4.85379852261456,23.1406771722329,
4.72942128924326));
#453523=CARTESIAN_POINT('Ctrl Pts',(-4.44222413342345,23.0691941015387,
5.82919498069919));
#453524=CARTESIAN_POINT('Ctrl Pts',(-5.14347668616413,22.9977110308445,
6.77105943752211));
#453525=CARTESIAN_POINT('Ctrl Pts',(-6.31507855179966,22.9262279601504,
6.69212899367236));
#453526=CARTESIAN_POINT('Ctrl Pts',(-6.88362364563197,22.8547448894562,
5.66464494341573));
#453527=CARTESIAN_POINT('Ctrl Pts',(-6.32821994284799,22.783261818762,4.63011853598606));
#453528=CARTESIAN_POINT('Ctrl Pts',(-5.15771839492687,22.7117787480678,
4.53608521045973));
#453529=CARTESIAN_POINT('Ctrl Pts',(-4.4445208236608,22.6402956773736,5.46925286619012));
#453530=CARTESIAN_POINT('Ctrl Pts',(-4.84204067651847,22.5688126066795,
6.57357515235991));
#453531=CARTESIAN_POINT('Ctrl Pts',(-5.98608844956735,22.4973295359852,
6.8394368280484));
#453532=CARTESIAN_POINT('Ctrl Pts',(-6.82851835303725,22.4258464652911,
6.01893246982621));
#453533=CARTESIAN_POINT('Ctrl Pts',(-6.67416374956871,22.3781910848283,
5.25534692011694));
#453534=CARTESIAN_POINT('Ctrl Pts',(-6.45251384441992,22.3543633945969,
4.99063298333217));
#453535=CARTESIAN_POINT('Ctrl Pts',(-6.77667668816907,26.0485455351344,
5.58972040746333));
#453536=CARTESIAN_POINT('Ctrl Pts',(-6.75434156236399,26.024717844903,5.21715836192049));
#453537=CARTESIAN_POINT('Ctrl Pts',(-6.30878252293169,25.9770624644402,
4.50252879876621));
#453538=CARTESIAN_POINT('Ctrl Pts',(-5.03767313923882,25.905579393746,4.4831428535712));
#453539=CARTESIAN_POINT('Ctrl Pts',(-4.33601886182374,25.8340963230518,
5.54135696992154));
#453540=CARTESIAN_POINT('Ctrl Pts',(-4.84344196766209,25.7626132523576,
6.70426114586778));
#453541=CARTESIAN_POINT('Ctrl Pts',(-6.09663420303223,25.6911301816635,
6.90811725457023));
#453542=CARTESIAN_POINT('Ctrl Pts',(-6.94663474805762,25.6196471109693,
5.96529161173539));
#453543=CARTESIAN_POINT('Ctrl Pts',(-6.61509398200833,25.5481640402751,
4.7400281794957));
#453544=CARTESIAN_POINT('Ctrl Pts',(-5.40555638379146,25.4766809695809,
4.35467204505866));
#453545=CARTESIAN_POINT('Ctrl Pts',(-4.42629001188529,25.4051978988867,
5.16239561447694));
#453546=CARTESIAN_POINT('Ctrl Pts',(-4.57443098853515,25.3337148281926,
6.42311533054124));
#453547=CARTESIAN_POINT('Ctrl Pts',(-5.71428225002475,25.2622317574984,
6.98180690592903));
#453548=CARTESIAN_POINT('Ctrl Pts',(-6.80151366539291,25.1907486868042,
6.32658964203686));
#453549=CARTESIAN_POINT('Ctrl Pts',(-6.84002597802966,25.11926561611,5.05777230853438));
#453550=CARTESIAN_POINT('Ctrl Pts',(-5.79453107008661,25.0477825454159,
4.33782392622387));
#453551=CARTESIAN_POINT('Ctrl Pts',(-4.62289884706407,24.9762994747217,
4.82635329907546));
#453552=CARTESIAN_POINT('Ctrl Pts',(-4.39856166152736,24.9048164040275,
6.07577551821105));
#453553=CARTESIAN_POINT('Ctrl Pts',(-5.32705463942152,24.8333333333333,
6.94138767747801));
#453554=CARTESIAN_POINT('Ctrl Pts',(-6.55770505428216,24.7618502626391,
6.63012757162215));
#453555=CARTESIAN_POINT('Ctrl Pts',(-6.96300807183686,24.690367191945,5.42716755876279));
#453556=CARTESIAN_POINT('Ctrl Pts',(-6.17163058503857,24.6188841212508,
4.4346429653087));
#453557=CARTESIAN_POINT('Ctrl Pts',(-4.90862178076926,24.5474010505566,
4.56189118942602));
#453558=CARTESIAN_POINT('Ctrl Pts',(-4.33113291369596,24.4759179798625,
5.69232914266462));
#453559=CARTESIAN_POINT('Ctrl Pts',(-4.96825133880203,24.4044349091683,
6.79026515070139));
#453560=CARTESIAN_POINT('Ctrl Pts',(-6.23625792548383,24.3329518384741,
6.84978535971091));
#453561=CARTESIAN_POINT('Ctrl Pts',(-6.97342250511928,24.2614687677799,
5.81635817656469));
#453562=CARTESIAN_POINT('Ctrl Pts',(-6.50436504145382,24.1899856970857,
4.63679535172919));
#453563=CARTESIAN_POINT('Ctrl Pts',(-5.2588295230962,24.1185026263916,4.39179610102783));
#453564=CARTESIAN_POINT('Ctrl Pts',(-4.37795843727393,24.0470195556974,
5.30582536167067));
#453565=CARTESIAN_POINT('Ctrl Pts',(-4.66879374102307,23.9755364850032,
6.54146211713177));
#453566=CARTESIAN_POINT('Ctrl Pts',(-5.86487613450725,23.904053414309,6.96663298362319));
#453567=CARTESIAN_POINT('Ctrl Pts',(-6.8703714022368,23.8325703436148,6.19180228161384));
#453568=CARTESIAN_POINT('Ctrl Pts',(-6.76405862808226,23.7610872729207,
4.92685920413015));
#453569=CARTESIAN_POINT('Ctrl Pts',(-5.64334011190815,23.6896042022265,
4.33072722538547));
#453570=CARTESIAN_POINT('Ctrl Pts',(-4.53500272215098,23.6181211315323,
4.94957415925549));
#453571=CARTESIAN_POINT('Ctrl Pts',(-4.45448991200439,23.5466380608381,
6.21642115383373));
#453572=CARTESIAN_POINT('Ctrl Pts',(-5.47556640632123,23.475154990144,6.97060007639641));
#453573=CARTESIAN_POINT('Ctrl Pts',(-6.66273598971974,23.4036719194498,
6.52114329936776));
#453574=CARTESIAN_POINT('Ctrl Pts',(-6.92833022917403,23.3321888487556,
5.27983553104633));
#453575=CARTESIAN_POINT('Ctrl Pts',(-6.02901536249358,23.2607057780614,
4.38394859923605));
#453576=CARTESIAN_POINT('Ctrl Pts',(-4.78873124130167,23.1892227073672,
4.6542763857934));
#453577=CARTESIAN_POINT('Ctrl Pts',(-4.34380918016856,23.1177396366731,
5.84315885864169));
#453578=CARTESIAN_POINT('Ctrl Pts',(-5.1018804774459,23.0462565659789,6.86133755596364));
#453579=CARTESIAN_POINT('Ctrl Pts',(-6.36841097734037,22.9747734952847,
6.77601180031397));
#453580=CARTESIAN_POINT('Ctrl Pts',(-6.98302223994139,22.9032904245905,
5.66527621173653));
#453581=CARTESIAN_POINT('Ctrl Pts',(-6.3826171450343,22.8318073538963,4.54692766144197));
#453582=CARTESIAN_POINT('Ctrl Pts',(-5.11727611571493,22.7603242832022,
4.4452753183732));
#453583=CARTESIAN_POINT('Ctrl Pts',(-4.34629195893472,22.688841212508,5.45405255931453));
#453584=CARTESIAN_POINT('Ctrl Pts',(-4.77602071980922,22.6173581418138,
6.64785217518362));
#453585=CARTESIAN_POINT('Ctrl Pts',(-6.01276456633487,22.5458750711197,
6.93525520080945));
#453586=CARTESIAN_POINT('Ctrl Pts',(-6.92345206015257,22.4743920004254,
6.04826976192828));
#453587=CARTESIAN_POINT('Ctrl Pts',(-6.75659092854625,22.4267366199627,
5.22281495825156));
#453588=CARTESIAN_POINT('Ctrl Pts',(-6.5169819168131,22.4029089297313,4.93665266667552));
#453589=CARTESIAN_POINT('Ctrl Pts',(-6.86060932929632,26.0970910702687,
5.58468863860454));
#453590=CARTESIAN_POINT('Ctrl Pts',(-6.83660014748639,26.0732633800373,
5.18420242845371));
#453591=CARTESIAN_POINT('Ctrl Pts',(-6.35764569349554,26.0256079995746,
4.41601015327873));
#453592=CARTESIAN_POINT('Ctrl Pts',(-4.99126448034597,25.9541249288803,
4.39517119822623));
#453593=CARTESIAN_POINT('Ctrl Pts',(-4.23702001084117,25.8826418581862,
5.53270027843017));
#453594=CARTESIAN_POINT('Ctrl Pts',(-4.7824753491703,25.811158787492,6.78276611783875));
#453595=CARTESIAN_POINT('Ctrl Pts',(-6.12959649298558,25.7396757167979,
7.00190159169352));
#453596=CARTESIAN_POINT('Ctrl Pts',(-7.04330603741155,25.6681926461036,
5.98840954909488));
#453597=CARTESIAN_POINT('Ctrl Pts',(-6.68691572204241,25.5967095754095,
4.67131052012887));
#453598=CARTESIAN_POINT('Ctrl Pts',(-5.38672120534384,25.5252265047153,
4.2570712821673));
#453599=CARTESIAN_POINT('Ctrl Pts',(-4.33405713849982,25.4537434340211,
5.12533511911963));
#453600=CARTESIAN_POINT('Ctrl Pts',(-4.49330153555078,25.382260363327,6.48054794122378));
#453601=CARTESIAN_POINT('Ctrl Pts',(-5.71858660500674,25.3107772926328,
7.0811144088688));
#453602=CARTESIAN_POINT('Ctrl Pts',(-6.88730788058188,25.2392942219386,
6.37678748673361));
#453603=CARTESIAN_POINT('Ctrl Pts',(-6.92870675713562,25.1678111512444,
5.01287011686923));
#453604=CARTESIAN_POINT('Ctrl Pts',(-5.80485021183448,25.0963280805502,
4.23896036791547));
#453605=CARTESIAN_POINT('Ctrl Pts',(-4.54540214324445,25.0248450098561,
4.76410585554996));
#453606=CARTESIAN_POINT('Ctrl Pts',(-4.30425050070234,24.9533619391619,
6.10717441394477));
#453607=CARTESIAN_POINT('Ctrl Pts',(-5.302335620529,24.8818788684677,7.03766568988833));
#453608=CARTESIAN_POINT('Ctrl Pts',(-6.62522539570715,24.8103957977735,
6.70307610499455));
#453609=CARTESIAN_POINT('Ctrl Pts',(-7.06090656990369,24.7389127270793,
5.40995217496278));
#453610=CARTESIAN_POINT('Ctrl Pts',(-6.21021398251268,24.6674296563851,
4.34303616011548));
#453611=CARTESIAN_POINT('Ctrl Pts',(-4.85254050111457,24.595946585691,4.47982185698087));
#453612=CARTESIAN_POINT('Ctrl Pts',(-4.23176785251722,24.5244635149968,
5.69498807457971));
#453613=CARTESIAN_POINT('Ctrl Pts',(-4.91663939684271,24.4529804443027,
6.87521627041245));
#453614=CARTESIAN_POINT('Ctrl Pts',(-6.27968525302103,24.3814973736084,
6.93919762122039));
#453615=CARTESIAN_POINT('Ctrl Pts',(-7.07210158283119,24.3100143029143,
5.82831329739714));
#453616=CARTESIAN_POINT('Ctrl Pts',(-6.567887457389,24.2385312322201,4.56034021477979));
#453617=CARTESIAN_POINT('Ctrl Pts',(-5.2289969146648,24.1670481615259,4.29697784983407));
#453618=CARTESIAN_POINT('Ctrl Pts',(-4.28210302943719,24.0955650908318,
5.27951517198252));
#453619=CARTESIAN_POINT('Ctrl Pts',(-4.59473693825861,24.0240820201375,
6.60776502254541));
#453620=CARTESIAN_POINT('Ctrl Pts',(-5.88046775954144,23.9525989494434,
7.06480317504856));
#453621=CARTESIAN_POINT('Ctrl Pts',(-6.96132662295805,23.8811158787492,
6.2318975823597));
#453622=CARTESIAN_POINT('Ctrl Pts',(-6.84704552395415,23.809632808055,4.87214485065071));
#453623=CARTESIAN_POINT('Ctrl Pts',(-5.64232723190575,23.7381497373609,
4.23133175717171));
#453624=CARTESIAN_POINT('Ctrl Pts',(-4.45091805294455,23.6666666666667,
4.89656233064023));
#453625=CARTESIAN_POINT('Ctrl Pts',(-4.3643706695222,23.5951835959725,6.258361681297));
#453626=CARTESIAN_POINT('Ctrl Pts',(-5.46197859919531,23.5237005252783,
7.06906760823243));
#453627=CARTESIAN_POINT('Ctrl Pts',(-6.73812857998267,23.4522174545842,
6.58592327452408));
#453628=CARTESIAN_POINT('Ctrl Pts',(-7.02362956342815,23.3807343838899,
5.25157735895588));
#453629=CARTESIAN_POINT('Ctrl Pts',(-6.05690950431861,23.3092513131958,
4.28854216431713));
#453630=CARTESIAN_POINT('Ctrl Pts',(-4.72366395998878,23.2377682425016,
4.57913148234355));
#453631=CARTESIAN_POINT('Ctrl Pts',(-4.24539422691366,23.1662851718074,
5.85712273658419));
#453632=CARTESIAN_POINT('Ctrl Pts',(-5.06028426872769,23.0948021011132,
6.95161567440517));
#453633=CARTESIAN_POINT('Ctrl Pts',(-6.42174340288107,23.0233190304191,
6.85989460695557));
#453634=CARTESIAN_POINT('Ctrl Pts',(-7.0824208342508,22.9518359597249,5.66590748005734));
#453635=CARTESIAN_POINT('Ctrl Pts',(-6.43701434722061,22.8803528890307,
4.46373678689787));
#453636=CARTESIAN_POINT('Ctrl Pts',(-5.07683383650298,22.8088698183366,
4.35446542628666));
#453637=CARTESIAN_POINT('Ctrl Pts',(-4.24806309420865,22.7373867476423,
5.43885225243895));
#453638=CARTESIAN_POINT('Ctrl Pts',(-4.71000076309996,22.6659036769482,
6.72212919800732));
#453639=CARTESIAN_POINT('Ctrl Pts',(-6.0394406831024,22.594420606254,7.03107357357049));
#453640=CARTESIAN_POINT('Ctrl Pts',(-7.01838576726789,22.5229375355598,
6.07760705403035));
#453641=CARTESIAN_POINT('Ctrl Pts',(-6.83901810752379,22.475282155097,5.19028299638618));
#453642=CARTESIAN_POINT('Ctrl Pts',(-6.58144998920627,22.4514544648656,
4.88267235001886));
#453643=CARTESIAN_POINT('Ctrl Pts',(-6.94454197042357,26.1456366054031,
5.57965686974575));
#453644=CARTESIAN_POINT('Ctrl Pts',(-6.91885873260879,26.1218089151717,
5.15124649498693));
#453645=CARTESIAN_POINT('Ctrl Pts',(-6.40650886405939,26.0741535347089,
4.32949150779126));
#453646=CARTESIAN_POINT('Ctrl Pts',(-4.94485582145312,26.0026704640147,
4.30719954288124));
#453647=CARTESIAN_POINT('Ctrl Pts',(-4.1380211598586,25.9311873933206,5.52404358693882));
#453648=CARTESIAN_POINT('Ctrl Pts',(-4.7215087306785,25.8597043226263,6.86127108980971));
#453649=CARTESIAN_POINT('Ctrl Pts',(-6.16255878293893,25.7882212519322,
7.09568592881682));
#453650=CARTESIAN_POINT('Ctrl Pts',(-7.13997732676548,25.716738181238,6.01152748645437));
#453651=CARTESIAN_POINT('Ctrl Pts',(-6.75873746207651,25.6452551105438,
4.60259286076204));
#453652=CARTESIAN_POINT('Ctrl Pts',(-5.36788602689621,25.5737720398497,
4.15947051927595));
#453653=CARTESIAN_POINT('Ctrl Pts',(-4.24182426511434,25.5022889691555,
5.0882746237623));
#453654=CARTESIAN_POINT('Ctrl Pts',(-4.41217208256641,25.4308058984613,
6.53798055190634));
#453655=CARTESIAN_POINT('Ctrl Pts',(-5.72289095998872,25.3593228277671,
7.18042191180854));
#453656=CARTESIAN_POINT('Ctrl Pts',(-6.97310209577086,25.287839757073,6.42698533143036));
#453657=CARTESIAN_POINT('Ctrl Pts',(-7.01738753624157,25.2163566863788,
4.96796792520407));
#453658=CARTESIAN_POINT('Ctrl Pts',(-5.81516935358237,25.1448736156846,
4.14009680960707));
#453659=CARTESIAN_POINT('Ctrl Pts',(-4.4679054394248,25.0733905449904,4.70185841202445));
#453660=CARTESIAN_POINT('Ctrl Pts',(-4.20993933987732,25.0019074742962,
6.13857330967851));
#453661=CARTESIAN_POINT('Ctrl Pts',(-5.27761660163647,24.930424403602,7.13394370229865));
#453662=CARTESIAN_POINT('Ctrl Pts',(-6.69274573713214,24.8589413329079,
6.77602463836695));
#453663=CARTESIAN_POINT('Ctrl Pts',(-7.15880506797054,24.7874582622137,
5.39273679116275));
#453664=CARTESIAN_POINT('Ctrl Pts',(-6.24879737998678,24.7159751915195,
4.25142935492228));
#453665=CARTESIAN_POINT('Ctrl Pts',(-4.79645922145989,24.6444921208253,
4.39775252453571));
#453666=CARTESIAN_POINT('Ctrl Pts',(-4.13240279133847,24.5730090501312,
5.69764700649482));
#453667=CARTESIAN_POINT('Ctrl Pts',(-4.86502745488341,24.501525979437,6.9601673901235));
#453668=CARTESIAN_POINT('Ctrl Pts',(-6.32311258055822,24.4300429087428,
7.0286098827299));
#453669=CARTESIAN_POINT('Ctrl Pts',(-7.17078066054311,24.3585598380486,
5.84026841822956));
#453670=CARTESIAN_POINT('Ctrl Pts',(-6.63140987332417,24.2870767673545,
4.4838850778304));
#453671=CARTESIAN_POINT('Ctrl Pts',(-5.19916430623342,24.2155936966603,
4.2021595986403));
#453672=CARTESIAN_POINT('Ctrl Pts',(-4.18624762160046,24.1441106259661,
5.25320498229437));
#453673=CARTESIAN_POINT('Ctrl Pts',(-4.52068013549415,24.0726275552719,
6.67406792795905));
#453674=CARTESIAN_POINT('Ctrl Pts',(-5.89605938457563,24.0011444845777,
7.16297336647392));
#453675=CARTESIAN_POINT('Ctrl Pts',(-7.0522818436793,23.9296614138836,6.27199288310558));
#453676=CARTESIAN_POINT('Ctrl Pts',(-6.93003241982605,23.8581783431894,
4.81743049717126));
#453677=CARTESIAN_POINT('Ctrl Pts',(-5.64131435190337,23.7866952724952,
4.13193628895796));
#453678=CARTESIAN_POINT('Ctrl Pts',(-4.3668333837381,23.715212201801,4.84355050202496));
#453679=CARTESIAN_POINT('Ctrl Pts',(-4.27425142704003,23.6437291311069,
6.30030220876029));
#453680=CARTESIAN_POINT('Ctrl Pts',(-5.44839079206937,23.5722460604127,
7.16753514006844));
#453681=CARTESIAN_POINT('Ctrl Pts',(-6.81352117024561,23.5007629897185,
6.65070324968042));
#453682=CARTESIAN_POINT('Ctrl Pts',(-7.11892889768229,23.4292799190243,
5.22331918686542));
#453683=CARTESIAN_POINT('Ctrl Pts',(-6.08480364614363,23.3577968483302,
4.19313572939823));
#453684=CARTESIAN_POINT('Ctrl Pts',(-4.65859667867589,23.2863137776359,
4.50398657889369));
#453685=CARTESIAN_POINT('Ctrl Pts',(-4.14697927365876,23.2148307069418,
5.8710866145267));
#453686=CARTESIAN_POINT('Ctrl Pts',(-5.01868806000948,23.1433476362476,
7.04189379284668));
#453687=CARTESIAN_POINT('Ctrl Pts',(-6.47507582842176,23.0718645655535,
6.94377741359718));
#453688=CARTESIAN_POINT('Ctrl Pts',(-7.18181942856023,23.0003814948592,
5.66653874837814));
#453689=CARTESIAN_POINT('Ctrl Pts',(-6.49141154940691,22.9288984241651,
4.38054591235378));
#453690=CARTESIAN_POINT('Ctrl Pts',(-5.03639155729104,22.8574153534709,
4.26365553420012));
#453691=CARTESIAN_POINT('Ctrl Pts',(-4.14983422948258,22.7859322827767,
5.42365194556336));
#453692=CARTESIAN_POINT('Ctrl Pts',(-4.6439808063907,22.7144492120825,6.79640622083105));
#453693=CARTESIAN_POINT('Ctrl Pts',(-6.06611679986992,22.6429661413884,
7.12689194633153));
#453694=CARTESIAN_POINT('Ctrl Pts',(-7.11331947438321,22.5714830706942,
6.10694434613243));
#453695=CARTESIAN_POINT('Ctrl Pts',(-6.92144528650133,22.5238276902314,
5.15775103452081));
#453696=CARTESIAN_POINT('Ctrl Pts',(-6.64591806159944,22.5,4.8286920333622));
#453697=CARTESIAN_POINT('Ctrl Pts',(-4.92197603118329,25.2730384757729,
6.39051881327128));
#453698=CARTESIAN_POINT('Ctrl Pts',(-4.8802577415671,25.2770820815347,6.34953594825859));
#453699=CARTESIAN_POINT('Ctrl Pts',(-4.84215579969383,25.2811256872965,
6.3050503566324));
#453700=CARTESIAN_POINT('Ctrl Pts',(-4.80845709106527,25.2851692930582,
6.25744773204304));
#453701=CARTESIAN_POINT('Ctrl Pts',(-4.60988125610327,25.3089969832896,
5.97694051651721));
#453702=CARTESIAN_POINT('Ctrl Pts',(-4.56420207068701,25.332824673521,5.58819831317574));
#453703=CARTESIAN_POINT('Ctrl Pts',(-4.69234059080694,25.3566523637524,
5.26929666119096));
#453704=CARTESIAN_POINT('Ctrl Pts',(-4.82047911092687,25.3804800539838,
4.95039500920618));
#453705=CARTESIAN_POINT('Ctrl Pts',(-5.12243533658298,25.4043077442152,
4.70133390857808));
#453706=CARTESIAN_POINT('Ctrl Pts',(-5.45989356270023,25.4281354344466,
4.6362155300828));
#453707=CARTESIAN_POINT('Ctrl Pts',(-5.79735178881747,25.451963124678,4.57109715158751));
#453708=CARTESIAN_POINT('Ctrl Pts',(-6.17031201539585,25.4757908149094,
4.68992149522503));
#453709=CARTESIAN_POINT('Ctrl Pts',(-6.40790733147329,25.4996185051408,
4.93823830629601));
#453710=CARTESIAN_POINT('Ctrl Pts',(-6.64550264755072,25.5234461953722,
5.186555117367));
#453711=CARTESIAN_POINT('Ctrl Pts',(-6.74773305312721,25.5472738856035,
5.56436439587144));
#453712=CARTESIAN_POINT('Ctrl Pts',(-6.66779966497798,25.5711015758349,
5.89862890896884));
#453713=CARTESIAN_POINT('Ctrl Pts',(-6.58786627682875,25.5949292660663,
6.23289342206624));
#453714=CARTESIAN_POINT('Ctrl Pts',(-6.32576909495381,25.6187569562977,
6.52361316975658));
#453715=CARTESIAN_POINT('Ctrl Pts',(-6.00150994952884,25.6425846465291,
6.63754358634341));
#453716=CARTESIAN_POINT('Ctrl Pts',(-5.67725080410387,25.6664123367605,
6.75147400293023));
#453717=CARTESIAN_POINT('Ctrl Pts',(-5.29082969512888,25.6902400269919,
6.68861508841353));
#453718=CARTESIAN_POINT('Ctrl Pts',(-5.01938732841678,25.7140677172233,
6.47789521240786));
#453719=CARTESIAN_POINT('Ctrl Pts',(-4.98532270432787,25.7170579700732,
6.45145094929911));
#453720=CARTESIAN_POINT('Ctrl Pts',(-4.95306887608107,25.720048222923,6.42267802952733));
#453721=CARTESIAN_POINT('Ctrl Pts',(-4.92276701974739,25.7230384757729,
6.39190058798136));
#453722=CARTESIAN_POINT('Ctrl Pts',(-4.53900700771688,26.,5.01302286563431));
#453723=CARTESIAN_POINT('Ctrl Pts',(-4.32480615636363,25.9761723097686,
5.38492752167559));
#453724=CARTESIAN_POINT('Ctrl Pts',(-4.30067277954968,25.9285169293058,
6.35301914505848));
#453725=CARTESIAN_POINT('Ctrl Pts',(-5.50907794609548,25.8570338586117,
7.17562648915451));
#453726=CARTESIAN_POINT('Ctrl Pts',(-6.8522203629011,25.7855507879174,6.60321033464885));
#453727=CARTESIAN_POINT('Ctrl Pts',(-7.1004834147237,25.7140677172233,5.16550356767203));
#453728=CARTESIAN_POINT('Ctrl Pts',(-6.02596364157129,25.6425846465291,
4.17707919799326));
#453729=CARTESIAN_POINT('Ctrl Pts',(-4.61334644908231,25.5711015758349,
4.5448553014618));
#453730=CARTESIAN_POINT('Ctrl Pts',(-4.15673773385264,25.4996185051408,
5.93119910857215));
#453731=CARTESIAN_POINT('Ctrl Pts',(-5.07453447980768,25.4281354344466,
7.06630891143689));
#453732=CARTESIAN_POINT('Ctrl Pts',(-6.5258341885166,25.3566523637524,6.91003560334641));
#453733=CARTESIAN_POINT('Ctrl Pts',(-7.18099123031483,25.2851692930582,
5.60564496305));
#453734=CARTESIAN_POINT('Ctrl Pts',(-6.43975200870338,25.213686222364,4.34815567114859));
#453735=CARTESIAN_POINT('Ctrl Pts',(-4.98123363545819,25.1422031516699,
4.28968558428151));
#453736=CARTESIAN_POINT('Ctrl Pts',(-4.14170854437417,25.0707200809757,
5.48379221455872));
#453737=CARTESIAN_POINT('Ctrl Pts',(-4.69033908735646,24.9992370102815,
6.83645762028281));
#453738=CARTESIAN_POINT('Ctrl Pts',(-6.12447699388038,24.9277539395873,
7.10838527255516));
#453739=CARTESIAN_POINT('Ctrl Pts',(-7.13018513270865,24.8562708688931,
6.05044038944422));
#453740=CARTESIAN_POINT('Ctrl Pts',(-6.78604742232836,24.784787798199,4.63189669239788));
#453741=CARTESIAN_POINT('Ctrl Pts',(-5.40735816264999,24.7133047275048,
4.15240479236238));
#453742=CARTESIAN_POINT('Ctrl Pts',(-4.25725342975252,24.6418216568106,
5.05126835371239));
#453743=CARTESIAN_POINT('Ctrl Pts',(-4.38944335790392,24.5703385861164,
6.50496106867921));
#453744=CARTESIAN_POINT('Ctrl Pts',(-5.68281734635597,24.4988555154223,
7.18162963832199));
#453745=CARTESIAN_POINT('Ctrl Pts',(-6.95240396480877,24.4273724447281,
6.4613196666284));
#453746=CARTESIAN_POINT('Ctrl Pts',(-7.03502543671246,24.3558893740339,
5.00396921476326));
#453747=CARTESIAN_POINT('Ctrl Pts',(-5.85498510857851,24.2844063033397,
4.14478270244581));
#453748=CARTESIAN_POINT('Ctrl Pts',(-4.49341967622111,24.2129232326456,
4.67093497503136));
#453749=CARTESIAN_POINT('Ctrl Pts',(-4.19777663638434,24.1414401619514,
6.10037256921808));
#453750=CARTESIAN_POINT('Ctrl Pts',(-5.23892007073304,24.0699570912572,
7.12346444664167));
#453751=CARTESIAN_POINT('Ctrl Pts',(-6.662968703113,23.998474020563,6.80286792203874));
#453752=CARTESIAN_POINT('Ctrl Pts',(-7.16522879152533,23.9269909498688,
5.43230911237055));
#453753=CARTESIAN_POINT('Ctrl Pts',(-6.2855365564656,23.8555078791747,4.26747512907024));
#453754=CARTESIAN_POINT('Ctrl Pts',(-4.82985391579145,23.7840248084805,
4.37557081254884));
#453755=CARTESIAN_POINT('Ctrl Pts',(-4.13185724083954,23.7125417377863,
5.6575604101698));
#453756=CARTESIAN_POINT('Ctrl Pts',(-4.83104150205929,23.6410586670921,
6.93890266242659));
#453757=CARTESIAN_POINT('Ctrl Pts',(-6.28682364983266,23.569575596398,7.04564953674368));
#453758=CARTESIAN_POINT('Ctrl Pts',(-7.16543624640093,23.4980925257038,
5.88000083782648));
#453759=CARTESIAN_POINT('Ctrl Pts',(-6.66190630419616,23.4266094550096,
4.50990820099156));
#453760=CARTESIAN_POINT('Ctrl Pts',(-5.23756146736659,23.3551263843154,
4.19063094092434));
#453761=CARTESIAN_POINT('Ctrl Pts',(-4.19736598356862,23.2836433136212,
5.21468783779196));
#453762=CARTESIAN_POINT('Ctrl Pts',(-4.49433434427902,23.2121602429271,
6.64384941569999));
#453763=CARTESIAN_POINT('Ctrl Pts',(-5.85638486317849,23.1406771722329,
7.16874271925581));
#453764=CARTESIAN_POINT('Ctrl Pts',(-7.03563221165043,23.0691941015387,
6.3084575374563));
#453765=CARTESIAN_POINT('Ctrl Pts',(-6.95165327175697,22.9977110308445,
4.85119529970875));
#453766=CARTESIAN_POINT('Ctrl Pts',(-5.68141376558384,22.9262279601503,
4.13204038713623));
#453767=CARTESIAN_POINT('Ctrl Pts',(-4.38863987327371,22.8547448894562,
4.80994952176022));
#453768=CARTESIAN_POINT('Ctrl Pts',(-4.25785081625158,22.783261818762,6.26368089065206));
#453769=CARTESIAN_POINT('Ctrl Pts',(-5.40868234342554,22.7117787480678,
7.16164157512573));
#453770=CARTESIAN_POINT('Ctrl Pts',(-6.78713386963137,22.6402956773736,
6.6805523241845));
#453771=CARTESIAN_POINT('Ctrl Pts',(-7.12954990426925,22.5688126066795,
5.26231872215201));
#453772=CARTESIAN_POINT('Ctrl Pts',(-6.12366999440581,22.4973295359852,
4.20406666678212));
#453773=CARTESIAN_POINT('Ctrl Pts',(-4.68809392709695,22.4258464652911,
4.47983331463011));
#453774=CARTESIAN_POINT('Ctrl Pts',(-4.32622391325397,22.3781910848283,
5.37807265034296));
#453775=CARTESIAN_POINT('Ctrl Pts',(-4.37532354240196,22.3543633945969,
5.80443435631943));
#453776=CARTESIAN_POINT('Ctrl Pts',(-4.61186924884874,26.0485455351344,
5.05498833669907));
#453777=CARTESIAN_POINT('Ctrl Pts',(-4.41163019717349,26.024717844903,5.40265192052163));
#453778=CARTESIAN_POINT('Ctrl Pts',(-4.38906985506273,25.9770624644402,
6.30764248137266));
#453779=CARTESIAN_POINT('Ctrl Pts',(-5.51871011120511,25.905579393746,7.07663155607638));
#453780=CARTESIAN_POINT('Ctrl Pts',(-6.77430532526158,25.8340963230518,
6.54152598941931));
#453781=CARTESIAN_POINT('Ctrl Pts',(-7.00638637325414,25.7626132523577,
5.1975302126156));
#453782=CARTESIAN_POINT('Ctrl Pts',(-6.00190474293836,25.6911301816635,
4.27353221173564));
#453783=CARTESIAN_POINT('Ctrl Pts',(-4.68136318011483,25.6196471109693,
4.61733634566934));
#453784=CARTESIAN_POINT('Ctrl Pts',(-4.25451662209878,25.5481640402751,
5.91331704545575));
#453785=CARTESIAN_POINT('Ctrl Pts',(-5.11249056981941,25.4766809695809,
6.97443939411569));
#453786=CARTESIAN_POINT('Ctrl Pts',(-6.46919328847102,25.4051978988868,
6.82835211754091));
#453787=CARTESIAN_POINT('Ctrl Pts',(-7.08164661869466,25.3337148281926,
5.60898280515531));
#453788=CARTESIAN_POINT('Ctrl Pts',(-6.38872202076577,25.2622317574984,
4.43345777007097));
#453789=CARTESIAN_POINT('Ctrl Pts',(-5.02527115647435,25.1907486868042,
4.37879881483496));
#453790=CARTESIAN_POINT('Ctrl Pts',(-4.24046704839446,25.1192656161101,
5.49507252586478));
#453791=CARTESIAN_POINT('Ctrl Pts',(-4.75333737058416,25.0477825454159,
6.75957001205556));
#453792=CARTESIAN_POINT('Ctrl Pts',(-6.09399690839474,24.9762994747217,
7.01377318104996));
#453793=CARTESIAN_POINT('Ctrl Pts',(-7.03415210716631,24.9048164040275,
6.0247860748808));
#453794=CARTESIAN_POINT('Ctrl Pts',(-6.71244559509181,24.8333333333333,
4.69870430227372));
#453795=CARTESIAN_POINT('Ctrl Pts',(-5.42362051261082,24.7618502626392,
4.25046610554157));
#453796=CARTESIAN_POINT('Ctrl Pts',(-4.34848061663154,24.6903671919449,
5.09074095026354));
#453797=CARTESIAN_POINT('Ctrl Pts',(-4.47205428913018,24.6188841212508,
6.44968069692277));
#453798=CARTESIAN_POINT('Ctrl Pts',(-5.68112502471735,24.5474010505566,
7.08224341470704));
#453799=CARTESIAN_POINT('Ctrl Pts',(-6.86795887198032,24.4759179798625,
6.40888387979891));
#453800=CARTESIAN_POINT('Ctrl Pts',(-6.94519500375797,24.4044349091682,
5.04652481074591));
#453801=CARTESIAN_POINT('Ctrl Pts',(-5.84207074093975,24.3329518384741,
4.24334083014216));
#453802=CARTESIAN_POINT('Ctrl Pts',(-4.56925333967074,24.2614687677799,
4.73519803534796));
#453803=CARTESIAN_POINT('Ctrl Pts',(-4.29288057290861,24.1899856970857,
6.07146363130893));
#453804=CARTESIAN_POINT('Ctrl Pts',(-5.2661613635068,24.1185026263916,7.02786948132164));
#453805=CARTESIAN_POINT('Ctrl Pts',(-6.59738925492609,24.0470195556973,
6.72816971985337));
#453806=CARTESIAN_POINT('Ctrl Pts',(-7.0669115895136,23.9755364850032,5.44694513750786));
#453807=CARTESIAN_POINT('Ctrl Pts',(-6.2445584671913,23.904053414309,4.35803605660743));
#453808=CARTESIAN_POINT('Ctrl Pts',(-4.88375849993059,23.8325703436148,
4.4590859684691));
#453809=CARTESIAN_POINT('Ctrl Pts',(-4.23125786147911,23.7610872729207,
5.65751435782136));
#453810=CARTESIAN_POINT('Ctrl Pts',(-4.88486867828213,23.6896042022265,
6.85533759634902));
#453811=CARTESIAN_POINT('Ctrl Pts',(-6.24576166668191,23.6181211315323,
6.95512661561532));
#453812=CARTESIAN_POINT('Ctrl Pts',(-7.06710552229816,23.5466380608381,
5.86545592297768));
#453813=CARTESIAN_POINT('Ctrl Pts',(-6.59639610410402,23.475154990144,4.58466712791061));
#453814=CARTESIAN_POINT('Ctrl Pts',(-5.26489131510139,23.4036719194498,
4.28620064015657));
#453815=CARTESIAN_POINT('Ctrl Pts',(-4.29249668680419,23.3321888487556,
5.24350860879812));
#453816=CARTESIAN_POINT('Ctrl Pts',(-4.57010838886107,23.2607057780614,
6.57951617946397));
#453817=CARTESIAN_POINT('Ctrl Pts',(-5.84337925830513,23.1892227073672,
7.07019647634744));
#453818=CARTESIAN_POINT('Ctrl Pts',(-6.94576222857241,23.1177396366731,
6.26598543850372));
#453819=CARTESIAN_POINT('Ctrl Pts',(-6.86725710976116,23.0462565659789,
4.90370883369462));
#453820=CARTESIAN_POINT('Ctrl Pts',(-5.67981293057308,22.9747734952847,
4.23142907013928));
#453821=CARTESIAN_POINT('Ctrl Pts',(-4.47130317633407,22.9032904245905,
4.86515149178938));
#453822=CARTESIAN_POINT('Ctrl Pts',(-4.34903906495375,22.8318073538964,
6.22412737287685));
#453823=CARTESIAN_POINT('Ctrl Pts',(-5.42485838212006,22.7603242832022,
7.06355819103049));
#453824=CARTESIAN_POINT('Ctrl Pts',(-6.7134612268051,22.688841212508,6.613826760128));
#453825=CARTESIAN_POINT('Ctrl Pts',(-7.03355828347467,22.6173581418138,
5.28803487026933));
#453826=CARTESIAN_POINT('Ctrl Pts',(-6.0932425098549,22.5458750711196,4.29876061359894));
#453827=CARTESIAN_POINT('Ctrl Pts',(-4.75123855184286,22.4743920004255,
4.55655254906459));
#453828=CARTESIAN_POINT('Ctrl Pts',(-4.41295554342414,22.4267366199627,
5.39624385572484));
#453829=CARTESIAN_POINT('Ctrl Pts',(-4.45885481560765,22.4029089297313,
5.79481493112442));
#453830=CARTESIAN_POINT('Ctrl Pts',(-4.6847314899806,26.0970910702687,5.09695380776383));
#453831=CARTESIAN_POINT('Ctrl Pts',(-4.49845423798335,26.0732633800373,
5.42037631936769));
#453832=CARTESIAN_POINT('Ctrl Pts',(-4.47746693057576,26.0256079995745,
6.26226581768684));
#453833=CARTESIAN_POINT('Ctrl Pts',(-5.52834227631476,25.9541249288804,
6.97763662299825));
#453834=CARTESIAN_POINT('Ctrl Pts',(-6.69639028762206,25.8826418581862,
6.47984164418979));
#453835=CARTESIAN_POINT('Ctrl Pts',(-6.91228933178459,25.811158787492,5.22955685755916));
#453836=CARTESIAN_POINT('Ctrl Pts',(-5.97784584430541,25.7396757167978,
4.36998522547805));
#453837=CARTESIAN_POINT('Ctrl Pts',(-4.74937991114736,25.6681926461037,
4.68981738987686));
#453838=CARTESIAN_POINT('Ctrl Pts',(-4.35229551034491,25.5967095754095,
5.89543498233936));
#453839=CARTESIAN_POINT('Ctrl Pts',(-5.15044665983114,25.5252265047153,
6.88256987679448));
#453840=CARTESIAN_POINT('Ctrl Pts',(-6.41255238842542,25.4537434340211,
6.74666863173542));
#453841=CARTESIAN_POINT('Ctrl Pts',(-6.9823020070745,25.3822603633269,5.61232064726061));
#453842=CARTESIAN_POINT('Ctrl Pts',(-6.33769203282816,25.3107772926328,
4.51875986899336));
#453843=CARTESIAN_POINT('Ctrl Pts',(-5.06930867749051,25.2392942219386,
4.46791204538842));
#453844=CARTESIAN_POINT('Ctrl Pts',(-4.33922555241473,25.1678111512444,
5.50635283717083));
#453845=CARTESIAN_POINT('Ctrl Pts',(-4.81633565381188,25.0963280805502,
6.68268240382831));
#453846=CARTESIAN_POINT('Ctrl Pts',(-6.06351682290909,25.0248450098561,
6.91916108954474));
#453847=CARTESIAN_POINT('Ctrl Pts',(-6.93811908162397,24.9533619391618,
5.99913176031738));
#453848=CARTESIAN_POINT('Ctrl Pts',(-6.63884376785526,24.8818788684677,
4.76551191214957));
#453849=CARTESIAN_POINT('Ctrl Pts',(-5.43988286257165,24.8103957977735,
4.34852741872076));
#453850=CARTESIAN_POINT('Ctrl Pts',(-4.43970780351055,24.7389127270793,
5.13021354681469));
#453851=CARTESIAN_POINT('Ctrl Pts',(-4.55466522035644,24.6674296563852,
6.39440032516631));
#453852=CARTESIAN_POINT('Ctrl Pts',(-5.67943270307874,24.595946585691,6.9828571910921));
#453853=CARTESIAN_POINT('Ctrl Pts',(-6.78351377915185,24.5244635149968,
6.35644809296942));
#453854=CARTESIAN_POINT('Ctrl Pts',(-6.85536457080349,24.4529804443026,
5.08908040672856));
#453855=CARTESIAN_POINT('Ctrl Pts',(-5.82915637330098,24.3814973736085,
4.34189895783853));
#453856=CARTESIAN_POINT('Ctrl Pts',(-4.64508700312038,24.3100143029143,
4.79946109566455));
#453857=CARTESIAN_POINT('Ctrl Pts',(-4.38798450943289,24.2385312322201,
6.0425546933998));
#453858=CARTESIAN_POINT('Ctrl Pts',(-5.29340265628057,24.1670481615259,
6.93227451600161));
#453859=CARTESIAN_POINT('Ctrl Pts',(-6.53180980673917,24.0955650908317,
6.65347151766801));
#453860=CARTESIAN_POINT('Ctrl Pts',(-6.96859438750187,24.0240820201376,
5.46158116264517));
#453861=CARTESIAN_POINT('Ctrl Pts',(-6.20358037791699,23.9525989494434,
4.44859698414461));
#453862=CARTESIAN_POINT('Ctrl Pts',(-4.93766308406974,23.8811158787492,
4.54260112438938));
#453863=CARTESIAN_POINT('Ctrl Pts',(-4.33065848211867,23.809632808055,5.65746830547292));
#453864=CARTESIAN_POINT('Ctrl Pts',(-4.93869585450498,23.7381497373608,
6.77177253027144));
#453865=CARTESIAN_POINT('Ctrl Pts',(-6.20469968353116,23.6666666666667,
6.86460369448697));
#453866=CARTESIAN_POINT('Ctrl Pts',(-6.96877479819537,23.5951835959725,
5.85091100812889));
#453867=CARTESIAN_POINT('Ctrl Pts',(-6.53088590401187,23.5237005252783,
4.65942605482967));
#453868=CARTESIAN_POINT('Ctrl Pts',(-5.29222116283617,23.4522174545841,
4.3817703393888));
#453869=CARTESIAN_POINT('Ctrl Pts',(-4.38762739003978,23.38073438389,5.27232937980428));
#453870=CARTESIAN_POINT('Ctrl Pts',(-4.6458824334431,23.3092513131958,6.51518294322794));
#453871=CARTESIAN_POINT('Ctrl Pts',(-5.83037365343178,23.2377682425016,
6.97165023343906));
#453872=CARTESIAN_POINT('Ctrl Pts',(-6.85589224549438,23.1662851718074,
6.22351333955115));
#453873=CARTESIAN_POINT('Ctrl Pts',(-6.78286094776533,23.0948021011132,
4.9562223676805));
#453874=CARTESIAN_POINT('Ctrl Pts',(-5.67821209556232,23.0233190304191,
4.33081775314232));
#453875=CARTESIAN_POINT('Ctrl Pts',(-4.55396647939442,22.9518359597249,
4.92035346181854));
#453876=CARTESIAN_POINT('Ctrl Pts',(-4.44022731365593,22.8803528890307,
6.18457385510163));
#453877=CARTESIAN_POINT('Ctrl Pts',(-5.44103442081457,22.8088698183366,
6.96547480693525));
#453878=CARTESIAN_POINT('Ctrl Pts',(-6.63978858397884,22.7373867476423,
6.5471011960715));
#453879=CARTESIAN_POINT('Ctrl Pts',(-6.93756666268008,22.6659036769482,
5.31375101838666));
#453880=CARTESIAN_POINT('Ctrl Pts',(-6.06281502530401,22.594420606254,4.39345456041576));
#453881=CARTESIAN_POINT('Ctrl Pts',(-4.81438317658877,22.5229375355598,
4.63327178349907));
#453882=CARTESIAN_POINT('Ctrl Pts',(-4.49968717359432,22.475282155097,5.41441506110672));
#453883=CARTESIAN_POINT('Ctrl Pts',(-4.54238608881333,22.4514544648656,
5.78519550592941));
#453884=CARTESIAN_POINT('Ctrl Pts',(-4.75759373111246,26.1456366054031,
5.13891927882859));
#453885=CARTESIAN_POINT('Ctrl Pts',(-4.58527827879321,26.1218089151717,
5.43810071821374));
#453886=CARTESIAN_POINT('Ctrl Pts',(-4.5658640060888,26.0741535347089,6.21688915400102));
#453887=CARTESIAN_POINT('Ctrl Pts',(-5.53797444142439,26.0026704640147,
6.87864168992013));
#453888=CARTESIAN_POINT('Ctrl Pts',(-6.61847524998255,25.9311873933205,
6.41815729896025));
#453889=CARTESIAN_POINT('Ctrl Pts',(-6.81819229031504,25.8597043226264,
5.26158350250274));
#453890=CARTESIAN_POINT('Ctrl Pts',(-5.95378694567247,25.7882212519322,
4.46643823922044));
#453891=CARTESIAN_POINT('Ctrl Pts',(-4.81739664217988,25.716738181238,4.76229843408439));
#453892=CARTESIAN_POINT('Ctrl Pts',(-4.45007439859105,25.6452551105439,
5.87755291922296));
#453893=CARTESIAN_POINT('Ctrl Pts',(-5.18840274984287,25.5737720398496,
6.79070035947327));
#453894=CARTESIAN_POINT('Ctrl Pts',(-6.35591148837984,25.5022889691555,
6.66498514592993));
#453895=CARTESIAN_POINT('Ctrl Pts',(-6.88295739545434,25.4308058984613,
5.61565848936591));
#453896=CARTESIAN_POINT('Ctrl Pts',(-6.28666204489054,25.3593228277671,
4.60406196791575));
#453897=CARTESIAN_POINT('Ctrl Pts',(-5.11334619850669,25.2878397570729,
4.55702527594187));
#453898=CARTESIAN_POINT('Ctrl Pts',(-4.43798405643501,25.2163566863788,
5.5176331484769));
#453899=CARTESIAN_POINT('Ctrl Pts',(-4.87933393703958,25.1448736156846,
6.60579479560105));
#453900=CARTESIAN_POINT('Ctrl Pts',(-6.03303673742344,25.0733905449905,
6.82454899803953));
#453901=CARTESIAN_POINT('Ctrl Pts',(-6.84208605608162,25.0019074742962,
5.97347744575396));
#453902=CARTESIAN_POINT('Ctrl Pts',(-6.56524194061871,24.9304244036021,
4.83231952202541));
#453903=CARTESIAN_POINT('Ctrl Pts',(-5.45614521253248,24.8589413329079,
4.44658873189996));
#453904=CARTESIAN_POINT('Ctrl Pts',(-4.53093499038958,24.7874582622137,
5.16968614336582));
#453905=CARTESIAN_POINT('Ctrl Pts',(-4.63727615158269,24.7159751915195,
6.33911995340987));
#453906=CARTESIAN_POINT('Ctrl Pts',(-5.67774038144014,24.6444921208253,
6.88347096747714));
#453907=CARTESIAN_POINT('Ctrl Pts',(-6.6990686863234,24.5730090501312,6.30401230613993));
#453908=CARTESIAN_POINT('Ctrl Pts',(-6.76553413784902,24.501525979437,5.13163600271121));
#453909=CARTESIAN_POINT('Ctrl Pts',(-5.81624200566219,24.4300429087428,
4.44045708553489));
#453910=CARTESIAN_POINT('Ctrl Pts',(-4.72092066657003,24.3585598380486,
4.86372415598115));
#453911=CARTESIAN_POINT('Ctrl Pts',(-4.48308844595715,24.2870767673544,
6.01364575549064));
#453912=CARTESIAN_POINT('Ctrl Pts',(-5.32064394905434,24.2155936966603,
6.83667955068161));
#453913=CARTESIAN_POINT('Ctrl Pts',(-6.46623035855224,24.1441106259661,
6.57877331548262));
#453914=CARTESIAN_POINT('Ctrl Pts',(-6.87027718549015,24.0726275552719,
5.4762171877825));
#453915=CARTESIAN_POINT('Ctrl Pts',(-6.16260228864268,24.0011444845777,
4.53915791168179));
#453916=CARTESIAN_POINT('Ctrl Pts',(-4.99156766820889,23.9296614138836,
4.62611628030965));
#453917=CARTESIAN_POINT('Ctrl Pts',(-4.43005910275823,23.8581783431894,
5.65742225312448));
#453918=CARTESIAN_POINT('Ctrl Pts',(-4.99252303072782,23.7866952724952,
6.68820746419386));
#453919=CARTESIAN_POINT('Ctrl Pts',(-6.16363770038041,23.715212201801,6.77408077335862));
#453920=CARTESIAN_POINT('Ctrl Pts',(-6.87044407409259,23.6437291311068,
5.83636609328008));
#453921=CARTESIAN_POINT('Ctrl Pts',(-6.46537570391973,23.5722460604127,
4.73418498174874));
#453922=CARTESIAN_POINT('Ctrl Pts',(-5.31955101057096,23.5007629897185,
4.47734003862102));
#453923=CARTESIAN_POINT('Ctrl Pts',(-4.48275809327536,23.4292799190243,
5.30115015081045));
#453924=CARTESIAN_POINT('Ctrl Pts',(-4.72165647802514,23.3577968483301,
6.4508497069919));
#453925=CARTESIAN_POINT('Ctrl Pts',(-5.81736804855842,23.286313777636,6.87310399053069));
#453926=CARTESIAN_POINT('Ctrl Pts',(-6.76602226241636,23.2148307069418,
6.18104124059857));
#453927=CARTESIAN_POINT('Ctrl Pts',(-6.69846478576951,23.1433476362476,
5.00873590166637));
#453928=CARTESIAN_POINT('Ctrl Pts',(-5.67661126055156,23.0718645655534,
4.43020643614536));
#453929=CARTESIAN_POINT('Ctrl Pts',(-4.63662978245478,23.0003814948593,
4.97555543184771));
#453930=CARTESIAN_POINT('Ctrl Pts',(-4.53141556235811,22.928898424165,6.1450203373264));
#453931=CARTESIAN_POINT('Ctrl Pts',(-5.4572104595091,22.8574153534709,6.86739142284002));
#453932=CARTESIAN_POINT('Ctrl Pts',(-6.56611594115258,22.7859322827767,
6.48037563201499));
#453933=CARTESIAN_POINT('Ctrl Pts',(-6.8415750418855,22.7144492120825,5.33946716650399));
#453934=CARTESIAN_POINT('Ctrl Pts',(-6.0323875407531,22.6429661413883,4.48814850723257));
#453935=CARTESIAN_POINT('Ctrl Pts',(-4.87752780133468,22.5714830706942,
4.70999101793355));
#453936=CARTESIAN_POINT('Ctrl Pts',(-4.58641880376449,22.5238276902314,
5.4325862664886));
#453937=CARTESIAN_POINT('Ctrl Pts',(-4.62591736201901,22.5,5.7755760807344));
#453938=CARTESIAN_POINT('Ctrl Pts',(-4.92443355077908,25.6019615242271,
6.39006796800886));
#453939=CARTESIAN_POINT('Ctrl Pts',(-5.02053320993752,25.5925650294346,
6.48712194011206));
#453940=CARTESIAN_POINT('Ctrl Pts',(-5.13467106978717,25.5831685346421,
6.56580235206401));
#453941=CARTESIAN_POINT('Ctrl Pts',(-5.25993281439039,25.5737720398497,
6.617556583841));
#453942=CARTESIAN_POINT('Ctrl Pts',(-5.57757232935519,25.5499443496183,
6.74879528829216));
#453943=CARTESIAN_POINT('Ctrl Pts',(-5.96674190886751,25.5261166593869,
6.70689021711104));
#453944=CARTESIAN_POINT('Ctrl Pts',(-6.24916768313609,25.5022889691555,
6.51104990542648));
#453945=CARTESIAN_POINT('Ctrl Pts',(-6.53159345740467,25.4784612789241,
6.31520959374192));
#453946=CARTESIAN_POINT('Ctrl Pts',(-6.7072754264295,25.4546335886927,5.96543404155391));
#453947=CARTESIAN_POINT('Ctrl Pts',(-6.69573385251462,25.4308058984613,
5.62194684521822));
#453948=CARTESIAN_POINT('Ctrl Pts',(-6.68419227859974,25.4069782082299,
5.27845964888252));
#453949=CARTESIAN_POINT('Ctrl Pts',(-6.48542716174514,25.3831505179985,
4.94126080839914));
#453950=CARTESIAN_POINT('Ctrl Pts',(-6.19049196225386,25.3593228277671,
4.76482193949513));
#453951=CARTESIAN_POINT('Ctrl Pts',(-5.89555676276259,25.3354951375357,
4.58838307059113));
#453952=CARTESIAN_POINT('Ctrl Pts',(-5.50445148063464,25.3116674473043,
4.5727041732665));
#453953=CARTESIAN_POINT('Ctrl Pts',(-5.19633848255872,25.2878397570729,
4.72496603669335));
#453954=CARTESIAN_POINT('Ctrl Pts',(-4.8882254844828,25.2640120668416,4.87722790012021));
#453955=CARTESIAN_POINT('Ctrl Pts',(-4.66310477045891,25.2401843766102,
5.19743052429855));
#453956=CARTESIAN_POINT('Ctrl Pts',(-4.62410272688105,25.2163566863788,
5.53889211090842));
#453957=CARTESIAN_POINT('Ctrl Pts',(-4.58896793348097,25.1948916323282,
5.84649605160076));
#453958=CARTESIAN_POINT('Ctrl Pts',(-4.70487246063661,25.1734265782776,
6.17135209942283));
#453959=CARTESIAN_POINT('Ctrl Pts',(-4.92254817630007,25.1519615242271,
6.39198798715976));
#453960=CARTESIAN_POINT('Origin',(-5.65685387860011,26.,5.65685387860011));
#453961=CARTESIAN_POINT('Origin',(-5.65685387860012,26.993675081176,-5.65685387860011));
#453962=CARTESIAN_POINT('Ctrl Pts',(-6.57057130100612,25.868675081176,-4.74432962138981));
#453963=CARTESIAN_POINT('Ctrl Pts',(-6.60882993708832,25.8656848283261,
-4.78199706987976));
#453964=CARTESIAN_POINT('Ctrl Pts',(-6.92960341635463,25.8388668852448,
-5.14157728587623));
#453965=CARTESIAN_POINT('Ctrl Pts',(-7.09568592881682,25.7882212519322,
-6.16255878293893));
#453966=CARTESIAN_POINT('Ctrl Pts',(-6.01152748645437,25.716738181238,-7.13997732676548));
#453967=CARTESIAN_POINT('Ctrl Pts',(-4.60259286076204,25.6452551105438,
-6.7587374620765));
#453968=CARTESIAN_POINT('Ctrl Pts',(-4.15947051927595,25.5737720398497,
-5.36788602689621));
#453969=CARTESIAN_POINT('Ctrl Pts',(-5.08827462376231,25.5022889691555,
-4.24182426511434));
#453970=CARTESIAN_POINT('Ctrl Pts',(-6.13675122222029,25.450589982931,-4.36502559631504));
#453971=CARTESIAN_POINT('Ctrl Pts',(-6.51790892062316,25.4227186869378,
-4.69148744470697));
#453972=CARTESIAN_POINT('Ctrl Pts',(-6.56885365284802,25.418675081176,-4.74334636410459));
#453973=CARTESIAN_POINT('Ctrl Pts',(-6.56704169373441,25.906324918824,-4.74450601134849));
#453974=CARTESIAN_POINT('Ctrl Pts',(-6.7750658664325,25.8898945654199,-4.95573944791419));
#453975=CARTESIAN_POINT('Ctrl Pts',(-7.11639071403833,25.8496365217844,
-5.64807137163848));
#453976=CARTESIAN_POINT('Ctrl Pts',(-6.60321033464885,25.7855507879174,
-6.8522203629011));
#453977=CARTESIAN_POINT('Ctrl Pts',(-5.16550356767203,25.7140677172233,
-7.1004834147237));
#453978=CARTESIAN_POINT('Ctrl Pts',(-4.17707919799325,25.6425846465291,
-6.02596364157129));
#453979=CARTESIAN_POINT('Ctrl Pts',(-4.5448553014618,25.5711015758349,-4.61334644908231));
#453980=CARTESIAN_POINT('Ctrl Pts',(-5.74896333949311,25.5090149999332,
-4.21675923787011));
#453981=CARTESIAN_POINT('Ctrl Pts',(-6.3830054663296,25.4707561142629,-4.5629353888518));
#453982=CARTESIAN_POINT('Ctrl Pts',(-6.56829321884323,25.456324918824,-4.74640124271564));
#453983=CARTESIAN_POINT('Ctrl Pts',(-5.59475217632212,26.,-6.69274404704181));
#453984=CARTESIAN_POINT('Ctrl Pts',(-5.25011429538726,25.9761723097686,
-6.67208297724159));
#453985=CARTESIAN_POINT('Ctrl Pts',(-4.58904744425369,25.9285169293058,
-6.25991935236784));
#453986=CARTESIAN_POINT('Ctrl Pts',(-4.5711145089162,25.8570338586116,-5.08408179813166));
#453987=CARTESIAN_POINT('Ctrl Pts',(-5.55001366141289,25.7855507879175,
-4.43501771280631));
#453988=CARTESIAN_POINT('Ctrl Pts',(-6.62575617389683,25.7140677172233,
-4.90440858615388));
#453989=CARTESIAN_POINT('Ctrl Pts',(-6.81433291744693,25.6425846465291,
-6.06367191307887));
#453990=CARTESIAN_POINT('Ctrl Pts',(-5.94217367437589,25.5711015758349,
-6.84996345870369));
#453991=CARTESIAN_POINT('Ctrl Pts',(-4.80874583886255,25.4996185051408,
-6.54327224197424));
#453992=CARTESIAN_POINT('Ctrl Pts',(-4.45227280795,25.4281354344466,-5.42439156223909));
#453993=CARTESIAN_POINT('Ctrl Pts',(-5.19945610983427,25.3566523637524,
-4.51852288527076));
#453994=CARTESIAN_POINT('Ctrl Pts',(-6.36568271985868,25.2851692930583,
-4.65556044151951));
#453995=CARTESIAN_POINT('Ctrl Pts',(-6.88249940298929,25.213686222364,-5.70997789504277));
#453996=CARTESIAN_POINT('Ctrl Pts',(-6.27639179734011,25.1422031516699,
-6.71571945020394));
#453997=CARTESIAN_POINT('Ctrl Pts',(-5.10267450019954,25.0707200809757,
-6.7513451989237));
#453998=CARTESIAN_POINT('Ctrl Pts',(-4.43668748453226,24.9992370102815,
-5.78421192833873));
#453999=CARTESIAN_POINT('Ctrl Pts',(-4.88860074260098,24.9277539395873,
-4.7003955508837));
#454000=CARTESIAN_POINT('Ctrl Pts',(-6.04437662247731,24.8562708688931,
-4.49287282235238));
#454001=CARTESIAN_POINT('Ctrl Pts',(-6.84510966506768,24.784787798199,-5.35177365831405));
#454002=CARTESIAN_POINT('Ctrl Pts',(-6.55717903824976,24.7133047275048,
-6.49018471285718));
#454003=CARTESIAN_POINT('Ctrl Pts',(-5.44438294256282,24.6418216568106,
-6.86510957377));
#454004=CARTESIAN_POINT('Ctrl Pts',(-4.52624977050191,24.5703385861164,
-6.13304718756448));
#454005=CARTESIAN_POINT('Ctrl Pts',(-4.64396052187118,24.4988555154223,
-4.96470306042393));
#454006=CARTESIAN_POINT('Ctrl Pts',(-5.68967021074952,24.4273724447281,
-4.43049797487471));
#454007=CARTESIAN_POINT('Ctrl Pts',(-6.70531403099034,24.3558893740339,
-5.01986328076133));
#454008=CARTESIAN_POINT('Ctrl Pts',(-6.76037309820141,24.2844063033397,
-6.19283059794665));
#454009=CARTESIAN_POINT('Ctrl Pts',(-5.80440305573226,24.2129232326455,
-6.87474342740734));
#454010=CARTESIAN_POINT('Ctrl Pts',(-4.71325048867858,24.1414401619514,
-6.44084262551865));
#454011=CARTESIAN_POINT('Ctrl Pts',(-4.4866143522216,24.0699570912572,-5.28866213152759));
#454012=CARTESIAN_POINT('Ctrl Pts',(-5.3321355513588,23.9984740205631,-4.47381384511066));
#454013=CARTESIAN_POINT('Ctrl Pts',(-6.47515921171814,23.9269909498688,
-4.74285054378755));
#454014=CARTESIAN_POINT('Ctrl Pts',(-6.86846279219781,23.8555078791747,
-5.84928450947304));
#454015=CARTESIAN_POINT('Ctrl Pts',(-6.15170698086798,23.7840248084805,
-6.77941618151556));
#454016=CARTESIAN_POINT('Ctrl Pts',(-4.98157355760958,23.7125417377863,
-6.68107173221035));
#454017=CARTESIAN_POINT('Ctrl Pts',(-4.43012269359923,23.6410586670921,
-5.64435299191054));
#454018=CARTESIAN_POINT('Ctrl Pts',(-5.00258598787076,23.569575596398,-4.61908739135743));
#454019=CARTESIAN_POINT('Ctrl Pts',(-6.17448062637044,23.4980925257038,
-4.54460915448656));
#454020=CARTESIAN_POINT('Ctrl Pts',(-6.87213254456039,23.4266094550096,
-5.48915421344718));
#454021=CARTESIAN_POINT('Ctrl Pts',(-6.45636332421143,23.3551263843154,
-6.58734339945679));
#454022=CARTESIAN_POINT('Ctrl Pts',(-5.30809370313679,23.2836433136213,
-6.8330308949199));
#454023=CARTESIAN_POINT('Ctrl Pts',(-4.47935503415496,23.212160242927,-6.00112122066856));
#454024=CARTESIAN_POINT('Ctrl Pts',(-4.72942128924326,23.1406771722329,
-4.85379852261455));
#454025=CARTESIAN_POINT('Ctrl Pts',(-5.82919498069919,23.0691941015387,
-4.44222413342346));
#454026=CARTESIAN_POINT('Ctrl Pts',(-6.77105943752212,22.9977110308445,
-5.14347668616411));
#454027=CARTESIAN_POINT('Ctrl Pts',(-6.69212899367236,22.9262279601504,
-6.31507855179967));
#454028=CARTESIAN_POINT('Ctrl Pts',(-5.66464494341573,22.8547448894562,
-6.88362364563197));
#454029=CARTESIAN_POINT('Ctrl Pts',(-4.63011853598606,22.783261818762,-6.32821994284799));
#454030=CARTESIAN_POINT('Ctrl Pts',(-4.53608521045973,22.7117787480678,
-5.15771839492686));
#454031=CARTESIAN_POINT('Ctrl Pts',(-5.46925286619013,22.6402956773736,
-4.4445208236608));
#454032=CARTESIAN_POINT('Ctrl Pts',(-6.57357515235991,22.5688126066795,
-4.84204067651847));
#454033=CARTESIAN_POINT('Ctrl Pts',(-6.8394368280484,22.4973295359852,-5.98608844956735));
#454034=CARTESIAN_POINT('Ctrl Pts',(-6.01893246982621,22.4258464652911,
-6.82851835303725));
#454035=CARTESIAN_POINT('Ctrl Pts',(-5.25534692011694,22.3781910848283,
-6.67416374956871));
#454036=CARTESIAN_POINT('Ctrl Pts',(-4.99063298333217,22.3543633945969,
-6.45251384441992));
#454037=CARTESIAN_POINT('Ctrl Pts',(-5.58972040746333,26.0485455351344,
-6.77667668816906));
#454038=CARTESIAN_POINT('Ctrl Pts',(-5.21715836192049,26.024717844903,-6.75434156236399));
#454039=CARTESIAN_POINT('Ctrl Pts',(-4.50252879876621,25.9770624644402,
-6.30878252293169));
#454040=CARTESIAN_POINT('Ctrl Pts',(-4.48314285357121,25.905579393746,-5.03767313923882));
#454041=CARTESIAN_POINT('Ctrl Pts',(-5.54135696992153,25.8340963230518,
-4.33601886182374));
#454042=CARTESIAN_POINT('Ctrl Pts',(-6.70426114586779,25.7626132523576,
-4.84344196766208));
#454043=CARTESIAN_POINT('Ctrl Pts',(-6.90811725457023,25.6911301816635,
-6.09663420303223));
#454044=CARTESIAN_POINT('Ctrl Pts',(-5.96529161173539,25.6196471109693,
-6.94663474805762));
#454045=CARTESIAN_POINT('Ctrl Pts',(-4.74002817949571,25.5481640402751,
-6.61509398200833));
#454046=CARTESIAN_POINT('Ctrl Pts',(-4.35467204505865,25.4766809695809,
-5.40555638379146));
#454047=CARTESIAN_POINT('Ctrl Pts',(-5.16239561447694,25.4051978988867,
-4.42629001188529));
#454048=CARTESIAN_POINT('Ctrl Pts',(-6.42311533054124,25.3337148281926,
-4.57443098853514));
#454049=CARTESIAN_POINT('Ctrl Pts',(-6.98180690592904,25.2622317574984,
-5.71428225002476));
#454050=CARTESIAN_POINT('Ctrl Pts',(-6.32658964203687,25.1907486868042,
-6.80151366539291));
#454051=CARTESIAN_POINT('Ctrl Pts',(-5.05777230853438,25.11926561611,-6.84002597802966));
#454052=CARTESIAN_POINT('Ctrl Pts',(-4.33782392622387,25.0477825454159,
-5.79453107008661));
#454053=CARTESIAN_POINT('Ctrl Pts',(-4.82635329907546,24.9762994747217,
-4.62289884706407));
#454054=CARTESIAN_POINT('Ctrl Pts',(-6.07577551821105,24.9048164040275,
-4.39856166152736));
#454055=CARTESIAN_POINT('Ctrl Pts',(-6.941387677478,24.8333333333333,-5.32705463942152));
#454056=CARTESIAN_POINT('Ctrl Pts',(-6.63012757162216,24.7618502626391,
-6.55770505428216));
#454057=CARTESIAN_POINT('Ctrl Pts',(-5.42716755876279,24.690367191945,-6.96300807183685));
#454058=CARTESIAN_POINT('Ctrl Pts',(-4.4346429653087,24.6188841212508,-6.17163058503857));
#454059=CARTESIAN_POINT('Ctrl Pts',(-4.56189118942603,24.5474010505566,
-4.90862178076926));
#454060=CARTESIAN_POINT('Ctrl Pts',(-5.69232914266461,24.4759179798625,
-4.33113291369596));
#454061=CARTESIAN_POINT('Ctrl Pts',(-6.7902651507014,24.4044349091683,-4.96825133880203));
#454062=CARTESIAN_POINT('Ctrl Pts',(-6.8497853597109,24.3329518384741,-6.23625792548383));
#454063=CARTESIAN_POINT('Ctrl Pts',(-5.8163581765647,24.2614687677799,-6.97342250511928));
#454064=CARTESIAN_POINT('Ctrl Pts',(-4.63679535172919,24.1899856970857,
-6.50436504145381));
#454065=CARTESIAN_POINT('Ctrl Pts',(-4.39179610102783,24.1185026263916,
-5.25882952309621));
#454066=CARTESIAN_POINT('Ctrl Pts',(-5.30582536167066,24.0470195556974,
-4.37795843727392));
#454067=CARTESIAN_POINT('Ctrl Pts',(-6.54146211713177,23.9755364850032,
-4.66879374102308));
#454068=CARTESIAN_POINT('Ctrl Pts',(-6.96663298362319,23.904053414309,-5.86487613450724));
#454069=CARTESIAN_POINT('Ctrl Pts',(-6.19180228161384,23.8325703436148,
-6.87037140223681));
#454070=CARTESIAN_POINT('Ctrl Pts',(-4.92685920413014,23.7610872729207,
-6.76405862808224));
#454071=CARTESIAN_POINT('Ctrl Pts',(-4.33072722538547,23.6896042022265,
-5.64334011190815));
#454072=CARTESIAN_POINT('Ctrl Pts',(-4.94957415925549,23.6181211315323,
-4.53500272215098));
#454073=CARTESIAN_POINT('Ctrl Pts',(-6.21642115383373,23.5466380608381,
-4.45448991200439));
#454074=CARTESIAN_POINT('Ctrl Pts',(-6.9706000763964,23.475154990144,-5.47556640632124));
#454075=CARTESIAN_POINT('Ctrl Pts',(-6.52114329936776,23.4036719194498,
-6.66273598971973));
#454076=CARTESIAN_POINT('Ctrl Pts',(-5.27983553104633,23.3321888487556,
-6.92833022917403));
#454077=CARTESIAN_POINT('Ctrl Pts',(-4.38394859923605,23.2607057780614,
-6.02901536249358));
#454078=CARTESIAN_POINT('Ctrl Pts',(-4.6542763857934,23.1892227073672,-4.78873124130167));
#454079=CARTESIAN_POINT('Ctrl Pts',(-5.8431588586417,23.1177396366731,-4.34380918016856));
#454080=CARTESIAN_POINT('Ctrl Pts',(-6.86133755596364,23.0462565659789,
-5.1018804774459));
#454081=CARTESIAN_POINT('Ctrl Pts',(-6.77601180031397,22.9747734952847,
-6.36841097734037));
#454082=CARTESIAN_POINT('Ctrl Pts',(-5.66527621173653,22.9032904245905,
-6.98302223994139));
#454083=CARTESIAN_POINT('Ctrl Pts',(-4.54692766144197,22.8318073538963,
-6.3826171450343));
#454084=CARTESIAN_POINT('Ctrl Pts',(-4.4452753183732,22.7603242832022,-5.11727611571493));
#454085=CARTESIAN_POINT('Ctrl Pts',(-5.45405255931454,22.688841212508,-4.34629195893472));
#454086=CARTESIAN_POINT('Ctrl Pts',(-6.64785217518362,22.6173581418138,
-4.77602071980922));
#454087=CARTESIAN_POINT('Ctrl Pts',(-6.93525520080945,22.5458750711197,
-6.01276456633487));
#454088=CARTESIAN_POINT('Ctrl Pts',(-6.04826976192828,22.4743920004254,
-6.92345206015257));
#454089=CARTESIAN_POINT('Ctrl Pts',(-5.22281495825156,22.4267366199627,
-6.75659092854625));
#454090=CARTESIAN_POINT('Ctrl Pts',(-4.93665266667552,22.4029089297313,
-6.5169819168131));
#454091=CARTESIAN_POINT('Ctrl Pts',(-5.58468863860454,26.0970910702687,
-6.86060932929632));
#454092=CARTESIAN_POINT('Ctrl Pts',(-5.18420242845371,26.0732633800373,
-6.83660014748639));
#454093=CARTESIAN_POINT('Ctrl Pts',(-4.41601015327874,26.0256079995746,
-6.35764569349554));
#454094=CARTESIAN_POINT('Ctrl Pts',(-4.39517119822623,25.9541249288803,
-4.99126448034597));
#454095=CARTESIAN_POINT('Ctrl Pts',(-5.53270027843018,25.8826418581862,
-4.23702001084117));
#454096=CARTESIAN_POINT('Ctrl Pts',(-6.78276611783875,25.811158787492,-4.7824753491703));
#454097=CARTESIAN_POINT('Ctrl Pts',(-7.00190159169353,25.7396757167979,
-6.12959649298558));
#454098=CARTESIAN_POINT('Ctrl Pts',(-5.98840954909488,25.6681926461036,
-7.04330603741155));
#454099=CARTESIAN_POINT('Ctrl Pts',(-4.67131052012888,25.5967095754095,
-6.68691572204242));
#454100=CARTESIAN_POINT('Ctrl Pts',(-4.2570712821673,25.5252265047153,-5.38672120534383));
#454101=CARTESIAN_POINT('Ctrl Pts',(-5.12533511911963,25.4537434340211,
-4.33405713849982));
#454102=CARTESIAN_POINT('Ctrl Pts',(-6.48054794122378,25.382260363327,-4.49330153555078));
#454103=CARTESIAN_POINT('Ctrl Pts',(-7.0811144088688,25.3107772926328,-5.71858660500674));
#454104=CARTESIAN_POINT('Ctrl Pts',(-6.37678748673361,25.2392942219386,
-6.88730788058188));
#454105=CARTESIAN_POINT('Ctrl Pts',(-5.01287011686923,25.1678111512444,
-6.92870675713562));
#454106=CARTESIAN_POINT('Ctrl Pts',(-4.23896036791547,25.0963280805502,
-5.80485021183448));
#454107=CARTESIAN_POINT('Ctrl Pts',(-4.76410585554996,25.0248450098561,
-4.54540214324444));
#454108=CARTESIAN_POINT('Ctrl Pts',(-6.10717441394478,24.9533619391619,
-4.30425050070234));
#454109=CARTESIAN_POINT('Ctrl Pts',(-7.03766568988833,24.8818788684677,
-5.302335620529));
#454110=CARTESIAN_POINT('Ctrl Pts',(-6.70307610499455,24.8103957977735,
-6.62522539570715));
#454111=CARTESIAN_POINT('Ctrl Pts',(-5.40995217496277,24.7389127270793,
-7.0609065699037));
#454112=CARTESIAN_POINT('Ctrl Pts',(-4.34303616011549,24.6674296563851,
-6.21021398251267));
#454113=CARTESIAN_POINT('Ctrl Pts',(-4.47982185698087,24.595946585691,-4.85254050111458));
#454114=CARTESIAN_POINT('Ctrl Pts',(-5.69498807457972,24.5244635149968,
-4.23176785251722));
#454115=CARTESIAN_POINT('Ctrl Pts',(-6.87521627041245,24.4529804443027,
-4.91663939684271));
#454116=CARTESIAN_POINT('Ctrl Pts',(-6.93919762122039,24.3814973736084,
-6.27968525302103));
#454117=CARTESIAN_POINT('Ctrl Pts',(-5.82831329739714,24.3100143029143,
-7.07210158283119));
#454118=CARTESIAN_POINT('Ctrl Pts',(-4.5603402147798,24.2385312322201,-6.567887457389));
#454119=CARTESIAN_POINT('Ctrl Pts',(-4.29697784983407,24.1670481615259,
-5.22899691466481));
#454120=CARTESIAN_POINT('Ctrl Pts',(-5.27951517198252,24.0955650908318,
-4.28210302943719));
#454121=CARTESIAN_POINT('Ctrl Pts',(-6.60776502254541,24.0240820201375,
-4.59473693825861));
#454122=CARTESIAN_POINT('Ctrl Pts',(-7.06480317504856,23.9525989494434,
-5.88046775954143));
#454123=CARTESIAN_POINT('Ctrl Pts',(-6.2318975823597,23.8811158787492,-6.96132662295805));
#454124=CARTESIAN_POINT('Ctrl Pts',(-4.87214485065071,23.809632808055,-6.84704552395415));
#454125=CARTESIAN_POINT('Ctrl Pts',(-4.23133175717171,23.7381497373609,
-5.64232723190575));
#454126=CARTESIAN_POINT('Ctrl Pts',(-4.89656233064023,23.6666666666667,
-4.45091805294454));
#454127=CARTESIAN_POINT('Ctrl Pts',(-6.258361681297,23.5951835959725,-4.3643706695222));
#454128=CARTESIAN_POINT('Ctrl Pts',(-7.06906760823243,23.5237005252783,
-5.4619785991953));
#454129=CARTESIAN_POINT('Ctrl Pts',(-6.58592327452408,23.4522174545842,
-6.73812857998267));
#454130=CARTESIAN_POINT('Ctrl Pts',(-5.25157735895588,23.3807343838899,
-7.02362956342815));
#454131=CARTESIAN_POINT('Ctrl Pts',(-4.28854216431714,23.3092513131958,
-6.05690950431861));
#454132=CARTESIAN_POINT('Ctrl Pts',(-4.57913148234355,23.2377682425016,
-4.72366395998878));
#454133=CARTESIAN_POINT('Ctrl Pts',(-5.85712273658419,23.1662851718074,
-4.24539422691366));
#454134=CARTESIAN_POINT('Ctrl Pts',(-6.95161567440516,23.0948021011132,
-5.06028426872769));
#454135=CARTESIAN_POINT('Ctrl Pts',(-6.85989460695557,23.0233190304191,
-6.42174340288106));
#454136=CARTESIAN_POINT('Ctrl Pts',(-5.66590748005734,22.9518359597249,
-7.08242083425081));
#454137=CARTESIAN_POINT('Ctrl Pts',(-4.46373678689788,22.8803528890307,
-6.4370143472206));
#454138=CARTESIAN_POINT('Ctrl Pts',(-4.35446542628666,22.8088698183366,
-5.07683383650299));
#454139=CARTESIAN_POINT('Ctrl Pts',(-5.43885225243895,22.7373867476423,
-4.24806309420865));
#454140=CARTESIAN_POINT('Ctrl Pts',(-6.72212919800733,22.6659036769482,
-4.71000076309996));
#454141=CARTESIAN_POINT('Ctrl Pts',(-7.03107357357049,22.594420606254,-6.03944068310239));
#454142=CARTESIAN_POINT('Ctrl Pts',(-6.07760705403035,22.5229375355598,
-7.01838576726789));
#454143=CARTESIAN_POINT('Ctrl Pts',(-5.19028299638619,22.475282155097,-6.83901810752379));
#454144=CARTESIAN_POINT('Ctrl Pts',(-4.88267235001886,22.4514544648656,
-6.58144998920627));
#454145=CARTESIAN_POINT('Ctrl Pts',(-5.57965686974575,26.1456366054031,
-6.94454197042357));
#454146=CARTESIAN_POINT('Ctrl Pts',(-5.15124649498693,26.1218089151717,
-6.91885873260879));
#454147=CARTESIAN_POINT('Ctrl Pts',(-4.32949150779126,26.0741535347089,
-6.4065088640594));
#454148=CARTESIAN_POINT('Ctrl Pts',(-4.30719954288124,26.0026704640147,
-4.94485582145311));
#454149=CARTESIAN_POINT('Ctrl Pts',(-5.52404358693881,25.9311873933206,
-4.1380211598586));
#454150=CARTESIAN_POINT('Ctrl Pts',(-6.86127108980971,25.8597043226263,
-4.7215087306785));
#454151=CARTESIAN_POINT('Ctrl Pts',(-7.09568592881682,25.7882212519322,
-6.16255878293893));
#454152=CARTESIAN_POINT('Ctrl Pts',(-6.01152748645437,25.716738181238,-7.13997732676548));
#454153=CARTESIAN_POINT('Ctrl Pts',(-4.60259286076204,25.6452551105438,
-6.7587374620765));
#454154=CARTESIAN_POINT('Ctrl Pts',(-4.15947051927595,25.5737720398497,
-5.36788602689621));
#454155=CARTESIAN_POINT('Ctrl Pts',(-5.08827462376231,25.5022889691555,
-4.24182426511434));
#454156=CARTESIAN_POINT('Ctrl Pts',(-6.53798055190634,25.4308058984613,
-4.41217208256641));
#454157=CARTESIAN_POINT('Ctrl Pts',(-7.18042191180854,25.3593228277671,
-5.72289095998872));
#454158=CARTESIAN_POINT('Ctrl Pts',(-6.42698533143036,25.287839757073,-6.97310209577086));
#454159=CARTESIAN_POINT('Ctrl Pts',(-4.96796792520408,25.2163566863788,
-7.01738753624157));
#454160=CARTESIAN_POINT('Ctrl Pts',(-4.14009680960707,25.1448736156846,
-5.81516935358236));
#454161=CARTESIAN_POINT('Ctrl Pts',(-4.70185841202445,25.0733905449904,
-4.46790543942481));
#454162=CARTESIAN_POINT('Ctrl Pts',(-6.1385733096785,25.0019074742962,-4.20993933987732));
#454163=CARTESIAN_POINT('Ctrl Pts',(-7.13394370229866,24.930424403602,-5.27761660163647));
#454164=CARTESIAN_POINT('Ctrl Pts',(-6.77602463836695,24.8589413329079,
-6.69274573713214));
#454165=CARTESIAN_POINT('Ctrl Pts',(-5.39273679116276,24.7874582622137,
-7.15880506797054));
#454166=CARTESIAN_POINT('Ctrl Pts',(-4.25142935492228,24.7159751915195,
-6.24879737998679));
#454167=CARTESIAN_POINT('Ctrl Pts',(-4.39775252453572,24.6444921208253,
-4.79645922145989));
#454168=CARTESIAN_POINT('Ctrl Pts',(-5.69764700649481,24.5730090501312,
-4.13240279133847));
#454169=CARTESIAN_POINT('Ctrl Pts',(-6.9601673901235,24.501525979437,-4.86502745488341));
#454170=CARTESIAN_POINT('Ctrl Pts',(-7.02860988272989,24.4300429087428,
-6.32311258055821));
#454171=CARTESIAN_POINT('Ctrl Pts',(-5.84026841822957,24.3585598380486,
-7.17078066054311));
#454172=CARTESIAN_POINT('Ctrl Pts',(-4.4838850778304,24.2870767673545,-6.63140987332417));
#454173=CARTESIAN_POINT('Ctrl Pts',(-4.2021595986403,24.2155936966603,-5.19916430623342));
#454174=CARTESIAN_POINT('Ctrl Pts',(-5.25320498229437,24.1441106259661,
-4.18624762160045));
#454175=CARTESIAN_POINT('Ctrl Pts',(-6.67406792795906,24.0726275552719,
-4.52068013549415));
#454176=CARTESIAN_POINT('Ctrl Pts',(-7.16297336647392,24.0011444845777,
-5.89605938457563));
#454177=CARTESIAN_POINT('Ctrl Pts',(-6.27199288310558,23.9296614138836,
-7.0522818436793));
#454178=CARTESIAN_POINT('Ctrl Pts',(-4.81743049717126,23.8581783431894,
-6.93003241982605));
#454179=CARTESIAN_POINT('Ctrl Pts',(-4.13193628895796,23.7866952724952,
-5.64131435190337));
#454180=CARTESIAN_POINT('Ctrl Pts',(-4.84355050202496,23.715212201801,-4.3668333837381));
#454181=CARTESIAN_POINT('Ctrl Pts',(-6.30030220876029,23.6437291311069,
-4.27425142704003));
#454182=CARTESIAN_POINT('Ctrl Pts',(-7.16753514006844,23.5722460604127,
-5.44839079206936));
#454183=CARTESIAN_POINT('Ctrl Pts',(-6.65070324968042,23.5007629897185,
-6.81352117024561));
#454184=CARTESIAN_POINT('Ctrl Pts',(-5.22331918686542,23.4292799190243,
-7.11892889768229));
#454185=CARTESIAN_POINT('Ctrl Pts',(-4.19313572939823,23.3577968483302,
-6.08480364614364));
#454186=CARTESIAN_POINT('Ctrl Pts',(-4.50398657889369,23.2863137776359,
-4.65859667867589));
#454187=CARTESIAN_POINT('Ctrl Pts',(-5.8710866145267,23.2148307069418,-4.14697927365876));
#454188=CARTESIAN_POINT('Ctrl Pts',(-7.04189379284668,23.1433476362476,
-5.01868806000948));
#454189=CARTESIAN_POINT('Ctrl Pts',(-6.94377741359719,23.0718645655535,
-6.47507582842176));
#454190=CARTESIAN_POINT('Ctrl Pts',(-5.66653874837813,23.0003814948592,
-7.18181942856023));
#454191=CARTESIAN_POINT('Ctrl Pts',(-4.38054591235379,22.9288984241651,
-6.49141154940691));
#454192=CARTESIAN_POINT('Ctrl Pts',(-4.26365553420012,22.8574153534709,
-5.03639155729104));
#454193=CARTESIAN_POINT('Ctrl Pts',(-5.42365194556336,22.7859322827767,
-4.14983422948258));
#454194=CARTESIAN_POINT('Ctrl Pts',(-6.79640622083105,22.7144492120825,
-4.6439808063907));
#454195=CARTESIAN_POINT('Ctrl Pts',(-7.12689194633153,22.6429661413884,
-6.06611679986992));
#454196=CARTESIAN_POINT('Ctrl Pts',(-6.10694434613243,22.5714830706942,
-7.11331947438321));
#454197=CARTESIAN_POINT('Ctrl Pts',(-5.15775103452081,22.5238276902314,
-6.92144528650133));
#454198=CARTESIAN_POINT('Ctrl Pts',(-4.8286920333622,22.5,-6.64591806159944));
#454199=CARTESIAN_POINT('Ctrl Pts',(-6.39051881327128,25.2730384757729,
-4.92197603118329));
#454200=CARTESIAN_POINT('Ctrl Pts',(-6.34953594825859,25.2770820815347,
-4.8802577415671));
#454201=CARTESIAN_POINT('Ctrl Pts',(-6.3050503566324,25.2811256872965,-4.84215579969382));
#454202=CARTESIAN_POINT('Ctrl Pts',(-6.25744773204304,25.2851692930582,
-4.80845709106527));
#454203=CARTESIAN_POINT('Ctrl Pts',(-5.97694051651721,25.3089969832896,
-4.60988125610326));
#454204=CARTESIAN_POINT('Ctrl Pts',(-5.58819831317574,25.332824673521,-4.56420207068701));
#454205=CARTESIAN_POINT('Ctrl Pts',(-5.26929666119096,25.3566523637524,
-4.69234059080694));
#454206=CARTESIAN_POINT('Ctrl Pts',(-4.95039500920618,25.3804800539838,
-4.82047911092687));
#454207=CARTESIAN_POINT('Ctrl Pts',(-4.70133390857809,25.4043077442152,
-5.12243533658298));
#454208=CARTESIAN_POINT('Ctrl Pts',(-4.6362155300828,25.4281354344466,-5.45989356270023));
#454209=CARTESIAN_POINT('Ctrl Pts',(-4.57109715158752,25.451963124678,-5.79735178881747));
#454210=CARTESIAN_POINT('Ctrl Pts',(-4.68992149522503,25.4757908149094,
-6.17031201539585));
#454211=CARTESIAN_POINT('Ctrl Pts',(-4.93823830629602,25.4996185051408,
-6.40790733147329));
#454212=CARTESIAN_POINT('Ctrl Pts',(-5.186555117367,25.5234461953722,-6.64550264755072));
#454213=CARTESIAN_POINT('Ctrl Pts',(-5.56436439587145,25.5472738856035,
-6.74773305312721));
#454214=CARTESIAN_POINT('Ctrl Pts',(-5.89862890896884,25.5711015758349,
-6.66779966497798));
#454215=CARTESIAN_POINT('Ctrl Pts',(-6.23289342206624,25.5949292660663,
-6.58786627682875));
#454216=CARTESIAN_POINT('Ctrl Pts',(-6.52361316975658,25.6187569562977,
-6.32576909495381));
#454217=CARTESIAN_POINT('Ctrl Pts',(-6.63754358634341,25.6425846465291,
-6.00150994952884));
#454218=CARTESIAN_POINT('Ctrl Pts',(-6.75147400293023,25.6664123367605,
-5.67725080410387));
#454219=CARTESIAN_POINT('Ctrl Pts',(-6.68861508841353,25.6902400269919,
-5.29082969512888));
#454220=CARTESIAN_POINT('Ctrl Pts',(-6.47789521240786,25.7140677172233,
-5.01938732841678));
#454221=CARTESIAN_POINT('Ctrl Pts',(-6.45145094929911,25.7170579700732,
-4.98532270432787));
#454222=CARTESIAN_POINT('Ctrl Pts',(-6.42267802952734,25.720048222923,-4.95306887608107));
#454223=CARTESIAN_POINT('Ctrl Pts',(-6.39190058798136,25.7230384757729,
-4.92276701974739));
#454224=CARTESIAN_POINT('Ctrl Pts',(-5.01302286563431,26.,-4.53900700771688));
#454225=CARTESIAN_POINT('Ctrl Pts',(-5.38492752167559,25.9761723097686,
-4.32480615636363));
#454226=CARTESIAN_POINT('Ctrl Pts',(-6.35301914505848,25.9285169293058,
-4.30067277954968));
#454227=CARTESIAN_POINT('Ctrl Pts',(-7.1756264891545,25.8570338586117,-5.50907794609547));
#454228=CARTESIAN_POINT('Ctrl Pts',(-6.60321033464885,25.7855507879174,
-6.8522203629011));
#454229=CARTESIAN_POINT('Ctrl Pts',(-5.16550356767203,25.7140677172233,
-7.1004834147237));
#454230=CARTESIAN_POINT('Ctrl Pts',(-4.17707919799325,25.6425846465291,
-6.02596364157129));
#454231=CARTESIAN_POINT('Ctrl Pts',(-4.5448553014618,25.5711015758349,-4.61334644908231));
#454232=CARTESIAN_POINT('Ctrl Pts',(-5.93119910857215,25.4996185051408,
-4.15673773385264));
#454233=CARTESIAN_POINT('Ctrl Pts',(-7.0663089114369,25.4281354344466,-5.07453447980768));
#454234=CARTESIAN_POINT('Ctrl Pts',(-6.9100356033464,25.3566523637524,-6.5258341885166));
#454235=CARTESIAN_POINT('Ctrl Pts',(-5.60564496305001,25.2851692930582,
-7.18099123031483));
#454236=CARTESIAN_POINT('Ctrl Pts',(-4.34815567114858,25.213686222364,-6.43975200870338));
#454237=CARTESIAN_POINT('Ctrl Pts',(-4.2896855842815,25.1422031516699,-4.98123363545819));
#454238=CARTESIAN_POINT('Ctrl Pts',(-5.48379221455872,25.0707200809757,
-4.14170854437417));
#454239=CARTESIAN_POINT('Ctrl Pts',(-6.83645762028281,24.9992370102815,
-4.69033908735646));
#454240=CARTESIAN_POINT('Ctrl Pts',(-7.10838527255516,24.9277539395874,
-6.12447699388038));
#454241=CARTESIAN_POINT('Ctrl Pts',(-6.05044038944422,24.8562708688931,
-7.13018513270865));
#454242=CARTESIAN_POINT('Ctrl Pts',(-4.63189669239788,24.784787798199,-6.78604742232836));
#454243=CARTESIAN_POINT('Ctrl Pts',(-4.15240479236239,24.7133047275048,
-5.40735816264999));
#454244=CARTESIAN_POINT('Ctrl Pts',(-5.0512683537124,24.6418216568106,-4.25725342975252));
#454245=CARTESIAN_POINT('Ctrl Pts',(-6.50496106867921,24.5703385861164,
-4.38944335790391));
#454246=CARTESIAN_POINT('Ctrl Pts',(-7.18162963832198,24.4988555154223,
-5.68281734635597));
#454247=CARTESIAN_POINT('Ctrl Pts',(-6.46131966662841,24.4273724447281,
-6.95240396480877));
#454248=CARTESIAN_POINT('Ctrl Pts',(-5.00396921476326,24.3558893740339,
-7.03502543671246));
#454249=CARTESIAN_POINT('Ctrl Pts',(-4.14478270244581,24.2844063033397,
-5.85498510857852));
#454250=CARTESIAN_POINT('Ctrl Pts',(-4.67093497503137,24.2129232326456,
-4.49341967622111));
#454251=CARTESIAN_POINT('Ctrl Pts',(-6.10037256921808,24.1414401619514,
-4.19777663638434));
#454252=CARTESIAN_POINT('Ctrl Pts',(-7.12346444664167,24.0699570912572,
-5.23892007073304));
#454253=CARTESIAN_POINT('Ctrl Pts',(-6.80286792203874,23.998474020563,-6.662968703113));
#454254=CARTESIAN_POINT('Ctrl Pts',(-5.43230911237055,23.9269909498688,
-7.16522879152533));
#454255=CARTESIAN_POINT('Ctrl Pts',(-4.26747512907024,23.8555078791747,
-6.2855365564656));
#454256=CARTESIAN_POINT('Ctrl Pts',(-4.37557081254884,23.7840248084805,
-4.82985391579145));
#454257=CARTESIAN_POINT('Ctrl Pts',(-5.6575604101698,23.7125417377863,-4.13185724083954));
#454258=CARTESIAN_POINT('Ctrl Pts',(-6.93890266242659,23.6410586670921,
-4.83104150205928));
#454259=CARTESIAN_POINT('Ctrl Pts',(-7.04564953674368,23.569575596398,-6.28682364983267));
#454260=CARTESIAN_POINT('Ctrl Pts',(-5.88000083782647,23.4980925257038,
-7.16543624640093));
#454261=CARTESIAN_POINT('Ctrl Pts',(-4.50990820099157,23.4266094550096,
-6.66190630419616));
#454262=CARTESIAN_POINT('Ctrl Pts',(-4.19063094092434,23.3551263843154,
-5.23756146736659));
#454263=CARTESIAN_POINT('Ctrl Pts',(-5.21468783779197,23.2836433136212,
-4.19736598356861));
#454264=CARTESIAN_POINT('Ctrl Pts',(-6.64384941569999,23.2121602429271,
-4.49433434427903));
#454265=CARTESIAN_POINT('Ctrl Pts',(-7.16874271925581,23.1406771722328,
-5.85638486317849));
#454266=CARTESIAN_POINT('Ctrl Pts',(-6.3084575374563,23.0691941015387,-7.03563221165043));
#454267=CARTESIAN_POINT('Ctrl Pts',(-4.85119529970874,22.9977110308445,
-6.95165327175697));
#454268=CARTESIAN_POINT('Ctrl Pts',(-4.13204038713624,22.9262279601503,
-5.68141376558385));
#454269=CARTESIAN_POINT('Ctrl Pts',(-4.80994952176022,22.8547448894562,
-4.38863987327371));
#454270=CARTESIAN_POINT('Ctrl Pts',(-6.26368089065207,22.783261818762,-4.25785081625157));
#454271=CARTESIAN_POINT('Ctrl Pts',(-7.16164157512573,22.7117787480678,
-5.40868234342555));
#454272=CARTESIAN_POINT('Ctrl Pts',(-6.68055232418451,22.6402956773736,
-6.78713386963136));
#454273=CARTESIAN_POINT('Ctrl Pts',(-5.26231872215201,22.5688126066795,
-7.12954990426926));
#454274=CARTESIAN_POINT('Ctrl Pts',(-4.20406666678213,22.4973295359853,
-6.1236699944058));
#454275=CARTESIAN_POINT('Ctrl Pts',(-4.4798333146301,22.4258464652911,-4.68809392709695));
#454276=CARTESIAN_POINT('Ctrl Pts',(-5.37807265034296,22.3781910848283,
-4.32622391325397));
#454277=CARTESIAN_POINT('Ctrl Pts',(-5.80443435631943,22.3543633945969,
-4.37532354240196));
#454278=CARTESIAN_POINT('Ctrl Pts',(-5.05498833669907,26.0485455351344,
-4.61186924884874));
#454279=CARTESIAN_POINT('Ctrl Pts',(-5.40265192052164,26.024717844903,-4.41163019717349));
#454280=CARTESIAN_POINT('Ctrl Pts',(-6.30764248137266,25.9770624644402,
-4.38906985506272));
#454281=CARTESIAN_POINT('Ctrl Pts',(-7.07663155607638,25.905579393746,-5.51871011120511));
#454282=CARTESIAN_POINT('Ctrl Pts',(-6.54152598941931,25.8340963230518,
-6.77430532526158));
#454283=CARTESIAN_POINT('Ctrl Pts',(-5.1975302126156,25.7626132523576,-7.00638637325414));
#454284=CARTESIAN_POINT('Ctrl Pts',(-4.27353221173565,25.6911301816635,
-6.00190474293836));
#454285=CARTESIAN_POINT('Ctrl Pts',(-4.61733634566933,25.6196471109693,
-4.68136318011483));
#454286=CARTESIAN_POINT('Ctrl Pts',(-5.91331704545576,25.5481640402751,
-4.25451662209878));
#454287=CARTESIAN_POINT('Ctrl Pts',(-6.97443939411568,25.4766809695809,
-5.11249056981941));
#454288=CARTESIAN_POINT('Ctrl Pts',(-6.82835211754092,25.4051978988868,
-6.46919328847102));
#454289=CARTESIAN_POINT('Ctrl Pts',(-5.60898280515531,25.3337148281926,
-7.08164661869466));
#454290=CARTESIAN_POINT('Ctrl Pts',(-4.43345777007097,25.2622317574984,
-6.38872202076577));
#454291=CARTESIAN_POINT('Ctrl Pts',(-4.37879881483497,25.1907486868042,
-5.02527115647435));
#454292=CARTESIAN_POINT('Ctrl Pts',(-5.49507252586477,25.1192656161101,
-4.24046704839444));
#454293=CARTESIAN_POINT('Ctrl Pts',(-6.75957001205557,25.0477825454159,
-4.75333737058418));
#454294=CARTESIAN_POINT('Ctrl Pts',(-7.01377318104995,24.9762994747217,
-6.09399690839473));
#454295=CARTESIAN_POINT('Ctrl Pts',(-6.0247860748808,24.9048164040275,-7.03415210716631));
#454296=CARTESIAN_POINT('Ctrl Pts',(-4.69870430227373,24.8333333333333,
-6.71244559509181));
#454297=CARTESIAN_POINT('Ctrl Pts',(-4.25046610554157,24.7618502626392,
-5.42362051261083));
#454298=CARTESIAN_POINT('Ctrl Pts',(-5.09074095026355,24.690367191945,-4.34848061663153));
#454299=CARTESIAN_POINT('Ctrl Pts',(-6.44968069692276,24.6188841212508,
-4.47205428913018));
#454300=CARTESIAN_POINT('Ctrl Pts',(-7.08224341470705,24.5474010505566,
-5.68112502471735));
#454301=CARTESIAN_POINT('Ctrl Pts',(-6.40888387979891,24.4759179798625,
-6.86795887198031));
#454302=CARTESIAN_POINT('Ctrl Pts',(-5.04652481074592,24.4044349091682,
-6.94519500375798));
#454303=CARTESIAN_POINT('Ctrl Pts',(-4.24334083014217,24.3329518384741,
-5.84207074093974));
#454304=CARTESIAN_POINT('Ctrl Pts',(-4.73519803534797,24.2614687677799,
-4.56925333967074));
#454305=CARTESIAN_POINT('Ctrl Pts',(-6.07146363130893,24.1899856970857,
-4.29288057290861));
#454306=CARTESIAN_POINT('Ctrl Pts',(-7.02786948132165,24.1185026263916,
-5.2661613635068));
#454307=CARTESIAN_POINT('Ctrl Pts',(-6.72816971985337,24.0470195556973,
-6.59738925492608));
#454308=CARTESIAN_POINT('Ctrl Pts',(-5.44694513750787,23.9755364850032,
-7.0669115895136));
#454309=CARTESIAN_POINT('Ctrl Pts',(-4.35803605660742,23.904053414309,-6.24455846719129));
#454310=CARTESIAN_POINT('Ctrl Pts',(-4.45908596846911,23.8325703436148,
-4.8837584999306));
#454311=CARTESIAN_POINT('Ctrl Pts',(-5.65751435782136,23.7610872729207,
-4.2312578614791));
#454312=CARTESIAN_POINT('Ctrl Pts',(-6.85533759634902,23.6896042022265,
-4.88486867828213));
#454313=CARTESIAN_POINT('Ctrl Pts',(-6.95512661561532,23.6181211315323,
-6.24576166668191));
#454314=CARTESIAN_POINT('Ctrl Pts',(-5.86545592297769,23.5466380608381,
-7.06710552229815));
#454315=CARTESIAN_POINT('Ctrl Pts',(-4.58466712791061,23.475154990144,-6.59639610410402));
#454316=CARTESIAN_POINT('Ctrl Pts',(-4.28620064015658,23.4036719194498,
-5.26489131510138));
#454317=CARTESIAN_POINT('Ctrl Pts',(-5.24350860879812,23.3321888487556,
-4.2924966868042));
#454318=CARTESIAN_POINT('Ctrl Pts',(-6.57951617946397,23.2607057780614,
-4.57010838886106));
#454319=CARTESIAN_POINT('Ctrl Pts',(-7.07019647634743,23.1892227073672,
-5.84337925830513));
#454320=CARTESIAN_POINT('Ctrl Pts',(-6.26598543850373,23.1177396366731,
-6.94576222857241));
#454321=CARTESIAN_POINT('Ctrl Pts',(-4.90370883369462,23.0462565659789,
-6.86725710976114));
#454322=CARTESIAN_POINT('Ctrl Pts',(-4.23142907013928,22.9747734952847,
-5.67981293057309));
#454323=CARTESIAN_POINT('Ctrl Pts',(-4.86515149178938,22.9032904245905,
-4.47130317633407));
#454324=CARTESIAN_POINT('Ctrl Pts',(-6.22412737287685,22.8318073538963,
-4.34903906495375));
#454325=CARTESIAN_POINT('Ctrl Pts',(-7.06355819103049,22.7603242832022,
-5.42485838212006));
#454326=CARTESIAN_POINT('Ctrl Pts',(-6.613826760128,22.688841212508,-6.7134612268051));
#454327=CARTESIAN_POINT('Ctrl Pts',(-5.28803487026933,22.6173581418138,
-7.03355828347467));
#454328=CARTESIAN_POINT('Ctrl Pts',(-4.29876061359894,22.5458750711196,
-6.0932425098549));
#454329=CARTESIAN_POINT('Ctrl Pts',(-4.55655254906459,22.4743920004255,
-4.75123855184285));
#454330=CARTESIAN_POINT('Ctrl Pts',(-5.39624385572484,22.4267366199627,
-4.41295554342414));
#454331=CARTESIAN_POINT('Ctrl Pts',(-5.79481493112442,22.4029089297313,
-4.45885481560764));
#454332=CARTESIAN_POINT('Ctrl Pts',(-5.09695380776383,26.0970910702687,
-4.6847314899806));
#454333=CARTESIAN_POINT('Ctrl Pts',(-5.42037631936769,26.0732633800373,
-4.49845423798335));
#454334=CARTESIAN_POINT('Ctrl Pts',(-6.26226581768684,26.0256079995745,
-4.47746693057576));
#454335=CARTESIAN_POINT('Ctrl Pts',(-6.97763662299825,25.9541249288804,
-5.52834227631475));
#454336=CARTESIAN_POINT('Ctrl Pts',(-6.47984164418979,25.8826418581862,
-6.69639028762207));
#454337=CARTESIAN_POINT('Ctrl Pts',(-5.22955685755916,25.811158787492,-6.91228933178459));
#454338=CARTESIAN_POINT('Ctrl Pts',(-4.36998522547805,25.7396757167978,
-5.97784584430541));
#454339=CARTESIAN_POINT('Ctrl Pts',(-4.68981738987686,25.6681926461037,
-4.74937991114735));
#454340=CARTESIAN_POINT('Ctrl Pts',(-5.89543498233936,25.5967095754095,
-4.35229551034492));
#454341=CARTESIAN_POINT('Ctrl Pts',(-6.88256987679449,25.5252265047153,
-5.15044665983114));
#454342=CARTESIAN_POINT('Ctrl Pts',(-6.74666863173542,25.4537434340211,
-6.41255238842542));
#454343=CARTESIAN_POINT('Ctrl Pts',(-5.61232064726062,25.3822603633269,
-6.9823020070745));
#454344=CARTESIAN_POINT('Ctrl Pts',(-4.51875986899335,25.3107772926328,
-6.33769203282816));
#454345=CARTESIAN_POINT('Ctrl Pts',(-4.46791204538843,25.2392942219386,
-5.06930867749052));
#454346=CARTESIAN_POINT('Ctrl Pts',(-5.50635283717082,25.1678111512444,
-4.33922555241473));
#454347=CARTESIAN_POINT('Ctrl Pts',(-6.68268240382832,25.0963280805502,
-4.81633565381187));
#454348=CARTESIAN_POINT('Ctrl Pts',(-6.91916108954474,25.0248450098561,
-6.06351682290909));
#454349=CARTESIAN_POINT('Ctrl Pts',(-5.99913176031739,24.9533619391618,
-6.93811908162396));
#454350=CARTESIAN_POINT('Ctrl Pts',(-4.76551191214956,24.8818788684677,
-6.63884376785526));
#454351=CARTESIAN_POINT('Ctrl Pts',(-4.34852741872077,24.8103957977735,
-5.43988286257166));
#454352=CARTESIAN_POINT('Ctrl Pts',(-5.13021354681468,24.7389127270794,
-4.43970780351055));
#454353=CARTESIAN_POINT('Ctrl Pts',(-6.39440032516632,24.6674296563851,
-4.55466522035644));
#454354=CARTESIAN_POINT('Ctrl Pts',(-6.98285719109209,24.595946585691,-5.67943270307874));
#454355=CARTESIAN_POINT('Ctrl Pts',(-6.35644809296943,24.5244635149968,
-6.78351377915186));
#454356=CARTESIAN_POINT('Ctrl Pts',(-5.08908040672856,24.4529804443026,
-6.85536457080349));
#454357=CARTESIAN_POINT('Ctrl Pts',(-4.34189895783853,24.3814973736085,
-5.82915637330097));
#454358=CARTESIAN_POINT('Ctrl Pts',(-4.79946109566455,24.3100143029142,
-4.64508700312038));
#454359=CARTESIAN_POINT('Ctrl Pts',(-6.04255469339979,24.2385312322201,
-4.38798450943288));
#454360=CARTESIAN_POINT('Ctrl Pts',(-6.93227451600163,24.1670481615259,
-5.29340265628057));
#454361=CARTESIAN_POINT('Ctrl Pts',(-6.653471517668,24.0955650908317,-6.53180980673916));
#454362=CARTESIAN_POINT('Ctrl Pts',(-5.46158116264518,24.0240820201376,
-6.96859438750187));
#454363=CARTESIAN_POINT('Ctrl Pts',(-4.44859698414461,23.9525989494434,
-6.20358037791699));
#454364=CARTESIAN_POINT('Ctrl Pts',(-4.54260112438938,23.8811158787492,
-4.93766308406974));
#454365=CARTESIAN_POINT('Ctrl Pts',(-5.65746830547292,23.809632808055,-4.33065848211866));
#454366=CARTESIAN_POINT('Ctrl Pts',(-6.77177253027144,23.7381497373608,
-4.93869585450499));
#454367=CARTESIAN_POINT('Ctrl Pts',(-6.86460369448698,23.6666666666667,
-6.20469968353115));
#454368=CARTESIAN_POINT('Ctrl Pts',(-5.85091100812889,23.5951835959725,
-6.96877479819537));
#454369=CARTESIAN_POINT('Ctrl Pts',(-4.65942605482967,23.5237005252783,
-6.53088590401188));
#454370=CARTESIAN_POINT('Ctrl Pts',(-4.3817703393888,23.4522174545841,-5.29222116283617));
#454371=CARTESIAN_POINT('Ctrl Pts',(-5.27232937980428,23.38073438389,-4.38762739003978));
#454372=CARTESIAN_POINT('Ctrl Pts',(-6.51518294322794,23.3092513131958,
-4.6458824334431));
#454373=CARTESIAN_POINT('Ctrl Pts',(-6.97165023343906,23.2377682425016,
-5.83037365343178));
#454374=CARTESIAN_POINT('Ctrl Pts',(-6.22351333955115,23.1662851718074,
-6.85589224549438));
#454375=CARTESIAN_POINT('Ctrl Pts',(-4.9562223676805,23.0948021011132,-6.78286094776533));
#454376=CARTESIAN_POINT('Ctrl Pts',(-4.33081775314232,23.0233190304191,
-5.67821209556232));
#454377=CARTESIAN_POINT('Ctrl Pts',(-4.92035346181854,22.9518359597249,
-4.55396647939442));
#454378=CARTESIAN_POINT('Ctrl Pts',(-6.18457385510163,22.8803528890307,
-4.44022731365593));
#454379=CARTESIAN_POINT('Ctrl Pts',(-6.96547480693525,22.8088698183366,
-5.44103442081458));
#454380=CARTESIAN_POINT('Ctrl Pts',(-6.54710119607151,22.7373867476423,
-6.63978858397884));
#454381=CARTESIAN_POINT('Ctrl Pts',(-5.31375101838665,22.6659036769482,
-6.93756666268009));
#454382=CARTESIAN_POINT('Ctrl Pts',(-4.39345456041576,22.594420606254,-6.062815025304));
#454383=CARTESIAN_POINT('Ctrl Pts',(-4.63327178349906,22.5229375355598,
-4.81438317658877));
#454384=CARTESIAN_POINT('Ctrl Pts',(-5.41441506110672,22.475282155097,-4.49968717359432));
#454385=CARTESIAN_POINT('Ctrl Pts',(-5.78519550592941,22.4514544648656,
-4.54238608881333));
#454386=CARTESIAN_POINT('Ctrl Pts',(-5.13891927882859,26.1456366054031,
-4.75759373111246));
#454387=CARTESIAN_POINT('Ctrl Pts',(-5.43810071821374,26.1218089151717,
-4.58527827879321));
#454388=CARTESIAN_POINT('Ctrl Pts',(-6.21688915400102,26.0741535347089,
-4.5658640060888));
#454389=CARTESIAN_POINT('Ctrl Pts',(-6.87864168992013,26.0026704640147,
-5.53797444142439));
#454390=CARTESIAN_POINT('Ctrl Pts',(-6.41815729896024,25.9311873933205,
-6.61847524998255));
#454391=CARTESIAN_POINT('Ctrl Pts',(-5.26158350250274,25.8597043226264,
-6.81819229031504));
#454392=CARTESIAN_POINT('Ctrl Pts',(-4.46643823922044,25.7882212519322,
-5.95378694567247));
#454393=CARTESIAN_POINT('Ctrl Pts',(-4.7622984340844,25.716738181238,-4.81739664217988));
#454394=CARTESIAN_POINT('Ctrl Pts',(-5.87755291922296,25.6452551105439,
-4.45007439859105));
#454395=CARTESIAN_POINT('Ctrl Pts',(-6.79070035947327,25.5737720398496,
-5.18840274984286));
#454396=CARTESIAN_POINT('Ctrl Pts',(-6.66498514592993,25.5022889691555,
-6.35591148837984));
#454397=CARTESIAN_POINT('Ctrl Pts',(-5.61565848936591,25.4308058984613,
-6.88295739545433));
#454398=CARTESIAN_POINT('Ctrl Pts',(-4.60406196791575,25.3593228277671,
-6.28666204489055));
#454399=CARTESIAN_POINT('Ctrl Pts',(-4.55702527594187,25.2878397570729,
-5.11334619850668));
#454400=CARTESIAN_POINT('Ctrl Pts',(-5.51763314847689,25.2163566863788,
-4.43798405643501));
#454401=CARTESIAN_POINT('Ctrl Pts',(-6.60579479560106,25.1448736156846,
-4.87933393703958));
#454402=CARTESIAN_POINT('Ctrl Pts',(-6.82454899803953,25.0733905449905,
-6.03303673742344));
#454403=CARTESIAN_POINT('Ctrl Pts',(-5.97347744575397,25.0019074742962,
-6.84208605608162));
#454404=CARTESIAN_POINT('Ctrl Pts',(-4.83231952202541,24.9304244036021,
-6.56524194061871));
#454405=CARTESIAN_POINT('Ctrl Pts',(-4.44658873189996,24.8589413329078,
-5.45614521253248));
#454406=CARTESIAN_POINT('Ctrl Pts',(-5.16968614336583,24.7874582622137,
-4.53093499038958));
#454407=CARTESIAN_POINT('Ctrl Pts',(-6.33911995340987,24.7159751915195,
-4.63727615158268));
#454408=CARTESIAN_POINT('Ctrl Pts',(-6.88347096747714,24.6444921208254,
-5.67774038144015));
#454409=CARTESIAN_POINT('Ctrl Pts',(-6.30401230613993,24.5730090501312,
-6.69906868632339));
#454410=CARTESIAN_POINT('Ctrl Pts',(-5.1316360027112,24.501525979437,-6.76553413784902));
#454411=CARTESIAN_POINT('Ctrl Pts',(-4.4404570855349,24.4300429087428,-5.8162420056622));
#454412=CARTESIAN_POINT('Ctrl Pts',(-4.86372415598114,24.3585598380486,
-4.72092066657002));
#454413=CARTESIAN_POINT('Ctrl Pts',(-6.01364575549065,24.2870767673545,
-4.48308844595715));
#454414=CARTESIAN_POINT('Ctrl Pts',(-6.83667955068161,24.2155936966602,
-5.32064394905434));
#454415=CARTESIAN_POINT('Ctrl Pts',(-6.57877331548262,24.1441106259661,
-6.46623035855224));
#454416=CARTESIAN_POINT('Ctrl Pts',(-5.4762171877825,24.0726275552719,-6.87027718549015));
#454417=CARTESIAN_POINT('Ctrl Pts',(-4.5391579116818,24.0011444845778,-6.16260228864267));
#454418=CARTESIAN_POINT('Ctrl Pts',(-4.62611628030964,23.9296614138835,
-4.99156766820889));
#454419=CARTESIAN_POINT('Ctrl Pts',(-5.65742225312448,23.8581783431894,
-4.43005910275823));
#454420=CARTESIAN_POINT('Ctrl Pts',(-6.68820746419386,23.7866952724952,
-4.99252303072782));
#454421=CARTESIAN_POINT('Ctrl Pts',(-6.77408077335862,23.715212201801,-6.16363770038041));
#454422=CARTESIAN_POINT('Ctrl Pts',(-5.83636609328009,23.6437291311068,
-6.87044407409259));
#454423=CARTESIAN_POINT('Ctrl Pts',(-4.73418498174874,23.5722460604127,
-6.46537570391973));
#454424=CARTESIAN_POINT('Ctrl Pts',(-4.47734003862102,23.5007629897185,
-5.31955101057097));
#454425=CARTESIAN_POINT('Ctrl Pts',(-5.30115015081045,23.4292799190243,
-4.48275809327536));
#454426=CARTESIAN_POINT('Ctrl Pts',(-6.4508497069919,23.3577968483301,-4.72165647802515));
#454427=CARTESIAN_POINT('Ctrl Pts',(-6.8731039905307,23.286313777636,-5.81736804855842));
#454428=CARTESIAN_POINT('Ctrl Pts',(-6.18104124059857,23.2148307069418,
-6.76602226241636));
#454429=CARTESIAN_POINT('Ctrl Pts',(-5.00873590166638,23.1433476362476,
-6.69846478576951));
#454430=CARTESIAN_POINT('Ctrl Pts',(-4.43020643614536,23.0718645655534,
-5.67661126055156));
#454431=CARTESIAN_POINT('Ctrl Pts',(-4.97555543184771,23.0003814948593,
-4.63662978245479));
#454432=CARTESIAN_POINT('Ctrl Pts',(-6.1450203373264,22.9288984241651,-4.5314155623581));
#454433=CARTESIAN_POINT('Ctrl Pts',(-6.86739142284001,22.8574153534709,
-5.45721045950911));
#454434=CARTESIAN_POINT('Ctrl Pts',(-6.48037563201499,22.7859322827767,
-6.56611594115257));
#454435=CARTESIAN_POINT('Ctrl Pts',(-5.33946716650399,22.7144492120825,
-6.84157504188551));
#454436=CARTESIAN_POINT('Ctrl Pts',(-4.48814850723257,22.6429661413884,
-6.0323875407531));
#454437=CARTESIAN_POINT('Ctrl Pts',(-4.70999101793355,22.5714830706942,
-4.87752780133468));
#454438=CARTESIAN_POINT('Ctrl Pts',(-5.4325862664886,22.5238276902314,-4.58641880376449));
#454439=CARTESIAN_POINT('Ctrl Pts',(-5.7755760807344,22.5,-4.62591736201901));
#454440=CARTESIAN_POINT('Ctrl Pts',(-6.39006796800885,25.6019615242271,
-4.92443355077908));
#454441=CARTESIAN_POINT('Ctrl Pts',(-6.48712194011206,25.5925650294346,
-5.02053320993752));
#454442=CARTESIAN_POINT('Ctrl Pts',(-6.56580235206401,25.5831685346421,
-5.13467106978717));
#454443=CARTESIAN_POINT('Ctrl Pts',(-6.617556583841,25.5737720398497,-5.25993281439039));
#454444=CARTESIAN_POINT('Ctrl Pts',(-6.74879528829216,25.5499443496183,
-5.57757232935518));
#454445=CARTESIAN_POINT('Ctrl Pts',(-6.70689021711105,25.5261166593869,
-5.96674190886751));
#454446=CARTESIAN_POINT('Ctrl Pts',(-6.51104990542648,25.5022889691555,
-6.24916768313609));
#454447=CARTESIAN_POINT('Ctrl Pts',(-6.31520959374192,25.4784612789241,
-6.53159345740467));
#454448=CARTESIAN_POINT('Ctrl Pts',(-5.96543404155392,25.4546335886927,
-6.7072754264295));
#454449=CARTESIAN_POINT('Ctrl Pts',(-5.62194684521822,25.4308058984613,
-6.69573385251462));
#454450=CARTESIAN_POINT('Ctrl Pts',(-5.27845964888252,25.4069782082299,
-6.68419227859974));
#454451=CARTESIAN_POINT('Ctrl Pts',(-4.94126080839914,25.3831505179985,
-6.48542716174514));
#454452=CARTESIAN_POINT('Ctrl Pts',(-4.76482193949513,25.3593228277671,
-6.19049196225387));
#454453=CARTESIAN_POINT('Ctrl Pts',(-4.58838307059113,25.3354951375357,
-5.89555676276259));
#454454=CARTESIAN_POINT('Ctrl Pts',(-4.5727041732665,25.3116674473043,-5.50445148063464));
#454455=CARTESIAN_POINT('Ctrl Pts',(-4.72496603669335,25.2878397570729,
-5.19633848255872));
#454456=CARTESIAN_POINT('Ctrl Pts',(-4.87722790012021,25.2640120668416,
-4.8882254844828));
#454457=CARTESIAN_POINT('Ctrl Pts',(-5.19743052429855,25.2401843766102,
-4.6631047704589));
#454458=CARTESIAN_POINT('Ctrl Pts',(-5.53889211090841,25.2163566863788,
-4.62410272688105));
#454459=CARTESIAN_POINT('Ctrl Pts',(-5.84649605160076,25.1948916323282,
-4.58896793348097));
#454460=CARTESIAN_POINT('Ctrl Pts',(-6.17135209942283,25.1734265782776,
-4.70487246063661));
#454461=CARTESIAN_POINT('Ctrl Pts',(-6.39198798715976,25.1519615242271,
-4.92254817630007));
#454462=CARTESIAN_POINT('Origin',(-5.65685387860012,26.,-5.65685387860011));
#454463=CARTESIAN_POINT('Origin',(5.65685387860011,26.993675081176,-5.65685387860012));
#454464=CARTESIAN_POINT('Ctrl Pts',(4.74432962138981,25.868675081176,-6.57057130100612));
#454465=CARTESIAN_POINT('Ctrl Pts',(4.78199706987976,25.8656848283261,-6.60882993708831));
#454466=CARTESIAN_POINT('Ctrl Pts',(5.14157728587623,25.8388668852448,-6.92960341635463));
#454467=CARTESIAN_POINT('Ctrl Pts',(6.16255878293893,25.7882212519322,-7.09568592881682));
#454468=CARTESIAN_POINT('Ctrl Pts',(7.13997732676548,25.716738181238,-6.01152748645437));
#454469=CARTESIAN_POINT('Ctrl Pts',(6.7587374620765,25.6452551105438,-4.60259286076204));
#454470=CARTESIAN_POINT('Ctrl Pts',(5.36788602689621,25.5737720398497,-4.15947051927595));
#454471=CARTESIAN_POINT('Ctrl Pts',(4.24182426511434,25.5022889691555,-5.08827462376231));
#454472=CARTESIAN_POINT('Ctrl Pts',(4.36502559631504,25.450589982931,-6.13675122222029));
#454473=CARTESIAN_POINT('Ctrl Pts',(4.69148744470697,25.4227186869378,-6.51790892062316));
#454474=CARTESIAN_POINT('Ctrl Pts',(4.74334636410459,25.418675081176,-6.56885365284802));
#454475=CARTESIAN_POINT('Ctrl Pts',(4.74450601134849,25.906324918824,-6.56704169373441));
#454476=CARTESIAN_POINT('Ctrl Pts',(4.95573944791419,25.8898945654199,-6.7750658664325));
#454477=CARTESIAN_POINT('Ctrl Pts',(5.64807137163848,25.8496365217844,-7.11639071403833));
#454478=CARTESIAN_POINT('Ctrl Pts',(6.8522203629011,25.7855507879174,-6.60321033464885));
#454479=CARTESIAN_POINT('Ctrl Pts',(7.1004834147237,25.7140677172233,-5.16550356767203));
#454480=CARTESIAN_POINT('Ctrl Pts',(6.02596364157129,25.6425846465291,-4.17707919799325));
#454481=CARTESIAN_POINT('Ctrl Pts',(4.61334644908231,25.5711015758349,-4.5448553014618));
#454482=CARTESIAN_POINT('Ctrl Pts',(4.21675923787011,25.5090149999332,-5.74896333949311));
#454483=CARTESIAN_POINT('Ctrl Pts',(4.5629353888518,25.4707561142629,-6.3830054663296));
#454484=CARTESIAN_POINT('Ctrl Pts',(4.74640124271564,25.456324918824,-6.56829321884323));
#454485=CARTESIAN_POINT('Ctrl Pts',(6.69274404704181,26.,-5.59475217632212));
#454486=CARTESIAN_POINT('Ctrl Pts',(6.67208297724159,25.9761723097686,-5.25011429538726));
#454487=CARTESIAN_POINT('Ctrl Pts',(6.25991935236784,25.9285169293058,-4.58904744425369));
#454488=CARTESIAN_POINT('Ctrl Pts',(5.08408179813166,25.8570338586116,-4.5711145089162));
#454489=CARTESIAN_POINT('Ctrl Pts',(4.43501771280631,25.7855507879175,-5.55001366141289));
#454490=CARTESIAN_POINT('Ctrl Pts',(4.90440858615388,25.7140677172233,-6.62575617389683));
#454491=CARTESIAN_POINT('Ctrl Pts',(6.06367191307887,25.6425846465291,-6.81433291744693));
#454492=CARTESIAN_POINT('Ctrl Pts',(6.84996345870369,25.5711015758349,-5.94217367437589));
#454493=CARTESIAN_POINT('Ctrl Pts',(6.54327224197424,25.4996185051408,-4.80874583886255));
#454494=CARTESIAN_POINT('Ctrl Pts',(5.42439156223908,25.4281354344466,-4.45227280795));
#454495=CARTESIAN_POINT('Ctrl Pts',(4.51852288527077,25.3566523637524,-5.19945610983427));
#454496=CARTESIAN_POINT('Ctrl Pts',(4.65556044151951,25.2851692930583,-6.36568271985867));
#454497=CARTESIAN_POINT('Ctrl Pts',(5.70997789504277,25.213686222364,-6.88249940298929));
#454498=CARTESIAN_POINT('Ctrl Pts',(6.71571945020394,25.1422031516699,-6.27639179734011));
#454499=CARTESIAN_POINT('Ctrl Pts',(6.7513451989237,25.0707200809757,-5.10267450019954));
#454500=CARTESIAN_POINT('Ctrl Pts',(5.78421192833873,24.9992370102815,-4.43668748453226));
#454501=CARTESIAN_POINT('Ctrl Pts',(4.7003955508837,24.9277539395873,-4.88860074260098));
#454502=CARTESIAN_POINT('Ctrl Pts',(4.49287282235238,24.8562708688931,-6.04437662247731));
#454503=CARTESIAN_POINT('Ctrl Pts',(5.35177365831405,24.784787798199,-6.84510966506768));
#454504=CARTESIAN_POINT('Ctrl Pts',(6.49018471285718,24.7133047275048,-6.55717903824976));
#454505=CARTESIAN_POINT('Ctrl Pts',(6.86510957377,24.6418216568106,-5.44438294256282));
#454506=CARTESIAN_POINT('Ctrl Pts',(6.13304718756448,24.5703385861164,-4.52624977050191));
#454507=CARTESIAN_POINT('Ctrl Pts',(4.96470306042393,24.4988555154223,-4.64396052187118));
#454508=CARTESIAN_POINT('Ctrl Pts',(4.43049797487471,24.4273724447281,-5.68967021074952));
#454509=CARTESIAN_POINT('Ctrl Pts',(5.01986328076133,24.3558893740339,-6.70531403099034));
#454510=CARTESIAN_POINT('Ctrl Pts',(6.19283059794665,24.2844063033397,-6.76037309820141));
#454511=CARTESIAN_POINT('Ctrl Pts',(6.87474342740734,24.2129232326455,-5.80440305573226));
#454512=CARTESIAN_POINT('Ctrl Pts',(6.44084262551865,24.1414401619514,-4.71325048867858));
#454513=CARTESIAN_POINT('Ctrl Pts',(5.28866213152759,24.0699570912572,-4.4866143522216));
#454514=CARTESIAN_POINT('Ctrl Pts',(4.47381384511066,23.9984740205631,-5.3321355513588));
#454515=CARTESIAN_POINT('Ctrl Pts',(4.74285054378755,23.9269909498688,-6.47515921171814));
#454516=CARTESIAN_POINT('Ctrl Pts',(5.84928450947304,23.8555078791747,-6.86846279219781));
#454517=CARTESIAN_POINT('Ctrl Pts',(6.77941618151556,23.7840248084805,-6.15170698086798));
#454518=CARTESIAN_POINT('Ctrl Pts',(6.68107173221035,23.7125417377863,-4.98157355760958));
#454519=CARTESIAN_POINT('Ctrl Pts',(5.64435299191054,23.6410586670921,-4.43012269359923));
#454520=CARTESIAN_POINT('Ctrl Pts',(4.61908739135743,23.569575596398,-5.00258598787076));
#454521=CARTESIAN_POINT('Ctrl Pts',(4.54460915448657,23.4980925257038,-6.17448062637044));
#454522=CARTESIAN_POINT('Ctrl Pts',(5.48915421344718,23.4266094550096,-6.87213254456039));
#454523=CARTESIAN_POINT('Ctrl Pts',(6.58734339945679,23.3551263843154,-6.45636332421143));
#454524=CARTESIAN_POINT('Ctrl Pts',(6.8330308949199,23.2836433136213,-5.30809370313679));
#454525=CARTESIAN_POINT('Ctrl Pts',(6.00112122066856,23.212160242927,-4.47935503415497));
#454526=CARTESIAN_POINT('Ctrl Pts',(4.85379852261455,23.1406771722329,-4.72942128924326));
#454527=CARTESIAN_POINT('Ctrl Pts',(4.44222413342346,23.0691941015387,-5.82919498069919));
#454528=CARTESIAN_POINT('Ctrl Pts',(5.14347668616412,22.9977110308445,-6.77105943752212));
#454529=CARTESIAN_POINT('Ctrl Pts',(6.31507855179967,22.9262279601504,-6.69212899367236));
#454530=CARTESIAN_POINT('Ctrl Pts',(6.88362364563197,22.8547448894562,-5.66464494341573));
#454531=CARTESIAN_POINT('Ctrl Pts',(6.32821994284799,22.783261818762,-4.63011853598606));
#454532=CARTESIAN_POINT('Ctrl Pts',(5.15771839492686,22.7117787480678,-4.53608521045973));
#454533=CARTESIAN_POINT('Ctrl Pts',(4.44452082366079,22.6402956773736,-5.46925286619013));
#454534=CARTESIAN_POINT('Ctrl Pts',(4.84204067651847,22.5688126066795,-6.57357515235991));
#454535=CARTESIAN_POINT('Ctrl Pts',(5.98608844956735,22.4973295359852,-6.8394368280484));
#454536=CARTESIAN_POINT('Ctrl Pts',(6.82851835303725,22.4258464652911,-6.01893246982621));
#454537=CARTESIAN_POINT('Ctrl Pts',(6.67416374956871,22.3781910848283,-5.25534692011694));
#454538=CARTESIAN_POINT('Ctrl Pts',(6.45251384441992,22.3543633945969,-4.99063298333217));
#454539=CARTESIAN_POINT('Ctrl Pts',(6.77667668816906,26.0485455351344,-5.58972040746333));
#454540=CARTESIAN_POINT('Ctrl Pts',(6.75434156236399,26.024717844903,-5.21715836192049));
#454541=CARTESIAN_POINT('Ctrl Pts',(6.30878252293169,25.9770624644402,-4.50252879876621));
#454542=CARTESIAN_POINT('Ctrl Pts',(5.03767313923882,25.905579393746,-4.48314285357121));
#454543=CARTESIAN_POINT('Ctrl Pts',(4.33601886182374,25.8340963230518,-5.54135696992153));
#454544=CARTESIAN_POINT('Ctrl Pts',(4.84344196766208,25.7626132523576,-6.70426114586779));
#454545=CARTESIAN_POINT('Ctrl Pts',(6.09663420303223,25.6911301816635,-6.90811725457023));
#454546=CARTESIAN_POINT('Ctrl Pts',(6.94663474805762,25.6196471109693,-5.96529161173539));
#454547=CARTESIAN_POINT('Ctrl Pts',(6.61509398200833,25.5481640402751,-4.74002817949571));
#454548=CARTESIAN_POINT('Ctrl Pts',(5.40555638379146,25.4766809695809,-4.35467204505865));
#454549=CARTESIAN_POINT('Ctrl Pts',(4.42629001188529,25.4051978988867,-5.16239561447694));
#454550=CARTESIAN_POINT('Ctrl Pts',(4.57443098853514,25.3337148281926,-6.42311533054124));
#454551=CARTESIAN_POINT('Ctrl Pts',(5.71428225002476,25.2622317574984,-6.98180690592904));
#454552=CARTESIAN_POINT('Ctrl Pts',(6.80151366539291,25.1907486868042,-6.32658964203687));
#454553=CARTESIAN_POINT('Ctrl Pts',(6.84002597802966,25.11926561611,-5.05777230853438));
#454554=CARTESIAN_POINT('Ctrl Pts',(5.79453107008661,25.0477825454159,-4.33782392622387));
#454555=CARTESIAN_POINT('Ctrl Pts',(4.62289884706407,24.9762994747217,-4.82635329907546));
#454556=CARTESIAN_POINT('Ctrl Pts',(4.39856166152736,24.9048164040275,-6.07577551821105));
#454557=CARTESIAN_POINT('Ctrl Pts',(5.32705463942152,24.8333333333333,-6.941387677478));
#454558=CARTESIAN_POINT('Ctrl Pts',(6.55770505428216,24.7618502626391,-6.63012757162216));
#454559=CARTESIAN_POINT('Ctrl Pts',(6.96300807183685,24.690367191945,-5.42716755876279));
#454560=CARTESIAN_POINT('Ctrl Pts',(6.17163058503857,24.6188841212508,-4.4346429653087));
#454561=CARTESIAN_POINT('Ctrl Pts',(4.90862178076926,24.5474010505566,-4.56189118942603));
#454562=CARTESIAN_POINT('Ctrl Pts',(4.33113291369596,24.4759179798625,-5.69232914266461));
#454563=CARTESIAN_POINT('Ctrl Pts',(4.96825133880203,24.4044349091683,-6.7902651507014));
#454564=CARTESIAN_POINT('Ctrl Pts',(6.23625792548383,24.3329518384741,-6.84978535971091));
#454565=CARTESIAN_POINT('Ctrl Pts',(6.97342250511928,24.2614687677799,-5.8163581765647));
#454566=CARTESIAN_POINT('Ctrl Pts',(6.50436504145381,24.1899856970857,-4.6367953517292));
#454567=CARTESIAN_POINT('Ctrl Pts',(5.25882952309621,24.1185026263916,-4.39179610102783));
#454568=CARTESIAN_POINT('Ctrl Pts',(4.37795843727392,24.0470195556974,-5.30582536167067));
#454569=CARTESIAN_POINT('Ctrl Pts',(4.66879374102308,23.9755364850032,-6.54146211713177));
#454570=CARTESIAN_POINT('Ctrl Pts',(5.86487613450724,23.904053414309,-6.96663298362319));
#454571=CARTESIAN_POINT('Ctrl Pts',(6.8703714022368,23.8325703436148,-6.19180228161384));
#454572=CARTESIAN_POINT('Ctrl Pts',(6.76405862808225,23.7610872729207,-4.92685920413014));
#454573=CARTESIAN_POINT('Ctrl Pts',(5.64334011190815,23.6896042022265,-4.33072722538547));
#454574=CARTESIAN_POINT('Ctrl Pts',(4.53500272215099,23.6181211315323,-4.94957415925549));
#454575=CARTESIAN_POINT('Ctrl Pts',(4.45448991200439,23.5466380608381,-6.21642115383373));
#454576=CARTESIAN_POINT('Ctrl Pts',(5.47556640632124,23.475154990144,-6.9706000763964));
#454577=CARTESIAN_POINT('Ctrl Pts',(6.66273598971973,23.4036719194498,-6.52114329936776));
#454578=CARTESIAN_POINT('Ctrl Pts',(6.92833022917403,23.3321888487556,-5.27983553104633));
#454579=CARTESIAN_POINT('Ctrl Pts',(6.02901536249358,23.2607057780614,-4.38394859923605));
#454580=CARTESIAN_POINT('Ctrl Pts',(4.78873124130167,23.1892227073672,-4.6542763857934));
#454581=CARTESIAN_POINT('Ctrl Pts',(4.34380918016856,23.1177396366731,-5.8431588586417));
#454582=CARTESIAN_POINT('Ctrl Pts',(5.1018804774459,23.0462565659789,-6.86133755596363));
#454583=CARTESIAN_POINT('Ctrl Pts',(6.36841097734036,22.9747734952847,-6.77601180031397));
#454584=CARTESIAN_POINT('Ctrl Pts',(6.98302223994139,22.9032904245905,-5.66527621173653));
#454585=CARTESIAN_POINT('Ctrl Pts',(6.3826171450343,22.8318073538963,-4.54692766144198));
#454586=CARTESIAN_POINT('Ctrl Pts',(5.11727611571492,22.7603242832022,-4.4452753183732));
#454587=CARTESIAN_POINT('Ctrl Pts',(4.34629195893472,22.688841212508,-5.45405255931454));
#454588=CARTESIAN_POINT('Ctrl Pts',(4.77602071980922,22.6173581418138,-6.64785217518362));
#454589=CARTESIAN_POINT('Ctrl Pts',(6.01276456633487,22.5458750711197,-6.93525520080945));
#454590=CARTESIAN_POINT('Ctrl Pts',(6.92345206015258,22.4743920004254,-6.04826976192828));
#454591=CARTESIAN_POINT('Ctrl Pts',(6.75659092854625,22.4267366199627,-5.22281495825156));
#454592=CARTESIAN_POINT('Ctrl Pts',(6.5169819168131,22.4029089297313,-4.93665266667552));
#454593=CARTESIAN_POINT('Ctrl Pts',(6.86060932929632,26.0970910702687,-5.58468863860454));
#454594=CARTESIAN_POINT('Ctrl Pts',(6.83660014748639,26.0732633800373,-5.18420242845371));
#454595=CARTESIAN_POINT('Ctrl Pts',(6.35764569349554,26.0256079995746,-4.41601015327873));
#454596=CARTESIAN_POINT('Ctrl Pts',(4.99126448034597,25.9541249288803,-4.39517119822623));
#454597=CARTESIAN_POINT('Ctrl Pts',(4.23702001084117,25.8826418581862,-5.53270027843017));
#454598=CARTESIAN_POINT('Ctrl Pts',(4.7824753491703,25.811158787492,-6.78276611783875));
#454599=CARTESIAN_POINT('Ctrl Pts',(6.12959649298558,25.7396757167979,-7.00190159169352));
#454600=CARTESIAN_POINT('Ctrl Pts',(7.04330603741155,25.6681926461036,-5.98840954909488));
#454601=CARTESIAN_POINT('Ctrl Pts',(6.68691572204242,25.5967095754095,-4.67131052012888));
#454602=CARTESIAN_POINT('Ctrl Pts',(5.38672120534383,25.5252265047153,-4.2570712821673));
#454603=CARTESIAN_POINT('Ctrl Pts',(4.33405713849982,25.4537434340211,-5.12533511911963));
#454604=CARTESIAN_POINT('Ctrl Pts',(4.49330153555078,25.382260363327,-6.48054794122378));
#454605=CARTESIAN_POINT('Ctrl Pts',(5.71858660500674,25.3107772926328,-7.0811144088688));
#454606=CARTESIAN_POINT('Ctrl Pts',(6.88730788058188,25.2392942219386,-6.37678748673361));
#454607=CARTESIAN_POINT('Ctrl Pts',(6.92870675713562,25.1678111512444,-5.01287011686923));
#454608=CARTESIAN_POINT('Ctrl Pts',(5.80485021183448,25.0963280805502,-4.23896036791547));
#454609=CARTESIAN_POINT('Ctrl Pts',(4.54540214324444,25.0248450098561,-4.76410585554996));
#454610=CARTESIAN_POINT('Ctrl Pts',(4.30425050070234,24.9533619391619,-6.10717441394478));
#454611=CARTESIAN_POINT('Ctrl Pts',(5.302335620529,24.8818788684677,-7.03766568988833));
#454612=CARTESIAN_POINT('Ctrl Pts',(6.62522539570715,24.8103957977735,-6.70307610499455));
#454613=CARTESIAN_POINT('Ctrl Pts',(7.06090656990369,24.7389127270793,-5.40995217496277));
#454614=CARTESIAN_POINT('Ctrl Pts',(6.21021398251268,24.6674296563851,-4.34303616011549));
#454615=CARTESIAN_POINT('Ctrl Pts',(4.85254050111457,24.595946585691,-4.47982185698087));
#454616=CARTESIAN_POINT('Ctrl Pts',(4.23176785251722,24.5244635149968,-5.69498807457972));
#454617=CARTESIAN_POINT('Ctrl Pts',(4.91663939684271,24.4529804443027,-6.87521627041245));
#454618=CARTESIAN_POINT('Ctrl Pts',(6.27968525302103,24.3814973736084,-6.93919762122039));
#454619=CARTESIAN_POINT('Ctrl Pts',(7.07210158283119,24.3100143029143,-5.82831329739714));
#454620=CARTESIAN_POINT('Ctrl Pts',(6.567887457389,24.2385312322201,-4.5603402147798));
#454621=CARTESIAN_POINT('Ctrl Pts',(5.22899691466481,24.1670481615259,-4.29697784983407));
#454622=CARTESIAN_POINT('Ctrl Pts',(4.28210302943719,24.0955650908318,-5.27951517198252));
#454623=CARTESIAN_POINT('Ctrl Pts',(4.59473693825861,24.0240820201375,-6.60776502254541));
#454624=CARTESIAN_POINT('Ctrl Pts',(5.88046775954143,23.9525989494434,-7.06480317504856));
#454625=CARTESIAN_POINT('Ctrl Pts',(6.96132662295805,23.8811158787492,-6.2318975823597));
#454626=CARTESIAN_POINT('Ctrl Pts',(6.84704552395415,23.809632808055,-4.87214485065071));
#454627=CARTESIAN_POINT('Ctrl Pts',(5.64232723190576,23.7381497373609,-4.23133175717171));
#454628=CARTESIAN_POINT('Ctrl Pts',(4.45091805294454,23.6666666666667,-4.89656233064023));
#454629=CARTESIAN_POINT('Ctrl Pts',(4.36437066952221,23.5951835959725,-6.25836168129701));
#454630=CARTESIAN_POINT('Ctrl Pts',(5.4619785991953,23.5237005252783,-7.06906760823242));
#454631=CARTESIAN_POINT('Ctrl Pts',(6.73812857998268,23.4522174545842,-6.58592327452409));
#454632=CARTESIAN_POINT('Ctrl Pts',(7.02362956342815,23.3807343838899,-5.25157735895587));
#454633=CARTESIAN_POINT('Ctrl Pts',(6.05690950431861,23.3092513131958,-4.28854216431714));
#454634=CARTESIAN_POINT('Ctrl Pts',(4.72366395998878,23.2377682425016,-4.57913148234355));
#454635=CARTESIAN_POINT('Ctrl Pts',(4.24539422691366,23.1662851718074,-5.8571227365842));
#454636=CARTESIAN_POINT('Ctrl Pts',(5.06028426872769,23.0948021011132,-6.95161567440516));
#454637=CARTESIAN_POINT('Ctrl Pts',(6.42174340288106,23.0233190304191,-6.85989460695557));
#454638=CARTESIAN_POINT('Ctrl Pts',(7.08242083425081,22.9518359597249,-5.66590748005734));
#454639=CARTESIAN_POINT('Ctrl Pts',(6.4370143472206,22.8803528890307,-4.46373678689788));
#454640=CARTESIAN_POINT('Ctrl Pts',(5.07683383650299,22.8088698183366,-4.35446542628666));
#454641=CARTESIAN_POINT('Ctrl Pts',(4.24806309420865,22.7373867476423,-5.43885225243895));
#454642=CARTESIAN_POINT('Ctrl Pts',(4.71000076309996,22.6659036769482,-6.72212919800733));
#454643=CARTESIAN_POINT('Ctrl Pts',(6.03944068310239,22.594420606254,-7.03107357357049));
#454644=CARTESIAN_POINT('Ctrl Pts',(7.01838576726789,22.5229375355598,-6.07760705403036));
#454645=CARTESIAN_POINT('Ctrl Pts',(6.83901810752379,22.475282155097,-5.19028299638619));
#454646=CARTESIAN_POINT('Ctrl Pts',(6.58144998920627,22.4514544648656,-4.88267235001886));
#454647=CARTESIAN_POINT('Ctrl Pts',(6.94454197042357,26.1456366054031,-5.57965686974575));
#454648=CARTESIAN_POINT('Ctrl Pts',(6.91885873260879,26.1218089151717,-5.15124649498694));
#454649=CARTESIAN_POINT('Ctrl Pts',(6.4065088640594,26.0741535347089,-4.32949150779126));
#454650=CARTESIAN_POINT('Ctrl Pts',(4.94485582145311,26.0026704640147,-4.30719954288124));
#454651=CARTESIAN_POINT('Ctrl Pts',(4.1380211598586,25.9311873933206,-5.52404358693881));
#454652=CARTESIAN_POINT('Ctrl Pts',(4.7215087306785,25.8597043226263,-6.86127108980971));
#454653=CARTESIAN_POINT('Ctrl Pts',(6.16255878293893,25.7882212519322,-7.09568592881682));
#454654=CARTESIAN_POINT('Ctrl Pts',(7.13997732676548,25.716738181238,-6.01152748645437));
#454655=CARTESIAN_POINT('Ctrl Pts',(6.7587374620765,25.6452551105438,-4.60259286076204));
#454656=CARTESIAN_POINT('Ctrl Pts',(5.36788602689621,25.5737720398497,-4.15947051927595));
#454657=CARTESIAN_POINT('Ctrl Pts',(4.24182426511434,25.5022889691555,-5.08827462376231));
#454658=CARTESIAN_POINT('Ctrl Pts',(4.41217208256641,25.4308058984613,-6.53798055190634));
#454659=CARTESIAN_POINT('Ctrl Pts',(5.72289095998872,25.3593228277671,-7.18042191180854));
#454660=CARTESIAN_POINT('Ctrl Pts',(6.97310209577086,25.287839757073,-6.42698533143036));
#454661=CARTESIAN_POINT('Ctrl Pts',(7.01738753624157,25.2163566863788,-4.96796792520408));
#454662=CARTESIAN_POINT('Ctrl Pts',(5.81516935358236,25.1448736156846,-4.14009680960707));
#454663=CARTESIAN_POINT('Ctrl Pts',(4.46790543942481,25.0733905449904,-4.70185841202445));
#454664=CARTESIAN_POINT('Ctrl Pts',(4.20993933987732,25.0019074742962,-6.1385733096785));
#454665=CARTESIAN_POINT('Ctrl Pts',(5.27761660163647,24.930424403602,-7.13394370229866));
#454666=CARTESIAN_POINT('Ctrl Pts',(6.69274573713214,24.8589413329079,-6.77602463836695));
#454667=CARTESIAN_POINT('Ctrl Pts',(7.15880506797054,24.7874582622137,-5.39273679116275));
#454668=CARTESIAN_POINT('Ctrl Pts',(6.24879737998679,24.7159751915195,-4.25142935492228));
#454669=CARTESIAN_POINT('Ctrl Pts',(4.79645922145989,24.6444921208253,-4.39775252453571));
#454670=CARTESIAN_POINT('Ctrl Pts',(4.13240279133847,24.5730090501312,-5.69764700649481));
#454671=CARTESIAN_POINT('Ctrl Pts',(4.86502745488341,24.501525979437,-6.9601673901235));
#454672=CARTESIAN_POINT('Ctrl Pts',(6.32311258055821,24.4300429087428,-7.02860988272989));
#454673=CARTESIAN_POINT('Ctrl Pts',(7.17078066054311,24.3585598380486,-5.84026841822957));
#454674=CARTESIAN_POINT('Ctrl Pts',(6.63140987332417,24.2870767673545,-4.4838850778304));
#454675=CARTESIAN_POINT('Ctrl Pts',(5.19916430623342,24.2155936966603,-4.2021595986403));
#454676=CARTESIAN_POINT('Ctrl Pts',(4.18624762160045,24.1441106259661,-5.25320498229437));
#454677=CARTESIAN_POINT('Ctrl Pts',(4.52068013549415,24.0726275552719,-6.67406792795906));
#454678=CARTESIAN_POINT('Ctrl Pts',(5.89605938457563,24.0011444845777,-7.16297336647392));
#454679=CARTESIAN_POINT('Ctrl Pts',(7.0522818436793,23.9296614138836,-6.27199288310558));
#454680=CARTESIAN_POINT('Ctrl Pts',(6.93003241982605,23.8581783431894,-4.81743049717126));
#454681=CARTESIAN_POINT('Ctrl Pts',(5.64131435190337,23.7866952724952,-4.13193628895796));
#454682=CARTESIAN_POINT('Ctrl Pts',(4.3668333837381,23.715212201801,-4.84355050202496));
#454683=CARTESIAN_POINT('Ctrl Pts',(4.27425142704003,23.6437291311069,-6.30030220876029));
#454684=CARTESIAN_POINT('Ctrl Pts',(5.44839079206936,23.5722460604127,-7.16753514006844));
#454685=CARTESIAN_POINT('Ctrl Pts',(6.81352117024561,23.5007629897185,-6.65070324968042));
#454686=CARTESIAN_POINT('Ctrl Pts',(7.11892889768229,23.4292799190243,-5.22331918686542));
#454687=CARTESIAN_POINT('Ctrl Pts',(6.08480364614364,23.3577968483302,-4.19313572939824));
#454688=CARTESIAN_POINT('Ctrl Pts',(4.65859667867589,23.2863137776359,-4.50398657889369));
#454689=CARTESIAN_POINT('Ctrl Pts',(4.14697927365876,23.2148307069418,-5.8710866145267));
#454690=CARTESIAN_POINT('Ctrl Pts',(5.01868806000948,23.1433476362476,-7.04189379284668));
#454691=CARTESIAN_POINT('Ctrl Pts',(6.47507582842176,23.0718645655535,-6.94377741359719));
#454692=CARTESIAN_POINT('Ctrl Pts',(7.18181942856023,23.0003814948592,-5.66653874837813));
#454693=CARTESIAN_POINT('Ctrl Pts',(6.49141154940691,22.9288984241651,-4.38054591235379));
#454694=CARTESIAN_POINT('Ctrl Pts',(5.03639155729104,22.8574153534709,-4.26365553420012));
#454695=CARTESIAN_POINT('Ctrl Pts',(4.14983422948258,22.7859322827767,-5.42365194556336));
#454696=CARTESIAN_POINT('Ctrl Pts',(4.6439808063907,22.7144492120825,-6.79640622083105));
#454697=CARTESIAN_POINT('Ctrl Pts',(6.06611679986992,22.6429661413884,-7.12689194633153));
#454698=CARTESIAN_POINT('Ctrl Pts',(7.11331947438321,22.5714830706942,-6.10694434613243));
#454699=CARTESIAN_POINT('Ctrl Pts',(6.92144528650133,22.5238276902314,-5.15775103452081));
#454700=CARTESIAN_POINT('Ctrl Pts',(6.64591806159944,22.5,-4.8286920333622));
#454701=CARTESIAN_POINT('Ctrl Pts',(4.92197603118329,25.2730384757729,-6.39051881327128));
#454702=CARTESIAN_POINT('Ctrl Pts',(4.8802577415671,25.2770820815347,-6.34953594825859));
#454703=CARTESIAN_POINT('Ctrl Pts',(4.84215579969382,25.2811256872965,-6.3050503566324));
#454704=CARTESIAN_POINT('Ctrl Pts',(4.80845709106526,25.2851692930582,-6.25744773204304));
#454705=CARTESIAN_POINT('Ctrl Pts',(4.60988125610326,25.3089969832896,-5.97694051651721));
#454706=CARTESIAN_POINT('Ctrl Pts',(4.56420207068701,25.332824673521,-5.58819831317574));
#454707=CARTESIAN_POINT('Ctrl Pts',(4.69234059080694,25.3566523637524,-5.26929666119096));
#454708=CARTESIAN_POINT('Ctrl Pts',(4.82047911092687,25.3804800539838,-4.95039500920618));
#454709=CARTESIAN_POINT('Ctrl Pts',(5.12243533658298,25.4043077442152,-4.70133390857809));
#454710=CARTESIAN_POINT('Ctrl Pts',(5.45989356270023,25.4281354344466,-4.6362155300828));
#454711=CARTESIAN_POINT('Ctrl Pts',(5.79735178881747,25.451963124678,-4.57109715158752));
#454712=CARTESIAN_POINT('Ctrl Pts',(6.17031201539585,25.4757908149094,-4.68992149522503));
#454713=CARTESIAN_POINT('Ctrl Pts',(6.40790733147329,25.4996185051408,-4.93823830629602));
#454714=CARTESIAN_POINT('Ctrl Pts',(6.64550264755072,25.5234461953722,-5.186555117367));
#454715=CARTESIAN_POINT('Ctrl Pts',(6.74773305312721,25.5472738856035,-5.56436439587145));
#454716=CARTESIAN_POINT('Ctrl Pts',(6.66779966497798,25.5711015758349,-5.89862890896884));
#454717=CARTESIAN_POINT('Ctrl Pts',(6.58786627682875,25.5949292660663,-6.23289342206624));
#454718=CARTESIAN_POINT('Ctrl Pts',(6.32576909495381,25.6187569562977,-6.52361316975658));
#454719=CARTESIAN_POINT('Ctrl Pts',(6.00150994952884,25.6425846465291,-6.63754358634341));
#454720=CARTESIAN_POINT('Ctrl Pts',(5.67725080410387,25.6664123367605,-6.75147400293023));
#454721=CARTESIAN_POINT('Ctrl Pts',(5.29082969512888,25.6902400269919,-6.68861508841353));
#454722=CARTESIAN_POINT('Ctrl Pts',(5.01938732841678,25.7140677172233,-6.47789521240786));
#454723=CARTESIAN_POINT('Ctrl Pts',(4.98532270432787,25.7170579700732,-6.45145094929911));
#454724=CARTESIAN_POINT('Ctrl Pts',(4.95306887608107,25.720048222923,-6.42267802952734));
#454725=CARTESIAN_POINT('Ctrl Pts',(4.92276701974739,25.7230384757729,-6.39190058798136));
#454726=CARTESIAN_POINT('Ctrl Pts',(4.53900700771688,26.,-5.01302286563431));
#454727=CARTESIAN_POINT('Ctrl Pts',(4.32480615636363,25.9761723097686,-5.38492752167559));
#454728=CARTESIAN_POINT('Ctrl Pts',(4.30067277954968,25.9285169293058,-6.35301914505848));
#454729=CARTESIAN_POINT('Ctrl Pts',(5.50907794609547,25.8570338586117,-7.1756264891545));
#454730=CARTESIAN_POINT('Ctrl Pts',(6.8522203629011,25.7855507879174,-6.60321033464885));
#454731=CARTESIAN_POINT('Ctrl Pts',(7.1004834147237,25.7140677172233,-5.16550356767203));
#454732=CARTESIAN_POINT('Ctrl Pts',(6.02596364157129,25.6425846465291,-4.17707919799325));
#454733=CARTESIAN_POINT('Ctrl Pts',(4.61334644908231,25.5711015758349,-4.5448553014618));
#454734=CARTESIAN_POINT('Ctrl Pts',(4.15673773385264,25.4996185051408,-5.93119910857215));
#454735=CARTESIAN_POINT('Ctrl Pts',(5.07453447980768,25.4281354344466,-7.0663089114369));
#454736=CARTESIAN_POINT('Ctrl Pts',(6.5258341885166,25.3566523637524,-6.9100356033464));
#454737=CARTESIAN_POINT('Ctrl Pts',(7.18099123031483,25.2851692930582,-5.60564496305001));
#454738=CARTESIAN_POINT('Ctrl Pts',(6.43975200870338,25.213686222364,-4.34815567114858));
#454739=CARTESIAN_POINT('Ctrl Pts',(4.98123363545819,25.1422031516699,-4.2896855842815));
#454740=CARTESIAN_POINT('Ctrl Pts',(4.14170854437417,25.0707200809757,-5.48379221455872));
#454741=CARTESIAN_POINT('Ctrl Pts',(4.69033908735646,24.9992370102815,-6.83645762028281));
#454742=CARTESIAN_POINT('Ctrl Pts',(6.12447699388038,24.9277539395874,-7.10838527255516));
#454743=CARTESIAN_POINT('Ctrl Pts',(7.13018513270865,24.8562708688931,-6.05044038944422));
#454744=CARTESIAN_POINT('Ctrl Pts',(6.78604742232836,24.784787798199,-4.63189669239788));
#454745=CARTESIAN_POINT('Ctrl Pts',(5.40735816264999,24.7133047275048,-4.15240479236239));
#454746=CARTESIAN_POINT('Ctrl Pts',(4.25725342975252,24.6418216568106,-5.0512683537124));
#454747=CARTESIAN_POINT('Ctrl Pts',(4.38944335790391,24.5703385861164,-6.50496106867921));
#454748=CARTESIAN_POINT('Ctrl Pts',(5.68281734635597,24.4988555154223,-7.18162963832198));
#454749=CARTESIAN_POINT('Ctrl Pts',(6.95240396480877,24.4273724447281,-6.46131966662841));
#454750=CARTESIAN_POINT('Ctrl Pts',(7.03502543671246,24.3558893740339,-5.00396921476326));
#454751=CARTESIAN_POINT('Ctrl Pts',(5.85498510857852,24.2844063033397,-4.14478270244581));
#454752=CARTESIAN_POINT('Ctrl Pts',(4.49341967622111,24.2129232326456,-4.67093497503137));
#454753=CARTESIAN_POINT('Ctrl Pts',(4.19777663638434,24.1414401619514,-6.10037256921808));
#454754=CARTESIAN_POINT('Ctrl Pts',(5.23892007073304,24.0699570912572,-7.12346444664167));
#454755=CARTESIAN_POINT('Ctrl Pts',(6.662968703113,23.998474020563,-6.80286792203874));
#454756=CARTESIAN_POINT('Ctrl Pts',(7.16522879152533,23.9269909498688,-5.43230911237055));
#454757=CARTESIAN_POINT('Ctrl Pts',(6.2855365564656,23.8555078791747,-4.26747512907024));
#454758=CARTESIAN_POINT('Ctrl Pts',(4.82985391579145,23.7840248084805,-4.37557081254884));
#454759=CARTESIAN_POINT('Ctrl Pts',(4.13185724083954,23.7125417377863,-5.6575604101698));
#454760=CARTESIAN_POINT('Ctrl Pts',(4.83104150205928,23.6410586670921,-6.93890266242659));
#454761=CARTESIAN_POINT('Ctrl Pts',(6.28682364983267,23.569575596398,-7.04564953674368));
#454762=CARTESIAN_POINT('Ctrl Pts',(7.16543624640093,23.4980925257038,-5.88000083782647));
#454763=CARTESIAN_POINT('Ctrl Pts',(6.66190630419616,23.4266094550096,-4.50990820099157));
#454764=CARTESIAN_POINT('Ctrl Pts',(5.23756146736659,23.3551263843154,-4.19063094092434));
#454765=CARTESIAN_POINT('Ctrl Pts',(4.19736598356861,23.2836433136212,-5.21468783779197));
#454766=CARTESIAN_POINT('Ctrl Pts',(4.49433434427903,23.2121602429271,-6.64384941569999));
#454767=CARTESIAN_POINT('Ctrl Pts',(5.85638486317849,23.1406771722328,-7.16874271925581));
#454768=CARTESIAN_POINT('Ctrl Pts',(7.03563221165043,23.0691941015387,-6.3084575374563));
#454769=CARTESIAN_POINT('Ctrl Pts',(6.95165327175697,22.9977110308445,-4.85119529970874));
#454770=CARTESIAN_POINT('Ctrl Pts',(5.68141376558385,22.9262279601503,-4.13204038713624));
#454771=CARTESIAN_POINT('Ctrl Pts',(4.38863987327371,22.8547448894562,-4.80994952176022));
#454772=CARTESIAN_POINT('Ctrl Pts',(4.25785081625157,22.783261818762,-6.26368089065207));
#454773=CARTESIAN_POINT('Ctrl Pts',(5.40868234342555,22.7117787480678,-7.16164157512573));
#454774=CARTESIAN_POINT('Ctrl Pts',(6.78713386963136,22.6402956773736,-6.68055232418451));
#454775=CARTESIAN_POINT('Ctrl Pts',(7.12954990426926,22.5688126066795,-5.26231872215201));
#454776=CARTESIAN_POINT('Ctrl Pts',(6.1236699944058,22.4973295359853,-4.20406666678213));
#454777=CARTESIAN_POINT('Ctrl Pts',(4.68809392709695,22.4258464652911,-4.4798333146301));
#454778=CARTESIAN_POINT('Ctrl Pts',(4.32622391325397,22.3781910848283,-5.37807265034296));
#454779=CARTESIAN_POINT('Ctrl Pts',(4.37532354240196,22.3543633945969,-5.80443435631943));
#454780=CARTESIAN_POINT('Ctrl Pts',(4.61186924884874,26.0485455351344,-5.05498833669907));
#454781=CARTESIAN_POINT('Ctrl Pts',(4.41163019717349,26.024717844903,-5.40265192052164));
#454782=CARTESIAN_POINT('Ctrl Pts',(4.38906985506272,25.9770624644402,-6.30764248137266));
#454783=CARTESIAN_POINT('Ctrl Pts',(5.51871011120511,25.905579393746,-7.07663155607638));
#454784=CARTESIAN_POINT('Ctrl Pts',(6.77430532526158,25.8340963230518,-6.54152598941931));
#454785=CARTESIAN_POINT('Ctrl Pts',(7.00638637325414,25.7626132523576,-5.1975302126156));
#454786=CARTESIAN_POINT('Ctrl Pts',(6.00190474293836,25.6911301816635,-4.27353221173565));
#454787=CARTESIAN_POINT('Ctrl Pts',(4.68136318011483,25.6196471109693,-4.61733634566933));
#454788=CARTESIAN_POINT('Ctrl Pts',(4.25451662209878,25.5481640402751,-5.91331704545576));
#454789=CARTESIAN_POINT('Ctrl Pts',(5.11249056981941,25.4766809695809,-6.97443939411568));
#454790=CARTESIAN_POINT('Ctrl Pts',(6.46919328847102,25.4051978988868,-6.82835211754092));
#454791=CARTESIAN_POINT('Ctrl Pts',(7.08164661869466,25.3337148281926,-5.60898280515531));
#454792=CARTESIAN_POINT('Ctrl Pts',(6.38872202076577,25.2622317574984,-4.43345777007097));
#454793=CARTESIAN_POINT('Ctrl Pts',(5.02527115647435,25.1907486868042,-4.37879881483497));
#454794=CARTESIAN_POINT('Ctrl Pts',(4.24046704839444,25.1192656161101,-5.49507252586477));
#454795=CARTESIAN_POINT('Ctrl Pts',(4.75333737058418,25.0477825454159,-6.75957001205557));
#454796=CARTESIAN_POINT('Ctrl Pts',(6.09399690839473,24.9762994747217,-7.01377318104995));
#454797=CARTESIAN_POINT('Ctrl Pts',(7.03415210716631,24.9048164040275,-6.0247860748808));
#454798=CARTESIAN_POINT('Ctrl Pts',(6.71244559509181,24.8333333333333,-4.69870430227373));
#454799=CARTESIAN_POINT('Ctrl Pts',(5.42362051261083,24.7618502626392,-4.25046610554157));
#454800=CARTESIAN_POINT('Ctrl Pts',(4.34848061663153,24.690367191945,-5.09074095026355));
#454801=CARTESIAN_POINT('Ctrl Pts',(4.47205428913018,24.6188841212508,-6.44968069692276));
#454802=CARTESIAN_POINT('Ctrl Pts',(5.68112502471735,24.5474010505566,-7.08224341470705));
#454803=CARTESIAN_POINT('Ctrl Pts',(6.86795887198031,24.4759179798625,-6.40888387979891));
#454804=CARTESIAN_POINT('Ctrl Pts',(6.94519500375798,24.4044349091682,-5.04652481074592));
#454805=CARTESIAN_POINT('Ctrl Pts',(5.84207074093974,24.3329518384741,-4.24334083014217));
#454806=CARTESIAN_POINT('Ctrl Pts',(4.56925333967074,24.2614687677799,-4.73519803534797));
#454807=CARTESIAN_POINT('Ctrl Pts',(4.29288057290861,24.1899856970857,-6.07146363130893));
#454808=CARTESIAN_POINT('Ctrl Pts',(5.2661613635068,24.1185026263916,-7.02786948132165));
#454809=CARTESIAN_POINT('Ctrl Pts',(6.59738925492608,24.0470195556973,-6.72816971985337));
#454810=CARTESIAN_POINT('Ctrl Pts',(7.0669115895136,23.9755364850032,-5.44694513750787));
#454811=CARTESIAN_POINT('Ctrl Pts',(6.24455846719129,23.904053414309,-4.35803605660742));
#454812=CARTESIAN_POINT('Ctrl Pts',(4.8837584999306,23.8325703436148,-4.45908596846911));
#454813=CARTESIAN_POINT('Ctrl Pts',(4.2312578614791,23.7610872729207,-5.65751435782136));
#454814=CARTESIAN_POINT('Ctrl Pts',(4.88486867828213,23.6896042022265,-6.85533759634902));
#454815=CARTESIAN_POINT('Ctrl Pts',(6.24576166668191,23.6181211315323,-6.95512661561532));
#454816=CARTESIAN_POINT('Ctrl Pts',(7.06710552229815,23.5466380608381,-5.86545592297769));
#454817=CARTESIAN_POINT('Ctrl Pts',(6.59639610410402,23.475154990144,-4.58466712791061));
#454818=CARTESIAN_POINT('Ctrl Pts',(5.26489131510138,23.4036719194498,-4.28620064015658));
#454819=CARTESIAN_POINT('Ctrl Pts',(4.2924966868042,23.3321888487556,-5.24350860879812));
#454820=CARTESIAN_POINT('Ctrl Pts',(4.57010838886106,23.2607057780614,-6.57951617946397));
#454821=CARTESIAN_POINT('Ctrl Pts',(5.84337925830513,23.1892227073672,-7.07019647634743));
#454822=CARTESIAN_POINT('Ctrl Pts',(6.94576222857241,23.1177396366731,-6.26598543850373));
#454823=CARTESIAN_POINT('Ctrl Pts',(6.86725710976114,23.0462565659789,-4.90370883369462));
#454824=CARTESIAN_POINT('Ctrl Pts',(5.67981293057309,22.9747734952847,-4.23142907013928));
#454825=CARTESIAN_POINT('Ctrl Pts',(4.47130317633407,22.9032904245905,-4.86515149178938));
#454826=CARTESIAN_POINT('Ctrl Pts',(4.34903906495375,22.8318073538963,-6.22412737287685));
#454827=CARTESIAN_POINT('Ctrl Pts',(5.42485838212006,22.7603242832022,-7.06355819103049));
#454828=CARTESIAN_POINT('Ctrl Pts',(6.7134612268051,22.688841212508,-6.613826760128));
#454829=CARTESIAN_POINT('Ctrl Pts',(7.03355828347467,22.6173581418138,-5.28803487026933));
#454830=CARTESIAN_POINT('Ctrl Pts',(6.0932425098549,22.5458750711196,-4.29876061359894));
#454831=CARTESIAN_POINT('Ctrl Pts',(4.75123855184285,22.4743920004255,-4.55655254906459));
#454832=CARTESIAN_POINT('Ctrl Pts',(4.41295554342414,22.4267366199627,-5.39624385572484));
#454833=CARTESIAN_POINT('Ctrl Pts',(4.45885481560764,22.4029089297313,-5.79481493112442));
#454834=CARTESIAN_POINT('Ctrl Pts',(4.6847314899806,26.0970910702687,-5.09695380776383));
#454835=CARTESIAN_POINT('Ctrl Pts',(4.49845423798335,26.0732633800373,-5.42037631936769));
#454836=CARTESIAN_POINT('Ctrl Pts',(4.47746693057576,26.0256079995745,-6.26226581768684));
#454837=CARTESIAN_POINT('Ctrl Pts',(5.52834227631475,25.9541249288804,-6.97763662299825));
#454838=CARTESIAN_POINT('Ctrl Pts',(6.69639028762207,25.8826418581862,-6.47984164418979));
#454839=CARTESIAN_POINT('Ctrl Pts',(6.91228933178459,25.811158787492,-5.22955685755916));
#454840=CARTESIAN_POINT('Ctrl Pts',(5.97784584430541,25.7396757167978,-4.36998522547805));
#454841=CARTESIAN_POINT('Ctrl Pts',(4.74937991114735,25.6681926461037,-4.68981738987686));
#454842=CARTESIAN_POINT('Ctrl Pts',(4.35229551034492,25.5967095754095,-5.89543498233936));
#454843=CARTESIAN_POINT('Ctrl Pts',(5.15044665983114,25.5252265047153,-6.88256987679449));
#454844=CARTESIAN_POINT('Ctrl Pts',(6.41255238842542,25.4537434340211,-6.74666863173542));
#454845=CARTESIAN_POINT('Ctrl Pts',(6.9823020070745,25.3822603633269,-5.61232064726062));
#454846=CARTESIAN_POINT('Ctrl Pts',(6.33769203282816,25.3107772926328,-4.51875986899335));
#454847=CARTESIAN_POINT('Ctrl Pts',(5.06930867749052,25.2392942219386,-4.46791204538843));
#454848=CARTESIAN_POINT('Ctrl Pts',(4.33922555241473,25.1678111512444,-5.50635283717082));
#454849=CARTESIAN_POINT('Ctrl Pts',(4.81633565381187,25.0963280805502,-6.68268240382832));
#454850=CARTESIAN_POINT('Ctrl Pts',(6.06351682290909,25.0248450098561,-6.91916108954474));
#454851=CARTESIAN_POINT('Ctrl Pts',(6.93811908162396,24.9533619391618,-5.99913176031739));
#454852=CARTESIAN_POINT('Ctrl Pts',(6.63884376785526,24.8818788684677,-4.76551191214956));
#454853=CARTESIAN_POINT('Ctrl Pts',(5.43988286257166,24.8103957977735,-4.34852741872077));
#454854=CARTESIAN_POINT('Ctrl Pts',(4.43970780351055,24.7389127270794,-5.13021354681468));
#454855=CARTESIAN_POINT('Ctrl Pts',(4.55466522035644,24.6674296563851,-6.39440032516632));
#454856=CARTESIAN_POINT('Ctrl Pts',(5.67943270307874,24.595946585691,-6.98285719109209));
#454857=CARTESIAN_POINT('Ctrl Pts',(6.78351377915186,24.5244635149968,-6.35644809296943));
#454858=CARTESIAN_POINT('Ctrl Pts',(6.85536457080349,24.4529804443026,-5.08908040672856));
#454859=CARTESIAN_POINT('Ctrl Pts',(5.82915637330097,24.3814973736085,-4.34189895783853));
#454860=CARTESIAN_POINT('Ctrl Pts',(4.64508700312038,24.3100143029142,-4.79946109566455));
#454861=CARTESIAN_POINT('Ctrl Pts',(4.38798450943288,24.2385312322201,-6.04255469339979));
#454862=CARTESIAN_POINT('Ctrl Pts',(5.29340265628057,24.1670481615259,-6.93227451600163));
#454863=CARTESIAN_POINT('Ctrl Pts',(6.53180980673916,24.0955650908317,-6.653471517668));
#454864=CARTESIAN_POINT('Ctrl Pts',(6.96859438750187,24.0240820201376,-5.46158116264518));
#454865=CARTESIAN_POINT('Ctrl Pts',(6.20358037791699,23.9525989494434,-4.44859698414461));
#454866=CARTESIAN_POINT('Ctrl Pts',(4.93766308406974,23.8811158787492,-4.54260112438938));
#454867=CARTESIAN_POINT('Ctrl Pts',(4.33065848211866,23.809632808055,-5.65746830547292));
#454868=CARTESIAN_POINT('Ctrl Pts',(4.93869585450499,23.7381497373608,-6.77177253027144));
#454869=CARTESIAN_POINT('Ctrl Pts',(6.20469968353115,23.6666666666667,-6.86460369448698));
#454870=CARTESIAN_POINT('Ctrl Pts',(6.96877479819537,23.5951835959725,-5.85091100812889));
#454871=CARTESIAN_POINT('Ctrl Pts',(6.53088590401188,23.5237005252783,-4.65942605482967));
#454872=CARTESIAN_POINT('Ctrl Pts',(5.29222116283617,23.4522174545841,-4.3817703393888));
#454873=CARTESIAN_POINT('Ctrl Pts',(4.38762739003978,23.38073438389,-5.27232937980428));
#454874=CARTESIAN_POINT('Ctrl Pts',(4.6458824334431,23.3092513131958,-6.51518294322794));
#454875=CARTESIAN_POINT('Ctrl Pts',(5.83037365343178,23.2377682425016,-6.97165023343906));
#454876=CARTESIAN_POINT('Ctrl Pts',(6.85589224549438,23.1662851718074,-6.22351333955115));
#454877=CARTESIAN_POINT('Ctrl Pts',(6.78286094776533,23.0948021011132,-4.9562223676805));
#454878=CARTESIAN_POINT('Ctrl Pts',(5.67821209556232,23.0233190304191,-4.33081775314232));
#454879=CARTESIAN_POINT('Ctrl Pts',(4.55396647939442,22.9518359597249,-4.92035346181854));
#454880=CARTESIAN_POINT('Ctrl Pts',(4.44022731365593,22.8803528890307,-6.18457385510163));
#454881=CARTESIAN_POINT('Ctrl Pts',(5.44103442081458,22.8088698183366,-6.96547480693525));
#454882=CARTESIAN_POINT('Ctrl Pts',(6.63978858397884,22.7373867476423,-6.54710119607151));
#454883=CARTESIAN_POINT('Ctrl Pts',(6.93756666268009,22.6659036769482,-5.31375101838665));
#454884=CARTESIAN_POINT('Ctrl Pts',(6.062815025304,22.594420606254,-4.39345456041576));
#454885=CARTESIAN_POINT('Ctrl Pts',(4.81438317658877,22.5229375355598,-4.63327178349906));
#454886=CARTESIAN_POINT('Ctrl Pts',(4.49968717359432,22.475282155097,-5.41441506110672));
#454887=CARTESIAN_POINT('Ctrl Pts',(4.54238608881333,22.4514544648656,-5.78519550592941));
#454888=CARTESIAN_POINT('Ctrl Pts',(4.75759373111246,26.1456366054031,-5.13891927882859));
#454889=CARTESIAN_POINT('Ctrl Pts',(4.58527827879321,26.1218089151717,-5.43810071821374));
#454890=CARTESIAN_POINT('Ctrl Pts',(4.5658640060888,26.0741535347089,-6.21688915400102));
#454891=CARTESIAN_POINT('Ctrl Pts',(5.53797444142439,26.0026704640147,-6.87864168992013));
#454892=CARTESIAN_POINT('Ctrl Pts',(6.61847524998255,25.9311873933205,-6.41815729896024));
#454893=CARTESIAN_POINT('Ctrl Pts',(6.81819229031504,25.8597043226264,-5.26158350250274));
#454894=CARTESIAN_POINT('Ctrl Pts',(5.95378694567247,25.7882212519322,-4.46643823922044));
#454895=CARTESIAN_POINT('Ctrl Pts',(4.81739664217988,25.716738181238,-4.7622984340844));
#454896=CARTESIAN_POINT('Ctrl Pts',(4.45007439859105,25.6452551105439,-5.87755291922296));
#454897=CARTESIAN_POINT('Ctrl Pts',(5.18840274984286,25.5737720398496,-6.79070035947327));
#454898=CARTESIAN_POINT('Ctrl Pts',(6.35591148837984,25.5022889691555,-6.66498514592993));
#454899=CARTESIAN_POINT('Ctrl Pts',(6.88295739545433,25.4308058984613,-5.61565848936591));
#454900=CARTESIAN_POINT('Ctrl Pts',(6.28666204489055,25.3593228277671,-4.60406196791575));
#454901=CARTESIAN_POINT('Ctrl Pts',(5.11334619850668,25.2878397570729,-4.55702527594187));
#454902=CARTESIAN_POINT('Ctrl Pts',(4.43798405643501,25.2163566863788,-5.51763314847689));
#454903=CARTESIAN_POINT('Ctrl Pts',(4.87933393703958,25.1448736156846,-6.60579479560106));
#454904=CARTESIAN_POINT('Ctrl Pts',(6.03303673742344,25.0733905449905,-6.82454899803953));
#454905=CARTESIAN_POINT('Ctrl Pts',(6.84208605608162,25.0019074742962,-5.97347744575397));
#454906=CARTESIAN_POINT('Ctrl Pts',(6.56524194061871,24.9304244036021,-4.83231952202541));
#454907=CARTESIAN_POINT('Ctrl Pts',(5.45614521253248,24.8589413329078,-4.44658873189996));
#454908=CARTESIAN_POINT('Ctrl Pts',(4.53093499038958,24.7874582622137,-5.16968614336583));
#454909=CARTESIAN_POINT('Ctrl Pts',(4.63727615158268,24.7159751915195,-6.33911995340987));
#454910=CARTESIAN_POINT('Ctrl Pts',(5.67774038144015,24.6444921208254,-6.88347096747714));
#454911=CARTESIAN_POINT('Ctrl Pts',(6.69906868632339,24.5730090501312,-6.30401230613993));
#454912=CARTESIAN_POINT('Ctrl Pts',(6.76553413784902,24.501525979437,-5.1316360027112));
#454913=CARTESIAN_POINT('Ctrl Pts',(5.8162420056622,24.4300429087428,-4.4404570855349));
#454914=CARTESIAN_POINT('Ctrl Pts',(4.72092066657002,24.3585598380486,-4.86372415598114));
#454915=CARTESIAN_POINT('Ctrl Pts',(4.48308844595715,24.2870767673545,-6.01364575549065));
#454916=CARTESIAN_POINT('Ctrl Pts',(5.32064394905434,24.2155936966602,-6.83667955068161));
#454917=CARTESIAN_POINT('Ctrl Pts',(6.46623035855224,24.1441106259661,-6.57877331548262));
#454918=CARTESIAN_POINT('Ctrl Pts',(6.87027718549015,24.0726275552719,-5.4762171877825));
#454919=CARTESIAN_POINT('Ctrl Pts',(6.16260228864267,24.0011444845778,-4.5391579116818));
#454920=CARTESIAN_POINT('Ctrl Pts',(4.99156766820889,23.9296614138835,-4.62611628030964));
#454921=CARTESIAN_POINT('Ctrl Pts',(4.43005910275823,23.8581783431894,-5.65742225312448));
#454922=CARTESIAN_POINT('Ctrl Pts',(4.99252303072782,23.7866952724952,-6.68820746419386));
#454923=CARTESIAN_POINT('Ctrl Pts',(6.16363770038041,23.715212201801,-6.77408077335862));
#454924=CARTESIAN_POINT('Ctrl Pts',(6.87044407409259,23.6437291311068,-5.83636609328009));
#454925=CARTESIAN_POINT('Ctrl Pts',(6.46537570391973,23.5722460604127,-4.73418498174874));
#454926=CARTESIAN_POINT('Ctrl Pts',(5.31955101057097,23.5007629897185,-4.47734003862102));
#454927=CARTESIAN_POINT('Ctrl Pts',(4.48275809327536,23.4292799190243,-5.30115015081045));
#454928=CARTESIAN_POINT('Ctrl Pts',(4.72165647802515,23.3577968483301,-6.4508497069919));
#454929=CARTESIAN_POINT('Ctrl Pts',(5.81736804855842,23.286313777636,-6.8731039905307));
#454930=CARTESIAN_POINT('Ctrl Pts',(6.76602226241636,23.2148307069418,-6.18104124059857));
#454931=CARTESIAN_POINT('Ctrl Pts',(6.69846478576951,23.1433476362476,-5.00873590166638));
#454932=CARTESIAN_POINT('Ctrl Pts',(5.67661126055156,23.0718645655534,-4.43020643614536));
#454933=CARTESIAN_POINT('Ctrl Pts',(4.63662978245479,23.0003814948593,-4.97555543184771));
#454934=CARTESIAN_POINT('Ctrl Pts',(4.5314155623581,22.9288984241651,-6.1450203373264));
#454935=CARTESIAN_POINT('Ctrl Pts',(5.45721045950911,22.8574153534709,-6.86739142284001));
#454936=CARTESIAN_POINT('Ctrl Pts',(6.56611594115257,22.7859322827767,-6.48037563201499));
#454937=CARTESIAN_POINT('Ctrl Pts',(6.84157504188551,22.7144492120825,-5.33946716650399));
#454938=CARTESIAN_POINT('Ctrl Pts',(6.0323875407531,22.6429661413884,-4.48814850723257));
#454939=CARTESIAN_POINT('Ctrl Pts',(4.87752780133468,22.5714830706942,-4.70999101793355));
#454940=CARTESIAN_POINT('Ctrl Pts',(4.58641880376449,22.5238276902314,-5.4325862664886));
#454941=CARTESIAN_POINT('Ctrl Pts',(4.62591736201901,22.5,-5.7755760807344));
#454942=CARTESIAN_POINT('Ctrl Pts',(4.92443355077908,25.6019615242271,-6.39006796800885));
#454943=CARTESIAN_POINT('Ctrl Pts',(5.02053320993752,25.5925650294346,-6.48712194011206));
#454944=CARTESIAN_POINT('Ctrl Pts',(5.13467106978717,25.5831685346421,-6.56580235206401));
#454945=CARTESIAN_POINT('Ctrl Pts',(5.25993281439039,25.5737720398497,-6.617556583841));
#454946=CARTESIAN_POINT('Ctrl Pts',(5.57757232935518,25.5499443496183,-6.74879528829216));
#454947=CARTESIAN_POINT('Ctrl Pts',(5.96674190886751,25.5261166593869,-6.70689021711105));
#454948=CARTESIAN_POINT('Ctrl Pts',(6.24916768313609,25.5022889691555,-6.51104990542648));
#454949=CARTESIAN_POINT('Ctrl Pts',(6.53159345740467,25.4784612789241,-6.31520959374192));
#454950=CARTESIAN_POINT('Ctrl Pts',(6.7072754264295,25.4546335886927,-5.96543404155392));
#454951=CARTESIAN_POINT('Ctrl Pts',(6.69573385251462,25.4308058984613,-5.62194684521822));
#454952=CARTESIAN_POINT('Ctrl Pts',(6.68419227859974,25.4069782082299,-5.27845964888252));
#454953=CARTESIAN_POINT('Ctrl Pts',(6.48542716174514,25.3831505179985,-4.94126080839914));
#454954=CARTESIAN_POINT('Ctrl Pts',(6.19049196225387,25.3593228277671,-4.76482193949513));
#454955=CARTESIAN_POINT('Ctrl Pts',(5.89555676276259,25.3354951375357,-4.58838307059113));
#454956=CARTESIAN_POINT('Ctrl Pts',(5.50445148063464,25.3116674473043,-4.5727041732665));
#454957=CARTESIAN_POINT('Ctrl Pts',(5.19633848255872,25.2878397570729,-4.72496603669335));
#454958=CARTESIAN_POINT('Ctrl Pts',(4.8882254844828,25.2640120668416,-4.87722790012021));
#454959=CARTESIAN_POINT('Ctrl Pts',(4.6631047704589,25.2401843766102,-5.19743052429855));
#454960=CARTESIAN_POINT('Ctrl Pts',(4.62410272688105,25.2163566863788,-5.53889211090841));
#454961=CARTESIAN_POINT('Ctrl Pts',(4.58896793348097,25.1948916323282,-5.84649605160076));
#454962=CARTESIAN_POINT('Ctrl Pts',(4.70487246063661,25.1734265782776,-6.17135209942283));
#454963=CARTESIAN_POINT('Ctrl Pts',(4.92254817630007,25.1519615242271,-6.39198798715976));
#454964=CARTESIAN_POINT('Origin',(5.65685387860011,26.,-5.65685387860012));
#454965=CARTESIAN_POINT('',(0.,0.,0.));
#454966=CARTESIAN_POINT('Origin',(0.,0.,0.));
#454967=CARTESIAN_POINT('',(0.00238312071812623,7.42232045465689,-3.44573997435601));
#454968=CARTESIAN_POINT('',(0.00358895744866569,7.2776795453431,-3.44504374594936));
#454969=CARTESIAN_POINT('',(-4.21523428266519E-16,0.,-3.442));
#454970=CARTESIAN_POINT('',(3.09271722244255,7.1,1.51078263890185));
#454971=CARTESIAN_POINT('Ctrl Pts',(0.00238312071812623,7.42232045465689,
-3.44573997435601));
#454972=CARTESIAN_POINT('Ctrl Pts',(0.134189165843592,7.41620645307186,
-3.44671132434039));
#454973=CARTESIAN_POINT('Ctrl Pts',(0.265886689822806,7.41009245148682,
-3.43980123267601));
#454974=CARTESIAN_POINT('Ctrl Pts',(0.396625140499449,7.40397844990179,
-3.42466879815526));
#454975=CARTESIAN_POINT('Ctrl Pts',(1.52472351508465,7.35122277462346,-3.29409608065693));
#454976=CARTESIAN_POINT('Ctrl Pts',(2.58141517031108,7.29846709934514,-2.55133811387537));
#454977=CARTESIAN_POINT('Ctrl Pts',(3.08712931628112,7.24571142406682,-1.5341055545258));
#454978=CARTESIAN_POINT('Ctrl Pts',(3.55272426880691,7.19714094937788,-0.597571844815975));
#454979=CARTESIAN_POINT('Ctrl Pts',(3.55129415105041,7.14857047468894,0.571614765840351));
#454980=CARTESIAN_POINT('Ctrl Pts',(3.09699338763787,7.1,1.51441171489142));
#454981=CARTESIAN_POINT('',(3.09271722244257,7.1,-1.51078263890182));
#454982=CARTESIAN_POINT('Origin',(0.,7.1,0.));
#454983=CARTESIAN_POINT('Ctrl Pts',(3.09271722244257,7.1,-1.51078263890182));
#454984=CARTESIAN_POINT('Ctrl Pts',(2.59193253573628,7.15275567527832,-2.53593700951191));
#454985=CARTESIAN_POINT('Ctrl Pts',(1.54584605382252,7.20551135055665,-3.28388805779909));
#454986=CARTESIAN_POINT('Ctrl Pts',(0.420315138273282,7.25826702583497,
-3.42154258483277));
#454987=CARTESIAN_POINT('Ctrl Pts',(0.282261170683799,7.26473786567101,
-3.43842684216513));
#454988=CARTESIAN_POINT('Ctrl Pts',(0.143011987085937,7.27120870550706,
-3.44612938419434));
#454989=CARTESIAN_POINT('Ctrl Pts',(0.00358895744866569,7.2776795453431,
-3.44504374594936));
#454990=CARTESIAN_POINT('Origin',(0.,0.,0.));
#454991=CARTESIAN_POINT('',(0.00119116194521041,8.42232045465689,-3.43683718515566));
#454992=CARTESIAN_POINT('',(0.00109290156775514,8.2776795453431,-3.43675318504777));
#454993=CARTESIAN_POINT('',(-4.21523428266519E-16,0.,-3.442));
#454994=CARTESIAN_POINT('Ctrl Pts',(0.00119116194521041,8.42232045465689,
-3.43683718515566));
#454995=CARTESIAN_POINT('Ctrl Pts',(0.49847441043924,8.39940717140846,-3.43838762583654));
#454996=CARTESIAN_POINT('Ctrl Pts',(0.995157371276851,8.37649388816004,
-3.33748454788281));
#454997=CARTESIAN_POINT('Ctrl Pts',(1.44316539496645,8.35358060491161,-3.1309843016151));
#454998=CARTESIAN_POINT('Ctrl Pts',(2.47466164819217,8.30082492963329,-2.65553694564786));
#454999=CARTESIAN_POINT('Ctrl Pts',(3.24812854171467,8.24806925435496,-1.62031136862869));
#455000=CARTESIAN_POINT('Ctrl Pts',(3.41165377002092,8.19531357907664,-0.496342238358058));
#455001=CARTESIAN_POINT('Ctrl Pts',(3.57517899832716,8.14255790379832,0.627626891912579));
#455002=CARTESIAN_POINT('Ctrl Pts',(3.12876256141716,8.08980222851999,1.84033957543469));
#455003=CARTESIAN_POINT('Ctrl Pts',(2.27548272011085,8.03704655324167,2.58998788073998));
#455004=CARTESIAN_POINT('Ctrl Pts',(1.42220287880454,7.98429087796335,3.33963618604527));
#455005=CARTESIAN_POINT('Ctrl Pts',(0.162059633101916,7.93153520268503,
3.62622011313374));
#455006=CARTESIAN_POINT('Ctrl Pts',(-0.931477912766307,7.8787795274067,
3.31935910596737));
#455007=CARTESIAN_POINT('Ctrl Pts',(-2.02501545863453,7.82602385212838,
3.01249809880101));
#455008=CARTESIAN_POINT('Ctrl Pts',(-2.95194730466835,7.77326817685005,
2.1121921573798));
#455009=CARTESIAN_POINT('Ctrl Pts',(-3.29068060623052,7.72051250157173,
1.02805540866212));
#455010=CARTESIAN_POINT('Ctrl Pts',(-3.62941390779269,7.66775682629341,
-0.0560813400555474));
#455011=CARTESIAN_POINT('Ctrl Pts',(-3.37994866488321,7.61500115101509,
-1.32404889606968));
#455012=CARTESIAN_POINT('Ctrl Pts',(-2.65546349645648,7.56224547573676,
-2.19883893996919));
#455013=CARTESIAN_POINT('Ctrl Pts',(-2.01494092437082,7.51560380204347,
-2.97224713846996));
#455014=CARTESIAN_POINT('Ctrl Pts',(-1.00312112425844,7.46896212835018,
-3.43832987012503));
#455015=CARTESIAN_POINT('Ctrl Pts',(0.00238312071812623,7.42232045465689,
-3.44573997435601));
#455016=CARTESIAN_POINT('Ctrl Pts',(0.00358895744866569,7.2776795453431,
-3.44504374594936));
#455017=CARTESIAN_POINT('Ctrl Pts',(-0.993680662435879,7.32396438078538,
-3.43727835709852));
#455018=CARTESIAN_POINT('Ctrl Pts',(-1.99984477020885,7.37024921622766,
-2.97988315053305));
#455019=CARTESIAN_POINT('Ctrl Pts',(-2.6411222941201,7.41653405166994,-2.21687640500152));
#455020=CARTESIAN_POINT('Ctrl Pts',(-3.3720534617795,7.46928972694826,-1.34719769235643));
#455021=CARTESIAN_POINT('Ctrl Pts',(-3.6289404479136,7.52204540222659,-0.080482261286085));
#455022=CARTESIAN_POINT('Ctrl Pts',(-3.29723843930749,7.57480107750491,
1.00601810569489));
#455023=CARTESIAN_POINT('Ctrl Pts',(-2.96553643070138,7.62755675278323,
2.09251847267586));
#455024=CARTESIAN_POINT('Ctrl Pts',(-2.04524542735508,7.68031242806155,
2.99880377556747));
#455025=CARTESIAN_POINT('Ctrl Pts',(-0.953932543642956,7.73306810333988,
3.31295667324589));
#455026=CARTESIAN_POINT('Ctrl Pts',(0.13738034006917,7.7858237786182,3.62710957092432));
#455027=CARTESIAN_POINT('Ctrl Pts',(1.39971510414711,7.83857945389653,3.34913006338957));
#455028=CARTESIAN_POINT('Ctrl Pts',(2.25808828818259,7.89133512917485,2.60526729131064));
#455029=CARTESIAN_POINT('Ctrl Pts',(3.11646147221806,7.94409080445317,1.86140451923172));
#455030=CARTESIAN_POINT('Ctrl Pts',(3.57087307621107,7.99684647973149,0.651658482608627));
#455031=CARTESIAN_POINT('Ctrl Pts',(3.41487509938555,8.04960215500982,-0.473400457015574));
#455032=CARTESIAN_POINT('Ctrl Pts',(3.25887712256003,8.10235783028814,-1.59845939663978));
#455033=CARTESIAN_POINT('Ctrl Pts',(2.49246956491597,8.15511350556647,-2.6388312392651));
#455034=CARTESIAN_POINT('Ctrl Pts',(1.4642134312474,8.20786918084479,-3.12119802101246));
#455035=CARTESIAN_POINT('Ctrl Pts',(1.01065758087162,8.23113930234422,-3.3339662883));
#455036=CARTESIAN_POINT('Ctrl Pts',(0.506155841458834,8.25440942384366,
-3.43816774821673));
#455037=CARTESIAN_POINT('Ctrl Pts',(0.00109290156775514,8.2776795453431,
-3.43675318504777));
#455038=CARTESIAN_POINT('Origin',(0.,0.,0.));
#455039=CARTESIAN_POINT('',(-0.00309368505836849,9.42232045465689,-3.44152090478281));
#455040=CARTESIAN_POINT('',(-0.00309581765146611,9.2776795453431,-3.4417505667627));
#455041=CARTESIAN_POINT('',(-4.21523428266519E-16,0.,-3.442));
#455042=CARTESIAN_POINT('Ctrl Pts',(-0.00309368505836849,9.42232045465689,
-3.44152090478281));
#455043=CARTESIAN_POINT('Ctrl Pts',(0.855820397317136,9.38260788974507,
-3.43381237529938));
#455044=CARTESIAN_POINT('Ctrl Pts',(1.71995527738355,9.34289532483326,-3.10781983641605));
#455045=CARTESIAN_POINT('Ctrl Pts',(2.34637752785182,9.30318275992144,-2.5259247880675));
#455046=CARTESIAN_POINT('Ctrl Pts',(3.17854057010811,9.25042708464312,-1.75291336750315));
#455047=CARTESIAN_POINT('Ctrl Pts',(3.5912009188089,9.19767140936479,-0.528298714120453));
#455048=CARTESIAN_POINT('Ctrl Pts',(3.39659380113874,9.14491573408646,0.590705393077353));
#455049=CARTESIAN_POINT('Ctrl Pts',(3.20198668346858,9.09216005880813,1.70970950027516));
#455050=CARTESIAN_POINT('Ctrl Pts',(2.40011209942749,9.03940438352981,2.72310306128807));
#455051=CARTESIAN_POINT('Ctrl Pts',(1.35583137668917,8.98664870825149,3.16978005845081));
#455052=CARTESIAN_POINT('Ctrl Pts',(0.311550653950845,8.93389303297317,
3.61645705561355));
#455053=CARTESIAN_POINT('Ctrl Pts',(-0.975136207484709,8.88113735769485,
3.49641748892612));
#455054=CARTESIAN_POINT('Ctrl Pts',(-1.91876999931101,8.82838168241653,
2.86428111708987));
#455055=CARTESIAN_POINT('Ctrl Pts',(-2.86240379113731,8.7756260071382,2.23214474525363));
#455056=CARTESIAN_POINT('Ctrl Pts',(-3.46298451335436,8.72287033185987,
1.08791156826856));
#455057=CARTESIAN_POINT('Ctrl Pts',(-3.44724434922051,8.67011465658155,
-0.0477797400067174));
#455058=CARTESIAN_POINT('Ctrl Pts',(-3.43150418508666,8.61735898130322,
-1.183471048282));
#455059=CARTESIAN_POINT('Ctrl Pts',(-2.79944313460191,8.56460330602491,
-2.31062048784749));
#455060=CARTESIAN_POINT('Ctrl Pts',(-1.83864980289507,8.51184763074659,
-2.91636064017258));
#455061=CARTESIAN_POINT('Ctrl Pts',(-1.29515621451355,8.48200523871669,
-3.25901069627681));
#455062=CARTESIAN_POINT('Ctrl Pts',(-0.646473404086736,8.45216284668679,
-3.43481788228595));
#455063=CARTESIAN_POINT('Ctrl Pts',(0.00119116194521041,8.42232045465689,
-3.43683718515566));
#455064=CARTESIAN_POINT('Ctrl Pts',(0.00109290156775514,8.2776795453431,
-3.43675318504777));
#455065=CARTESIAN_POINT('Ctrl Pts',(-0.638871976838291,8.30716509912199,
-3.43496079310031));
#455066=CARTESIAN_POINT('Ctrl Pts',(-1.27973788536319,8.33665065290087,
-3.26359759443701));
#455067=CARTESIAN_POINT('Ctrl Pts',(-1.81900325993667,8.36613620667976,
-2.92866660332892));
#455068=CARTESIAN_POINT('Ctrl Pts',(-2.78385910775911,8.41889188195808,
-2.32940668302862));
#455069=CARTESIAN_POINT('Ctrl Pts',(-3.42346609371094,8.4716475572364,-1.20652512155862));
#455070=CARTESIAN_POINT('Ctrl Pts',(-3.44683967457762,8.52440323251473,
-0.0709631335329957));
#455071=CARTESIAN_POINT('Ctrl Pts',(-3.4702132554443,8.57715890779305,1.06459885449263));
#455072=CARTESIAN_POINT('Ctrl Pts',(-2.87735343122583,8.62991458307138,
2.21284126907387));
#455073=CARTESIAN_POINT('Ctrl Pts',(-1.93799541836559,8.6826702583497,2.85130935660359));
#455074=CARTESIAN_POINT('Ctrl Pts',(-0.998637405505343,8.73542593362803,
3.4897774441333));
#455075=CARTESIAN_POINT('Ctrl Pts',(0.287218795996676,8.78818160890635,
3.6184712046115));
#455076=CARTESIAN_POINT('Ctrl Pts',(1.33448180904785,8.84093728418467,3.17882887749084));
#455077=CARTESIAN_POINT('Ctrl Pts',(2.38174482209902,8.89369295946299,2.73918655037018));
#455078=CARTESIAN_POINT('Ctrl Pts',(3.19041464669936,8.94644863474132,1.73120813565067));
#455079=CARTESIAN_POINT('Ctrl Pts',(3.39254330235197,8.99920431001964,0.613537900451479));
#455080=CARTESIAN_POINT('Ctrl Pts',(3.59467195800459,9.05195998529796,-0.504132334747713));
#455081=CARTESIAN_POINT('Ctrl Pts',(3.19025944470949,9.10471566057628,-1.73149439042658));
#455082=CARTESIAN_POINT('Ctrl Pts',(2.36331494236584,9.1574713358546,-2.51008553228953));
#455083=CARTESIAN_POINT('Ctrl Pts',(1.73522758526385,9.19754073901743,-3.1014471668004));
#455084=CARTESIAN_POINT('Ctrl Pts',(0.863388912503553,9.23761014218027,
-3.43392070879517));
#455085=CARTESIAN_POINT('Ctrl Pts',(-0.0030958176514661,9.2776795453431,
-3.4417505667627));
#455086=CARTESIAN_POINT('Origin',(0.,0.,0.));
#455087=CARTESIAN_POINT('',(0.00142507496518784,10.4223204546569,-3.44683866470506));
#455088=CARTESIAN_POINT('',(0.00154693548059185,10.2776795453431,-3.44670349103507));
#455089=CARTESIAN_POINT('',(-4.21523428266519E-16,0.,-3.442));
#455090=CARTESIAN_POINT('Ctrl Pts',(0.00142507496518784,10.4223204546569,
-3.44683866470506));
#455091=CARTESIAN_POINT('Ctrl Pts',(0.0823396048270201,10.41856428336,-3.44726368601611));
#455092=CARTESIAN_POINT('Ctrl Pts',(0.163226312415324,10.4148081120631,
-3.44465965322517));
#455093=CARTESIAN_POINT('Ctrl Pts',(0.243891972020051,10.4110519407662,
-3.43893878754763));
#455094=CARTESIAN_POINT('Ctrl Pts',(1.37684651744847,10.3582962654879,-3.35858884923533));
#455095=CARTESIAN_POINT('Ctrl Pts',(2.46619627771366,10.3055405902096,-2.66340033058106));
#455096=CARTESIAN_POINT('Ctrl Pts',(3.01627446688699,10.2527849149312,-1.6696920751257));
#455097=CARTESIAN_POINT('Ctrl Pts',(3.56635265606032,10.2000292396529,-0.675983819670343));
#455098=CARTESIAN_POINT('Ctrl Pts',(3.5771592741418,10.1472735643746,0.616244172586106));
#455099=CARTESIAN_POINT('Ctrl Pts',(3.04377719383542,10.0945178890963,1.61901317285293));
#455100=CARTESIAN_POINT('Ctrl Pts',(2.51039511352904,10.041762213818,2.62178217311977));
#455101=CARTESIAN_POINT('Ctrl Pts',(1.43282433483482,9.98900653853964,3.33509218139697));
#455102=CARTESIAN_POINT('Ctrl Pts',(0.301372047598186,9.93625086326132,
3.43437886338635));
#455103=CARTESIAN_POINT('Ctrl Pts',(-0.830080239638436,9.88349518798299,
3.53366554537574));
#455104=CARTESIAN_POINT('Ctrl Pts',(-2.01541403541746,9.83073951270466,
3.0189289010773));
#455105=CARTESIAN_POINT('Ctrl Pts',(-2.71528867421011,9.77798383742634,
2.12438008348235));
#455106=CARTESIAN_POINT('Ctrl Pts',(-3.41516331300278,9.72522816214802,
1.22983126588738));
#455107=CARTESIAN_POINT('Ctrl Pts',(-3.62957879480908,9.6724724868697,-0.0445297250041106));
#455108=CARTESIAN_POINT('Ctrl Pts',(-3.26097365394768,9.61971681159138,
-1.11885386515457));
#455109=CARTESIAN_POINT('Ctrl Pts',(-2.89236851308627,9.56696113631306,
-2.19317800530503));
#455110=CARTESIAN_POINT('Ctrl Pts',(-1.94074274955717,9.51420546103472,
-3.06746529471446));
#455111=CARTESIAN_POINT('Ctrl Pts',(-0.839096999886727,9.4614497857564,
-3.34390484554616));
#455112=CARTESIAN_POINT('Ctrl Pts',(-0.566730339391244,9.44840667538989,
-3.41225069747854));
#455113=CARTESIAN_POINT('Ctrl Pts',(-0.285193599698565,9.43536356502339,
-3.44405267781331));
#455114=CARTESIAN_POINT('Ctrl Pts',(-0.00309368505836849,9.42232045465689,
-3.44152090478281));
#455115=CARTESIAN_POINT('Ctrl Pts',(-0.0030958176514661,9.2776795453431,
-3.4417505667627));
#455116=CARTESIAN_POINT('Ctrl Pts',(-0.277431350576604,9.29036581745859,
-3.44422955823652));
#455117=CARTESIAN_POINT('Ctrl Pts',(-0.551230202762694,9.30305208957409,
-3.4141661739107));
#455118=CARTESIAN_POINT('Ctrl Pts',(-0.816586564771066,9.31573836168958,
-3.34947354022971));
#455119=CARTESIAN_POINT('Ctrl Pts',(-1.92006707817213,9.36849403696791,
-3.08045017825992));
#455120=CARTESIAN_POINT('Ctrl Pts',(-2.87755161358206,9.42124971224623,
-2.21258322627329));
#455121=CARTESIAN_POINT('Ctrl Pts',(-3.25337446224197,9.47400538752455,
-1.14076255284959));
#455122=CARTESIAN_POINT('Ctrl Pts',(-3.62919731090188,9.52676106280287,
-0.0689418794258828));
#455123=CARTESIAN_POINT('Ctrl Pts',(-3.42335847281178,9.5795167380812,1.2068325154349));
#455124=CARTESIAN_POINT('Ctrl Pts',(-2.72951655849602,9.63227241335952,
2.10606865285624));
#455125=CARTESIAN_POINT('Ctrl Pts',(-2.03567464418025,9.68502808863784,
3.00530479027758));
#455126=CARTESIAN_POINT('Ctrl Pts',(-0.853829653638802,9.73778376391616,
3.52800267025948));
#455127=CARTESIAN_POINT('Ctrl Pts',(0.278264995679193,9.79053943919449,
3.43632860190599));
#455128=CARTESIAN_POINT('Ctrl Pts',(1.41035964499719,9.84329511447281,3.3446545335525));
#455129=CARTESIAN_POINT('Ctrl Pts',(2.49270395309174,9.89605078975114,2.63860851686363));
#455130=CARTESIAN_POINT('Ctrl Pts',(3.03281882209306,9.94880646502946,1.63944972893749));
#455131=CARTESIAN_POINT('Ctrl Pts',(3.57293369109439,10.0015621403078,0.640290941011352));
#455132=CARTESIAN_POINT('Ctrl Pts',(3.5708191210025,10.0543178155861,-0.651980618152043));
#455133=CARTESIAN_POINT('Ctrl Pts',(3.02743720280062,10.1070734908644,-1.6493664187819));
#455134=CARTESIAN_POINT('Ctrl Pts',(2.48405528459874,10.1598291661428,-2.64675221941176));
#455135=CARTESIAN_POINT('Ctrl Pts',(1.39940601828685,10.2125848414211,-3.34925226150807));
#455136=CARTESIAN_POINT('Ctrl Pts',(0.267017438351514,10.2653405166994,
-3.43722086185585));
#455137=CARTESIAN_POINT('Ctrl Pts',(0.178732623179784,10.2694535262473,
-3.44407918925355));
#455138=CARTESIAN_POINT('Ctrl Pts',(0.0901576348521517,10.2735665357952,
-3.44720221938116));
#455139=CARTESIAN_POINT('Ctrl Pts',(0.00154693548059185,10.2776795453431,
-3.44670349103507));
#455140=CARTESIAN_POINT('Origin',(0.,0.,0.));
#455141=CARTESIAN_POINT('',(0.00190492198109293,11.4223204546569,-3.43753765796313));
#455142=CARTESIAN_POINT('',(0.00180381072558041,11.2776795453431,-3.43741114558699));
#455143=CARTESIAN_POINT('',(-4.21523428266519E-16,0.,-3.442));
#455144=CARTESIAN_POINT('Ctrl Pts',(0.00190492198109293,11.4223204546569,
-3.43753765796313));
#455145=CARTESIAN_POINT('Ctrl Pts',(0.447788094031521,11.4017650016966,
-3.43979577453365));
#455146=CARTESIAN_POINT('Ctrl Pts',(0.892886862129609,11.3812095487363,
-3.359223800869));
#455147=CARTESIAN_POINT('Ctrl Pts',(1.30262881999811,11.3606540957761,-3.19201212953924));
#455148=CARTESIAN_POINT('Ctrl Pts',(2.35423365298245,11.3078984204977,-2.76286251885132));
#455149=CARTESIAN_POINT('Ctrl Pts',(3.17294499666008,11.2551427452194,-1.76302167864693));
#455150=CARTESIAN_POINT('Ctrl Pts',(3.38623968972603,11.2023870699411,-0.647428792793382));
#455151=CARTESIAN_POINT('Ctrl Pts',(3.59953438279198,11.1496313946627,0.468164093060168));
#455152=CARTESIAN_POINT('Ctrl Pts',(3.20741242524624,11.0968757193844,1.69950902456289));
#455153=CARTESIAN_POINT('Ctrl Pts',(2.38829385790398,11.0441200441061,2.48632977012805));
#455154=CARTESIAN_POINT('Ctrl Pts',(1.56917529056172,10.9913643688278,3.27315051569321));
#455155=CARTESIAN_POINT('Ctrl Pts',(0.323060113422929,10.9386086935495,
3.61544707532083));
#455156=CARTESIAN_POINT('Ctrl Pts',(-0.783054809091477,10.8858530182711,
3.35747054250294));
#455157=CARTESIAN_POINT('Ctrl Pts',(-1.88916973160589,10.8330973429928,
3.09949400968504));
#455158=CARTESIAN_POINT('Ctrl Pts',(-2.85528439949591,10.7803416677145,
2.24124438442165));
#455159=CARTESIAN_POINT('Ctrl Pts',(-3.24180542797521,10.7275859924362,
1.17323520496348));
#455160=CARTESIAN_POINT('Ctrl Pts',(-3.62832645645451,10.6748303171578,
0.105226025505309));
#455161=CARTESIAN_POINT('Ctrl Pts',(-3.43525384552309,10.6220746418795,
-1.17254270814764));
#455162=CARTESIAN_POINT('Ctrl Pts',(-2.75043787476155,10.5693189666012,
-2.07867139598895));
#455163=CARTESIAN_POINT('Ctrl Pts',(-2.11438037556645,10.5203194626198,
-2.92028428433378));
#455164=CARTESIAN_POINT('Ctrl Pts',(-1.05411033988768,10.4713199586383,
-3.44129423348055));
#455165=CARTESIAN_POINT('Ctrl Pts',(0.00142507496518784,10.4223204546569,
-3.44683866470506));
#455166=CARTESIAN_POINT('Ctrl Pts',(0.00154693548059185,10.2776795453431,
-3.44670349103507));
#455167=CARTESIAN_POINT('Ctrl Pts',(-1.04641091131577,10.3263222110735,
-3.44080526105365));
#455168=CARTESIAN_POINT('Ctrl Pts',(-2.09936355514549,10.3749648768039,
-2.92834249274513));
#455169=CARTESIAN_POINT('Ctrl Pts',(-2.73639437423741,10.4236075425344,
-2.09712454699236));
#455170=CARTESIAN_POINT('Ctrl Pts',(-3.42728971333225,10.4763632178127,
-1.19562247318185));
#455171=CARTESIAN_POINT('Ctrl Pts',(-3.62895249796314,10.529118893091,0.0808188330383952));
#455172=CARTESIAN_POINT('Ctrl Pts',(-3.24962381232915,10.5818745683694,
1.15140376969445));
#455173=CARTESIAN_POINT('Ctrl Pts',(-2.87029512669516,10.6346302436477,
2.2219887063505));
#455174=CARTESIAN_POINT('Ctrl Pts',(-1.90997497079629,10.687385918926,3.08671727344235));
#455175=CARTESIAN_POINT('Ctrl Pts',(-0.805620163128287,10.7401415942043,
3.35212793737453));
#455176=CARTESIAN_POINT('Ctrl Pts',(0.298734644539725,10.7928972694826,
3.61753860130671));
#455177=CARTESIAN_POINT('Ctrl Pts',(1.54712410397688,10.845652944761,3.28363136207922));
#455178=CARTESIAN_POINT('Ctrl Pts',(2.37151652795347,10.8984086200393,2.50233788892262));
#455179=CARTESIAN_POINT('Ctrl Pts',(3.19590895193005,10.9511642953176,1.72104441576602));
#455180=CARTESIAN_POINT('Ctrl Pts',(3.59630434044607,11.0039199705959,0.49236470868034));
#455181=CARTESIAN_POINT('Ctrl Pts',(3.39051814454231,11.0566756458742,-0.62463770922453));
#455182=CARTESIAN_POINT('Ctrl Pts',(3.18473194863855,11.1094313211526,-1.7416401271294));
#455183=CARTESIAN_POINT('Ctrl Pts',(2.37276416831501,11.1621869964309,-2.74696525585346));
#455184=CARTESIAN_POINT('Ctrl Pts',(1.32406956584938,11.2149426717092,-3.18317849638681));
#455185=CARTESIAN_POINT('Ctrl Pts',(0.908368187698639,11.2358549629205,
-3.35609294147976));
#455186=CARTESIAN_POINT('Ctrl Pts',(0.455469431275188,11.2567672541318,
-3.43958165106471));
#455187=CARTESIAN_POINT('Ctrl Pts',(0.00180381072558041,11.2776795453431,
-3.43741114558699));
#455188=CARTESIAN_POINT('Origin',(0.,0.,0.));
#455189=CARTESIAN_POINT('',(-0.00294480074326642,12.4223204546569,-3.44006114644949));
#455190=CARTESIAN_POINT('',(-0.00298197493165331,12.2776795453431,-3.44027416367858));
#455191=CARTESIAN_POINT('',(-4.21523428266519E-16,0.,-3.442));
#455192=CARTESIAN_POINT('Ctrl Pts',(-0.00294480074326642,12.4223204546569,
-3.44006114644949));
#455193=CARTESIAN_POINT('Ctrl Pts',(0.805845936783274,12.3849657200332,
-3.43339405105818));
#455194=CARTESIAN_POINT('Ctrl Pts',(1.61886853933875,12.3476109854095,-3.14830562263054));
#455195=CARTESIAN_POINT('Ctrl Pts',(2.23183508531966,12.3102562507859,-2.62767871509275));
#455196=CARTESIAN_POINT('Ctrl Pts',(3.09752090485561,12.2575005755075,-1.89240313752745));
#455197=CARTESIAN_POINT('Ctrl Pts',(3.56418295590633,12.2047449002292,-0.687331977828459));
#455198=CARTESIAN_POINT('Ctrl Pts',(3.41948459040631,12.1519892249509,0.439213403454665));
#455199=CARTESIAN_POINT('Ctrl Pts',(3.2747862249063,12.0992335496726,1.56575878473779));
#455200=CARTESIAN_POINT('Ctrl Pts',(2.51872744285554,12.0464778743942,2.61377838760505));
#455201=CARTESIAN_POINT('Ctrl Pts',(1.49532376292829,11.9937221991159,3.10641113213925));
#455202=CARTESIAN_POINT('Ctrl Pts',(0.471920083001049,11.9409665238376,
3.59904387667346));
#455203=CARTESIAN_POINT('Ctrl Pts',(-0.81882849480268,11.8882108485593,
3.53628976287462));
#455204=CARTESIAN_POINT('Ctrl Pts',(-1.78961639050565,11.835455173281,2.94670264069157));
#455205=CARTESIAN_POINT('Ctrl Pts',(-2.76040428620862,11.7826994980026,
2.35711551850853));
#455206=CARTESIAN_POINT('Ctrl Pts',(-3.41123149981084,11.7299438227243,
1.24069538794127));
#455207=CARTESIAN_POINT('Ctrl Pts',(-3.44596409730449,11.677188147446,0.105426362666967));
#455208=CARTESIAN_POINT('Ctrl Pts',(-3.48069669479813,11.6244324721677,
-1.02984266260733));
#455209=CARTESIAN_POINT('Ctrl Pts',(-2.89933467618322,11.5716767968893,
-2.18396058258869));
#455210=CARTESIAN_POINT('Ctrl Pts',(-1.96640450573024,11.518921121611,-2.83179035199364));
#455211=CARTESIAN_POINT('Ctrl Pts',(-1.39697650130591,11.486720899293,-3.22720302539858));
#455212=CARTESIAN_POINT('Ctrl Pts',(-0.696573350214575,11.4545206769749,
-3.43400030679256));
#455213=CARTESIAN_POINT('Ctrl Pts',(0.00190492198109293,11.4223204546569,
-3.43753765796313));
#455214=CARTESIAN_POINT('Ctrl Pts',(0.00180381072558041,11.2776795453431,
-3.43741114558699));
#455215=CARTESIAN_POINT('Ctrl Pts',(-0.688997997991005,11.3095229294101,
-3.43410609216896));
#455216=CARTESIAN_POINT('Ctrl Pts',(-1.38157789620168,11.3413663134772,
-3.23218730108958));
#455217=CARTESIAN_POINT('Ctrl Pts',(-1.94731304484871,11.3732096975442,
-2.8449529803043));
#455218=CARTESIAN_POINT('Ctrl Pts',(-2.88457962847346,11.4259653728225,
-2.20341287134578));
#455219=CARTESIAN_POINT('Ctrl Pts',(-3.47369137111525,11.4787210481008,
-1.05323130108607));
#455220=CARTESIAN_POINT('Ctrl Pts',(-3.44659559399869,11.5314767233792,
0.0822457700539528));
#455221=CARTESIAN_POINT('Ctrl Pts',(-3.41949981688212,11.5842323986575,
1.21772284119398));
#455222=CARTESIAN_POINT('Ctrl Pts',(-2.7761965200072,11.6369880739358,2.33849541321433));
#455223=CARTESIAN_POINT('Ctrl Pts',(-1.80939616804833,11.6897437492141,
2.93459896103683));
#455224=CARTESIAN_POINT('Ctrl Pts',(-0.842595816089467,11.7424994244925,
3.53070250885933));
#455225=CARTESIAN_POINT('Ctrl Pts',(0.447701590953337,11.7952550997708,
3.60213703248398));
#455226=CARTESIAN_POINT('Ctrl Pts',(1.47439576108161,11.8480107750491,3.1163989947945));
#455227=CARTESIAN_POINT('Ctrl Pts',(2.50108993120989,11.9007664503274,2.63066095710503));
#455228=CARTESIAN_POINT('Ctrl Pts',(3.26418086442365,11.9535221256058,1.58775035810145));
#455229=CARTESIAN_POINT('Ctrl Pts',(3.41645333163715,12.0062778008841,0.462203621635271));
#455230=CARTESIAN_POINT('Ctrl Pts',(3.56872579885066,12.0590334761624,-0.663343114830906));
#455231=CARTESIAN_POINT('Ctrl Pts',(3.11017980006393,12.1117891514407,-1.87152598875967));
#455232=CARTESIAN_POINT('Ctrl Pts',(2.24945908542769,12.164544826719,-2.61260777348285));
#455233=CARTESIAN_POINT('Ctrl Pts',(1.63418628712663,12.2022563995937,-3.14235854594947));
#455234=CARTESIAN_POINT('Ctrl Pts',(0.813406931721569,12.2399679724684,
-3.43342614695064));
#455235=CARTESIAN_POINT('Ctrl Pts',(-0.00298197493165331,12.2776795453431,
-3.44027416367858));
#455236=CARTESIAN_POINT('Origin',(0.,0.,0.));
#455237=CARTESIAN_POINT('',(0.000551455541893276,13.4223204546569,-3.44746546819473));
#455238=CARTESIAN_POINT('',(0.000689626542513858,13.2776795453431,-3.44740402518832));
#455239=CARTESIAN_POINT('',(-4.21523428266519E-16,0.,-3.442));
#455240=CARTESIAN_POINT('Ctrl Pts',(0.000551455541893276,13.4223204546569,
-3.44746546819473));
#455241=CARTESIAN_POINT('Ctrl Pts',(0.0306595665508508,13.4209221136481,
-3.44753286857709));
#455242=CARTESIAN_POINT('Ctrl Pts',(0.0607660228121984,13.4195237726394,
-3.44717233639977));
#455243=CARTESIAN_POINT('Ctrl Pts',(0.0908610660097724,13.4181254316307,
-3.44637890430166));
#455244=CARTESIAN_POINT('Ctrl Pts',(1.22626674780566,13.3653697563523,-3.41644482823507));
#455245=CARTESIAN_POINT('Ctrl Pts',(2.34542762737645,13.312614081074,-2.77034197086878));
#455246=CARTESIAN_POINT('Ctrl Pts',(2.93911251532146,13.2598584057957,-1.80205463313301));
#455247=CARTESIAN_POINT('Ctrl Pts',(3.53279740326646,13.2071027305174,-0.833767295397236));
#455248=CARTESIAN_POINT('Ctrl Pts',(3.60100629958569,13.154347055239,0.456704522708029));
#455249=CARTESIAN_POINT('Ctrl Pts',(3.11270336662071,13.1015913799607,1.48218117207498));
#455250=CARTESIAN_POINT('Ctrl Pts',(2.62440043365574,13.0488357046824,2.50765782144194));
#455251=CARTESIAN_POINT('Ctrl Pts',(1.57958567140657,12.9960800294041,3.26813930207059));
#455252=CARTESIAN_POINT('Ctrl Pts',(0.453661919259777,12.9433243541257,
3.41759771506665));
#455253=CARTESIAN_POINT('Ctrl Pts',(-0.672261832887001,12.8905686788474,
3.5670561280627));
#455254=CARTESIAN_POINT('Ctrl Pts',(-1.8792945749314,12.8378130035691,3.10549147342618));
#455255=CARTESIAN_POINT('Ctrl Pts',(-2.61822240311915,12.7850573282908,
2.24292102527514));
#455256=CARTESIAN_POINT('Ctrl Pts',(-3.3571502313069,12.7323016530125,1.38035057712408));
#455257=CARTESIAN_POINT('Ctrl Pts',(-3.62797314563799,12.6795459777341,
0.116774335458481));
#455258=CARTESIAN_POINT('Ctrl Pts',(-3.30746357785179,12.6267903024558,
-0.972865848260009));
#455259=CARTESIAN_POINT('Ctrl Pts',(-2.9869540100656,12.5740346271775,-2.0625060319785));
#455260=CARTESIAN_POINT('Ctrl Pts',(-2.07511196016212,12.5212789518992,
-2.97821015774988));
#455261=CARTESIAN_POINT('Ctrl Pts',(-0.986836141199789,12.4685232766208,
-3.30332222291977));
#455262=CARTESIAN_POINT('Ctrl Pts',(-0.669136268810636,12.4531223359662,
-3.39823204248659));
#455263=CARTESIAN_POINT('Ctrl Pts',(-0.336400205423888,12.4377213953115,
-3.44280991555452));
#455264=CARTESIAN_POINT('Ctrl Pts',(-0.00294480074326642,12.4223204546569,
-3.44006114644949));
#455265=CARTESIAN_POINT('Ctrl Pts',(-0.00298197493165331,12.2776795453431,
-3.44027416367858));
#455266=CARTESIAN_POINT('Ctrl Pts',(-0.328660205158152,12.2927236477467,
-3.44300601114777));
#455267=CARTESIAN_POINT('Ctrl Pts',(-0.653639733070962,12.3077677501504,
-3.40050674618356));
#455268=CARTESIAN_POINT('Ctrl Pts',(-0.964595131274779,12.322811852554,
-3.3098854644577));
#455269=CARTESIAN_POINT('Ctrl Pts',(-2.05503320285527,12.3755675278323,
-2.9921006751918));
#455270=CARTESIAN_POINT('Ctrl Pts',(-2.97301391553049,12.4283232031107,
-2.08255040114239));
#455271=CARTESIAN_POINT('Ctrl Pts',(-3.30084539334331,12.481078878389,-0.995090570900892));
#455272=CARTESIAN_POINT('Ctrl Pts',(-3.62867687115614,12.5338345536673,
0.0923692593406071));
#455273=CARTESIAN_POINT('Ctrl Pts',(-3.36635911410655,12.5865902289456,
1.35773864577421));
#455274=CARTESIAN_POINT('Ctrl Pts',(-2.63324974540749,12.6393459042239,
2.22525983502552));
#455275=CARTESIAN_POINT('Ctrl Pts',(-1.90014037670843,12.6921015795023,
3.09278102427684));
#455276=CARTESIAN_POINT('Ctrl Pts',(-0.69623939635987,12.7448572547806,
3.56245401634588));
#455277=CARTESIAN_POINT('Ctrl Pts',(0.430664280185392,12.7976129300589,
3.42057214995318));
#455278=CARTESIAN_POINT('Ctrl Pts',(1.55756795673064,12.8503686053373,3.27869028356049));
#455279=CARTESIAN_POINT('Ctrl Pts',(2.60747432947258,12.9031242806156,2.52525355870611));
#455280=CARTESIAN_POINT('Ctrl Pts',(3.10266381641936,12.9558799558939,1.50308442778917));
#455281=CARTESIAN_POINT('Ctrl Pts',(3.59785330336615,13.0086356311722,0.480915296872219));
#455282=CARTESIAN_POINT('Ctrl Pts',(3.53832590451775,13.0613913064505,-0.809986240107284));
#455283=CARTESIAN_POINT('Ctrl Pts',(2.95116727689351,13.1141469817289,-1.78224500528432));
#455284=CARTESIAN_POINT('Ctrl Pts',(2.36400864926926,13.1669026570072,-2.75450377046135));
#455285=CARTESIAN_POINT('Ctrl Pts',(1.24921879286915,13.2196583322855,-3.40811976383592));
#455286=CARTESIAN_POINT('Ctrl Pts',(0.114040028051502,13.2724140075638,
-3.44569012365563));
#455287=CARTESIAN_POINT('Ctrl Pts',(0.0762726748025813,13.2741691868236,
-3.44694008806209));
#455288=CARTESIAN_POINT('Ctrl Pts',(0.038482753268587,13.2759243660833,
-3.44750815752882));
#455289=CARTESIAN_POINT('Ctrl Pts',(0.000689626542513858,13.2776795453431,
-3.44740402518832));
#455290=CARTESIAN_POINT('Origin',(0.,0.,0.));
#455291=CARTESIAN_POINT('',(0.00248787001207174,14.4223204546569,-3.43854544754782));
#455292=CARTESIAN_POINT('',(0.00241009727763581,14.2776795453431,-3.43837553245923));
#455293=CARTESIAN_POINT('',(-4.21523428266519E-16,0.,-3.442));
#455294=CARTESIAN_POINT('Ctrl Pts',(0.00248787001207174,14.4223204546569,
-3.43854544754782));
#455295=CARTESIAN_POINT('Ctrl Pts',(0.396934926497801,14.4041228319848,
-3.44120536324132));
#455296=CARTESIAN_POINT('Ctrl Pts',(0.790562293081628,14.3859252093126,
-3.37850410109726));
#455297=CARTESIAN_POINT('Ctrl Pts',(1.15952320178319,14.3677275866405,-3.24673520366357));
#455298=CARTESIAN_POINT('Ctrl Pts',(2.22915643028483,14.3149719113622,-2.8647316150609));
#455299=CARTESIAN_POINT('Ctrl Pts',(3.09148175965367,14.2622162360838,-1.90225285493972));
#455300=CARTESIAN_POINT('Ctrl Pts',(3.35413100037242,14.2094605608055,-0.797238122286408));
#455301=CARTESIAN_POINT('Ctrl Pts',(3.61678024109116,14.1567048855272,0.307776610366904));
#455302=CARTESIAN_POINT('Ctrl Pts',(3.27975339315982,14.1039492102489,1.55532731555235));
#455303=CARTESIAN_POINT('Ctrl Pts',(2.49640166552181,14.0511935349705,2.37776404794338));
#455304=CARTESIAN_POINT('Ctrl Pts',(1.71304993788381,13.9984378596922,3.20020078033441));
#455305=CARTESIAN_POINT('Ctrl Pts',(0.483373330539141,13.9456821844139,
3.59752353993101));
#455306=CARTESIAN_POINT('Ctrl Pts',(-0.633111074588675,13.8929265091356,
3.38894580815677));
#455307=CARTESIAN_POINT('Ctrl Pts',(-1.74959547971649,13.8401708338572,
3.18036807638253));
#455308=CARTESIAN_POINT('Ctrl Pts',(-2.75288768262745,13.7874151585789,
2.36588985323744));
#455309=CARTESIAN_POINT('Ctrl Pts',(-3.18647806713122,13.7346594833006,
1.31610820833249));
#455310=CARTESIAN_POINT('Ctrl Pts',(-3.62006845163498,13.6819038080223,
0.266326563427543));
#455311=CARTESIAN_POINT('Ctrl Pts',(-3.48395701773154,13.6291481327439,
-1.01875850323727));
#455312=CARTESIAN_POINT('Ctrl Pts',(-2.84007605876933,13.5763924574656,
-1.95441838918622));
#455313=CARTESIAN_POINT('Ctrl Pts',(-2.21326179727459,13.525035123196,-2.86527769051828));
#455314=CARTESIAN_POINT('Ctrl Pts',(-1.10523912890168,13.4736777889265,
-3.44499003198518));
#455315=CARTESIAN_POINT('Ctrl Pts',(0.000551455541893276,13.4223204546569,
-3.44746546819473));
#455316=CARTESIAN_POINT('Ctrl Pts',(0.000689626542513858,13.2776795453431,
-3.44740402518832));
#455317=CARTESIAN_POINT('Ctrl Pts',(-1.0974706886562,13.3286800413617,-3.44437823680371));
#455318=CARTESIAN_POINT('Ctrl Pts',(-2.1983372039437,13.3796805373802,-2.87380063074141));
#455319=CARTESIAN_POINT('Ctrl Pts',(-2.82686629247264,13.4306810333988,
-1.9734772654318));
#455320=CARTESIAN_POINT('Ctrl Pts',(-3.47702617494399,13.4834367086771,
-1.04216932112342));
#455321=CARTESIAN_POINT('Ctrl Pts',(-3.62177826665152,13.5361923839554,
0.241971293758206));
#455322=CARTESIAN_POINT('Ctrl Pts',(-3.19525868498632,13.5889480592338,
1.29464570125774));
#455323=CARTESIAN_POINT('Ctrl Pts',(-2.76873910332111,13.6417037345121,
2.34732010875727));
#455324=CARTESIAN_POINT('Ctrl Pts',(-1.77094784828316,13.6944594097904,
3.1685283088747));
#455325=CARTESIAN_POINT('Ctrl Pts',(-0.655891521124064,13.7472150850688,
3.38461103748138));
#455326=CARTESIAN_POINT('Ctrl Pts',(0.459164806035046,13.7999707603471,
3.60069376608806));
#455327=CARTESIAN_POINT('Ctrl Pts',(1.69148620531532,13.8527264356254,3.21165102318395));
#455328=CARTESIAN_POINT('Ctrl Pts',(2.4803521456137,13.9054821109037,2.39450177922372));
#455329=CARTESIAN_POINT('Ctrl Pts',(3.26921808591208,13.958237786182,1.57735253526349));
#455330=CARTESIAN_POINT('Ctrl Pts',(3.6146285672286,14.0109934614604,0.332096790247161));
#455331=CARTESIAN_POINT('Ctrl Pts',(3.35941780359704,14.0637491367387,-0.774659658454042));
#455332=CARTESIAN_POINT('Ctrl Pts',(3.10420703996547,14.116504812017,-1.88141610715523));
#455333=CARTESIAN_POINT('Ctrl Pts',(2.24837503138585,14.1692604872953,-2.84967325954128));
#455334=CARTESIAN_POINT('Ctrl Pts',(1.18133528971154,14.2220161625737,-3.2388628457514));
#455335=CARTESIAN_POINT('Ctrl Pts',(0.806051548466779,14.2405706234968,
-3.37574296207889));
#455336=CARTESIAN_POINT('Ctrl Pts',(0.404642095862786,14.2591250844199,
-3.44099429914845));
#455337=CARTESIAN_POINT('Ctrl Pts',(0.00241009727763581,14.2776795453431,
-3.43837553245923));
#455338=CARTESIAN_POINT('Origin',(0.,0.,0.));
#455339=CARTESIAN_POINT('',(-0.00257283171653078,15.4223204546569,-3.43875668620077));
#455340=CARTESIAN_POINT('',(-0.00264566132197309,15.2776795453431,-3.43894503739979));
#455341=CARTESIAN_POINT('',(-4.21523428266519E-16,0.,-3.442));
#455342=CARTESIAN_POINT('Ctrl Pts',(-0.00257283171653078,15.4223204546569,
-3.43875668620077));
#455343=CARTESIAN_POINT('Ctrl Pts',(0.755888892797501,15.3873235503214,
-3.43343588809486));
#455344=CARTESIAN_POINT('Ctrl Pts',(1.5175038776905,15.3523266459858,-3.18601278121568));
#455345=CARTESIAN_POINT('Ctrl Pts',(2.11288261599305,15.3173297416503,-2.72424597002973));
#455346=CARTESIAN_POINT('Ctrl Pts',(3.01037935125762,15.264574066372,-2.02816097600645));
#455347=CARTESIAN_POINT('Ctrl Pts',(3.53012577026604,15.2118183910936,-0.845007705659107));
#455348=CARTESIAN_POINT('Ctrl Pts',(3.43562315009899,15.1590627158153,0.286855454432574));
#455349=CARTESIAN_POINT('Ctrl Pts',(3.34112052993194,15.106307040537,1.41871861452425));
#455350=CARTESIAN_POINT('Ctrl Pts',(2.63236887058942,15.0535513652587,2.49929166436027));
#455351=CARTESIAN_POINT('Ctrl Pts',(1.63186259450475,15.0007956899804,3.03690648184037));
#455352=CARTESIAN_POINT('Ctrl Pts',(0.631356318420086,14.948040014702,3.57452129932047));
#455353=CARTESIAN_POINT('Ctrl Pts',(-0.66090457440673,14.8952843394237,
3.56917788444466));
#455354=CARTESIAN_POINT('Ctrl Pts',(-1.65692856184199,14.8425286641454,
3.02330487528562));
#455355=CARTESIAN_POINT('Ctrl Pts',(-2.65295254927725,14.7897729888671,
2.47743186612658));
#455356=CARTESIAN_POINT('Ctrl Pts',(-3.35273963132095,14.7370173135887,
1.39102926268431));
#455357=CARTESIAN_POINT('Ctrl Pts',(-3.43787743377992,14.6842616383104,
0.258424246683737));
#455358=CARTESIAN_POINT('Ctrl Pts',(-3.52301523623888,14.6315059630321,
-0.87418076931683));
#455359=CARTESIAN_POINT('Ctrl Pts',(-2.99350375911311,14.5787502877538,
-2.0529881978757));
#455360=CARTESIAN_POINT('Ctrl Pts',(-2.090277456733,14.5259946124754,-2.74162770361305));
#455361=CARTESIAN_POINT('Ctrl Pts',(-1.49861140548322,14.4914365598693,
-3.19272685342806));
#455362=CARTESIAN_POINT('Ctrl Pts',(-0.746583718842133,14.4568785072631,
-3.43349415551258));
#455363=CARTESIAN_POINT('Ctrl Pts',(0.00248787001207174,14.4223204546569,
-3.43854544754782));
#455364=CARTESIAN_POINT('Ctrl Pts',(0.00241009727763581,14.2776795453431,
-3.43837553245923));
#455365=CARTESIAN_POINT('Ctrl Pts',(-0.739019301350593,14.3118807596983,
-3.43354839136065));
#455366=CARTESIAN_POINT('Ctrl Pts',(-1.48324347308736,14.3460819740534,
-3.19811828677568));
#455367=CARTESIAN_POINT('Ctrl Pts',(-2.07178973503114,14.3802831884086,
-2.7556256485914));
#455368=CARTESIAN_POINT('Ctrl Pts',(-2.97962754333046,14.4330388636869,
-2.0730768451871));
#455369=CARTESIAN_POINT('Ctrl Pts',(-3.51705568516008,14.4857945389653,
-0.897857218344334));
#455370=CARTESIAN_POINT('Ctrl Pts',(-3.43953805554209,14.5385502142436,
0.235294778045084));
#455371=CARTESIAN_POINT('Ctrl Pts',(-3.36202042592409,14.5913058895219,
1.3684467744345));
#455372=CARTESIAN_POINT('Ctrl Pts',(-2.66955702485847,14.6440615648002,
2.45953114037057));
#455373=CARTESIAN_POINT('Ctrl Pts',(-1.67722685885009,14.6968172400786,
3.01209161175412));
#455374=CARTESIAN_POINT('Ctrl Pts',(-0.684896692841708,14.7495729153569,
3.56465208313766));
#455375=CARTESIAN_POINT('Ctrl Pts',(0.607300238109442,14.8023285906352,
3.57868865996868));
#455376=CARTESIAN_POINT('Ctrl Pts',(1.6113995754516,14.8550842659135,3.04781495530594));
#455377=CARTESIAN_POINT('Ctrl Pts',(2.61549891279374,14.9078399411919,2.5169412506432));
#455378=CARTESIAN_POINT('Ctrl Pts',(3.3315006565269,14.9605956164702,1.44115726448671));
#455379=CARTESIAN_POINT('Ctrl Pts',(3.43361524521218,15.0133512917485,0.309956387754804));
#455380=CARTESIAN_POINT('Ctrl Pts',(3.53572983389747,15.0661069670268,-0.821244488977105));
#455381=CARTESIAN_POINT('Ctrl Pts',(3.02395726753487,15.1188626423052,-2.00786225628442));
#455382=CARTESIAN_POINT('Ctrl Pts',(2.13116088774389,15.1716183175835,-2.70997051031363));
#455383=CARTESIAN_POINT('Ctrl Pts',(1.53286140191971,15.20697206017,-3.18048205906893));
#455384=CARTESIAN_POINT('Ctrl Pts',(0.763448312546386,15.2423258027566,
-3.43340571476085));
#455385=CARTESIAN_POINT('Ctrl Pts',(-0.00264566132197309,15.2776795453431,
-3.43894503739979));
#455386=CARTESIAN_POINT('Origin',(0.,0.,0.));
#455387=CARTESIAN_POINT('',(-0.000142136989979558,16.4223204546569,-3.44723320560186));
#455388=CARTESIAN_POINT('',(-0.000213030569266609,16.2776795453431,-3.44751024702897));
#455389=CARTESIAN_POINT('',(-4.21523428266519E-16,0.,-3.442));
#455390=CARTESIAN_POINT('Ctrl Pts',(-0.000142136989979558,16.4223204546569,
-3.44723320560186));
#455391=CARTESIAN_POINT('Ctrl Pts',(1.11523026578114,16.370524268658,-3.44525091864187));
#455392=CARTESIAN_POINT('Ctrl Pts',(2.23158337703984,16.318728082659,-2.85471407152575));
#455393=CARTESIAN_POINT('Ctrl Pts',(2.85602730912618,16.2669318966601,-1.93100385516442));
#455394=CARTESIAN_POINT('Ctrl Pts',(3.49203864230329,16.2141762213818,-0.990182532400653));
#455395=CARTESIAN_POINT('Ctrl Pts',(3.61774742836716,16.1614205461035,0.29627011044174));
#455396=CARTESIAN_POINT('Ctrl Pts',(3.17554384765381,16.1086648708251,1.34249779760182));
#455397=CARTESIAN_POINT('Ctrl Pts',(2.73334026694047,16.0559091955468,2.38872548476189));
#455398=CARTESIAN_POINT('Ctrl Pts',(1.72322431944992,16.0031535202685,3.19472821623966));
#455399=CARTESIAN_POINT('Ctrl Pts',(0.605023750021618,15.9503978449902,
3.39402755401468));
#455400=CARTESIAN_POINT('Ctrl Pts',(-0.513176819406664,15.8976421697119,
3.59332689178971));
#455401=CARTESIAN_POINT('Ctrl Pts',(-1.73946201077269,15.8448864944335,
3.18592283586202));
#455402=CARTESIAN_POINT('Ctrl Pts',(-2.51596861503884,15.7921308191552,
2.35705280052856));
#455403=CARTESIAN_POINT('Ctrl Pts',(-3.29247521930499,15.7393751438769,
1.5281827651951));
#455404=CARTESIAN_POINT('Ctrl Pts',(-3.61920323647126,15.6866194685986,
0.277846750455868));
#455405=CARTESIAN_POINT('Ctrl Pts',(-3.34743007316696,15.6338637933202,
-0.824967112775094));
#455406=CARTESIAN_POINT('Ctrl Pts',(-3.07565690986267,15.5811081180419,
-1.92778097600606));
#455407=CARTESIAN_POINT('Ctrl Pts',(-2.2053825660878,15.5283524427636,-2.88307268772875));
#455408=CARTESIAN_POINT('Ctrl Pts',(-1.13262186844002,15.4755967674853,
-3.25621018474049));
#455409=CARTESIAN_POINT('Ctrl Pts',(-0.771505999759574,15.4578379965425,
-3.38181682904251));
#455410=CARTESIAN_POINT('Ctrl Pts',(-0.387445388025546,15.4400792255997,
-3.44145666314416));
#455411=CARTESIAN_POINT('Ctrl Pts',(-0.00257283171653078,15.4223204546569,
-3.43875668620077));
#455412=CARTESIAN_POINT('Ctrl Pts',(-0.00264566132197309,15.2776795453431,
-3.43894503739979));
#455413=CARTESIAN_POINT('Ctrl Pts',(-0.379734896958102,15.2950814780349,
-3.44167162057511));
#455414=CARTESIAN_POINT('Ctrl Pts',(-0.756019965044454,15.3124834107267,
-3.38446101486161));
#455415=CARTESIAN_POINT('Ctrl Pts',(-1.11069842846604,15.3298853434184,
-3.26375976668423));
#455416=CARTESIAN_POINT('Ctrl Pts',(-2.18594117166558,15.3826410186968,
-2.89784202827451));
#455417=CARTESIAN_POINT('Ctrl Pts',(-3.06260646484528,15.4353966939751,
-1.94840781070399));
#455418=CARTESIAN_POINT('Ctrl Pts',(-3.34179814439852,15.4881523692534,
-0.847454950509992));
#455419=CARTESIAN_POINT('Ctrl Pts',(-3.62098982395176,15.5409080445317,
0.253497909683986));
#455420=CARTESIAN_POINT('Ctrl Pts',(-3.30270788987855,15.5936637198101,
1.50596941250144));
#455421=CARTESIAN_POINT('Ctrl Pts',(-2.53178063602364,15.6464193950884,
2.34005942226194));
#455422=CARTESIAN_POINT('Ctrl Pts',(-1.76085338216871,15.6991750703667,
3.17414943202246));
#455423=CARTESIAN_POINT('Ctrl Pts',(-0.537280808532051,15.751930745645,
3.58985794872603));
#455424=CARTESIAN_POINT('Ctrl Pts',(0.582209535696286,15.8046864209234,
3.39805408507685));
#455425=CARTESIAN_POINT('Ctrl Pts',(1.70169987992463,15.8574420962017,3.20625022142767));
#455426=CARTESIAN_POINT('Ctrl Pts',(2.71710799474464,15.91019777148,2.40693397742575));
#455427=CARTESIAN_POINT('Ctrl Pts',(3.16638797553546,15.9629534467583,1.36376248720178));
#455428=CARTESIAN_POINT('Ctrl Pts',(3.61566795632629,16.0157091220366,0.320590996977814));
#455429=CARTESIAN_POINT('Ctrl Pts',(3.49881980308792,16.068464797315,-0.966435739468192));
#455430=CARTESIAN_POINT('Ctrl Pts',(2.8690558925296,16.1212204725933,-1.9116266225805));
#455431=CARTESIAN_POINT('Ctrl Pts',(2.24648604908041,16.1733734968432,-2.84602017905969));
#455432=CARTESIAN_POINT('Ctrl Pts',(1.12265203508462,16.2255265210932,-3.44634315369573));
#455433=CARTESIAN_POINT('Ctrl Pts',(-0.000213030569266609,16.2776795453431,
-3.44751024702897));
#455434=CARTESIAN_POINT('Origin',(0.,5.25141010809499,0.));
#455435=CARTESIAN_POINT('',(-0.000118598906288441,16.751410108095,-2.87636657945628));
#455436=CARTESIAN_POINT('',(-1.47936051206424E-13,16.9,-2.872));
#455437=CARTESIAN_POINT('',(-1.47936051206424E-13,5.25141010809499,-2.872));
#455438=CARTESIAN_POINT('',(-2.30844912129813,16.9,-1.70863883087617));
#455439=CARTESIAN_POINT('Ctrl Pts',(-0.00011859890628823,16.751410108095,
-2.87636657945628));
#455440=CARTESIAN_POINT('Ctrl Pts',(-0.0173585412542118,16.7523695973744,
-2.87639721901023));
#455441=CARTESIAN_POINT('Ctrl Pts',(-0.907290126313184,16.8018995613427,
-2.86927979781993));
#455442=CARTESIAN_POINT('Ctrl Pts',(-1.78950708297451,16.8514295253111,
-2.40949662694586));
#455443=CARTESIAN_POINT('Ctrl Pts',(-2.312781279227,16.9,-1.71040874167461));
#455444=CARTESIAN_POINT('Origin',(0.,16.9,0.));
#455445=CARTESIAN_POINT('Origin',(0.,5.25141010809499,0.));
#455446=CARTESIAN_POINT('',(-0.00214676719638619,15.751410108095,-2.86929378348885));
#455447=CARTESIAN_POINT('',(-0.00017775241010487,15.948589891905,-2.87659774243672));
#455448=CARTESIAN_POINT('',(-1.47936051206424E-13,5.25141010809499,-2.872));
#455449=CARTESIAN_POINT('Ctrl Pts',(-0.00214676719638623,15.751410108095,
-2.86929378348885));
#455450=CARTESIAN_POINT('Ctrl Pts',(-0.323283891461201,15.7691688790378,
-2.87154664048518));
#455451=CARTESIAN_POINT('Ctrl Pts',(-1.59572746551707,15.8396833252589,
-2.67395198656385));
#455452=CARTESIAN_POINT('Ctrl Pts',(-3.29247953528384,15.9629534467583,
-0.811443685944723));
#455453=CARTESIAN_POINT('Ctrl Pts',(-2.47461532961719,16.1212204725933,
2.31839219522703));
#455454=CARTESIAN_POINT('Ctrl Pts',(0.595016631106169,16.2794874984283,
3.33820432360382));
#455455=CARTESIAN_POINT('Ctrl Pts',(3.12353464492909,16.4377545242632,1.32062165817314));
#455456=CARTESIAN_POINT('Ctrl Pts',(2.81076863784611,16.5950620608188,-1.88009858582563));
#455457=CARTESIAN_POINT('Ctrl Pts',(0.930546578536684,16.6996139220961,
-2.87471256198127));
#455458=CARTESIAN_POINT('Ctrl Pts',(-0.00011859890628823,16.751410108095,
-2.87636657945628));
#455459=CARTESIAN_POINT('',(0.863261863496793,16.9,-2.73919020059434));
#455460=CARTESIAN_POINT('Origin',(0.,16.9,0.));
#455461=CARTESIAN_POINT('Ctrl Pts',(-0.000177752410104636,15.948589891905,
-2.87659774243672));
#455462=CARTESIAN_POINT('Ctrl Pts',(-0.0110042390567035,15.9491925429334,
-2.8766089953653));
#455463=CARTESIAN_POINT('Ctrl Pts',(-0.969564698895354,16.0025508692401,
-2.87169484567401));
#455464=CARTESIAN_POINT('Ctrl Pts',(-2.86409573659214,16.1086648708252,
-1.81589248079735));
#455465=CARTESIAN_POINT('Ctrl Pts',(-3.08280821480706,16.2669318966601,
1.4122865025187));
#455466=CARTESIAN_POINT('Ctrl Pts',(-0.497155858873794,16.4251989224951,
3.35338935516332));
#455467=CARTESIAN_POINT('Ctrl Pts',(2.54297493246889,16.58346594833,2.24645259117239));
#455468=CARTESIAN_POINT('Ctrl Pts',(3.26488853074936,16.741732974165,-0.912123640571359));
#455469=CARTESIAN_POINT('Ctrl Pts',(1.77123132985941,16.8472443247217,-2.45304161063505));
#455470=CARTESIAN_POINT('Ctrl Pts',(0.863261863496793,16.9,-2.73919020059434));
#455471=CARTESIAN_POINT('Origin',(0.,5.25141010809499,0.));
#455472=CARTESIAN_POINT('',(0.00207587526855749,14.751410108095,-2.8691175262514));
#455473=CARTESIAN_POINT('',(-0.00220753611772651,14.948589891905,-2.86945094346665));
#455474=CARTESIAN_POINT('',(-1.47936051206424E-13,5.25141010809499,-2.872));
#455475=CARTESIAN_POINT('Ctrl Pts',(0.00207587526855756,14.751410108095,
-2.8691175262514));
#455476=CARTESIAN_POINT('Ctrl Pts',(-0.622948413862524,14.7859681607012,
-2.8649027352214));
#455477=CARTESIAN_POINT('Ctrl Pts',(-2.20835504002284,14.8732818885857,
-2.3573229175255));
#455478=CARTESIAN_POINT('Ctrl Pts',(-3.38142263822873,15.0133512917485,
0.254180059658117));
#455479=CARTESIAN_POINT('Ctrl Pts',(-1.62971854209606,15.1716183175835,
2.97365851150546));
#455480=CARTESIAN_POINT('Ctrl Pts',(1.60506351850703,15.3298853434185,2.98703412526777));
#455481=CARTESIAN_POINT('Ctrl Pts',(3.37920770702971,15.4881523692534,0.282148187618979));
#455482=CARTESIAN_POINT('Ctrl Pts',(2.22416583374883,15.6286606241456,-2.34719473766286));
#455483=CARTESIAN_POINT('Ctrl Pts',(0.630712638034381,15.7164132037595,
-2.86485411696934));
#455484=CARTESIAN_POINT('Ctrl Pts',(-0.00214676719638623,15.751410108095,
-2.86929378348885));
#455485=CARTESIAN_POINT('Ctrl Pts',(-0.0022075361177263,14.948589891905,
-2.86945094346665));
#455486=CARTESIAN_POINT('Ctrl Pts',(-0.316850268467174,14.9659918245968,
-2.87172600066579));
#455487=CARTESIAN_POINT('Ctrl Pts',(-1.58265828892416,15.0361494325669,
-2.6792717958374));
#455488=CARTESIAN_POINT('Ctrl Pts',(-3.28692286143165,15.1590627158153,
-0.833542173003866));
#455489=CARTESIAN_POINT('Ctrl Pts',(-2.49020085562839,15.3173297416503,
2.30163925299127));
#455490=CARTESIAN_POINT('Ctrl Pts',(0.572640891743325,15.4755967674853,
3.34223907283957));
#455491=CARTESIAN_POINT('Ctrl Pts',(3.11440623668499,15.6338637933202,1.34139399488469));
#455492=CARTESIAN_POINT('Ctrl Pts',(2.82302618968387,15.7915281681268,-1.8680183968737));
#455493=CARTESIAN_POINT('Ctrl Pts',(0.936739292493483,15.8964368676551,
-2.87562392138709));
#455494=CARTESIAN_POINT('Ctrl Pts',(-0.000177752410104636,15.948589891905,
-2.87659774243672));
#455495=CARTESIAN_POINT('Origin',(0.,5.25141010809499,0.));
#455496=CARTESIAN_POINT('',(0.000460133735044288,13.751410108095,-2.87656037903988));
#455497=CARTESIAN_POINT('',(0.00201098180729872,13.948589891905,-2.86897574933844));
#455498=CARTESIAN_POINT('',(-1.47936051206424E-13,5.25141010809499,-2.872));
#455499=CARTESIAN_POINT('Ctrl Pts',(0.000460133735044324,13.751410108095,
-2.87656037903988));
#455500=CARTESIAN_POINT('Ctrl Pts',(-0.922209987857596,13.8027674423646,
-2.87449487851869));
#455501=CARTESIAN_POINT('Ctrl Pts',(-2.79644800244617,13.9068804519124,
-1.89390220752309));
#455502=CARTESIAN_POINT('Ctrl Pts',(-3.13415125835744,14.0637491367387,
1.29449570064652));
#455503=CARTESIAN_POINT('Ctrl Pts',(-0.622714413418182,14.2220161625736,
3.33329418136064));
#455504=CARTESIAN_POINT('Ctrl Pts',(2.4554069255945,14.3802831884086,2.33871751178352));
#455505=CARTESIAN_POINT('Ctrl Pts',(3.29905112134591,14.5385502142436,-0.784146194165878));
#455506=CARTESIAN_POINT('Ctrl Pts',(1.61181164346249,14.6622591874724,-2.66734747028903));
#455507=CARTESIAN_POINT('Ctrl Pts',(0.331201949128838,14.7332124854229,
-2.87133695619672));
#455508=CARTESIAN_POINT('Ctrl Pts',(0.00207587526855756,14.751410108095,
-2.8691175262514));
#455509=CARTESIAN_POINT('Ctrl Pts',(0.00201098180729838,13.948589891905,
-2.86897574933844));
#455510=CARTESIAN_POINT('Ctrl Pts',(-0.616636674456527,13.9827911062602,
-2.86494798953738));
#455511=CARTESIAN_POINT('Ctrl Pts',(-2.19548282131563,14.0697479958937,
-2.3654910683637));
#455512=CARTESIAN_POINT('Ctrl Pts',(-3.3830556511082,14.2094605608055,0.231430806858688));
#455513=CARTESIAN_POINT('Ctrl Pts',(-1.64968416256043,14.3677275866405,
2.96262862699381));
#455514=CARTESIAN_POINT('Ctrl Pts',(1.58493778894308,14.5259946124754,2.99776492739358));
#455515=CARTESIAN_POINT('Ctrl Pts',(3.37723035838085,14.6842616383104,0.304866953911748));
#455516=CARTESIAN_POINT('Ctrl Pts',(2.23702055240126,14.8251267314536,-2.33887228332351));
#455517=CARTESIAN_POINT('Ctrl Pts',(0.637020207330869,14.9132361493185,
-2.86482894038154));
#455518=CARTESIAN_POINT('Ctrl Pts',(-0.0022075361177263,14.948589891905,
-2.86945094346665));
#455519=CARTESIAN_POINT('Origin',(0.,5.25141010809499,0.));
#455520=CARTESIAN_POINT('',(-0.00245713763363008,12.751410108095,-2.87038222330126));
#455521=CARTESIAN_POINT('',(0.000575423425195377,12.948589891905,-2.87650911108102));
#455522=CARTESIAN_POINT('',(-1.47936051206424E-13,5.25141010809499,-2.872));
#455523=CARTESIAN_POINT('Ctrl Pts',(-0.00245713763363003,12.751410108095,
-2.87038222330126));
#455524=CARTESIAN_POINT('Ctrl Pts',(-0.280691862282867,12.7668110487496,
-2.87267579240923));
#455525=CARTESIAN_POINT('Ctrl Pts',(-1.50935892272592,12.8349676646826,
-2.70806675152048));
#455526=CARTESIAN_POINT('Ctrl Pts',(-3.25314999541872,12.9558799558939,
-0.956889911280283));
#455527=CARTESIAN_POINT('Ctrl Pts',(-2.5752272092837,13.1141469817289,2.20608885054153));
#455528=CARTESIAN_POINT('Ctrl Pts',(0.446212100842591,13.2724140075638,
3.36147556301922));
#455529=CARTESIAN_POINT('Ctrl Pts',(3.06158804260283,13.4306810333988,1.45784150227068));
#455530=CARTESIAN_POINT('Ctrl Pts',(2.89084781869623,13.5889480592338,-1.77246215397422));
#455531=CARTESIAN_POINT('Ctrl Pts',(0.998443281277944,13.6958577507992,
-2.86496636962172));
#455532=CARTESIAN_POINT('Ctrl Pts',(0.0255822995740321,13.7500117670862,
-2.87661661782493));
#455533=CARTESIAN_POINT('Ctrl Pts',(0.000460133735044324,13.751410108095,
-2.87656037903988));
#455534=CARTESIAN_POINT('Ctrl Pts',(0.00057542342519559,12.948589891905,
-2.87650911108102));
#455535=CARTESIAN_POINT('Ctrl Pts',(-0.915728012150204,12.9995903879236,
-2.87398439747242));
#455536=CARTESIAN_POINT('Ctrl Pts',(-2.78446322534953,13.1033465592205,
-1.90542149769778));
#455537=CARTESIAN_POINT('Ctrl Pts',(-3.14278767844486,13.2598584057957,
1.27338564834797));
#455538=CARTESIAN_POINT('Ctrl Pts',(-0.645120783207451,13.4181254316307,
3.32903057926365));
#455539=CARTESIAN_POINT('Ctrl Pts',(2.43962098791356,13.5763924574656,2.35518041283082));
#455540=CARTESIAN_POINT('Ctrl Pts',(3.30425105968087,13.7346594833006,-0.761938558424485));
#455541=CARTESIAN_POINT('Ctrl Pts',(1.62488632563581,13.8587252947804,-2.66191063110109));
#455542=CARTESIAN_POINT('Ctrl Pts',(0.337632800498971,13.9300354309819,
-2.87116084461198));
#455543=CARTESIAN_POINT('Ctrl Pts',(0.00201098180729838,13.948589891905,
-2.86897574933844));
#455544=CARTESIAN_POINT('Origin',(0.,5.25141010809499,0.));
#455545=CARTESIAN_POINT('',(0.00158946424445254,11.751410108095,-2.86827662802734));
#455546=CARTESIAN_POINT('',(-0.00248815572466116,11.948589891905,-2.87055996458015));
#455547=CARTESIAN_POINT('',(-1.47936051206424E-13,5.25141010809499,-2.872));
#455548=CARTESIAN_POINT('Ctrl Pts',(0.00158946424445229,11.751410108095,
-2.86827662802734));
#455549=CARTESIAN_POINT('Ctrl Pts',(-0.581219832021058,11.783610330413,
-2.86532506714357));
#455550=CARTESIAN_POINT('Ctrl Pts',(-2.12312024035974,11.8685662280094,
-2.41007181460196));
#455551=CARTESIAN_POINT('Ctrl Pts',(-3.38937612577637,12.0062778008841,
0.103695101446341));
#455552=CARTESIAN_POINT('Ctrl Pts',(-1.76022816749725,12.164544826719,2.89831330161118));
#455553=CARTESIAN_POINT('Ctrl Pts',(1.470768272467,12.322811852554,3.05539913673341));
#455554=CARTESIAN_POINT('Ctrl Pts',(3.36333145263819,12.481078878389,0.432000851345749));
#455555=CARTESIAN_POINT('Ctrl Pts',(2.30885711969421,12.6239449635693,-2.29099023912859));
#455556=CARTESIAN_POINT('Ctrl Pts',(0.67239672586907,12.7140553734713,-2.86481920820428));
#455557=CARTESIAN_POINT('Ctrl Pts',(-0.00245713763363003,12.751410108095,
-2.87038222330126));
#455558=CARTESIAN_POINT('Ctrl Pts',(-0.0024881557246614,11.948589891905,
-2.87055996458015));
#455559=CARTESIAN_POINT('Ctrl Pts',(-0.274233616854917,11.9636339943087,
-2.87283941429877));
#455560=CARTESIAN_POINT('Ctrl Pts',(-1.4962908949992,12.0314337719906,-2.71302462104432));
#455561=CARTESIAN_POINT('Ctrl Pts',(-3.24664049163476,12.1519892249509,
-0.978749670253043));
#455562=CARTESIAN_POINT('Ctrl Pts',(-2.59000777962451,12.3102562507859,
2.18871768405023));
#455563=CARTESIAN_POINT('Ctrl Pts',(0.423592117726756,12.4685232766209,
3.36440115286681));
#455564=CARTESIAN_POINT('Ctrl Pts',(3.05171335757124,12.6267903024558,1.47840149529983));
#455565=CARTESIAN_POINT('Ctrl Pts',(2.90270462181359,12.7850573282908,-1.75297783143327));
#455566=CARTESIAN_POINT('Ctrl Pts',(1.01139939624214,12.8923238581072,-2.86187502554507));
#455567=CARTESIAN_POINT('Ctrl Pts',(0.0321099556615316,12.9468347126453,
-2.87659599896072));
#455568=CARTESIAN_POINT('Ctrl Pts',(0.00057542342519559,12.948589891905,
-2.87650911108102));
#455569=CARTESIAN_POINT('Origin',(0.,5.25141010809499,0.));
#455570=CARTESIAN_POINT('',(0.00118908056354697,10.751410108095,-2.8760373750822));
#455571=CARTESIAN_POINT('',(0.00150509715381469,10.948589891905,-2.86817106627712));
#455572=CARTESIAN_POINT('',(-1.47936051206424E-13,5.25141010809499,-2.872));
#455573=CARTESIAN_POINT('Ctrl Pts',(0.00118908056354687,10.751410108095,
-2.8760373750822));
#455574=CARTESIAN_POINT('Ctrl Pts',(-0.87954819760536,10.8004096120764,
-2.87141110940037));
#455575=CARTESIAN_POINT('Ctrl Pts',(-2.71674168632202,10.9021647913362,
-1.96862591891224));
#455576=CARTESIAN_POINT('Ctrl Pts',(-3.18857005274037,11.0566756458742,
1.15396889840285));
#455577=CARTESIAN_POINT('Ctrl Pts',(-0.770195857929068,11.2149426717092,
3.30233576977685));
#455578=CARTESIAN_POINT('Ctrl Pts',(2.34907444021962,11.3732096975442,2.44550045375373));
#455579=CARTESIAN_POINT('Ctrl Pts',(3.33063248386109,11.5314767233792,-0.636797027311755));
#455580=CARTESIAN_POINT('Ctrl Pts',(1.69819735393824,11.6575435268961,-2.63038771649106));
#455581=CARTESIAN_POINT('Ctrl Pts',(0.373633761202303,11.7308546551347,
-2.87016079734477));
#455582=CARTESIAN_POINT('Ctrl Pts',(0.00158946424445229,11.751410108095,
-2.86827662802734));
#455583=CARTESIAN_POINT('Ctrl Pts',(0.00150509715381476,10.948589891905,
-2.86817106627712));
#455584=CARTESIAN_POINT('Ctrl Pts',(-0.574898968689857,10.980433275972,
-2.86541333431411));
#455585=CARTESIAN_POINT('Ctrl Pts',(-2.11018667018124,11.0650323353174,
-2.41780658533811));
#455586=CARTESIAN_POINT('Ctrl Pts',(-3.38999725238531,11.2023870699411,
0.0808951693976638));
#455587=CARTESIAN_POINT('Ctrl Pts',(-1.77968313098077,11.360654095776,2.88640838279897));
#455588=CARTESIAN_POINT('Ctrl Pts',(1.45018394022225,11.518921121611,3.06522298348167));
#455589=CARTESIAN_POINT('Ctrl Pts',(3.36034997176485,11.677188147446,0.454613535191446));
#455590=CARTESIAN_POINT('Ctrl Pts',(2.32162678658566,11.8204110708773,-2.28222762448876));
#455591=CARTESIAN_POINT('Ctrl Pts',(0.678705609501433,11.9108783190303,
-2.86484598897222));
#455592=CARTESIAN_POINT('Ctrl Pts',(-0.0024881557246614,11.948589891905,
-2.87055996458015));
#455593=CARTESIAN_POINT('Origin',(0.,5.25141010809499,0.));
#455594=CARTESIAN_POINT('',(-0.00258136649849588,9.75141010809498,-2.87160024361889));
#455595=CARTESIAN_POINT('',(0.00129076080759852,9.94858989190502,-2.87592458636046));
#455596=CARTESIAN_POINT('',(-1.47936051206424E-13,5.25141010809499,-2.872));
#455597=CARTESIAN_POINT('Ctrl Pts',(-0.00258136649849569,9.75141010809498,
-2.87160024361889));
#455598=CARTESIAN_POINT('Ctrl Pts',(-0.237965141875198,9.76445321846148,
-2.87371275150489));
#455599=CARTESIAN_POINT('Ctrl Pts',(-1.42303883068652,9.8302520041063,-2.73984855250909));
#455600=CARTESIAN_POINT('Ctrl Pts',(-3.20742346381156,9.94880646502946,
-1.10048057409996));
#455601=CARTESIAN_POINT('Ctrl Pts',(-2.67069952678566,10.1070734908644,
2.08949452686489));
#455602=CARTESIAN_POINT('Ctrl Pts',(0.29642307182911,10.2653405166994,3.3779811414132));
#455603=CARTESIAN_POINT('Ctrl Pts',(2.99379373691612,10.4236075425344,1.59242651290754));
#455604=CARTESIAN_POINT('Ctrl Pts',(2.96674265574526,10.5818745683693,-1.64227319112547));
#455605=CARTESIAN_POINT('Ctrl Pts',(1.08412200216352,10.6911420902229,-2.84370207199545));
#455606=CARTESIAN_POINT('Ctrl Pts',(0.0687040514418887,10.7476539367981,
-2.87639201227143));
#455607=CARTESIAN_POINT('Ctrl Pts',(0.00118908056354687,10.751410108095,
-2.8760373750822));
#455608=CARTESIAN_POINT('Ctrl Pts',(0.0012907608075984,9.94858989190502,
-2.87592458636046));
#455609=CARTESIAN_POINT('Ctrl Pts',(-0.873123805142145,9.99723255763544,
-2.87100311148923));
#455610=CARTESIAN_POINT('Ctrl Pts',(-2.70457728265256,10.0986308986442,
-1.97965085114474));
#455611=CARTESIAN_POINT('Ctrl Pts',(-3.19626004985765,10.2527849149312,
1.13249596744652));
#455612=CARTESIAN_POINT('Ctrl Pts',(-0.792390653220595,10.4110519407662,
3.29708089890013));
#455613=CARTESIAN_POINT('Ctrl Pts',(2.33257261886262,10.5693189666012,2.46124569460491));
#455614=CARTESIAN_POINT('Ctrl Pts',(3.33484068029608,10.7275859924362,-0.614380207850174));
#455615=CARTESIAN_POINT('Ctrl Pts',(1.71126896779768,10.8540096342041,-2.62457997243907));
#455616=CARTESIAN_POINT('Ctrl Pts',(0.380043058286468,10.9276776006937,
-2.86998213302089));
#455617=CARTESIAN_POINT('Ctrl Pts',(0.00150509715381476,10.948589891905,
-2.86817106627712));
#455618=CARTESIAN_POINT('Origin',(0.,5.25141010809499,0.));
#455619=CARTESIAN_POINT('',(0.000993903865917874,8.75141010809498,-2.86769215449362));
#455620=CARTESIAN_POINT('',(-0.00258314593131442,8.94858989190502,-2.87179187325464));
#455621=CARTESIAN_POINT('',(-1.47936051206424E-13,5.25141010809499,-2.872));
#455622=CARTESIAN_POINT('Ctrl Pts',(0.000993903865917981,8.75141010809497,
-2.86769215449362));
#455623=CARTESIAN_POINT('Ctrl Pts',(-0.539416506838244,8.78125250012487,
-2.86600725099512));
#455624=CARTESIAN_POINT('Ctrl Pts',(-2.0375213686481,8.8638505674331,-2.45998816760348));
#455625=CARTESIAN_POINT('Ctrl Pts',(-3.39063316576441,8.99920431001964,
-0.0469946717703988));
#455626=CARTESIAN_POINT('Ctrl Pts',(-1.88726201450869,9.1574713358546,2.81724502982847));
#455627=CARTESIAN_POINT('Ctrl Pts',(1.33356715403539,9.31573836168959,3.11772757096118));
#455628=CARTESIAN_POINT('Ctrl Pts',(3.34081625807316,9.47400538752454,0.581005048681307));
#455629=CARTESIAN_POINT('Ctrl Pts',(2.392975748847,9.61922930299303,-2.23181518064891));
#455630=CARTESIAN_POINT('Ctrl Pts',(0.714095346047257,9.71169754318316,
-2.86516825736777));
#455631=CARTESIAN_POINT('Ctrl Pts',(-0.00258136649849569,9.75141010809498,
-2.87160024361889));
#455632=CARTESIAN_POINT('Ctrl Pts',(-0.00258314593131425,8.94858989190502,
-2.87179187325464));
#455633=CARTESIAN_POINT('Ctrl Pts',(-0.231488332032663,8.96127616402051,
-2.87386034028333));
#455634=CARTESIAN_POINT('Ctrl Pts',(-1.40998235584436,9.02671811141432,
-2.7444605327945));
#455635=CARTESIAN_POINT('Ctrl Pts',(-3.19994881461505,9.14491573408647,
-1.12202938400675));
#455636=CARTESIAN_POINT('Ctrl Pts',(-2.68469389625817,9.30318275992144,
2.07148374386093));
#455637=CARTESIAN_POINT('Ctrl Pts',(0.273695539681721,9.4614497857564,3.37989889026531));
#455638=CARTESIAN_POINT('Ctrl Pts',(2.98301528359298,9.61971681159137,1.61252745511383));
#455639=CARTESIAN_POINT('Ctrl Pts',(2.97772210058549,9.77798383742635,-1.62228130541839));
#455640=CARTESIAN_POINT('Ctrl Pts',(1.09710326595299,9.88760819753089,-2.8403108118492));
#455641=CARTESIAN_POINT('Ctrl Pts',(0.0752274047922757,9.94447688235712,
-2.87634072459695));
#455642=CARTESIAN_POINT('Ctrl Pts',(0.0012907608075984,9.94858989190502,
-2.87592458636046));
#455643=CARTESIAN_POINT('Origin',(0.,5.25141010809499,0.));
#455644=CARTESIAN_POINT('',(0.00198847260380099,7.75141010809497,-2.87512062938712));
#455645=CARTESIAN_POINT('',(0.000911915543898995,7.94858989190502,-2.86762206492074));
#455646=CARTESIAN_POINT('',(-1.47936051206424E-13,5.25141010809499,-2.872));
#455647=CARTESIAN_POINT('Ctrl Pts',(0.00198847260380112,7.75141010809497,
-2.87512062938712));
#455648=CARTESIAN_POINT('Ctrl Pts',(-0.837002867190702,7.79805178178826,
-2.86893764875045));
#455649=CARTESIAN_POINT('Ctrl Pts',(-2.63619448267628,7.89744913075989,
-2.04016147455094));
#455650=CARTESIAN_POINT('Ctrl Pts',(-3.23653135410128,8.0496021550098,1.01119616857442));
#455651=CARTESIAN_POINT('Ctrl Pts',(-0.91623943503461,8.2078691808448,3.26483823460727));
#455652=CARTESIAN_POINT('Ctrl Pts',(2.23814586565504,8.36613620667974,2.54746254727596));
#455653=CARTESIAN_POINT('Ctrl Pts',(3.355613622894,8.52440323251474,-0.488194768594614));
#455654=CARTESIAN_POINT('Ctrl Pts',(1.78454755545998,8.6528278663198,-2.59094511229407));
#455655=CARTESIAN_POINT('Ctrl Pts',(0.415926352928926,8.72849682484655,
-2.86898584003561));
#455656=CARTESIAN_POINT('Ctrl Pts',(0.000993903865917981,8.75141010809497,
-2.86769215449362));
#455657=CARTESIAN_POINT('Ctrl Pts',(0.000911915543898995,7.94858989190502,
-2.86762206492074));
#455658=CARTESIAN_POINT('Ctrl Pts',(-0.533073886542687,7.9780754456839,
-2.86612649557932));
#455659=CARTESIAN_POINT('Ctrl Pts',(-2.02456627808555,8.06031667474111,
-2.46731154287715));
#455660=CARTESIAN_POINT('Ctrl Pts',(-3.39022251156056,8.19531357907665,
-0.0697920698937834));
#455661=CARTESIAN_POINT('Ctrl Pts',(-1.90617827987364,8.3535806049116,2.80448353848272));
#455662=CARTESIAN_POINT('Ctrl Pts',(1.31257158419998,8.5118476307466,3.12662922130667));
#455663=CARTESIAN_POINT('Ctrl Pts',(3.33683050597697,8.67011465658154,0.603461870573552));
#455664=CARTESIAN_POINT('Ctrl Pts',(2.40565202370955,8.81569541030104,-2.22259592592606));
#455665=CARTESIAN_POINT('Ctrl Pts',(0.720410504564146,8.90852048874219,
-2.86525865068561));
#455666=CARTESIAN_POINT('Ctrl Pts',(-0.00258314593131425,8.94858989190502,
-2.87179187325464));
#455667=CARTESIAN_POINT('Origin',(0.,0.,0.));
#455668=CARTESIAN_POINT('',(0.00234742734116236,0.322176117089595,-2.94408456759461));
#455669=CARTESIAN_POINT('',(0.00309359675299801,0.177823882910405,-2.94421791268484));
#455670=CARTESIAN_POINT('',(-3.60291088309151E-16,0.,-2.942));
#455671=CARTESIAN_POINT('',(2.64462557919718,0.,1.28892185405323));
#455672=CARTESIAN_POINT('Ctrl Pts',(0.00234742734116236,0.322176117089595,
-2.94408456759461));
#455673=CARTESIAN_POINT('Ctrl Pts',(0.152623335834112,0.31402898266599,
-2.94532683936105));
#455674=CARTESIAN_POINT('Ctrl Pts',(0.302716573408032,0.305881848242384,
-2.93478849511196));
#455675=CARTESIAN_POINT('Ctrl Pts',(0.450880220883188,0.297734713818779,
-2.9118552212362));
#455676=CARTESIAN_POINT('Ctrl Pts',(1.40105040066211,0.245487321750099,
-2.76478464533735));
#455677=CARTESIAN_POINT('Ctrl Pts',(2.27186370990282,0.193239929681419,
-2.10795667259909));
#455678=CARTESIAN_POINT('Ctrl Pts',(2.67509378307532,0.140992537612738,
-1.23478030777358));
#455679=CARTESIAN_POINT('Ctrl Pts',(3.0378068232696,0.0939950250751588,
-0.449341733165658));
#455680=CARTESIAN_POINT('Ctrl Pts',(3.02218231782814,0.0469975125375793,
0.511151705155529));
#455681=CARTESIAN_POINT('Ctrl Pts',(2.64767078191736,-2.62376925741492E-16,
1.2919591116057));
#455682=CARTESIAN_POINT('',(2.64462557919717,0.,-1.28892185405323));
#455683=CARTESIAN_POINT('Origin',(0.,0.,0.));
#455684=CARTESIAN_POINT('Ctrl Pts',(2.64462557919718,0.,-1.28892185405323));
#455685=CARTESIAN_POINT('Ctrl Pts',(2.22149825342052,0.0522473920686802,
-2.15709966133247));
#455686=CARTESIAN_POINT('Ctrl Pts',(1.34158650816433,0.104494784137361,
-2.79385315646035));
#455687=CARTESIAN_POINT('Ctrl Pts',(0.389878440861619,0.156742176206041,
-2.92042183738268));
#455688=CARTESIAN_POINT('Ctrl Pts',(0.26187441011064,0.163769411774162,
-2.93744523130095));
#455689=CARTESIAN_POINT('Ctrl Pts',(0.132571580237253,0.170796647342284,
-2.94523935594652));
#455690=CARTESIAN_POINT('Ctrl Pts',(0.00309359675299801,0.177823882910405,
-2.94421791268484));
#455691=CARTESIAN_POINT('Origin',(0.,0.,0.));
#455692=CARTESIAN_POINT('',(-0.000533914549282755,1.3221761170896,-2.93754474843028));
#455693=CARTESIAN_POINT('',(-0.000201976967395493,1.1778238829104,-2.93745911239609));
#455694=CARTESIAN_POINT('',(-3.60291088309151E-16,0.,-2.942));
#455695=CARTESIAN_POINT('Ctrl Pts',(-0.000533914549282755,1.3221761170896,
-2.93754474843028));
#455696=CARTESIAN_POINT('Ctrl Pts',(0.518827038902267,1.29418000174474,
-2.93667747579154));
#455697=CARTESIAN_POINT('Ctrl Pts',(1.03859776609672,1.26618388639988,-2.80518365811747));
#455698=CARTESIAN_POINT('Ctrl Pts',(1.48377366790336,1.23818777105502,-2.54571195061657));
#455699=CARTESIAN_POINT('Ctrl Pts',(2.31457749888888,1.18594037898634,-2.06147619627931));
#455700=CARTESIAN_POINT('Ctrl Pts',(2.8855793906847,1.13369298691766,-1.13151376080079));
#455701=CARTESIAN_POINT('Ctrl Pts',(2.94155991415087,1.08144559484898,-0.171517343472406));
#455702=CARTESIAN_POINT('Ctrl Pts',(2.99754043761704,1.0291982027803,0.788479073855973));
#455703=CARTESIAN_POINT('Ctrl Pts',(2.53849959275358,0.976950810711622,
1.77850947303422));
#455704=CARTESIAN_POINT('Ctrl Pts',(1.7695909716078,0.924703418642942,2.35601906999579));
#455705=CARTESIAN_POINT('Ctrl Pts',(1.00068235046202,0.872456026574262,
2.93352866695737));
#455706=CARTESIAN_POINT('Ctrl Pts',(-0.0780940469660901,0.820208634505582,
3.09851746170227));
#455707=CARTESIAN_POINT('Ctrl Pts',(-0.984445713078919,0.767961242436901,
2.77724933044992));
#455708=CARTESIAN_POINT('Ctrl Pts',(-1.89079737919174,0.715713850368221,
2.45598119919756));
#455709=CARTESIAN_POINT('Ctrl Pts',(-2.62472431398929,0.66346645829954,
1.64845614194797));
#455710=CARTESIAN_POINT('Ctrl Pts',(-2.85830324984526,0.61121906623086,
0.715613073331115));
#455711=CARTESIAN_POINT('Ctrl Pts',(-3.09188218570122,0.55897167416218,
-0.217229995285738));
#455712=CARTESIAN_POINT('Ctrl Pts',(-2.8251131226156,0.5067242820935,-1.27539107526984));
#455713=CARTESIAN_POINT('Ctrl Pts',(-2.17696506591423,0.45447689002482,
-1.98581502573217));
#455714=CARTESIAN_POINT('Ctrl Pts',(-1.62988519913137,0.410376632379746,
-2.58545986946785));
#455715=CARTESIAN_POINT('Ctrl Pts',(-0.811092726927701,0.36627637473467,
-2.93736017812011));
#455716=CARTESIAN_POINT('Ctrl Pts',(0.00234742734116236,0.322176117089595,
-2.94408456759461));
#455717=CARTESIAN_POINT('Ctrl Pts',(0.00309359675299801,0.177823882910405,
-2.94421791268484));
#455718=CARTESIAN_POINT('Ctrl Pts',(-0.830095303743749,0.223044039410964,
-2.93764494046812));
#455719=CARTESIAN_POINT('Ctrl Pts',(-1.67053714603895,0.268264195911523,
-2.56602781851946));
#455720=CARTESIAN_POINT('Ctrl Pts',(-2.2188180236089,0.313484352412081,
-1.93960410903164));
#455721=CARTESIAN_POINT('Ctrl Pts',(-2.85230203142748,0.365731744480761,
-1.2158338330415));
#455722=CARTESIAN_POINT('Ctrl Pts',(-3.09576565771542,0.417979136549442,
-0.151909414344424));
#455723=CARTESIAN_POINT('Ctrl Pts',(-2.84232694733696,0.470226528618122,
0.775884131996558));
#455724=CARTESIAN_POINT('Ctrl Pts',(-2.5888882369585,0.522473920686802,
1.70367767833754));
#455725=CARTESIAN_POINT('Ctrl Pts',(-1.83854718991364,0.574721312755483,
2.49534035232244));
#455726=CARTESIAN_POINT('Ctrl Pts',(-0.925728335606107,0.626968704824163,
2.79735991175273));
#455727=CARTESIAN_POINT('Ctrl Pts',(-0.0129094812985767,0.679216096892843,
3.09937947118302));
#455728=CARTESIAN_POINT('Ctrl Pts',(1.06238718027163,0.731463488961522,
2.91175591605871));
#455729=CARTESIAN_POINT('Ctrl Pts',(1.8189927749781,0.783710881030203,2.31816853201152));
#455730=CARTESIAN_POINT('Ctrl Pts',(2.57559836968458,0.835958273098883,
1.72458114796434));
#455731=CARTESIAN_POINT('Ctrl Pts',(3.01351289752732,0.888205665167564,
0.725029934994281));
#455732=CARTESIAN_POINT('Ctrl Pts',(2.93725089347923,0.940453057236245,
-0.233583529514978));
#455733=CARTESIAN_POINT('Ctrl Pts',(2.86098888943113,0.992700449304925,
-1.19219699402423));
#455734=CARTESIAN_POINT('Ctrl Pts',(2.2705503534922,1.0449478413736,-2.10987271007269));
#455735=CARTESIAN_POINT('Ctrl Pts',(1.42972599524097,1.09719523344228,-2.57645757349211));
#455736=CARTESIAN_POINT('Ctrl Pts',(0.99720340249237,1.12407144993166,-2.81647023830494));
#455737=CARTESIAN_POINT('Ctrl Pts',(0.498426099280125,1.15094766642103,
-2.93711953997791));
#455738=CARTESIAN_POINT('Ctrl Pts',(-0.000201976967395493,1.1778238829104,
-2.93745911239609));
#455739=CARTESIAN_POINT('Origin',(0.,0.,0.));
#455740=CARTESIAN_POINT('',(-0.00134644729286121,2.3221761170896,-2.94573633641246));
#455741=CARTESIAN_POINT('',(-0.00163187090823506,2.1778238829104,-2.94531716671524));
#455742=CARTESIAN_POINT('',(-3.60291088309151E-16,0.,-2.942));
#455743=CARTESIAN_POINT('Ctrl Pts',(-0.00134644729286121,2.3221761170896,
-2.94573633641246));
#455744=CARTESIAN_POINT('Ctrl Pts',(0.879913779079956,2.27433102082349,
-2.94064754527962));
#455745=CARTESIAN_POINT('Ctrl Pts',(1.7654150896307,2.22648592455738,-2.51813317797539));
#455746=CARTESIAN_POINT('Ctrl Pts',(2.31152197537838,2.17864082829127,-1.82731873918827));
#455747=CARTESIAN_POINT('Ctrl Pts',(2.90787693749131,2.12639343622259,-1.07294147491715));
#455748=CARTESIAN_POINT('Ctrl Pts',(3.09950779265045,2.07414604415391,0.00138066437529602));
#455749=CARTESIAN_POINT('Ctrl Pts',(2.80075519910971,2.02189865208523,0.915421823845812));
#455750=CARTESIAN_POINT('Ctrl Pts',(2.50200260556897,1.96965126001655,1.82946298331634));
#455751=CARTESIAN_POINT('Ctrl Pts',(1.71286656332835,1.91740386794787,2.58322316296495));
#455752=CARTESIAN_POINT('Ctrl Pts',(0.786093029068817,1.86515647587919,
2.83976862276147));
#455753=CARTESIAN_POINT('Ctrl Pts',(-0.140680505190703,1.81290908381051,
3.09631408255799));
#455754=CARTESIAN_POINT('Ctrl Pts',(-1.20509153146913,1.76066169174183,
2.85564482250244));
#455755=CARTESIAN_POINT('Ctrl Pts',(-1.93134289750084,1.70841429967315,
2.22534118511019));
#455756=CARTESIAN_POINT('Ctrl Pts',(-2.65759426353255,1.65616690760447,
1.59503754771794));
#455757=CARTESIAN_POINT('Ctrl Pts',(-3.04568596931755,1.60391951553579,
0.575099532988995));
#455758=CARTESIAN_POINT('Ctrl Pts',(-2.92214249359839,1.55167212346711,
-0.378557369309796));
#455759=CARTESIAN_POINT('Ctrl Pts',(-2.79859901787924,1.49942473139842,
-1.33221427160858));
#455760=CARTESIAN_POINT('Ctrl Pts',(-2.16342036065593,1.44717733932974,
-2.21959006147722));
#455761=CARTESIAN_POINT('Ctrl Pts',(-1.30052814695666,1.39492994726106,
-2.64402341981353));
#455762=CARTESIAN_POINT('Ctrl Pts',(-0.900005995922876,1.37067867053724,
-2.84102944090459));
#455763=CARTESIAN_POINT('Ctrl Pts',(-0.450423695561913,1.34642739381342,
-2.93829601225735));
#455764=CARTESIAN_POINT('Ctrl Pts',(-0.000533914549282755,1.3221761170896,
-2.93754474843028));
#455765=CARTESIAN_POINT('Ctrl Pts',(-0.000201976967395493,1.1778238829104,
-2.93745911239609));
#455766=CARTESIAN_POINT('Ctrl Pts',(-0.470907385827677,1.20319505848971,
-2.93777966910268));
#455767=CARTESIAN_POINT('Ctrl Pts',(-0.941479812882249,1.22856623406902,
-2.83088766492598));
#455768=CARTESIAN_POINT('Ctrl Pts',(-1.35605793578947,1.25393740964832,
-2.61598698348122));
#455769=CARTESIAN_POINT('Ctrl Pts',(-2.20980732800516,1.30618480171701,
-2.17343751926055));
#455770=CARTESIAN_POINT('Ctrl Pts',(-2.82609593187302,1.35843219378569,
-1.27284458002884));
#455771=CARTESIAN_POINT('Ctrl Pts',(-2.92947779976765,1.41067958585437,
-0.31679046293656));
#455772=CARTESIAN_POINT('Ctrl Pts',(-3.03285966766227,1.46292697792305,
0.639263654155722));
#455773=CARTESIAN_POINT('Ctrl Pts',(-2.62333479958367,1.51517436999173,
1.65077894910857));
#455774=CARTESIAN_POINT('Ctrl Pts',(-1.88394286986409,1.56742176206041,
2.2656116195793));
#455775=CARTESIAN_POINT('Ctrl Pts',(-1.14455094014452,1.61966915412909,
2.88044429005002));
#455776=CARTESIAN_POINT('Ctrl Pts',(-0.0752919487839852,1.67191654619777,
3.09859433603862));
#455777=CARTESIAN_POINT('Ctrl Pts',(0.845861261610144,1.72416393826645,
2.82254409907328));
#455778=CARTESIAN_POINT('Ctrl Pts',(1.76701447200428,1.77641133033513,2.54649386210794));
#455779=CARTESIAN_POINT('Ctrl Pts',(2.54006190143201,1.82865872240381,1.77624334218867));
#455780=CARTESIAN_POINT('Ctrl Pts',(2.81945377803531,1.88090611447249,0.856099332179975));
#455781=CARTESIAN_POINT('Ctrl Pts',(3.09884565463862,1.93315350654117,-0.0640446778287201));
#455782=CARTESIAN_POINT('Ctrl Pts',(2.88458197841751,1.98540089860985,-1.13408217792684));
#455783=CARTESIAN_POINT('Ctrl Pts',(2.2724366580869,2.03764829067853,-1.87570349193988));
#455784=CARTESIAN_POINT('Ctrl Pts',(1.72499094254115,2.08437348808915,-2.53894046758902));
#455785=CARTESIAN_POINT('Ctrl Pts',(0.859325602669026,2.13109868549978,
-2.93951522469678));
#455786=CARTESIAN_POINT('Ctrl Pts',(-0.00163187090823506,2.1778238829104,
-2.94531716671524));
#455787=CARTESIAN_POINT('Origin',(0.,0.,0.));
#455788=CARTESIAN_POINT('',(0.00237334009290435,3.3221761170896,-2.94031398119338));
#455789=CARTESIAN_POINT('',(0.00246242204629553,3.1778238829104,-2.94087084915089));
#455790=CARTESIAN_POINT('',(-3.60291088309151E-16,0.,-2.942));
#455791=CARTESIAN_POINT('Ctrl Pts',(0.00237334009290435,3.3221761170896,
-2.94031398119338));
#455792=CARTESIAN_POINT('Ctrl Pts',(0.288247022003705,3.30672943197091,
-2.94257327477183));
#455793=CARTESIAN_POINT('Ctrl Pts',(0.573526739760804,3.29128274685223,
-2.90415646478538));
#455794=CARTESIAN_POINT('Ctrl Pts',(0.845861119733735,3.27583606173355,
-2.82254358189058));
#455795=CARTESIAN_POINT('Ctrl Pts',(1.76701417068956,3.22358866966487,-2.54649339651438));
#455796=CARTESIAN_POINT('Ctrl Pts',(2.54006143235309,3.17134127759619,-1.77624301496856));
#455797=CARTESIAN_POINT('Ctrl Pts',(2.81945325191896,3.11909388552751,-0.856099173574967));
#455798=CARTESIAN_POINT('Ctrl Pts',(3.09884507148485,3.06684649345883,0.06404466781863));
#455799=CARTESIAN_POINT('Ctrl Pts',(2.88458144895307,3.01459910139015,1.13408196906));
#455800=CARTESIAN_POINT('Ctrl Pts',(2.27243624440142,2.96235170932147,1.87570314629083));
#455801=CARTESIAN_POINT('Ctrl Pts',(1.66029103984977,2.91010431725279,2.61732432352167));
#455802=CARTESIAN_POINT('Ctrl Pts',(0.650264253278263,2.85785692518411,
3.03052937674198));
#455803=CARTESIAN_POINT('Ctrl Pts',(-0.306156988195277,2.80560953311543,
2.93061358417489));
#455804=CARTESIAN_POINT('Ctrl Pts',(-1.26257822966882,2.75336214104675,
2.8306977916078));
#455805=CARTESIAN_POINT('Ctrl Pts',(-2.16539392604439,2.70111474897807,
2.21766115325329));
#455806=CARTESIAN_POINT('Ctrl Pts',(-2.61104285907814,2.64886735690939,
1.36553359130061));
#455807=CARTESIAN_POINT('Ctrl Pts',(-3.05669179211189,2.59661996484071,
0.51340602934793));
#455808=CARTESIAN_POINT('Ctrl Pts',(-3.04517396180382,2.54437257277203,
-0.577812456202931));
#455809=CARTESIAN_POINT('Ctrl Pts',(-2.58163754554515,2.49212518070335,
-1.42034333901256));
#455810=CARTESIAN_POINT('Ctrl Pts',(-2.11810112928649,2.43987778863467,
-2.26287422182219));
#455811=CARTESIAN_POINT('Ctrl Pts',(-1.20254612707725,2.38763039656599,
-2.85671750189059));
#455812=CARTESIAN_POINT('Ctrl Pts',(-0.244229091439268,2.33538300449731,
-2.93642294729989));
#455813=CARTESIAN_POINT('Ctrl Pts',(-0.163482571919671,2.33098070869474,
-2.9431388221766));
#455814=CARTESIAN_POINT('Ctrl Pts',(-0.0824324623351636,2.32657841289217,
-2.94620456336972));
#455815=CARTESIAN_POINT('Ctrl Pts',(-0.00134644729286121,2.3221761170896,
-2.94573633641246));
#455816=CARTESIAN_POINT('Ctrl Pts',(-0.00163187090823506,2.1778238829104,
-2.94531716671524));
#455817=CARTESIAN_POINT('Ctrl Pts',(-0.103383709848986,2.18334607756846,
-2.94600286640184));
#455818=CARTESIAN_POINT('Ctrl Pts',(-0.205069791295828,2.18886827222651,
-2.94117454564737));
#455819=CARTESIAN_POINT('Ctrl Pts',(-0.306157042210219,2.19439046688457,
-2.93061412268682));
#455820=CARTESIAN_POINT('Ctrl Pts',(-1.26257845773664,2.24663785895325,
-2.83069831149277));
#455821=CARTESIAN_POINT('Ctrl Pts',(-2.16539432434938,2.29888525102193,
-2.2176615611767));
#455822=CARTESIAN_POINT('Ctrl Pts',(-2.6110433404237,2.35113264309061,-1.36553384267249));
#455823=CARTESIAN_POINT('Ctrl Pts',(-3.05669235649802,2.40338003515929,
-0.513406124168287));
#455824=CARTESIAN_POINT('Ctrl Pts',(-3.04517452203392,2.45562742722797,
0.577812562524056));
#455825=CARTESIAN_POINT('Ctrl Pts',(-2.58163801980982,2.50787481929665,
1.42034360036398));
#455826=CARTESIAN_POINT('Ctrl Pts',(-2.11810151758573,2.56012221136533,
2.2628746382039));
#455827=CARTESIAN_POINT('Ctrl Pts',(-1.20254634760163,2.61236960343401,
2.8567180271914));
#455828=CARTESIAN_POINT('Ctrl Pts',(-0.244229136344604,2.66461699550269,
2.93642348720734));
#455829=CARTESIAN_POINT('Ctrl Pts',(0.714088074912416,2.71686438757137,
3.01612894722328));
#455830=CARTESIAN_POINT('Ctrl Pts',(1.71516732744236,2.76911177964005,2.58169647826766));
#455831=CARTESIAN_POINT('Ctrl Pts',(2.31152239995082,2.82135917170873,1.82731907529804));
#455832=CARTESIAN_POINT('Ctrl Pts',(2.90787747245929,2.87360656377741,1.07294167232842));
#455833=CARTESIAN_POINT('Ctrl Pts',(3.09950836494629,2.92585395584609,-0.00138066465518699));
#455834=CARTESIAN_POINT('Ctrl Pts',(2.80075571536857,2.97810134791477,-0.915421992244635));
#455835=CARTESIAN_POINT('Ctrl Pts',(2.50200306579085,3.03034873998345,-1.82946331983409));
#455836=CARTESIAN_POINT('Ctrl Pts',(1.71286687414841,3.08259613205213,-2.58322363802937));
#455837=CARTESIAN_POINT('Ctrl Pts',(0.786093171304736,3.13484352412081,
-2.83976914495077));
#455838=CARTESIAN_POINT('Ctrl Pts',(0.531962041897567,3.14917031038401,
-2.91011663023032));
#455839=CARTESIAN_POINT('Ctrl Pts',(0.26748175157528,3.16349709664721,-2.94307782418315));
#455840=CARTESIAN_POINT('Ctrl Pts',(0.00246242204629553,3.1778238829104,
-2.94087084915089));
#455841=CARTESIAN_POINT('Origin',(0.,0.,0.));
#455842=CARTESIAN_POINT('',(-0.00235626413880502,4.3221761170896,-2.93955723260335));
#455843=CARTESIAN_POINT('',(-0.00203590851197863,4.17782388291041,-2.93914442058615));
#455844=CARTESIAN_POINT('',(-3.60291088309151E-16,0.,-2.942));
#455845=CARTESIAN_POINT('Ctrl Pts',(-0.00235626413880502,4.3221761170896,
-2.93955723260335));
#455846=CARTESIAN_POINT('Ctrl Pts',(0.651304352142019,4.28688045104966,
-2.93489446451832));
#455847=CARTESIAN_POINT('Ctrl Pts',(1.30786871926028,4.25158478500973,-2.71916533387861));
#455848=CARTESIAN_POINT('Ctrl Pts',(1.81899283066209,4.2162891189698,-2.31816809067732));
#455849=CARTESIAN_POINT('Ctrl Pts',(2.57559852309904,4.16404172690112,-1.72458076014517));
#455850=CARTESIAN_POINT('Ctrl Pts',(3.01351225985306,4.11179433483244,-0.725029779266838));
#455851=CARTESIAN_POINT('Ctrl Pts',(2.93725012432094,4.05954694276376,0.233583488232732));
#455852=CARTESIAN_POINT('Ctrl Pts',(2.86098798878882,4.00729955069508,1.1921967557323));
#455853=CARTESIAN_POINT('Ctrl Pts',(2.27054998097057,3.9550521586264,2.10987230985309));
#455854=CARTESIAN_POINT('Ctrl Pts',(1.42972586492197,3.90280476655772,2.57645709389019));
#455855=CARTESIAN_POINT('Ctrl Pts',(0.588901748873358,3.85055737448904,
3.0430418779273));
#455856=CARTESIAN_POINT('Ctrl Pts',(-0.502308475405612,3.79830998242035,
3.05853589188072));
#455857=CARTESIAN_POINT('Ctrl Pts',(-1.35605776241588,3.74606259035167,
2.61598650798725));
#455858=CARTESIAN_POINT('Ctrl Pts',(-2.20980704942615,3.69381519828299,
2.17343712409378));
#455859=CARTESIAN_POINT('Ctrl Pts',(-2.82609539916772,3.64156780621432,
1.27284434235344));
#455860=CARTESIAN_POINT('Ctrl Pts',(-2.92947721784002,3.58932041414564,
0.316790400434435));
#455861=CARTESIAN_POINT('Ctrl Pts',(-3.03285903651231,3.53707302207696,
-0.639263541484576));
#455862=CARTESIAN_POINT('Ctrl Pts',(-2.62333432411533,3.48482563000827,
-1.65077864358225));
#455863=CARTESIAN_POINT('Ctrl Pts',(-1.88394254779278,3.43257823793959,
-2.26561120002781));
#455864=CARTESIAN_POINT('Ctrl Pts',(-1.36314832239072,3.39577753098959,
-2.69867152777258));
#455865=CARTESIAN_POINT('Ctrl Pts',(-0.678701823405697,3.35897682403959,
-2.93493136348248));
#455866=CARTESIAN_POINT('Ctrl Pts',(0.00237334009290435,3.3221761170896,
-2.94031398119338));
#455867=CARTESIAN_POINT('Ctrl Pts',(0.00246242204629553,3.1778238829104,
-2.94087084915089));
#455868=CARTESIAN_POINT('Ctrl Pts',(-0.698999395089763,3.21574448871589,
-2.93502935555397));
#455869=CARTESIAN_POINT('Ctrl Pts',(-1.40423757166641,3.25366509452137,
-2.68280940691118));
#455870=CARTESIAN_POINT('Ctrl Pts',(-1.93134324840035,3.29158570032686,
-2.22534159435153));
#455871=CARTESIAN_POINT('Ctrl Pts',(-2.65759475121686,3.34383309239554,
-1.59503784118338));
#455872=CARTESIAN_POINT('Ctrl Pts',(-3.04568654280498,3.39608048446422,
-0.575099639199598));
#455873=CARTESIAN_POINT('Ctrl Pts',(-2.92214303868762,3.4483278765329,0.378557438820167));
#455874=CARTESIAN_POINT('Ctrl Pts',(-2.79859953457026,3.50057526860158,
1.33221451683994));
#455875=CARTESIAN_POINT('Ctrl Pts',(-2.16342073474742,3.55282266067026,
2.21959047089569));
#455876=CARTESIAN_POINT('Ctrl Pts',(-1.30052837232317,3.60507005273893,
2.64402390645178));
#455877=CARTESIAN_POINT('Ctrl Pts',(-0.437636009898931,3.65731744480762,
3.06845734200787));
#455878=CARTESIAN_POINT('Ctrl Pts',(0.652969915126714,3.7095648368763,3.02994825906432));
#455879=CARTESIAN_POINT('Ctrl Pts',(1.48377391623871,3.76181222894498,2.54571241761008));
#455880=CARTESIAN_POINT('Ctrl Pts',(2.3145779173507,3.81405962101366,2.06147657615583));
#455881=CARTESIAN_POINT('Ctrl Pts',(2.88557999454904,3.86630701308234,1.13151397619092));
#455882=CARTESIAN_POINT('Ctrl Pts',(2.94156049840815,3.91855440515102,0.171517377964578));
#455883=CARTESIAN_POINT('Ctrl Pts',(2.99754100226726,3.9708017972197,-0.788479220261775));
#455884=CARTESIAN_POINT('Ctrl Pts',(2.53849993278712,4.02304918928838,-1.77850981674955));
#455885=CARTESIAN_POINT('Ctrl Pts',(1.76959122115166,4.07529658135706,-2.35601951031475));
#455886=CARTESIAN_POINT('Ctrl Pts',(1.2666370243105,4.10947234854151,-2.7337768691529));
#455887=CARTESIAN_POINT('Ctrl Pts',(0.631101141471884,4.14364811572596,
-2.93503074915652));
#455888=CARTESIAN_POINT('Ctrl Pts',(-0.00203590851197863,4.17782388291041,
-2.93914442058615));
#455889=CARTESIAN_POINT('Origin',(0.,-1.84858989190502,0.));
#455890=CARTESIAN_POINT('',(-0.00189954774684422,4.65141010809498,-2.3697807159847));
#455891=CARTESIAN_POINT('',(-1.42212172806258E-5,4.84858989190502,-2.37515968171377));
#455892=CARTESIAN_POINT('',(-1.14631214242372E-14,-1.84858989190502,-2.37175));
#455893=CARTESIAN_POINT('',(-1.93106208855764,5.,1.37702479013102));
#455894=CARTESIAN_POINT('Ctrl Pts',(-0.00189954774684462,4.65141010809498,
-2.3697807159847));
#455895=CARTESIAN_POINT('Ctrl Pts',(-0.254987285068325,4.66836183412373,
-2.37158607092717));
#455896=CARTESIAN_POINT('Ctrl Pts',(-1.28591963123153,4.73756095222115,
-2.21873566508313));
#455897=CARTESIAN_POINT('Ctrl Pts',(-2.63119954910018,4.85375758285616,
-0.799366116563622));
#455898=CARTESIAN_POINT('Ctrl Pts',(-2.3348384767276,4.95300248746242,0.808908954735007));
#455899=CARTESIAN_POINT('Ctrl Pts',(-1.93307880200418,5.,1.37984525234445));
#455900=CARTESIAN_POINT('',(-1.93106208855765,5.,-1.37702479013102));
#455901=CARTESIAN_POINT('Origin',(0.,5.,0.));
#455902=CARTESIAN_POINT('Ctrl Pts',(-1.42212172806475E-5,4.84858989190502,
-2.37515968171377));
#455903=CARTESIAN_POINT('Ctrl Pts',(-0.747581930412603,4.89905992793668,
-2.37328899234637));
#455904=CARTESIAN_POINT('Ctrl Pts',(-1.49439019245277,4.94952996396834,
-1.98938888825773));
#455905=CARTESIAN_POINT('Ctrl Pts',(-1.93106208855765,5.,-1.37702479013102));
#455906=CARTESIAN_POINT('Origin',(0.,-1.84858989190502,0.));
#455907=CARTESIAN_POINT('',(0.0019133138563352,3.65141010809498,-2.37039078344507));
#455908=CARTESIAN_POINT('',(-0.00164128688419168,3.84858989190502,-2.36944791962108));
#455909=CARTESIAN_POINT('',(-1.14631214242372E-14,-1.84858989190502,-2.37175));
#455910=CARTESIAN_POINT('Ctrl Pts',(0.00191331385633514,3.65141010809498,
-2.37039078344507));
#455911=CARTESIAN_POINT('Ctrl Pts',(-0.547148555289758,3.68821081504498,
-2.36605148244037));
#455912=CARTESIAN_POINT('Ctrl Pts',(-1.88231140024366,3.77725891406365,
-1.90517491303348));
#455913=CARTESIAN_POINT('Ctrl Pts',(-2.77514400288091,3.91855440515103,
0.300097769845058));
#455914=CARTESIAN_POINT('Ctrl Pts',(-1.28464581100504,4.07529658135705,
2.47818845314823));
#455915=CARTESIAN_POINT('Ctrl Pts',(1.35445464728892,4.2320387575631,2.44071605927262));
#455916=CARTESIAN_POINT('Ctrl Pts',(2.78243358513013,4.38878093376914,0.221310557417421));
#455917=CARTESIAN_POINT('Ctrl Pts',(1.83787761908733,4.52857138394644,-1.93466620949292));
#455918=CARTESIAN_POINT('Ctrl Pts',(0.525061555809934,4.61611444205505,
-2.36602173562927));
#455919=CARTESIAN_POINT('Ctrl Pts',(-0.00189954774684462,4.65141010809498,
-2.3697807159847));
#455920=CARTESIAN_POINT('Ctrl Pts',(-0.00164128688419168,3.84858989190502,
-2.36944791962108));
#455921=CARTESIAN_POINT('Ctrl Pts',(-0.271541296495615,3.86666151678925,
-2.3712015367225));
#455922=CARTESIAN_POINT('Ctrl Pts',(-1.31965288321337,3.93698053374216,
-2.20510919750293));
#455923=CARTESIAN_POINT('Ctrl Pts',(-2.70764255999216,4.05954694276376,
-0.677933051861301));
#455924=CARTESIAN_POINT('Ctrl Pts',(-2.06245770113408,4.2162891189698,1.88123866225974));
#455925=CARTESIAN_POINT('Ctrl Pts',(0.427459215478939,4.37303129517583,
2.75839888164688));
#455926=CARTESIAN_POINT('Ctrl Pts',(2.53353286025567,4.52977347138188,1.16985680540038));
#455927=CARTESIAN_POINT('Ctrl Pts',(2.37788705609658,4.68651564758791,-1.46517155291796));
#455928=CARTESIAN_POINT('Ctrl Pts',(0.826561294082925,4.7927877877623,-2.36282686983047));
#455929=CARTESIAN_POINT('Ctrl Pts',(0.0263121713413973,4.846812535868,-2.37522556003093));
#455930=CARTESIAN_POINT('Ctrl Pts',(-1.42212172806475E-5,4.84858989190502,
-2.37515968171377));
#455931=CARTESIAN_POINT('Origin',(0.,-1.84858989190502,0.));
#455932=CARTESIAN_POINT('',(-0.0010854644346883,2.65141010809498,-2.37476211960784));
#455933=CARTESIAN_POINT('',(0.00198512898990283,2.84858989190502,-2.37083971328131));
#455934=CARTESIAN_POINT('',(-1.14631214242372E-14,-1.84858989190502,-2.37175));
#455935=CARTESIAN_POINT('Ctrl Pts',(-0.00108546443468895,2.65141010809498,
-2.37476211960784));
#455936=CARTESIAN_POINT('Ctrl Pts',(-0.0664545181996722,2.65581240389755,
-2.37513958979338));
#455937=CARTESIAN_POINT('Ctrl Pts',(-0.907265059639853,2.7124620917688,
-2.34333571530495));
#455938=CARTESIAN_POINT('Ctrl Pts',(-2.44564035685759,2.82135917170873,
-1.34552146026667));
#455939=CARTESIAN_POINT('Ctrl Pts',(-2.47349631950189,2.97810134791478,
1.29359897797797));
#455940=CARTESIAN_POINT('Ctrl Pts',(-0.29002949977508,3.13484352412081,
2.77623288044292));
#455941=CARTESIAN_POINT('Ctrl Pts',(2.15272817974667,3.29158570032686,1.77689322887057));
#455942=CARTESIAN_POINT('Ctrl Pts',(2.67092642591228,3.44832787653289,-0.811000349531056));
#455943=CARTESIAN_POINT('Ctrl Pts',(1.24026445200505,3.56826934578894,-2.23648619743872));
#455944=CARTESIAN_POINT('Ctrl Pts',(0.232375892058898,3.6359634229763,-2.37221215650581));
#455945=CARTESIAN_POINT('Ctrl Pts',(0.00191331385633514,3.65141010809498,
-2.37039078344507));
#455946=CARTESIAN_POINT('Ctrl Pts',(0.0019851289899029,2.84858989190502,
-2.37083971328131));
#455947=CARTESIAN_POINT('Ctrl Pts',(-0.563511833889923,2.8865104977105,
-2.36613048063736));
#455948=CARTESIAN_POINT('Ctrl Pts',(-1.91539516889925,2.97667849558466,
-1.88264567131773));
#455949=CARTESIAN_POINT('Ctrl Pts',(-2.76820658211993,3.11909388552752,
0.358615180585798));
#455950=CARTESIAN_POINT('Ctrl Pts',(-1.23202168904057,3.27583606173355,
2.50474086280712));
#455951=CARTESIAN_POINT('Ctrl Pts',(1.40561726678495,3.4325782379396,2.4116063446514));
#455952=CARTESIAN_POINT('Ctrl Pts',(2.78659025447549,3.58932041414563,0.162484526364377));
#455953=CARTESIAN_POINT('Ctrl Pts',(1.80439595705469,3.72799096546744,-1.95584969423954));
#455954=CARTESIAN_POINT('Ctrl Pts',(0.508774348159733,3.81441412472057,
-2.36613160411692));
#455955=CARTESIAN_POINT('Ctrl Pts',(-0.00164128688419168,3.84858989190502,
-2.36944791962108));
#455956=CARTESIAN_POINT('Origin',(0.,-1.84858989190502,0.));
#455957=CARTESIAN_POINT('',(-0.000430425503821624,1.65141010809498,-2.36815831308277));
#455958=CARTESIAN_POINT('',(-0.00131556418306894,1.84858989190502,-2.37442419787793));
#455959=CARTESIAN_POINT('',(-1.14631214242372E-14,-1.84858989190502,-2.37175));
#455960=CARTESIAN_POINT('Ctrl Pts',(-0.000430425503821948,1.65141010809498,
-2.36815831308277));
#455961=CARTESIAN_POINT('Ctrl Pts',(-0.363117743014602,1.6756613848188,
-2.36876395889577));
#455962=CARTESIAN_POINT('Ctrl Pts',(-1.50640329832999,1.7521600536113,-2.12141555137754));
#455963=CARTESIAN_POINT('Ctrl Pts',(-2.76820605062014,1.88090611447249,
-0.358615115250419));
#455964=CARTESIAN_POINT('Ctrl Pts',(-1.82960322615152,2.03764829067853,
2.10811294705418));
#455965=CARTESIAN_POINT('Ctrl Pts',(0.744683162267116,2.19439046688457,
2.69017343400533));
#455966=CARTESIAN_POINT('Ctrl Pts',(2.65321484974249,2.35113264309061,0.867198546770537));
#455967=CARTESIAN_POINT('Ctrl Pts',(2.2027709898381,2.50347252349408,-1.65808273322866));
#455968=CARTESIAN_POINT('Ctrl Pts',(0.70935945123483,2.60356501182887,-2.37065969256184));
#455969=CARTESIAN_POINT('Ctrl Pts',(-0.00108546443468895,2.65141010809498,
-2.37476211960784));
#455970=CARTESIAN_POINT('Ctrl Pts',(-0.00131556418306908,1.84858989190502,
-2.37442419787793));
#455971=CARTESIAN_POINT('Ctrl Pts',(-0.0833447701680231,1.85411208656308,
-2.3749769878955));
#455972=CARTESIAN_POINT('Ctrl Pts',(-0.940926068943489,1.91188167328981,
-2.33425678779921));
#455973=CARTESIAN_POINT('Ctrl Pts',(-2.4734967778431,2.02189865208523,-1.29359921657332));
#455974=CARTESIAN_POINT('Ctrl Pts',(-2.44564080514743,2.17864082829127,
1.34552170813359));
#455975=CARTESIAN_POINT('Ctrl Pts',(-0.231363468903584,2.33538300449731,
2.78173658695524));
#455976=CARTESIAN_POINT('Ctrl Pts',(2.18975452958847,2.49212518070335,1.73105826447513));
#455977=CARTESIAN_POINT('Ctrl Pts',(2.65321534120238,2.64886735690939,-0.867198706368743));
#455978=CARTESIAN_POINT('Ctrl Pts',(1.20641409926552,2.76768892730995,-2.24914186907922));
#455979=CARTESIAN_POINT('Ctrl Pts',(0.215635569102197,2.83426310564182,
-2.37261890873773));
#455980=CARTESIAN_POINT('Ctrl Pts',(0.0019851289899029,2.84858989190502,
-2.37083971328131));
#455981=CARTESIAN_POINT('Origin',(0.,-1.84858989190502,0.));
#455982=CARTESIAN_POINT('',(0.00189242379211233,0.651410108094979,-2.37343051434144));
#455983=CARTESIAN_POINT('',(-0.000162827624894668,0.848589891905021,-2.36808927594338));
#455984=CARTESIAN_POINT('',(-1.14631214242372E-14,-1.84858989190502,-2.37175));
#455985=CARTESIAN_POINT('Ctrl Pts',(0.00189242379211238,0.651410108094979,
-2.37343051434144));
#455986=CARTESIAN_POINT('Ctrl Pts',(-0.653878033681435,0.695510365740054,
-2.36800951817008));
#455987=CARTESIAN_POINT('Ctrl Pts',(-2.09599365201939,0.79185801545381,
-1.74821763141818));
#455988=CARTESIAN_POINT('Ctrl Pts',(-2.7076414341639,0.940453057236244,
0.677932800861099));
#455989=CARTESIAN_POINT('Ctrl Pts',(-0.932633404653946,1.09719523344229,
2.63093846489754));
#455990=CARTESIAN_POINT('Ctrl Pts',(1.67639574619592,1.25393740964833,2.23191177495579));
#455991=CARTESIAN_POINT('Ctrl Pts',(2.78658961819278,1.41067958585437,-0.162484485327371));
#455992=CARTESIAN_POINT('Ctrl Pts',(1.61928227105817,1.54317048533659,-2.06362001410675));
#455993=CARTESIAN_POINT('Ctrl Pts',(0.41826241655896,1.62341399275012,-2.36745914453045));
#455994=CARTESIAN_POINT('Ctrl Pts',(-0.000430425503821948,1.65141010809498,
-2.36815831308277));
#455995=CARTESIAN_POINT('Ctrl Pts',(-0.00016282762489446,0.848589891905021,
-2.36808927594338));
#455996=CARTESIAN_POINT('Ctrl Pts',(-0.3796310646964,0.873961067484328,
-2.36834769891036));
#455997=CARTESIAN_POINT('Ctrl Pts',(-1.54021819528391,0.951579635132315,
-2.10471668851161));
#455998=CARTESIAN_POINT('Ctrl Pts',(-2.77514463720035,1.08144559484898,
-0.300097834486946));
#455999=CARTESIAN_POINT('Ctrl Pts',(-1.78470554216421,1.23818777105502,
2.14625981419194));
#456000=CARTESIAN_POINT('Ctrl Pts',(0.801305687705963,1.39492994726106,
2.67385740587119));
#456001=CARTESIAN_POINT('Ctrl Pts',(2.67092693931563,1.5516721234671,0.811000501773433));
#456002=CARTESIAN_POINT('Ctrl Pts',(2.17098524681304,1.70289210501509,-1.68571927954979));
#456003=CARTESIAN_POINT('Ctrl Pts',(0.692761896033403,1.8018646944944,-2.36974685050122));
#456004=CARTESIAN_POINT('Ctrl Pts',(-0.00131556418306908,1.84858989190502,
-2.37442419787793));
#456005=CARTESIAN_POINT('Ctrl Pts',(2.13201587949045,-0.329233991005384,
-1.03908919352506));
#456006=CARTESIAN_POINT('Ctrl Pts',(1.79090363105035,-0.276986598936704,
-1.73898746491002));
#456007=CARTESIAN_POINT('Ctrl Pts',(0.372188007793122,-0.172491814799343,
-2.76564966890019));
#456008=CARTESIAN_POINT('Ctrl Pts',(-2.10316535941187,-0.0157496385933029,
-1.8378710515163));
#456009=CARTESIAN_POINT('Ctrl Pts',(-2.69198404294186,0.140992537612738,
0.735238472662612));
#456010=CARTESIAN_POINT('Ctrl Pts',(-0.877278354639368,0.297734713818778,
2.64988083876425));
#456011=CARTESIAN_POINT('Ctrl Pts',(1.72333502783425,0.454476890024819,
2.1961118038906));
#456012=CARTESIAN_POINT('Ctrl Pts',(2.78243473695495,0.61121906623086,-0.221310618979959));
#456013=CARTESIAN_POINT('Ctrl Pts',(1.35445452184974,0.7679612424369,-2.44071651245848));
#456014=CARTESIAN_POINT('Ctrl Pts',(-1.2846458307181,0.924703418642942,
-2.47818889868423));
#456015=CARTESIAN_POINT('Ctrl Pts',(-2.77514463720035,1.08144559484898,
-0.300097834486946));
#456016=CARTESIAN_POINT('Ctrl Pts',(-1.78470554216421,1.23818777105502,
2.14625981419194));
#456017=CARTESIAN_POINT('Ctrl Pts',(0.801305687705963,1.39492994726106,
2.67385740587119));
#456018=CARTESIAN_POINT('Ctrl Pts',(2.67092693931563,1.5516721234671,0.811000501773433));
#456019=CARTESIAN_POINT('Ctrl Pts',(2.15272856330194,1.70841429967315,-1.77689355756481));
#456020=CARTESIAN_POINT('Ctrl Pts',(-0.290029546396374,1.86515647587919,
-2.77623338981819));
#456021=CARTESIAN_POINT('Ctrl Pts',(-2.4734967778431,2.02189865208523,-1.29359921657332));
#456022=CARTESIAN_POINT('Ctrl Pts',(-2.44564080514743,2.17864082829127,
1.34552170813359));
#456023=CARTESIAN_POINT('Ctrl Pts',(-0.231363468903584,2.33538300449731,
2.78173658695524));
#456024=CARTESIAN_POINT('Ctrl Pts',(2.18975452958847,2.49212518070335,1.73105826447513));
#456025=CARTESIAN_POINT('Ctrl Pts',(2.65321534120238,2.64886735690939,-0.867198706368743));
#456026=CARTESIAN_POINT('Ctrl Pts',(0.744683292397524,2.80560953311543,
-2.69017392867975));
#456027=CARTESIAN_POINT('Ctrl Pts',(-1.82960355013577,2.96235170932147,
-2.10811333459611));
#456028=CARTESIAN_POINT('Ctrl Pts',(-2.76820658211993,3.11909388552752,
0.358615180585798));
#456029=CARTESIAN_POINT('Ctrl Pts',(-1.23202168904057,3.27583606173355,
2.50474086280712));
#456030=CARTESIAN_POINT('Ctrl Pts',(1.40561726678495,3.4325782379396,2.4116063446514));
#456031=CARTESIAN_POINT('Ctrl Pts',(2.78659025447549,3.58932041414563,0.162484526364377));
#456032=CARTESIAN_POINT('Ctrl Pts',(1.67639583924145,3.74606259035167,-2.2319122111134));
#456033=CARTESIAN_POINT('Ctrl Pts',(-0.932633206071211,3.90280476655772,
-2.63093889113374));
#456034=CARTESIAN_POINT('Ctrl Pts',(-2.70764255999216,4.05954694276376,
-0.677933051861301));
#456035=CARTESIAN_POINT('Ctrl Pts',(-2.06245770113408,4.2162891189698,1.88123866225974));
#456036=CARTESIAN_POINT('Ctrl Pts',(0.427459215478939,4.37303129517583,
2.75839888164688));
#456037=CARTESIAN_POINT('Ctrl Pts',(2.53353286025567,4.52977347138188,1.16985680540038));
#456038=CARTESIAN_POINT('Ctrl Pts',(2.37788705609658,4.68651564758791,-1.46517155291796));
#456039=CARTESIAN_POINT('Ctrl Pts',(0.0898163016776116,4.84325782379396,
-2.7891351771088));
#456040=CARTESIAN_POINT('Ctrl Pts',(-1.47901232685639,4.94775260793132,
-2.01095394174764));
#456041=CARTESIAN_POINT('Ctrl Pts',(-1.93106208855765,5.,-1.37702479013102));
#456042=CARTESIAN_POINT('Ctrl Pts',(2.30288577939269,-0.219489327336923,
-1.12236674703445));
#456043=CARTESIAN_POINT('Ctrl Pts',(1.93443517184041,-0.167241935268243,
-1.87835819705084));
#456044=CARTESIAN_POINT('Ctrl Pts',(0.402016926164794,-0.0627471511308819,
-2.98730199646287));
#456045=CARTESIAN_POINT('Ctrl Pts',(-2.2717230413211,0.0939950250751584,
-1.98516678492372));
#456046=CARTESIAN_POINT('Ctrl Pts',(-2.90773245662903,0.250737201281199,
0.794163983225957));
#456047=CARTESIAN_POINT('Ctrl Pts',(-0.947587617382505,0.40747937748724,
2.86225490127861));
#456048=CARTESIAN_POINT('Ctrl Pts',(1.86145129917011,0.564221553693281,
2.37211865623853));
#456049=CARTESIAN_POINT('Ctrl Pts',(3.00543229975999,0.720963729899321,
-0.239047505311898));
#456050=CARTESIAN_POINT('Ctrl Pts',(1.46300695375092,0.877705906105364,
-2.63632715034604));
#456051=CARTESIAN_POINT('Ctrl Pts',(-1.38760346185783,1.0344480823114,-2.67680275195357));
#456052=CARTESIAN_POINT('Ctrl Pts',(-2.99755793671386,1.19119025851744,
-0.324149103257007));
#456053=CARTESIAN_POINT('Ctrl Pts',(-1.92774033861116,1.34793243472348,
2.3182712908151));
#456054=CARTESIAN_POINT('Ctrl Pts',(0.865526139329494,1.50467461092953,
2.88815306458986));
#456055=CARTESIAN_POINT('Ctrl Pts',(2.884987736497,1.66141678713557,0.875997941938753));
#456056=CARTESIAN_POINT('Ctrl Pts',(2.32525847626676,1.81815896334161,-1.91930226438486));
#456057=CARTESIAN_POINT('Ctrl Pts',(-0.313273894638884,1.97490113954765,
-2.9987339471484));
#456058=CARTESIAN_POINT('Ctrl Pts',(-2.6717345822161,2.13164331575369,-1.39727441466909));
#456059=CARTESIAN_POINT('Ctrl Pts',(-2.64164609928823,2.28838549195973,
1.45335822182786));
#456060=CARTESIAN_POINT('Ctrl Pts',(-0.2499060384749,2.44512766816577,3.00467819669646));
#456061=CARTESIAN_POINT('Ctrl Pts',(2.36525187971641,2.60186984437181,1.8697935127541));
#456062=CARTESIAN_POINT('Ctrl Pts',(2.86585664661268,2.75861202057785,-0.936700138125429));
#456063=CARTESIAN_POINT('Ctrl Pts',(0.804365755767006,2.91535419678389,
-2.90577727119472));
#456064=CARTESIAN_POINT('Ctrl Pts',(-1.97623668663343,3.07209637298993,
-2.27706757078646));
#456065=CARTESIAN_POINT('Ctrl Pts',(-2.99006383287765,3.22883854919597,
0.387356307985263));
#456066=CARTESIAN_POINT('Ctrl Pts',(-1.33076177100191,3.38558072540201,
2.70548271685522));
#456067=CARTESIAN_POINT('Ctrl Pts',(1.51827012457408,3.54232290160805,2.60488395514119));
#456068=CARTESIAN_POINT('Ctrl Pts',(3.00992086023279,3.6990650778141,0.175506809651583));
#456069=CARTESIAN_POINT('Ctrl Pts',(1.81075018059663,3.85580725402013,-2.41078827848804));
#456070=CARTESIAN_POINT('Ctrl Pts',(-1.00737887006926,4.01254943022618,
-2.84179485581088));
#456071=CARTESIAN_POINT('Ctrl Pts',(-2.92464592176238,4.16929160643222,
-0.732265833256742));
#456072=CARTESIAN_POINT('Ctrl Pts',(-2.22775287756101,4.32603378263826,
2.03201008240009));
#456073=CARTESIAN_POINT('Ctrl Pts',(0.461717831497611,4.48277595884429,
2.97947009660899));
#456074=CARTESIAN_POINT('Ctrl Pts',(2.73658224201468,4.63951813505034,1.26361469771331));
#456075=CARTESIAN_POINT('Ctrl Pts',(2.56846224231478,4.79626031125638,-1.58259737464615));
#456076=CARTESIAN_POINT('Ctrl Pts',(0.0970146075743366,4.95300248746242,
-3.01266974507848));
#456077=CARTESIAN_POINT('Ctrl Pts',(-1.5975474140831,5.05749727159978,-2.17212136176543));
#456078=CARTESIAN_POINT('Ctrl Pts',(-2.08582659521588,5.10974466366846,
-1.48738611075535));
#456079=CARTESIAN_POINT('Ctrl Pts',(2.47375567929493,-0.109744663668462,
-1.20564430054383));
#456080=CARTESIAN_POINT('Ctrl Pts',(2.07796671263047,-0.0574972715997812,
-2.01772892919166));
#456081=CARTESIAN_POINT('Ctrl Pts',(0.431845844536463,0.0469975125375793,
-3.20895432402555));
#456082=CARTESIAN_POINT('Ctrl Pts',(-2.44028072323032,0.20373968874362,
-2.13246251833114));
#456083=CARTESIAN_POINT('Ctrl Pts',(-3.1234808703162,0.360481864949661,
0.853089493789302));
#456084=CARTESIAN_POINT('Ctrl Pts',(-1.01789688012564,0.517224041155701,
3.07462896379297));
#456085=CARTESIAN_POINT('Ctrl Pts',(1.99956757050596,0.673966217361742,
2.54812550858646));
#456086=CARTESIAN_POINT('Ctrl Pts',(3.22842986256503,0.830708393567783,
-0.256784391643832));
#456087=CARTESIAN_POINT('Ctrl Pts',(1.57155938565209,0.987450569773824,
-2.8319377882336));
#456088=CARTESIAN_POINT('Ctrl Pts',(-1.49056109299756,1.14419274597986,
-2.87541660522291));
#456089=CARTESIAN_POINT('Ctrl Pts',(-3.21997123622737,1.30093492218591,
-0.348200372027069));
#456090=CARTESIAN_POINT('Ctrl Pts',(-2.07077513505811,1.45767709839195,
2.49028276743826));
#456091=CARTESIAN_POINT('Ctrl Pts',(0.929746590953023,1.61441927459799,
3.10244872330854));
#456092=CARTESIAN_POINT('Ctrl Pts',(3.09904853367837,1.77116145080403,0.940995382104076));
#456093=CARTESIAN_POINT('Ctrl Pts',(2.49778838923158,1.92790362701007,-2.0617109712049));
#456094=CARTESIAN_POINT('Ctrl Pts',(-0.336518242881397,2.08464580321611,
-3.22123450447862));
#456095=CARTESIAN_POINT('Ctrl Pts',(-2.8699723865891,2.24138797942214,-1.50094961276486));
#456096=CARTESIAN_POINT('Ctrl Pts',(-2.83765139342903,2.3981301556282,1.56119473552213));
#456097=CARTESIAN_POINT('Ctrl Pts',(-0.268448608046208,2.55487233183423,
3.22761980643768));
#456098=CARTESIAN_POINT('Ctrl Pts',(2.54074922984435,2.71161450804027,2.00852876103307));
#456099=CARTESIAN_POINT('Ctrl Pts',(3.07849795202298,2.86835668424631,-1.00620156988212));
#456100=CARTESIAN_POINT('Ctrl Pts',(0.864048219136484,3.02509886045235,
-3.12138061370969));
#456101=CARTESIAN_POINT('Ctrl Pts',(-2.12286982313108,3.18184103665839,
-2.44602180697682));
#456102=CARTESIAN_POINT('Ctrl Pts',(-3.21192108363538,3.33858321286443,
0.416097435384728));
#456103=CARTESIAN_POINT('Ctrl Pts',(-1.42950185296324,3.49532538907048,
2.90622457090332));
#456104=CARTESIAN_POINT('Ctrl Pts',(1.63092298236321,3.65206756527651,2.79816156563098));
#456105=CARTESIAN_POINT('Ctrl Pts',(3.23325146599009,3.80880974148256,0.188529092938788));
#456106=CARTESIAN_POINT('Ctrl Pts',(1.94510452195181,3.96555191768859,-2.58966434586268));
#456107=CARTESIAN_POINT('Ctrl Pts',(-1.08212453406731,4.12229409389464,
-3.05265082048802));
#456108=CARTESIAN_POINT('Ctrl Pts',(-3.14164928353259,4.27903627010068,
-0.786598614652181));
#456109=CARTESIAN_POINT('Ctrl Pts',(-2.39304805398794,4.43577844630672,
2.18278150254044));
#456110=CARTESIAN_POINT('Ctrl Pts',(0.495976447516285,4.59252062251276,
3.2005413115711));
#456111=CARTESIAN_POINT('Ctrl Pts',(2.93963162377369,4.7492627987188,1.35737259002624));
#456112=CARTESIAN_POINT('Ctrl Pts',(2.75903742853299,4.90600497492484,-1.70002319637433));
#456113=CARTESIAN_POINT('Ctrl Pts',(0.10421291347106,5.06274715113088,-3.23620431304816));
#456114=CARTESIAN_POINT('Ctrl Pts',(-1.71608250130981,5.16724193526824,
-2.33328878178322));
#456115=CARTESIAN_POINT('Ctrl Pts',(-2.24059110187411,5.21948932733692,
-1.59774743137967));
#456116=CARTESIAN_POINT('Ctrl Pts',(2.64462557919718,-2.77555756156289E-16,
-1.28892185405322));
#456117=CARTESIAN_POINT('Ctrl Pts',(2.22149825342052,0.05224739206868,-2.15709966133247));
#456118=CARTESIAN_POINT('Ctrl Pts',(0.461674762908137,0.156742176206041,
-3.43060665158822));
#456119=CARTESIAN_POINT('Ctrl Pts',(-2.60883840513955,0.313484352412081,
-2.27975825173857));
#456120=CARTESIAN_POINT('Ctrl Pts',(-3.33922928400336,0.470226528618122,
0.91201500435265));
#456121=CARTESIAN_POINT('Ctrl Pts',(-1.08820614286878,0.626968704824163,
3.28700302630733));
#456122=CARTESIAN_POINT('Ctrl Pts',(2.13768384184183,0.783710881030202,
2.72413236093439));
#456123=CARTESIAN_POINT('Ctrl Pts',(3.45142742537007,0.940453057236245,
-0.27452127797577));
#456124=CARTESIAN_POINT('Ctrl Pts',(1.68011181755326,1.09719523344228,-3.02754842612115));
#456125=CARTESIAN_POINT('Ctrl Pts',(-1.5935187241373,1.25393740964832,-3.07403045849226));
#456126=CARTESIAN_POINT('Ctrl Pts',(-3.44238453574088,1.41067958585437,
-0.372251640797132));
#456127=CARTESIAN_POINT('Ctrl Pts',(-2.21380993150506,1.5674217620604,2.66229424406142));
#456128=CARTESIAN_POINT('Ctrl Pts',(0.993967042576552,1.72416393826645,
3.31674438202721));
#456129=CARTESIAN_POINT('Ctrl Pts',(3.31310933085974,1.88090611447249,1.0059928222694));
#456130=CARTESIAN_POINT('Ctrl Pts',(2.67031830219639,2.03764829067853,-2.20411967802495));
#456131=CARTESIAN_POINT('Ctrl Pts',(-0.359762591123905,2.19439046688457,
-3.44373506180883));
#456132=CARTESIAN_POINT('Ctrl Pts',(-3.06821019096211,2.35113264309061,
-1.60462481086063));
#456133=CARTESIAN_POINT('Ctrl Pts',(-3.03365668756983,2.50787481929665,
1.6690312492164));
#456134=CARTESIAN_POINT('Ctrl Pts',(-0.286991177617524,2.6646169955027,
3.45056141617891));
#456135=CARTESIAN_POINT('Ctrl Pts',(2.71624657997229,2.82135917170873,2.14726400931204));
#456136=CARTESIAN_POINT('Ctrl Pts',(3.29113925743328,2.97810134791478,-1.0757030016388));
#456137=CARTESIAN_POINT('Ctrl Pts',(0.923730682505967,3.13484352412081,
-3.33698395622466));
#456138=CARTESIAN_POINT('Ctrl Pts',(-2.26950295962873,3.29158570032686,
-2.61497604316717));
#456139=CARTESIAN_POINT('Ctrl Pts',(-3.43377833439311,3.4483278765329,0.444838562784192));
#456140=CARTESIAN_POINT('Ctrl Pts',(-1.52824193492458,3.60507005273893,
3.10696642495143));
#456141=CARTESIAN_POINT('Ctrl Pts',(1.74357584015234,3.76181222894498,2.99143917612077));
#456142=CARTESIAN_POINT('Ctrl Pts',(3.4565820717474,3.91855440515102,0.201551376225996));
#456143=CARTESIAN_POINT('Ctrl Pts',(2.07945886330698,4.07529658135705,-2.76854041323733));
#456144=CARTESIAN_POINT('Ctrl Pts',(-1.15687019806535,4.2320387575631,-3.26350678516516));
#456145=CARTESIAN_POINT('Ctrl Pts',(-3.35865264530281,4.38878093376914,
-0.840931396047624));
#456146=CARTESIAN_POINT('Ctrl Pts',(-2.55834323041487,4.54552310997518,
2.33355292268079));
#456147=CARTESIAN_POINT('Ctrl Pts',(0.530235063534957,4.70226528618122,
3.42161252653321));
#456148=CARTESIAN_POINT('Ctrl Pts',(3.1426810055327,4.85900746238726,1.45113048233917));
#456149=CARTESIAN_POINT('Ctrl Pts',(2.94961261475119,5.0157496385933,-1.81744901810252));
#456150=CARTESIAN_POINT('Ctrl Pts',(0.111411219367783,5.17249181479934,
-3.45973888101785));
#456151=CARTESIAN_POINT('Ctrl Pts',(-1.83461758853652,5.2769865989367,-2.49445620180102));
#456152=CARTESIAN_POINT('Ctrl Pts',(-2.39535560853235,5.32923399100538,
-1.70810875200399));
#456153=CARTESIAN_POINT('',(2.64462557919717,5.,-1.28892185405324));
#456154=CARTESIAN_POINT('Ctrl Pts',(2.64766952698147,5.,-1.2919603520133));
#456155=CARTESIAN_POINT('Ctrl Pts',(2.59777169898683,5.,-1.37498714432249));
#456156=CARTESIAN_POINT('Ctrl Pts',(2.54371038927642,5.,-1.45514089331332));
#456157=CARTESIAN_POINT('Ctrl Pts',(2.48549510771317,5.,-1.53206201799603));
#456158=CARTESIAN_POINT('Ctrl Pts',(2.42718170236622,5.,-1.60911279578009));
#456159=CARTESIAN_POINT('Ctrl Pts',(2.36469961903881,5.,-1.68292056059732));
#456160=CARTESIAN_POINT('Ctrl Pts',(2.2984276527278,5.,-1.75333415410535));
#456161=CARTESIAN_POINT('Ctrl Pts',(2.22837518703592,5.,-1.82776450705904));
#456162=CARTESIAN_POINT('Ctrl Pts',(2.15408724664126,5.,-1.89840328930852));
#456163=CARTESIAN_POINT('Ctrl Pts',(2.07598025051918,5.,-1.965018936113));
#456164=CARTESIAN_POINT('Ctrl Pts',(2.04180843971577,5.,-1.99416328158996));
#456165=CARTESIAN_POINT('Ctrl Pts',(2.006905334995,5.,-2.02253683217268));
#456166=CARTESIAN_POINT('Ctrl Pts',(1.97130480013543,5.,-2.05011658752475));
#456167=CARTESIAN_POINT('Ctrl Pts',(1.94660081204988,5.,-2.06925478166446));
#456168=CARTESIAN_POINT('Ctrl Pts',(1.92156098161269,5.,-2.08801069507471));
#456169=CARTESIAN_POINT('Ctrl Pts',(1.89619655797919,5.,-2.10637598129296));
#456170=CARTESIAN_POINT('Ctrl Pts',(1.88438047127152,5.,-2.11493150053131));
#456171=CARTESIAN_POINT('Ctrl Pts',(1.87250080990167,5.,-2.12339724242785));
#456172=CARTESIAN_POINT('Ctrl Pts',(1.8605620114611,5.,-2.13177054329346));
#456173=CARTESIAN_POINT('Ctrl Pts',(1.78200362920114,5.,-2.18686762642564));
#456174=CARTESIAN_POINT('Ctrl Pts',(1.70084366480229,5.,-2.23799730804012));
#456175=CARTESIAN_POINT('Ctrl Pts',(1.61744916104773,5.,-2.28501302782822));
#456176=CARTESIAN_POINT('Ctrl Pts',(1.53432547022518,5.,-2.33187607010938));
#456177=CARTESIAN_POINT('Ctrl Pts',(1.44898075932165,5.,-2.37465210593129));
#456178=CARTESIAN_POINT('Ctrl Pts',(1.36176167588437,5.,-2.41314743430364));
#456179=CARTESIAN_POINT('Ctrl Pts',(1.27604812534558,5.,-2.45097827526087));
#456180=CARTESIAN_POINT('Ctrl Pts',(1.18852347245503,5.,-2.48467505469784));
#456181=CARTESIAN_POINT('Ctrl Pts',(1.09951413378954,5.,-2.51400404744347));
#456182=CARTESIAN_POINT('Ctrl Pts',(1.05865424614969,5.,-2.5274675712281));
#456183=CARTESIAN_POINT('Ctrl Pts',(1.01748153675728,5.,-2.54000996680563));
#456184=CARTESIAN_POINT('Ctrl Pts',(0.976028153801408,5.,-2.55160488811041));
#456185=CARTESIAN_POINT('Ctrl Pts',(0.957566358606986,5.,-2.55676883486603));
#456186=CARTESIAN_POINT('Ctrl Pts',(0.939048899883842,5.,-2.56174481989958));
#456187=CARTESIAN_POINT('Ctrl Pts',(0.920478659872387,5.,-2.56653035938024));
#456188=CARTESIAN_POINT('Ctrl Pts',(0.907359430777782,5.,-2.5699111766852));
#456189=CARTESIAN_POINT('Ctrl Pts',(0.894223325226895,5.,-2.57319450150697));
#456190=CARTESIAN_POINT('Ctrl Pts',(0.881071607747158,5.,-2.57637981427696));
#456191=CARTESIAN_POINT('Ctrl Pts',(0.791886436427642,5.,-2.59798023760843));
#456192=CARTESIAN_POINT('Ctrl Pts',(0.701979962263147,5.,-2.61507864060924));
#456193=CARTESIAN_POINT('Ctrl Pts',(0.611667974021129,5.,-2.62750345202927));
#456194=CARTESIAN_POINT('Ctrl Pts',(0.523982886910535,5.,-2.6395668634645));
#456195=CARTESIAN_POINT('Ctrl Pts',(0.435914782332347,5.,-2.6472245845699));
#456196=CARTESIAN_POINT('Ctrl Pts',(0.347756020174879,5.,-2.65027173618512));
#456197=CARTESIAN_POINT('Ctrl Pts',(0.261159272931329,5.,-2.65326489774705));
#456198=CARTESIAN_POINT('Ctrl Pts',(0.174474421690037,5.,-2.65180947160144));
#456199=CARTESIAN_POINT('Ctrl Pts',(0.087991872332091,5.,-2.645664129397));
#456200=CARTESIAN_POINT('Ctrl Pts',(0.0366551246938374,5.,-2.64201620407285));
#456201=CARTESIAN_POINT('Ctrl Pts',(-0.0146100375789589,5.,-2.63671460852521));
#456202=CARTESIAN_POINT('Ctrl Pts',(-0.0657395497789789,5.,-2.62978719346761));
#456203=CARTESIAN_POINT('Ctrl Pts',(-0.0799569026170698,5.,-2.6278609184086));
#456204=CARTESIAN_POINT('Ctrl Pts',(-0.0941655555404146,5.,-2.62580863159305));
#456205=CARTESIAN_POINT('Ctrl Pts',(-0.108358376628224,5.,-2.62363175914501));
#456206=CARTESIAN_POINT('Ctrl Pts',(-0.195234128720159,5.,-2.61030689371046));
#456207=CARTESIAN_POINT('Ctrl Pts',(-0.281231397385426,5.,-2.59236346059264));
#456208=CARTESIAN_POINT('Ctrl Pts',(-0.366064031431315,5.,-2.57003255344105));
#456209=CARTESIAN_POINT('Ctrl Pts',(-0.452588039204867,5.,-2.54725641775098));
#456210=CARTESIAN_POINT('Ctrl Pts',(-0.537901385141664,5.,-2.51991561409353));
#456211=CARTESIAN_POINT('Ctrl Pts',(-0.621678841171493,5.,-2.48820642097155));
#456212=CARTESIAN_POINT('Ctrl Pts',(-0.704710490888595,5.,-2.45677951042919));
#456213=CARTESIAN_POINT('Ctrl Pts',(-0.786234206302495,5.,-2.42106095415721));
#456214=CARTESIAN_POINT('Ctrl Pts',(-0.865900432570674,5.,-2.38120349844864));
#456215=CARTESIAN_POINT('Ctrl Pts',(-0.901637362928322,5.,-2.36332411359997));
#456216=CARTESIAN_POINT('Ctrl Pts',(-0.937000006729313,5.,-2.34461141659527));
#456217=CARTESIAN_POINT('Ctrl Pts',(-0.971954039217656,5.,-2.32507720525684));
#456218=CARTESIAN_POINT('Ctrl Pts',(-0.992269863313026,5.,-2.31372361961473));
#456219=CARTESIAN_POINT('Ctrl Pts',(-1.01244761935627,5.,-2.30209249607874));
#456220=CARTESIAN_POINT('Ctrl Pts',(-1.03248026178061,5.,-2.29018599166716));
#456221=CARTESIAN_POINT('Ctrl Pts',(-1.04555625392411,5.,-2.28241420825265));
#456222=CARTESIAN_POINT('Ctrl Pts',(-1.05856245336876,5.,-2.27452980761246));
#456223=CARTESIAN_POINT('Ctrl Pts',(-1.07149500085763,5.,-2.26653512611973));
#456224=CARTESIAN_POINT('Ctrl Pts',(-1.14590971351802,5.,-2.22053321299281));
#456225=CARTESIAN_POINT('Ctrl Pts',(-1.21791340134486,5.,-2.17086827794226));
#456226=CARTESIAN_POINT('Ctrl Pts',(-1.28718056809639,5.,-2.1177080547548));
#456227=CARTESIAN_POINT('Ctrl Pts',(-1.35260286286025,5.,-2.06749864163476));
#456228=CARTESIAN_POINT('Ctrl Pts',(-1.41558423704355,5.,-2.01417045251016));
#456229=CARTESIAN_POINT('Ctrl Pts',(-1.47581393671382,5.,-1.95784078111152));
#456230=CARTESIAN_POINT('Ctrl Pts',(-1.49258058151295,5.,-1.94215981977247));
#456231=CARTESIAN_POINT('Ctrl Pts',(-1.50913374759254,5.,-1.92624614509165));
#456232=CARTESIAN_POINT('Ctrl Pts',(-1.52546615283854,5.,-1.91010204310153));
#456233=CARTESIAN_POINT('Ctrl Pts',(-1.54179078985554,5.,-1.89396561977719));
#456234=CARTESIAN_POINT('Ctrl Pts',(-1.55789860538532,5.,-1.87759488117163));
#456235=CARTESIAN_POINT('Ctrl Pts',(-1.57376018959548,5.,-1.86101550415345));
#456236=CARTESIAN_POINT('Ctrl Pts',(-1.63176973842762,5.,-1.80038081798342));
#456237=CARTESIAN_POINT('Ctrl Pts',(-1.68654047451408,5.,-1.73690977802179));
#456238=CARTESIAN_POINT('Ctrl Pts',(-1.73775463425817,5.,-1.67073898254984));
#456239=CARTESIAN_POINT('Ctrl Pts',(-1.78752683631336,5.,-1.60643125556886));
#456240=CARTESIAN_POINT('Ctrl Pts',(-1.83394024106878,5.,-1.53957306420248));
#456241=CARTESIAN_POINT('Ctrl Pts',(-1.87665739561666,5.,-1.47027246234511));
#456242=CARTESIAN_POINT('Ctrl Pts',(-1.89552476650306,5.,-1.43966367831601));
#456243=CARTESIAN_POINT('Ctrl Pts',(-1.91367042541382,5.,-1.40857824435308));
#456244=CARTESIAN_POINT('Ctrl Pts',(-1.93106208855765,5.,-1.37702479013102));
#456245=CARTESIAN_POINT('Ctrl Pts',(-0.00203590851197863,4.17782388291041,
-2.93914442058615));
#456246=CARTESIAN_POINT('Ctrl Pts',(-0.336829132197776,4.19589550779464,
-2.9413196673501));
#456247=CARTESIAN_POINT('Ctrl Pts',(-0.670951610256496,4.21396713267887,
-2.8883718851961));
#456248=CARTESIAN_POINT('Ctrl Pts',(-0.984445762376185,4.2320387575631,
-2.77724982499094));
#456249=CARTESIAN_POINT('Ctrl Pts',(-1.89079768047782,4.28428614963178,
-2.45598165545933));
#456250=CARTESIAN_POINT('Ctrl Pts',(-2.62472516289032,4.33653354170046,
-1.64845652575348));
#456251=CARTESIAN_POINT('Ctrl Pts',(-2.85830400161524,4.38878093376914,
-0.715613241112485));
#456252=CARTESIAN_POINT('Ctrl Pts',(-3.09188284034016,4.44102832583782,
0.21723004352851));
#456253=CARTESIAN_POINT('Ctrl Pts',(-2.82511303537752,4.4932757179065,1.27539148310465));
#456254=CARTESIAN_POINT('Ctrl Pts',(-2.17696508390455,4.54552310997518,
1.98581547020146));
#456255=CARTESIAN_POINT('Ctrl Pts',(-1.52881713243159,4.59777050204386,
2.69623945729826));
#456256=CARTESIAN_POINT('Ctrl Pts',(-0.499291034448317,4.65001789411254,
3.05892599191573));
#456257=CARTESIAN_POINT('Ctrl Pts',(0.450879671542943,4.70226528618122,
2.91185558519213));
#456258=CARTESIAN_POINT('Ctrl Pts',(1.4010503775342,4.7545126782499,2.76478517846853));
#456259=CARTESIAN_POINT('Ctrl Pts',(2.27186569153346,4.80676007031858,2.10795783040384));
#456260=CARTESIAN_POINT('Ctrl Pts',(2.67509528340283,4.85900746238726,1.23478090629788));
#456261=CARTESIAN_POINT('Ctrl Pts',(3.03780789065589,4.90600497492484,0.449341828606679));
#456262=CARTESIAN_POINT('Ctrl Pts',(3.02218094071591,4.95300248746242,-0.511153070775355));
#456263=CARTESIAN_POINT('Ctrl Pts',(2.64766952698147,5.,-1.2919603520133));
#456264=CARTESIAN_POINT('',(-1.933077639016,-4.14165229889463E-16,-1.37984607144989));
#456265=CARTESIAN_POINT('Ctrl Pts',(-1.933077639016,-1.28369537222284E-16,
-1.37984607144989));
#456266=CARTESIAN_POINT('Ctrl Pts',(-1.89532807647297,-1.52156718602721E-16,
-1.44943289486579));
#456267=CARTESIAN_POINT('Ctrl Pts',(-1.85404567179292,-5.5994545724509E-16,
-1.5167973757771));
#456268=CARTESIAN_POINT('Ctrl Pts',(-1.80931650950957,-4.71844785465692E-16,
-1.58163386949399));
#456269=CARTESIAN_POINT('Ctrl Pts',(-1.76313966209286,-4.1029866518598E-16,
-1.64856883372233));
#456270=CARTESIAN_POINT('Ctrl Pts',(-1.71329020780722,-3.33757425938898E-17,
-1.71281097695907));
#456271=CARTESIAN_POINT('Ctrl Pts',(-1.66013224533709,-1.17961196366423E-16,
-1.77428904127593));
#456272=CARTESIAN_POINT('Ctrl Pts',(-1.60565559962016,-2.04644951421197E-16,
-1.83729218461563));
#456273=CARTESIAN_POINT('Ctrl Pts',(-1.54770382896436,-9.8490908232494E-17,
-1.89739296998819));
#456274=CARTESIAN_POINT('Ctrl Pts',(-1.48661891555315,-1.04083408558608E-16,
-1.95449269968886));
#456275=CARTESIAN_POINT('Ctrl Pts',(-1.45602320550481,-1.06884534219067E-16,
-1.9830923436304));
#456276=CARTESIAN_POINT('Ctrl Pts',(-1.42464074526194,2.32982061359826E-17,
-2.01093871168437));
#456277=CARTESIAN_POINT('Ctrl Pts',(-1.39251053984076,5.55111512312578E-17,
-2.03801671409802));
#456278=CARTESIAN_POINT('Ctrl Pts',(-1.3768777861536,7.1184161397586E-17,
-2.05119134950803));
#456279=CARTESIAN_POINT('Ctrl Pts',(-1.36106798614324,-3.743924605594E-16,
-2.06418406406673));
#456280=CARTESIAN_POINT('Ctrl Pts',(-1.34508543738201,-3.95516952522712E-16,
-2.07699294275887));
#456281=CARTESIAN_POINT('Ctrl Pts',(-1.33369101195484,-4.1057721931486E-16,
-2.08612476617724));
#456282=CARTESIAN_POINT('Ctrl Pts',(-1.32220764071915,-2.65297351874512E-16,
-2.09516392713986));
#456283=CARTESIAN_POINT('Ctrl Pts',(-1.31065148118413,-2.63677968348475E-16,
-2.10409868877453));
#456284=CARTESIAN_POINT('Ctrl Pts',(-1.24222625606192,-2.54089429700109E-16,
-2.15700234369662));
#456285=CARTESIAN_POINT('Ctrl Pts',(-1.17114186898617,-4.67606722770874E-16,
-2.20633836212491));
#456286=CARTESIAN_POINT('Ctrl Pts',(-1.09779843894241,-4.30211422042248E-16,
-2.25202821416137));
#456287=CARTESIAN_POINT('Ctrl Pts',(-1.02293203288172,-3.92039608050997E-16,
-2.29866681578355));
#456288=CARTESIAN_POINT('Ctrl Pts',(-0.945711177090165,-1.63700498024063E-16,
-2.3415068643473));
#456289=CARTESIAN_POINT('Ctrl Pts',(-0.866514269650375,-9.71445146547012E-17,
-2.3804362849433));
#456290=CARTESIAN_POINT('Ctrl Pts',(-0.786645850745298,-3.00242023568398E-17,
-2.41969578853259));
#456291=CARTESIAN_POINT('Ctrl Pts',(-0.704766937132996,-2.88590153679237E-16,
-2.45497867949436));
#456292=CARTESIAN_POINT('Ctrl Pts',(-0.621228987646033,-3.19189119579733E-16,
-2.48613204577019));
#456293=CARTESIAN_POINT('Ctrl Pts',(-0.581673633799112,-3.33677779296391E-16,
-2.50088321495893));
#456294=CARTESIAN_POINT('Ctrl Pts',(-0.541745863454635,6.25627410058756E-18,
-2.51470792407002));
#456295=CARTESIAN_POINT('Ctrl Pts',(-0.501480960483928,2.77555756156289E-17,
-2.52758639081626));
#456296=CARTESIAN_POINT('Ctrl Pts',(-0.487866421796609,3.50250100518627E-17,
-2.53194091226829));
#456297=CARTESIAN_POINT('Ctrl Pts',(-0.474211239587608,-3.14606215261237E-16,
-2.5361878604183));
#456298=CARTESIAN_POINT('Ctrl Pts',(-0.460523451066253,-3.19189119579733E-16,
-2.54032438870088));
#456299=CARTESIAN_POINT('Ctrl Pts',(-0.372759577575939,-3.48573956596984E-16,
-2.56684713518507));
#456300=CARTESIAN_POINT('Ctrl Pts',(-0.283929367672986,1.93097192062426E-16,
-2.58875295217812));
#456301=CARTESIAN_POINT('Ctrl Pts',(-0.194437403031281,1.11022302462516E-16,
-2.6059343032564));
#456302=CARTESIAN_POINT('Ctrl Pts',(-0.103893064284477,2.79822593000515E-17,
-2.62331769715538));
#456303=CARTESIAN_POINT('Ctrl Pts',(-0.0126704435857078,-3.49772123788992E-16,
-2.63586550789051));
#456304=CARTESIAN_POINT('Ctrl Pts',(0.0788443475852407,-4.44089209850063E-16,
-2.64342393748993));
#456305=CARTESIAN_POINT('Ctrl Pts',(0.170359138756189,-5.38406295911133E-16,
-2.65098236708935));
#456306=CARTESIAN_POINT('Ctrl Pts',(0.262167072908716,-3.46469882950404E-16,
-2.65355201154631));
#456307=CARTESIAN_POINT('Ctrl Pts',(0.353900769383215,-3.60822483003176E-16,
-2.65092764013621));
#456308=CARTESIAN_POINT('Ctrl Pts',(0.385666279468855,-3.65792495978269E-16,
-2.65001887378644));
#456309=CARTESIAN_POINT('Ctrl Pts',(0.417422984221464,-3.15737365300549E-16,
-2.64848679865193));
#456310=CARTESIAN_POINT('Ctrl Pts',(0.449159149942652,-3.60822483003176E-16,
-2.64634069604619));
#456311=CARTESIAN_POINT('Ctrl Pts',(0.478242203475635,-4.02138529283176E-16,
-2.64437400550397));
#456312=CARTESIAN_POINT('Ctrl Pts',(0.507308011629989,2.3581128298129E-16,
-2.64189164976937));
#456313=CARTESIAN_POINT('Ctrl Pts',(0.536347540593685,2.4980018054066E-16,
-2.6389001481074));
#456314=CARTESIAN_POINT('Ctrl Pts',(0.551459749915564,2.57080021352259E-16,
-2.63734336668167));
#456315=CARTESIAN_POINT('Ctrl Pts',(0.566557585451425,-7.49710942941346E-17,
-2.63564938922174));
#456316=CARTESIAN_POINT('Ctrl Pts',(0.581631815384825,-8.32667268468867E-17,
-2.63382058033555));
#456317=CARTESIAN_POINT('Ctrl Pts',(0.670051497316618,-1.31925742596153E-16,
-2.62309348510443));
#456318=CARTESIAN_POINT('Ctrl Pts',(0.757742399593695,-4.64943073742605E-16,
-2.60772302192463));
#456319=CARTESIAN_POINT('Ctrl Pts',(0.844442802535061,-4.44089209850063E-16,
-2.58799378064736));
#456320=CARTESIAN_POINT('Ctrl Pts',(0.936342565858583,-4.21984754840762E-16,
-2.5670813910572));
#456321=CARTESIAN_POINT('Ctrl Pts',(1.02713016079202,-4.81429995614911E-17,
-2.5412720037515));
#456322=CARTESIAN_POINT('Ctrl Pts',(1.11650347932395,-5.55111512312578E-17,
-2.51084435510587));
#456323=CARTESIAN_POINT('Ctrl Pts',(1.19470513303939,-6.19582839423037E-17,
-2.48422016254094));
#456324=CARTESIAN_POINT('Ctrl Pts',(1.27182449504503,-1.67579479506498E-16,
-2.45405903679538));
#456325=CARTESIAN_POINT('Ctrl Pts',(1.34765770122539,-1.94289029309402E-16,
-2.42051198984039));
#456326=CARTESIAN_POINT('Ctrl Pts',(1.38721814572807,-2.08222788883755E-16,
-2.40301126481321));
#456327=CARTESIAN_POINT('Ctrl Pts',(1.42642849848376,-4.25350705594898E-16,
-2.38458854018203));
#456328=CARTESIAN_POINT('Ctrl Pts',(1.46525900971977,-4.44089209850063E-16,
-2.36526192397698));
#456329=CARTESIAN_POINT('Ctrl Pts',(1.484999107099,-4.53615221405509E-16,
-2.35543693651854));
#456330=CARTESIAN_POINT('Ctrl Pts',(1.50464102824796,-4.87876039166925E-16,
-2.34537831594886));
#456331=CARTESIAN_POINT('Ctrl Pts',(1.5241807798872,-4.9960036108132E-16,
-2.33508822707005));
#456332=CARTESIAN_POINT('Ctrl Pts',(1.54114636093401,-5.09780118599735E-16,
-2.3261537564547));
#456333=CARTESIAN_POINT('Ctrl Pts',(1.55803735509877,-7.87150475752769E-16,
-2.31704331667934));
#456334=CARTESIAN_POINT('Ctrl Pts',(1.57482950976773,-7.49400541621981E-16,
-2.30777053426273));
#456335=CARTESIAN_POINT('Ctrl Pts',(1.6591161715088,-5.59918251138288E-16,
-2.2612266636067));
#456336=CARTESIAN_POINT('Ctrl Pts',(1.74102715047747,-4.04388893131409E-16,
-2.21053856448965));
#456337=CARTESIAN_POINT('Ctrl Pts',(1.82025851350983,-3.33066907387547E-16,
-2.15596765860826));
#456338=CARTESIAN_POINT('Ctrl Pts',(1.90298412714173,-2.58599489305927E-16,
-2.09899007419332));
#456339=CARTESIAN_POINT('Ctrl Pts',(1.98278965579871,-3.73079251431402E-16,
-2.03777961061421));
#456340=CARTESIAN_POINT('Ctrl Pts',(2.05931407031973,-3.33066907387547E-16,
-1.97257640891715));
#456341=CARTESIAN_POINT('Ctrl Pts',(2.08396786441214,-3.20176170524201E-16,
-1.95156995863763));
#456342=CARTESIAN_POINT('Ctrl Pts',(2.10828091810247,-2.11292956691504E-16,
-1.93014866511807));
#456343=CARTESIAN_POINT('Ctrl Pts',(2.13224054147413,-1.66533453693773E-16,
-1.90831938598655));
#456344=CARTESIAN_POINT('Ctrl Pts',(2.1496381596241,-1.34032577963915E-16,
-1.89246865841341));
#456345=CARTESIAN_POINT('Ctrl Pts',(2.16685262378074,2.800261672271E-16,
-1.8763995725127));
#456346=CARTESIAN_POINT('Ctrl Pts',(2.18385811644504,2.22044604925031E-16,
-1.86013502292615));
#456347=CARTESIAN_POINT('Ctrl Pts',(2.25541917496481,-2.19484421966021E-17,
-1.79169193763969));
#456348=CARTESIAN_POINT('Ctrl Pts',(2.32334946150237,3.44588198098228E-16,
-1.71973181756775));
#456349=CARTESIAN_POINT('Ctrl Pts',(2.38732344826083,2.22044604925031E-16,
-1.6444973753988));
#456350=CARTESIAN_POINT('Ctrl Pts',(2.4505231820554,1.00984110508486E-16,
-1.57017346722636));
#456351=CARTESIAN_POINT('Ctrl Pts',(2.50986262459353,-7.05684391623025E-17,
-1.49265350674278));
#456352=CARTESIAN_POINT('Ctrl Pts',(2.56500198087084,1.11022302462516E-16,
-1.41212853769079));
#456353=CARTESIAN_POINT('Ctrl Pts',(2.59261215492151,2.01951038681995E-16,
-1.37180691333651));
#456354=CARTESIAN_POINT('Ctrl Pts',(2.61916873567462,-2.90545575616215E-16,
-1.3307311985444));
#456355=CARTESIAN_POINT('Ctrl Pts',(2.64462557919718,-2.77555756156289E-16,
-1.28892185405322));
#456356=CARTESIAN_POINT('Ctrl Pts',(-1.933077639016,-4.11996825544492E-16,
-1.37984607144989));
#456357=CARTESIAN_POINT('Ctrl Pts',(-2.33483719992212,0.046997512537579,
-0.808909857124196));
#456358=CARTESIAN_POINT('Ctrl Pts',(-2.63120278751596,0.146242417143839,
0.799366979810314));
#456359=CARTESIAN_POINT('Ctrl Pts',(-0.877278354639368,0.297734713818778,
2.64988083876425));
#456360=CARTESIAN_POINT('Ctrl Pts',(1.72333502783425,0.454476890024819,
2.1961118038906));
#456361=CARTESIAN_POINT('Ctrl Pts',(2.78243473695495,0.61121906623086,-0.221310618979959));
#456362=CARTESIAN_POINT('Ctrl Pts',(1.58559547981109,0.742590066857593,
-2.08147091584782));
#456363=CARTESIAN_POINT('Ctrl Pts',(0.401815805903339,0.821713675415647,
-2.36781552309403));
#456364=CARTESIAN_POINT('Ctrl Pts',(-0.00016282762489446,0.848589891905021,
-2.36808927594338));
#456365=CARTESIAN_POINT('Origin',(0.,-1.84858989190502,0.));
#456366=CARTESIAN_POINT('',(-1.93106208855765,0.,1.37702479013102));
#456367=CARTESIAN_POINT('Origin',(0.,0.,0.));
#456368=CARTESIAN_POINT('Ctrl Pts',(-1.93106208855765,0.,1.37702479013102));
#456369=CARTESIAN_POINT('Ctrl Pts',(-1.4790123268564,0.0522473920686803,
2.01095394174763));
#456370=CARTESIAN_POINT('Ctrl Pts',(0.0898090403048579,0.15674217620604,
2.78913936379167));
#456371=CARTESIAN_POINT('Ctrl Pts',(2.37789101898706,0.313484352412081,
1.46516877387106));
#456372=CARTESIAN_POINT('Ctrl Pts',(2.53352964655122,0.470226528618122,
-1.16985536842112));
#456373=CARTESIAN_POINT('Ctrl Pts',(1.02001467838193,0.582868447179088,
-2.31145363948848));
#456374=CARTESIAN_POINT('Ctrl Pts',(0.123040243631729,0.643262973671374,
-2.37443199566777));
#456375=CARTESIAN_POINT('Ctrl Pts',(0.00189242379211238,0.651410108094979,
-2.37343051434144));
#456376=CARTESIAN_POINT('Ctrl Pts',(-2.39535560853235,-0.329233991005384,
1.70810875200399));
#456377=CARTESIAN_POINT('Ctrl Pts',(-1.83461758853653,-0.276986598936704,
2.49445620180101));
#456378=CARTESIAN_POINT('Ctrl Pts',(0.111402212112104,-0.172491814799343,
3.45974407432279));
#456379=CARTESIAN_POINT('Ctrl Pts',(2.94961753045639,-0.0157496385933027,
1.81744557087748));
#456380=CARTESIAN_POINT('Ctrl Pts',(3.14267701914353,0.140992537612738,
-1.45112869986083));
#456381=CARTESIAN_POINT('Ctrl Pts',(0.530237091421392,0.297734713818779,
-3.42161261807561));
#456382=CARTESIAN_POINT('Ctrl Pts',(-2.55834405952998,0.454476890024821,
-2.33355215525395));
#456383=CARTESIAN_POINT('Ctrl Pts',(-3.35865124878684,0.61121906623086,
0.840931084698363));
#456384=CARTESIAN_POINT('Ctrl Pts',(-1.15687044439419,0.767961242436902,
3.26350625644717));
#456385=CARTESIAN_POINT('Ctrl Pts',(2.07945874789012,0.924703418642941,
2.76853987221247));
#456386=CARTESIAN_POINT('Ctrl Pts',(3.45658128248051,1.08144559484898,-0.201551325322282));
#456387=CARTESIAN_POINT('Ctrl Pts',(1.74357560709307,1.23818777105502,-2.99143863175781));
#456388=CARTESIAN_POINT('Ctrl Pts',(-1.52824170343262,1.39492994726106,
-3.10696585134584));
#456389=CARTESIAN_POINT('Ctrl Pts',(-3.43377767510254,1.55167212346711,
-0.444838481739954));
#456390=CARTESIAN_POINT('Ctrl Pts',(-2.26950255774756,1.70841429967315,
2.61497556244688));
#456391=CARTESIAN_POINT('Ctrl Pts',(0.923730521087739,1.86515647587919,
3.33698334261355));
#456392=CARTESIAN_POINT('Ctrl Pts',(3.2911386478096,2.02189865208523,1.07570280366772));
#456393=CARTESIAN_POINT('Ctrl Pts',(2.71624608233216,2.17864082829127,-2.1472636142096));
#456394=CARTESIAN_POINT('Ctrl Pts',(-0.286991124867996,2.33538300449731,
-3.450560781959));
#456395=CARTESIAN_POINT('Ctrl Pts',(-3.03365613149575,2.49212518070335,
-1.66903094175379));
#456396=CARTESIAN_POINT('Ctrl Pts',(-3.06820962241996,2.64886735690939,
1.60462451489878));
#456397=CARTESIAN_POINT('Ctrl Pts',(-0.359762533293265,2.80560953311543,
3.44373442996229));
#456398=CARTESIAN_POINT('Ctrl Pts',(2.6703178264213,2.96235170932147,2.20411927030135));
#456399=CARTESIAN_POINT('Ctrl Pts',(3.31310869401662,3.11909388552751,-1.00599263342273));
#456400=CARTESIAN_POINT('Ctrl Pts',(0.993966909026026,3.27583606173356,
-3.31674377806021));
#456401=CARTESIAN_POINT('Ctrl Pts',(-2.21380961171835,3.43257823793959,
-2.66229374567994));
#456402=CARTESIAN_POINT('Ctrl Pts',(-3.4423837489093,3.58932041414564,0.372251560613112));
#456403=CARTESIAN_POINT('Ctrl Pts',(-1.59351869968456,3.74606259035167,
3.07402990583413));
#456404=CARTESIAN_POINT('Ctrl Pts',(1.68011197315232,3.90280476655772,3.02754786397388));
#456405=CARTESIAN_POINT('Ctrl Pts',(3.45142599660708,4.05954694276376,0.274521201611494));
#456406=CARTESIAN_POINT('Ctrl Pts',(2.13768478634502,4.2162891189698,-2.72413174102351));
#456407=CARTESIAN_POINT('Ctrl Pts',(-1.08820815801459,4.37303129517584,
-3.28700278158138));
#456408=CARTESIAN_POINT('Ctrl Pts',(-3.33922505791938,4.52977347138188,
-0.912013904924703));
#456409=CARTESIAN_POINT('Ctrl Pts',(-2.60884382278974,4.68651564758792,
2.27975566396261));
#456410=CARTESIAN_POINT('Ctrl Pts',(0.461684504345609,4.84325782379396,
3.43061028552098));
#456411=CARTESIAN_POINT('Ctrl Pts',(2.22149825342054,4.94775260793132,2.15709966133245));
#456412=CARTESIAN_POINT('Ctrl Pts',(2.64462557919719,5.,1.2889218540532));
#456413=CARTESIAN_POINT('Ctrl Pts',(-2.24059110187412,-0.219489327336923,
1.59774743137966));
#456414=CARTESIAN_POINT('Ctrl Pts',(-1.71608250130982,-0.167241935268243,
2.33328878178322));
#456415=CARTESIAN_POINT('Ctrl Pts',(0.104204488176356,-0.0627471511308821,
3.23620917081242));
#456416=CARTESIAN_POINT('Ctrl Pts',(2.75904202663328,0.093995025075159,
1.70001997187534));
#456417=CARTESIAN_POINT('Ctrl Pts',(2.9396278949461,0.250737201281199,-1.35737092271426));
#456418=CARTESIAN_POINT('Ctrl Pts',(0.495978344380483,0.407479377487241,
-3.20054139719892));
#456419=CARTESIAN_POINT('Ctrl Pts',(-2.39304882953372,0.564221553693281,
-2.18278078469723));
#456420=CARTESIAN_POINT('Ctrl Pts',(-3.14164797724586,0.720963729899322,
0.786598323419274));
#456421=CARTESIAN_POINT('Ctrl Pts',(-1.08212476448077,0.877705906105362,
3.05265032593063));
#456422=CARTESIAN_POINT('Ctrl Pts',(1.94510441399205,1.0344480823114,2.58966383979358));
#456423=CARTESIAN_POINT('Ctrl Pts',(3.23325072771793,1.19119025851744,-0.188529045323978));
#456424=CARTESIAN_POINT('Ctrl Pts',(1.63092276436196,1.34793243472348,-2.79816105643945));
#456425=CARTESIAN_POINT('Ctrl Pts',(-1.42950163642804,1.50467461092953,
-2.90622403435854));
#456426=CARTESIAN_POINT('Ctrl Pts',(-3.21192046694174,1.66141678713557,
-0.416097359576775));
#456427=CARTESIAN_POINT('Ctrl Pts',(-2.12286944721554,1.81815896334161,
2.44602135731598));
#456428=CARTESIAN_POINT('Ctrl Pts',(0.864048068147532,1.97490113954765,
3.12138003974414));
#456429=CARTESIAN_POINT('Ctrl Pts',(3.07849738178723,2.13164331575369,1.00620138470199));
#456430=CARTESIAN_POINT('Ctrl Pts',(2.54074876435687,2.28838549195973,-2.00852839145829));
#456431=CARTESIAN_POINT('Ctrl Pts',(-0.268448558704848,2.44512766816577,
-3.22761921319488));
#456432=CARTESIAN_POINT('Ctrl Pts',(-2.83765087328303,2.60186984437181,
-1.56119444792475));
#456433=CARTESIAN_POINT('Ctrl Pts',(-2.8699718547806,2.75861202057785,1.50094933592518));
#456434=CARTESIAN_POINT('Ctrl Pts',(-0.336518188787201,2.91535419678389,
3.22123391345584));
#456435=CARTESIAN_POINT('Ctrl Pts',(2.49778794419642,3.07209637298993,2.06171058982443));
#456436=CARTESIAN_POINT('Ctrl Pts',(3.09904793798184,3.22883854919597,-0.940995205458836));
#456437=CARTESIAN_POINT('Ctrl Pts',(0.929746466031224,3.38558072540202,
-3.10244815836399));
#456438=CARTESIAN_POINT('Ctrl Pts',(-2.07077483593289,3.54232290160805,
-2.49028230125733));
#456439=CARTESIAN_POINT('Ctrl Pts',(-3.21997050023317,3.6990650778141,0.348200297023759));
#456440=CARTESIAN_POINT('Ctrl Pts',(-1.49056107012472,3.85580725402014,
2.87541608827217));
#456441=CARTESIAN_POINT('Ctrl Pts',(1.57155953119785,4.01254943022618,2.83193726240679));
#456442=CARTESIAN_POINT('Ctrl Pts',(3.22842852611477,4.16929160643222,0.256784320213471));
#456443=CARTESIAN_POINT('Ctrl Pts',(1.99956845398457,4.32603378263826,-2.54812492872817));
#456444=CARTESIAN_POINT('Ctrl Pts',(-1.0178987650724,4.4827759588443,-3.07462873487882));
#456445=CARTESIAN_POINT('Ctrl Pts',(-3.12347691728053,4.63951813505034,
-0.853088465395663));
#456446=CARTESIAN_POINT('Ctrl Pts',(-2.44028579084482,4.79626031125639,
2.13246009775202));
#456447=CARTESIAN_POINT('Ctrl Pts',(0.431854956577303,4.95300248746242,
3.20895772316902));
#456448=CARTESIAN_POINT('Ctrl Pts',(2.07796671263048,5.05749727159978,2.01772892919164));
#456449=CARTESIAN_POINT('Ctrl Pts',(2.47375567929495,5.10974466366846,1.20564430054381));
#456450=CARTESIAN_POINT('Ctrl Pts',(-2.08582659521588,-0.109744663668461,
1.48738611075534));
#456451=CARTESIAN_POINT('Ctrl Pts',(-1.59754741408311,-0.0574972715997809,
2.17212136176543));
#456452=CARTESIAN_POINT('Ctrl Pts',(0.0970067642406067,0.0469975125375791,
3.01267426730204));
#456453=CARTESIAN_POINT('Ctrl Pts',(2.56846652281017,0.20373968874362,1.5825943728732));
#456454=CARTESIAN_POINT('Ctrl Pts',(2.73657877074866,0.360481864949661,
-1.26361314556769));
#456455=CARTESIAN_POINT('Ctrl Pts',(0.461719597339576,0.517224041155702,
-2.97947017632224));
#456456=CARTESIAN_POINT('Ctrl Pts',(-2.22775359953746,0.673966217361742,
-2.03200941414052));
#456457=CARTESIAN_POINT('Ctrl Pts',(-2.92464470570488,0.830708393567783,
0.732265562140186));
#456458=CARTESIAN_POINT('Ctrl Pts',(-1.00737908456736,0.987450569773825,
2.84179439541409));
#456459=CARTESIAN_POINT('Ctrl Pts',(1.81075008009398,1.14419274597986,2.41078780737468));
#456460=CARTESIAN_POINT('Ctrl Pts',(3.00992017295535,1.30093492218591,-0.175506765325674));
#456461=CARTESIAN_POINT('Ctrl Pts',(1.51826992163084,1.45767709839194,-2.60488348112109));
#456462=CARTESIAN_POINT('Ctrl Pts',(-1.33076156942346,1.61441927459799,
-2.70548221737123));
#456463=CARTESIAN_POINT('Ctrl Pts',(-2.99006325878094,1.77116145080402,
-0.387356237413599));
#456464=CARTESIAN_POINT('Ctrl Pts',(-1.97623633668353,1.92790362701007,
2.27706715218508));
#456465=CARTESIAN_POINT('Ctrl Pts',(0.804365615207322,2.08464580321611,
2.90577673687474));
#456466=CARTESIAN_POINT('Ctrl Pts',(2.86585611576487,2.24138797942215,0.936699965736267));
#456467=CARTESIAN_POINT('Ctrl Pts',(2.36525144638157,2.39813015562819,-1.86979316870699));
#456468=CARTESIAN_POINT('Ctrl Pts',(-0.249905992541696,2.55487233183423,
-3.00467764443076));
#456469=CARTESIAN_POINT('Ctrl Pts',(-2.64164561507031,2.71161450804028,
-1.45335795409571));
#456470=CARTESIAN_POINT('Ctrl Pts',(-2.67173408714124,2.86835668424631,
1.39727415695158));
#456471=CARTESIAN_POINT('Ctrl Pts',(-0.313273844281141,3.02509886045236,
2.99873339694938));
#456472=CARTESIAN_POINT('Ctrl Pts',(2.32525806197155,3.18184103665839,1.9193019093475));
#456473=CARTESIAN_POINT('Ctrl Pts',(2.88498718194706,3.33858321286444,-0.875997777494947));
#456474=CARTESIAN_POINT('Ctrl Pts',(0.865526023036425,3.49532538907048,
-2.88815253866777));
#456475=CARTESIAN_POINT('Ctrl Pts',(-1.92774006014744,3.65206756527652,
-2.31827085683471));
#456476=CARTESIAN_POINT('Ctrl Pts',(-2.99755725155704,3.80880974148256,
0.32414903343441));
#456477=CARTESIAN_POINT('Ctrl Pts',(-1.38760344056488,3.9655519176886,2.6768022707102));
#456478=CARTESIAN_POINT('Ctrl Pts',(1.46300708924339,4.12229409389464,2.63632666083971));
#456479=CARTESIAN_POINT('Ctrl Pts',(3.00543105562245,4.27903627010068,0.239047438815444));
#456480=CARTESIAN_POINT('Ctrl Pts',(1.86145212162413,4.43577844630672,-2.37211811643283));
#456481=CARTESIAN_POINT('Ctrl Pts',(-0.947589372130199,4.59252062251276,
-2.86225468817626));
#456482=CARTESIAN_POINT('Ctrl Pts',(-2.90772877664167,4.74926279871881,
-0.794163025866617));
#456483=CARTESIAN_POINT('Ctrl Pts',(-2.2717277588999,4.90600497492485,1.98516453154143));
#456484=CARTESIAN_POINT('Ctrl Pts',(0.402025408808995,5.06274715113088,
2.98730516081707));
#456485=CARTESIAN_POINT('Ctrl Pts',(1.93443517184043,5.16724193526824,1.87835819705082));
#456486=CARTESIAN_POINT('Ctrl Pts',(2.3028857793927,5.21948932733692,1.12236674703442));
#456487=CARTESIAN_POINT('Ctrl Pts',(-1.93106208855765,0.,1.37702479013102));
#456488=CARTESIAN_POINT('Ctrl Pts',(-1.4790123268564,0.0522473920686803,
2.01095394174763));
#456489=CARTESIAN_POINT('Ctrl Pts',(0.0898090403048579,0.15674217620604,
2.78913936379167));
#456490=CARTESIAN_POINT('Ctrl Pts',(2.37789101898706,0.313484352412081,
1.46516877387106));
#456491=CARTESIAN_POINT('Ctrl Pts',(2.53352964655122,0.470226528618122,
-1.16985536842112));
#456492=CARTESIAN_POINT('Ctrl Pts',(0.427460850298667,0.626968704824163,
-2.75839895544555));
#456493=CARTESIAN_POINT('Ctrl Pts',(-2.06245836954121,0.783710881030204,
-1.88123804358381));
#456494=CARTESIAN_POINT('Ctrl Pts',(-2.7076414341639,0.940453057236244,
0.677932800861099));
#456495=CARTESIAN_POINT('Ctrl Pts',(-0.932633404653946,1.09719523344229,
2.63093846489754));
#456496=CARTESIAN_POINT('Ctrl Pts',(1.67639574619592,1.25393740964833,2.23191177495579));
#456497=CARTESIAN_POINT('Ctrl Pts',(2.78658961819278,1.41067958585437,-0.162484485327371));
#456498=CARTESIAN_POINT('Ctrl Pts',(1.40561707889972,1.56742176206041,-2.41160590580272));
#456499=CARTESIAN_POINT('Ctrl Pts',(-1.23202150241888,1.72416393826645,
-2.50474040038392));
#456500=CARTESIAN_POINT('Ctrl Pts',(-2.76820605062014,1.88090611447249,
-0.358615115250419));
#456501=CARTESIAN_POINT('Ctrl Pts',(-1.82960322615152,2.03764829067853,
2.10811294705418));
#456502=CARTESIAN_POINT('Ctrl Pts',(0.744683162267116,2.19439046688457,
2.69017343400533));
#456503=CARTESIAN_POINT('Ctrl Pts',(2.65321484974249,2.35113264309061,0.867198546770537));
#456504=CARTESIAN_POINT('Ctrl Pts',(2.18975412840629,2.50787481929665,-1.73105794595568));
#456505=CARTESIAN_POINT('Ctrl Pts',(-0.231363426378548,2.66461699550269,
-2.78173607566664));
#456506=CARTESIAN_POINT('Ctrl Pts',(-2.44564035685759,2.82135917170873,
-1.34552146026667));
#456507=CARTESIAN_POINT('Ctrl Pts',(-2.47349631950189,2.97810134791478,
1.29359897797797));
#456508=CARTESIAN_POINT('Ctrl Pts',(-0.29002949977508,3.13484352412081,
2.77623288044292));
#456509=CARTESIAN_POINT('Ctrl Pts',(2.15272817974667,3.29158570032686,1.77689322887057));
#456510=CARTESIAN_POINT('Ctrl Pts',(2.67092642591228,3.44832787653289,-0.811000349531056));
#456511=CARTESIAN_POINT('Ctrl Pts',(0.801305580041626,3.60507005273894,
-2.67385691897155));
#456512=CARTESIAN_POINT('Ctrl Pts',(-1.78470528436199,3.76181222894497,
-2.1462594124121));
#456513=CARTESIAN_POINT('Ctrl Pts',(-2.77514400288091,3.91855440515103,
0.300097769845058));
#456514=CARTESIAN_POINT('Ctrl Pts',(-1.28464581100504,4.07529658135705,
2.47818845314823));
#456515=CARTESIAN_POINT('Ctrl Pts',(1.35445464728892,4.2320387575631,2.44071605927262));
#456516=CARTESIAN_POINT('Ctrl Pts',(2.78243358513013,4.38878093376914,0.221310557417421));
#456517=CARTESIAN_POINT('Ctrl Pts',(1.72333578926369,4.54552310997518,-2.19611130413749));
#456518=CARTESIAN_POINT('Ctrl Pts',(-0.877279979188005,4.70226528618122,
-2.6498806414737));
#456519=CARTESIAN_POINT('Ctrl Pts',(-2.69198063600282,4.85900746238726,
-0.735237586337578));
#456520=CARTESIAN_POINT('Ctrl Pts',(-2.10316972695498,5.01574963859331,
1.83786896533084));
#456521=CARTESIAN_POINT('Ctrl Pts',(0.372195861040687,5.17249181479935,
2.76565259846512));
#456522=CARTESIAN_POINT('Ctrl Pts',(1.79090363105037,5.27698659893671,1.73898746491001));
#456523=CARTESIAN_POINT('Ctrl Pts',(2.13201587949046,5.32923399100539,1.03908919352504));
#456524=CARTESIAN_POINT('',(2.64462557919717,5.,1.28892185405323));
#456525=CARTESIAN_POINT('Ctrl Pts',(-1.93307880200417,5.,1.37984525234447));
#456526=CARTESIAN_POINT('Ctrl Pts',(-1.89532923114376,5.,1.44943208196965));
#456527=CARTESIAN_POINT('Ctrl Pts',(-1.8540467895405,5.,1.51679658079351));
#456528=CARTESIAN_POINT('Ctrl Pts',(-1.80931755641146,5.,1.58163310600374));
#456529=CARTESIAN_POINT('Ctrl Pts',(-1.76314072863898,5.,1.64856796825283));
#456530=CARTESIAN_POINT('Ctrl Pts',(-1.71329127262828,5.,1.71281003478393));
#456531=CARTESIAN_POINT('Ctrl Pts',(-1.66013329288395,5.,1.7742880449691));
#456532=CARTESIAN_POINT('Ctrl Pts',(-1.60565658732334,5.,1.83729118157092));
#456533=CARTESIAN_POINT('Ctrl Pts',(-1.54770473511596,5.,1.8973919794258));
#456534=CARTESIAN_POINT('Ctrl Pts',(-1.48661972537529,5.,1.95449173807213));
#456535=CARTESIAN_POINT('Ctrl Pts',(-1.45602391706679,5.,1.98309144326039));
#456536=CARTESIAN_POINT('Ctrl Pts',(-1.42464135228175,5.,2.01093787423408));
#456537=CARTESIAN_POINT('Ctrl Pts',(-1.39251103708368,5.,2.03801594084573));
#456538=CARTESIAN_POINT('Ctrl Pts',(-1.37687840864276,5.,2.05119045692593));
#456539=CARTESIAN_POINT('Ctrl Pts',(-1.36106873668559,5.,2.06418305661536));
#456540=CARTESIAN_POINT('Ctrl Pts',(-1.34508631875706,5.,2.07699182491987));
#456541=CARTESIAN_POINT('Ctrl Pts',(-1.33369143914598,5.,2.08612400838853));
#456542=CARTESIAN_POINT('Ctrl Pts',(-1.32220760631118,5.,2.09516352299594));
#456543=CARTESIAN_POINT('Ctrl Pts',(-1.31065097934111,5.,2.10409863074976));
#456544=CARTESIAN_POINT('Ctrl Pts',(-1.24222560571871,5.,2.15700230999759));
#456545=CARTESIAN_POINT('Ctrl Pts',(-1.17114106324171,5.,2.20633836739357));
#456546=CARTESIAN_POINT('Ctrl Pts',(-1.09779747805985,5.,2.25202826990409));
#456547=CARTESIAN_POINT('Ctrl Pts',(-1.02293085554802,5.,2.29866695923699));
#456548=CARTESIAN_POINT('Ctrl Pts',(-0.945709779919864,5.,2.34150710161237));
#456549=CARTESIAN_POINT('Ctrl Pts',(-0.866512657585552,5.,2.38043661881683));
#456550=CARTESIAN_POINT('Ctrl Pts',(-0.786643980132719,5.,2.41969624039592));
#456551=CARTESIAN_POINT('Ctrl Pts',(-0.70476481087952,5.,2.4549792480358));
#456552=CARTESIAN_POINT('Ctrl Pts',(-0.62122661766354,5.,2.48613272617783));
#456553=CARTESIAN_POINT('Ctrl Pts',(-0.581671214473811,5.,2.50088392369876));
#456554=CARTESIAN_POINT('Ctrl Pts',(-0.541743398700346,5.,2.51470866315734));
#456555=CARTESIAN_POINT('Ctrl Pts',(-0.501478455000533,5.,2.52758716199342));
#456556=CARTESIAN_POINT('Ctrl Pts',(-0.487863882992778,5.,2.53194170054842));
#456557=CARTESIAN_POINT('Ctrl Pts',(-0.474208668049177,5.,2.53618866564346));
#456558=CARTESIAN_POINT('Ctrl Pts',(-0.460520846856072,5.,2.54032521086352));
#456559=CARTESIAN_POINT('Ctrl Pts',(-0.372756764672366,5.,2.56684806570853));
#456560=CARTESIAN_POINT('Ctrl Pts',(-0.283926366055009,5.,2.5887539852999));
#456561=CARTESIAN_POINT('Ctrl Pts',(-0.19443424169612,5.,2.60593542971511));
#456562=CARTESIAN_POINT('Ctrl Pts',(-0.103889636373118,5.,2.62331893820371));
#456563=CARTESIAN_POINT('Ctrl Pts',(-0.0126667771947791,5.,2.63586684285107));
#456564=CARTESIAN_POINT('Ctrl Pts',(0.078848213731232,5.,2.64342534156938));
#456565=CARTESIAN_POINT('Ctrl Pts',(0.170363204657243,5.,2.65098384028769));
#456566=CARTESIAN_POINT('Ctrl Pts',(0.262171299865505,5.,2.65355352908114));
#456567=CARTESIAN_POINT('Ctrl Pts',(0.353905107892403,5.,2.65092917282106));
#456568=CARTESIAN_POINT('Ctrl Pts',(0.385670645239163,5.,2.65002041204263));
#456569=CARTESIAN_POINT('Ctrl Pts',(0.417427371319863,5.,2.64848833942243));
#456570=CARTESIAN_POINT('Ctrl Pts',(0.449163552816194,5.,2.64634223644399));
#456571=CARTESIAN_POINT('Ctrl Pts',(0.478246692955225,5.,2.64437554068124));
#456572=CARTESIAN_POINT('Ctrl Pts',(0.5073125829666,5.,2.64189317474323));
#456573=CARTESIAN_POINT('Ctrl Pts',(0.536352189258467,5.,2.63890165807019));
#456574=CARTESIAN_POINT('Ctrl Pts',(0.55146429954055,5.,2.63734488318077));
#456575=CARTESIAN_POINT('Ctrl Pts',(0.566562034763081,5.,2.63565091351987));
#456576=CARTESIAN_POINT('Ctrl Pts',(0.581636163657774,5.,2.63382211363912));
#456577=CARTESIAN_POINT('Ctrl Pts',(0.670055756250796,5.,2.62309501016801));
#456578=CARTESIAN_POINT('Ctrl Pts',(0.757746531289113,5.,2.60772452781098));
#456579=CARTESIAN_POINT('Ctrl Pts',(0.844446778749971,5.,2.58799525961142));
#456580=CARTESIAN_POINT('Ctrl Pts',(0.936346421350173,5.,2.56708283145346));
#456581=CARTESIAN_POINT('Ctrl Pts',(1.0271338627505,5.,2.54127339218079));
#456582=CARTESIAN_POINT('Ctrl Pts',(1.11650700532631,5.,2.51084568220488));
#456583=CARTESIAN_POINT('Ctrl Pts',(1.19470850508015,5.,2.48422143597595));
#456584=CARTESIAN_POINT('Ctrl Pts',(1.27182769593864,5.,2.45406024939045));
#456585=CARTESIAN_POINT('Ctrl Pts',(1.34766072047862,5.,2.42051313701281));
#456586=CARTESIAN_POINT('Ctrl Pts',(1.38722105531367,5.,2.40301238445205));
#456587=CARTESIAN_POINT('Ctrl Pts',(1.42643129580676,5.,2.38458963173364));
#456588=CARTESIAN_POINT('Ctrl Pts',(1.46526169315625,5.,2.3652629872301));
#456589=CARTESIAN_POINT('Ctrl Pts',(1.48500186360994,5.,2.35543792019914));
#456590=CARTESIAN_POINT('Ctrl Pts',(1.50464385611093,5.,2.34537921690229));
#456591=CARTESIAN_POINT('Ctrl Pts',(1.52418367742757,5.,2.33508904222946));
#456592=CARTESIAN_POINT('Ctrl Pts',(1.54114915715179,5.,2.32615458234155));
#456593=CARTESIAN_POINT('Ctrl Pts',(1.55804005009276,5.,2.31704415436288));
#456594=CARTESIAN_POINT('Ctrl Pts',(1.57483210399388,5.,2.30777138474885));
#456595=CARTESIAN_POINT('Ctrl Pts',(1.65911847268188,5.,2.26122746087573));
#456596=CARTESIAN_POINT('Ctrl Pts',(1.74102915795926,5.,2.21053931269157));
#456597=CARTESIAN_POINT('Ctrl Pts',(1.82026023750243,5.,2.15596836522314));
#456598=CARTESIAN_POINT('Ctrl Pts',(1.90298562056131,5.,2.09899069232961));
#456599=CARTESIAN_POINT('Ctrl Pts',(1.98279092512795,5.,2.03778014173156));
#456600=CARTESIAN_POINT('Ctrl Pts',(2.05931513335921,5.,1.97257685889539));
#456601=CARTESIAN_POINT('Ctrl Pts',(2.08396884136544,5.,1.95157039919793));
#456602=CARTESIAN_POINT('Ctrl Pts',(2.10828181135941,5.,1.93014909753088));
#456603=CARTESIAN_POINT('Ctrl Pts',(2.13224135383482,5.,1.90831981165407));
#456604=CARTESIAN_POINT('Ctrl Pts',(2.14963896322531,5.,1.89246903364578));
#456605=CARTESIAN_POINT('Ctrl Pts',(2.16685341904675,5.,1.8763998967844));
#456606=CARTESIAN_POINT('Ctrl Pts',(2.18385890387661,5.,1.86013529589314));
#456607=CARTESIAN_POINT('Ctrl Pts',(2.25541977559558,5.,1.79169214184112));
#456608=CARTESIAN_POINT('Ctrl Pts',(2.32334989974494,5.,1.71973196190852));
#456609=CARTESIAN_POINT('Ctrl Pts',(2.38732375899673,5.,1.64449747278477));
#456610=CARTESIAN_POINT('Ctrl Pts',(2.45052346277645,5.,1.57017340538836));
#456611=CARTESIAN_POINT('Ctrl Pts',(2.50986289761011,5.,1.49265328857437));
#456612=CARTESIAN_POINT('Ctrl Pts',(2.56500227712659,5.,1.41212817082369));
#456613=CARTESIAN_POINT('Ctrl Pts',(2.59261233427658,5.,1.37180665972577));
#456614=CARTESIAN_POINT('Ctrl Pts',(2.61916881569582,5.,1.33073106712064));
#456615=CARTESIAN_POINT('Ctrl Pts',(2.64462557919719,5.,1.2889218540532));
#456616=CARTESIAN_POINT('Ctrl Pts',(2.64767078191736,2.08166817117217E-17,
1.29195911160569));
#456617=CARTESIAN_POINT('Ctrl Pts',(2.59777293643844,-9.41002177091934E-18,
1.37498592169266));
#456618=CARTESIAN_POINT('Ctrl Pts',(2.54371157748951,-6.47715074628022E-17,
1.45513970804844));
#456619=CARTESIAN_POINT('Ctrl Pts',(2.48549620893604,0.,1.53206089300545));
#456620=CARTESIAN_POINT('Ctrl Pts',(2.42718272400871,7.79025300962201E-17,
1.60911172118088));
#456621=CARTESIAN_POINT('Ctrl Pts',(2.36470052429476,1.68964082133378E-16,
1.68291956022001));
#456622=CARTESIAN_POINT('Ctrl Pts',(2.29842841323133,1.04083408558608E-16,
1.753333246675));
#456623=CARTESIAN_POINT('Ctrl Pts',(2.22837578437846,3.55015922753236E-17,
1.82776370866335));
#456624=CARTESIAN_POINT('Ctrl Pts',(2.1540876478833,-1.73068786219787E-16,
1.89840261978313));
#456625=CARTESIAN_POINT('Ctrl Pts',(2.07598043274033,-1.38777878078145E-16,
1.96501840927444));
#456626=CARTESIAN_POINT('Ctrl Pts',(2.04180852611527,-1.23775605766176E-16,
1.99416281717689));
#456627=CARTESIAN_POINT('Ctrl Pts',(2.00690532118568,-1.61221863714727E-16,
2.02253643282966));
#456628=CARTESIAN_POINT('Ctrl Pts',(1.97130468257589,-2.0122792321331E-16,
2.05011625538801));
#456629=CARTESIAN_POINT('Ctrl Pts',(1.9466006592944,-2.28988959639827E-16,
2.06925446765574));
#456630=CARTESIAN_POINT('Ctrl Pts',(1.92156079295665,3.52147159119889E-16,
2.0880104013613));
#456631=CARTESIAN_POINT('Ctrl Pts',(1.89619633295332,3.60822483003176E-16,
2.10637570990819));
#456632=CARTESIAN_POINT('Ctrl Pts',(1.88438018844951,3.6486392053462E-16,
2.11493126912839));
#456633=CARTESIAN_POINT('Ctrl Pts',(1.87250046861909,3.5548778546167E-16,
2.12339705091612));
#456634=CARTESIAN_POINT('Ctrl Pts',(1.86056161129017,3.60822483003176E-16,
2.13177039141816));
#456635=CARTESIAN_POINT('Ctrl Pts',(1.7820029969632,3.95925209769072E-16,
2.18686762635492));
#456636=CARTESIAN_POINT('Ctrl Pts',(1.70084278960875,-6.39194753652185E-16,
2.23799746638749));
#456637=CARTESIAN_POINT('Ctrl Pts',(1.61744804048977,-5.68989300120393E-16,
2.2850133461233));
#456638=CARTESIAN_POINT('Ctrl Pts',(1.53432414409267,-4.99011862601365E-16,
2.33187652584943));
#456639=CARTESIAN_POINT('Ctrl Pts',(1.4489792272881,2.66553321917947E-16,
2.37465270447628));
#456640=CARTESIAN_POINT('Ctrl Pts',(1.36175994557255,3.7470027081099E-16,
2.41314817623965));
#456641=CARTESIAN_POINT('Ctrl Pts',(1.27604626988848,4.80980353853544E-16,
2.45097912734508));
#456642=CARTESIAN_POINT('Ctrl Pts',(1.18852150214909,2.31652411642962E-17,
2.48467602422174));
#456643=CARTESIAN_POINT('Ctrl Pts',(1.09951206593735,9.71445146547012E-17,
2.514005137696));
#456644=CARTESIAN_POINT('Ctrl Pts',(1.05865205862629,1.31104887670592E-16,
2.52746874157878));
#456645=CARTESIAN_POINT('Ctrl Pts',(1.01747923206645,3.9815101041052E-16,
2.54001121457231));
#456646=CARTESIAN_POINT('Ctrl Pts',(0.976025735328773,4.02455846426619E-16,
2.55160621007744));
#456647=CARTESIAN_POINT('Ctrl Pts',(0.957564524483282,4.04372994353883E-16,
2.55677001225624));
#456648=CARTESIAN_POINT('Ctrl Pts',(0.939047654610198,2.79685920519915E-17,
2.56174586500462));
#456649=CARTESIAN_POINT('Ctrl Pts',(0.920478007731592,2.77555756156289E-17,
2.56653128470133));
#456650=CARTESIAN_POINT('Ctrl Pts',(0.907358149967187,2.76050748891031E-17,
2.56991228737597));
#456651=CARTESIAN_POINT('Ctrl Pts',(0.894221412269896,4.16935637140537E-16,
2.5731957889532));
#456652=CARTESIAN_POINT('Ctrl Pts',(0.881069062795557,4.16333634234434E-16,
2.57638126889446));
#456653=CARTESIAN_POINT('Ctrl Pts',(0.791883790902668,4.12251489598156E-16,
2.59798181222135));
#456654=CARTESIAN_POINT('Ctrl Pts',(0.701977238002251,-8.43023025612678E-17,
2.6150803310287));
#456655=CARTESIAN_POINT('Ctrl Pts',(0.611665199798742,5.55111512312578E-17,
2.62750524997846));
#456656=CARTESIAN_POINT('Ctrl Pts',(0.523980164752349,1.91257701078017E-16,
2.6395687519792));
#456657=CARTESIAN_POINT('Ctrl Pts',(0.435912140235754,-1.98170145761692E-17,
2.64722656595151));
#456658=CARTESIAN_POINT('Ctrl Pts',(0.347753491767775,0.,2.65027380970596));
#456659=CARTESIAN_POINT('Ctrl Pts',(0.26115622397153,1.94660347906529E-17,
2.65326708362781));
#456660=CARTESIAN_POINT('Ctrl Pts',(0.174470883311766,-9.45420770462548E-17,
2.65181170424695));
#456661=CARTESIAN_POINT('Ctrl Pts',(0.0879878877595678,-2.22044604925031E-16,
2.64566633498951));
#456662=CARTESIAN_POINT('Ctrl Pts',(0.0366511445548616,-2.97730749812473E-16,
2.64201841274245));
#456663=CARTESIAN_POINT('Ctrl Pts',(-0.0146139987793563,-2.74135710604959E-16,
2.63671681157407));
#456664=CARTESIAN_POINT('Ctrl Pts',(-0.0657434791662867,-3.33066907387547E-16,
2.62978938315714));
#456665=CARTESIAN_POINT('Ctrl Pts',(-0.0799608240973768,-3.49453640550479E-16,
2.62786310425613));
#456666=CARTESIAN_POINT('Ctrl Pts',(-0.0941694681167345,1.46489281919524E-16,
2.62581081298278));
#456667=CARTESIAN_POINT('Ctrl Pts',(-0.108362279338616,1.38777878078145E-16,
2.62363393548456));
#456668=CARTESIAN_POINT('Ctrl Pts',(-0.195237834838755,9.15756373146707E-17,
2.61030906002775));
#456669=CARTESIAN_POINT('Ctrl Pts',(-0.281234873934964,-1.80842283591821E-16,
2.59236560928012));
#456670=CARTESIAN_POINT('Ctrl Pts',(-0.366067255626018,-1.11022302462516E-16,
2.57003468112992));
#456671=CARTESIAN_POINT('Ctrl Pts',(-0.452591139793857,-3.98101563526326E-17,
2.54725848880674));
#456672=CARTESIAN_POINT('Ctrl Pts',(-0.537904334660485,3.59163319751851E-16,
2.5199176109006));
#456673=CARTESIAN_POINT('Ctrl Pts',(-0.621681621332169,4.16333634234434E-16,
2.48820833141206));
#456674=CARTESIAN_POINT('Ctrl Pts',(-0.704713214603355,4.72995081362776E-16,
2.45678129310593));
#456675=CARTESIAN_POINT('Ctrl Pts',(-0.786236851551895,-7.23320616115926E-17,
2.42106258564705));
#456676=CARTESIAN_POINT('Ctrl Pts',(-0.865902984875024,-8.32667268468867E-17,
2.38120496126432));
#456677=CARTESIAN_POINT('Ctrl Pts',(-0.901639793419379,-8.81718229236015E-17,
2.36332554083581));
#456678=CARTESIAN_POINT('Ctrl Pts',(-0.937002314170247,2.77664426612253E-16,
2.34461280846694));
#456679=CARTESIAN_POINT('Ctrl Pts',(-0.971956223286635,3.05311331771918E-16,
2.32507856243581));
#456680=CARTESIAN_POINT('Ctrl Pts',(-0.992272043074096,3.21380193799183E-16,
2.31372491896403));
#456681=CARTESIAN_POINT('Ctrl Pts',(-1.01244979378511,3.7665599969535E-16,
2.30209373598401));
#456682=CARTESIAN_POINT('Ctrl Pts',(-1.03248242996565,3.88578058618805E-16,
2.29018717062679));
#456683=CARTESIAN_POINT('Ctrl Pts',(-1.04555838107585,3.96359973001472E-16,
2.28241536939711));
#456684=CARTESIAN_POINT('Ctrl Pts',(-1.05856453943241,7.49772963088282E-17,
2.2745309510009));
#456685=CARTESIAN_POINT('Ctrl Pts',(-1.07149704589891,8.32667268468867E-17,
2.26653625180142));
#456686=CARTESIAN_POINT('Ctrl Pts',(-1.14591162693116,1.30964711926809E-16,
2.22053417223948));
#456687=CARTESIAN_POINT('Ctrl Pts',(-1.21791517776447,-5.54854112154195E-17,
2.17086906248028));
#456688=CARTESIAN_POINT('Ctrl Pts',(-1.28718220994981,0.,2.11770866201185));
#456689=CARTESIAN_POINT('Ctrl Pts',(-1.35260428900227,5.24054639598309E-17,
2.06749914946049));
#456690=CARTESIAN_POINT('Ctrl Pts',(-1.41558545623252,4.02940859333988E-16,
2.01417086704383));
#456691=CARTESIAN_POINT('Ctrl Pts',(-1.47581496564193,3.33066907387547E-16,
1.95784111287787));
#456692=CARTESIAN_POINT('Ctrl Pts',(-1.49258172621148,3.1361531573717E-16,
1.94215997068854));
#456693=CARTESIAN_POINT('Ctrl Pts',(-1.50913500506103,1.49129398006594E-16,
1.92624611129061));
#456694=CARTESIAN_POINT('Ctrl Pts',(-1.5254675200324,1.66533453693773E-16,
1.91010182088324));
#456695=CARTESIAN_POINT('Ctrl Pts',(-1.54179187160703,1.83928810401539E-16,
1.8939655997933));
#456696=CARTESIAN_POINT('Ctrl Pts',(-1.5578994091293,2.07719017048048E-16,
1.87759507106596));
#456697=CARTESIAN_POINT('Ctrl Pts',(-1.57376072394509,2.22044604925031E-16,
1.86101591094124));
#456698=CARTESIAN_POINT('Ctrl Pts',(-1.63177025543134,2.74437527621558E-16,
1.80038100630439));
#456699=CARTESIAN_POINT('Ctrl Pts',(-1.6865409807442,-5.20802644289233E-17,
1.73690974699413));
#456700=CARTESIAN_POINT('Ctrl Pts',(-1.73775514238363,-1.11022302462516E-16,
1.67073873704775));
#456701=CARTESIAN_POINT('Ctrl Pts',(-1.78752738553671,-1.68304846099581E-16,
1.60643075091055));
#456702=CARTESIAN_POINT('Ctrl Pts',(-1.83394083805679,4.77778439695772E-16,
1.53957230095707));
#456703=CARTESIAN_POINT('Ctrl Pts',(-1.87665805183407,4.9960036108132E-16,
1.4702714467312));
#456704=CARTESIAN_POINT('Ctrl Pts',(-1.89552518062833,5.09238559945739E-16,
1.43966298642645));
#456705=CARTESIAN_POINT('Ctrl Pts',(-1.9136706201995,1.36541150579267E-17,
1.40857789095612));
#456706=CARTESIAN_POINT('Ctrl Pts',(-1.93106208855765,0.,1.37702479013102));
#456707=CARTESIAN_POINT('Ctrl Pts',(2.64462557919719,5.,1.2889218540532));
#456708=CARTESIAN_POINT('Ctrl Pts',(2.22149825342054,4.94775260793132,2.15709966133245));
#456709=CARTESIAN_POINT('Ctrl Pts',(1.34159137888307,4.89550521586264,2.79385497342672));
#456710=CARTESIAN_POINT('Ctrl Pts',(0.389883220425111,4.84325782379396,
2.92042352588079));
#456711=CARTESIAN_POINT('Ctrl Pts',(-0.561824938032845,4.79101043172528,
3.04699207833485));
#456712=CARTESIAN_POINT('Ctrl Pts',(-1.58533438041129,4.7387630396566,2.66337387114873));
#456713=CARTESIAN_POINT('Ctrl Pts',(-2.21881930745545,4.68651564758792,
1.93960317274112));
#456714=CARTESIAN_POINT('Ctrl Pts',(-2.85230423449962,4.63426825551924,
1.21583247433351));
#456715=CARTESIAN_POINT('Ctrl Pts',(-3.0957646462095,4.58202086345056,0.151909284704409));
#456716=CARTESIAN_POINT('Ctrl Pts',(-2.84232536874697,4.52977347138188,
-0.775883789552923));
#456717=CARTESIAN_POINT('Ctrl Pts',(-2.58888609128445,4.4775260793132,-1.70367686381026));
#456718=CARTESIAN_POINT('Ctrl Pts',(-1.83854712464952,4.42527868724452,
-2.49533982269582));
#456719=CARTESIAN_POINT('Ctrl Pts',(-0.925728817272116,4.37303129517584,
-2.79735946204562));
#456720=CARTESIAN_POINT('Ctrl Pts',(-0.629563874908174,4.35607956914709,
-2.89535007897113));
#456721=CARTESIAN_POINT('Ctrl Pts',(-0.316294968976919,4.33912784311834,
-2.94179665675882));
#456722=CARTESIAN_POINT('Ctrl Pts',(-0.00235626413880502,4.3221761170896,
-2.93955723260335));
#456723=CARTESIAN_POINT('Origin',(3.,5.,0.));
#456724=CARTESIAN_POINT('Origin',(0.,5.,0.));
#456725=CARTESIAN_POINT('',(-1.71450551880629E-16,5.,-1.4));
#456726=CARTESIAN_POINT('Origin',(0.,5.,0.));
#456727=CARTESIAN_POINT('Origin',(0.,0.,0.));
#456728=CARTESIAN_POINT('Origin',(-5.65994024385247E-16,16.9,0.));
#456729=CARTESIAN_POINT('',(2.08623127625816,16.9,-2.15132589821367));
#456730=CARTESIAN_POINT('',(-3.67394039744206E-16,16.9,-3.));
#456731=CARTESIAN_POINT('Origin',(0.,16.9,0.));
#456732=CARTESIAN_POINT('Ctrl Pts',(2.08484969764298,16.9,-2.14815125844468));
#456733=CARTESIAN_POINT('Ctrl Pts',(2.04033184400282,16.9,-2.18402695258335));
#456734=CARTESIAN_POINT('Ctrl Pts',(1.99479799836031,16.9,-2.21871156426885));
#456735=CARTESIAN_POINT('Ctrl Pts',(1.94829228233076,16.9,-2.25214199615432));
#456736=CARTESIAN_POINT('Ctrl Pts',(1.93304371715383,16.9,-2.26310336097181));
#456737=CARTESIAN_POINT('Ctrl Pts',(1.91769066004217,16.9,-2.27392984482344));
#456738=CARTESIAN_POINT('Ctrl Pts',(1.90223464967274,16.9,-2.28461908837391));
#456739=CARTESIAN_POINT('Ctrl Pts',(1.8913609280757,16.9,-2.29213926050583));
#456740=CARTESIAN_POINT('Ctrl Pts',(1.88043666951372,16.9,-2.2995911555075));
#456741=CARTESIAN_POINT('Ctrl Pts',(1.86947174693695,16.9,-2.30696784701081));
#456742=CARTESIAN_POINT('Ctrl Pts',(1.78751170222814,16.9,-2.36210676488104));
#456743=CARTESIAN_POINT('Ctrl Pts',(1.70314050175845,16.9,-2.41314579558716));
#456744=CARTESIAN_POINT('Ctrl Pts',(1.61662095764565,16.9,-2.45984009817923));
#456745=CARTESIAN_POINT('Ctrl Pts',(1.53131758125062,16.9,-2.50587803920584));
#456746=CARTESIAN_POINT('Ctrl Pts',(1.44392509555319,16.9,-2.54769287785561));
#456747=CARTESIAN_POINT('Ctrl Pts',(1.35467911748674,16.9,-2.58500289820093));
#456748=CARTESIAN_POINT('Ctrl Pts',(1.26823404221274,16.9,-2.62114197793429));
#456749=CARTESIAN_POINT('Ctrl Pts',(1.1800493652205,16.9,-2.65305469538287));
#456750=CARTESIAN_POINT('Ctrl Pts',(1.09033375493529,16.9,-2.6804373720982));
#456751=CARTESIAN_POINT('Ctrl Pts',(1.01566330819408,16.9,-2.70322801797135));
#456752=CARTESIAN_POINT('Ctrl Pts',(0.939932095011573,16.9,-2.72287985795654));
#456753=CARTESIAN_POINT('Ctrl Pts',(0.863261863496793,16.9,-2.73919020059434));
#456754=CARTESIAN_POINT('',(-2.95306835703349,16.9,-0.516208692970735));
#456755=CARTESIAN_POINT('Ctrl Pts',(-2.312781279227,16.9,-1.71040874167461));
#456756=CARTESIAN_POINT('Ctrl Pts',(-2.36394961038129,16.9,-1.65422188238401));
#456757=CARTESIAN_POINT('Ctrl Pts',(-2.41264488535713,16.9,-1.59599660500464));
#456758=CARTESIAN_POINT('Ctrl Pts',(-2.45869800638489,16.9,-1.53582544180072));
#456759=CARTESIAN_POINT('Ctrl Pts',(-2.5162098854388,16.9,-1.4606827243586));
#456760=CARTESIAN_POINT('Ctrl Pts',(-2.56960306603727,16.9,-1.38250657480199));
#456761=CARTESIAN_POINT('Ctrl Pts',(-2.61891115144116,16.9,-1.30168621892116));
#456762=CARTESIAN_POINT('Ctrl Pts',(-2.6576091123471,16.9,-1.23825680472547));
#456763=CARTESIAN_POINT('Ctrl Pts',(-2.6937902591549,16.9,-1.17319770675496));
#456764=CARTESIAN_POINT('Ctrl Pts',(-2.72745504689701,16.9,-1.10668186268529));
#456765=CARTESIAN_POINT('Ctrl Pts',(-2.73624314508487,16.9,-1.08931808860744));
#456766=CARTESIAN_POINT('Ctrl Pts',(-2.74486020807011,16.9,-1.07185368213596));
#456767=CARTESIAN_POINT('Ctrl Pts',(-2.75329837869529,16.9,-1.05430827125652));
#456768=CARTESIAN_POINT('Ctrl Pts',(-2.79594224914987,16.9,-0.965639262077881));
#456769=CARTESIAN_POINT('Ctrl Pts',(-2.83406860032868,16.9,-0.874811518173496));
#456770=CARTESIAN_POINT('Ctrl Pts',(-2.86771440442525,16.9,-0.782245644902387));
#456771=CARTESIAN_POINT('Ctrl Pts',(-2.89939603998739,16.9,-0.695083565076656));
#456772=CARTESIAN_POINT('Ctrl Pts',(-2.92710481817242,16.9,-0.606379438499839));
#456773=CARTESIAN_POINT('Ctrl Pts',(-2.95083879450907,16.9,-0.51645788495648));
#456774=CARTESIAN_POINT('Origin',(0.,16.9,0.));
#456775=CARTESIAN_POINT('Ctrl Pts',(2.5805589374942,6.77091034656191,-1.26059492705579));
#456776=CARTESIAN_POINT('Ctrl Pts',(2.16270489326978,6.82366602184023,-2.11598230427607));
#456777=CARTESIAN_POINT('Ctrl Pts',(0.416998689866887,6.92917737239689,
-3.36416092756532));
#456778=CARTESIAN_POINT('Ctrl Pts',(-2.59929056306034,7.08744439823184,
-2.18104546498594));
#456779=CARTESIAN_POINT('Ctrl Pts',(-3.24232899203514,7.24571142406682,
0.989791302620714));
#456780=CARTESIAN_POINT('Ctrl Pts',(-0.93866040260113,7.4039784499018,3.25840088127091));
#456781=CARTESIAN_POINT('Ctrl Pts',(2.22121069771714,7.56224547573676,2.5625637409689));
#456782=CARTESIAN_POINT('Ctrl Pts',(3.3586919237496,7.72051250157174,-0.465667476795367));
#456783=CARTESIAN_POINT('Ctrl Pts',(1.44022373180849,7.8787795274067,-3.06992192074064));
#456784=CARTESIAN_POINT('Ctrl Pts',(-1.78916098019484,8.03704655324167,
-2.88058449686228));
#456785=CARTESIAN_POINT('Ctrl Pts',(-3.39022251156056,8.19531357907665,
-0.0697920698937834));
#456786=CARTESIAN_POINT('Ctrl Pts',(-1.90617827987364,8.3535806049116,2.80448353848272));
#456787=CARTESIAN_POINT('Ctrl Pts',(1.31257158419998,8.5118476307466,3.12662922130667));
#456788=CARTESIAN_POINT('Ctrl Pts',(3.33683050597697,8.67011465658154,0.603461870573552));
#456789=CARTESIAN_POINT('Ctrl Pts',(2.32450679460257,8.82838168241653,-2.46886569239248));
#456790=CARTESIAN_POINT('Ctrl Pts',(-0.803177531322823,8.98664870825149,
-3.29447030739919));
#456791=CARTESIAN_POINT('Ctrl Pts',(-3.19994881461505,9.14491573408647,
-1.12202938400675));
#456792=CARTESIAN_POINT('Ctrl Pts',(-2.68469389625817,9.30318275992144,
2.07148374386093));
#456793=CARTESIAN_POINT('Ctrl Pts',(0.273695539681721,9.4614497857564,3.37989889026531));
#456794=CARTESIAN_POINT('Ctrl Pts',(2.98301528359298,9.61971681159137,1.61252745511383));
#456795=CARTESIAN_POINT('Ctrl Pts',(2.97772210058549,9.77798383742635,-1.62228130541839));
#456796=CARTESIAN_POINT('Ctrl Pts',(0.262632594907607,9.9362508632613,-3.3807764718047));
#456797=CARTESIAN_POINT('Ctrl Pts',(-2.69145861104891,10.0945178890963,
-2.06268657014607));
#456798=CARTESIAN_POINT('Ctrl Pts',(-3.19626004985765,10.2527849149312,
1.13249596744652));
#456799=CARTESIAN_POINT('Ctrl Pts',(-0.792390653220595,10.4110519407662,
3.29708089890013));
#456800=CARTESIAN_POINT('Ctrl Pts',(2.33257261886262,10.5693189666012,2.46124569460491));
#456801=CARTESIAN_POINT('Ctrl Pts',(3.33484068029608,10.7275859924362,-0.614380207850174));
#456802=CARTESIAN_POINT('Ctrl Pts',(1.30232632955009,10.8858530182711,-3.13090586417973));
#456803=CARTESIAN_POINT('Ctrl Pts',(-1.91533520282064,11.0441200441061,
-2.7982345253605));
#456804=CARTESIAN_POINT('Ctrl Pts',(-3.38999725238531,11.2023870699411,
0.0808951693976638));
#456805=CARTESIAN_POINT('Ctrl Pts',(-1.77968313098077,11.360654095776,2.88640838279897));
#456806=CARTESIAN_POINT('Ctrl Pts',(1.45018394022225,11.518921121611,3.06522298348167));
#456807=CARTESIAN_POINT('Ctrl Pts',(3.36034997176485,11.677188147446,0.454613535191446));
#456808=CARTESIAN_POINT('Ctrl Pts',(2.21251954598142,11.835455173281,-2.56970478025603));
#456809=CARTESIAN_POINT('Ctrl Pts',(-0.948755012143288,11.9937221991159,
-3.2555321110461));
#456810=CARTESIAN_POINT('Ctrl Pts',(-3.24664049163476,12.1519892249509,
-0.978749670253043));
#456811=CARTESIAN_POINT('Ctrl Pts',(-2.59000777962451,12.3102562507859,
2.18871768405023));
#456812=CARTESIAN_POINT('Ctrl Pts',(0.423592117726756,12.4685232766209,
3.36440115286681));
#456813=CARTESIAN_POINT('Ctrl Pts',(3.05171335757124,12.6267903024558,1.47840149529983));
#456814=CARTESIAN_POINT('Ctrl Pts',(2.90270462181359,12.7850573282908,-1.75297783143327));
#456815=CARTESIAN_POINT('Ctrl Pts',(0.112167317123486,12.9433243541258,
-3.38910665157133));
#456816=CARTESIAN_POINT('Ctrl Pts',(-2.78044484806947,13.1015913799607,
-1.94106976647485));
#456817=CARTESIAN_POINT('Ctrl Pts',(-3.14278767844486,13.2598584057957,
1.27338564834797));
#456818=CARTESIAN_POINT('Ctrl Pts',(-0.645120783207451,13.4181254316307,
3.32903057926365));
#456819=CARTESIAN_POINT('Ctrl Pts',(2.43962098791356,13.5763924574656,2.35518041283082));
#456820=CARTESIAN_POINT('Ctrl Pts',(3.30425105968087,13.7346594833006,-0.761938558424485));
#456821=CARTESIAN_POINT('Ctrl Pts',(1.16193595627524,13.8929265091356,-3.18567581146292));
#456822=CARTESIAN_POINT('Ctrl Pts',(-2.03776777487231,14.0511935349705,
-2.71037404638865));
#456823=CARTESIAN_POINT('Ctrl Pts',(-3.3830556511082,14.2094605608055,0.231430806858688));
#456824=CARTESIAN_POINT('Ctrl Pts',(-1.64968416256043,14.3677275866405,
2.96262862699381));
#456825=CARTESIAN_POINT('Ctrl Pts',(1.58493778894308,14.5259946124754,2.99776492739358));
#456826=CARTESIAN_POINT('Ctrl Pts',(3.37723035838085,14.6842616383104,0.304866953911748));
#456827=CARTESIAN_POINT('Ctrl Pts',(2.09616341132095,14.8425286641454,-2.66546967686099));
#456828=CARTESIAN_POINT('Ctrl Pts',(-1.09245796717358,15.0007956899804,
-3.21016193435995));
#456829=CARTESIAN_POINT('Ctrl Pts',(-3.28692286143165,15.1590627158153,
-0.833542173003866));
#456830=CARTESIAN_POINT('Ctrl Pts',(-2.49020085562839,15.3173297416503,
2.30163925299127));
#456831=CARTESIAN_POINT('Ctrl Pts',(0.572640891743325,15.4755967674853,
3.34223907283957));
#456832=CARTESIAN_POINT('Ctrl Pts',(3.11440623668499,15.6338637933202,1.34139399488469));
#456833=CARTESIAN_POINT('Ctrl Pts',(2.82191242834627,15.7921308191552,-1.88028594736362));
#456834=CARTESIAN_POINT('Ctrl Pts',(-0.0384385357557312,15.9503978449902,
-3.39060173370077));
#456835=CARTESIAN_POINT('Ctrl Pts',(-2.86409573659214,16.1086648708252,
-1.81589248079735));
#456836=CARTESIAN_POINT('Ctrl Pts',(-3.08280821480706,16.2669318966601,
1.4122865025187));
#456837=CARTESIAN_POINT('Ctrl Pts',(-0.497155858873794,16.4251989224951,
3.35338935516332));
#456838=CARTESIAN_POINT('Ctrl Pts',(2.54297493246889,16.58346594833,2.24645259117239));
#456839=CARTESIAN_POINT('Ctrl Pts',(3.26488853074936,16.741732974165,-0.912123640571359));
#456840=CARTESIAN_POINT('Ctrl Pts',(1.77123132985941,16.8472443247217,-2.45304161063505));
#456841=CARTESIAN_POINT('Ctrl Pts',(0.863261863496793,16.9,-2.73919020059434));
#456842=CARTESIAN_POINT('Ctrl Pts',(2.75127836581033,6.88060689770794,-1.34399083100445));
#456843=CARTESIAN_POINT('Ctrl Pts',(2.30578077409195,6.93336257298626,-2.25596720602134));
#456844=CARTESIAN_POINT('Ctrl Pts',(0.444585650547508,7.03887392354292,
-3.58672032040565));
#456845=CARTESIAN_POINT('Ctrl Pts',(-2.7712492005887,7.19714094937788,-2.32533468446622));
#456846=CARTESIAN_POINT('Ctrl Pts',(-3.45682847270599,7.35540797521285,
1.05527192500856));
#456847=CARTESIAN_POINT('Ctrl Pts',(-1.00075840973701,7.51367500104783,
3.47396361366696));
#456848=CARTESIAN_POINT('Ctrl Pts',(2.36815708788644,7.67194202688279,2.73209267926421));
#456849=CARTESIAN_POINT('Ctrl Pts',(3.58088950923443,7.83020905271776,-0.496474169201734));
#456850=CARTESIAN_POINT('Ctrl Pts',(1.53550315696296,7.98847607855273,-3.2730156411239));
#456851=CARTESIAN_POINT('Ctrl Pts',(-1.90752469406565,8.1467431043877,-3.07115241274106));
#456852=CARTESIAN_POINT('Ctrl Pts',(-3.6145060342613,8.30501013022267,-0.0744092332920613));
#456853=CARTESIAN_POINT('Ctrl Pts',(-2.03228338891822,8.46327715605764,
2.99001692020684));
#456854=CARTESIAN_POINT('Ctrl Pts',(1.39940605529955,8.62154418189262,3.33347446923435));
#456855=CARTESIAN_POINT('Ctrl Pts',(3.55758182775121,8.77981120772758,0.643384487359417));
#456856=CARTESIAN_POINT('Ctrl Pts',(2.4782868402065,8.93807823356255,-2.63219594363013));
#456857=CARTESIAN_POINT('Ctrl Pts',(-0.856312535135949,9.09634525939753,
-3.5124192483483));
#456858=CARTESIAN_POINT('Ctrl Pts',(-3.4116445927407,9.2546122852325,-1.19625834743339));
#456859=CARTESIAN_POINT('Ctrl Pts',(-2.86230247574601,9.41287931106746,
2.20852479933918));
#456860=CARTESIAN_POINT('Ctrl Pts',(0.29180213875536,9.57114633690244,3.60349944359066));
#456861=CARTESIAN_POINT('Ctrl Pts',(3.18035960945741,9.7294133627374,1.71920580346748));
#456862=CARTESIAN_POINT('Ctrl Pts',(3.17471625069386,9.88768038857238,-1.72960492938408));
#456863=CARTESIAN_POINT('Ctrl Pts',(0.280007313930059,10.0459474144073,
-3.60443508240459));
#456864=CARTESIAN_POINT('Ctrl Pts',(-2.86951471693306,10.2042144402423,
-2.19914563989808));
#456865=CARTESIAN_POINT('Ctrl Pts',(-3.40771179410311,10.3624814660773,
1.20741735805057));
#456866=CARTESIAN_POINT('Ctrl Pts',(-0.844812040446202,10.5207484919123,
3.51520254611148));
#456867=CARTESIAN_POINT('Ctrl Pts',(2.48688626704642,10.6790155177472,2.62407183735385));
#456868=CARTESIAN_POINT('Ctrl Pts',(3.55546036318475,10.8372825435822,-0.655025138035238));
#456869=CARTESIAN_POINT('Ctrl Pts',(1.38848301569722,10.9955495694172,-3.33803403764565));
#456870=CARTESIAN_POINT('Ctrl Pts',(-2.04204609715766,11.1538165952521,
-2.98335449744216));
#456871=CARTESIAN_POINT('Ctrl Pts',(-3.61426587284255,11.3120836210871,
0.0862468693229847));
#456872=CARTESIAN_POINT('Ctrl Pts',(-1.8974198283646,11.4703506469221,3.07736158361088));
#456873=CARTESIAN_POINT('Ctrl Pts',(1.54612229281355,11.628617672757,3.26800584102399));
#456874=CARTESIAN_POINT('Ctrl Pts',(3.5826572470557,11.786884698592,0.484688943160252));
#456875=CARTESIAN_POINT('Ctrl Pts',(2.35889096441335,11.945151724427,-2.73970614106683));
#456876=CARTESIAN_POINT('Ctrl Pts',(-1.01152083815554,12.1034187502619,
-3.47090505711113));
#456877=CARTESIAN_POINT('Ctrl Pts',(-3.46142520382508,12.2616857760969,
-1.04349982253303));
#456878=CARTESIAN_POINT('Ctrl Pts',(-2.76135230543533,12.4199528019319,
2.33351446676942));
#456879=CARTESIAN_POINT('Ctrl Pts',(0.451615273147389,12.5782198277669,
3.58697643804951));
#456880=CARTESIAN_POINT('Ctrl Pts',(3.25360247245234,12.7364868536018,1.57620660815046));
#456881=CARTESIAN_POINT('Ctrl Pts',(3.09473591643218,12.8947538794368,-1.86894781331778));
#456882=CARTESIAN_POINT('Ctrl Pts',(0.119587856905344,13.0530209052718,
-3.61331635345105));
#456883=CARTESIAN_POINT('Ctrl Pts',(-2.96438792645846,13.2112879311067,
-2.06948315631825));
#456884=CARTESIAN_POINT('Ctrl Pts',(-3.35070190508293,13.3695549569417,
1.35762773511193));
#456885=CARTESIAN_POINT('Ctrl Pts',(-0.68779938655336,13.5278219827767,
3.54926588917315));
#456886=CARTESIAN_POINT('Ctrl Pts',(2.60101652680755,13.6860890086117,2.5109897019805));
#456887=CARTESIAN_POINT('Ctrl Pts',(3.52284705596895,13.8443560344466,-0.812345357206038));
#456888=CARTESIAN_POINT('Ctrl Pts',(1.23880497845224,14.0026230602816,-3.39642734495106));
#456889=CARTESIAN_POINT('Ctrl Pts',(-2.17257831708182,14.1608900861166,
-2.88968152160239));
#456890=CARTESIAN_POINT('Ctrl Pts',(-3.6068650430687,14.3191571119515,0.246741340738604));
#456891=CARTESIAN_POINT('Ctrl Pts',(-1.7588206496379,14.4774241377865,3.15862425343142));
#456892=CARTESIAN_POINT('Ctrl Pts',(1.68979091564891,14.6356911636215,3.19608503052896));
#456893=CARTESIAN_POINT('Ctrl Pts',(3.60065437234059,14.7939581894564,0.325035728717899));
#456894=CARTESIAN_POINT('Ctrl Pts',(2.23483717460472,14.9522252152914,-2.84180645910457));
#456895=CARTESIAN_POINT('Ctrl Pts',(-1.16473060427767,15.1104922411264,
-3.42253337152165));
#456896=CARTESIAN_POINT('Ctrl Pts',(-3.50437249362942,15.2687592669614,
-0.888685979713743));
#456897=CARTESIAN_POINT('Ctrl Pts',(-2.65494255568738,15.4270262927963,
2.45390647376714));
#456898=CARTESIAN_POINT('Ctrl Pts',(0.610524516197086,15.5852933186313,
3.56334820370292));
#456899=CARTESIAN_POINT('Ctrl Pts',(3.32044286097821,15.7435603444663,1.4301352410644));
#456900=CARTESIAN_POINT('Ctrl Pts',(3.00859883551403,15.9018273703012,-2.00467812354714));
#456901=CARTESIAN_POINT('Ctrl Pts',(-0.040981475098891,16.0600943961362,
-3.61491034421719));
#456902=CARTESIAN_POINT('Ctrl Pts',(-3.05357282223019,16.2183614219712,
-1.9360246435242));
#456903=CARTESIAN_POINT('Ctrl Pts',(-3.28675444071701,16.3766284478061,
1.50571771264353));
#456904=CARTESIAN_POINT('Ctrl Pts',(-0.53004569633412,16.5348954736411,
3.57523614397983));
#456905=CARTESIAN_POINT('Ctrl Pts',(2.71120795376732,16.6931624994761,2.39506888376388));
#456906=CARTESIAN_POINT('Ctrl Pts',(3.48088046001204,16.8514295253111,-0.972466081974047));
#456907=CARTESIAN_POINT('Ctrl Pts',(1.88840888998243,16.9569408758677,-2.61532500409627));
#456908=CARTESIAN_POINT('Ctrl Pts',(0.92037180571978,17.009696551146,-2.92040403698463));
#456909=CARTESIAN_POINT('Ctrl Pts',(2.92199779412645,6.99030344885397,-1.42738673495312));
#456910=CARTESIAN_POINT('Ctrl Pts',(2.44885665491412,7.04305912413229,-2.39595210776662));
#456911=CARTESIAN_POINT('Ctrl Pts',(0.47217261122813,7.14857047468894,-3.80927971324597));
#456912=CARTESIAN_POINT('Ctrl Pts',(-2.94320783811705,7.3068375005239,-2.4696239039465));
#456913=CARTESIAN_POINT('Ctrl Pts',(-3.67132795337684,7.46510452635888,
1.12075254739641));
#456914=CARTESIAN_POINT('Ctrl Pts',(-1.06285641687289,7.62337155219385,
3.68952634606302));
#456915=CARTESIAN_POINT('Ctrl Pts',(2.51510347805574,7.78163857802882,2.90162161755951));
#456916=CARTESIAN_POINT('Ctrl Pts',(3.80308709471926,7.93990560386379,-0.5272808616081));
#456917=CARTESIAN_POINT('Ctrl Pts',(1.63078258211743,8.09817262969876,-3.47610936150716));
#456918=CARTESIAN_POINT('Ctrl Pts',(-2.02588840793647,8.25643965553374,
-3.26172032861983));
#456919=CARTESIAN_POINT('Ctrl Pts',(-3.83878955696203,8.41470668136869,
-0.07902639669034));
#456920=CARTESIAN_POINT('Ctrl Pts',(-2.15838849796279,8.57297370720367,
3.17555030193098));
#456921=CARTESIAN_POINT('Ctrl Pts',(1.48624052639912,8.73124073303864,3.54031971716202));
#456922=CARTESIAN_POINT('Ctrl Pts',(3.77833314952545,8.88950775887361,0.683307104145285));
#456923=CARTESIAN_POINT('Ctrl Pts',(2.63206688581044,9.04777478470857,-2.79552619486779));
#456924=CARTESIAN_POINT('Ctrl Pts',(-0.909447538949081,9.20604181054356,
-3.73036818929741));
#456925=CARTESIAN_POINT('Ctrl Pts',(-3.62334037086634,9.36430883637851,
-1.27048731086003));
#456926=CARTESIAN_POINT('Ctrl Pts',(-3.03991105523385,9.52257586221349,
2.34556585481744));
#456927=CARTESIAN_POINT('Ctrl Pts',(0.309908737829001,9.68084288804846,
3.82709999691602));
#456928=CARTESIAN_POINT('Ctrl Pts',(3.37770393532185,9.83910991388343,1.82588415182111));
#456929=CARTESIAN_POINT('Ctrl Pts',(3.37171040080224,9.9973769397184,-1.83692855334977));
#456930=CARTESIAN_POINT('Ctrl Pts',(0.297382032952511,10.1556439655534,
-3.82809369300449));
#456931=CARTESIAN_POINT('Ctrl Pts',(-3.04757082281721,10.3139109913884,
-2.33560470965009));
#456932=CARTESIAN_POINT('Ctrl Pts',(-3.61916353834856,10.4721780172233,
1.2823387486546));
#456933=CARTESIAN_POINT('Ctrl Pts',(-0.897233427671811,10.6304450430583,
3.73332419332284));
#456934=CARTESIAN_POINT('Ctrl Pts',(2.64119991523022,10.7887120688932,2.78689798010279));
#456935=CARTESIAN_POINT('Ctrl Pts',(3.77608004607342,10.9469790947282,-0.695670068220297));
#456936=CARTESIAN_POINT('Ctrl Pts',(1.47463970184435,11.1052461205632,-3.54516221111158));
#456937=CARTESIAN_POINT('Ctrl Pts',(-2.16875699149466,11.2635131463982,
-3.16847446952381));
#456938=CARTESIAN_POINT('Ctrl Pts',(-3.8385344932998,11.4217801722331,0.0915985692483058));
#456939=CARTESIAN_POINT('Ctrl Pts',(-2.01515652574843,11.5800471980681,
3.26831478442278));
#456940=CARTESIAN_POINT('Ctrl Pts',(1.64206064540484,11.7383142239031,3.47078869856631));
#456941=CARTESIAN_POINT('Ctrl Pts',(3.80496452234655,11.896581249738,0.514764351129056));
#456942=CARTESIAN_POINT('Ctrl Pts',(2.50526238284528,12.054848275573,-2.90970750187763));
#456943=CARTESIAN_POINT('Ctrl Pts',(-1.0742866641678,12.213115301408,-3.68627800317616));
#456944=CARTESIAN_POINT('Ctrl Pts',(-3.6762099160154,12.371382327243,-1.10824997481301));
#456945=CARTESIAN_POINT('Ctrl Pts',(-2.93269683124615,12.5296493530779,
2.47831124948861));
#456946=CARTESIAN_POINT('Ctrl Pts',(0.479638428568019,12.6879163789129,
3.8095517232322));
#456947=CARTESIAN_POINT('Ctrl Pts',(3.45549158733344,12.8461834047478,1.67401172100108));
#456948=CARTESIAN_POINT('Ctrl Pts',(3.28676721105077,13.0044504305828,-1.98491779520228));
#456949=CARTESIAN_POINT('Ctrl Pts',(0.127008396687204,13.1627174564178,
-3.83752605533076));
#456950=CARTESIAN_POINT('Ctrl Pts',(-3.14833100484746,13.3209844822528,
-2.19789654616165));
#456951=CARTESIAN_POINT('Ctrl Pts',(-3.55861613172099,13.4792515080877,
1.44186982187588));
#456952=CARTESIAN_POINT('Ctrl Pts',(-0.730477989899271,13.6375185339227,
3.76950119908265));
#456953=CARTESIAN_POINT('Ctrl Pts',(2.76241206570155,13.7957855597577,2.66679899113018));
#456954=CARTESIAN_POINT('Ctrl Pts',(3.74144305225704,13.9540525855927,-0.862752155987591));
#456955=CARTESIAN_POINT('Ctrl Pts',(1.31567400062923,14.1123196114276,-3.6071788784392));
#456956=CARTESIAN_POINT('Ctrl Pts',(-2.30738885929133,14.2705866372626,
-3.06898899681613));
#456957=CARTESIAN_POINT('Ctrl Pts',(-3.8306744350292,14.4288536630976,0.262051874618519));
#456958=CARTESIAN_POINT('Ctrl Pts',(-1.86795713671538,14.5871206889325,
3.35461987986903));
#456959=CARTESIAN_POINT('Ctrl Pts',(1.79464404235475,14.7453877147675,3.39440513366433));
#456960=CARTESIAN_POINT('Ctrl Pts',(3.82407838630033,14.9036547406025,0.345204503524049));
#456961=CARTESIAN_POINT('Ctrl Pts',(2.3735109378885,15.0619217664374,-3.01814324134815));
#456962=CARTESIAN_POINT('Ctrl Pts',(-1.23700324138176,15.2201887922724,
-3.63490480868335));
#456963=CARTESIAN_POINT('Ctrl Pts',(-3.72182212582719,15.3784558181074,
-0.943829786423622));
#456964=CARTESIAN_POINT('Ctrl Pts',(-2.81968425574637,15.5367228439423,
2.60617369454302));
#456965=CARTESIAN_POINT('Ctrl Pts',(0.648408140650847,15.6949898697773,
3.78445733456626));
#456966=CARTESIAN_POINT('Ctrl Pts',(3.52647948527143,15.8532568956123,1.51887648724411));
#456967=CARTESIAN_POINT('Ctrl Pts',(3.19528524268179,16.0115239214473,-2.12907029973066));
#456968=CARTESIAN_POINT('Ctrl Pts',(-0.0435244144420506,16.1697909472822,
-3.83921895473361));
#456969=CARTESIAN_POINT('Ctrl Pts',(-3.24304990786825,16.3280579731172,
-2.05615680625106));
#456970=CARTESIAN_POINT('Ctrl Pts',(-3.49070066662695,16.4863249989522,
1.59914892276836));
#456971=CARTESIAN_POINT('Ctrl Pts',(-0.562935533794447,16.6445920247871,
3.79708293279634));
#456972=CARTESIAN_POINT('Ctrl Pts',(2.87944097506574,16.8028590506221,2.54368517635538));
#456973=CARTESIAN_POINT('Ctrl Pts',(3.6968723892747,16.9611260764571,-1.03280852337674));
#456974=CARTESIAN_POINT('Ctrl Pts',(2.00558645010545,17.0666374270137,-2.7776083975575));
#456975=CARTESIAN_POINT('Ctrl Pts',(0.977481747942766,17.1193931022921,
-3.10161787337492));
#456976=CARTESIAN_POINT('Ctrl Pts',(3.09271722244258,7.1,-1.51078263890179));
#456977=CARTESIAN_POINT('Ctrl Pts',(2.5919325357363,7.15275567527832,-2.53593700951189));
#456978=CARTESIAN_POINT('Ctrl Pts',(0.49975957190875,7.25826702583497,-4.03183910608629));
#456979=CARTESIAN_POINT('Ctrl Pts',(-3.11516647564541,7.41653405166994,
-2.61391312342677));
#456980=CARTESIAN_POINT('Ctrl Pts',(-3.88582743404769,7.57480107750491,
1.18623316978426));
#456981=CARTESIAN_POINT('Ctrl Pts',(-1.12495442400877,7.73306810333987,
3.90508907845907));
#456982=CARTESIAN_POINT('Ctrl Pts',(2.66204986822505,7.89133512917485,3.07115055585482));
#456983=CARTESIAN_POINT('Ctrl Pts',(4.02528468020409,8.04960215500981,-0.558087554014467));
#456984=CARTESIAN_POINT('Ctrl Pts',(1.72606200727191,8.20786918084479,-3.67920308189041));
#456985=CARTESIAN_POINT('Ctrl Pts',(-2.14425212180729,8.36613620667976,
-3.45228824449861));
#456986=CARTESIAN_POINT('Ctrl Pts',(-4.06307307966276,8.52440323251473,
-0.0836435600886169));
#456987=CARTESIAN_POINT('Ctrl Pts',(-2.28449360700737,8.6826702583497,3.3610836836551));
#456988=CARTESIAN_POINT('Ctrl Pts',(1.5730749974987,8.84093728418467,3.7471649650897));
#456989=CARTESIAN_POINT('Ctrl Pts',(3.99908447129969,8.99920431001965,0.723229720931148));
#456990=CARTESIAN_POINT('Ctrl Pts',(2.78584693141438,9.1574713358546,-2.95885644610544));
#456991=CARTESIAN_POINT('Ctrl Pts',(-0.962582542762211,9.31573836168959,
-3.94831713024653));
#456992=CARTESIAN_POINT('Ctrl Pts',(-3.83503614899198,9.47400538752455,
-1.34471627428667));
#456993=CARTESIAN_POINT('Ctrl Pts',(-3.21751963472169,9.63227241335952,
2.48260691029569));
#456994=CARTESIAN_POINT('Ctrl Pts',(0.328015336902643,9.79053943919449,
4.05070055024137));
#456995=CARTESIAN_POINT('Ctrl Pts',(3.57504826118628,9.94880646502946,1.93256250017476));
#456996=CARTESIAN_POINT('Ctrl Pts',(3.56870455091062,10.1070734908644,-1.94425217731546));
#456997=CARTESIAN_POINT('Ctrl Pts',(0.31475675197496,10.2653405166994,-4.05175230360438));
#456998=CARTESIAN_POINT('Ctrl Pts',(-3.22562692870135,10.4236075425344,
-2.4720637794021));
#456999=CARTESIAN_POINT('Ctrl Pts',(-3.83061528259403,10.5818745683694,
1.35726013925865));
#457000=CARTESIAN_POINT('Ctrl Pts',(-0.949654814897419,10.7401415942043,
3.9514458405342));
#457001=CARTESIAN_POINT('Ctrl Pts',(2.79551356341402,10.8984086200393,2.94972412285173));
#457002=CARTESIAN_POINT('Ctrl Pts',(3.99669972896209,11.0566756458742,-0.736314998405361));
#457003=CARTESIAN_POINT('Ctrl Pts',(1.56079638799147,11.2149426717092,-3.7522903845775));
#457004=CARTESIAN_POINT('Ctrl Pts',(-2.29546788583168,11.3732096975442,
-3.35359444160547));
#457005=CARTESIAN_POINT('Ctrl Pts',(-4.06280311375705,11.5314767233792,
0.0969502691736263));
#457006=CARTESIAN_POINT('Ctrl Pts',(-2.13289322313227,11.6897437492141,
3.45926798523469));
#457007=CARTESIAN_POINT('Ctrl Pts',(1.73799899799614,11.8480107750491,3.67357155610862));
#457008=CARTESIAN_POINT('Ctrl Pts',(4.0272717976374,12.0062778008841,0.544839759097863));
#457009=CARTESIAN_POINT('Ctrl Pts',(2.6516338012772,12.164544826719,-3.07970886268844));
#457010=CARTESIAN_POINT('Ctrl Pts',(-1.13705249018005,12.322811852554,-3.90165094924119));
#457011=CARTESIAN_POINT('Ctrl Pts',(-3.89099462820572,12.481078878389,-1.17300012709299));
#457012=CARTESIAN_POINT('Ctrl Pts',(-3.10404135705697,12.6393459042239,
2.62310803220781));
#457013=CARTESIAN_POINT('Ctrl Pts',(0.507661583988647,12.7976129300589,
4.0321270084149));
#457014=CARTESIAN_POINT('Ctrl Pts',(3.65738070221454,12.9558799558939,1.77181683385171));
#457015=CARTESIAN_POINT('Ctrl Pts',(3.47879850566936,13.1141469817289,-2.10088777708678));
#457016=CARTESIAN_POINT('Ctrl Pts',(0.134428936469064,13.2724140075638,
-4.06173575721048));
#457017=CARTESIAN_POINT('Ctrl Pts',(-3.33227408323645,13.4306810333988,
-2.32630993600505));
#457018=CARTESIAN_POINT('Ctrl Pts',(-3.76653035835906,13.5889480592338,
1.52611190863984));
#457019=CARTESIAN_POINT('Ctrl Pts',(-0.77315659324518,13.7472150850688,
3.98973650899216));
#457020=CARTESIAN_POINT('Ctrl Pts',(2.92380760459554,13.9054821109037,2.82260828027986));
#457021=CARTESIAN_POINT('Ctrl Pts',(3.96003904854512,14.0637491367387,-0.913158954769142));
#457022=CARTESIAN_POINT('Ctrl Pts',(1.39254302280623,14.2220161625737,-3.81793041192735));
#457023=CARTESIAN_POINT('Ctrl Pts',(-2.44219940150084,14.3802831884086,
-3.24829647202987));
#457024=CARTESIAN_POINT('Ctrl Pts',(-4.0544838269897,14.5385502142436,0.277362408498434));
#457025=CARTESIAN_POINT('Ctrl Pts',(-1.97709362379286,14.6968172400786,
3.55061550630664));
#457026=CARTESIAN_POINT('Ctrl Pts',(1.89949716906058,14.8550842659136,3.59272523679971));
#457027=CARTESIAN_POINT('Ctrl Pts',(4.04750240026006,15.0133512917485,0.365373278330201));
#457028=CARTESIAN_POINT('Ctrl Pts',(2.51218470117228,15.1716183175835,-3.19448002359174));
#457029=CARTESIAN_POINT('Ctrl Pts',(-1.30927587848586,15.3298853434184,
-3.84727624584505));
#457030=CARTESIAN_POINT('Ctrl Pts',(-3.93927175802497,15.4881523692534,
-0.998973593133498));
#457031=CARTESIAN_POINT('Ctrl Pts',(-2.98442595580535,15.6464193950884,
2.7584409153189));
#457032=CARTESIAN_POINT('Ctrl Pts',(0.686291765104606,15.8046864209234,
4.0055664654296));
#457033=CARTESIAN_POINT('Ctrl Pts',(3.73251610956465,15.9629534467583,1.60761773342382));
#457034=CARTESIAN_POINT('Ctrl Pts',(3.38197164984955,16.1212204725933,-2.25346247591418));
#457035=CARTESIAN_POINT('Ctrl Pts',(-0.0460673537852081,16.2794874984283,
-4.06352756525002));
#457036=CARTESIAN_POINT('Ctrl Pts',(-3.4325269935063,16.4377545242632,-2.17628896897791));
#457037=CARTESIAN_POINT('Ctrl Pts',(-3.69464689253689,16.5960215500982,
1.6925801328932));
#457038=CARTESIAN_POINT('Ctrl Pts',(-0.595825371254773,16.7542885759332,
4.01892972161286));
#457039=CARTESIAN_POINT('Ctrl Pts',(3.04767399636416,16.9125556017682,2.69230146894688));
#457040=CARTESIAN_POINT('Ctrl Pts',(3.91286431853737,17.0708226276031,-1.09315096477943));
#457041=CARTESIAN_POINT('Ctrl Pts',(2.12276401022847,17.1763339781598,-2.93989179101872));
#457042=CARTESIAN_POINT('Ctrl Pts',(1.03459169016575,17.2290896534381,-3.28283170976521));
#457043=CARTESIAN_POINT('',(2.39254185396403,16.9,2.47449135723493));
#457044=CARTESIAN_POINT('Ctrl Pts',(2.39731517556588,16.9,2.47743591026517));
#457045=CARTESIAN_POINT('Ctrl Pts',(2.45735129193582,16.9,2.40997489184385));
#457046=CARTESIAN_POINT('Ctrl Pts',(2.51441069681728,16.9,2.34016593608869));
#457047=CARTESIAN_POINT('Ctrl Pts',(2.56829255542063,16.9,2.26807636518897));
#457048=CARTESIAN_POINT('Ctrl Pts',(2.63330364256217,16.9,2.18109678621307));
#457049=CARTESIAN_POINT('Ctrl Pts',(2.69369047677463,16.9,2.09079745741881));
#457050=CARTESIAN_POINT('Ctrl Pts',(2.74943143050006,16.9,1.99760261840811));
#457051=CARTESIAN_POINT('Ctrl Pts',(2.80611642770575,16.9,1.9028294070467));
#457052=CARTESIAN_POINT('Ctrl Pts',(2.85799705096988,16.9,1.80506084443894));
#457053=CARTESIAN_POINT('Ctrl Pts',(2.905000287014,16.9,1.70472487063112));
#457054=CARTESIAN_POINT('Ctrl Pts',(2.95127556121475,16.9,1.6059428485636));
#457055=CARTESIAN_POINT('Ctrl Pts',(2.99282330137881,16.9,1.50467138010401));
#457056=CARTESIAN_POINT('Ctrl Pts',(3.02952479600555,16.9,1.40131545622776));
#457057=CARTESIAN_POINT('Ctrl Pts',(3.03577281165996,16.9,1.38372027551583));
#457058=CARTESIAN_POINT('Ctrl Pts',(3.04188026153191,16.9,1.36606469584655));
#457059=CARTESIAN_POINT('Ctrl Pts',(3.04784641699272,16.9,1.34835073551));
#457060=CARTESIAN_POINT('Ctrl Pts',(3.05280703409911,16.9,1.33362229351004));
#457061=CARTESIAN_POINT('Ctrl Pts',(3.05766701641074,16.9,1.3188622323021));
#457062=CARTESIAN_POINT('Ctrl Pts',(3.062425668889,16.9,1.30407382307151));
#457063=CARTESIAN_POINT('Ctrl Pts',(3.09578122089829,16.9,1.20041516014575));
#457064=CARTESIAN_POINT('Ctrl Pts',(3.12417343625608,16.9,1.09533201835296));
#457065=CARTESIAN_POINT('Ctrl Pts',(3.1475702326327,16.9,0.989239984693864));
#457066=CARTESIAN_POINT('Ctrl Pts',(3.17093000708061,16.9,0.88331582580031));
#457067=CARTESIAN_POINT('Ctrl Pts',(3.18931018407837,16.9,0.776384998044518));
#457068=CARTESIAN_POINT('Ctrl Pts',(3.20262740083768,16.9,0.668856247340615));
#457069=CARTESIAN_POINT('Ctrl Pts',(3.21574256775655,16.9,0.562958931140931));
#457070=CARTESIAN_POINT('Ctrl Pts',(3.22394715946814,16.9,0.456480829259066));
#457071=CARTESIAN_POINT('Ctrl Pts',(3.22711221816567,16.9,0.349821217468776));
#457072=CARTESIAN_POINT('Ctrl Pts',(3.22862484445679,16.9,0.298847081311038));
#457073=CARTESIAN_POINT('Ctrl Pts',(3.22898570853728,16.9,0.247831699353688));
#457074=CARTESIAN_POINT('Ctrl Pts',(3.22817673574291,16.9,0.196820252878376));
#457075=CARTESIAN_POINT('Ctrl Pts',(3.22763618635905,16.9,0.162734797651577));
#457076=CARTESIAN_POINT('Ctrl Pts',(3.22657327371452,16.9,0.128651123411333));
#457077=CARTESIAN_POINT('Ctrl Pts',(3.22498195597518,16.9,0.094583064930471));
#457078=CARTESIAN_POINT('Ctrl Pts',(3.22426784467463,16.9,0.0792948638707587));
#457079=CARTESIAN_POINT('Ctrl Pts',(3.22344752043097,16.9,0.0640149857196622));
#457080=CARTESIAN_POINT('Ctrl Pts',(3.22252120818967,16.9,0.0487525626872403));
#457081=CARTESIAN_POINT('Ctrl Pts',(3.21617357369505,16.9,-0.0558345069773061));
#457082=CARTESIAN_POINT('Ctrl Pts',(3.20484788704636,16.9,-0.159716937956681));
#457083=CARTESIAN_POINT('Ctrl Pts',(3.18847069149561,16.9,-0.262520661788208));
#457084=CARTESIAN_POINT('Ctrl Pts',(3.17254566312765,16.9,-0.362486019915367));
#457085=CARTESIAN_POINT('Ctrl Pts',(3.15184400884743,16.9,-0.461432124162015));
#457086=CARTESIAN_POINT('Ctrl Pts',(3.12625233656091,16.9,-0.559000390964261));
#457087=CARTESIAN_POINT('Ctrl Pts',(3.10090297957557,16.9,-0.655644830527274));
#457088=CARTESIAN_POINT('Ctrl Pts',(3.07075571579294,16.9,-0.750938069922472));
#457089=CARTESIAN_POINT('Ctrl Pts',(3.03565640665044,16.9,-0.844506858436016));
#457090=CARTESIAN_POINT('Ctrl Pts',(3.01435271014496,16.9,-0.901298890005243));
#457091=CARTESIAN_POINT('Ctrl Pts',(2.99122368350055,16.9,-0.957455063351064));
#457092=CARTESIAN_POINT('Ctrl Pts',(2.96632347592632,16.9,-1.01291655518183));
#457093=CARTESIAN_POINT('Ctrl Pts',(2.95748571229695,16.9,-1.03260135314472));
#457094=CARTESIAN_POINT('Ctrl Pts',(2.94842479238806,16.9,-1.05219859840326));
#457095=CARTESIAN_POINT('Ctrl Pts',(2.93914302970222,16.9,-1.07170551931792));
#457096=CARTESIAN_POINT('Ctrl Pts',(2.9310199030181,16.9,-1.0887774048175));
#457097=CARTESIAN_POINT('Ctrl Pts',(2.92272610853918,16.9,-1.10578292304522));
#457098=CARTESIAN_POINT('Ctrl Pts',(2.91427468627422,16.9,-1.12269777829202));
#457099=CARTESIAN_POINT('Ctrl Pts',(2.86885951147453,16.9,-1.21359266954957));
#457100=CARTESIAN_POINT('Ctrl Pts',(2.81883571822984,16.9,-1.30200379923635));
#457101=CARTESIAN_POINT('Ctrl Pts',(2.76453606118357,16.9,-1.38770856780535));
#457102=CARTESIAN_POINT('Ctrl Pts',(2.70969650094221,16.9,-1.47426550157946));
#457103=CARTESIAN_POINT('Ctrl Pts',(2.65049488456746,16.9,-1.55806261189768));
#457104=CARTESIAN_POINT('Ctrl Pts',(2.58723209997326,16.9,-1.638836948331));
#457105=CARTESIAN_POINT('Ctrl Pts',(2.5244237260005,16.9,-1.71903109031586));
#457106=CARTESIAN_POINT('Ctrl Pts',(2.45761150944921,16.9,-1.79624623243237));
#457107=CARTESIAN_POINT('Ctrl Pts',(2.38706056192649,16.9,-1.87018374462621));
#457108=CARTESIAN_POINT('Ctrl Pts',(2.33201555442374,16.9,-1.92787100548312));
#457109=CARTESIAN_POINT('Ctrl Pts',(2.27469394955488,16.9,-1.98356231505416));
#457110=CARTESIAN_POINT('Ctrl Pts',(2.21521378714993,16.9,-2.03709518630478));
#457111=CARTESIAN_POINT('Ctrl Pts',(2.17274572791687,16.9,-2.07531695731658));
#457112=CARTESIAN_POINT('Ctrl Pts',(2.1292737737331,16.9000000000006,-2.1123511370141));
#457113=CARTESIAN_POINT('Ctrl Pts',(2.08484969764403,16.9000000000009,-2.14815125844571));
#457114=CARTESIAN_POINT('Ctrl Pts',(-0.000213030569266609,16.2776795453431,
-3.44751024702897));
#457115=CARTESIAN_POINT('Ctrl Pts',(-0.0131882280058195,16.2782821963715,
-3.4475237333034));
#457116=CARTESIAN_POINT('Ctrl Pts',(-0.0261632960604996,16.2788848473999,
-3.44745721540563));
#457117=CARTESIAN_POINT('Ctrl Pts',(-0.0391374597995815,16.2794874984283,
-3.44731028431536));
#457118=CARTESIAN_POINT('Ctrl Pts',(-1.17488723369223,16.3322431737066,
-3.43444803315932));
#457119=CARTESIAN_POINT('Ctrl Pts',(-2.30370711359927,16.3849988489849,
-2.80536850106861));
#457120=CARTESIAN_POINT('Ctrl Pts',(-2.91180370339122,16.4377545242632,
-1.84601721804475));
#457121=CARTESIAN_POINT('Ctrl Pts',(-3.51990029318317,16.4905101995416,
-0.886665935020874));
#457122=CARTESIAN_POINT('Ctrl Pts',(-3.60727359286003,16.5432658748199,
0.402957098936157));
#457123=CARTESIAN_POINT('Ctrl Pts',(-3.13448998915144,16.5960215500982,
1.43549354736796));
#457124=CARTESIAN_POINT('Ctrl Pts',(-2.66170638544285,16.6487772253765,
2.46802999579975));
#457125=CARTESIAN_POINT('Ctrl Pts',(-1.62876587834881,16.7015329006548,
3.2434798587063));
#457126=CARTESIAN_POINT('Ctrl Pts',(-0.505045730198636,16.7542885759332,
3.41010008138192));
#457127=CARTESIAN_POINT('Ctrl Pts',(0.52952772043461,16.8028590506221,3.56350202847929));
#457128=CARTESIAN_POINT('Ctrl Pts',(1.64104871889364,16.8514295253111,3.20084170308472));
#457129=CARTESIAN_POINT('Ctrl Pts',(2.39731517556588,16.9,2.47743591026517));
#457130=CARTESIAN_POINT('',(-2.33836210323076,7.1,-1.66746714335672));
#457131=CARTESIAN_POINT('Ctrl Pts',(-2.34138343307718,7.1,-1.67104082391619));
#457132=CARTESIAN_POINT('Ctrl Pts',(-2.30373709690902,7.1,-1.73710495792299));
#457133=CARTESIAN_POINT('Ctrl Pts',(-2.26340583681328,7.1,-1.8014079853077));
#457134=CARTESIAN_POINT('Ctrl Pts',(-2.22043566451384,7.1,-1.86376505338026));
#457135=CARTESIAN_POINT('Ctrl Pts',(-2.16722286282088,7.1,-1.94098592823214));
#457136=CARTESIAN_POINT('Ctrl Pts',(-2.10996506901757,7.1,-2.01522395346306));
#457137=CARTESIAN_POINT('Ctrl Pts',(-2.04905120510384,7.1,-2.08640434099551));
#457138=CARTESIAN_POINT('Ctrl Pts',(-1.98660349854121,7.1,-2.15937708756));
#457139=CARTESIAN_POINT('Ctrl Pts',(-1.92031284996429,7.1,-2.22913678539083));
#457140=CARTESIAN_POINT('Ctrl Pts',(-1.85054859855047,7.1,-2.29557990141108));
#457141=CARTESIAN_POINT('Ctrl Pts',(-1.77672045443771,7.1,-2.36589344804037));
#457142=CARTESIAN_POINT('Ctrl Pts',(-1.69900186632332,7.1,-2.4324936506496));
#457143=CARTESIAN_POINT('Ctrl Pts',(-1.61778142754668,7.1,-2.49522128635037));
#457144=CARTESIAN_POINT('Ctrl Pts',(-1.60259405024534,7.1,-2.50695070181474));
#457145=CARTESIAN_POINT('Ctrl Pts',(-1.58728087558103,7.1,-2.51854687198231));
#457146=CARTESIAN_POINT('Ctrl Pts',(-1.57186648200357,7.1,-2.52999246926519));
#457147=CARTESIAN_POINT('Ctrl Pts',(-1.49169164059863,7.1,-2.58952442180871));
#457148=CARTESIAN_POINT('Ctrl Pts',(-1.40867503025123,7.1,-2.64507039187443));
#457149=CARTESIAN_POINT('Ctrl Pts',(-1.32323616805416,7.1,-2.69654192373782));
#457150=CARTESIAN_POINT('Ctrl Pts',(-1.23618678154192,7.1,-2.74898369503879));
#457151=CARTESIAN_POINT('Ctrl Pts',(-1.14662232673984,7.1,-2.79719654281982));
#457152=CARTESIAN_POINT('Ctrl Pts',(-1.05494136675663,7.1,-2.8410556336148));
#457153=CARTESIAN_POINT('Ctrl Pts',(-0.962668701398649,7.1,-2.88519778928781));
#457154=CARTESIAN_POINT('Ctrl Pts',(-0.868251334078741,7.1,-2.92493036313033));
#457155=CARTESIAN_POINT('Ctrl Pts',(-0.772061266501809,7.1,-2.96008626738923));
#457156=CARTESIAN_POINT('Ctrl Pts',(-0.725618951099568,7.1,-2.9770601778456));
#457157=CARTESIAN_POINT('Ctrl Pts',(-0.678762960049247,7.1,-2.99296656202763));
#457158=CARTESIAN_POINT('Ctrl Pts',(-0.631533175966222,7.1,-3.00778272556646));
#457159=CARTESIAN_POINT('Ctrl Pts',(-0.610048859625699,7.1,-3.01452243760625));
#457160=CARTESIAN_POINT('Ctrl Pts',(-0.588487182318978,7.1,-3.02103651981684));
#457161=CARTESIAN_POINT('Ctrl Pts',(-0.566851836242806,7.1,-3.02732264566703));
#457162=CARTESIAN_POINT('Ctrl Pts',(-0.549634368029798,7.1,-3.03232516199506));
#457163=CARTESIAN_POINT('Ctrl Pts',(-0.532368322853267,7.1,-3.03718373790698));
#457164=CARTESIAN_POINT('Ctrl Pts',(-0.515077130872961,7.1,-3.04189155649519));
#457165=CARTESIAN_POINT('Ctrl Pts',(-0.413793396541499,7.1,-3.06946776105711));
#457166=CARTESIAN_POINT('Ctrl Pts',(-0.311489387944635,7.1,-3.09192266352597));
#457167=CARTESIAN_POINT('Ctrl Pts',(-0.208582244309945,7.1,-3.10913113842233));
#457168=CARTESIAN_POINT('Ctrl Pts',(-0.106239991649575,7.1,-3.12624515037076));
#457169=CARTESIAN_POINT('Ctrl Pts',(-0.00330032138165767,7.1,-3.13817062977676));
#457170=CARTESIAN_POINT('Ctrl Pts',(0.0998536181159393,7.1,-3.14474156889126));
#457171=CARTESIAN_POINT('Ctrl Pts',(0.195429067372106,7.1,-3.15082975574056));
#457172=CARTESIAN_POINT('Ctrl Pts',(0.29118926919932,7.1,-3.15232115511315));
#457173=CARTESIAN_POINT('Ctrl Pts',(0.386840550730246,7.1,-3.14904531704776));
#457174=CARTESIAN_POINT('Ctrl Pts',(0.454955630096398,7.1,-3.14671253105427));
#457175=CARTESIAN_POINT('Ctrl Pts',(0.523015704606009,7.1,-3.1419613991929));
#457176=CARTESIAN_POINT('Ctrl Pts',(0.590937668894151,7.1,-3.13485612111357));
#457177=CARTESIAN_POINT('Ctrl Pts',(0.610040322753848,7.1,-3.13285780335069));
#457178=CARTESIAN_POINT('Ctrl Pts',(0.629132049928093,7.1,-3.1306732129464));
#457179=CARTESIAN_POINT('Ctrl Pts',(0.648210991323371,7.1,-3.12830363025409));
#457180=CARTESIAN_POINT('Ctrl Pts',(0.662368701450295,7.1,-3.12654525885472));
#457181=CARTESIAN_POINT('Ctrl Pts',(0.67651570470214,7.1,-3.12468543554251));
#457182=CARTESIAN_POINT('Ctrl Pts',(0.690643043116382,7.1,-3.12272607557076));
#457183=CARTESIAN_POINT('Ctrl Pts',(0.791166298898776,7.1,-3.10878422482474));
#457184=CARTESIAN_POINT('Ctrl Pts',(0.890816293294953,7.1,-3.08979193939395));
#457185=CARTESIAN_POINT('Ctrl Pts',(0.989319276565167,7.1,-3.06604774520952));
#457186=CARTESIAN_POINT('Ctrl Pts',(1.09029556873711,7.1,-3.04170735865719));
#457187=CARTESIAN_POINT('Ctrl Pts',(1.19006716835258,7.1,-3.01237334165454));
#457188=CARTESIAN_POINT('Ctrl Pts',(1.28834555064191,7.1,-2.97831324493603));
#457189=CARTESIAN_POINT('Ctrl Pts',(1.38872832987599,7.1,-2.94352383255519));
#457190=CARTESIAN_POINT('Ctrl Pts',(1.48755403371945,7.1,-2.90380361678363));
#457191=CARTESIAN_POINT('Ctrl Pts',(1.58451087530088,7.1,-2.85938404168432));
#457192=CARTESIAN_POINT('Ctrl Pts',(1.66204961236623,7.1,-2.8238606304634));
#457193=CARTESIAN_POINT('Ctrl Pts',(1.73839317987524,7.1,-2.7853305896715));
#457194=CARTESIAN_POINT('Ctrl Pts',(1.81337498090191,7.1,-2.74388965300041));
#457195=CARTESIAN_POINT('Ctrl Pts',(1.83201173369785,7.1,-2.73358949373781));
#457196=CARTESIAN_POINT('Ctrl Pts',(1.85056706527456,7.1,-2.72310771383178));
#457197=CARTESIAN_POINT('Ctrl Pts',(1.86901608090916,7.1,-2.71245879056604));
#457198=CARTESIAN_POINT('Ctrl Pts',(1.96370706453454,7.1,-2.65780237753265));
#457199=CARTESIAN_POINT('Ctrl Pts',(2.05571727561232,7.1,-2.59868305315288));
#457200=CARTESIAN_POINT('Ctrl Pts',(2.14472625872352,7.1,-2.53537052888058));
#457201=CARTESIAN_POINT('Ctrl Pts',(2.23431822939319,7.1,-2.47164332271151));
#457202=CARTESIAN_POINT('Ctrl Pts',(2.32087037637371,7.1,-2.40366745534427));
#457203=CARTESIAN_POINT('Ctrl Pts',(2.40403967322767,7.1,-2.33166808527891));
#457204=CARTESIAN_POINT('Ctrl Pts',(2.44227422344943,7.1,-2.29856856857224));
#457205=CARTESIAN_POINT('Ctrl Pts',(2.47979353198495,7.1,-2.264618059125));
#457206=CARTESIAN_POINT('Ctrl Pts',(2.51656236325742,7.1,-2.22983524836611));
#457207=CARTESIAN_POINT('Ctrl Pts',(2.53389141267929,7.1,-2.21344220497005));
#457208=CARTESIAN_POINT('Ctrl Pts',(2.55105569210745,7.1,-2.19686218293923));
#457209=CARTESIAN_POINT('Ctrl Pts',(2.56803402823707,7.1,-2.1801146041988));
#457210=CARTESIAN_POINT('Ctrl Pts',(2.64761340219944,7.1,-2.10161681611318));
#457211=CARTESIAN_POINT('Ctrl Pts',(2.72319134043281,7.1,-2.01936632456138));
#457212=CARTESIAN_POINT('Ctrl Pts',(2.7944263119065,7.1,-1.93361058917696));
#457213=CARTESIAN_POINT('Ctrl Pts',(2.86463899052335,7.1,-1.84908553408765));
#457214=CARTESIAN_POINT('Ctrl Pts',(2.93063320931567,7.1,-1.76115460554111));
#457215=CARTESIAN_POINT('Ctrl Pts',(2.99205373512871,7.1,-1.67001353083844));
#457216=CARTESIAN_POINT('Ctrl Pts',(3.02712386093307,7.1,-1.61797345281149));
#457217=CARTESIAN_POINT('Ctrl Pts',(3.06070228237189,7.1,-1.56488607880856));
#457218=CARTESIAN_POINT('Ctrl Pts',(3.09271722244258,7.1,-1.51078263890179));
#457219=CARTESIAN_POINT('Ctrl Pts',(-2.34138343307717,7.1,-1.67104082391619));
#457220=CARTESIAN_POINT('Ctrl Pts',(-2.84455475580173,7.14857047468894,
-0.957347532745108));
#457221=CARTESIAN_POINT('Ctrl Pts',(-3.18141096386486,7.24989662465621,
1.04978223311021));
#457222=CARTESIAN_POINT('Ctrl Pts',(-0.93866040260113,7.4039784499018,3.25840088127091));
#457223=CARTESIAN_POINT('Ctrl Pts',(2.22121069771714,7.56224547573676,2.5625637409689));
#457224=CARTESIAN_POINT('Ctrl Pts',(3.3586919237496,7.72051250157174,-0.465667476795367));
#457225=CARTESIAN_POINT('Ctrl Pts',(1.7976392878798,7.84929397362782,-2.58474262293216));
#457226=CARTESIAN_POINT('Ctrl Pts',(0.422335728259563,7.92531977040558,
-2.86880237445628));
#457227=CARTESIAN_POINT('Ctrl Pts',(0.000911915543898995,7.94858989190502,
-2.86762206492074));
#457228=CARTESIAN_POINT('Origin',(0.,5.25141010809499,0.));
#457229=CARTESIAN_POINT('',(-2.33836210323078,7.1,1.66746714335669));
#457230=CARTESIAN_POINT('Origin',(0.,7.1,0.));
#457231=CARTESIAN_POINT('Ctrl Pts',(-2.33836210323078,7.1,1.66746714335669));
#457232=CARTESIAN_POINT('Ctrl Pts',(-1.78564062664172,7.15275567527832,
2.44257264372404));
#457233=CARTESIAN_POINT('Ctrl Pts',(0.141420484832718,7.25826702583498,
3.38695776202909));
#457234=CARTESIAN_POINT('Ctrl Pts',(2.92232820013613,7.41653405166992,1.72431918607449));
#457235=CARTESIAN_POINT('Ctrl Pts',(3.03563126175005,7.57480107750492,-1.50907675260125));
#457236=CARTESIAN_POINT('Ctrl Pts',(1.1700442784882,7.68642642964658,-2.82041444291808));
#457237=CARTESIAN_POINT('Ctrl Pts',(0.111967252847952,7.74529610650994,
-2.87593112245951));
#457238=CARTESIAN_POINT('Ctrl Pts',(0.00198847260380112,7.75141010809497,
-2.87512062938712));
#457239=CARTESIAN_POINT('Ctrl Pts',(-2.80245207497228,6.77091034656191,
1.99840595662732));
#457240=CARTESIAN_POINT('Ctrl Pts',(-2.14003309084293,6.82366602184023,
2.92734506953276));
#457241=CARTESIAN_POINT('Ctrl Pts',(0.169487920889316,6.92917737239688,
4.05916038193041));
#457242=CARTESIAN_POINT('Ctrl Pts',(3.50231673567846,7.08744439823185,2.06654130865895));
#457243=CARTESIAN_POINT('Ctrl Pts',(3.63810682553751,7.24571142406682,-1.8085801470938));
#457244=CARTESIAN_POINT('Ctrl Pts',(0.468031859858225,7.40397844990178,
-4.03685404743849));
#457245=CARTESIAN_POINT('Ctrl Pts',(-3.13048342197373,7.56224547573677,
-2.59201645208381));
#457246=CARTESIAN_POINT('Ctrl Pts',(-3.87887915070217,7.72051250157172,
1.21188621595859));
#457247=CARTESIAN_POINT('Ctrl Pts',(-1.09808361260071,7.87877952740671,
3.91280404022221));
#457248=CARTESIAN_POINT('Ctrl Pts',(2.68234612450716,8.03704655324167,3.0530522589568));
#457249=CARTESIAN_POINT('Ctrl Pts',(4.02159543523717,8.19531357907664,-0.58508579160953));
#457250=CARTESIAN_POINT('Ctrl Pts',(1.70119475466967,8.35358060491161,-3.69076252266703));
#457251=CARTESIAN_POINT('Ctrl Pts',(-2.16738208411717,8.51184763074659,
-3.43776992741298));
#457252=CARTESIAN_POINT('Ctrl Pts',(-4.06356523557141,8.67011465658154,
-0.0563216087165039));
#457253=CARTESIAN_POINT('Ctrl Pts',(-2.26182306892026,8.82838168241653,
3.37637792223869));
#457254=CARTESIAN_POINT('Ctrl Pts',(1.59823751538639,8.98664870825149,3.73649662230098));
#457255=CARTESIAN_POINT('Ctrl Pts',(4.00386126750968,9.14491573408645,0.696315939262238));
#457256=CARTESIAN_POINT('Ctrl Pts',(2.76588022140732,9.30318275992145,-2.97752802088584));
#457257=CARTESIAN_POINT('Ctrl Pts',(-0.989116986028071,9.46144978575638,
-3.94175258412388));
#457258=CARTESIAN_POINT('Ctrl Pts',(-3.84399427661538,9.61971681159139,
-1.3188907158956));
#457259=CARTESIAN_POINT('Ctrl Pts',(-3.20074783119648,9.77798383742633,
2.50419225677886));
#457260=CARTESIAN_POINT('Ctrl Pts',(0.355253556140568,9.93625086326132,
4.04840218967418));
#457261=CARTESIAN_POINT('Ctrl Pts',(3.58796589222327,10.0945178890963,1.90847216484256));
#457262=CARTESIAN_POINT('Ctrl Pts',(3.55554603797885,10.2527849149312,-1.9682118119268));
#457263=CARTESIAN_POINT('Ctrl Pts',(0.287496757183279,10.4110519407662,
-4.05377736788959));
#457264=CARTESIAN_POINT('Ctrl Pts',(-3.24218123459167,10.5693189666012,
-2.45031144180059));
#457265=CARTESIAN_POINT('Ctrl Pts',(-3.82139906738593,10.7275859924362,
1.38299475915826));
#457266=CARTESIAN_POINT('Ctrl Pts',(-0.923055063715857,10.8858530182711,
3.95774363494844));
#457267=CARTESIAN_POINT('Ctrl Pts',(2.8152904677005,11.0441200441061,2.9308539560656));
#457268=CARTESIAN_POINT('Ctrl Pts',(3.99165634033771,11.2023870699411,-0.763180838442537));
#457269=CARTESIAN_POINT('Ctrl Pts',(1.53552230930483,11.3606540957761,-3.7627033590557));
#457270=CARTESIAN_POINT('Ctrl Pts',(-2.3179726575683,11.518921121611,-3.33807850257005));
#457271=CARTESIAN_POINT('Ctrl Pts',(-4.06205871341305,11.677188147446,0.124275257374031));
#457272=CARTESIAN_POINT('Ctrl Pts',(-2.10957707260641,11.835455173281,3.47353564907578));
#457273=CARTESIAN_POINT('Ctrl Pts',(1.76266866080478,11.9937221991159,3.6617979904723));
#457274=CARTESIAN_POINT('Ctrl Pts',(4.03084500695705,12.1519892249509,0.51773918187053));
#457275=CARTESIAN_POINT('Ctrl Pts',(2.63085885380488,12.3102562507859,-3.09747429722644));
#457276=CARTESIAN_POINT('Ctrl Pts',(-1.16326991025864,12.4685232766208,
-3.89391428352127));
#457277=CARTESIAN_POINT('Ctrl Pts',(-3.89879605996908,12.6267903024558,
-1.14680190620711));
#457278=CARTESIAN_POINT('Ctrl Pts',(-3.08632731697582,12.7850573282908,
2.64392681878965));
#457279=CARTESIAN_POINT('Ctrl Pts',(0.534770909157417,12.9433243541257,
4.02862078269923));
#457280=CARTESIAN_POINT('Ctrl Pts',(3.66921519590491,13.1015913799607,1.74717634081329));
#457281=CARTESIAN_POINT('Ctrl Pts',(3.46458850694724,13.2598584057957,-2.1242391135025));
#457282=CARTESIAN_POINT('Ctrl Pts',(0.107105868234875,13.4181254316307,
-4.06254768560135));
#457283=CARTESIAN_POINT('Ctrl Pts',(-3.34784558382811,13.5763924574656,
-2.30384356990207));
#457284=CARTESIAN_POINT('Ctrl Pts',(-3.75617988553842,13.7346594833006,
1.55141163009235));
#457285=CARTESIAN_POINT('Ctrl Pts',(-0.746303276805527,13.8929265091356,
3.99484629952762));
#457286=CARTESIAN_POINT('Ctrl Pts',(2.94272654522848,14.0511935349705,2.8028780207378));
#457287=CARTESIAN_POINT('Ctrl Pts',(3.95380708902251,14.2094605608055,-0.939774094818543));
#457288=CARTESIAN_POINT('Ctrl Pts',(1.36683110091601,14.3677275866405,-3.82721037518206));
#457289=CARTESIAN_POINT('Ctrl Pts',(-2.46399228198733,14.5259946124754,
-3.23179562643458));
#457290=CARTESIAN_POINT('Ctrl Pts',(-4.05252671336466,14.6842616383104,
0.304626659242042));
#457291=CARTESIAN_POINT('Ctrl Pts',(-1.95316546723355,14.8425286641454,
3.56383446956885));
#457292=CARTESIAN_POINT('Ctrl Pts',(1.9236172112469,15.0007956899804,3.57986471419629));
#457293=CARTESIAN_POINT('Ctrl Pts',(4.04987218927447,15.1590627158153,0.338145564688239));
#457294=CARTESIAN_POINT('Ctrl Pts',(2.49063293224919,15.3173297416503,-3.2113142463538));
#457295=CARTESIAN_POINT('Ctrl Pts',(-1.33510822231294,15.4755967674853,
-3.83836439945144));
#457296=CARTESIAN_POINT('Ctrl Pts',(-3.94593125363753,15.6338637933202,
-0.972489264283366));
#457297=CARTESIAN_POINT('Ctrl Pts',(-2.96574720213873,15.7921308191552,
2.77851877993432));
#457298=CARTESIAN_POINT('Ctrl Pts',(0.713108371959378,15.9503978449902,
4.00073094771741));
#457299=CARTESIAN_POINT('Ctrl Pts',(3.74345621443102,16.1086648708251,1.58272275328413));
#457300=CARTESIAN_POINT('Ctrl Pts',(3.36632985623942,16.2669318966601,-2.27663517524305));
#457301=CARTESIAN_POINT('Ctrl Pts',(-0.0726117846316149,16.4251989224951,
-4.06220518329848));
#457302=CARTESIAN_POINT('Ctrl Pts',(-3.44861801907735,16.58346594833,-2.15495922372147));
#457303=CARTESIAN_POINT('Ctrl Pts',(-3.68007291451166,16.741732974165,1.72121251024924));
#457304=CARTESIAN_POINT('Ctrl Pts',(-1.61086821599449,16.8472443247217,
3.24872196051297));
#457305=CARTESIAN_POINT('Ctrl Pts',(-0.481137492902315,16.9,3.40820637768954));
#457306=CARTESIAN_POINT('Ctrl Pts',(-2.64775541772511,6.88060689770794,
1.88809301887045));
#457307=CARTESIAN_POINT('Ctrl Pts',(-2.02190226944253,6.93336257298626,
2.76575426092985));
#457308=CARTESIAN_POINT('Ctrl Pts',(0.160132108870451,7.03887392354293,
3.8350928419633));
#457309=CARTESIAN_POINT('Ctrl Pts',(3.30898722383101,7.19714094937786,1.95246726779747));
#457310=CARTESIAN_POINT('Ctrl Pts',(3.43728163760836,7.35540797521287,-1.70874568226295));
#457311=CARTESIAN_POINT('Ctrl Pts',(0.442196283631292,7.51367500104779,
-3.81401782750434));
#457312=CARTESIAN_POINT('Ctrl Pts',(-2.95767928188803,7.6719420268828,-2.44893593904025));
#457313=CARTESIAN_POINT('Ctrl Pts',(-3.66476321850187,7.83020905271775,
1.1449895334972));
#457314=CARTESIAN_POINT('Ctrl Pts',(-1.03746888674534,7.98847607855273,
3.69681543835056));
#457315=CARTESIAN_POINT('Ctrl Pts',(2.53427937155645,8.1467431043877,2.88452235506319));
#457316=CARTESIAN_POINT('Ctrl Pts',(3.79960149778944,8.30501013022267,-0.552788783937892));
#457317=CARTESIAN_POINT('Ctrl Pts',(1.60728801341828,8.46327715605764,-3.48703071577954));
#457318=CARTESIAN_POINT('Ctrl Pts',(-2.04774158557497,8.62154418189262,
-3.24800342938611));
#457319=CARTESIAN_POINT('Ctrl Pts',(-3.83925454563574,8.77981120772757,
-0.05321262973447));
#457320=CARTESIAN_POINT('Ctrl Pts',(-2.1369693841164,8.93807823356256,3.19000029143528));
#457321=CARTESIAN_POINT('Ctrl Pts',(1.51001406160273,9.09634525939752,3.53024027185438));
#457322=CARTESIAN_POINT('Ctrl Pts',(3.78284626436418,9.25461228523249,0.657878975735262));
#457323=CARTESIAN_POINT('Ctrl Pts',(2.61320234747722,9.41287931106747,-2.8131670900409));
#457324=CARTESIAN_POINT('Ctrl Pts',(-0.934517268612236,9.57114633690243,
-3.72416600917225));
#457325=CARTESIAN_POINT('Ctrl Pts',(-3.63180400568077,9.7294133627374,-1.24608733529705));
#457326=CARTESIAN_POINT('Ctrl Pts',(-3.02406506305954,9.88768038857237,
2.36595968014087));
#457327=CARTESIAN_POINT('Ctrl Pts',(0.335643394703413,10.0459474144073,
3.82492850692052));
#457328=CARTESIAN_POINT('Ctrl Pts',(3.38990850712089,10.2042144402423,1.80312361419755));
#457329=CARTESIAN_POINT('Ctrl Pts',(3.35927824390098,10.3624814660773,-1.85956560499302));
#457330=CARTESIAN_POINT('Ctrl Pts',(0.271626802545034,10.5207484919123,
-3.83000697279982));
#457331=CARTESIAN_POINT('Ctrl Pts',(-3.06321132332717,10.6790155177472,
-2.31505311119566));
#457332=CARTESIAN_POINT('Ctrl Pts',(-3.61045606250408,10.8372825435822,
1.30665280557312));
#457333=CARTESIAN_POINT('Ctrl Pts',(-0.872101995120261,10.9955495694172,
3.73927434655792));
#457334=CARTESIAN_POINT('Ctrl Pts',(2.65988512520687,11.1538165952521,2.76906945529497));
#457335=CARTESIAN_POINT('Ctrl Pts',(3.77131505484551,11.3120836210871,-0.72105290139894));
#457336=CARTESIAN_POINT('Ctrl Pts',(1.45076076404976,11.4703506469221,-3.55500038455815));
#457337=CARTESIAN_POINT('Ctrl Pts',(-2.19001948937017,11.6286176727571,
-3.15381501753567));
#457338=CARTESIAN_POINT('Ctrl Pts',(-3.83783118420082,11.786884698592,0.11741520539813));
#457339=CARTESIAN_POINT('Ctrl Pts',(-1.99312743757002,11.945151724427,3.28179486658758));
#457340=CARTESIAN_POINT('Ctrl Pts',(1.66536853135885,12.1034187502619,3.459665039226));
#457341=CARTESIAN_POINT('Ctrl Pts',(3.80834048885077,12.2616857760969,0.489159738362271));
#457342=CARTESIAN_POINT('Ctrl Pts',(2.48563422213058,12.4199528019319,-2.92649227617094));
#457343=CARTESIAN_POINT('Ctrl Pts',(-1.09905687047098,12.5782198277669,
-3.67896840500034));
#457344=CARTESIAN_POINT('Ctrl Pts',(-3.68358070511896,12.7364868536018,
-1.08349790789817));
#457345=CARTESIAN_POINT('Ctrl Pts',(-2.91596061441178,12.8947538794368,
2.49798082937362));
#457346=CARTESIAN_POINT('Ctrl Pts',(0.505251306385807,13.0530209052718,
3.80623904280589));
#457347=CARTESIAN_POINT('Ctrl Pts',(3.46667281147088,13.2112879311067,1.65073139463242));
#457348=CARTESIAN_POINT('Ctrl Pts',(3.27334161086357,13.3695549569417,-2.00698012699307));
#457349=CARTESIAN_POINT('Ctrl Pts',(0.101193574520564,13.5278219827767,
-3.83829316489704));
#457350=CARTESIAN_POINT('Ctrl Pts',(-3.16304295136811,13.6860890086117,
-2.17667033391095));
#457351=CARTESIAN_POINT('Ctrl Pts',(-3.54883700981142,13.8443560344466,
1.46577298694374));
#457352=CARTESIAN_POINT('Ctrl Pts',(-0.705106989009746,14.0026230602816,
3.7743289268053));
#457353=CARTESIAN_POINT('Ctrl Pts',(2.78028667201715,14.1608900861166,2.64815785108637));
#457354=CARTESIAN_POINT('Ctrl Pts',(3.73555509979697,14.3191571119515,-0.887898127934317));
#457355=CARTESIAN_POINT('Ctrl Pts',(1.29138138877944,14.4774241377865,-3.61594658340851));
#457356=CARTESIAN_POINT('Ctrl Pts',(-2.32797876264463,14.6356911636215,
-3.05339900556805));
#457357=CARTESIAN_POINT('Ctrl Pts',(-3.82882535498602,14.7939581894564,
0.287811126047398));
#457358=CARTESIAN_POINT('Ctrl Pts',(-1.84534982552105,14.9522252152914,
3.36710915021439));
#457359=CARTESIAN_POINT('Ctrl Pts',(1.81743264700028,15.1104922411264,3.38225451788678));
#457360=CARTESIAN_POINT('Ctrl Pts',(3.82631736185955,15.2687592669614,0.319479772331821));
#457361=CARTESIAN_POINT('Ctrl Pts',(2.35314883662822,15.4270262927963,-3.03404820718843));
#457362=CARTESIAN_POINT('Ctrl Pts',(-1.26140962782153,15.5852933186313,
-3.6264849003533));
#457363=CARTESIAN_POINT('Ctrl Pts',(-3.7281140141863,15.7435603444663,-0.918807404837155));
#457364=CARTESIAN_POINT('Ctrl Pts',(-2.80203657796488,15.9018273703012,
2.62514325169856));
#457365=CARTESIAN_POINT('Ctrl Pts',(0.67374445834164,16.0600943961362,3.77988873967954));
#457366=CARTESIAN_POINT('Ctrl Pts',(3.53681569126371,16.2183614219712,1.49535572158047));
#457367=CARTESIAN_POINT('Ctrl Pts',(3.18050688334997,16.3766284478062,-2.15096385528484));
#457368=CARTESIAN_POINT('Ctrl Pts',(-0.0686035803666589,16.5348954736411,
-3.8379695688805));
#457369=CARTESIAN_POINT('Ctrl Pts',(-3.25825270134793,16.6931624994761,
-2.03600447284782));
#457370=CARTESIAN_POINT('Ctrl Pts',(-3.47693117896336,16.851429525311,1.62620077958471));
#457371=CARTESIAN_POINT('Ctrl Pts',(-1.52194754166591,16.9569408758677,
3.06939099813719));
#457372=CARTESIAN_POINT('Ctrl Pts',(-0.454578479639251,17.009696551146,
3.22007180134991));
#457373=CARTESIAN_POINT('Ctrl Pts',(-2.49305876047795,6.99030344885397,
1.77778008111357));
#457374=CARTESIAN_POINT('Ctrl Pts',(-1.90377144804213,7.04305912413229,
2.60416345232695));
#457375=CARTESIAN_POINT('Ctrl Pts',(0.150776296851584,7.14857047468894,
3.6110253019962));
#457376=CARTESIAN_POINT('Ctrl Pts',(3.11565771198357,7.3068375005239,1.83839322693598));
#457377=CARTESIAN_POINT('Ctrl Pts',(3.2364564496792,7.46510452635889,-1.6089112174321));
#457378=CARTESIAN_POINT('Ctrl Pts',(0.416360707404361,7.62337155219384,
-3.59118160757021));
#457379=CARTESIAN_POINT('Ctrl Pts',(-2.78487514180233,7.78163857802882,
-2.30585542599669));
#457380=CARTESIAN_POINT('Ctrl Pts',(-3.45064728630157,7.93990560386378,
1.07809285103581));
#457381=CARTESIAN_POINT('Ctrl Pts',(-0.976854160889977,8.09817262969876,
3.48082683647892));
#457382=CARTESIAN_POINT('Ctrl Pts',(2.38621261860575,8.25643965553374,2.71599245116957));
#457383=CARTESIAN_POINT('Ctrl Pts',(3.57760756034172,8.41470668136869,-0.520491776266254));
#457384=CARTESIAN_POINT('Ctrl Pts',(1.51338127216689,8.57297370720367,-3.28329890889206));
#457385=CARTESIAN_POINT('Ctrl Pts',(-1.92810108703277,8.73124073303864,
-3.05823693135924));
#457386=CARTESIAN_POINT('Ctrl Pts',(-3.61494385570008,8.8895077588736,-0.0501036507524327));
#457387=CARTESIAN_POINT('Ctrl Pts',(-2.01211569931255,9.04777478470859,
3.00362266063187));
#457388=CARTESIAN_POINT('Ctrl Pts',(1.42179060781906,9.20604181054354,3.32398392140778));
#457389=CARTESIAN_POINT('Ctrl Pts',(3.56183126121867,9.36430883637851,0.619442012208283));
#457390=CARTESIAN_POINT('Ctrl Pts',(2.46052447354711,9.5225758622135,-2.64880615919596));
#457391=CARTESIAN_POINT('Ctrl Pts',(-0.879917551196401,9.68084288804845,
-3.50657943422061));
#457392=CARTESIAN_POINT('Ctrl Pts',(-3.41961373474617,9.83910991388344,
-1.1732839546985));
#457393=CARTESIAN_POINT('Ctrl Pts',(-2.8473822949226,9.99737693971839,2.22772710350288));
#457394=CARTESIAN_POINT('Ctrl Pts',(0.316033233266263,10.1556439655534,
3.60145482416686));
#457395=CARTESIAN_POINT('Ctrl Pts',(3.19185112201851,10.3139109913883,1.69777506355255));
#457396=CARTESIAN_POINT('Ctrl Pts',(3.16301044982312,10.4721780172233,-1.75091939805924));
#457397=CARTESIAN_POINT('Ctrl Pts',(0.255756847906782,10.6304450430583,
-3.60623657771004));
#457398=CARTESIAN_POINT('Ctrl Pts',(-2.88424141206268,10.7887120688932,
-2.17979478059074));
#457399=CARTESIAN_POINT('Ctrl Pts',(-3.39951305762222,10.9469790947282,
1.23031085198798));
#457400=CARTESIAN_POINT('Ctrl Pts',(-0.821148926524665,11.1052461205632,
3.52080505816739));
#457401=CARTESIAN_POINT('Ctrl Pts',(2.50447978271324,11.2635131463982,2.60728495452435));
#457402=CARTESIAN_POINT('Ctrl Pts',(3.5509737693533,11.4217801722331,-0.678924964355346));
#457403=CARTESIAN_POINT('Ctrl Pts',(1.36599921879469,11.5800471980681,-3.3472974100606));
#457404=CARTESIAN_POINT('Ctrl Pts',(-2.06206632117205,11.7383142239031,
-2.96955153250129));
#457405=CARTESIAN_POINT('Ctrl Pts',(-3.6136036549886,11.896581249738,0.110555153422237));
#457406=CARTESIAN_POINT('Ctrl Pts',(-1.87667780253363,12.054848275573,3.09005408409938));
#457407=CARTESIAN_POINT('Ctrl Pts',(1.56806840191293,12.213115301408,3.25753208797971));
#457408=CARTESIAN_POINT('Ctrl Pts',(3.58583597074448,12.371382327243,0.460580294854009));
#457409=CARTESIAN_POINT('Ctrl Pts',(2.34040959045628,12.5296493530779,-2.75551025511545));
#457410=CARTESIAN_POINT('Ctrl Pts',(-1.03484383068333,12.6879163789129,
-3.4640225264794));
#457411=CARTESIAN_POINT('Ctrl Pts',(-3.46836535026884,12.8461834047479,
-1.02019390958923));
#457412=CARTESIAN_POINT('Ctrl Pts',(-2.74559391184774,13.0044504305828,
2.35203483995757));
#457413=CARTESIAN_POINT('Ctrl Pts',(0.4757317036142,13.1627174564178,3.58385730291256));
#457414=CARTESIAN_POINT('Ctrl Pts',(3.26413042703685,13.3209844822528,1.55428644845155));
#457415=CARTESIAN_POINT('Ctrl Pts',(3.0820947147799,13.4792515080877,-1.88972114048365));
#457416=CARTESIAN_POINT('Ctrl Pts',(0.0952812808062532,13.6375185339227,
-3.61403864419272));
#457417=CARTESIAN_POINT('Ctrl Pts',(-2.97824031890811,13.7957855597577,
-2.04949709791984));
#457418=CARTESIAN_POINT('Ctrl Pts',(-3.34149413408443,13.9540525855927,
1.38013434379513));
#457419=CARTESIAN_POINT('Ctrl Pts',(-0.663910701213964,14.1123196114276,
3.55381155408297));
#457420=CARTESIAN_POINT('Ctrl Pts',(2.61784679880582,14.2705866372626,2.49343768143495));
#457421=CARTESIAN_POINT('Ctrl Pts',(3.51730311057144,14.4288536630976,-0.8360221610501));
#457422=CARTESIAN_POINT('Ctrl Pts',(1.21593167664287,14.5871206889325,-3.40468279163495));
#457423=CARTESIAN_POINT('Ctrl Pts',(-2.19196524330193,14.7453877147675,
-2.87500238470152));
#457424=CARTESIAN_POINT('Ctrl Pts',(-3.60512399660737,14.9036547406025,
0.270995592852758));
#457425=CARTESIAN_POINT('Ctrl Pts',(-1.73753418380856,15.0619217664374,
3.17038383085992));
#457426=CARTESIAN_POINT('Ctrl Pts',(1.71124808275365,15.2201887922724,3.18464432157728));
#457427=CARTESIAN_POINT('Ctrl Pts',(3.60276253444463,15.3784558181074,0.300813979975401));
#457428=CARTESIAN_POINT('Ctrl Pts',(2.21566474100726,15.5367228439424,-2.85678216802306));
#457429=CARTESIAN_POINT('Ctrl Pts',(-1.18771103333013,15.6949898697773,
-3.41460540125516));
#457430=CARTESIAN_POINT('Ctrl Pts',(-3.51029677473507,15.8532568956123,
-0.865125545390938));
#457431=CARTESIAN_POINT('Ctrl Pts',(-2.63832595379104,16.0115239214473,
2.47176772346279));
#457432=CARTESIAN_POINT('Ctrl Pts',(0.634380544723908,16.1697909472822,
3.55904653164168));
#457433=CARTESIAN_POINT('Ctrl Pts',(3.3301751680964,16.3280579731172,1.4079886898768));
#457434=CARTESIAN_POINT('Ctrl Pts',(2.99468391046051,16.4863249989522,-2.02529253532663));
#457435=CARTESIAN_POINT('Ctrl Pts',(-0.0645953761017088,16.6445920247872,
-3.61373395446251));
#457436=CARTESIAN_POINT('Ctrl Pts',(-3.0678873836185,16.8028590506221,-1.91704972197417));
#457437=CARTESIAN_POINT('Ctrl Pts',(-3.27378944341507,16.9611260764571,
1.53118904892018));
#457438=CARTESIAN_POINT('Ctrl Pts',(-1.43302686733732,17.0666374270137,
2.8900600357614));
#457439=CARTESIAN_POINT('Ctrl Pts',(-0.428019466376186,17.1193931022921,
3.03193722501028));
#457440=CARTESIAN_POINT('Ctrl Pts',(-2.33836210323078,7.1,1.66746714335669));
#457441=CARTESIAN_POINT('Ctrl Pts',(-1.78564062664172,7.15275567527832,
2.44257264372404));
#457442=CARTESIAN_POINT('Ctrl Pts',(0.141420484832718,7.25826702583498,
3.38695776202909));
#457443=CARTESIAN_POINT('Ctrl Pts',(2.92232820013613,7.41653405166992,1.72431918607449));
#457444=CARTESIAN_POINT('Ctrl Pts',(3.03563126175005,7.57480107750492,-1.50907675260125));
#457445=CARTESIAN_POINT('Ctrl Pts',(0.390525131177429,7.73306810333986,
-3.36834538763607));
#457446=CARTESIAN_POINT('Ctrl Pts',(-2.61207100171662,7.89133512917486,
-2.16277491295312));
#457447=CARTESIAN_POINT('Ctrl Pts',(-3.23653135410128,8.0496021550098,1.01119616857442));
#457448=CARTESIAN_POINT('Ctrl Pts',(-0.91623943503461,8.2078691808448,3.26483823460727));
#457449=CARTESIAN_POINT('Ctrl Pts',(2.23814586565504,8.36613620667974,2.54746254727596));
#457450=CARTESIAN_POINT('Ctrl Pts',(3.355613622894,8.52440323251474,-0.488194768594614));
#457451=CARTESIAN_POINT('Ctrl Pts',(1.41947453091551,8.68267025834969,-3.07956710200458));
#457452=CARTESIAN_POINT('Ctrl Pts',(-1.80846058849058,8.84093728418467,
-2.86847043333237));
#457453=CARTESIAN_POINT('Ctrl Pts',(-3.39063316576441,8.99920431001964,
-0.0469946717703988));
#457454=CARTESIAN_POINT('Ctrl Pts',(-1.88726201450869,9.1574713358546,2.81724502982847));
#457455=CARTESIAN_POINT('Ctrl Pts',(1.33356715403539,9.31573836168959,3.11772757096118));
#457456=CARTESIAN_POINT('Ctrl Pts',(3.34081625807316,9.47400538752454,0.581005048681307));
#457457=CARTESIAN_POINT('Ctrl Pts',(2.30784659961701,9.63227241335953,-2.48444522835102));
#457458=CARTESIAN_POINT('Ctrl Pts',(-0.825317833780566,9.79053943919448,
-3.28899285926896));
#457459=CARTESIAN_POINT('Ctrl Pts',(-3.20742346381156,9.94880646502946,
-1.10048057409996));
#457460=CARTESIAN_POINT('Ctrl Pts',(-2.67069952678566,10.1070734908644,
2.08949452686489));
#457461=CARTESIAN_POINT('Ctrl Pts',(0.29642307182911,10.2653405166994,3.3779811414132));
#457462=CARTESIAN_POINT('Ctrl Pts',(2.99379373691612,10.4236075425344,1.59242651290754));
#457463=CARTESIAN_POINT('Ctrl Pts',(2.96674265574526,10.5818745683693,-1.64227319112547));
#457464=CARTESIAN_POINT('Ctrl Pts',(0.239886893268533,10.7401415942043,
-3.38246618262026));
#457465=CARTESIAN_POINT('Ctrl Pts',(-2.70527150079818,10.8984086200393,
-2.04453644998582));
#457466=CARTESIAN_POINT('Ctrl Pts',(-3.18857005274037,11.0566756458742,
1.15396889840285));
#457467=CARTESIAN_POINT('Ctrl Pts',(-0.770195857929068,11.2149426717092,
3.30233576977685));
#457468=CARTESIAN_POINT('Ctrl Pts',(2.34907444021962,11.3732096975442,2.44550045375373));
#457469=CARTESIAN_POINT('Ctrl Pts',(3.33063248386109,11.5314767233792,-0.636797027311755));
#457470=CARTESIAN_POINT('Ctrl Pts',(1.28123767353962,11.6897437492141,-3.13959443556305));
#457471=CARTESIAN_POINT('Ctrl Pts',(-1.93411315297392,11.8480107750491,
-2.78528804746691));
#457472=CARTESIAN_POINT('Ctrl Pts',(-3.38937612577637,12.0062778008841,
0.103695101446341));
#457473=CARTESIAN_POINT('Ctrl Pts',(-1.76022816749725,12.164544826719,2.89831330161118));
#457474=CARTESIAN_POINT('Ctrl Pts',(1.470768272467,12.322811852554,3.05539913673341));
#457475=CARTESIAN_POINT('Ctrl Pts',(3.36333145263819,12.481078878389,0.432000851345749));
#457476=CARTESIAN_POINT('Ctrl Pts',(2.19518495878197,12.6393459042239,-2.58452823405996));
#457477=CARTESIAN_POINT('Ctrl Pts',(-0.970630790895669,12.7976129300589,
-3.24907664795847));
#457478=CARTESIAN_POINT('Ctrl Pts',(-3.25314999541872,12.9558799558939,
-0.956889911280283));
#457479=CARTESIAN_POINT('Ctrl Pts',(-2.5752272092837,13.1141469817289,2.20608885054153));
#457480=CARTESIAN_POINT('Ctrl Pts',(0.446212100842591,13.2724140075638,
3.36147556301922));
#457481=CARTESIAN_POINT('Ctrl Pts',(3.06158804260283,13.4306810333988,1.45784150227068));
#457482=CARTESIAN_POINT('Ctrl Pts',(2.89084781869623,13.5889480592338,-1.77246215397422));
#457483=CARTESIAN_POINT('Ctrl Pts',(0.0893689870919405,13.7472150850687,
-3.3897841234884));
#457484=CARTESIAN_POINT('Ctrl Pts',(-2.7934376864481,13.9054821109037,-1.92232386192872));
#457485=CARTESIAN_POINT('Ctrl Pts',(-3.13415125835744,14.0637491367387,
1.29449570064652));
#457486=CARTESIAN_POINT('Ctrl Pts',(-0.622714413418182,14.2220161625736,
3.33329418136064));
#457487=CARTESIAN_POINT('Ctrl Pts',(2.4554069255945,14.3802831884086,2.33871751178352));
#457488=CARTESIAN_POINT('Ctrl Pts',(3.29905112134591,14.5385502142436,-0.784146194165878));
#457489=CARTESIAN_POINT('Ctrl Pts',(1.1404819645063,14.6968172400786,-3.19341899986139));
#457490=CARTESIAN_POINT('Ctrl Pts',(-2.05595172395924,14.8550842659135,
-2.696605763835));
#457491=CARTESIAN_POINT('Ctrl Pts',(-3.38142263822873,15.0133512917485,
0.254180059658117));
#457492=CARTESIAN_POINT('Ctrl Pts',(-1.62971854209606,15.1716183175835,
2.97365851150546));
#457493=CARTESIAN_POINT('Ctrl Pts',(1.60506351850703,15.3298853434185,2.98703412526777));
#457494=CARTESIAN_POINT('Ctrl Pts',(3.37920770702971,15.4881523692534,0.282148187618979));
#457495=CARTESIAN_POINT('Ctrl Pts',(2.07818064538629,15.6464193950884,-2.67951612885769));
#457496=CARTESIAN_POINT('Ctrl Pts',(-1.11401243883872,15.8046864209233,
-3.20272590215703));
#457497=CARTESIAN_POINT('Ctrl Pts',(-3.29247953528384,15.9629534467583,
-0.811443685944723));
#457498=CARTESIAN_POINT('Ctrl Pts',(-2.47461532961719,16.1212204725933,
2.31839219522703));
#457499=CARTESIAN_POINT('Ctrl Pts',(0.595016631106169,16.2794874984283,
3.33820432360382));
#457500=CARTESIAN_POINT('Ctrl Pts',(3.12353464492909,16.4377545242632,1.32062165817314));
#457501=CARTESIAN_POINT('Ctrl Pts',(2.80886093757105,16.5960215500982,-1.89962121536842));
#457502=CARTESIAN_POINT('Ctrl Pts',(-0.0605871718367519,16.7542885759332,
-3.38949834004452));
#457503=CARTESIAN_POINT('Ctrl Pts',(-2.87752206588908,16.9125556017681,
-1.79809497110052));
#457504=CARTESIAN_POINT('Ctrl Pts',(-3.07064770786678,17.0708226276031,
1.43617731825564));
#457505=CARTESIAN_POINT('Ctrl Pts',(-1.34410619300874,17.1763339781598,
2.71072907338562));
#457506=CARTESIAN_POINT('Ctrl Pts',(-0.401460453113122,17.2290896534381,
2.84380264867065));
#457507=CARTESIAN_POINT('Ctrl Pts',(3.09699338763788,7.1,1.51441171489139));
#457508=CARTESIAN_POINT('Ctrl Pts',(3.05138631168995,7.1,1.59235606784553));
#457509=CARTESIAN_POINT('Ctrl Pts',(3.00262634822843,7.1,1.66819495986494));
#457510=CARTESIAN_POINT('Ctrl Pts',(2.9507154613905,7.1,1.74171658295999));
#457511=CARTESIAN_POINT('Ctrl Pts',(2.88808245753381,7.1,1.83042398873481));
#457512=CARTESIAN_POINT('Ctrl Pts',(2.82086319276517,7.1,1.91575934092478));
#457513=CARTESIAN_POINT('Ctrl Pts',(2.74945446377628,7.1,1.99757097072423));
#457514=CARTESIAN_POINT('Ctrl Pts',(2.67683632715039,7.1,2.08076819597225));
#457515=CARTESIAN_POINT('Ctrl Pts',(2.59988479291176,7.1,2.16032181447893));
#457516=CARTESIAN_POINT('Ctrl Pts',(2.51898429832516,7.1,2.23603014307834));
#457517=CARTESIAN_POINT('Ctrl Pts',(2.43933674623876,7.1,2.31056594259736));
#457518=CARTESIAN_POINT('Ctrl Pts',(2.35586069002669,7.1,2.38137487814425));
#457519=CARTESIAN_POINT('Ctrl Pts',(2.26890461941283,7.1,2.4482188967034));
#457520=CARTESIAN_POINT('Ctrl Pts',(2.25410139539327,7.1,2.45959828602163));
#457521=CARTESIAN_POINT('Ctrl Pts',(2.2391972920332,7.1,2.47086265479881));
#457522=CARTESIAN_POINT('Ctrl Pts',(2.22419400368059,7.1,2.48201068638687));
#457523=CARTESIAN_POINT('Ctrl Pts',(2.21171926433338,7.1,2.49127990690887));
#457524=CARTESIAN_POINT('Ctrl Pts',(2.19918335459787,7.1,2.50046318838471));
#457525=CARTESIAN_POINT('Ctrl Pts',(2.18658917112344,7.1,2.50955885869257));
#457526=CARTESIAN_POINT('Ctrl Pts',(2.09831122456602,7.1,2.5733142501375));
#457527=CARTESIAN_POINT('Ctrl Pts',(2.00714475761466,7.1,2.63278941917963));
#457528=CARTESIAN_POINT('Ctrl Pts',(1.91347510734792,7.1,2.68782542766927));
#457529=CARTESIAN_POINT('Ctrl Pts',(1.81995369108995,7.1,2.7427743406254));
#457530=CARTESIAN_POINT('Ctrl Pts',(1.72393609567924,7.1,2.79329845475051));
#457531=CARTESIAN_POINT('Ctrl Pts',(1.62578530520389,7.1,2.83919217540819));
#457532=CARTESIAN_POINT('Ctrl Pts',(1.52912370021484,7.1,2.88438957704099));
#457533=CARTESIAN_POINT('Ctrl Pts',(1.43039228956228,7.1,2.92509621946273));
#457534=CARTESIAN_POINT('Ctrl Pts',(1.32993096063056,7.1,2.96106607137733));
#457535=CARTESIAN_POINT('Ctrl Pts',(1.28191903464677,7.1,2.97825658524108));
#457536=CARTESIAN_POINT('Ctrl Pts',(1.23351196898821,7.1,2.99436445226978));
#457537=CARTESIAN_POINT('Ctrl Pts',(1.18474714873503,7.1,3.00935852034605));
#457538=CARTESIAN_POINT('Ctrl Pts',(1.15216287588125,7.1,3.01937743978118));
#457539=CARTESIAN_POINT('Ctrl Pts',(1.11941887866099,7.1,3.02889901118082));
#457540=CARTESIAN_POINT('Ctrl Pts',(1.08652644784596,7.1,3.03791321314893));
#457541=CARTESIAN_POINT('Ctrl Pts',(1.07176586969083,7.1,3.04195836363977));
#457542=CARTESIAN_POINT('Ctrl Pts',(1.05698038570037,7.1,3.04589992835325));
#457543=CARTESIAN_POINT('Ctrl Pts',(1.04217875085674,7.1,3.04973529915006));
#457544=CARTESIAN_POINT('Ctrl Pts',(0.940748947441955,7.1,3.07601759229222));
#457545=CARTESIAN_POINT('Ctrl Pts',(0.838451004717897,7.1,3.09734772782833));
#457546=CARTESIAN_POINT('Ctrl Pts',(0.73561798721121,7.1,3.11354024858967));
#457547=CARTESIAN_POINT('Ctrl Pts',(0.635624197682169,7.1,3.12928569253571));
#457548=CARTESIAN_POINT('Ctrl Pts',(0.535123733143622,7.1,3.14017332852956));
#457549=CARTESIAN_POINT('Ctrl Pts',(0.434422589760872,7.1,3.14598450424585));
#457550=CARTESIAN_POINT('Ctrl Pts',(0.334674581213765,7.1,3.15174067726976));
#457551=CARTESIAN_POINT('Ctrl Pts',(0.234729022424078,7.1,3.15251618885277));
#457552=CARTESIAN_POINT('Ctrl Pts',(0.134893270904415,7.1,3.14804909926986));
#457553=CARTESIAN_POINT('Ctrl Pts',(0.0727576360140052,7.1,3.14526887832575));
#457554=CARTESIAN_POINT('Ctrl Pts',(0.0106647685361902,7.1,3.14045671729177));
#457555=CARTESIAN_POINT('Ctrl Pts',(-0.0513069284014181,7.1,3.13364847640455));
#457556=CARTESIAN_POINT('Ctrl Pts',(-0.0783570039498824,7.1,3.13067674189587));
#457557=CARTESIAN_POINT('Ctrl Pts',(-0.10538394980607,7.1,3.12732463473769));
#457558=CARTESIAN_POINT('Ctrl Pts',(-0.132381022310655,7.1,3.12359482034564));
#457559=CARTESIAN_POINT('Ctrl Pts',(-0.148018419670001,7.1,3.12143441611236));
#457560=CARTESIAN_POINT('Ctrl Pts',(-0.163637581507457,7.1,3.1191483935117));
#457561=CARTESIAN_POINT('Ctrl Pts',(-0.179232128568581,7.1,3.11673850867025));
#457562=CARTESIAN_POINT('Ctrl Pts',(-0.278819614987809,7.1,3.10134887452577));
#457563=CARTESIAN_POINT('Ctrl Pts',(-0.377472084912431,7.1,3.08090281406002));
#457564=CARTESIAN_POINT('Ctrl Pts',(-0.474882184244777,7.1,3.05564016293009));
#457565=CARTESIAN_POINT('Ctrl Pts',(-0.574147134205758,7.1,3.02989646882155));
#457566=CARTESIAN_POINT('Ctrl Pts',(-0.672122792687237,7.1,2.99915057478039));
#457567=CARTESIAN_POINT('Ctrl Pts',(-0.76846447382552,7.1,2.96360641162069));
#457568=CARTESIAN_POINT('Ctrl Pts',(-0.864056331237232,7.1,2.9283388873629));
#457569=CARTESIAN_POINT('Ctrl Pts',(-0.958040274144051,7.1,2.88834687741555));
#457570=CARTESIAN_POINT('Ctrl Pts',(-1.05004898277166,7.1,2.8437891483571));
#457571=CARTESIAN_POINT('Ctrl Pts',(-1.09079293778152,7.1,2.82405777580358));
#457572=CARTESIAN_POINT('Ctrl Pts',(-1.13114908788126,7.1,2.8034306057743));
#457573=CARTESIAN_POINT('Ctrl Pts',(-1.17108303261526,7.1,2.78191933314891));
#457574=CARTESIAN_POINT('Ctrl Pts',(-1.19552288845622,7.1,2.76875428257797));
#457575=CARTESIAN_POINT('Ctrl Pts',(-1.21980457394424,7.1,2.7552580655895));
#457576=CARTESIAN_POINT('Ctrl Pts',(-1.24391987476384,7.1,2.74143315798034));
#457577=CARTESIAN_POINT('Ctrl Pts',(-1.25788504493234,7.1,2.73342715429123));
#457578=CARTESIAN_POINT('Ctrl Pts',(-1.27179184625963,7.1,2.72531232938243));
#457579=CARTESIAN_POINT('Ctrl Pts',(-1.28562993894826,7.1,2.71709465128527));
#457580=CARTESIAN_POINT('Ctrl Pts',(-1.372340524926,7.1,2.66560202876751));
#457581=CARTESIAN_POINT('Ctrl Pts',(-1.45645830167012,7.1,2.61001589207157));
#457582=CARTESIAN_POINT('Ctrl Pts',(-1.53764003195818,7.1,2.55051510841358));
#457583=CARTESIAN_POINT('Ctrl Pts',(-1.61843699822156,7.1,2.49129633107538));
#457584=CARTESIAN_POINT('Ctrl Pts',(-1.69632636725415,7.1,2.4281993445793));
#457585=CARTESIAN_POINT('Ctrl Pts',(-1.77092888084013,7.1,2.36136796463788));
#457586=CARTESIAN_POINT('Ctrl Pts',(-1.79272875583386,7.1,2.34183892120018));
#457587=CARTESIAN_POINT('Ctrl Pts',(-1.81424766634448,7.1,2.32199082074022));
#457588=CARTESIAN_POINT('Ctrl Pts',(-1.83547535662103,7.1,2.30182683287202));
#457589=CARTESIAN_POINT('Ctrl Pts',(-1.84945973062044,7.1,2.28854320455472));
#457590=CARTESIAN_POINT('Ctrl Pts',(-1.86331923229643,7.1,2.27512097363059));
#457591=CARTESIAN_POINT('Ctrl Pts',(-1.8770459964819,7.1,2.26156579733141));
#457592=CARTESIAN_POINT('Ctrl Pts',(-1.94633415556125,7.1,2.19314375706934));
#457593=CARTESIAN_POINT('Ctrl Pts',(-2.01210277297389,7.1,2.12147745509268));
#457594=CARTESIAN_POINT('Ctrl Pts',(-2.07401739382647,7.1,2.04671449447803));
#457595=CARTESIAN_POINT('Ctrl Pts',(-2.13419826203252,7.1,1.97404506975267));
#457596=CARTESIAN_POINT('Ctrl Pts',(-2.19073831622834,7.1,1.89844941478769));
#457597=CARTESIAN_POINT('Ctrl Pts',(-2.24328693920311,7.1,1.8200412855861));
#457598=CARTESIAN_POINT('Ctrl Pts',(-2.27661878753152,7.1,1.77030662609718));
#457599=CARTESIAN_POINT('Ctrl Pts',(-2.30834382556741,7.1,1.71943998109422));
#457600=CARTESIAN_POINT('Ctrl Pts',(-2.33836210323078,7.1,1.66746714335669));
#457601=CARTESIAN_POINT('',(-0.481137492902315,16.9,3.40820637768954));
#457602=CARTESIAN_POINT('Ctrl Pts',(-0.481137492902315,16.9,3.40820637768954));
#457603=CARTESIAN_POINT('Ctrl Pts',(-1.61086821599449,16.8472443247217,
3.24872196051297));
#457604=CARTESIAN_POINT('Ctrl Pts',(-2.64547056525308,16.7944886494434,
2.4849672353811));
#457605=CARTESIAN_POINT('Ctrl Pts',(-3.12419592397665,16.741732974165,1.45706125048672));
#457606=CARTESIAN_POINT('Ctrl Pts',(-3.60292128270023,16.6889772988867,
0.429155265592336));
#457607=CARTESIAN_POINT('Ctrl Pts',(-3.52576965088879,16.6362216236084,
-0.862901979064563));
#457608=CARTESIAN_POINT('Ctrl Pts',(-2.92452612924211,16.5834659483301,
-1.82680492798919));
#457609=CARTESIAN_POINT('Ctrl Pts',(-2.32328260759544,16.5307102730517,
-2.79070787691381));
#457610=CARTESIAN_POINT('Ctrl Pts',(-1.19794719611352,16.4779545977734,
-3.42645653010615));
#457611=CARTESIAN_POINT('Ctrl Pts',(-0.062122550227398,16.4251989224951,
-3.44673585535974));
#457612=CARTESIAN_POINT('Ctrl Pts',(-0.0414648377584936,16.4242394332157,
-3.44710468383311));
#457613=CARTESIAN_POINT('Ctrl Pts',(-0.0208036556395614,16.4232799439363,
-3.44726992612577));
#457614=CARTESIAN_POINT('Ctrl Pts',(-0.000142136989979558,16.4223204546569,
-3.44723320560186));
#457615=CARTESIAN_POINT('Ctrl Pts',(-2.95083879450908,16.9,-0.516457884956439));
#457616=CARTESIAN_POINT('Ctrl Pts',(-2.97665665724874,16.9,-0.418641055033343));
#457617=CARTESIAN_POINT('Ctrl Pts',(-2.99771031524562,16.9,-0.319615847049016));
#457618=CARTESIAN_POINT('Ctrl Pts',(-3.01401797859282,16.9,-0.219802864251303));
#457619=CARTESIAN_POINT('Ctrl Pts',(-3.03050300001566,16.9,-0.118904340369248));
#457620=CARTESIAN_POINT('Ctrl Pts',(-3.04213854325016,16.9,-0.01719992756052));
#457621=CARTESIAN_POINT('Ctrl Pts',(-3.04889618900187,16.9,0.0849005471415487));
#457622=CARTESIAN_POINT('Ctrl Pts',(-3.05595054381229,16.9,0.191483964107199));
#457623=CARTESIAN_POINT('Ctrl Pts',(-3.05768994941762,16.9,0.298500029301654));
#457624=CARTESIAN_POINT('Ctrl Pts',(-3.0540226994191,16.9,0.405494501672288));
#457625=CARTESIAN_POINT('Ctrl Pts',(-3.05352154435089,16.9,0.420116036097146));
#457626=CARTESIAN_POINT('Ctrl Pts',(-3.05291931902786,16.9,0.43473565270573));
#457627=CARTESIAN_POINT('Ctrl Pts',(-3.05221650494449,16.9,0.449340169749314));
#457628=CARTESIAN_POINT('Ctrl Pts',(-3.04717082651286,16.9,0.554189657535853));
#457629=CARTESIAN_POINT('Ctrl Pts',(-3.03693930777746,16.9,0.658428042447195));
#457630=CARTESIAN_POINT('Ctrl Pts',(-3.0215319722778,16.9,0.761619901782156));
#457631=CARTESIAN_POINT('Ctrl Pts',(-3.00620861576567,16.9,0.864249305144831));
#457632=CARTESIAN_POINT('Ctrl Pts',(-2.9857658698597,16.9,0.965844543239253));
#457633=CARTESIAN_POINT('Ctrl Pts',(-2.96016437649631,16.9,1.06598987532431));
#457634=CARTESIAN_POINT('Ctrl Pts',(-2.93637971082258,16.9,1.15902832462952));
#457635=CARTESIAN_POINT('Ctrl Pts',(-2.90814215886226,16.9,1.25081609535364));
#457636=CARTESIAN_POINT('Ctrl Pts',(-2.87537983234519,16.9,1.34101850078862));
#457637=CARTESIAN_POINT('Ctrl Pts',(-2.85211250745606,16.9,1.40507892921831));
#457638=CARTESIAN_POINT('Ctrl Pts',(-2.82656219568971,16.9,1.4683397228178));
#457639=CARTESIAN_POINT('Ctrl Pts',(-2.79881563558833,16.9,1.53074168394433));
#457640=CARTESIAN_POINT('Ctrl Pts',(-2.79101207619887,16.9,1.54829187423423));
#457641=CARTESIAN_POINT('Ctrl Pts',(-2.78303473738331,16.9,1.56577411033552));
#457642=CARTESIAN_POINT('Ctrl Pts',(-2.77488541132478,16.9,1.58318701982711));
#457643=CARTESIAN_POINT('Ctrl Pts',(-2.76883812508864,16.9,1.59610843776319));
#457644=CARTESIAN_POINT('Ctrl Pts',(-2.76269766084434,16.9,1.6089883219928));
#457645=CARTESIAN_POINT('Ctrl Pts',(-2.75646860826711,16.9,1.62181874485785));
#457646=CARTESIAN_POINT('Ctrl Pts',(-2.71214573987275,16.9,1.71311371099289));
#457647=CARTESIAN_POINT('Ctrl Pts',(-2.66328947658821,16.9,1.80201746569949));
#457648=CARTESIAN_POINT('Ctrl Pts',(-2.61026832672044,16.9,1.88836191237357));
#457649=CARTESIAN_POINT('Ctrl Pts',(-2.55591587729441,16.9,1.97687436792717));
#457650=CARTESIAN_POINT('Ctrl Pts',(-2.4971864760472,16.9,2.06269796096898));
#457651=CARTESIAN_POINT('Ctrl Pts',(-2.43442373776504,16.9,2.14564097133398));
#457652=CARTESIAN_POINT('Ctrl Pts',(-2.3703172711337,16.9,2.23035976263915));
#457653=CARTESIAN_POINT('Ctrl Pts',(-2.30200252139198,16.9,2.31207399252615));
#457654=CARTESIAN_POINT('Ctrl Pts',(-2.22979594959464,16.9,2.39055866186983));
#457655=CARTESIAN_POINT('Ctrl Pts',(-2.17205037665802,16.9,2.45332500134807));
#457656=CARTESIAN_POINT('Ctrl Pts',(-2.11181465263588,16.9,2.514025560767));
#457657=CARTESIAN_POINT('Ctrl Pts',(-2.04923130743126,16.9,2.57253148290693));
#457658=CARTESIAN_POINT('Ctrl Pts',(-2.03367601033663,16.9,2.58707332303559));
#457659=CARTESIAN_POINT('Ctrl Pts',(-2.01797313835135,16.9,2.6014815998716));
#457660=CARTESIAN_POINT('Ctrl Pts',(-2.00214415374043,16.9,2.61573711032485));
#457661=CARTESIAN_POINT('Ctrl Pts',(-1.92090172313698,16.9,2.68890366820473));
#457662=CARTESIAN_POINT('Ctrl Pts',(-1.83624321763956,16.9,2.75814154583534));
#457663=CARTESIAN_POINT('Ctrl Pts',(-1.74852417421841,16.9,2.82322932329071));
#457664=CARTESIAN_POINT('Ctrl Pts',(-1.66023056131919,16.9,2.88874343291823));
#457665=CARTESIAN_POINT('Ctrl Pts',(-1.56883558826159,16.9,2.95005359433295));
#457666=CARTESIAN_POINT('Ctrl Pts',(-1.4746593948356,16.9,3.00690315349514));
#457667=CARTESIAN_POINT('Ctrl Pts',(-1.43136482290328,16.9,3.03303796781425));
#457668=CARTESIAN_POINT('Ctrl Pts',(-1.38748193232619,16.9,3.05822958055756));
#457669=CARTESIAN_POINT('Ctrl Pts',(-1.34303938800765,16.9,3.08245025734981));
#457670=CARTESIAN_POINT('Ctrl Pts',(-1.32209356895734,16.9,3.09386548843402));
#457671=CARTESIAN_POINT('Ctrl Pts',(-1.30102083757109,16.9,3.10506623219387));
#457672=CARTESIAN_POINT('Ctrl Pts',(-1.27984620853268,16.9,3.11603835315651));
#457673=CARTESIAN_POINT('Ctrl Pts',(-1.18059898650193,16.9,3.1674655835156));
#457674=CARTESIAN_POINT('Ctrl Pts',(-1.07901924295251,16.9,3.2139275868326));
#457675=CARTESIAN_POINT('Ctrl Pts',(-0.975447865270529,16.9,3.25517602269448));
#457676=CARTESIAN_POINT('Ctrl Pts',(-0.873362763874905,16.9,3.29583253274208));
#457677=CARTESIAN_POINT('Ctrl Pts',(-0.769342057532994,16.9,3.3314245874836));
#457678=CARTESIAN_POINT('Ctrl Pts',(-0.663681668072933,16.9,3.36167482802888));
#457679=CARTESIAN_POINT('Ctrl Pts',(-0.603351390250923,16.9,3.37894719874042));
#457680=CARTESIAN_POINT('Ctrl Pts',(-0.54248603792155,16.9,3.39447725268593));
#457681=CARTESIAN_POINT('Ctrl Pts',(-0.481137492902315,16.9,3.40820637768954));
#457682=CARTESIAN_POINT('Origin',(0.,21.9,0.));
#457683=CARTESIAN_POINT('',(3.67394039744206E-16,21.4,-3.));
#457684=CARTESIAN_POINT('',(-3.67394039744206E-16,21.4,3.));
#457685=CARTESIAN_POINT('Origin',(0.,21.4,0.));
#457686=CARTESIAN_POINT('Origin',(0.,21.4,0.));
#457687=CARTESIAN_POINT('',(-3.06161699786838E-16,21.9,2.5));
#457688=CARTESIAN_POINT('',(-3.06161699786838E-16,21.9,2.5));
#457689=CARTESIAN_POINT('Origin',(0.,21.9,0.));
#457690=CARTESIAN_POINT('Origin',(0.,0.,0.));
#457691=CARTESIAN_POINT('',(-1.71450551880629E-16,7.1,-1.4));
#457692=CARTESIAN_POINT('Origin',(0.,7.1,0.));
#457693=CARTESIAN_POINT('',(-1.71450551880629E-16,0.,-1.4));
#457694=CARTESIAN_POINT('Origin',(0.,0.,0.));
#457695=CARTESIAN_POINT('Origin',(0.,16.9,0.));
#457696=CARTESIAN_POINT('Origin',(0.,0.,0.));
#457697=CARTESIAN_POINT('',(-3.67394039744206E-16,0.,-3.));
#457698=CARTESIAN_POINT('Origin',(0.,16.9,0.));
#457699=CARTESIAN_POINT('Origin',(0.,0.,0.));
#457700=CARTESIAN_POINT('',(-2.57175827820944E-16,16.9,-2.1));
#457701=CARTESIAN_POINT('Origin',(0.,16.9,0.));
#457702=CARTESIAN_POINT('',(-2.57175827820944E-16,21.9,-2.1));
#457703=CARTESIAN_POINT('',(-2.57175827820944E-16,0.,-2.1));
#457704=CARTESIAN_POINT('Origin',(0.,21.9,0.));
#457705=CARTESIAN_POINT('Origin',(0.,16.9,0.));
#457706=CARTESIAN_POINT('',(-1.22464679914735E-16,15.8,-0.999999999999999));
#457707=CARTESIAN_POINT('Origin',(0.,15.8,0.));
#457708=CARTESIAN_POINT('',(-2.57175827820944E-16,16.9,-2.1));
#457709=CARTESIAN_POINT('Origin',(0.,0.,0.));
#457710=CARTESIAN_POINT('',(-1.22464679914735E-16,0.,-1.));
#457711=CARTESIAN_POINT('Origin',(0.,0.,0.));
#457712=CARTESIAN_POINT('',(-1.22464679914735E-16,0.,-1.));
#457713=CARTESIAN_POINT('Origin',(2.1,21.9,0.));
#457714=CARTESIAN_POINT('Origin',(3.5,16.9,0.));
#457715=CARTESIAN_POINT('Origin',(1.4,7.1,0.));
#457716=CARTESIAN_POINT('Origin',(1.,0.,0.));
#457717=CARTESIAN_POINT('',(0.,0.,0.));
#457718=CARTESIAN_POINT('Origin',(1.66533478931514E-15,-5.24520618636721E-7,
16.));
#457719=CARTESIAN_POINT('',(-2.,-5.24520618391792E-7,16.));
#457720=CARTESIAN_POINT('Origin',(1.66533478931514E-15,-5.24520618636721E-7,
16.));
#457721=CARTESIAN_POINT('',(-0.999999999999998,-5.24520618514257E-7,16.));
#457722=CARTESIAN_POINT('Origin',(1.66533478931514E-15,-5.24520618636721E-7,
16.));
#457723=CARTESIAN_POINT('Origin',(2.52377408738871E-22,-5.2452070126943E-7,
3.10862446895044E-14));
#457724=CARTESIAN_POINT('',(-1.,-5.24520737298776E-7,-6.99999999999997));
#457725=CARTESIAN_POINT('Origin',(-6.93889138013314E-16,-5.2452073742124E-7,
-6.99999999999997));
#457726=CARTESIAN_POINT('',(-1.,-5.24520701146966E-7,3.11853717452745E-14));
#457727=CARTESIAN_POINT('Origin',(2.52377408738871E-22,-5.2452070126943E-7,
3.10862446895044E-14));
#457728=CARTESIAN_POINT('',(-2.,-5.24520737176311E-7,-6.99999999999997));
#457729=CARTESIAN_POINT('Origin',(-6.93889138013314E-16,-5.2452073742124E-7,
-6.99999999999997));
#457730=CARTESIAN_POINT('',(-2.,-5.24520701024501E-7,3.12844988010446E-14));
#457731=CARTESIAN_POINT('Origin',(-6.93889138013314E-16,-5.2452073742124E-7,
-6.99999999999997));
#457732=CARTESIAN_POINT('',(0.,0.,0.));
#457733=CARTESIAN_POINT('Origin',(0.,3.,0.));
#457734=CARTESIAN_POINT('',(0.00204489390602899,4.82217611708959,-2.94517214357972));
#457735=CARTESIAN_POINT('',(0.00306920594250255,4.6778238829104,-2.94456560854251));
#457736=CARTESIAN_POINT('',(-3.60291088309151E-16,3.,-2.942));
#457737=CARTESIAN_POINT('',(2.64462557919717,4.5,1.28892185405325));
#457738=CARTESIAN_POINT('Ctrl Pts',(0.00204489390602899,4.82217611708959,
-2.94517214357972));
#457739=CARTESIAN_POINT('Ctrl Pts',(0.115595709257588,4.81601388075811,
-2.94601231310178));
#457740=CARTESIAN_POINT('Ctrl Pts',(0.229051990736059,4.80985164442663,
-2.94001182656897));
#457741=CARTESIAN_POINT('Ctrl Pts',(0.341669115408411,4.80368940809515,
-2.92687312091722));
#457742=CARTESIAN_POINT('Ctrl Pts',(1.3055780156619,4.75094579150344,-2.81441673071565));
#457743=CARTESIAN_POINT('Ctrl Pts',(2.2080108266608,4.69820217491173,-2.17901898739065));
#457744=CARTESIAN_POINT('Ctrl Pts',(2.63957178730816,4.64545855832002,-1.3094537656246));
#457745=CARTESIAN_POINT('Ctrl Pts',(3.03629742742308,4.59697237221335,-0.51007928395386));
#457746=CARTESIAN_POINT('Ctrl Pts',(3.0351001382147,4.54848618610667,0.487184727328701));
#457747=CARTESIAN_POINT('Ctrl Pts',(2.64824696753857,4.5,1.29202795241196));
#457748=CARTESIAN_POINT('',(2.64462557919718,4.5,-1.28892185405322));
#457749=CARTESIAN_POINT('Origin',(0.,4.5,0.));
#457750=CARTESIAN_POINT('Ctrl Pts',(2.64462557919718,4.5,-1.28892185405322));
#457751=CARTESIAN_POINT('Ctrl Pts',(2.21747956182461,4.55274361659171,-2.16534526175893));
#457752=CARTESIAN_POINT('Ctrl Pts',(1.32424522902399,4.60548723318342,-2.80537305816962));
#457753=CARTESIAN_POINT('Ctrl Pts',(0.362562604027333,4.65823084977513,
-2.92409687808116));
#457754=CARTESIAN_POINT('Ctrl Pts',(0.243481656386912,4.66476186082022,
-2.93879792873454));
#457755=CARTESIAN_POINT('Ctrl Pts',(0.123351205849263,4.67129287186531,
-2.94550593798222));
#457756=CARTESIAN_POINT('Ctrl Pts',(0.00306920594250255,4.6778238829104,
-2.94456560854251));
#457757=CARTESIAN_POINT('Origin',(0.,3.,0.));
#457758=CARTESIAN_POINT('',(0.000981781161582679,5.8221761170896,-2.93756896724413));
#457759=CARTESIAN_POINT('',(0.000893653388113867,5.67782388291041,-2.93749789116703));
#457760=CARTESIAN_POINT('',(-3.60291088309151E-16,3.,-2.942));
#457761=CARTESIAN_POINT('Ctrl Pts',(0.000981781161582679,5.8221761170896,
-2.93756896724413));
#457762=CARTESIAN_POINT('Ctrl Pts',(0.428271775376875,5.79914224697505,
-2.93885349412934));
#457763=CARTESIAN_POINT('Ctrl Pts',(0.855061811092587,5.77610837686051,
-2.85165705277319));
#457764=CARTESIAN_POINT('Ctrl Pts',(1.23960299590781,5.75307450674596,-2.67334968914282));
#457765=CARTESIAN_POINT('Ctrl Pts',(2.12013643274481,5.70033089015425,-2.26505637256028));
#457766=CARTESIAN_POINT('Ctrl Pts',(2.77914581809647,5.64758727356254,-1.37903975211099));
#457767=CARTESIAN_POINT('Ctrl Pts',(2.9169201456039,5.59484365697083,-0.418274554268889));
#457768=CARTESIAN_POINT('Ctrl Pts',(3.05469447311133,5.54210004037911,0.542490643573213));
#457769=CARTESIAN_POINT('Ctrl Pts',(2.67123374277452,5.4893564237874,1.57800441880812));
#457770=CARTESIAN_POINT('Ctrl Pts',(1.94090479190002,5.43661280719569,2.21728508663937));
#457771=CARTESIAN_POINT('Ctrl Pts',(1.21057584102552,5.38386919060398,2.85656575447061));
#457772=CARTESIAN_POINT('Ctrl Pts',(0.133378669613329,5.33112557401227,
3.09961331489819));
#457773=CARTESIAN_POINT('Ctrl Pts',(-0.800679302822102,5.27838195742056,
2.83590049151496));
#457774=CARTESIAN_POINT('Ctrl Pts',(-1.73473727525754,5.22563834082884,
2.57218766813174));
#457775=CARTESIAN_POINT('Ctrl Pts',(-2.52565604871622,5.17289472423713,
1.80171446093771));
#457776=CARTESIAN_POINT('Ctrl Pts',(-2.81385459239328,5.12015110764542,
0.87487771750423));
#457777=CARTESIAN_POINT('Ctrl Pts',(-3.10205313607034,5.06740749105371,
-0.0519590259292509));
#457778=CARTESIAN_POINT('Ctrl Pts',(-2.88753144996578,5.014663874462,-1.13515930560218));
#457779=CARTESIAN_POINT('Ctrl Pts',(-2.26757811215946,4.96192025787029,
-1.88200192689957));
#457780=CARTESIAN_POINT('Ctrl Pts',(-1.72005626898549,4.91533887761006,
-2.54158809836943));
#457781=CARTESIAN_POINT('Ctrl Pts',(-0.856304806466375,4.86875749734983,
-2.93882116093559));
#457782=CARTESIAN_POINT('Ctrl Pts',(0.00204489390602899,4.82217611708959,
-2.94517214357972));
#457783=CARTESIAN_POINT('Ctrl Pts',(0.00306920594250255,4.6778238829104,
-2.94456560854251));
#457784=CARTESIAN_POINT('Ctrl Pts',(-0.848030964869353,4.72403648845702,
-2.93791195672947));
#457785=CARTESIAN_POINT('Ctrl Pts',(-1.70671890654028,4.77024909400365,
-2.5483214325781));
#457786=CARTESIAN_POINT('Ctrl Pts',(-2.25487242219768,4.81646169955027,
-1.89791348056393));
#457787=CARTESIAN_POINT('Ctrl Pts',(-2.88049390623335,4.86920531614198,
-1.15558641972276));
#457788=CARTESIAN_POINT('Ctrl Pts',(-3.10160595711201,4.92194893273369,
-0.073512454628034));
#457789=CARTESIAN_POINT('Ctrl Pts',(-2.81962896312916,4.9746925493254,0.855399811136087));
#457790=CARTESIAN_POINT('Ctrl Pts',(-2.53765196914631,5.02743616591711,
1.78431207690021));
#457791=CARTESIAN_POINT('Ctrl Pts',(-1.75258593030197,5.08017978250882,
2.56006264333372));
#457792=CARTESIAN_POINT('Ctrl Pts',(-0.820498884581772,5.13292339910054,
2.83021329833381));
#457793=CARTESIAN_POINT('Ctrl Pts',(0.111588161138428,5.18566701569225,
3.1003639533339));
#457794=CARTESIAN_POINT('Ctrl Pts',(1.19069621373448,5.23841063228397,2.86491469690055));
#457795=CARTESIAN_POINT('Ctrl Pts',(1.92551094486043,5.29115424887568,2.23075121842718));
#457796=CARTESIAN_POINT('Ctrl Pts',(2.66032567598638,5.34389786546738,1.5965877399538));
#457797=CARTESIAN_POINT('Ctrl Pts',(3.05084708564221,5.39664148205909,0.563710039440399));
#457798=CARTESIAN_POINT('Ctrl Pts',(2.91972366900985,5.4493850986508,-0.398002862116583));
#457799=CARTESIAN_POINT('Ctrl Pts',(2.78860025237749,5.50212871524251,-1.35971576367356));
#457800=CARTESIAN_POINT('Ctrl Pts',(2.13583200945693,5.55487233183423,-2.25026386627412));
#457801=CARTESIAN_POINT('Ctrl Pts',(1.2581738224207,5.60761594842594,-2.66466135998438));
#457802=CARTESIAN_POINT('Ctrl Pts',(0.868751857091186,5.6310185932541,-2.84853190185583));
#457803=CARTESIAN_POINT('Ctrl Pts',(0.435054734933217,5.65442123808225,
-2.93866040041147));
#457804=CARTESIAN_POINT('Ctrl Pts',(0.000893653388113867,5.67782388291041,
-2.93749789116703));
#457805=CARTESIAN_POINT('Origin',(0.,3.,0.));
#457806=CARTESIAN_POINT('',(-0.00264271788274373,6.82217611708959,-2.9417027311706));
#457807=CARTESIAN_POINT('',(-0.00264177732640618,6.6778238829104,-2.94190629230735));
#457808=CARTESIAN_POINT('',(-3.60291088309151E-16,3.,-2.942));
#457809=CARTESIAN_POINT('Ctrl Pts',(-0.00264271788274373,6.82217611708959,
-2.9417027311706));
#457810=CARTESIAN_POINT('Ctrl Pts',(0.734997799300586,6.78227061319198,
-2.93506069017881));
#457811=CARTESIAN_POINT('Ctrl Pts',(1.4771604329565,6.74236510929437,-2.65342570259176));
#457812=CARTESIAN_POINT('Ctrl Pts',(2.01336848140481,6.70245960539677,-2.15168714141107));
#457813=CARTESIAN_POINT('Ctrl Pts',(2.72208153996718,6.64971598880506,-1.48853284650247));
#457814=CARTESIAN_POINT('Ctrl Pts',(3.07100742352953,6.59697237221335,-0.440874157720627));
#457815=CARTESIAN_POINT('Ctrl Pts',(2.90144769528211,6.54422875562164,0.514791795945116));
#457816=CARTESIAN_POINT('Ctrl Pts',(2.73188796703469,6.49148513902993,1.47045774961087));
#457817=CARTESIAN_POINT('Ctrl Pts',(2.04384262697749,6.43874152243821,2.33413096816052));
#457818=CARTESIAN_POINT('Ctrl Pts',(1.15024840682446,6.3859979058465,2.71299454039048));
#457819=CARTESIAN_POINT('Ctrl Pts',(0.256654186671437,6.33325428925479,
3.09185811262044));
#457820=CARTESIAN_POINT('Ctrl Pts',(-0.842488913577421,6.28051067266308,
2.98591203853071));
#457821=CARTESIAN_POINT('Ctrl Pts',(-1.64726601382998,6.22776705607136,
2.44334313153912));
#457822=CARTESIAN_POINT('Ctrl Pts',(-2.45204311408254,6.17502343947965,
1.90077422454753));
#457823=CARTESIAN_POINT('Ctrl Pts',(-2.96245421433879,6.12227982288795,
0.921582484654079));
#457824=CARTESIAN_POINT('Ctrl Pts',(-2.94635644829672,6.06953620629623,
-0.0488756812789066));
#457825=CARTESIAN_POINT('Ctrl Pts',(-2.93025868225464,6.01679258970452,
-1.01933384721189));
#457826=CARTESIAN_POINT('Ctrl Pts',(-2.38765204991423,5.96404897311281,
-1.98105843918441));
#457827=CARTESIAN_POINT('Ctrl Pts',(-1.56531998958287,5.91130535652109,
-2.49663572881278));
#457828=CARTESIAN_POINT('Ctrl Pts',(-1.102111764375,5.88159561004393,-2.7870532533223));
#457829=CARTESIAN_POINT('Ctrl Pts',(-0.550149111616638,5.85188586356676,
-2.93591214761665));
#457830=CARTESIAN_POINT('Ctrl Pts',(0.000981781161582679,5.8221761170896,
-2.93756896724413));
#457831=CARTESIAN_POINT('Ctrl Pts',(0.000893653388113867,5.67782388291041,
-2.93749789116703));
#457832=CARTESIAN_POINT('Ctrl Pts',(-0.543434055210251,5.70716485467396,
-2.93604039988063));
#457833=CARTESIAN_POINT('Ctrl Pts',(-1.0884910518124,5.73650582643752,-2.79108449324106));
#457834=CARTESIAN_POINT('Ctrl Pts',(-1.54793699155054,5.76584679820108,
-2.50746051746281));
#457835=CARTESIAN_POINT('Ctrl Pts',(-2.37384148733363,5.81859041479279,
-1.99761529641102));
#457836=CARTESIAN_POINT('Ctrl Pts',(-2.9231023477479,5.8713340313845,-1.03967796948751));
#457837=CARTESIAN_POINT('Ctrl Pts',(-2.94594125892771,5.92407764797621,
-0.0693531678554593));
#457838=CARTESIAN_POINT('Ctrl Pts',(-2.96878017010752,5.97682126456792,
0.900971633776593));
#457839=CARTESIAN_POINT('Ctrl Pts',(-2.46519713205287,6.02956488115963,
1.88368391011718));
#457840=CARTESIAN_POINT('Ctrl Pts',(-1.66421307231912,6.08230849775135,
2.43183300596836));
#457841=CARTESIAN_POINT('Ctrl Pts',(-0.863229012585371,6.13505211434306,
2.97998210181954));
#457842=CARTESIAN_POINT('Ctrl Pts',(0.235156068827473,6.18779573093477,
3.0935680171813));
#457843=CARTESIAN_POINT('Ctrl Pts',(1.13136355306654,6.24053934752648,2.72092556542027));
#457844=CARTESIAN_POINT('Ctrl Pts',(2.02757103730561,6.29328296411819,2.34828311365924));
#457845=CARTESIAN_POINT('Ctrl Pts',(2.72160092437091,6.34602658070991,1.48941229477542));
#457846=CARTESIAN_POINT('Ctrl Pts',(2.89779899417553,6.39877019730162,0.534947661132899));
#457847=CARTESIAN_POINT('Ctrl Pts',(3.07399706398015,6.45151381389333,-0.41951697250962));
#457848=CARTESIAN_POINT('Ctrl Pts',(2.73236331652411,6.50425743048504,-1.46957542091083));
#457849=CARTESIAN_POINT('Ctrl Pts',(2.02827728417431,6.55700104707675,-2.13764006536679));
#457850=CARTESIAN_POINT('Ctrl Pts',(1.49064716198093,6.59727532568796,-2.64776476594244));
#457851=CARTESIAN_POINT('Ctrl Pts',(0.741684403530869,6.63754960429918,
-2.93516288708673));
#457852=CARTESIAN_POINT('Ctrl Pts',(-0.00264177732640618,6.6778238829104,
-2.94190629230735));
#457853=CARTESIAN_POINT('Origin',(0.,3.,0.));
#457854=CARTESIAN_POINT('',(0.00129800184776322,7.82217611708959,-2.94604313323476));
#457855=CARTESIAN_POINT('',(0.00140312681252501,7.6778238829104,-2.94591746634222));
#457856=CARTESIAN_POINT('',(-3.60291088309151E-16,3.,-2.942));
#457857=CARTESIAN_POINT('Ctrl Pts',(0.00129800184776322,7.82217611708959,
-2.94604313323476));
#457858=CARTESIAN_POINT('Ctrl Pts',(0.0755715349378736,7.81814259600063,
-2.94645485212743));
#457859=CARTESIAN_POINT('Ctrl Pts',(0.149816148931046,7.81410907491166,
-2.94388766332912));
#457860=CARTESIAN_POINT('Ctrl Pts',(0.223826844685575,7.8100755538227,-2.93824975742655));
#457861=CARTESIAN_POINT('Ctrl Pts',(1.19161446112962,7.75733193723099,-2.86452668997584));
#457862=CARTESIAN_POINT('Ctrl Pts',(2.11940435786337,7.70458832063929,-2.26574117865999));
#457863=CARTESIAN_POINT('Ctrl Pts',(2.58521826822479,7.65184470404758,-1.41423351224767));
#457864=CARTESIAN_POINT('Ctrl Pts',(3.05103217858622,7.59910108745587,-0.562725845835348));
#457865=CARTESIAN_POINT('Ctrl Pts',(3.05487010257533,7.54635747086415,0.541503975673445));
#457866=CARTESIAN_POINT('Ctrl Pts',(2.59498642658716,7.49361385427244,1.3962290203992));
#457867=CARTESIAN_POINT('Ctrl Pts',(2.13510275059898,7.44087023768072,2.25095406512496));
#457868=CARTESIAN_POINT('Ctrl Pts',(1.21149747463351,7.38812662108902,2.85617433306768));
#457869=CARTESIAN_POINT('Ctrl Pts',(0.244245721932247,7.33538300449731,
2.93662289957016));
#457870=CARTESIAN_POINT('Ctrl Pts',(-0.723006030769017,7.2826393879056,
3.01707146607263));
#457871=CARTESIAN_POINT('Ctrl Pts',(-1.73390426020608,7.22989577131388,
2.57274833113485));
#457872=CARTESIAN_POINT('Ctrl Pts',(-2.3286711692656,7.17715215472217,1.80574101603959));
#457873=CARTESIAN_POINT('Ctrl Pts',(-2.92343807832512,7.12440853813046,
1.03873370094433));
#457874=CARTESIAN_POINT('Ctrl Pts',(-3.10207366700711,7.07166492153875,
-0.0509577943084069));
#457875=CARTESIAN_POINT('Ctrl Pts',(-2.78333075944698,7.01892130494704,
-0.967718866739653));
#457876=CARTESIAN_POINT('Ctrl Pts',(-2.46458785188685,6.96617768835533,
-1.8844799391709));
#457877=CARTESIAN_POINT('Ctrl Pts',(-1.64846644808462,6.91343407176362,
-2.62831058878065));
#457878=CARTESIAN_POINT('Ctrl Pts',(-0.706155629402298,6.8606904551719,
-2.86090096306784));
#457879=CARTESIAN_POINT('Ctrl Pts',(-0.476791523092288,6.8478523424778,
-2.91751485550865));
#457880=CARTESIAN_POINT('Ctrl Pts',(-0.239951138085479,6.8350142297837,
-2.94383956099213));
#457881=CARTESIAN_POINT('Ctrl Pts',(-0.00264271788274373,6.82217611708959,
-2.9417027311706));
#457882=CARTESIAN_POINT('Ctrl Pts',(-0.00264177732640618,6.6778238829104,
-2.94190629230735));
#457883=CARTESIAN_POINT('Ctrl Pts',(-0.233092949560548,6.6902932208909,
-2.94399412110863));
#457884=CARTESIAN_POINT('Ctrl Pts',(-0.463099665782757,6.70276255887139,
-2.9191787711594));
#457885=CARTESIAN_POINT('Ctrl Pts',(-0.686252210885122,6.71523189685188,
-2.86574100273549));
#457886=CARTESIAN_POINT('Ctrl Pts',(-1.63015735635119,6.7679755134436,-2.63970645513751));
#457887=CARTESIAN_POINT('Ctrl Pts',(-2.45142933003978,6.82071913003531,
-1.90156651943084));
#457888=CARTESIAN_POINT('Ctrl Pts',(-2.7765370813594,6.87346274662702,-0.987043051743171));
#457889=CARTESIAN_POINT('Ctrl Pts',(-3.10164483267902,6.92620636321873,
-0.0725195840554919));
#457890=CARTESIAN_POINT('Ctrl Pts',(-2.93058836162966,6.97894997981044,
1.01838741561319));
#457891=CARTESIAN_POINT('Ctrl Pts',(-2.3411673766406,7.03169359640215,1.78951064022412));
#457892=CARTESIAN_POINT('Ctrl Pts',(-1.75174639165153,7.08443721299386,
2.56063386483504));
#457893=CARTESIAN_POINT('Ctrl Pts',(-0.743960892722759,7.13718082958557,
3.0119733143882));
#457894=CARTESIAN_POINT('Ctrl Pts',(0.223826880773889,7.18992444617729,
2.93825023490967));
#457895=CARTESIAN_POINT('Ctrl Pts',(1.19161465427054,7.242668062769,2.86452715543114));
#457896=CARTESIAN_POINT('Ctrl Pts',(2.11940470233506,7.29541167936071,2.26574154692092));
#457897=CARTESIAN_POINT('Ctrl Pts',(2.58521868854488,7.34815529595242,1.41423374213998));
#457898=CARTESIAN_POINT('Ctrl Pts',(3.0510326747547,7.40089891254413,0.562725937359059));
#457899=CARTESIAN_POINT('Ctrl Pts',(3.05487059910983,7.45364252913584,-0.541504063692575));
#457900=CARTESIAN_POINT('Ctrl Pts',(2.59498684828562,7.50638614572756,-1.39622924734966));
#457901=CARTESIAN_POINT('Ctrl Pts',(2.1351030974614,7.55912976231927,-2.25095443100676));
#457902=CARTESIAN_POINT('Ctrl Pts',(1.21149767145785,7.61187337891098,-2.8561747972693));
#457903=CARTESIAN_POINT('Ctrl Pts',(0.244245761627965,7.66461699550269,
-2.93662337684054));
#457904=CARTESIAN_POINT('Ctrl Pts',(0.163513166902145,7.66901929130526,
-2.94333809355992));
#457905=CARTESIAN_POINT('Ctrl Pts',(0.0824765061543352,7.67342158710783,
-2.94639695405348));
#457906=CARTESIAN_POINT('Ctrl Pts',(0.00140312681252501,7.6778238829104,
-2.94591746634222));
#457907=CARTESIAN_POINT('Origin',(0.,3.,0.));
#457908=CARTESIAN_POINT('',(0.00153914408188974,8.8221761170896,-2.93808272452622));
#457909=CARTESIAN_POINT('',(0.00144847389154757,8.6778238829104,-2.93797820450178));
#457910=CARTESIAN_POINT('',(-3.60291088309151E-16,3.,-2.942));
#457911=CARTESIAN_POINT('Ctrl Pts',(0.00153914408188974,8.8221761170896,
-2.93808272452622));
#457912=CARTESIAN_POINT('Ctrl Pts',(0.389170831585484,8.80127096221757,
-2.93993704747556));
#457913=CARTESIAN_POINT('Ctrl Pts',(0.776147818545245,8.78036580734554,
-2.86862350780525));
#457914=CARTESIAN_POINT('Ctrl Pts',(1.13136337989906,8.75946065247352,-2.7209251248051));
#457915=CARTESIAN_POINT('Ctrl Pts',(2.02757072637158,8.70671703588181,-2.34828273435812));
#457916=CARTESIAN_POINT('Ctrl Pts',(2.72160048053392,8.65397341929009,-1.4894120522401));
#457917=CARTESIAN_POINT('Ctrl Pts',(2.89779851724907,8.60122980269838,-0.534947573196851));
#457918=CARTESIAN_POINT('Ctrl Pts',(3.07399655396423,8.54848618610667,0.419516905846398));
#457919=CARTESIAN_POINT('Ctrl Pts',(2.7323628732322,8.49574256951496,1.46957518181485));
#457920=CARTESIAN_POINT('Ctrl Pts',(2.02827695781208,8.44299895292325,2.13763971734417));
#457921=CARTESIAN_POINT('Ctrl Pts',(1.32419104239198,8.39025533633153,2.80570425287348));
#457922=CARTESIAN_POINT('Ctrl Pts',(0.25765289228379,8.33751171973983,3.09177504796364));
#457923=CARTESIAN_POINT('Ctrl Pts',(-0.686252101162055,8.28476810314811,
2.8657405373204));
#457924=CARTESIAN_POINT('Ctrl Pts',(-1.63015709460791,8.2320244865564,2.63970602667716));
#457925=CARTESIAN_POINT('Ctrl Pts',(-2.45142893139143,8.17928086996469,
1.90156621030051));
#457926=CARTESIAN_POINT('Ctrl Pts',(-2.77653662909856,8.12653725337298,
0.987042891116816));
#457927=CARTESIAN_POINT('Ctrl Pts',(-3.1016443268057,8.07379363678127,0.0725195719331172));
#457928=CARTESIAN_POINT('Ctrl Pts',(-2.93058788543645,8.02105002018956,
-1.01838725005763));
#457929=CARTESIAN_POINT('Ctrl Pts',(-2.34116699667465,7.96830640359785,
-1.78951034926022));
#457930=CARTESIAN_POINT('Ctrl Pts',(-1.79682154525911,7.9195963080951,-2.50166249645367));
#457931=CARTESIAN_POINT('Ctrl Pts',(-0.895653026881721,7.87088621259234,
-2.9410710837177));
#457932=CARTESIAN_POINT('Ctrl Pts',(0.00129800184776322,7.82217611708959,
-2.94604313323476));
#457933=CARTESIAN_POINT('Ctrl Pts',(0.00140312681252501,7.6778238829104,
-2.94591746634222));
#457934=CARTESIAN_POINT('Ctrl Pts',(-0.888858321755623,7.72616520369954,
-2.94065224330773));
#457935=CARTESIAN_POINT('Ctrl Pts',(-1.78354733206521,7.77450652448868,
-2.50872974849562));
#457936=CARTESIAN_POINT('Ctrl Pts',(-2.32867154767716,7.82284784527782,
-1.80574130953711));
#457937=CARTESIAN_POINT('Ctrl Pts',(-2.92343855349618,7.87559146186954,
-1.03873386978253));
#457938=CARTESIAN_POINT('Ctrl Pts',(-3.10207417147801,7.92833507846125,
0.0509578026065476));
#457939=CARTESIAN_POINT('Ctrl Pts',(-2.78333121197043,7.98107869505296,
0.967719024035481));
#457940=CARTESIAN_POINT('Ctrl Pts',(-2.46458825246286,8.03382231164468,
1.88448024546441));
#457941=CARTESIAN_POINT('Ctrl Pts',(-1.64846671546588,8.08656592823639,
2.62831101593321));
#457942=CARTESIAN_POINT('Ctrl Pts',(-0.706155743875934,8.1393095448281,
2.86090142802836));
#457943=CARTESIAN_POINT('Ctrl Pts',(0.236155227714015,8.19205316141981,
3.09349184012353));
#457944=CARTESIAN_POINT('Ctrl Pts',(1.30465563389693,8.24479677801152,2.81484189384505));
#457945=CARTESIAN_POINT('Ctrl Pts',(2.01336880808209,8.29754039460323,2.15168749114821));
#457946=CARTESIAN_POINT('Ctrl Pts',(2.72208198226726,8.35028401119494,1.48853308845135));
#457947=CARTESIAN_POINT('Ctrl Pts',(3.07100792445466,8.40302762778665,0.440874229336113));
#457948=CARTESIAN_POINT('Ctrl Pts',(2.90144816786456,8.45577124437836,-0.514791879650031));
#457949=CARTESIAN_POINT('Ctrl Pts',(2.73188841127446,8.50851486097007,-1.47045798863617));
#457950=CARTESIAN_POINT('Ctrl Pts',(2.04384295590686,8.56125847756179,-2.33413134749321));
#457951=CARTESIAN_POINT('Ctrl Pts',(1.1502485919274,8.6140020941535,-2.71299498128419));
#457952=CARTESIAN_POINT('Ctrl Pts',(0.78982083202278,8.63527602373913,-2.86580813268824));
#457953=CARTESIAN_POINT('Ctrl Pts',(0.395952723327252,8.65654995332477,
-2.93974854079768));
#457954=CARTESIAN_POINT('Ctrl Pts',(0.00144847389154757,8.6778238829104,
-2.93797820450178));
#457955=CARTESIAN_POINT('Origin',(0.,3.,0.));
#457956=CARTESIAN_POINT('',(-0.00272715277824687,9.82217611708959,-2.94049646102293));
#457957=CARTESIAN_POINT('',(-0.00260485525275486,9.6778238829104,-2.94075152484336));
#457958=CARTESIAN_POINT('',(-3.60291088309151E-16,3.,-2.942));
#457959=CARTESIAN_POINT('Ctrl Pts',(-0.00272715277824687,9.82217611708959,
-2.94049646102293));
#457960=CARTESIAN_POINT('Ctrl Pts',(0.696291822549949,9.7843993284345,-2.93463308864337));
#457961=CARTESIAN_POINT('Ctrl Pts',(1.39921136012617,9.74662253977941,-2.68496045607899));
#457962=CARTESIAN_POINT('Ctrl Pts',(1.92551094701935,9.70884575112432,-2.23075084680181));
#457963=CARTESIAN_POINT('Ctrl Pts',(2.66032575292875,9.65610213453261,-1.5965874269644));
#457964=CARTESIAN_POINT('Ctrl Pts',(3.05084652446068,9.6033585179409,-0.56370992856744));
#457965=CARTESIAN_POINT('Ctrl Pts',(2.91972301055158,9.55061490134919,0.398002800710947));
#457966=CARTESIAN_POINT('Ctrl Pts',(2.78859949664248,9.49787128475748,1.35971552998933));
#457967=CARTESIAN_POINT('Ctrl Pts',(2.13583169729234,9.44512766816577,2.25026349014915));
#457968=CARTESIAN_POINT('Ctrl Pts',(1.25817372386208,9.39238405157406,2.66466092107898));
#457969=CARTESIAN_POINT('Ctrl Pts',(0.380515750431826,9.33964043498235,
3.07905835200882));
#457970=CARTESIAN_POINT('Ctrl Pts',(-0.722032397078542,9.28689681839064,
3.01730525370867));
#457971=CARTESIAN_POINT('Ctrl Pts',(-1.54793680036479,9.23415320179892,
2.50746011508263));
#457972=CARTESIAN_POINT('Ctrl Pts',(-2.37384120365104,9.18140958520721,
1.9976149764566));
#457973=CARTESIAN_POINT('Ctrl Pts',(-2.92310186271316,9.1286659686155,1.03967779750468));
#457974=CARTESIAN_POINT('Ctrl Pts',(-2.94594074597149,9.07592235202378,
0.0693531528026049));
#457975=CARTESIAN_POINT('Ctrl Pts',(-2.96877962922981,9.02317873543207,
-0.900971491899467));
#457976=CARTESIAN_POINT('Ctrl Pts',(-2.46519673668434,8.97043511884037,
-1.8836836023517));
#457977=CARTESIAN_POINT('Ctrl Pts',(-1.66421282102025,8.91769150224865,
-2.43183260818985));
#457978=CARTESIAN_POINT('Ctrl Pts',(-1.18070225832283,8.88585304052897,
-2.76272044385269));
#457979=CARTESIAN_POINT('Ctrl Pts',(-0.588822262923787,8.85401457880928,
-2.93525859858217));
#457980=CARTESIAN_POINT('Ctrl Pts',(0.00153914408188974,8.8221761170896,
-2.93808272452622));
#457981=CARTESIAN_POINT('Ctrl Pts',(0.00144847389154757,8.6778238829104,
-2.93797820450178));
#457982=CARTESIAN_POINT('Ctrl Pts',(-0.582126140395611,8.70929356991648,
-2.93535941567374));
#457983=CARTESIAN_POINT('Ctrl Pts',(-1.16709276553782,8.74076325692255,
-2.76706946101668));
#457984=CARTESIAN_POINT('Ctrl Pts',(-1.64726627821386,8.77223294392863,
-2.44334352869553));
#457985=CARTESIAN_POINT('Ctrl Pts',(-2.45204351178437,8.82497656052034,
-1.90077453359098));
#457986=CARTESIAN_POINT('Ctrl Pts',(-2.96245470633408,8.87772017711206,
-0.921582634656987));
#457987=CARTESIAN_POINT('Ctrl Pts',(-2.9463569331973,8.93046379370377,0.0488756892174912));
#457988=CARTESIAN_POINT('Ctrl Pts',(-2.93025916006052,8.98320741029548,
1.01933401309197));
#457989=CARTESIAN_POINT('Ctrl Pts',(-2.38765241923725,9.03595102688719,
1.98105876190693));
#457990=CARTESIAN_POINT('Ctrl Pts',(-1.56532023316149,9.0886946434789,2.49663613476619));
#457991=CARTESIAN_POINT('Ctrl Pts',(-0.74298804708572,9.14143826007061,
3.01221350762545));
#457992=CARTESIAN_POINT('Ctrl Pts',(0.359069584242541,9.19418187666233,
3.081643504529));
#457993=CARTESIAN_POINT('Ctrl Pts',(1.23960317803997,9.24692549325404,2.67335012297083));
#457994=CARTESIAN_POINT('Ctrl Pts',(2.12013677183739,9.29966910984575,2.26505674141266));
#457995=CARTESIAN_POINT('Ctrl Pts',(2.77914632810399,9.35241272643746,1.37903998139278));
#457996=CARTESIAN_POINT('Ctrl Pts',(2.91692065399873,9.40515634302917,0.418274624164282));
#457997=CARTESIAN_POINT('Ctrl Pts',(3.05469497989347,9.45789995962088,-0.542490733064212));
#457998=CARTESIAN_POINT('Ctrl Pts',(2.67123407541636,9.51064357621259,-1.57800468750131));
#457999=CARTESIAN_POINT('Ctrl Pts',(1.94090504693286,9.5633871928043,-2.21728545190643));
#458000=CARTESIAN_POINT('Ctrl Pts',(1.41271198706605,9.601532756173,-2.679630025237));
#458001=CARTESIAN_POINT('Ctrl Pts',(0.703087445768586,9.6396783195417,-2.93472241918262));
#458002=CARTESIAN_POINT('Ctrl Pts',(-0.00260485525275486,9.6778238829104,
-2.94075152484336));
#458003=CARTESIAN_POINT('Origin',(0.,2.65141010809498,0.));
#458004=CARTESIAN_POINT('',(-0.00219854677154521,10.151410108095,-2.37053789307653));
#458005=CARTESIAN_POINT('',(0.000181708292718678,10.348589891905,-2.37522148111239));
#458006=CARTESIAN_POINT('',(-5.32714559963614E-14,2.65141010809498,-2.37175));
#458007=CARTESIAN_POINT('',(-1.9335277545108,10.5,1.37997672390729));
#458008=CARTESIAN_POINT('Ctrl Pts',(-0.00219854677154546,10.151410108095,
-2.37053789307653));
#458009=CARTESIAN_POINT('Ctrl Pts',(-0.225463181207916,10.1663769360316,
-2.37241063721809));
#458010=CARTESIAN_POINT('Ctrl Pts',(-1.23328706850035,10.2340873805599,
-2.24130665952044));
#458011=CARTESIAN_POINT('Ctrl Pts',(-2.62758348517719,10.3502840111949,
-0.863551348926038));
#458012=CARTESIAN_POINT('Ctrl Pts',(-2.34830127392877,10.4515138138933,
0.791573397958322));
#458013=CARTESIAN_POINT('Ctrl Pts',(-1.9335277545108,10.5,1.37997672390729));
#458014=CARTESIAN_POINT('',(-1.93106208855764,10.5,-1.37702479013103));
#458015=CARTESIAN_POINT('Origin',(0.,10.5,0.));
#458016=CARTESIAN_POINT('Ctrl Pts',(0.000181708292718774,10.348589891905,
-2.37522148111239));
#458017=CARTESIAN_POINT('Ctrl Pts',(-0.747222935425508,10.3990599279367,
-2.37281386287285));
#458018=CARTESIAN_POINT('Ctrl Pts',(-1.49439019245277,10.4495299639683,
-1.98938888825773));
#458019=CARTESIAN_POINT('Ctrl Pts',(-1.93106208855764,10.5,-1.37702479013103));
#458020=CARTESIAN_POINT('Origin',(0.,2.65141010809498,0.));
#458021=CARTESIAN_POINT('',(0.00124081066488494,9.15141010809498,-2.36859201288072));
#458022=CARTESIAN_POINT('',(-0.00209995426439569,9.34858989190501,-2.37074351769111));
#458023=CARTESIAN_POINT('',(-5.32714559963614E-14,2.65141010809498,-2.37175));
#458024=CARTESIAN_POINT('Ctrl Pts',(0.00124081066488493,9.15141010809498,
-2.36859201288071));
#458025=CARTESIAN_POINT('Ctrl Pts',(-0.47469041539415,9.18324856981467,
-2.36631528932265));
#458026=CARTESIAN_POINT('Ctrl Pts',(-1.74230193799465,9.26783064812606,
-1.99679553071707));
#458027=CARTESIAN_POINT('Ctrl Pts',(-2.79931196839583,9.40515634302917,
0.0658967750008794));
#458028=CARTESIAN_POINT('Ctrl Pts',(-1.47092077043804,9.56338719280431,
2.3826753312679));
#458029=CARTESIAN_POINT('Ctrl Pts',(1.19560054382884,9.72161804257944,2.53202568228086));
#458030=CARTESIAN_POINT('Ctrl Pts',(2.77432456977243,9.87984889235458,0.378228478498683));
#458031=CARTESIAN_POINT('Ctrl Pts',(1.91918379943006,10.0231129141931,-1.88350949816164));
#458032=CARTESIAN_POINT('Ctrl Pts',(0.561329072104955,10.1136333194399,
-2.36581102243029));
#458033=CARTESIAN_POINT('Ctrl Pts',(-0.00219854677154546,10.151410108095,
-2.37053789307653));
#458034=CARTESIAN_POINT('Ctrl Pts',(-0.00209995426439569,9.34858989190501,
-2.37074351769111));
#458035=CARTESIAN_POINT('Ctrl Pts',(-0.219817048625936,9.36318794512803,
-2.37260359093287));
#458036=CARTESIAN_POINT('Ctrl Pts',(-1.22201699419431,9.43052961494275,
-2.24553205649247));
#458037=CARTESIAN_POINT('Ctrl Pts',(-2.67372165333505,9.5506149013492,-0.831355243680753));
#458038=CARTESIAN_POINT('Ctrl Pts',(-2.15489783705297,9.70884575112431,
1.78837383802425));
#458039=CARTESIAN_POINT('Ctrl Pts',(0.325001931376548,9.86707660089947,
2.78113441285149));
#458040=CARTESIAN_POINT('Ctrl Pts',(2.50754674652922,10.0253074506746,1.24442120982437));
#458041=CARTESIAN_POINT('Ctrl Pts',(2.41246714519292,10.1835383004498,-1.42496845308012));
#458042=CARTESIAN_POINT('Ctrl Pts',(0.848605545785018,10.2912991141932,
-2.35924393469853));
#458043=CARTESIAN_POINT('Ctrl Pts',(0.0338508871176543,10.346316311345,
-2.37532993980305));
#458044=CARTESIAN_POINT('Ctrl Pts',(0.000181708292718774,10.348589891905,
-2.37522148111239));
#458045=CARTESIAN_POINT('Origin',(0.,2.65141010809498,0.));
#458046=CARTESIAN_POINT('',(0.00104640920538959,8.15141010809498,-2.3750094497789));
#458047=CARTESIAN_POINT('',(0.00116771514349009,8.34858989190502,-2.36850775204864));
#458048=CARTESIAN_POINT('',(-5.32714559963614E-14,2.65141010809498,-2.37175));
#458049=CARTESIAN_POINT('Ctrl Pts',(0.00104640920538944,8.15141010809498,
-2.3750094497789));
#458050=CARTESIAN_POINT('Ctrl Pts',(-0.722047949186556,8.20012020359773,
-2.37100113623637));
#458051=CARTESIAN_POINT('Ctrl Pts',(-2.23519527081121,8.30157391569219,
-1.63319248740048));
#458052=CARTESIAN_POINT('Ctrl Pts',(-2.63835079772906,8.45577124437837,
0.937918609717529));
#458053=CARTESIAN_POINT('Ctrl Pts',(-0.652098439920106,8.61400209415349,
2.72311552626202));
#458054=CARTESIAN_POINT('Ctrl Pts',(1.92733241411022,8.77223294392864,2.03125107188904));
#458055=CARTESIAN_POINT('Ctrl Pts',(2.75357614178819,8.93046379370376,-0.508323077697843));
#458056=CARTESIAN_POINT('Ctrl Pts',(1.4128028681317,9.05685618175922,-2.16754712278337));
#458057=CARTESIAN_POINT('Ctrl Pts',(0.313737566217802,9.13050495322295,
-2.37008691106396));
#458058=CARTESIAN_POINT('Ctrl Pts',(0.00124081066488493,9.15141010809498,
-2.36859201288071));
#458059=CARTESIAN_POINT('Ctrl Pts',(0.00116771514349023,8.34858989190502,
-2.36850775204864));
#458060=CARTESIAN_POINT('Ctrl Pts',(-0.469292207166344,8.38005957891109,
-2.36639656496403));
#458061=CARTESIAN_POINT('Ctrl Pts',(-1.7312522681202,8.46427288250889,-2.00334131991425));
#458062=CARTESIAN_POINT('Ctrl Pts',(-2.79971777716557,8.60122980269838,
0.0464428186774438));
#458063=CARTESIAN_POINT('Ctrl Pts',(-1.48741913248753,8.75946065247352,
2.37238164226875));
#458064=CARTESIAN_POINT('Ctrl Pts',(1.17791586455814,8.91769150224865,2.54029863257058));
#458065=CARTESIAN_POINT('Ctrl Pts',(2.77173562840107,9.07592235202379,0.397460171750882));
#458066=CARTESIAN_POINT('Ctrl Pts',(1.92989274718027,9.21955514857591,-1.87588775177829));
#458067=CARTESIAN_POINT('Ctrl Pts',(0.566807494731995,9.31044432853632,
-2.36588303796615));
#458068=CARTESIAN_POINT('Ctrl Pts',(-0.00209995426439569,9.34858989190501,
-2.37074351769111));
#458069=CARTESIAN_POINT('Origin',(0.,2.65141010809498,0.));
#458070=CARTESIAN_POINT('',(-0.00213047795326273,7.15141010809498,-2.37151035100404));
#458071=CARTESIAN_POINT('',(0.00113115772178901,7.34858989190502,-2.37490814099156));
#458072=CARTESIAN_POINT('',(-5.32714559963614E-14,2.65141010809498,-2.37175));
#458073=CARTESIAN_POINT('Ctrl Pts',(-0.00213047795326283,7.15141010809498,
-2.37151035100404));
#458074=CARTESIAN_POINT('Ctrl Pts',(-0.19344123445082,7.16424822078908,
-2.37323299754693));
#458075=CARTESIAN_POINT('Ctrl Pts',(-1.16879840192096,7.22982995007489,
-2.26482247383448));
#458076=CARTESIAN_POINT('Ctrl Pts',(-2.64480699428301,7.34815529595243,
-0.91955640806139));
#458077=CARTESIAN_POINT('Ctrl Pts',(-2.21277542651634,7.50638614572755,
1.71587099220952));
#458078=CARTESIAN_POINT('Ctrl Pts',(0.232089844388488,7.6646169955027,2.79046996769084));
#458079=CARTESIAN_POINT('Ctrl Pts',(2.46583642488247,7.82284784527782,1.32674001817368));
#458080=CARTESIAN_POINT('Ctrl Pts',(2.45655437571063,7.98107869505296,-1.3438484378054));
#458081=CARTESIAN_POINT('Ctrl Pts',(0.903443717085102,8.09059944932534,
-2.34620916961456));
#458082=CARTESIAN_POINT('Ctrl Pts',(0.0609234493503653,8.14737658700602,
-2.37534136489913));
#458083=CARTESIAN_POINT('Ctrl Pts',(0.00104640920538944,8.15141010809498,
-2.3750094497789));
#458084=CARTESIAN_POINT('Ctrl Pts',(0.00113115772178904,7.34858989190502,
-2.37490814099156));
#458085=CARTESIAN_POINT('Ctrl Pts',(-0.716570266697475,7.39693121269416,
-2.37066347996774));
#458086=CARTESIAN_POINT('Ctrl Pts',(-2.22479576229617,7.49801615007502,
-1.64254844637319));
#458087=CARTESIAN_POINT('Ctrl Pts',(-2.64480742459258,7.65184470404756,
0.919556557552984));
#458088=CARTESIAN_POINT('Ctrl Pts',(-0.671011107081431,7.81007555382272,
2.71851709106015));
#458089=CARTESIAN_POINT('Ctrl Pts',(1.9131654786062,7.96830640359783,2.04460001755302));
#458090=CARTESIAN_POINT('Ctrl Pts',(2.75704559762349,8.12653725337299,-0.489171123616138));
#458091=CARTESIAN_POINT('Ctrl Pts',(1.42395495486713,8.25329841614203,-2.16254148615291));
#458092=CARTESIAN_POINT('Ctrl Pts',(0.31920491895014,8.32731596231938,-2.36993494277258));
#458093=CARTESIAN_POINT('Ctrl Pts',(0.00116771514349023,8.34858989190502,
-2.36850775204864));
#458094=CARTESIAN_POINT('Origin',(0.,2.65141010809498,0.));
#458095=CARTESIAN_POINT('',(0.000791481804837191,6.15141010809498,-2.36817783754632));
#458096=CARTESIAN_POINT('',(-0.00212971970566161,6.34858989190502,-2.37167445573758));
#458097=CARTESIAN_POINT('',(-5.32714559963614E-14,2.65141010809498,-2.37175));
#458098=CARTESIAN_POINT('Ctrl Pts',(0.000791481804836985,6.15141010809498,
-2.36817783754632));
#458099=CARTESIAN_POINT('Ctrl Pts',(-0.44351330913558,6.18111985457215,
-2.36684216047238));
#458100=CARTESIAN_POINT('Ctrl Pts',(-1.67845190049489,6.26357321764102,
-2.03379137829988));
#458101=CARTESIAN_POINT('Ctrl Pts',(-2.79971730451761,6.39877019730161,
-0.0464428113915518));
#458102=CARTESIAN_POINT('Ctrl Pts',(-1.56528406825032,6.55700104707675,
2.32174006667672));
#458103=CARTESIAN_POINT('Ctrl Pts',(1.09300211259457,6.71523189685188,2.5779714751291));
#458104=CARTESIAN_POINT('Ctrl Pts',(2.75704514653133,6.87346274662702,0.48917104403278));
#458105=CARTESIAN_POINT('Ctrl Pts',(1.98163365229979,7.01885548370805,-1.83902135321545));
#458106=CARTESIAN_POINT('Ctrl Pts',(0.592532641227426,7.11150460419737,
-2.36615574164909));
#458107=CARTESIAN_POINT('Ctrl Pts',(-0.00213047795326283,7.15141010809498,
-2.37151035100404));
#458108=CARTESIAN_POINT('Ctrl Pts',(-0.00212971970566156,6.34858989190502,
-2.37167445573758));
#458109=CARTESIAN_POINT('Ctrl Pts',(-0.187912373596309,6.36105922988551,
-2.37335759916362));
#458110=CARTESIAN_POINT('Ctrl Pts',(-1.15765668108355,6.42627218445772,
-2.26873220062386));
#458111=CARTESIAN_POINT('Ctrl Pts',(-2.6383512294758,6.54422875562164,-0.937918762728673));
#458112=CARTESIAN_POINT('Ctrl Pts',(-2.22464981695575,6.70245960539676,
1.70044834447479));
#458113=CARTESIAN_POINT('Ctrl Pts',(0.212687290880062,6.86069045517191,
2.79201633170562));
#458114=CARTESIAN_POINT('Ctrl Pts',(2.45655477541136,7.01892130494703,1.34384865633091));
#458115=CARTESIAN_POINT('Ctrl Pts',(2.46583682546838,7.17715215472218,-1.32674023387393));
#458116=CARTESIAN_POINT('Ctrl Pts',(0.914524930039516,7.28704168370816,
-2.34328423318916));
#458117=CARTESIAN_POINT('Ctrl Pts',(0.0664900249733059,7.34418759610245,
-2.37529468925097));
#458118=CARTESIAN_POINT('Ctrl Pts',(0.00113115772178904,7.34858989190502,
-2.37490814099156));
#458119=CARTESIAN_POINT('Origin',(0.,2.65141010809498,0.));
#458120=CARTESIAN_POINT('',(0.00164853063274011,5.15141010809498,-2.37430728468226));
#458121=CARTESIAN_POINT('',(0.000720435901828409,5.34858989190502,-2.36812053819694));
#458122=CARTESIAN_POINT('',(-5.32714559963614E-14,2.65141010809498,-2.37175));
#458123=CARTESIAN_POINT('Ctrl Pts',(0.00164853063274016,5.15141010809498,
-2.37430728468225));
#458124=CARTESIAN_POINT('Ctrl Pts',(-0.690326622956052,5.19799148835521,
-2.36918731762371));
#458125=CARTESIAN_POINT('Ctrl Pts',(-2.17510366416648,5.29731648520715,
-1.68634907433112));
#458126=CARTESIAN_POINT('Ctrl Pts',(-2.67372071192838,5.44938509865081,
0.831355011409453));
#458127=CARTESIAN_POINT('Ctrl Pts',(-0.760877475065064,5.60761594842594,
2.69475048642212));
#458128=CARTESIAN_POINT('Ctrl Pts',(1.84433230531922,5.76584679820107,2.10693806142813));
#458129=CARTESIAN_POINT('Ctrl Pts',(2.77173507946231,5.92407764797621,-0.397460099428512));
#458130=CARTESIAN_POINT('Ctrl Pts',(1.47717449489275,6.05259875127418,-2.13795457432145));
#458131=CARTESIAN_POINT('Ctrl Pts',(0.34525954563222,6.12837623798044,-2.36921338365101));
#458132=CARTESIAN_POINT('Ctrl Pts',(0.000791481804836985,6.15141010809498,
-2.36817783754632));
#458133=CARTESIAN_POINT('Ctrl Pts',(0.000720435901828305,5.34858989190502,
-2.36812053819695));
#458134=CARTESIAN_POINT('Ctrl Pts',(-0.438099836996933,5.37793086366857,
-2.36694555350675));
#458135=CARTESIAN_POINT('Ctrl Pts',(-1.66739250361399,5.46001545202384,
-2.04001968313778));
#458136=CARTESIAN_POINT('Ctrl Pts',(-2.79931252173984,5.59484365697083,
-0.0658967943579637));
#458137=CARTESIAN_POINT('Ctrl Pts',(-1.58139300728764,5.75307450674595,
2.3108005286306));
#458138=CARTESIAN_POINT('Ctrl Pts',(1.07505989907631,5.9113053565211,2.58550895292624));
#458139=CARTESIAN_POINT('Ctrl Pts',(2.75357660673821,6.06953620629623,0.508323162965956));
#458140=CARTESIAN_POINT('Ctrl Pts',(1.99244463689641,6.21529771809087,-1.83112093830349));
#458141=CARTESIAN_POINT('Ctrl Pts',(0.597923176095928,6.3083156132938,-2.36623812965602));
#458142=CARTESIAN_POINT('Ctrl Pts',(-0.00212971970566156,6.34858989190502,
-2.37167445573758));
#458143=CARTESIAN_POINT('Ctrl Pts',(2.13201587949045,4.17076600899461,-1.03908919352506));
#458144=CARTESIAN_POINT('Ctrl Pts',(1.78766388536965,4.22350962558633,-1.74563481460801));
#458145=CARTESIAN_POINT('Ctrl Pts',(0.347467740692633,4.32899685876975,
-2.77757630076507));
#458146=CARTESIAN_POINT('Ctrl Pts',(-2.14391193590671,4.48722770854489,
-1.80393304476234));
#458147=CARTESIAN_POINT('Ctrl Pts',(-2.67867315956894,4.64545855832002,
0.813071299269003));
#458148=CARTESIAN_POINT('Ctrl Pts',(-0.779984807125968,4.80368940809515,
2.68923010885977));
#458149=CARTESIAN_POINT('Ctrl Pts',(1.82984645434041,4.96192025787029,2.11979424147793));
#458150=CARTESIAN_POINT('Ctrl Pts',(2.77432553661561,5.12015110764542,-0.378228552056395));
#458151=CARTESIAN_POINT('Ctrl Pts',(1.19560043789348,5.27838195742056,-2.53202610033261));
#458152=CARTESIAN_POINT('Ctrl Pts',(-1.47092083681034,5.43661280719569,
-2.38267570849546));
#458153=CARTESIAN_POINT('Ctrl Pts',(-2.79931252173984,5.59484365697083,
-0.0658967943579637));
#458154=CARTESIAN_POINT('Ctrl Pts',(-1.58139300728764,5.75307450674595,
2.3108005286306));
#458155=CARTESIAN_POINT('Ctrl Pts',(1.07505989907631,5.9113053565211,2.58550895292624));
#458156=CARTESIAN_POINT('Ctrl Pts',(2.75357660673821,6.06953620629623,0.508323162965956));
#458157=CARTESIAN_POINT('Ctrl Pts',(1.92733271768767,6.22776705607136,-2.03125140365088));
#458158=CARTESIAN_POINT('Ctrl Pts',(-0.652098540560857,6.3859979058465,
-2.72311596787379));
#458159=CARTESIAN_POINT('Ctrl Pts',(-2.6383512294758,6.54422875562164,-0.937918762728673));
#458160=CARTESIAN_POINT('Ctrl Pts',(-2.22464981695575,6.70245960539676,
1.70044834447479));
#458161=CARTESIAN_POINT('Ctrl Pts',(0.212687290880062,6.86069045517191,
2.79201633170562));
#458162=CARTESIAN_POINT('Ctrl Pts',(2.45655477541136,7.01892130494703,1.34384865633091));
#458163=CARTESIAN_POINT('Ctrl Pts',(2.46583682546838,7.17715215472218,-1.32674023387393));
#458164=CARTESIAN_POINT('Ctrl Pts',(0.232089882106114,7.3353830044973,-2.79047042117834));
#458165=CARTESIAN_POINT('Ctrl Pts',(-2.21277578596402,7.49361385427245,
-1.71587127112355));
#458166=CARTESIAN_POINT('Ctrl Pts',(-2.64480742459258,7.65184470404756,
0.919556557552984));
#458167=CARTESIAN_POINT('Ctrl Pts',(-0.671011107081431,7.81007555382272,
2.71851709106015));
#458168=CARTESIAN_POINT('Ctrl Pts',(1.9131654786062,7.96830640359783,2.04460001755302));
#458169=CARTESIAN_POINT('Ctrl Pts',(2.75704559762349,8.12653725337299,-0.489171123616138));
#458170=CARTESIAN_POINT('Ctrl Pts',(1.0930022848076,8.2847681031481,-2.57797189404698));
#458171=CARTESIAN_POINT('Ctrl Pts',(-1.56528431284886,8.44299895292325,
-2.32174044403164));
#458172=CARTESIAN_POINT('Ctrl Pts',(-2.79971777716557,8.60122980269838,
0.0464428186774438));
#458173=CARTESIAN_POINT('Ctrl Pts',(-1.48741913248753,8.75946065247352,
2.37238164226875));
#458174=CARTESIAN_POINT('Ctrl Pts',(1.17791586455814,8.91769150224865,2.54029863257058));
#458175=CARTESIAN_POINT('Ctrl Pts',(2.77173562840107,9.07592235202379,0.397460171750882));
#458176=CARTESIAN_POINT('Ctrl Pts',(1.84433243309827,9.23415320179892,-2.10693842250765));
#458177=CARTESIAN_POINT('Ctrl Pts',(-0.760877301522333,9.39238405157405,
-2.69475088122905));
#458178=CARTESIAN_POINT('Ctrl Pts',(-2.67372165333505,9.5506149013492,-0.831355243680753));
#458179=CARTESIAN_POINT('Ctrl Pts',(-2.15489783705297,9.70884575112431,
1.78837383802425));
#458180=CARTESIAN_POINT('Ctrl Pts',(0.325001931376548,9.86707660089947,
2.78113441285149));
#458181=CARTESIAN_POINT('Ctrl Pts',(2.50754674652922,10.0253074506746,1.24442120982437));
#458182=CARTESIAN_POINT('Ctrl Pts',(2.41246714519292,10.1835383004498,-1.42496845308012));
#458183=CARTESIAN_POINT('Ctrl Pts',(0.116167208241161,10.3417691502248,
-2.79681410128083));
#458184=CARTESIAN_POINT('Ctrl Pts',(-1.47471894170346,10.4472563834083,
-2.01697474352246));
#458185=CARTESIAN_POINT('Ctrl Pts',(-1.93106208855764,10.5,-1.37702479013103));
#458186=CARTESIAN_POINT('Ctrl Pts',(2.3028857793927,4.28051067266308,-1.12236674703444));
#458187=CARTESIAN_POINT('Ctrl Pts',(1.93093577752131,4.33325428925479,-1.88553829699165));
#458188=CARTESIAN_POINT('Ctrl Pts',(0.375315459202878,4.43874152243821,
-3.00018448537015));
#458189=CARTESIAN_POINT('Ctrl Pts',(-2.31573524238938,4.59697237221334,
-1.94850882478072));
#458190=CARTESIAN_POINT('Ctrl Pts',(-2.89335477570951,4.75520322198849,
0.878234703001565));
#458191=CARTESIAN_POINT('Ctrl Pts',(-0.842496501903189,4.91343407176361,
2.90475780916226));
#458192=CARTESIAN_POINT('Ctrl Pts',(1.97649905833712,5.07166492153876,2.28968464114102));
#458193=CARTESIAN_POINT('Ctrl Pts',(2.99667318950976,5.22989577131387,-0.408541588395264));
#458194=CARTESIAN_POINT('Ctrl Pts',(1.29142154744111,5.38812662108903,-2.73495472317997));
#458195=CARTESIAN_POINT('Ctrl Pts',(-1.58880743351335,5.54635747086414,
-2.57363468010849));
#458196=CARTESIAN_POINT('Ctrl Pts',(-3.02366275054728,5.7045883206393,-0.0711780770933066));
#458197=CARTESIAN_POINT('Ctrl Pts',(-1.7081333695245,5.86281917041441,2.49599908123966));
#458198=CARTESIAN_POINT('Ctrl Pts',(1.16122031613098,6.02105002018957,2.79272394613185));
#458199=CARTESIAN_POINT('Ctrl Pts',(2.97426134163754,6.17928086996468,0.54906260060783));
#458200=CARTESIAN_POINT('Ctrl Pts',(2.08179833481447,6.33751171973983,-2.19404555887126));
#458201=CARTESIAN_POINT('Ctrl Pts',(-0.70436082126144,6.49574256951496,
-2.94135944219726));
#458202=CARTESIAN_POINT('Ctrl Pts',(-2.84980125422665,6.6539734192901,-1.01308803639383));
#458203=CARTESIAN_POINT('Ctrl Pts',(-2.40294384149727,6.81220426906522,
1.83673036807715));
#458204=CARTESIAN_POINT('Ctrl Pts',(0.229733062655383,6.97043511884037,
3.01578180911754));
#458205=CARTESIAN_POINT('Ctrl Pts',(2.6534347670741,7.12866596861549,1.45155108369084));
#458206=CARTESIAN_POINT('Ctrl Pts',(2.66346072480057,7.28689681839065,-1.43307151083069));
#458207=CARTESIAN_POINT('Ctrl Pts',(0.250690669888841,7.44512766816575,
-3.01411200196285));
#458208=CARTESIAN_POINT('Ctrl Pts',(-2.39011816914746,7.60335851794091,
-1.8533893614729));
#458209=CARTESIAN_POINT('Ctrl Pts',(-2.85677487954834,7.76158936771603,
0.993254196700526));
#458210=CARTESIAN_POINT('Ctrl Pts',(-0.724789130877252,7.91982021749118,
2.93639198950744));
#458211=CARTESIAN_POINT('Ctrl Pts',(2.06649566576409,8.0780510672663,2.2084639942242));
#458212=CARTESIAN_POINT('Ctrl Pts',(2.97800835396301,8.23628191704144,-0.528375625670466));
#458213=CARTESIAN_POINT('Ctrl Pts',(1.18060069005149,8.39451276681658,-2.78458283148141));
#458214=CARTESIAN_POINT('Ctrl Pts',(-1.69073364764413,8.55274361659171,
-2.50781577352942));
#458215=CARTESIAN_POINT('Ctrl Pts',(-3.02410048507164,8.71097446636685,
0.0501649672106313));
#458216=CARTESIAN_POINT('Ctrl Pts',(-1.60662798112968,8.86920531614197,
2.5625155984198));
#458217=CARTESIAN_POINT('Ctrl Pts',(1.27231964822903,9.02743616591713,2.74389025552457));
#458218=CARTESIAN_POINT('Ctrl Pts',(2.99387571372424,9.18566701569223,0.429314521624885));
#458219=CARTESIAN_POINT('Ctrl Pts',(1.99214601237859,9.3438978654674,-2.27579849565125));
#458220=CARTESIAN_POINT('Ctrl Pts',(-0.821857629858379,9.5021287152425,
-2.91072104250531));
#458221=CARTESIAN_POINT('Ctrl Pts',(-2.88800643219936,9.66035956501767,
-0.897984009740833));
#458222=CARTESIAN_POINT('Ctrl Pts',(-2.32760160594085,9.81859041479278,
1.93170262916065));
#458223=CARTESIAN_POINT('Ctrl Pts',(0.35104913300227,9.97682126456792,3.004027761494));
#458224=CARTESIAN_POINT('Ctrl Pts',(2.7085134774534,10.1350521143431,1.34415504839679));
#458225=CARTESIAN_POINT('Ctrl Pts',(2.60581374433508,10.2932829641182,-1.53917220704083));
#458226=CARTESIAN_POINT('Ctrl Pts',(0.125477401206913,10.4515138138933,
-3.02096409478147));
#458227=CARTESIAN_POINT('Ctrl Pts',(-1.59290993660967,10.5570010470767,
-2.17862469925046));
#458228=CARTESIAN_POINT('Ctrl Pts',(-2.08582659521587,10.6097446636685,
-1.48738611075536));
#458229=CARTESIAN_POINT('Ctrl Pts',(2.47375567929494,4.39025533633154,-1.20564430054382));
#458230=CARTESIAN_POINT('Ctrl Pts',(2.07420766967296,4.44299895292325,-2.02544177937529));
#458231=CARTESIAN_POINT('Ctrl Pts',(0.403163177713119,4.54848618610666,
-3.22279266997523));
#458232=CARTESIAN_POINT('Ctrl Pts',(-2.48755854887204,4.70671703588182,
-2.0930846047991));
#458233=CARTESIAN_POINT('Ctrl Pts',(-3.10803639185008,4.86494788565693,
0.943398106734127));
#458234=CARTESIAN_POINT('Ctrl Pts',(-0.905008196680407,5.02317873543208,
3.12028550946475));
#458235=CARTESIAN_POINT('Ctrl Pts',(2.12315166233383,5.18140958520721,2.45957504080411));
#458236=CARTESIAN_POINT('Ctrl Pts',(3.2190208424039,5.33964043498234,-0.43885462473413));
#458237=CARTESIAN_POINT('Ctrl Pts',(1.38724265698875,5.49787128475748,-2.93788334602733));
#458238=CARTESIAN_POINT('Ctrl Pts',(-1.70669403021636,5.65610213453261,
-2.76459365172151));
#458239=CARTESIAN_POINT('Ctrl Pts',(-3.24801297935472,5.81433298430775,
-0.0764593598286509));
#458240=CARTESIAN_POINT('Ctrl Pts',(-1.83487373176136,5.97256383408288,
2.68119763384871));
#458241=CARTESIAN_POINT('Ctrl Pts',(1.24738073318565,6.13079468385802,2.99993893933746));
#458242=CARTESIAN_POINT('Ctrl Pts',(3.19494607653687,6.28902553363315,0.589802038249709));
#458243=CARTESIAN_POINT('Ctrl Pts',(2.23626395194126,6.44725638340828,-2.35683971409166));
#458244=CARTESIAN_POINT('Ctrl Pts',(-0.756623101962018,6.60548723318342,
-3.15960291652072));
#458245=CARTESIAN_POINT('Ctrl Pts',(-3.06125127897751,6.76371808295856,
-1.088257310059));
#458246=CARTESIAN_POINT('Ctrl Pts',(-2.58123786603879,6.92194893273369,
1.97301239167952));
#458247=CARTESIAN_POINT('Ctrl Pts',(0.246778834430699,7.08017978250883,
3.23954728652945));
#458248=CARTESIAN_POINT('Ctrl Pts',(2.85031475873684,7.23841063228396,1.55925351105077));
#458249=CARTESIAN_POINT('Ctrl Pts',(2.86108462413276,7.3966414820591,-1.53940278778745));
#458250=CARTESIAN_POINT('Ctrl Pts',(0.269291457671566,7.55487233183422,
-3.23775358274735));
#458251=CARTESIAN_POINT('Ctrl Pts',(-2.5674605523309,7.71310318160937,-1.99090745182226));
#458252=CARTESIAN_POINT('Ctrl Pts',(-3.06874233450409,7.87133403138449,
1.06695183584807));
#458253=CARTESIAN_POINT('Ctrl Pts',(-0.778567154673073,8.02956488115964,
3.15426688795472));
#458254=CARTESIAN_POINT('Ctrl Pts',(2.21982585292198,8.18779573093476,2.37232797089539));
#458255=CARTESIAN_POINT('Ctrl Pts',(3.19897111030254,8.3460265807099,-0.567580127724795));
#458256=CARTESIAN_POINT('Ctrl Pts',(1.26819909529537,8.50425743048504,-2.99119376891583));
#458257=CARTESIAN_POINT('Ctrl Pts',(-1.8161829824394,8.66248828026016,-2.69389110302719));
#458258=CARTESIAN_POINT('Ctrl Pts',(-3.24848319297771,8.82071913003531,
0.0538871157438198));
#458259=CARTESIAN_POINT('Ctrl Pts',(-1.72583682977183,8.97894997981043,
2.75264955457085));
#458260=CARTESIAN_POINT('Ctrl Pts',(1.36672343189991,9.13718082958558,2.94748187847856));
#458261=CARTESIAN_POINT('Ctrl Pts',(3.21601579904741,9.29541167936071,0.461168871498884));
#458262=CARTESIAN_POINT('Ctrl Pts',(2.13995959165892,9.45364252913584,-2.44465856879484));
#458263=CARTESIAN_POINT('Ctrl Pts',(-0.882837958194431,9.61187337891097,
-3.12669120378156));
#458264=CARTESIAN_POINT('Ctrl Pts',(-3.10229121106367,9.77010422868613,
-0.964612775800914));
#458265=CARTESIAN_POINT('Ctrl Pts',(-2.50030537482873,9.92833507846123,
2.07503142029706));
#458266=CARTESIAN_POINT('Ctrl Pts',(0.377096334627995,10.0865659282364,
3.2269211101365));
#458267=CARTESIAN_POINT('Ctrl Pts',(2.90948020837758,10.2447967780115,1.44388888696921));
#458268=CARTESIAN_POINT('Ctrl Pts',(2.79916034347724,10.4030276277867,-1.65337596100153));
#458269=CARTESIAN_POINT('Ctrl Pts',(0.134787594172663,10.5612584775618,
-3.2451140882821));
#458270=CARTESIAN_POINT('Ctrl Pts',(-1.71110093151587,10.6667457107452,
-2.34027465497847));
#458271=CARTESIAN_POINT('Ctrl Pts',(-2.2405911018741,10.7194893273369,-1.59774743137968));
#458272=CARTESIAN_POINT('Ctrl Pts',(2.64462557919718,4.5,-1.28892185405321));
#458273=CARTESIAN_POINT('Ctrl Pts',(2.21747956182462,4.55274361659171,-2.16534526175893));
#458274=CARTESIAN_POINT('Ctrl Pts',(0.431010896223362,4.65823084977513,
-3.4454008545803));
#458275=CARTESIAN_POINT('Ctrl Pts',(-2.6593818553547,4.81646169955027,-2.23766038481748));
#458276=CARTESIAN_POINT('Ctrl Pts',(-3.32271800799066,4.9746925493254,1.00856151046669));
#458277=CARTESIAN_POINT('Ctrl Pts',(-0.967519891457628,5.13292339910054,
3.33581320976724));
#458278=CARTESIAN_POINT('Ctrl Pts',(2.26980426633054,5.29115424887568,2.62946544046721));
#458279=CARTESIAN_POINT('Ctrl Pts',(3.44136849529805,5.4493850986508,-0.469167661072997));
#458280=CARTESIAN_POINT('Ctrl Pts',(1.48306376653638,5.60761594842594,-3.14081196887468));
#458281=CARTESIAN_POINT('Ctrl Pts',(-1.82458062691936,5.76584679820108,
-2.95555262333453));
#458282=CARTESIAN_POINT('Ctrl Pts',(-3.47236320816217,5.92407764797621,
-0.0817406425639971));
#458283=CARTESIAN_POINT('Ctrl Pts',(-1.96161409399822,6.08230849775135,
2.86639618645777));
#458284=CARTESIAN_POINT('Ctrl Pts',(1.33354115024032,6.24053934752648,3.20715393254307));
#458285=CARTESIAN_POINT('Ctrl Pts',(3.4156308114362,6.39877019730162,0.630541475891585));
#458286=CARTESIAN_POINT('Ctrl Pts',(2.39072956906805,6.55700104707675,-2.51963386931204));
#458287=CARTESIAN_POINT('Ctrl Pts',(-0.808885382662597,6.71523189685188,
-3.37784639084419));
#458288=CARTESIAN_POINT('Ctrl Pts',(-3.27270130372837,6.87346274662702,
-1.16342658372416));
#458289=CARTESIAN_POINT('Ctrl Pts',(-2.75953189058031,7.03169359640215,
2.10929441528188));
#458290=CARTESIAN_POINT('Ctrl Pts',(0.263824606206016,7.18992444617729,
3.46331276394136));
#458291=CARTESIAN_POINT('Ctrl Pts',(3.04719475039958,7.34815529595242,1.6669559384107));
#458292=CARTESIAN_POINT('Ctrl Pts',(3.05870852346495,7.50638614572756,-1.64573406474421));
#458293=CARTESIAN_POINT('Ctrl Pts',(0.287892245454292,7.66461699550269,
-3.46139516353185));
#458294=CARTESIAN_POINT('Ctrl Pts',(-2.74480293551434,7.82284784527782,
-2.12842554217161));
#458295=CARTESIAN_POINT('Ctrl Pts',(-3.28070978945985,7.98107869505297,
1.14064947499561));
#458296=CARTESIAN_POINT('Ctrl Pts',(-0.832345178468896,8.1393095448281,
3.372141786402));
#458297=CARTESIAN_POINT('Ctrl Pts',(2.37315604007987,8.29754039460323,2.53619194756657));
#458298=CARTESIAN_POINT('Ctrl Pts',(3.41993386664206,8.45577124437836,-0.606784629779126));
#458299=CARTESIAN_POINT('Ctrl Pts',(1.35579750053926,8.6140020941535,-3.19780470635025));
#458300=CARTESIAN_POINT('Ctrl Pts',(-1.94163231723467,8.77223294392863,
-2.87996643252497));
#458301=CARTESIAN_POINT('Ctrl Pts',(-3.47286590088378,8.93046379370378,
0.0576092642770099));
#458302=CARTESIAN_POINT('Ctrl Pts',(-1.84504567841398,9.08869464347889,
2.94278351072189));
#458303=CARTESIAN_POINT('Ctrl Pts',(1.4611272155708,9.24692549325405,3.15107350143256));
#458304=CARTESIAN_POINT('Ctrl Pts',(3.43815588437058,9.40515634302917,0.493023221372883));
#458305=CARTESIAN_POINT('Ctrl Pts',(2.28777317093924,9.56338719280431,-2.61351864193844));
#458306=CARTESIAN_POINT('Ctrl Pts',(-0.94381828653048,9.72161804257944,
-3.34266136505782));
#458307=CARTESIAN_POINT('Ctrl Pts',(-3.31657598992799,9.87984889235457,
-1.03124154186099));
#458308=CARTESIAN_POINT('Ctrl Pts',(-2.6730091437166,10.0380797421297,2.21836021143347));
#458309=CARTESIAN_POINT('Ctrl Pts',(0.403143536253721,10.1963105919048,
3.449814458779));
#458310=CARTESIAN_POINT('Ctrl Pts',(3.11044693930176,10.35454144168,1.54362272554162));
#458311=CARTESIAN_POINT('Ctrl Pts',(2.9925069426194,10.5127722914551,-1.76757971496224));
#458312=CARTESIAN_POINT('Ctrl Pts',(0.144097787138415,10.6710031412302,
-3.46926408178274));
#458313=CARTESIAN_POINT('Ctrl Pts',(-1.82929192642208,10.7764903744137,
-2.50192461070648));
#458314=CARTESIAN_POINT('Ctrl Pts',(-2.39535560853233,10.8292339910054,
-1.70810875200401));
#458315=CARTESIAN_POINT('',(2.64462557919718,10.5,-1.28892185405321));
#458316=CARTESIAN_POINT('Ctrl Pts',(2.64824598975247,10.5,-1.29202896123931));
#458317=CARTESIAN_POINT('Ctrl Pts',(2.60771619382387,10.5,-1.35933450742876));
#458318=CARTESIAN_POINT('Ctrl Pts',(2.56441662780042,10.5,-1.42473933770506));
#458319=CARTESIAN_POINT('Ctrl Pts',(2.51834864997374,10.5,-1.48805257224755));
#458320=CARTESIAN_POINT('Ctrl Pts',(2.46163544863068,10.5,-1.56599600253655));
#458321=CARTESIAN_POINT('Ctrl Pts',(2.40072724532931,10.5,-1.64077094747289));
#458322=CARTESIAN_POINT('Ctrl Pts',(2.33600265773614,10.5,-1.71222878628969));
#458323=CARTESIAN_POINT('Ctrl Pts',(2.27034001215003,10.5,-1.78472226858221));
#458324=CARTESIAN_POINT('Ctrl Pts',(2.20074864978629,10.5,-1.85380226653537));
#458325=CARTESIAN_POINT('Ctrl Pts',(2.12759454936083,10.5,-1.91926945747153));
#458326=CARTESIAN_POINT('Ctrl Pts',(2.05934819428053,10.5,-1.98034460066587));
#458327=CARTESIAN_POINT('Ctrl Pts',(1.98800018894453,10.5,-2.0382752489574));
#458328=CARTESIAN_POINT('Ctrl Pts',(1.91383583320847,10.5,-2.0928604138062));
#458329=CARTESIAN_POINT('Ctrl Pts',(1.89913026926798,10.5,-2.10368374833017));
#458330=CARTESIAN_POINT('Ctrl Pts',(1.88431109821332,10.5,-2.11437733101274));
#458331=CARTESIAN_POINT('Ctrl Pts',(1.86940169672113,10.5,-2.12492478316224));
#458332=CARTESIAN_POINT('Ctrl Pts',(1.79101206381128,10.5,-2.18038045672278));
#458333=CARTESIAN_POINT('Ctrl Pts',(1.71001931992823,10.5,-2.23188418819323));
#458334=CARTESIAN_POINT('Ctrl Pts',(1.62678831297684,10.5,-2.27928484823614));
#458335=CARTESIAN_POINT('Ctrl Pts',(1.54383436022366,10.5,-2.32652772391066));
#458336=CARTESIAN_POINT('Ctrl Pts',(1.45865605470346,10.5,-2.3696950901587));
#458337=CARTESIAN_POINT('Ctrl Pts',(1.37159731217441,10.5,-2.4085889373803));
#458338=CARTESIAN_POINT('Ctrl Pts',(1.28604562437318,10.5,-2.44680950177429));
#458339=CARTESIAN_POINT('Ctrl Pts',(1.19867716260142,10.5,-2.48090337149433));
#458340=CARTESIAN_POINT('Ctrl Pts',(1.10981519656415,10.5,-2.51063277138866));
#458341=CARTESIAN_POINT('Ctrl Pts',(1.06957438776739,10.5,-2.52409561888281));
#458342=CARTESIAN_POINT('Ctrl Pts',(1.02902734314805,10.5,-2.53666274743738));
#458343=CARTESIAN_POINT('Ctrl Pts',(0.988204590736997,10.5,-2.54830849653204));
#458344=CARTESIAN_POINT('Ctrl Pts',(0.970017103524089,10.5,-2.55349694905506));
#458345=CARTESIAN_POINT('Ctrl Pts',(0.951774897571772,10.5,-2.55850248556718));
#458346=CARTESIAN_POINT('Ctrl Pts',(0.933480710930056,10.5,-2.56332268796363));
#458347=CARTESIAN_POINT('Ctrl Pts',(0.919786916179137,10.5,-2.56693076650615));
#458348=CARTESIAN_POINT('Ctrl Pts',(0.906064200589163,10.5,-2.57043487177004));
#458349=CARTESIAN_POINT('Ctrl Pts',(0.892327544296003,10.5,-2.57383077308029));
#458350=CARTESIAN_POINT('Ctrl Pts',(0.803237047065952,10.5,-2.59585524030274));
#458351=CARTESIAN_POINT('Ctrl Pts',(0.713413144578129,10.5,-2.61337205193708));
#458352=CARTESIAN_POINT('Ctrl Pts',(0.623168812775264,10.5,-2.62620601955926));
#458353=CARTESIAN_POINT('Ctrl Pts',(0.535511273105374,10.5,-2.63867211026534));
#458354=CARTESIAN_POINT('Ctrl Pts',(0.447456310351838,10.5,-2.64671995731359));
#458355=CARTESIAN_POINT('Ctrl Pts',(0.359293568760839,10.5,-2.65014101013498));
#458356=CARTESIAN_POINT('Ctrl Pts',(0.277158771371026,10.5,-2.65332815558071));
#458357=CARTESIAN_POINT('Ctrl Pts',(0.194930001718235,10.5,-2.65249925476907));
#458358=CARTESIAN_POINT('Ctrl Pts',(0.112851981779055,10.5,-2.64744628332432));
#458359=CARTESIAN_POINT('Ctrl Pts',(0.0609940227456513,10.5,-2.64425375033713));
#458360=CARTESIAN_POINT('Ctrl Pts',(0.00919647160993013,10.5,-2.63937407072592));
#458361=CARTESIAN_POINT('Ctrl Pts',(-0.0424749391095783,10.5,-2.63283620327292));
#458362=CARTESIAN_POINT('Ctrl Pts',(-0.0620658531138328,10.5,-2.6303574089598));
#458363=CARTESIAN_POINT('Ctrl Pts',(-0.0816386013910069,10.5,-2.62764020594587));
#458364=CARTESIAN_POINT('Ctrl Pts',(-0.101189471878621,10.5,-2.62468601872786));
#458365=CARTESIAN_POINT('Ctrl Pts',(-0.115303261028124,10.5,-2.62255338859614));
#458366=CARTESIAN_POINT('Ctrl Pts',(-0.129397347287274,10.5,-2.62029848263161));
#458367=CARTESIAN_POINT('Ctrl Pts',(-0.14346590111654,10.5,-2.6179230757838));
#458368=CARTESIAN_POINT('Ctrl Pts',(-0.230435410481023,10.5,-2.60323869737492));
#458369=CARTESIAN_POINT('Ctrl Pts',(-0.31648699838215,10.5,-2.58394495861822));
#458370=CARTESIAN_POINT('Ctrl Pts',(-0.401327675911426,10.5,-2.5602666881306));
#458371=CARTESIAN_POINT('Ctrl Pts',(-0.487502461110045,10.5,-2.53621608018441));
#458372=CARTESIAN_POINT('Ctrl Pts',(-0.572428822757296,10.5,-2.50764143553735));
#458373=CARTESIAN_POINT('Ctrl Pts',(-0.65577645030467,10.5,-2.47473082422679));
#458374=CARTESIAN_POINT('Ctrl Pts',(-0.726987573478882,10.5,-2.44661242824194));
#458375=CARTESIAN_POINT('Ctrl Pts',(-0.797046149211874,10.5,-2.41532786870213));
#458376=CARTESIAN_POINT('Ctrl Pts',(-0.865725859582572,10.5,-2.38097213975327));
#458377=CARTESIAN_POINT('Ctrl Pts',(-0.901494993200354,10.5,-2.3630793057172));
#458378=CARTESIAN_POINT('Ctrl Pts',(-0.936889771212117,10.5,-2.34435312802347));
#458379=CARTESIAN_POINT('Ctrl Pts',(-0.971875679297644,10.5,-2.32480524291415));
#458380=CARTESIAN_POINT('Ctrl Pts',(-0.992179376615159,10.5,-2.31346083700401));
#458381=CARTESIAN_POINT('Ctrl Pts',(-1.01234533454571,10.5,-2.30183966418763));
#458382=CARTESIAN_POINT('Ctrl Pts',(-1.03236650126545,10.5,-2.28994383949602));
#458383=CARTESIAN_POINT('Ctrl Pts',(-1.04542406763977,10.5,-2.28218552437571));
#458384=CARTESIAN_POINT('Ctrl Pts',(-1.05841203814074,10.5,-2.27431512371611));
#458385=CARTESIAN_POINT('Ctrl Pts',(-1.07132666184416,10.5,-2.26633489438608));
#458386=CARTESIAN_POINT('Ctrl Pts',(-1.14575428967272,10.5,-2.22034443022684));
#458387=CARTESIAN_POINT('Ctrl Pts',(-1.21777234782126,10.5,-2.17069518002373));
#458388=CARTESIAN_POINT('Ctrl Pts',(-1.28705417295897,10.5,-2.11755280292195));
#458389=CARTESIAN_POINT('Ctrl Pts',(-1.35249212373918,10.5,-2.06735885594931));
#458390=CARTESIAN_POINT('Ctrl Pts',(-1.415489277666,10.5,-2.01404789178091));
#458391=CARTESIAN_POINT('Ctrl Pts',(-1.47573385565858,10.5,-1.9577354512363));
#458392=CARTESIAN_POINT('Ctrl Pts',(-1.49251044505074,10.5,-1.94205386254954));
#458393=CARTESIAN_POINT('Ctrl Pts',(-1.50907333787789,10.5,-1.92613939965935));
#458394=CARTESIAN_POINT('Ctrl Pts',(-1.52541522173048,10.5,-1.90999431236728));
#458395=CARTESIAN_POINT('Ctrl Pts',(-1.54173607886171,10.5,-1.89386999858304));
#458396=CARTESIAN_POINT('Ctrl Pts',(-1.55784021947521,10.5,-1.87751155401848));
#458397=CARTESIAN_POINT('Ctrl Pts',(-1.57369823646274,10.5,-1.86094458549311));
#458398=CARTESIAN_POINT('Ctrl Pts',(-1.63170583048885,10.5,-1.8003436928835));
#458399=CARTESIAN_POINT('Ctrl Pts',(-1.68647481388708,10.5,-1.7369069111149));
#458400=CARTESIAN_POINT('Ctrl Pts',(-1.73768658552469,10.5,-1.67076882779136));
#458401=CARTESIAN_POINT('Ctrl Pts',(-1.78745015137664,10.5,-1.60650104795194));
#458402=CARTESIAN_POINT('Ctrl Pts',(-1.83385517232625,10.5,-1.53968199449149));
#458403=CARTESIAN_POINT('Ctrl Pts',(-1.87656356493191,10.5,-1.47041778850723));
#458404=CARTESIAN_POINT('Ctrl Pts',(-1.89546529830993,10.5,-1.4397630746611));
#458405=CARTESIAN_POINT('Ctrl Pts',(-1.91364231818278,10.5,-1.40862923891412));
#458406=CARTESIAN_POINT('Ctrl Pts',(-1.93106208855764,10.5,-1.37702479013103));
#458407=CARTESIAN_POINT('Ctrl Pts',(-0.00260485525275486,9.6778238829104,
-2.94075152484336));
#458408=CARTESIAN_POINT('Ctrl Pts',(-0.272668602111271,9.69242193613341,
-2.94305882345295));
#458409=CARTESIAN_POINT('Ctrl Pts',(-0.542156455881996,9.70701998935643,
-2.90888975844439));
#458410=CARTESIAN_POINT('Ctrl Pts',(-0.800679327518445,9.72161804257944,
-2.83590094067178));
#458411=CARTESIAN_POINT('Ctrl Pts',(-1.73473752099632,9.77436165917115,
-2.57218809065888));
#458412=CARTESIAN_POINT('Ctrl Pts',(-2.52565675546215,9.82710527576286,
-1.80171481625993));
#458413=CARTESIAN_POINT('Ctrl Pts',(-2.81385523165984,9.87984889235458,
-0.874877886844715));
#458414=CARTESIAN_POINT('Ctrl Pts',(-3.10205370785753,9.93259250894629,
0.0519590425704969));
#458415=CARTESIAN_POINT('Ctrl Pts',(-2.88753142578707,9.985336125538,1.13515962700197));
#458416=CARTESIAN_POINT('Ctrl Pts',(-2.26757817142345,10.0380797421297,
1.88200229377531));
#458417=CARTESIAN_POINT('Ctrl Pts',(-1.64762491705984,10.0908233587214,
2.62884496054864));
#458418=CARTESIAN_POINT('Ctrl Pts',(-0.622240690403053,10.1435669753131,
3.03932970966382));
#458419=CARTESIAN_POINT('Ctrl Pts',(0.341668656766673,10.1963105919048,
2.92687346201518));
#458420=CARTESIAN_POINT('Ctrl Pts',(1.30557800393641,10.2490542084966,2.81441721436654));
#458421=CARTESIAN_POINT('Ctrl Pts',(2.20801247161908,10.3017978250883,2.17901996995408));
#458422=CARTESIAN_POINT('Ctrl Pts',(2.6395730393467,10.35454144168,1.30945427433054));
#458423=CARTESIAN_POINT('Ctrl Pts',(3.03629831825809,10.4030276277867,0.510079357051782));
#458424=CARTESIAN_POINT('Ctrl Pts',(3.03509893577357,10.4515138138933,-0.487185911904285));
#458425=CARTESIAN_POINT('Ctrl Pts',(2.64824598975249,10.5,-1.29202896123927));
#458426=CARTESIAN_POINT('',(-1.16757930174901,4.5,-2.20857791054889));
#458427=CARTESIAN_POINT('Ctrl Pts',(-1.16720946766529,4.5,-2.20674979140378));
#458428=CARTESIAN_POINT('Ctrl Pts',(-1.09418489924995,4.5,-2.25558279540327));
#458429=CARTESIAN_POINT('Ctrl Pts',(-1.01871064242017,4.5,-2.30069007211117));
#458430=CARTESIAN_POINT('Ctrl Pts',(-0.941171421508105,4.5,-2.34196444480317));
#458431=CARTESIAN_POINT('Ctrl Pts',(-0.862652120175966,4.5,-2.38376051740458));
#458432=CARTESIAN_POINT('Ctrl Pts',(-0.782014582806237,4.5,-2.42162681390361));
#458433=CARTESIAN_POINT('Ctrl Pts',(-0.699617970959709,4.5,-2.45541705646166));
#458434=CARTESIAN_POINT('Ctrl Pts',(-0.658822312174829,4.5,-2.47214705512015));
#458435=CARTESIAN_POINT('Ctrl Pts',(-0.617594890723472,4.5,-2.48787726556793));
#458436=CARTESIAN_POINT('Ctrl Pts',(-0.575976592450254,4.5,-2.5025860725845));
#458437=CARTESIAN_POINT('Ctrl Pts',(-0.553919435071559,4.5,-2.51038154920604));
#458438=CARTESIAN_POINT('Ctrl Pts',(-0.531752459925753,4.5,-2.51789008166673));
#458439=CARTESIAN_POINT('Ctrl Pts',(-0.509481600949336,4.5,-2.52510812556613));
#458440=CARTESIAN_POINT('Ctrl Pts',(-0.495436663612055,4.5,-2.52966012665295));
#458441=CARTESIAN_POINT('Ctrl Pts',(-0.481350408747885,4.5,-2.53409659314146));
#458442=CARTESIAN_POINT('Ctrl Pts',(-0.467224306955522,4.5,-2.53841658707718));
#458443=CARTESIAN_POINT('Ctrl Pts',(-0.454324673369296,4.5,-2.54236150689191));
#458444=CARTESIAN_POINT('Ctrl Pts',(-0.441400473321808,4.5,-2.54620664063633));
#458445=CARTESIAN_POINT('Ctrl Pts',(-0.428454934226926,4.5,-2.54995109762075));
#458446=CARTESIAN_POINT('Ctrl Pts',(-0.340329570016068,4.5,-2.5754410855699));
#458447=CARTESIAN_POINT('Ctrl Pts',(-0.251189447245526,4.5,-2.59627753658197));
#458448=CARTESIAN_POINT('Ctrl Pts',(-0.161434310388018,4.5,-2.6123411462201));
#458449=CARTESIAN_POINT('Ctrl Pts',(-0.0719442988975715,4.5,-2.62835730597902));
#458450=CARTESIAN_POINT('Ctrl Pts',(0.0181580072313792,4.5,-2.6396293173294));
#458451=CARTESIAN_POINT('Ctrl Pts',(0.108506185982615,4.5,-2.64599744291219));
#458452=CARTESIAN_POINT('Ctrl Pts',(0.181833237901982,4.5,-2.65116584676594));
#458453=CARTESIAN_POINT('Ctrl Pts',(0.255323010375989,4.5,-2.65310340109756));
#458454=CARTESIAN_POINT('Ctrl Pts',(0.328787855288838,4.5,-2.65170078359385));
#458455=CARTESIAN_POINT('Ctrl Pts',(0.386688202235693,4.5,-2.6505953291388));
#458456=CARTESIAN_POINT('Ctrl Pts',(0.444573253679694,4.5,-2.64741466692496));
#458457=CARTESIAN_POINT('Ctrl Pts',(0.502371499748814,4.5,-2.64221382737986));
#458458=CARTESIAN_POINT('Ctrl Pts',(0.517067712750352,4.5,-2.64089142313856));
#458459=CARTESIAN_POINT('Ctrl Pts',(0.531760578384411,4.5,-2.63943811642234));
#458460=CARTESIAN_POINT('Ctrl Pts',(0.546441660979092,4.5,-2.63785550692038));
#458461=CARTESIAN_POINT('Ctrl Pts',(0.63475323233854,4.5,-2.62833558691002));
#458462=CARTESIAN_POINT('Ctrl Pts',(0.722383507378646,4.5,-2.61417000942873));
#458463=CARTESIAN_POINT('Ctrl Pts',(0.80906990177474,4.5,-2.5956457375465));
#458464=CARTESIAN_POINT('Ctrl Pts',(0.898018902058379,4.5,-2.5766379627234));
#458465=CARTESIAN_POINT('Ctrl Pts',(0.985974751507412,4.5,-2.55304093462189));
#458466=CARTESIAN_POINT('Ctrl Pts',(1.0726638111339,4.5,-2.525111147678));
#458467=CARTESIAN_POINT('Ctrl Pts',(1.16137360737258,4.5,-2.49653031268617));
#458468=CARTESIAN_POINT('Ctrl Pts',(1.24875765965886,4.5,-2.46341225247124));
#458469=CARTESIAN_POINT('Ctrl Pts',(1.33452205891312,4.5,-2.42597784958751));
#458470=CARTESIAN_POINT('Ctrl Pts',(1.37056586003357,4.5,-2.41024546896879));
#458471=CARTESIAN_POINT('Ctrl Pts',(1.40632351482737,4.5,-2.39375009028297));
#458472=CARTESIAN_POINT('Ctrl Pts',(1.44177263485956,4.5,-2.37650544881492));
#458473=CARTESIAN_POINT('Ctrl Pts',(1.46835451291241,4.5,-2.36357438152319));
#458474=CARTESIAN_POINT('Ctrl Pts',(1.49476289766104,4.5,-2.35022197907058));
#458475=CARTESIAN_POINT('Ctrl Pts',(1.52098814208497,4.5,-2.33645348486302));
#458476=CARTESIAN_POINT('Ctrl Pts',(1.53874744731609,4.5,-2.32712968649332));
#458477=CARTESIAN_POINT('Ctrl Pts',(1.5564261955549,4.5,-2.31761305195935));
#458478=CARTESIAN_POINT('Ctrl Pts',(1.5739973348238,4.5,-2.30791870221317));
#458479=CARTESIAN_POINT('Ctrl Pts',(1.65834632926029,4.5,-2.26138167121633));
#458480=CARTESIAN_POINT('Ctrl Pts',(1.74032087554525,4.5,-2.2107006612154));
#458481=CARTESIAN_POINT('Ctrl Pts',(1.81961506685248,4.5,-2.15613558536194));
#458482=CARTESIAN_POINT('Ctrl Pts',(1.90241102244278,4.5,-2.099160824378));
#458483=CARTESIAN_POINT('Ctrl Pts',(1.98228575781152,4.5,-2.03795133014415));
#458484=CARTESIAN_POINT('Ctrl Pts',(2.05887599007727,4.5,-1.97274553631761));
#458485=CARTESIAN_POINT('Ctrl Pts',(2.08337611964662,4.5,-1.95188712722075));
#458486=CARTESIAN_POINT('Ctrl Pts',(2.1075399741187,4.5,-1.93061936836532));
#458487=CARTESIAN_POINT('Ctrl Pts',(2.13135505862694,4.5,-1.90894891688576));
#458488=CARTESIAN_POINT('Ctrl Pts',(2.149031917455,4.5,-1.89286392204091));
#458489=CARTESIAN_POINT('Ctrl Pts',(2.16652003582568,4.5,-1.87655361111569));
#458490=CARTESIAN_POINT('Ctrl Pts',(2.18379266535965,4.5,-1.86004160965249));
#458491=CARTESIAN_POINT('Ctrl Pts',(2.25538608654167,4.5,-1.79160092012178));
#458492=CARTESIAN_POINT('Ctrl Pts',(2.32334545706174,4.5,-1.71964110348878));
#458493=CARTESIAN_POINT('Ctrl Pts',(2.38734340910508,4.5,-1.64440303111735));
#458494=CARTESIAN_POINT('Ctrl Pts',(2.45054242915136,4.5,-1.57010420916713));
#458495=CARTESIAN_POINT('Ctrl Pts',(2.50987914554644,4.5,-1.49260796472081));
#458496=CARTESIAN_POINT('Ctrl Pts',(2.56501236813317,4.5,-1.41210333829057));
#458497=CARTESIAN_POINT('Ctrl Pts',(2.59262003696796,4.5,-1.37179107352755));
#458498=CARTESIAN_POINT('Ctrl Pts',(2.61917321494964,4.5,-1.33072384195471));
#458499=CARTESIAN_POINT('Ctrl Pts',(2.64462557919718,4.5,-1.28892185405321));
#458500=CARTESIAN_POINT('',(-1.93106208855765,4.5,-1.37702479013102));
#458501=CARTESIAN_POINT('Ctrl Pts',(-1.9335268427243,4.5,-1.37997739579602));
#458502=CARTESIAN_POINT('Ctrl Pts',(-1.90294786357442,4.5,-1.4362477131916));
#458503=CARTESIAN_POINT('Ctrl Pts',(-1.87001560750643,4.5,-1.49108118098694));
#458504=CARTESIAN_POINT('Ctrl Pts',(-1.8347642883134,4.5,-1.54431081872619));
#458505=CARTESIAN_POINT('Ctrl Pts',(-1.79134862867028,4.5,-1.60986864430315));
#458506=CARTESIAN_POINT('Ctrl Pts',(-1.74441685771687,4.5,-1.67299484320599));
#458507=CARTESIAN_POINT('Ctrl Pts',(-1.69428976219437,4.5,-1.73361425041499));
#458508=CARTESIAN_POINT('Ctrl Pts',(-1.65405833423722,4.5,-1.78226668655782));
#458509=CARTESIAN_POINT('Ctrl Pts',(-1.61176765181253,4.5,-1.82930421487226));
#458510=CARTESIAN_POINT('Ctrl Pts',(-1.56756501121874,4.5,-1.87467965146355));
#458511=CARTESIAN_POINT('Ctrl Pts',(-1.55597691131931,4.5,-1.8865752098541));
#458512=CARTESIAN_POINT('Ctrl Pts',(-1.5442570150119,4.5,-1.89835665926739));
#458513=CARTESIAN_POINT('Ctrl Pts',(-1.53241908406833,4.5,-1.91001237096306));
#458514=CARTESIAN_POINT('Ctrl Pts',(-1.47170002051753,4.5,-1.96979679634561));
#458515=CARTESIAN_POINT('Ctrl Pts',(-1.40781138555655,4.5,-2.02634614990377));
#458516=CARTESIAN_POINT('Ctrl Pts',(-1.34114315453392,4.5,-2.07956945339699));
#458517=CARTESIAN_POINT('Ctrl Pts',(-1.28506408411193,4.5,-2.12433910363226));
#458518=CARTESIAN_POINT('Ctrl Pts',(-1.22701711413373,4.5,-2.1667552100927));
#458519=CARTESIAN_POINT('Ctrl Pts',(-1.1672094676653,4.5,-2.20674979140377));
#458520=CARTESIAN_POINT('Ctrl Pts',(-1.93352684272429,4.5,-1.37997739579603));
#458521=CARTESIAN_POINT('Ctrl Pts',(-2.3483001601145,4.54848618610667,-0.791574179663466));
#458522=CARTESIAN_POINT('Ctrl Pts',(-2.6275861959031,4.64971598880506,0.863552072911287));
#458523=CARTESIAN_POINT('Ctrl Pts',(-0.779984807125968,4.80368940809515,
2.68923010885977));
#458524=CARTESIAN_POINT('Ctrl Pts',(1.82984645434041,4.96192025787029,2.11979424147793));
#458525=CARTESIAN_POINT('Ctrl Pts',(2.77432553661561,5.12015110764542,-0.378228552056395));
#458526=CARTESIAN_POINT('Ctrl Pts',(1.48834568074501,5.249040985657,-2.13264435436969));
#458527=CARTESIAN_POINT('Ctrl Pts',(0.350727759203873,5.32518724707686,
-2.36905771742893));
#458528=CARTESIAN_POINT('Ctrl Pts',(0.000720435901828305,5.34858989190502,
-2.36812053819695));
#458529=CARTESIAN_POINT('Origin',(3.51939854619125E-16,4.5,1.42943244214557E-16));
#458530=CARTESIAN_POINT('',(-1.16578764820077,4.49999999999947,2.20849593760086));
#458531=CARTESIAN_POINT('Origin',(0.,4.5,0.));
#458532=CARTESIAN_POINT('',(-1.93106208855765,4.5,1.37702479013101));
#458533=CARTESIAN_POINT('Ctrl Pts',(-1.16362616052841,4.5,2.20658584552698));
#458534=CARTESIAN_POINT('Ctrl Pts',(-1.20304899293036,4.5,2.17987034616207));
#458535=CARTESIAN_POINT('Ctrl Pts',(-1.24176754454475,4.5,2.15205514598253));
#458536=CARTESIAN_POINT('Ctrl Pts',(-1.27971972775532,4.5,2.12315938972328));
#458537=CARTESIAN_POINT('Ctrl Pts',(-1.29274526297021,4.5,2.11324210278811));
#458538=CARTESIAN_POINT('Ctrl Pts',(-1.30568048702961,4.5,2.10319751816554));
#458539=CARTESIAN_POINT('Ctrl Pts',(-1.31852276478251,4.5,2.09302636184682));
#458540=CARTESIAN_POINT('Ctrl Pts',(-1.32890886006521,4.5,2.08480051587978));
#458541=CARTESIAN_POINT('Ctrl Pts',(-1.33923486955066,4.5,2.07649122274235));
#458542=CARTESIAN_POINT('Ctrl Pts',(-1.34948781355063,4.5,2.0681085469444));
#458543=CARTESIAN_POINT('Ctrl Pts',(-1.41555082150238,4.5,2.01409627711253));
#458544=CARTESIAN_POINT('Ctrl Pts',(-1.47870564375788,4.5,1.95694451970025));
#458545=CARTESIAN_POINT('Ctrl Pts',(-1.53865732185489,4.5,1.89681347866715));
#458546=CARTESIAN_POINT('Ctrl Pts',(-1.59768214555386,4.5,1.83761206498743));
#458547=CARTESIAN_POINT('Ctrl Pts',(-1.65360262165799,4.5,1.77552213293353));
#458548=CARTESIAN_POINT('Ctrl Pts',(-1.70609505968126,4.5,1.71067029915434));
#458549=CARTESIAN_POINT('Ctrl Pts',(-1.75694521695872,4.5,1.64784742272514));
#458550=CARTESIAN_POINT('Ctrl Pts',(-1.80457876892434,4.5,1.58243218655813));
#458551=CARTESIAN_POINT('Ctrl Pts',(-1.8486558967636,4.5,1.51452373186239));
#458552=CARTESIAN_POINT('Ctrl Pts',(-1.87770703286451,4.5,1.46976542168023));
#458553=CARTESIAN_POINT('Ctrl Pts',(-1.90521228813023,4.5,1.42392372599992));
#458554=CARTESIAN_POINT('Ctrl Pts',(-1.93106208855765,4.5,1.37702479013102));
#458555=CARTESIAN_POINT('Origin',(0.,4.5,0.));
#458556=CARTESIAN_POINT('Origin',(0.,2.65141010809498,0.));
#458557=CARTESIAN_POINT('Ctrl Pts',(-1.93106208855765,4.5,1.37702479013101));
#458558=CARTESIAN_POINT('Ctrl Pts',(-1.47471894170348,4.55274361659171,
2.01697474352245));
#458559=CARTESIAN_POINT('Ctrl Pts',(0.116161058328033,4.65823084977513,
2.79681763637796));
#458560=CARTESIAN_POINT('Ctrl Pts',(2.41247039077219,4.81646169955027,1.42496614872057));
#458561=CARTESIAN_POINT('Ctrl Pts',(2.50754408484683,4.9746925493254,-1.24442001550399));
#458562=CARTESIAN_POINT('Ctrl Pts',(0.967518711764578,5.08634201884031,
-2.32874300863249));
#458563=CARTESIAN_POINT('Ctrl Pts',(0.0931897088482703,5.1452478717635,
-2.37498460353472));
#458564=CARTESIAN_POINT('Ctrl Pts',(0.00164853063274016,5.15141010809498,
-2.37430728468225));
#458565=CARTESIAN_POINT('Ctrl Pts',(-2.39535560853236,4.17076600899462,
1.70810875200397));
#458566=CARTESIAN_POINT('Ctrl Pts',(-1.82929192642212,4.22350962558633,
2.50192461070645));
#458567=CARTESIAN_POINT('Ctrl Pts',(0.144090158575332,4.32899685876975,
3.46926846683839));
#458568=CARTESIAN_POINT('Ctrl Pts',(2.99251096854717,4.48722770854488,1.76757685655568));
#458569=CARTESIAN_POINT('Ctrl Pts',(3.1104436376597,4.64545855832002,-1.54362124406565));
#458570=CARTESIAN_POINT('Ctrl Pts',(0.403145204663006,4.80368940809515,
-3.44981447404064));
#458571=CARTESIAN_POINT('Ctrl Pts',(-2.67300976386123,4.96192025787029,
-2.21835958527511));
#458572=CARTESIAN_POINT('Ctrl Pts',(-3.3165748221749,5.12015110764542,1.03124125374368));
#458573=CARTESIAN_POINT('Ctrl Pts',(-0.943818501798861,5.27838195742055,
3.34266087532576));
#458574=CARTESIAN_POINT('Ctrl Pts',(2.2877730124377,5.4366128071957,2.61351819404304));
#458575=CARTESIAN_POINT('Ctrl Pts',(3.43815520344814,5.59484365697082,-0.493023131661703));
#458576=CARTESIAN_POINT('Ctrl Pts',(1.46112704739312,5.75307450674597,-3.15107299300958));
#458577=CARTESIAN_POINT('Ctrl Pts',(-1.84504541757382,5.91130535652109,
-2.94278303115694));
#458578=CARTESIAN_POINT('Ctrl Pts',(-3.47286531459505,6.06953620629624,
-0.0576092552393699));
#458579=CARTESIAN_POINT('Ctrl Pts',(-1.94163201382627,6.22776705607136,
2.87996596444098));
#458580=CARTESIAN_POINT('Ctrl Pts',(1.35579728692029,6.3859979058465,3.19780418671017));
#458581=CARTESIAN_POINT('Ctrl Pts',(3.41993330709188,6.54422875562164,0.60678453106123));
#458582=CARTESIAN_POINT('Ctrl Pts',(2.37315565640484,6.70245960539676,-2.53619153528431));
#458583=CARTESIAN_POINT('Ctrl Pts',(-0.832345044282379,6.8606904551719,
-3.3721412383904));
#458584=CARTESIAN_POINT('Ctrl Pts',(-3.28070925568909,7.01892130494704,
-1.14064928956114));
#458585=CARTESIAN_POINT('Ctrl Pts',(-2.74480248964314,7.17715215472217,
2.12842519619706));
#458586=CARTESIAN_POINT('Ctrl Pts',(0.287892198668033,7.33538300449732,
3.46139460101041));
#458587=CARTESIAN_POINT('Ctrl Pts',(3.05870802656444,7.49361385427243,1.64573379718225));
#458588=CARTESIAN_POINT('Ctrl Pts',(3.04719425459711,7.65184470404759,-1.66695566734414));
#458589=CARTESIAN_POINT('Ctrl Pts',(0.263824564395874,7.8100755538227,-3.4633122012917));
#458590=CARTESIAN_POINT('Ctrl Pts',(-2.75953144406721,7.96830640359785,
-2.10929407204838));
#458591=CARTESIAN_POINT('Ctrl Pts',(-3.27270076817495,8.12653725337297,
1.16342639392387));
#458592=CARTESIAN_POINT('Ctrl Pts',(-0.808885257824385,8.28476810314812,
3.37784584305381));
#458593=CARTESIAN_POINT('Ctrl Pts',(2.39072919250016,8.44299895292324,2.51963345778332));
#458594=CARTESIAN_POINT('Ctrl Pts',(3.41563023469626,8.60122980269838,-0.630541370122069));
#458595=CARTESIAN_POINT('Ctrl Pts',(1.33354097220925,8.75946065247352,-3.20715341647614));
#458596=CARTESIAN_POINT('Ctrl Pts',(-1.96161384413887,8.91769150224866,
-2.86639571280394));
#458597=CARTESIAN_POINT('Ctrl Pts',(-3.47236252177528,9.07592235202378,
0.0817406185527763));
#458598=CARTESIAN_POINT('Ctrl Pts',(-1.82458054458892,9.23415320179893,
2.95555215540851));
#458599=CARTESIAN_POINT('Ctrl Pts',(1.4830638979422,9.39238405157406,3.14081145030897));
#458600=CARTESIAN_POINT('Ctrl Pts',(3.44136729599262,9.55061490134919,0.469167569829518));
#458601=CARTESIAN_POINT('Ctrl Pts',(2.26980498139681,9.70884575112431,-2.62946492536136));
#458602=CARTESIAN_POINT('Ctrl Pts',(-0.967521539463769,9.86707660089947,
-3.33581294919496));
#458603=CARTESIAN_POINT('Ctrl Pts',(-3.32271450697131,10.0253074506746,
-1.0085605947839));
#458604=CARTESIAN_POINT('Ctrl Pts',(-2.65938629817939,10.1835383004497,
2.23765823077655));
#458605=CARTESIAN_POINT('Ctrl Pts',(0.431019144387391,10.3417691502249,
3.44540391913185));
#458606=CARTESIAN_POINT('Ctrl Pts',(2.21747956182459,10.4472563834083,2.16534526175896));
#458607=CARTESIAN_POINT('Ctrl Pts',(2.64462557919717,10.5,1.28892185405324));
#458608=CARTESIAN_POINT('Ctrl Pts',(-2.24059110187412,4.28051067266308,
1.59774743137965));
#458609=CARTESIAN_POINT('Ctrl Pts',(-1.7111009315159,4.33325428925479,2.34027465497845));
#458610=CARTESIAN_POINT('Ctrl Pts',(0.134780458492896,4.43874152243821,
3.24511819001825));
#458611=CARTESIAN_POINT('Ctrl Pts',(2.79916410928885,4.59697237221335,1.65337328727731));
#458612=CARTESIAN_POINT('Ctrl Pts',(2.90947712005541,4.75520322198848,-1.44388750121177));
#458613=CARTESIAN_POINT('Ctrl Pts',(0.377097895240948,4.91343407176362,
-3.22692112441208));
#458614=CARTESIAN_POINT('Ctrl Pts',(-2.50030595490566,5.07166492153874,
-2.07503083459494));
#458615=CARTESIAN_POINT('Ctrl Pts',(-3.10229011875939,5.22989577131389,
0.964612506298938));
#458616=CARTESIAN_POINT('Ctrl Pts',(-0.882838159554263,5.38812662108902,
3.12669074569122));
#458617=CARTESIAN_POINT('Ctrl Pts',(2.13995944339821,5.54635747086415,2.44465814983807));
#458618=CARTESIAN_POINT('Ctrl Pts',(3.21601516211953,5.70458832063929,-0.461168787583972));
#458619=CARTESIAN_POINT('Ctrl Pts',(1.36672327458824,5.86281917041442,-2.94748140290493));
#458620=CARTESIAN_POINT('Ctrl Pts',(-1.72583658578463,6.02105002018956,
-2.75264910599069));
#458621=CARTESIAN_POINT('Ctrl Pts',(-3.24848264456924,6.17928086996469,
-0.0538871072901001));
#458622=CARTESIAN_POINT('Ctrl Pts',(-1.81618269863429,6.33751171973983,
2.69389066518623));
#458623=CARTESIAN_POINT('Ctrl Pts',(1.26819889547839,6.49574256951496,2.99119328284981));
#458624=CARTESIAN_POINT('Ctrl Pts',(3.19897058690502,6.65397341929009,0.56758003538508));
#458625=CARTESIAN_POINT('Ctrl Pts',(2.21982549403628,6.81220426906523,-2.37232758525079));
#458626=CARTESIAN_POINT('Ctrl Pts',(-0.778567029156389,6.97043511884036,
-3.15426637535028));
#458627=CARTESIAN_POINT('Ctrl Pts',(-3.0687418352204,7.1286659686155,-1.06695166239456));
#458628=CARTESIAN_POINT('Ctrl Pts',(-2.56746013526754,7.28689681839063,
1.99090712820122));
#458629=CARTESIAN_POINT('Ctrl Pts',(0.269291413908186,7.44512766816577,
3.23775305657055));
#458630=CARTESIAN_POINT('Ctrl Pts',(2.86108415933712,7.60335851794091,1.53940253751273));
#458631=CARTESIAN_POINT('Ctrl Pts',(2.85031429496828,7.76158936771603,-1.5592532574979));
#458632=CARTESIAN_POINT('Ctrl Pts',(0.246778795321915,7.91982021749117,
-3.23954676023271));
#458633=CARTESIAN_POINT('Ctrl Pts',(-2.58123744837501,8.07805106726631,
-1.97301207062241));
#458634=CARTESIAN_POINT('Ctrl Pts',(-3.06125077802632,8.23628191704144,
1.08825713252175));
#458635=CARTESIAN_POINT('Ctrl Pts',(-0.756622985189625,8.39451276681658,
3.15960240412321));
#458636=CARTESIAN_POINT('Ctrl Pts',(2.23626359970351,8.55274361659171,2.35683932915189));
#458637=CARTESIAN_POINT('Ctrl Pts',(3.19494553706024,8.71097446636684,-0.589801939313997));
#458638=CARTESIAN_POINT('Ctrl Pts',(1.2473805666572,8.86920531614198,-2.99993845661374));
#458639=CARTESIAN_POINT('Ctrl Pts',(-1.83487349804549,9.02743616591711,
-2.68119719079777));
#458640=CARTESIAN_POINT('Ctrl Pts',(-3.24801233731547,9.18566701569225,
0.0764593373688121));
#458641=CARTESIAN_POINT('Ctrl Pts',(-1.70669395320529,9.34389786546738,
2.76459321402831));
#458642=CARTESIAN_POINT('Ctrl Pts',(1.38724277990442,9.50212871524252,2.93788286096626));
#458643=CARTESIAN_POINT('Ctrl Pts',(3.21901972058589,9.66035956501766,0.438854539385907));
#458644=CARTESIAN_POINT('Ctrl Pts',(2.12315233119949,9.81859041479278,-2.45957455897939));
#458645=CARTESIAN_POINT('Ctrl Pts',(-0.905009738208482,9.97682126456792,
-3.1202852657281));
#458646=CARTESIAN_POINT('Ctrl Pts',(-3.10803311703245,10.1350521143431,
-0.943397250213819));
#458647=CARTESIAN_POINT('Ctrl Pts',(-2.48756270464474,10.2932829641182,
2.09308258993129));
#458648=CARTESIAN_POINT('Ctrl Pts',(0.403170892961278,10.4515138138933,
3.22279553652535));
#458649=CARTESIAN_POINT('Ctrl Pts',(2.07420766967294,10.5570010470767,2.02544177937531));
#458650=CARTESIAN_POINT('Ctrl Pts',(2.47375567929493,10.6097446636685,1.20564430054384));
#458651=CARTESIAN_POINT('Ctrl Pts',(-2.08582659521589,4.39025533633154,
1.48738611075533));
#458652=CARTESIAN_POINT('Ctrl Pts',(-1.59290993660969,4.44299895292325,
2.17862469925045));
#458653=CARTESIAN_POINT('Ctrl Pts',(0.125470758410464,4.54848618610667,
3.0209679131981));
#458654=CARTESIAN_POINT('Ctrl Pts',(2.60581725003052,4.70671703588181,1.53916971799893));
#458655=CARTESIAN_POINT('Ctrl Pts',(2.70851060245112,4.86494788565694,-1.34415375835788));
#458656=CARTESIAN_POINT('Ctrl Pts',(0.351050585818886,5.02317873543207,
-3.00402777478352));
#458657=CARTESIAN_POINT('Ctrl Pts',(-2.32760214595009,5.18140958520721,
-1.93170208391477));
#458658=CARTESIAN_POINT('Ctrl Pts',(-2.88800541534388,5.33964043498234,
0.897983758854196));
#458659=CARTESIAN_POINT('Ctrl Pts',(-0.821857817309664,5.49787128475748,
2.91072061605667));
#458660=CARTESIAN_POINT('Ctrl Pts',(1.99214587435872,5.65610213453262,2.2757981056331));
#458661=CARTESIAN_POINT('Ctrl Pts',(2.99387512079092,5.81433298430775,-0.429314443506242));
#458662=CARTESIAN_POINT('Ctrl Pts',(1.27231950178335,5.97256383408288,-2.74388981280027));
#458663=CARTESIAN_POINT('Ctrl Pts',(-1.60662775399543,6.13079468385802,
-2.56251518082445));
#458664=CARTESIAN_POINT('Ctrl Pts',(-3.02409997454343,6.28902553363315,
-0.0501649593408253));
#458665=CARTESIAN_POINT('Ctrl Pts',(-1.6907333834423,6.4472563834083,2.50781536593148));
#458666=CARTESIAN_POINT('Ctrl Pts',(1.18060050403648,6.60548723318341,2.78458237898946));
#458667=CARTESIAN_POINT('Ctrl Pts',(2.97800786671818,6.76371808295857,0.52837553970893));
#458668=CARTESIAN_POINT('Ctrl Pts',(2.06649533166772,6.92194893273368,-2.20846363521727));
#458669=CARTESIAN_POINT('Ctrl Pts',(-0.724789014030395,7.08017978250883,
-2.93639151231016));
#458670=CARTESIAN_POINT('Ctrl Pts',(-2.85677441475171,7.23841063228396,
-0.993254035227974));
#458671=CARTESIAN_POINT('Ctrl Pts',(-2.39011778089194,7.39664148205909,
1.85338906020537));
#458672=CARTESIAN_POINT('Ctrl Pts',(0.250690629148338,7.55487233183423,
3.01411151213069));
#458673=CARTESIAN_POINT('Ctrl Pts',(2.66346029210979,7.71310318160936,1.4330712778432));
#458674=CARTESIAN_POINT('Ctrl Pts',(2.65343433533946,7.8713340313845,-1.45155084765165));
#458675=CARTESIAN_POINT('Ctrl Pts',(0.229733026247954,8.02956488115963,
-3.01578131917373));
#458676=CARTESIAN_POINT('Ctrl Pts',(-2.40294345268282,8.18779573093476,
-1.83673006919644));
#458677=CARTESIAN_POINT('Ctrl Pts',(-2.84980078787769,8.3460265807099,1.01308787111964));
#458678=CARTESIAN_POINT('Ctrl Pts',(-0.704360712554865,8.50425743048505,
2.94135896519262));
#458679=CARTESIAN_POINT('Ctrl Pts',(2.08179800690687,8.66248828026016,2.19404520052047));
#458680=CARTESIAN_POINT('Ctrl Pts',(2.97426083942421,8.82071913003532,-0.549062508505919));
#458681=CARTESIAN_POINT('Ctrl Pts',(1.16122016110515,8.97894997981042,-2.79272349675135));
#458682=CARTESIAN_POINT('Ctrl Pts',(-1.70813315195211,9.13718082958559,
-2.4959986687916));
#458683=CARTESIAN_POINT('Ctrl Pts',(-3.02366215285565,9.2954116793607,0.0711780561848446));
#458684=CARTESIAN_POINT('Ctrl Pts',(-1.58880736182167,9.45364252913585,
2.5736342726481));
#458685=CARTESIAN_POINT('Ctrl Pts',(1.29142166186663,9.61187337891097,2.73495427162356));
#458686=CARTESIAN_POINT('Ctrl Pts',(2.99667214517916,9.77010422868612,0.408541508942294));
#458687=CARTESIAN_POINT('Ctrl Pts',(1.97649968100217,9.92833507846124,-2.28968419259741));
#458688=CARTESIAN_POINT('Ctrl Pts',(-0.84249793695319,10.0865659282364,
-2.90475758226125));
#458689=CARTESIAN_POINT('Ctrl Pts',(-2.89335172709359,10.2447967780115,
-0.878233905643736));
#458690=CARTESIAN_POINT('Ctrl Pts',(-2.31573911111009,10.4030276277867,
1.94850694908602));
#458691=CARTESIAN_POINT('Ctrl Pts',(0.375322641535166,10.5612584775618,
3.00018715391885));
#458692=CARTESIAN_POINT('Ctrl Pts',(1.9309357775213,10.6667457107452,1.88553829699167));
#458693=CARTESIAN_POINT('Ctrl Pts',(2.30288577939269,10.7194893273369,1.12236674703445));
#458694=CARTESIAN_POINT('Ctrl Pts',(-1.93106208855765,4.5,1.37702479013101));
#458695=CARTESIAN_POINT('Ctrl Pts',(-1.47471894170348,4.55274361659171,
2.01697474352245));
#458696=CARTESIAN_POINT('Ctrl Pts',(0.116161058328033,4.65823084977513,
2.79681763637796));
#458697=CARTESIAN_POINT('Ctrl Pts',(2.41247039077219,4.81646169955027,1.42496614872057));
#458698=CARTESIAN_POINT('Ctrl Pts',(2.50754408484683,4.9746925493254,-1.24442001550399));
#458699=CARTESIAN_POINT('Ctrl Pts',(0.325003276396823,5.13292339910054,
-2.78113442515496));
#458700=CARTESIAN_POINT('Ctrl Pts',(-2.15489833699452,5.29115424887567,
-1.78837333323461));
#458701=CARTESIAN_POINT('Ctrl Pts',(-2.67372071192838,5.44938509865081,
0.831355011409453));
#458702=CARTESIAN_POINT('Ctrl Pts',(-0.760877475065064,5.60761594842594,
2.69475048642212));
#458703=CARTESIAN_POINT('Ctrl Pts',(1.84433230531922,5.76584679820107,2.10693806142813));
#458704=CARTESIAN_POINT('Ctrl Pts',(2.77173507946231,5.92407764797621,-0.397460099428512));
#458705=CARTESIAN_POINT('Ctrl Pts',(1.17791572897846,6.08230849775135,-2.54029822269561));
#458706=CARTESIAN_POINT('Ctrl Pts',(-1.48741892220623,6.24053934752648,
-2.37238125565821));
#458707=CARTESIAN_POINT('Ctrl Pts',(-2.79971730451761,6.39877019730161,
-0.0464428113915518));
#458708=CARTESIAN_POINT('Ctrl Pts',(-1.56528406825032,6.55700104707675,
2.32174006667672));
#458709=CARTESIAN_POINT('Ctrl Pts',(1.09300211259457,6.71523189685188,2.5779714751291));
#458710=CARTESIAN_POINT('Ctrl Pts',(2.75704514653133,6.87346274662702,0.48917104403278));
#458711=CARTESIAN_POINT('Ctrl Pts',(1.91316516929916,7.03169359640215,-2.04459968518375));
#458712=CARTESIAN_POINT('Ctrl Pts',(-0.671010998904404,7.18992444617728,
-2.71851664927003));
#458713=CARTESIAN_POINT('Ctrl Pts',(-2.64480699428301,7.34815529595243,
-0.91955640806139));
#458714=CARTESIAN_POINT('Ctrl Pts',(-2.21277542651634,7.50638614572755,
1.71587099220952));
#458715=CARTESIAN_POINT('Ctrl Pts',(0.232089844388488,7.6646169955027,2.79046996769084));
#458716=CARTESIAN_POINT('Ctrl Pts',(2.46583642488247,7.82284784527782,1.32674001817368));
#458717=CARTESIAN_POINT('Ctrl Pts',(2.45655437571063,7.98107869505296,-1.3438484378054));
#458718=CARTESIAN_POINT('Ctrl Pts',(0.212687257173993,8.13930954482809,
-2.79201587811474));
#458719=CARTESIAN_POINT('Ctrl Pts',(-2.22464945699063,8.29754039460322,
-1.70044806777047));
#458720=CARTESIAN_POINT('Ctrl Pts',(-2.63835079772906,8.45577124437837,
0.937918609717529));
#458721=CARTESIAN_POINT('Ctrl Pts',(-0.652098439920106,8.61400209415349,
2.72311552626202));
#458722=CARTESIAN_POINT('Ctrl Pts',(1.92733241411022,8.77223294392864,2.03125107188904));
#458723=CARTESIAN_POINT('Ctrl Pts',(2.75357614178819,8.93046379370376,-0.508323077697843));
#458724=CARTESIAN_POINT('Ctrl Pts',(1.07505975555311,9.08869464347891,-2.58550853688895));
#458725=CARTESIAN_POINT('Ctrl Pts',(-1.58139280585873,9.24692549325404,
-2.31080014678543));
#458726=CARTESIAN_POINT('Ctrl Pts',(-2.79931196839583,9.40515634302917,
0.0658967750008794));
#458727=CARTESIAN_POINT('Ctrl Pts',(-1.47092077043804,9.56338719280431,
2.3826753312679));
#458728=CARTESIAN_POINT('Ctrl Pts',(1.19560054382884,9.72161804257944,2.53202568228086));
#458729=CARTESIAN_POINT('Ctrl Pts',(2.77432456977243,9.87984889235458,0.378228478498683));
#458730=CARTESIAN_POINT('Ctrl Pts',(1.82984703080485,10.0380797421297,-2.11979382621544));
#458731=CARTESIAN_POINT('Ctrl Pts',(-0.779986135697901,10.1963105919048,
-2.6892298987944));
#458732=CARTESIAN_POINT('Ctrl Pts',(-2.67867033715473,10.35454144168,-0.813070561073652));
#458733=CARTESIAN_POINT('Ctrl Pts',(-2.14391551757544,10.5127722914551,
1.80393130824076));
#458734=CARTESIAN_POINT('Ctrl Pts',(0.347474390109052,10.6710031412303,
2.77757877131235));
#458735=CARTESIAN_POINT('Ctrl Pts',(1.78766388536965,10.7764903744137,1.74563481460802));
#458736=CARTESIAN_POINT('Ctrl Pts',(2.13201587949045,10.8292339910054,1.03908919352506));
#458737=CARTESIAN_POINT('',(2.64462557919716,10.5,1.28892185405325));
#458738=CARTESIAN_POINT('Ctrl Pts',(-1.93352775451079,10.5,1.37997672390732));
#458739=CARTESIAN_POINT('Ctrl Pts',(-1.90293201992144,10.5,1.43627785405326));
#458740=CARTESIAN_POINT('Ctrl Pts',(-1.86999681433948,10.5,1.49111021602056));
#458741=CARTESIAN_POINT('Ctrl Pts',(-1.8347651050013,10.5,1.5443101900256));
#458742=CARTESIAN_POINT('Ctrl Pts',(-1.7900193777493,10.5,1.61187635616855));
#458743=CARTESIAN_POINT('Ctrl Pts',(-1.74157148575129,10.5,1.6768108101035));
#458744=CARTESIAN_POINT('Ctrl Pts',(-1.68978892437989,10.5,1.73904025834759));
#458745=CARTESIAN_POINT('Ctrl Pts',(-1.63668135242531,10.5,1.80286203179394));
#458746=CARTESIAN_POINT('Ctrl Pts',(-1.58006586614171,10.5,1.86383915010342));
#458747=CARTESIAN_POINT('Ctrl Pts',(-1.52028803521347,10.5,1.92187250786994));
#458748=CARTESIAN_POINT('Ctrl Pts',(-1.48972286756875,10.5,1.95154570412974));
#458749=CARTESIAN_POINT('Ctrl Pts',(-1.45833016372759,10.5,1.98044891066153));
#458750=CARTESIAN_POINT('Ctrl Pts',(-1.42615174940177,10.5,2.0085661977242));
#458751=CARTESIAN_POINT('Ctrl Pts',(-1.40036665218304,10.5,2.03109704629544));
#458752=CARTESIAN_POINT('Ctrl Pts',(-1.37407698425746,10.5,2.05312321691266));
#458753=CARTESIAN_POINT('Ctrl Pts',(-1.34730309531695,10.5,2.07463552167975));
#458754=CARTESIAN_POINT('Ctrl Pts',(-1.33461070247932,10.5,2.0848336151862));
#458755=CARTESIAN_POINT('Ctrl Pts',(-1.32180757375966,10.5,2.09491754969286));
#458756=CARTESIAN_POINT('Ctrl Pts',(-1.308914368549,10.5,2.10487233321642));
#458757=CARTESIAN_POINT('Ctrl Pts',(-1.24034243428984,10.5,2.15781640338273));
#458758=CARTESIAN_POINT('Ctrl Pts',(-1.16911897693905,10.5,2.20719752107313));
#458759=CARTESIAN_POINT('Ctrl Pts',(-1.09564307477449,10.5,2.25293032857407));
#458760=CARTESIAN_POINT('Ctrl Pts',(-1.02066177812422,10.5,2.2996001224093));
#458761=CARTESIAN_POINT('Ctrl Pts',(-0.943334175939478,10.5,2.34247120277103));
#458762=CARTESIAN_POINT('Ctrl Pts',(-0.86403728996427,10.5,2.38142443284025));
#458763=CARTESIAN_POINT('Ctrl Pts',(-0.784119794595999,10.5,2.42068252658947));
#458764=CARTESIAN_POINT('Ctrl Pts',(-0.70220127611034,10.5,2.45596182783755));
#458765=CARTESIAN_POINT('Ctrl Pts',(-0.618631206215791,10.5,2.48710241424406));
#458766=CARTESIAN_POINT('Ctrl Pts',(-0.58008069536278,10.5,2.50146743171679));
#458767=CARTESIAN_POINT('Ctrl Pts',(-0.541178311910448,10.5,2.51495117139024));
#458768=CARTESIAN_POINT('Ctrl Pts',(-0.50195650947317,10.5,2.52753467091725));
#458769=CARTESIAN_POINT('Ctrl Pts',(-0.48835256408482,10.5,2.53189921384292));
#458770=CARTESIAN_POINT('Ctrl Pts',(-0.474708349225656,10.5,2.53615599028542));
#458771=CARTESIAN_POINT('Ctrl Pts',(-0.461031006634646,10.5,2.54030238856025));
#458772=CARTESIAN_POINT('Ctrl Pts',(-0.373267658314182,10.5,2.56690856542884));
#458773=CARTESIAN_POINT('Ctrl Pts',(-0.284440130000807,10.5,2.58888438978311));
#458774=CARTESIAN_POINT('Ctrl Pts',(-0.194951403411607,10.5,2.60611557525187));
#458775=CARTESIAN_POINT('Ctrl Pts',(-0.105531652285557,10.5,2.6233334793941));
#458776=CARTESIAN_POINT('Ctrl Pts',(-0.0154508240420797,10.5,2.6358146085091));
#458777=CARTESIAN_POINT('Ctrl Pts',(0.0749205728510989,10.5,2.64340437315386));
#458778=CARTESIAN_POINT('Ctrl Pts',(0.159385537871289,10.5,2.65049809115834));
#458779=CARTESIAN_POINT('Ctrl Pts',(0.244105219500255,10.5,2.65331892769926));
#458780=CARTESIAN_POINT('Ctrl Pts',(0.328791547014414,10.5,2.65170207915546));
#458781=CARTESIAN_POINT('Ctrl Pts',(0.386691905404672,10.5,2.65059663376779));
#458782=CARTESIAN_POINT('Ctrl Pts',(0.444576952017961,10.5,2.64741597427053));
#458783=CARTESIAN_POINT('Ctrl Pts',(0.50237517897069,10.5,2.6422151318513));
#458784=CARTESIAN_POINT('Ctrl Pts',(0.517071391465386,10.5,2.64089272648743));
#458785=CARTESIAN_POINT('Ctrl Pts',(0.531764255669784,10.5,2.63943941820881));
#458786=CARTESIAN_POINT('Ctrl Pts',(0.546445335927502,10.5,2.63785680672043));
#458787=CARTESIAN_POINT('Ctrl Pts',(0.634756839225468,10.5,2.62833688058269));
#458788=CARTESIAN_POINT('Ctrl Pts',(0.72238701460618,10.5,2.61417128734121));
#458789=CARTESIAN_POINT('Ctrl Pts',(0.809073285620467,10.5,2.59564699272082));
#458790=CARTESIAN_POINT('Ctrl Pts',(0.898022133870498,10.5,2.57663920000061));
#458791=CARTESIAN_POINT('Ctrl Pts',(0.985977806866194,10.5,2.5530421492732));
#458792=CARTESIAN_POINT('Ctrl Pts',(1.07266667384712,10.5,2.52511233750083));
#458793=CARTESIAN_POINT('Ctrl Pts',(1.16137627943129,10.5,2.49653147501346));
#458794=CARTESIAN_POINT('Ctrl Pts',(1.24876012389857,10.5,2.46341338432988));
#458795=CARTESIAN_POINT('Ctrl Pts',(1.33452430658295,10.5,2.42597895074645));
#458796=CARTESIAN_POINT('Ctrl Pts',(1.37056793894989,10.5,2.41024659115631));
#458797=CARTESIAN_POINT('Ctrl Pts',(1.40632542467597,10.5,2.39375123674891));
#458798=CARTESIAN_POINT('Ctrl Pts',(1.4417743760889,10.5,2.37650662292701));
#458799=CARTESIAN_POINT('Ctrl Pts',(1.46835581178172,10.5,2.36357573004911));
#458800=CARTESIAN_POINT('Ctrl Pts',(1.4947637585459,10.5,2.35022351391824));
#458801=CARTESIAN_POINT('Ctrl Pts',(1.52098857002974,10.5,2.33645521781124));
#458802=CARTESIAN_POINT('Ctrl Pts',(1.53874837765608,10.5,2.32713113590684));
#458803=CARTESIAN_POINT('Ctrl Pts',(1.55642762364687,10.5,2.31761420582139));
#458804=CARTESIAN_POINT('Ctrl Pts',(1.57399925430577,10.5,2.30791954956832));
#458805=CARTESIAN_POINT('Ctrl Pts',(1.65834800744353,10.5,2.26138248178446));
#458806=CARTESIAN_POINT('Ctrl Pts',(1.74032231269373,10.5,2.21070143831119));
#458807=CARTESIAN_POINT('Ctrl Pts',(1.8196162721435,10.5,2.1561363350773));
#458808=CARTESIAN_POINT('Ctrl Pts',(1.90241205938819,10.5,2.09916149475293));
#458809=CARTESIAN_POINT('Ctrl Pts',(1.98228663119651,10.5,2.0379519202785));
#458810=CARTESIAN_POINT('Ctrl Pts',(2.0588767137448,10.5,1.97274604914905));
#458811=CARTESIAN_POINT('Ctrl Pts',(2.08337669125452,10.5,1.95188770400801));
#458812=CARTESIAN_POINT('Ctrl Pts',(2.10754039794249,10.5,1.93062001288887));
#458813=CARTESIAN_POINT('Ctrl Pts',(2.13135533939967,10.5,1.9089496329668));
#458814=CARTESIAN_POINT('Ctrl Pts',(2.14903233282523,10.5,1.89286447214032));
#458815=CARTESIAN_POINT('Ctrl Pts',(2.16652058329141,10.5,1.87655399116408));
#458816=CARTESIAN_POINT('Ctrl Pts',(2.1837933420161,10.5,1.8600418161316));
#458817=CARTESIAN_POINT('Ctrl Pts',(2.25538660784956,10.5,1.79160106758462));
#458818=CARTESIAN_POINT('Ctrl Pts',(2.3233458434253,10.5,1.7196411993018));
#458819=CARTESIAN_POINT('Ctrl Pts',(2.38734368950084,10.5,1.64440308592963));
#458820=CARTESIAN_POINT('Ctrl Pts',(2.45054268378508,10.5,1.57010413075304));
#458821=CARTESIAN_POINT('Ctrl Pts',(2.50987939302537,10.5,1.49260775548549));
#458822=CARTESIAN_POINT('Ctrl Pts',(2.56501263411554,10.5,1.41210300451611));
#458823=CARTESIAN_POINT('Ctrl Pts',(2.59262019869487,10.5,1.37179084315241));
#458824=CARTESIAN_POINT('Ctrl Pts',(2.61917328752526,10.5,1.3307237227593));
#458825=CARTESIAN_POINT('Ctrl Pts',(2.64462557919716,10.5,1.28892185405325));
#458826=CARTESIAN_POINT('Ctrl Pts',(2.64824696753858,4.5,1.29202795241196));
#458827=CARTESIAN_POINT('Ctrl Pts',(2.60771714947459,4.5,1.35933351652819));
#458828=CARTESIAN_POINT('Ctrl Pts',(2.56441754363406,4.5,1.4247383756481));
#458829=CARTESIAN_POINT('Ctrl Pts',(2.51834950574105,4.5,1.48805165137538));
#458830=CARTESIAN_POINT('Ctrl Pts',(2.46163624014362,4.5,1.56599511904605));
#458831=CARTESIAN_POINT('Ctrl Pts',(2.40072794333669,4.5,1.64077012114675));
#458832=CARTESIAN_POINT('Ctrl Pts',(2.33600323974202,4.5,1.71222803280316));
#458833=CARTESIAN_POINT('Ctrl Pts',(2.27034046414919,4.5,1.78472160259702));
#458834=CARTESIAN_POINT('Ctrl Pts',(2.20074894713909,4.5,1.85380170291241));
#458835=CARTESIAN_POINT('Ctrl Pts',(2.12759467457488,4.5,1.91926900677611));
#458836=CARTESIAN_POINT('Ctrl Pts',(2.05934815866359,4.5,1.98034425553731));
#458837=CARTESIAN_POINT('Ctrl Pts',(1.98799997724039,4.5,2.03827501857495));
#458838=CARTESIAN_POINT('Ctrl Pts',(1.9138354360245,4.5,2.09286030382211));
#458839=CARTESIAN_POINT('Ctrl Pts',(1.8991298360776,4.5,2.1036836616515));
#458840=CARTESIAN_POINT('Ctrl Pts',(1.88431062863931,4.5,2.11437726788929));
#458841=CARTESIAN_POINT('Ctrl Pts',(1.86940119048916,4.5,2.12492474377812));
#458842=CARTESIAN_POINT('Ctrl Pts',(1.7910113621017,4.5,2.18038054409198));
#458843=CARTESIAN_POINT('Ctrl Pts',(1.71001841492429,4.5,2.23188440715045));
#458844=CARTESIAN_POINT('Ctrl Pts',(1.62678720374559,4.5,2.27928519947701));
#458845=CARTESIAN_POINT('Ctrl Pts',(1.54383307892295,4.5,2.32652818906787));
#458846=CARTESIAN_POINT('Ctrl Pts',(1.45865460208077,4.5,2.36969567302112));
#458847=CARTESIAN_POINT('Ctrl Pts',(1.37159569544087,4.5,2.40858963785122));
#458848=CARTESIAN_POINT('Ctrl Pts',(1.2860439028092,4.5,2.4468102926032));
#458849=CARTESIAN_POINT('Ctrl Pts',(1.19867534555845,4.5,2.48090425803352));
#458850=CARTESIAN_POINT('Ctrl Pts',(1.10981329910479,4.5,2.51063375573629));
#458851=CARTESIAN_POINT('Ctrl Pts',(1.06957239483518,4.5,2.52409666728047));
#458852=CARTESIAN_POINT('Ctrl Pts',(1.02902525693667,4.5,2.53666385768734));
#458853=CARTESIAN_POINT('Ctrl Pts',(0.988202414126667,4.5,2.54830966602011));
#458854=CARTESIAN_POINT('Ctrl Pts',(0.970015193399782,4.5,2.55349805742334));
#458855=CARTESIAN_POINT('Ctrl Pts',(0.951773256351282,4.5,2.55850353846662));
#458856=CARTESIAN_POINT('Ctrl Pts',(0.933479340954419,4.5,2.5633236911305));
#458857=CARTESIAN_POINT('Ctrl Pts',(0.919785355999881,4.5,2.56693183605878));
#458858=CARTESIAN_POINT('Ctrl Pts',(0.906062449265792,4.5,2.57043600510489));
#458859=CARTESIAN_POINT('Ctrl Pts',(0.892325601918445,4.5,2.57383196727938));
#458860=CARTESIAN_POINT('Ctrl Pts',(0.803235023294982,4.5,2.59585654303964));
#458861=CARTESIAN_POINT('Ctrl Pts',(0.713411057690886,4.5,2.61337345925915));
#458862=CARTESIAN_POINT('Ctrl Pts',(0.623166686713777,4.5,2.62620752424572));
#458863=CARTESIAN_POINT('Ctrl Pts',(0.535509189698101,4.5,2.63867369804779));
#458864=CARTESIAN_POINT('Ctrl Pts',(0.447454292914566,4.5,2.64672162951279));
#458865=CARTESIAN_POINT('Ctrl Pts',(0.359291645228602,4.5,2.65014276565555));
#458866=CARTESIAN_POINT('Ctrl Pts',(0.277156330183277,4.5,2.65333001220807));
#458867=CARTESIAN_POINT('Ctrl Pts',(0.194927065717652,4.5,2.65250115242705));
#458868=CARTESIAN_POINT('Ctrl Pts',(0.112848583223775,4.5,2.6474481553123));
#458869=CARTESIAN_POINT('Ctrl Pts',(0.0625995065854971,4.5,2.64435467171517));
#458870=CARTESIAN_POINT('Ctrl Pts',(0.0124071748506151,4.5,2.63967707697624));
#458871=CARTESIAN_POINT('Ctrl Pts',(-0.0376686571506802,4.5,2.63344177754326));
#458872=CARTESIAN_POINT('Ctrl Pts',(-0.054260435162054,4.5,2.63137581678151));
#458873=CARTESIAN_POINT('Ctrl Pts',(-0.0708394004908746,4.5,2.62913881817626));
#458874=CARTESIAN_POINT('Ctrl Pts',(-0.0874033066697733,4.5,2.62673165442483));
#458875=CARTESIAN_POINT('Ctrl Pts',(-0.10199693768225,4.5,2.62461082258749));
#458876=CARTESIAN_POINT('Ctrl Pts',(-0.116580014851888,4.5,2.62235762930158));
#458877=CARTESIAN_POINT('Ctrl Pts',(-0.131133790593703,4.5,2.61997571054922));
#458878=CARTESIAN_POINT('Ctrl Pts',(-0.218834447725095,4.5,2.60562233287448));
#458879=CARTESIAN_POINT('Ctrl Pts',(-0.305617184281958,4.5,2.58657904245835));
#458880=CARTESIAN_POINT('Ctrl Pts',(-0.391183164324067,4.5,2.56307793284766));
#458881=CARTESIAN_POINT('Ctrl Pts',(-0.477472281209514,4.5,2.53937821021098));
#458882=CARTESIAN_POINT('Ctrl Pts',(-0.562524840120038,4.5,2.5111444090929));
#458883=CARTESIAN_POINT('Ctrl Pts',(-0.64601149379796,4.5,2.47856640462203));
#458884=CARTESIAN_POINT('Ctrl Pts',(-0.728597897145357,4.5,2.4463396941365));
#458885=CARTESIAN_POINT('Ctrl Pts',(-0.809652699324017,4.5,2.40986127665925));
#458886=CARTESIAN_POINT('Ctrl Pts',(-0.888823239576293,4.5,2.36927780216127));
#458887=CARTESIAN_POINT('Ctrl Pts',(-0.937945665329352,4.5,2.34409723996635));
#458888=CARTESIAN_POINT('Ctrl Pts',(-0.986341987732194,4.5,2.31733564127829));
#458889=CARTESIAN_POINT('Ctrl Pts',(-1.03391949521965,4.5,2.28902244361092));
#458890=CARTESIAN_POINT('Ctrl Pts',(-1.07798620625875,4.5,2.2627985078461));
#458891=CARTESIAN_POINT('Ctrl Pts',(-1.12124270740235,4.49999999999929,
2.23530765586229));
#458892=CARTESIAN_POINT('Ctrl Pts',(-1.16362616052922,4.49999999999893,
2.20658584552865));
#458893=CARTESIAN_POINT('Ctrl Pts',(2.64462557919715,10.5,1.28892185405327));
#458894=CARTESIAN_POINT('Ctrl Pts',(2.21747956182456,10.4472563834083,2.16534526175899));
#458895=CARTESIAN_POINT('Ctrl Pts',(1.32424935310596,10.3945127668166,2.80537459044542));
#458896=CARTESIAN_POINT('Ctrl Pts',(0.36256667498553,10.3417691502249,2.92409830672941));
#458897=CARTESIAN_POINT('Ctrl Pts',(-0.599116003134894,10.2890255336332,
3.0428220230134));
#458898=CARTESIAN_POINT('Ctrl Pts',(-1.62925115065715,10.2362819170414,
2.64024012689497));
#458899=CARTESIAN_POINT('Ctrl Pts',(-2.25487342588359,10.1835383004497,
1.89791270790901));
#458900=CARTESIAN_POINT('Ctrl Pts',(-2.88049570111003,10.130794683858,1.15558528892306));
#458901=CARTESIAN_POINT('Ctrl Pts',(-3.10160510404067,10.0780510672663,
0.0735123470695868));
#458902=CARTESIAN_POINT('Ctrl Pts',(-2.81962764425474,10.0253074506746,
-0.85539951625899));
#458903=CARTESIAN_POINT('Ctrl Pts',(-2.5376501844688,9.97256383408289,-1.78431137958758));
#458904=CARTESIAN_POINT('Ctrl Pts',(-1.75258586196629,9.91982021749118,
-2.56006216439127));
#458905=CARTESIAN_POINT('Ctrl Pts',(-0.820499280571597,9.86707660089946,
-2.83021288615418));
#458906=CARTESIAN_POINT('Ctrl Pts',(-0.556005103129074,9.85210977296284,
-2.90687238792629));
#458907=CARTESIAN_POINT('Ctrl Pts',(-0.279672258506851,9.83714294502622,
-2.94281947705097));
#458908=CARTESIAN_POINT('Ctrl Pts',(-0.00272715277824687,9.82217611708959,
-2.94049646102293));
#458909=CARTESIAN_POINT('Origin',(3.,4.5,0.));
#458910=CARTESIAN_POINT('',(-3.06161699786838E-16,4.5,-2.5));
#458911=CARTESIAN_POINT('Origin',(0.,4.5,0.));
#458912=CARTESIAN_POINT('Origin',(0.,4.5,0.));
#458913=CARTESIAN_POINT('Origin',(1.5,10.5,0.));
#458914=CARTESIAN_POINT('Origin',(0.,10.5,0.));
#458915=CARTESIAN_POINT('',(-1.83697019872103E-16,10.5,-1.5));
#458916=CARTESIAN_POINT('Origin',(0.,10.5,0.));
#458917=CARTESIAN_POINT('Origin',(0.,3.,0.));
#458918=CARTESIAN_POINT('Origin',(0.,-0.227272727272729,0.));
#458919=CARTESIAN_POINT('',(-9.18485099360515E-17,-0.227272727272729,-0.75));
#458920=CARTESIAN_POINT('Origin',(0.,-0.227272727272729,0.));
#458921=CARTESIAN_POINT('',(-1.22464679914735E-16,-1.70002900645727E-15,
-1.));
#458922=CARTESIAN_POINT('',(-9.18485099360515E-17,-0.227272727272729,-0.75));
#458923=CARTESIAN_POINT('',(1.22464679914735E-16,-1.73472347597681E-15,
1.));
#458924=CARTESIAN_POINT('Origin',(0.,-1.73472347597681E-15,0.));
#458925=CARTESIAN_POINT('Origin',(0.,-1.73472347597681E-15,0.));
#458926=CARTESIAN_POINT('Origin',(0.,3.,0.));
#458927=CARTESIAN_POINT('',(-9.18485099360515E-17,-0.700000000000002,-0.75));
#458928=CARTESIAN_POINT('Origin',(0.,-0.700000000000002,0.));
#458929=CARTESIAN_POINT('',(-9.18485099360515E-17,3.,-0.75));
#458930=CARTESIAN_POINT('Origin',(0.,-1.2,0.));
#458931=CARTESIAN_POINT('',(-2.44929359829471E-17,-1.2,-0.2));
#458932=CARTESIAN_POINT('Origin',(0.,-1.2,0.));
#458933=CARTESIAN_POINT('',(-2.44929359829471E-17,-1.2,-0.2));
#458934=CARTESIAN_POINT('Origin',(0.,-2.,0.));
#458935=CARTESIAN_POINT('',(-3.06161699786837E-16,2.77555756156289E-16,
-2.49999999999999));
#458936=CARTESIAN_POINT('Origin',(0.,0.,0.));
#458937=CARTESIAN_POINT('',(-6.12323399573677E-17,-2.,-0.5));
#458938=CARTESIAN_POINT('',(-6.12323399573677E-17,-2.,-0.5));
#458939=CARTESIAN_POINT('Origin',(0.,-2.,0.));
#458940=CARTESIAN_POINT('Origin',(0.,3.,0.));
#458941=CARTESIAN_POINT('',(-3.06161699786838E-16,3.,-2.5));
#458942=CARTESIAN_POINT('',(-3.06161699786838E-16,3.,-2.5));
#458943=CARTESIAN_POINT('Origin',(0.,3.,0.));
#458944=CARTESIAN_POINT('Origin',(0.,10.5,0.));
#458945=CARTESIAN_POINT('',(1.22464679914735E-16,10.,1.));
#458946=CARTESIAN_POINT('',(-1.22464679914735E-16,10.,-1.));
#458947=CARTESIAN_POINT('Origin',(0.,10.,0.));
#458948=CARTESIAN_POINT('Origin',(0.,10.,0.));
#458949=CARTESIAN_POINT('',(-1.83697019872103E-16,10.5,-1.5));
#458950=CARTESIAN_POINT('Origin',(0.,3.,0.));
#458951=CARTESIAN_POINT('',(-1.22464679914735E-16,3.,1.));
#458952=CARTESIAN_POINT('Origin',(0.,3.,0.));
#458953=CARTESIAN_POINT('',(-2.44929359829471E-17,-2.,-0.2));
#458954=CARTESIAN_POINT('Origin',(0.,-2.,0.));
#458955=CARTESIAN_POINT('',(-2.44929359829471E-17,3.,-0.2));
#458956=CARTESIAN_POINT('Origin',(0.,0.,0.));
#458957=CARTESIAN_POINT('',(-2.02072594216369,0.,3.5));
#458958=CARTESIAN_POINT('',(2.02072594216369,0.,3.5));
#458959=CARTESIAN_POINT('',(-2.02072594216369,0.,3.5));
#458960=CARTESIAN_POINT('',(-4.04145188432738,0.,1.02894934683325E-15));
#458961=CARTESIAN_POINT('',(-4.04145188432738,0.,1.02894934683325E-15));
#458962=CARTESIAN_POINT('',(-2.02072594216369,0.,-3.5));
#458963=CARTESIAN_POINT('',(-2.02072594216369,0.,-3.5));
#458964=CARTESIAN_POINT('',(2.02072594216369,0.,-3.5));
#458965=CARTESIAN_POINT('',(2.02072594216369,0.,-3.5));
#458966=CARTESIAN_POINT('',(4.04145188432738,0.,-3.74163398848454E-16));
#458967=CARTESIAN_POINT('',(4.04145188432738,0.,-3.74163398848454E-16));
#458968=CARTESIAN_POINT('',(2.02072594216369,0.,3.5));
#458969=CARTESIAN_POINT('Origin',(0.,3.,0.));
#458970=CARTESIAN_POINT('',(-2.02072594216369,3.,3.5));
#458971=CARTESIAN_POINT('',(2.02072594216369,3.,3.5));
#458972=CARTESIAN_POINT('',(-2.02072594216369,3.,3.5));
#458973=CARTESIAN_POINT('',(4.04145188432738,3.,-3.74163398848454E-16));
#458974=CARTESIAN_POINT('',(2.02072594216369,3.,3.5));
#458975=CARTESIAN_POINT('',(2.02072594216369,3.,-3.5));
#458976=CARTESIAN_POINT('',(4.04145188432738,3.,-3.74163398848454E-16));
#458977=CARTESIAN_POINT('',(-2.02072594216369,3.,-3.5));
#458978=CARTESIAN_POINT('',(2.02072594216369,3.,-3.5));
#458979=CARTESIAN_POINT('',(-4.04145188432738,3.,1.02894934683325E-15));
#458980=CARTESIAN_POINT('',(-2.02072594216369,3.,-3.5));
#458981=CARTESIAN_POINT('',(-4.04145188432738,3.,1.02894934683325E-15));
#458982=CARTESIAN_POINT('Origin',(-2.02072594216369,3.,3.5));
#458983=CARTESIAN_POINT('',(2.02072594216369,3.,3.5));
#458984=CARTESIAN_POINT('',(-2.02072594216369,3.,3.5));
#458985=CARTESIAN_POINT('Origin',(2.02072594216369,3.,3.5));
#458986=CARTESIAN_POINT('',(4.04145188432738,3.,-3.74163398848454E-16));
#458987=CARTESIAN_POINT('Origin',(4.04145188432738,3.,-3.74163398848454E-16));
#458988=CARTESIAN_POINT('',(2.02072594216369,3.,-3.5));
#458989=CARTESIAN_POINT('Origin',(2.02072594216369,3.,-3.5));
#458990=CARTESIAN_POINT('',(-2.02072594216369,3.,-3.5));
#458991=CARTESIAN_POINT('Origin',(-2.02072594216369,3.,-3.5));
#458992=CARTESIAN_POINT('',(-4.04145188432738,3.,1.02894934683325E-15));
#458993=CARTESIAN_POINT('Origin',(-4.04145188432738,3.,1.02894934683325E-15));
#458994=CARTESIAN_POINT('Origin',(0.2,-2.,0.));
#458995=CARTESIAN_POINT('',(0.,0.,0.));
#458996=CARTESIAN_POINT('Origin',(5.50000000000001,0.,-6.93889390390723E-15));
#458997=CARTESIAN_POINT('',(5.50000000000001,0.,-3.00000000000001));
#458998=CARTESIAN_POINT('Origin',(5.50000000000001,0.,-6.93889390390723E-15));
#458999=CARTESIAN_POINT('',(5.50000000000001,11.5,-3.00000000000001));
#459000=CARTESIAN_POINT('',(5.50000000000001,0.,-3.00000000000001));
#459001=CARTESIAN_POINT('Origin',(5.50000000000001,11.5,-6.93889390390723E-15));
#459002=CARTESIAN_POINT('Origin',(-7.5,0.,-6.93889390390723E-15));
#459003=CARTESIAN_POINT('',(-7.5,0.,-1.50000000000001));
#459004=CARTESIAN_POINT('Origin',(-7.5,0.,-6.93889390390723E-15));
#459005=CARTESIAN_POINT('',(-7.5,3.5,-1.50000000000001));
#459006=CARTESIAN_POINT('',(-7.5,0.,-1.50000000000001));
#459007=CARTESIAN_POINT('Origin',(-7.5,3.5,-6.93889390390723E-15));
#459008=CARTESIAN_POINT('Origin',(-7.5,0.,-6.93889390390723E-15));
#459009=CARTESIAN_POINT('',(-7.5,4.5,-1.50000000000001));
#459010=CARTESIAN_POINT('Origin',(-7.5,4.5,-6.93889390390723E-15));
#459011=CARTESIAN_POINT('',(-7.5,11.5,-1.50000000000001));
#459012=CARTESIAN_POINT('',(-7.5,0.,-1.50000000000001));
#459013=CARTESIAN_POINT('Origin',(-7.5,11.5,-6.93889390390723E-15));
#459014=CARTESIAN_POINT('Origin',(8.00000000000001,2.,3.49999999999999));
#459015=CARTESIAN_POINT('',(7.25000000000001,2.,3.49999999999999));
#459016=CARTESIAN_POINT('Origin',(8.00000000000001,2.,3.49999999999999));
#459017=CARTESIAN_POINT('',(7.25000000000001,2.,7.99999999999999));
#459018=CARTESIAN_POINT('',(7.25000000000001,2.,3.49999999999999));
#459019=CARTESIAN_POINT('Origin',(8.00000000000001,2.,7.99999999999999));
#459020=CARTESIAN_POINT('Origin',(6.50000000000001,4.8,4.49999999999999));
#459021=CARTESIAN_POINT('',(5.00000000000001,4.8,4.49999999999999));
#459022=CARTESIAN_POINT('Origin',(6.50000000000001,4.8,4.49999999999999));
#459023=CARTESIAN_POINT('',(5.00000000000001,4.8,7.99999999999999));
#459024=CARTESIAN_POINT('',(5.00000000000001,4.8,4.49999999999999));
#459025=CARTESIAN_POINT('Origin',(6.50000000000001,4.8,7.99999999999999));
#459026=CARTESIAN_POINT('Origin',(-1.49999999999999,4.,-8.00000000000001));
#459027=CARTESIAN_POINT('',(-4.4580398915498,3.5,-8.00000000000001));
#459028=CARTESIAN_POINT('',(-4.4580398915498,4.5,-8.00000000000001));
#459029=CARTESIAN_POINT('Origin',(-1.49999999999999,4.,-8.00000000000001));
#459030=CARTESIAN_POINT('',(-4.4580398915498,3.5,7.99999999999999));
#459031=CARTESIAN_POINT('',(-4.4580398915498,3.5,-8.00000000000001));
#459032=CARTESIAN_POINT('',(-4.4580398915498,4.5,7.99999999999999));
#459033=CARTESIAN_POINT('Origin',(-1.49999999999999,4.,7.99999999999999));
#459034=CARTESIAN_POINT('',(-4.4580398915498,4.5,-8.00000000000001));
#459035=CARTESIAN_POINT('Origin',(-10.,11.5,-8.00000000000001));
#459036=CARTESIAN_POINT('',(-10.,0.249999999999997,-7.75000000000001));
#459037=CARTESIAN_POINT('',(-10.,0.249999999999997,7.74999999999999));
#459038=CARTESIAN_POINT('',(-10.,0.249999999999997,-8.00000000000001));
#459039=CARTESIAN_POINT('',(-10.,3.5,7.74999999999999));
#459040=CARTESIAN_POINT('',(-10.,11.5,7.74999999999999));
#459041=CARTESIAN_POINT('',(-10.,3.5,-7.75000000000001));
#459042=CARTESIAN_POINT('',(-10.,3.5,-8.00000000000001));
#459043=CARTESIAN_POINT('',(-10.,11.5,-7.75000000000001));
#459044=CARTESIAN_POINT('Origin',(-10.,11.5,-8.00000000000001));
#459045=CARTESIAN_POINT('',(-10.,4.5,-7.75000000000001));
#459046=CARTESIAN_POINT('',(-10.,4.5,7.74999999999999));
#459047=CARTESIAN_POINT('',(-10.,4.5,-8.00000000000001));
#459048=CARTESIAN_POINT('',(-10.,11.25,7.74999999999999));
#459049=CARTESIAN_POINT('',(-10.,11.5,7.74999999999999));
#459050=CARTESIAN_POINT('',(-10.,11.25,-7.75000000000001));
#459051=CARTESIAN_POINT('',(-10.,11.25,-8.00000000000001));
#459052=CARTESIAN_POINT('',(-10.,11.5,-7.75000000000001));
#459053=CARTESIAN_POINT('Origin',(-10.,11.5,7.99999999999999));
#459054=CARTESIAN_POINT('',(-9.75,3.5,7.99999999999999));
#459055=CARTESIAN_POINT('',(-10.,3.5,7.99999999999999));
#459056=CARTESIAN_POINT('',(-9.75,0.249999999999997,7.99999999999999));
#459057=CARTESIAN_POINT('',(-9.75,11.5,7.99999999999999));
#459058=CARTESIAN_POINT('',(9.75000000000001,0.249999999999997,7.99999999999999));
#459059=CARTESIAN_POINT('',(-10.,0.249999999999997,7.99999999999999));
#459060=CARTESIAN_POINT('',(9.75000000000001,11.25,7.99999999999999));
#459061=CARTESIAN_POINT('',(9.75000000000001,11.5,7.99999999999999));
#459062=CARTESIAN_POINT('',(-9.75,11.25,7.99999999999999));
#459063=CARTESIAN_POINT('',(-10.,11.25,7.99999999999999));
#459064=CARTESIAN_POINT('',(-9.75,4.5,7.99999999999999));
#459065=CARTESIAN_POINT('',(-9.75,11.5,7.99999999999999));
#459066=CARTESIAN_POINT('',(-4.4580398915498,4.5,7.99999999999999));
#459067=CARTESIAN_POINT('Origin',(10.,11.5,-8.00000000000001));
#459068=CARTESIAN_POINT('',(10.,11.25,-7.75000000000001));
#459069=CARTESIAN_POINT('',(10.,11.25,7.75));
#459070=CARTESIAN_POINT('',(10.,11.25,7.99999999999999));
#459071=CARTESIAN_POINT('',(10.,0.249999999999997,7.75));
#459072=CARTESIAN_POINT('',(10.,11.5,7.75));
#459073=CARTESIAN_POINT('',(10.,0.249999999999997,-7.75000000000001));
#459074=CARTESIAN_POINT('',(10.,0.249999999999997,-8.00000000000001));
#459075=CARTESIAN_POINT('',(10.,11.5,-7.75000000000001));
#459076=CARTESIAN_POINT('Origin',(-10.,11.5,-8.00000000000001));
#459077=CARTESIAN_POINT('',(9.75000000000001,0.249999999999997,-8.00000000000001));
#459078=CARTESIAN_POINT('',(-9.75,0.249999999999997,-8.00000000000001));
#459079=CARTESIAN_POINT('',(-10.,0.249999999999997,-8.00000000000001));
#459080=CARTESIAN_POINT('',(-9.75,3.5,-8.00000000000001));
#459081=CARTESIAN_POINT('',(-9.75,11.5,-8.00000000000001));
#459082=CARTESIAN_POINT('',(-10.,3.5,-8.00000000000001));
#459083=CARTESIAN_POINT('',(-9.75,4.5,-8.00000000000001));
#459084=CARTESIAN_POINT('',(-4.4580398915498,4.5,-8.00000000000001));
#459085=CARTESIAN_POINT('',(-9.75,11.25,-8.00000000000001));
#459086=CARTESIAN_POINT('',(-9.75,11.5,-8.00000000000001));
#459087=CARTESIAN_POINT('',(9.75000000000001,11.25,-8.00000000000001));
#459088=CARTESIAN_POINT('',(10.,11.25,-8.00000000000001));
#459089=CARTESIAN_POINT('',(9.75000000000001,11.5,-8.00000000000001));
#459090=CARTESIAN_POINT('Origin',(0.,11.5,0.));
#459091=CARTESIAN_POINT('',(-9.75,11.5,7.75));
#459092=CARTESIAN_POINT('',(9.75000000000001,11.5,7.75));
#459093=CARTESIAN_POINT('',(10.,11.5,7.75));
#459094=CARTESIAN_POINT('',(9.75000000000001,11.5,-7.75000000000001));
#459095=CARTESIAN_POINT('',(9.75000000000001,11.5,-8.00000000000001));
#459096=CARTESIAN_POINT('',(-9.75,11.5,-7.75000000000001));
#459097=CARTESIAN_POINT('',(-10.,11.5,-7.75000000000001));
#459098=CARTESIAN_POINT('',(-9.75,11.5,7.99999999999999));
#459099=CARTESIAN_POINT('Origin',(0.,0.,0.));
#459100=CARTESIAN_POINT('',(-9.74999999999999,0.,-7.75000000000001));
#459101=CARTESIAN_POINT('',(9.75,0.,-7.75000000000001));
#459102=CARTESIAN_POINT('',(0.,0.,-7.75000000000001));
#459103=CARTESIAN_POINT('',(9.75000000000001,0.,7.74999999999999));
#459104=CARTESIAN_POINT('',(9.75000000000001,0.,-2.11419423634673E-15));
#459105=CARTESIAN_POINT('',(-9.74999999999999,0.,7.74999999999999));
#459106=CARTESIAN_POINT('',(0.,0.,7.74999999999999));
#459107=CARTESIAN_POINT('',(-9.74999999999999,0.,1.05709711817337E-15));
#459108=CARTESIAN_POINT('Origin',(-10.,3.5,-8.00000000000001));
#459109=CARTESIAN_POINT('',(-9.75,3.5,7.99999999999999));
#459110=CARTESIAN_POINT('',(-10.,3.5,-7.75000000000001));
#459111=CARTESIAN_POINT('Origin',(-4.4580398915498,4.5,-8.00000000000001));
#459112=CARTESIAN_POINT('',(-9.75,4.5,7.99999999999999));
#459113=CARTESIAN_POINT('',(-10.,4.5,-7.75000000000001));
#459114=CARTESIAN_POINT('Origin',(6.50000000000001,4.8,4.49999999999999));
#459115=CARTESIAN_POINT('Origin',(8.00000000000001,2.,3.49999999999999));
#459116=CARTESIAN_POINT('Origin',(-10.,11.5,-7.75000000000001));
#459117=CARTESIAN_POINT('',(-9.75,11.25,-8.00000000000001));
#459118=CARTESIAN_POINT('Origin',(-10.,11.5,-7.75000000000001));
#459119=CARTESIAN_POINT('',(-10.,0.249999999999997,-7.75000000000001));
#459120=CARTESIAN_POINT('Origin',(-9.75,11.25,-8.00000000000001));
#459121=CARTESIAN_POINT('',(-9.75,11.25,-8.00000000000001));
#459122=CARTESIAN_POINT('',(-9.875,11.375,-7.75000000000001));
#459123=CARTESIAN_POINT('Origin',(-10.,0.249999999999997,-7.75000000000001));
#459124=CARTESIAN_POINT('',(-10.,0.249999999999997,-7.75000000000001));
#459125=CARTESIAN_POINT('',(-9.74999999999999,0.125,-7.87500000000001));
#459126=CARTESIAN_POINT('Origin',(-9.75,11.5,7.99999999999999));
#459127=CARTESIAN_POINT('',(-10.,11.25,7.74999999999999));
#459128=CARTESIAN_POINT('Origin',(-9.75,11.5,1.05709711817337E-15));
#459129=CARTESIAN_POINT('',(-10.,11.25,7.74999999999999));
#459130=CARTESIAN_POINT('Origin',(0.,11.5,-7.75000000000001));
#459131=CARTESIAN_POINT('',(9.75000000000001,11.5,-7.75000000000001));
#459132=CARTESIAN_POINT('Origin',(9.75000000000001,11.5,-8.00000000000001));
#459133=CARTESIAN_POINT('',(10.,0.249999999999997,-7.75000000000001));
#459134=CARTESIAN_POINT('',(9.87500000000001,11.25,-7.87500000000001));
#459135=CARTESIAN_POINT('Origin',(-10.,0.249999999999997,-8.00000000000001));
#459136=CARTESIAN_POINT('',(9.75000000000001,0.124999999999998,-7.87500000000001));
#459137=CARTESIAN_POINT('Origin',(-10.,0.249999999999997,-8.00000000000001));
#459138=CARTESIAN_POINT('',(-9.87499999999999,0.124999999999999,7.74999999999999));
#459139=CARTESIAN_POINT('Origin',(-9.75,11.5,7.99999999999999));
#459140=CARTESIAN_POINT('',(-9.75,0.249999999999997,7.99999999999999));
#459141=CARTESIAN_POINT('Origin',(-10.,11.25,7.74999999999999));
#459142=CARTESIAN_POINT('',(-9.75,11.375,7.875));
#459143=CARTESIAN_POINT('Origin',(9.75000000000001,11.5,-7.75000000000001));
#459144=CARTESIAN_POINT('',(9.75000000000001,11.5,-7.75000000000001));
#459145=CARTESIAN_POINT('Origin',(10.,0.249999999999997,-7.75000000000001));
#459146=CARTESIAN_POINT('',(10.,0.249999999999997,-7.75000000000001));
#459147=CARTESIAN_POINT('Origin',(-9.75,0.249999999999997,7.99999999999999));
#459148=CARTESIAN_POINT('',(-9.75,0.249999999999997,7.99999999999999));
#459149=CARTESIAN_POINT('Origin',(0.,11.5,7.75));
#459150=CARTESIAN_POINT('',(9.75000000000001,11.25,7.99999999999999));
#459151=CARTESIAN_POINT('Origin',(9.75000000000001,11.5,-2.11419423634674E-15));
#459152=CARTESIAN_POINT('',(9.87500000000001,11.375,7.75));
#459153=CARTESIAN_POINT('Origin',(10.,0.249999999999997,-8.00000000000001));
#459154=CARTESIAN_POINT('',(10.,0.249999999999997,7.75));
#459155=CARTESIAN_POINT('Origin',(-10.,0.249999999999997,7.99999999999999));
#459156=CARTESIAN_POINT('',(9.75000000000001,0.124999999999998,7.87499999999999));
#459157=CARTESIAN_POINT('Origin',(9.75000000000001,11.25,7.99999999999999));
#459158=CARTESIAN_POINT('',(9.75000000000001,11.25,7.99999999999999));
#459159=CARTESIAN_POINT('Origin',(10.,0.249999999999997,7.75));
#459160=CARTESIAN_POINT('',(10.,0.249999999999997,7.75));
#459161=CARTESIAN_POINT('Origin',(10.,11.5,7.75));
#459162=CARTESIAN_POINT('',(5.35200894938521E-16,1.73194791841524E-13,25.9999999999999));
#459163=CARTESIAN_POINT('',(-9.89335608677562E-15,9.32587340685131E-14,
33.0999999999999));
#459164=CARTESIAN_POINT('',(0.,0.,0.));
#459165=CARTESIAN_POINT('',(-9.84356169695829E-15,1.37667655053519E-13,
43.5999999999998));
#459166=CARTESIAN_POINT('',(3.75585139660399E-14,-5.49999999999994,28.0999999999999));
#459167=CARTESIAN_POINT('',(0.707106796050871,-5.99999999999995,-0.707106766322221));
#459168=CARTESIAN_POINT('',(3.36353395222894E-15,-18.2000000000001,13.));
#459169=CARTESIAN_POINT('',(0.,0.,0.));
#459170=CARTESIAN_POINT('',(15.1,-22.1000000000001,-15.1));
#459171=CARTESIAN_POINT('',(15.1,-1.4,-15.1));
#459172=CARTESIAN_POINT('',(-0.503120076364691,-118.215520572543,-19.1178367667898));
#459173=CARTESIAN_POINT('',(-9.35,-18.2,-3.050000000037));
#459174=CARTESIAN_POINT('',(18.0968799236353,-117.815520572543,-19.1178367667898));
#459175=CARTESIAN_POINT('',(-9.35,-16.2000000000001,-3.05000000003699));
#459176=CARTESIAN_POINT('',(9.25,-18.2,-3.050000000037));
#459177=CARTESIAN_POINT('',(-8.47750127826601,-18.0000000000001,10.5062825051013));
#459178=CARTESIAN_POINT('',(-8.47750127826606,-1.35,10.5062825051013));
#459179=CARTESIAN_POINT('',(9.25,-16.2000000000001,-3.050000000037));
#459180=CARTESIAN_POINT('',(29.5999999999996,-14.7,12.6999999999631));
#459181=CARTESIAN_POINT('',(-8.47750127826606,-16.7499999999999,10.5062825051013));
#459182=CARTESIAN_POINT('',(5.65685424949694,-12.5431457505076,-19.3998529783646));
#459183=CARTESIAN_POINT('',(15.5209938470448,-6.69999999999995,15.5209938470447));
#459184=CARTESIAN_POINT('',(-5.66314575050306,-12.5431457505076,-19.3998529783646));
#459185=CARTESIAN_POINT('',(5.65685424949694,-23.8631457505076,-19.3998529783646));
#459186=CARTESIAN_POINT('',(-5.66314575050306,-23.8631457505076,-19.3998529783646));
#459187=CARTESIAN_POINT('',(7.1,-14.8,10.2));
#459188=CARTESIAN_POINT('',(-15.5,-9.80000000000008,-15.5));
#459189=CARTESIAN_POINT('',(2.04697370165263E-15,-18.2,-19.1));
#459190=CARTESIAN_POINT('',(0.,0.,0.));
#459191=UNCERTAINTY_MEASURE_WITH_UNIT(LENGTH_MEASURE(0.01),#459243,
'DISTANCE_ACCURACY_VALUE',
'Maximum model space distance between geometric entities at asserted c
onnectivities');
#459192=UNCERTAINTY_MEASURE_WITH_UNIT(LENGTH_MEASURE(0.01),#459243,
'DISTANCE_ACCURACY_VALUE',
'Maximum model space distance between geometric entities at asserted c
onnectivities');
#459193=UNCERTAINTY_MEASURE_WITH_UNIT(LENGTH_MEASURE(0.01),#459243,
'DISTANCE_ACCURACY_VALUE',
'Maximum model space distance between geometric entities at asserted c
onnectivities');
#459194=UNCERTAINTY_MEASURE_WITH_UNIT(LENGTH_MEASURE(0.01),#459243,
'DISTANCE_ACCURACY_VALUE',
'Maximum model space distance between geometric entities at asserted c
onnectivities');
#459195=UNCERTAINTY_MEASURE_WITH_UNIT(LENGTH_MEASURE(0.01),#459243,
'DISTANCE_ACCURACY_VALUE',
'Maximum model space distance between geometric entities at asserted c
onnectivities');
#459196=UNCERTAINTY_MEASURE_WITH_UNIT(LENGTH_MEASURE(0.01),#459243,
'DISTANCE_ACCURACY_VALUE',
'Maximum model space distance between geometric entities at asserted c
onnectivities');
#459197=UNCERTAINTY_MEASURE_WITH_UNIT(LENGTH_MEASURE(0.01),#459243,
'DISTANCE_ACCURACY_VALUE',
'Maximum model space distance between geometric entities at asserted c
onnectivities');
#459198=UNCERTAINTY_MEASURE_WITH_UNIT(LENGTH_MEASURE(0.01),#459243,
'DISTANCE_ACCURACY_VALUE',
'Maximum model space distance between geometric entities at asserted c
onnectivities');
#459199=UNCERTAINTY_MEASURE_WITH_UNIT(LENGTH_MEASURE(0.01),#459243,
'DISTANCE_ACCURACY_VALUE',
'Maximum model space distance between geometric entities at asserted c
onnectivities');
#459200=UNCERTAINTY_MEASURE_WITH_UNIT(LENGTH_MEASURE(0.01),#459243,
'DISTANCE_ACCURACY_VALUE',
'Maximum model space distance between geometric entities at asserted c
onnectivities');
#459201=UNCERTAINTY_MEASURE_WITH_UNIT(LENGTH_MEASURE(0.01),#459243,
'DISTANCE_ACCURACY_VALUE',
'Maximum model space distance between geometric entities at asserted c
onnectivities');
#459202=UNCERTAINTY_MEASURE_WITH_UNIT(LENGTH_MEASURE(0.01),#459243,
'DISTANCE_ACCURACY_VALUE',
'Maximum model space distance between geometric entities at asserted c
onnectivities');
#459203=UNCERTAINTY_MEASURE_WITH_UNIT(LENGTH_MEASURE(0.01),#459243,
'DISTANCE_ACCURACY_VALUE',
'Maximum model space distance between geometric entities at asserted c
onnectivities');
#459204=UNCERTAINTY_MEASURE_WITH_UNIT(LENGTH_MEASURE(0.01),#459243,
'DISTANCE_ACCURACY_VALUE',
'Maximum model space distance between geometric entities at asserted c
onnectivities');
#459205=UNCERTAINTY_MEASURE_WITH_UNIT(LENGTH_MEASURE(0.01),#459243,
'DISTANCE_ACCURACY_VALUE',
'Maximum model space distance between geometric entities at asserted c
onnectivities');
#459206=UNCERTAINTY_MEASURE_WITH_UNIT(LENGTH_MEASURE(0.01),#459243,
'DISTANCE_ACCURACY_VALUE',
'Maximum model space distance between geometric entities at asserted c
onnectivities');
#459207=UNCERTAINTY_MEASURE_WITH_UNIT(LENGTH_MEASURE(0.01),#459243,
'DISTANCE_ACCURACY_VALUE',
'Maximum model space distance between geometric entities at asserted c
onnectivities');
#459208=UNCERTAINTY_MEASURE_WITH_UNIT(LENGTH_MEASURE(0.01),#459243,
'DISTANCE_ACCURACY_VALUE',
'Maximum model space distance between geometric entities at asserted c
onnectivities');
#459209=UNCERTAINTY_MEASURE_WITH_UNIT(LENGTH_MEASURE(0.01),#459243,
'DISTANCE_ACCURACY_VALUE',
'Maximum model space distance between geometric entities at asserted c
onnectivities');
#459210=UNCERTAINTY_MEASURE_WITH_UNIT(LENGTH_MEASURE(0.01),#459243,
'DISTANCE_ACCURACY_VALUE',
'Maximum model space distance between geometric entities at asserted c
onnectivities');
#459211=UNCERTAINTY_MEASURE_WITH_UNIT(LENGTH_MEASURE(0.01),#459243,
'DISTANCE_ACCURACY_VALUE',
'Maximum model space distance between geometric entities at asserted c
onnectivities');
#459212=UNCERTAINTY_MEASURE_WITH_UNIT(LENGTH_MEASURE(0.01),#459243,
'DISTANCE_ACCURACY_VALUE',
'Maximum model space distance between geometric entities at asserted c
onnectivities');
#459213=UNCERTAINTY_MEASURE_WITH_UNIT(LENGTH_MEASURE(0.01),#459243,
'DISTANCE_ACCURACY_VALUE',
'Maximum model space distance between geometric entities at asserted c
onnectivities');
#459214=UNCERTAINTY_MEASURE_WITH_UNIT(LENGTH_MEASURE(0.01),#459243,
'DISTANCE_ACCURACY_VALUE',
'Maximum model space distance between geometric entities at asserted c
onnectivities');
#459215=UNCERTAINTY_MEASURE_WITH_UNIT(LENGTH_MEASURE(0.01),#459243,
'DISTANCE_ACCURACY_VALUE',
'Maximum model space distance between geometric entities at asserted c
onnectivities');
#459216=UNCERTAINTY_MEASURE_WITH_UNIT(LENGTH_MEASURE(0.01),#459243,
'DISTANCE_ACCURACY_VALUE',
'Maximum model space distance between geometric entities at asserted c
onnectivities');
#459217=(
GEOMETRIC_REPRESENTATION_CONTEXT(3)
GLOBAL_UNCERTAINTY_ASSIGNED_CONTEXT((#459191))
GLOBAL_UNIT_ASSIGNED_CONTEXT((#459243,#459245,#459246))
REPRESENTATION_CONTEXT('','3D')
);
#459218=(
GEOMETRIC_REPRESENTATION_CONTEXT(3)
GLOBAL_UNCERTAINTY_ASSIGNED_CONTEXT((#459192))
GLOBAL_UNIT_ASSIGNED_CONTEXT((#459243,#459245,#459246))
REPRESENTATION_CONTEXT('','3D')
);
#459219=(
GEOMETRIC_REPRESENTATION_CONTEXT(3)
GLOBAL_UNCERTAINTY_ASSIGNED_CONTEXT((#459193))
GLOBAL_UNIT_ASSIGNED_CONTEXT((#459243,#459245,#459246))
REPRESENTATION_CONTEXT('','3D')
);
#459220=(
GEOMETRIC_REPRESENTATION_CONTEXT(3)
GLOBAL_UNCERTAINTY_ASSIGNED_CONTEXT((#459194))
GLOBAL_UNIT_ASSIGNED_CONTEXT((#459243,#459245,#459246))
REPRESENTATION_CONTEXT('','3D')
);
#459221=(
GEOMETRIC_REPRESENTATION_CONTEXT(3)
GLOBAL_UNCERTAINTY_ASSIGNED_CONTEXT((#459195))
GLOBAL_UNIT_ASSIGNED_CONTEXT((#459243,#459245,#459246))
REPRESENTATION_CONTEXT('','3D')
);
#459222=(
GEOMETRIC_REPRESENTATION_CONTEXT(3)
GLOBAL_UNCERTAINTY_ASSIGNED_CONTEXT((#459196))
GLOBAL_UNIT_ASSIGNED_CONTEXT((#459243,#459245,#459246))
REPRESENTATION_CONTEXT('','3D')
);
#459223=(
GEOMETRIC_REPRESENTATION_CONTEXT(3)
GLOBAL_UNCERTAINTY_ASSIGNED_CONTEXT((#459197))
GLOBAL_UNIT_ASSIGNED_CONTEXT((#459243,#459245,#459246))
REPRESENTATION_CONTEXT('','3D')
);
#459224=(
GEOMETRIC_REPRESENTATION_CONTEXT(3)
GLOBAL_UNCERTAINTY_ASSIGNED_CONTEXT((#459198))
GLOBAL_UNIT_ASSIGNED_CONTEXT((#459243,#459245,#459246))
REPRESENTATION_CONTEXT('','3D')
);
#459225=(
GEOMETRIC_REPRESENTATION_CONTEXT(3)
GLOBAL_UNCERTAINTY_ASSIGNED_CONTEXT((#459199))
GLOBAL_UNIT_ASSIGNED_CONTEXT((#459243,#459245,#459246))
REPRESENTATION_CONTEXT('','3D')
);
#459226=(
GEOMETRIC_REPRESENTATION_CONTEXT(3)
GLOBAL_UNCERTAINTY_ASSIGNED_CONTEXT((#459200))
GLOBAL_UNIT_ASSIGNED_CONTEXT((#459243,#459245,#459246))
REPRESENTATION_CONTEXT('','3D')
);
#459227=(
GEOMETRIC_REPRESENTATION_CONTEXT(3)
GLOBAL_UNCERTAINTY_ASSIGNED_CONTEXT((#459201))
GLOBAL_UNIT_ASSIGNED_CONTEXT((#459243,#459245,#459246))
REPRESENTATION_CONTEXT('','3D')
);
#459228=(
GEOMETRIC_REPRESENTATION_CONTEXT(3)
GLOBAL_UNCERTAINTY_ASSIGNED_CONTEXT((#459202))
GLOBAL_UNIT_ASSIGNED_CONTEXT((#459243,#459245,#459246))
REPRESENTATION_CONTEXT('','3D')
);
#459229=(
GEOMETRIC_REPRESENTATION_CONTEXT(3)
GLOBAL_UNCERTAINTY_ASSIGNED_CONTEXT((#459203))
GLOBAL_UNIT_ASSIGNED_CONTEXT((#459243,#459245,#459246))
REPRESENTATION_CONTEXT('','3D')
);
#459230=(
GEOMETRIC_REPRESENTATION_CONTEXT(3)
GLOBAL_UNCERTAINTY_ASSIGNED_CONTEXT((#459204))
GLOBAL_UNIT_ASSIGNED_CONTEXT((#459243,#459245,#459246))
REPRESENTATION_CONTEXT('','3D')
);
#459231=(
GEOMETRIC_REPRESENTATION_CONTEXT(3)
GLOBAL_UNCERTAINTY_ASSIGNED_CONTEXT((#459205))
GLOBAL_UNIT_ASSIGNED_CONTEXT((#459243,#459245,#459246))
REPRESENTATION_CONTEXT('','3D')
);
#459232=(
GEOMETRIC_REPRESENTATION_CONTEXT(3)
GLOBAL_UNCERTAINTY_ASSIGNED_CONTEXT((#459206))
GLOBAL_UNIT_ASSIGNED_CONTEXT((#459243,#459245,#459246))
REPRESENTATION_CONTEXT('','3D')
);
#459233=(
GEOMETRIC_REPRESENTATION_CONTEXT(3)
GLOBAL_UNCERTAINTY_ASSIGNED_CONTEXT((#459207))
GLOBAL_UNIT_ASSIGNED_CONTEXT((#459243,#459245,#459246))
REPRESENTATION_CONTEXT('','3D')
);
#459234=(
GEOMETRIC_REPRESENTATION_CONTEXT(3)
GLOBAL_UNCERTAINTY_ASSIGNED_CONTEXT((#459208))
GLOBAL_UNIT_ASSIGNED_CONTEXT((#459243,#459245,#459246))
REPRESENTATION_CONTEXT('','3D')
);
#459235=(
GEOMETRIC_REPRESENTATION_CONTEXT(3)
GLOBAL_UNCERTAINTY_ASSIGNED_CONTEXT((#459209))
GLOBAL_UNIT_ASSIGNED_CONTEXT((#459243,#459245,#459246))
REPRESENTATION_CONTEXT('','3D')
);
#459236=(
GEOMETRIC_REPRESENTATION_CONTEXT(3)
GLOBAL_UNCERTAINTY_ASSIGNED_CONTEXT((#459210))
GLOBAL_UNIT_ASSIGNED_CONTEXT((#459243,#459245,#459246))
REPRESENTATION_CONTEXT('','3D')
);
#459237=(
GEOMETRIC_REPRESENTATION_CONTEXT(3)
GLOBAL_UNCERTAINTY_ASSIGNED_CONTEXT((#459211))
GLOBAL_UNIT_ASSIGNED_CONTEXT((#459243,#459245,#459246))
REPRESENTATION_CONTEXT('','3D')
);
#459238=(
GEOMETRIC_REPRESENTATION_CONTEXT(3)
GLOBAL_UNCERTAINTY_ASSIGNED_CONTEXT((#459212))
GLOBAL_UNIT_ASSIGNED_CONTEXT((#459243,#459245,#459246))
REPRESENTATION_CONTEXT('','3D')
);
#459239=(
GEOMETRIC_REPRESENTATION_CONTEXT(3)
GLOBAL_UNCERTAINTY_ASSIGNED_CONTEXT((#459213))
GLOBAL_UNIT_ASSIGNED_CONTEXT((#459243,#459245,#459246))
REPRESENTATION_CONTEXT('','3D')
);
#459240=(
GEOMETRIC_REPRESENTATION_CONTEXT(3)
GLOBAL_UNCERTAINTY_ASSIGNED_CONTEXT((#459214))
GLOBAL_UNIT_ASSIGNED_CONTEXT((#459243,#459245,#459246))
REPRESENTATION_CONTEXT('','3D')
);
#459241=(
GEOMETRIC_REPRESENTATION_CONTEXT(3)
GLOBAL_UNCERTAINTY_ASSIGNED_CONTEXT((#459215))
GLOBAL_UNIT_ASSIGNED_CONTEXT((#459243,#459245,#459246))
REPRESENTATION_CONTEXT('','3D')
);
#459242=(
GEOMETRIC_REPRESENTATION_CONTEXT(3)
GLOBAL_UNCERTAINTY_ASSIGNED_CONTEXT((#459216))
GLOBAL_UNIT_ASSIGNED_CONTEXT((#459243,#459245,#459246))
REPRESENTATION_CONTEXT('','3D')
);
#459243=(
LENGTH_UNIT()
NAMED_UNIT(*)
SI_UNIT(.MILLI.,.METRE.)
);
#459244=(
LENGTH_UNIT()
NAMED_UNIT(*)
SI_UNIT($,.METRE.)
);
#459245=(
NAMED_UNIT(*)
PLANE_ANGLE_UNIT()
SI_UNIT($,.RADIAN.)
);
#459246=(
NAMED_UNIT(*)
SI_UNIT($,.STERADIAN.)
SOLID_ANGLE_UNIT()
);
#459247=SHAPE_DEFINITION_REPRESENTATION(#459272,#459328);
#459248=SHAPE_DEFINITION_REPRESENTATION(#459273,#459329);
#459249=SHAPE_DEFINITION_REPRESENTATION(#459274,#459330);
#459250=SHAPE_DEFINITION_REPRESENTATION(#459275,#459331);
#459251=SHAPE_DEFINITION_REPRESENTATION(#459276,#459332);
#459252=SHAPE_DEFINITION_REPRESENTATION(#459277,#459333);
#459253=SHAPE_DEFINITION_REPRESENTATION(#459278,#459334);
#459254=SHAPE_DEFINITION_REPRESENTATION(#459279,#459335);
#459255=SHAPE_DEFINITION_REPRESENTATION(#459280,#459336);
#459256=SHAPE_DEFINITION_REPRESENTATION(#459281,#459337);
#459257=SHAPE_DEFINITION_REPRESENTATION(#459282,#459338);
#459258=SHAPE_DEFINITION_REPRESENTATION(#459283,#459339);
#459259=SHAPE_DEFINITION_REPRESENTATION(#459284,#459340);
#459260=SHAPE_DEFINITION_REPRESENTATION(#459285,#459341);
#459261=SHAPE_DEFINITION_REPRESENTATION(#459288,#459342);
#459262=SHAPE_DEFINITION_REPRESENTATION(#459289,#459343);
#459263=SHAPE_DEFINITION_REPRESENTATION(#459290,#459344);
#459264=SHAPE_DEFINITION_REPRESENTATION(#459291,#459345);
#459265=SHAPE_DEFINITION_REPRESENTATION(#459292,#459346);
#459266=SHAPE_DEFINITION_REPRESENTATION(#459293,#459347);
#459267=SHAPE_DEFINITION_REPRESENTATION(#459294,#459348);
#459268=SHAPE_DEFINITION_REPRESENTATION(#459295,#459349);
#459269=SHAPE_DEFINITION_REPRESENTATION(#459296,#459350);
#459270=SHAPE_DEFINITION_REPRESENTATION(#459297,#459351);
#459271=SHAPE_DEFINITION_REPRESENTATION(#459298,#459352);
#459272=PRODUCT_DEFINITION_SHAPE('',$,#459354);
#459273=PRODUCT_DEFINITION_SHAPE('',$,#459355);
#459274=PRODUCT_DEFINITION_SHAPE('',$,#459356);
#459275=PRODUCT_DEFINITION_SHAPE('',$,#459357);
#459276=PRODUCT_DEFINITION_SHAPE('',$,#459358);
#459277=PRODUCT_DEFINITION_SHAPE('',$,#459359);
#459278=PRODUCT_DEFINITION_SHAPE('',$,#459360);
#459279=PRODUCT_DEFINITION_SHAPE('',$,#459361);
#459280=PRODUCT_DEFINITION_SHAPE('',$,#459362);
#459281=PRODUCT_DEFINITION_SHAPE('',$,#459363);
#459282=PRODUCT_DEFINITION_SHAPE('',$,#459364);
#459283=PRODUCT_DEFINITION_SHAPE('',$,#459365);
#459284=PRODUCT_DEFINITION_SHAPE('',$,#459366);
#459285=PRODUCT_DEFINITION_SHAPE('',$,#459367);
#459286=PRODUCT_DEFINITION_SHAPE($,$,#104);
#459287=PRODUCT_DEFINITION_SHAPE($,$,#105);
#459288=PRODUCT_DEFINITION_SHAPE('',$,#459368);
#459289=PRODUCT_DEFINITION_SHAPE('',$,#459369);
#459290=PRODUCT_DEFINITION_SHAPE('',$,#459370);
#459291=PRODUCT_DEFINITION_SHAPE('',$,#459371);
#459292=PRODUCT_DEFINITION_SHAPE('',$,#459372);
#459293=PRODUCT_DEFINITION_SHAPE('',$,#459373);
#459294=PRODUCT_DEFINITION_SHAPE('',$,#459374);
#459295=PRODUCT_DEFINITION_SHAPE('',$,#459375);
#459296=PRODUCT_DEFINITION_SHAPE('',$,#459376);
#459297=PRODUCT_DEFINITION_SHAPE('',$,#459377);
#459298=PRODUCT_DEFINITION_SHAPE('',$,#459378);
#459299=PRODUCT_DEFINITION_SHAPE($,$,#106);
#459300=PRODUCT_DEFINITION_SHAPE($,$,#107);
#459301=PRODUCT_DEFINITION_SHAPE($,$,#108);
#459302=PRODUCT_DEFINITION_SHAPE($,$,#109);
#459303=PRODUCT_DEFINITION_SHAPE($,$,#110);
#459304=PRODUCT_DEFINITION_SHAPE($,$,#111);
#459305=PRODUCT_DEFINITION_SHAPE($,$,#112);
#459306=PRODUCT_DEFINITION_SHAPE($,$,#113);
#459307=PRODUCT_DEFINITION_SHAPE($,$,#114);
#459308=PRODUCT_DEFINITION_SHAPE($,$,#115);
#459309=PRODUCT_DEFINITION_SHAPE($,$,#116);
#459310=PRODUCT_DEFINITION_SHAPE($,$,#117);
#459311=PRODUCT_DEFINITION_SHAPE($,$,#118);
#459312=PRODUCT_DEFINITION_SHAPE($,$,#119);
#459313=PRODUCT_DEFINITION_SHAPE($,$,#120);
#459314=PRODUCT_DEFINITION_SHAPE($,$,#121);
#459315=PRODUCT_DEFINITION_SHAPE($,$,#122);
#459316=PRODUCT_DEFINITION_SHAPE($,$,#123);
#459317=PRODUCT_DEFINITION_SHAPE($,$,#124);
#459318=PRODUCT_DEFINITION_SHAPE($,$,#125);
#459319=PRODUCT_DEFINITION_SHAPE($,$,#126);
#459320=PRODUCT_DEFINITION_SHAPE($,$,#127);
#459321=PRODUCT_DEFINITION_SHAPE($,$,#128);
#459322=PRODUCT_DEFINITION_SHAPE($,$,#129);
#459323=PRODUCT_DEFINITION_SHAPE($,$,#130);
#459324=PRODUCT_DEFINITION_SHAPE($,$,#131);
#459325=PRODUCT_DEFINITION_SHAPE($,$,#132);
#459326=PRODUCT_DEFINITION_SHAPE($,$,#133);
#459327=PRODUCT_DEFINITION_SHAPE($,$,#134);
#459328=SHAPE_REPRESENTATION('',(#94904,#105574),#459217);
#459329=SHAPE_REPRESENTATION('',(#94905,#105551,#105552,#105553,#105554,
#105555,#105556,#105557,#105558,#105559,#105560,#105561,#105562,#105563,
#105564,#105565,#105566,#105567,#105568,#105569,#105570,#105571,#105572,
#105573),#459218);
#459330=SHAPE_REPRESENTATION('',(#94906),#459219);
#459331=SHAPE_REPRESENTATION('',(#95243),#459220);
#459332=SHAPE_REPRESENTATION('',(#95341),#459221);
#459333=SHAPE_REPRESENTATION('',(#97093),#459222);
#459334=SHAPE_REPRESENTATION('',(#97223),#459223);
#459335=SHAPE_REPRESENTATION('',(#97233),#459224);
#459336=SHAPE_REPRESENTATION('',(#97243),#459225);
#459337=SHAPE_REPRESENTATION('',(#98432),#459226);
#459338=SHAPE_REPRESENTATION('',(#98856),#459227);
#459339=SHAPE_REPRESENTATION('',(#99051,#99169,#99170),#459228);
#459340=SHAPE_REPRESENTATION('',(#99052),#459229);
#459341=SHAPE_REPRESENTATION('',(#99154),#459230);
#459342=SHAPE_REPRESENTATION('',(#99171),#459231);
#459343=SHAPE_REPRESENTATION('',(#99248),#459232);
#459344=SHAPE_REPRESENTATION('',(#99318),#459233);
#459345=SHAPE_REPRESENTATION('',(#99385),#459234);
#459346=SHAPE_REPRESENTATION('',(#102648),#459235);
#459347=SHAPE_REPRESENTATION('',(#105174,#105546,#105547,#105548,#105549,
#105550),#459236);
#459348=SHAPE_REPRESENTATION('',(#105175),#459237);
#459349=SHAPE_REPRESENTATION('',(#105363),#459238);
#459350=SHAPE_REPRESENTATION('',(#105431),#459239);
#459351=SHAPE_REPRESENTATION('',(#105440),#459240);
#459352=SHAPE_REPRESENTATION('',(#105494),#459241);
#459353=PRODUCT_DEFINITION_CONTEXT('part definition',#459430,'design');
#459354=PRODUCT_DEFINITION('MAT-056',
'MAT-056',#459379,#459353);
#459355=PRODUCT_DEFINITION('EX-3D Direct Drive Extruder Assembly',
'Filament Drive System',#459380,#459353);
#459356=PRODUCT_DEFINITION('Stepper Motor','Stepper Motor',#459381,#459353);
#459357=PRODUCT_DEFINITION('Pneumatic Adapter','Pneumatic Adapter',#459382,
#459353);
#459358=PRODUCT_DEFINITION('Extruder Housing and Cover',
'Extruder Housing and Cover',#459383,#459353);
#459359=PRODUCT_DEFINITION('Tension Rocker Arm','Tension Rocker Arm',#459384,
#459353);
#459360=PRODUCT_DEFINITION('Rocker Shaft','Rocker Shaft',#459385,#459353);
#459361=PRODUCT_DEFINITION('Drive Shaft','Drive Shaft',#459386,#459353);
#459362=PRODUCT_DEFINITION('Filament Drive Gear','Filament Drive Gear',
#459387,#459353);
#459363=PRODUCT_DEFINITION('Main Reduction Gear','Main Reduction Gear',
#459388,#459353);
#459364=PRODUCT_DEFINITION('Needle Bearing','Needle Bearing',#459389,#459353);
#459365=PRODUCT_DEFINITION('Tension Adjustment Set',
'Tension Adjustment Set',#459390,#459353);
#459366=PRODUCT_DEFINITION('Flanged Screw M3x16','Flanged Screw M3x16',
#459391,#459353);
#459367=PRODUCT_DEFINITION('Compression Spring 0.8x5x10',
'Compression Spring 0.8x5x10',#459392,#459353);
#459368=PRODUCT_DEFINITION('Shaft Ball Bearing','Shaft Ball Bearing',#459393,
#459353);
#459369=PRODUCT_DEFINITION('Assembly Screw 1','Assembly Screw 1',#459394,
#459353);
#459370=PRODUCT_DEFINITION('Housing Fastener','Housing Fastener',#459395,
#459353);
#459371=PRODUCT_DEFINITION('Assembly Screw 2','Assembly Screw 2',#459396,
#459353);
#459372=PRODUCT_DEFINITION('Assembly Screw 3','Assembly Screw 3',#459397,
#459353);
#459373=PRODUCT_DEFINITION('Hotend Subassembly','Hotend Subassembly',#459398,
#459353);
#459374=PRODUCT_DEFINITION('Hotend Heatsink','Hotend Heatsink',#459399,
#459353);
#459375=PRODUCT_DEFINITION('Hotend Heatbreak','Hotend Heatbreak',#459400,
#459353);
#459376=PRODUCT_DEFINITION('Hotend PTFE Tube','Hotend PTFE Tube',#459401,
#459353);
#459377=PRODUCT_DEFINITION('Hotend Nozzle','Hotend Nozzle',#459402,#459353);
#459378=PRODUCT_DEFINITION('Hotend Heater Block','Hotend Heater Block',
#459403,#459353);
#459379=PRODUCT_DEFINITION_FORMATION('',$,#459432);
#459380=PRODUCT_DEFINITION_FORMATION('',$,#459433);
#459381=PRODUCT_DEFINITION_FORMATION('',$,#459434);
#459382=PRODUCT_DEFINITION_FORMATION('',$,#459435);
#459383=PRODUCT_DEFINITION_FORMATION('',$,#459436);
#459384=PRODUCT_DEFINITION_FORMATION('',$,#459437);
#459385=PRODUCT_DEFINITION_FORMATION('',$,#459438);
#459386=PRODUCT_DEFINITION_FORMATION('',$,#459439);
#459387=PRODUCT_DEFINITION_FORMATION('',$,#459440);
#459388=PRODUCT_DEFINITION_FORMATION('',$,#459441);
#459389=PRODUCT_DEFINITION_FORMATION('',$,#459442);
#459390=PRODUCT_DEFINITION_FORMATION('',$,#459443);
#459391=PRODUCT_DEFINITION_FORMATION('',$,#459444);
#459392=PRODUCT_DEFINITION_FORMATION('',$,#459445);
#459393=PRODUCT_DEFINITION_FORMATION('',$,#459446);
#459394=PRODUCT_DEFINITION_FORMATION('',$,#459447);
#459395=PRODUCT_DEFINITION_FORMATION('',$,#459448);
#459396=PRODUCT_DEFINITION_FORMATION('',$,#459449);
#459397=PRODUCT_DEFINITION_FORMATION('',$,#459450);
#459398=PRODUCT_DEFINITION_FORMATION('',$,#459451);
#459399=PRODUCT_DEFINITION_FORMATION('',$,#459452);
#459400=PRODUCT_DEFINITION_FORMATION('',$,#459453);
#459401=PRODUCT_DEFINITION_FORMATION('',$,#459454);
#459402=PRODUCT_DEFINITION_FORMATION('',$,#459455);
#459403=PRODUCT_DEFINITION_FORMATION('',$,#459456);
#459404=PRODUCT_RELATED_PRODUCT_CATEGORY('MAT-056',
'MAT-056',(#459432));
#459405=PRODUCT_RELATED_PRODUCT_CATEGORY('Filament Drive System',
'Filament Drive System',(#459433));
#459406=PRODUCT_RELATED_PRODUCT_CATEGORY('Stepper Motor',
'Stepper Motor',(#459434));
#459407=PRODUCT_RELATED_PRODUCT_CATEGORY('Pneumatic Adapter',
'Pneumatic Adapter',(#459435));
#459408=PRODUCT_RELATED_PRODUCT_CATEGORY('Extruder Housing and Cover',
'Extruder Housing and Cover',(#459436));
#459409=PRODUCT_RELATED_PRODUCT_CATEGORY('Tension Rocker Arm',
'Tension Rocker Arm',(#459437));
#459410=PRODUCT_RELATED_PRODUCT_CATEGORY('Rocker Shaft','Rocker Shaft',
(#459438));
#459411=PRODUCT_RELATED_PRODUCT_CATEGORY('Drive Shaft','Drive Shaft',(#459439));
#459412=PRODUCT_RELATED_PRODUCT_CATEGORY('Filament Drive Gear',
'Filament Drive Gear',(#459440));
#459413=PRODUCT_RELATED_PRODUCT_CATEGORY('Main Reduction Gear',
'Main Reduction Gear',(#459441));
#459414=PRODUCT_RELATED_PRODUCT_CATEGORY('Needle Bearing',
'Needle Bearing',(#459442));
#459415=PRODUCT_RELATED_PRODUCT_CATEGORY('Tension Adjustment Set',
'Tension Adjustment Set',(#459443));
#459416=PRODUCT_RELATED_PRODUCT_CATEGORY('Flanged Screw M3x16',
'Flanged Screw M3x16',(#459444));
#459417=PRODUCT_RELATED_PRODUCT_CATEGORY('Compression Spring 0.8x5x10',
'Compression Spring 0.8x5x10',(#459445));
#459418=PRODUCT_RELATED_PRODUCT_CATEGORY('Shaft Ball Bearing',
'Shaft Ball Bearing',(#459446));
#459419=PRODUCT_RELATED_PRODUCT_CATEGORY('Assembly Screw 1',
'Assembly Screw 1',(#459447));
#459420=PRODUCT_RELATED_PRODUCT_CATEGORY('Housing Fastener',
'Housing Fastener',(#459448));
#459421=PRODUCT_RELATED_PRODUCT_CATEGORY('Assembly Screw 2',
'Assembly Screw 2',(#459449));
#459422=PRODUCT_RELATED_PRODUCT_CATEGORY('Assembly Screw 3',
'Assembly Screw 3',(#459450));
#459423=PRODUCT_RELATED_PRODUCT_CATEGORY('Hotend Subassembly',
'Hotend Subassembly',(#459451));
#459424=PRODUCT_RELATED_PRODUCT_CATEGORY('Hotend Heatsink',
'Hotend Heatsink',(#459452));
#459425=PRODUCT_RELATED_PRODUCT_CATEGORY('Hotend Heatbreak',
'Hotend Heatbreak',(#459453));
#459426=PRODUCT_RELATED_PRODUCT_CATEGORY('Hotend PTFE Tube',
'Hotend PTFE Tube',(#459454));
#459427=PRODUCT_RELATED_PRODUCT_CATEGORY('Hotend Nozzle',
'Hotend Nozzle',(#459455));
#459428=PRODUCT_RELATED_PRODUCT_CATEGORY('Hotend Heater Block',
'Hotend Heater Block',(#459456));
#459429=APPLICATION_PROTOCOL_DEFINITION('international standard',
'automotive_design',2009,#459430);
#459430=APPLICATION_CONTEXT(
'Core Data for Automotive Mechanical Design Process');
#459431=PRODUCT_CONTEXT('part definition',#459430,'mechanical');
#459432=PRODUCT('MAT-056','MAT-056',
$,(#459431));
#459433=PRODUCT('EX-3D Direct Drive Extruder Assembly',
'Filament Drive System',$,(#459431));
#459434=PRODUCT('Stepper Motor','Stepper Motor',$,(#459431));
#459435=PRODUCT('Pneumatic Adapter','Pneumatic Adapter',$,(#459431));
#459436=PRODUCT('Extruder Housing and Cover',
'Extruder Housing and Cover',$,(#459431));
#459437=PRODUCT('Tension Rocker Arm','Tension Rocker Arm',$,(#459431));
#459438=PRODUCT('Rocker Shaft','Rocker Shaft',$,(#459431));
#459439=PRODUCT('Drive Shaft','Drive Shaft',$,(#459431));
#459440=PRODUCT('Filament Drive Gear','Filament Drive Gear',$,(#459431));
#459441=PRODUCT('Main Reduction Gear','Main Reduction Gear',$,(#459431));
#459442=PRODUCT('Needle Bearing','Needle Bearing',$,(#459431));
#459443=PRODUCT('Tension Adjustment Set','Tension Adjustment Set',$,(#459431));
#459444=PRODUCT('Flanged Screw M3x16','Flanged Screw M3x16',$,(#459431));
#459445=PRODUCT('Compression Spring 0.8x5x10',
'Compression Spring 0.8x5x10',$,(#459431));
#459446=PRODUCT('Shaft Ball Bearing','Shaft Ball Bearing',$,(#459431));
#459447=PRODUCT('Assembly Screw 1','Assembly Screw 1',$,(#459431));
#459448=PRODUCT('Housing Fastener','Housing Fastener',$,(#459431));
#459449=PRODUCT('Assembly Screw 2','Assembly Screw 2',$,(#459431));
#459450=PRODUCT('Assembly Screw 3','Assembly Screw 3',$,(#459431));
#459451=PRODUCT('Hotend Subassembly','Hotend Subassembly',$,(#459431));
#459452=PRODUCT('Hotend Heatsink','Hotend Heatsink',$,(#459431));
#459453=PRODUCT('Hotend Heatbreak','Hotend Heatbreak',$,(#459431));
#459454=PRODUCT('Hotend PTFE Tube','Hotend PTFE Tube',$,(#459431));
#459455=PRODUCT('Hotend Nozzle','Hotend Nozzle',$,(#459431));
#459456=PRODUCT('Hotend Heater Block','Hotend Heater Block',$,(#459431));
#459457=PRESENTATION_STYLE_ASSIGNMENT((#459463));
#459458=PRESENTATION_STYLE_ASSIGNMENT((#459464));
#459459=PRESENTATION_STYLE_ASSIGNMENT((#459465));
#459460=PRESENTATION_STYLE_ASSIGNMENT((#459466));
#459461=PRESENTATION_STYLE_ASSIGNMENT((#459467));
#459462=PRESENTATION_STYLE_ASSIGNMENT((#459468));
#459463=SURFACE_STYLE_USAGE(.BOTH.,#459469);
#459464=SURFACE_STYLE_USAGE(.BOTH.,#459470);
#459465=SURFACE_STYLE_USAGE(.BOTH.,#459471);
#459466=SURFACE_STYLE_USAGE(.BOTH.,#459472);
#459467=SURFACE_STYLE_USAGE(.BOTH.,#459473);
#459468=SURFACE_STYLE_USAGE(.BOTH.,#459474);
#459469=SURFACE_SIDE_STYLE('',(#459475));
#459470=SURFACE_SIDE_STYLE('',(#459476));
#459471=SURFACE_SIDE_STYLE('',(#459477));
#459472=SURFACE_SIDE_STYLE('',(#459478));
#459473=SURFACE_SIDE_STYLE('',(#459479));
#459474=SURFACE_SIDE_STYLE('',(#459480));
#459475=SURFACE_STYLE_FILL_AREA(#459481);
#459476=SURFACE_STYLE_FILL_AREA(#459482);
#459477=SURFACE_STYLE_FILL_AREA(#459483);
#459478=SURFACE_STYLE_FILL_AREA(#459484);
#459479=SURFACE_STYLE_FILL_AREA(#459485);
#459480=SURFACE_STYLE_FILL_AREA(#459486);
#459481=FILL_AREA_STYLE('Steel - Satin',(#459487));
#459482=FILL_AREA_STYLE('Paint - Enamel Glossy (Black)',(#459488));
#459483=FILL_AREA_STYLE('Aluminum - Polished',(#459489));
#459484=FILL_AREA_STYLE('Brass - Polished',(#459490));
#459485=FILL_AREA_STYLE('Stainless Steel - Polished',(#459491));
#459486=FILL_AREA_STYLE('Paint - Enamel Glossy (Grey)',(#459492));
#459487=FILL_AREA_STYLE_COLOUR('Steel - Satin',#459493);
#459488=FILL_AREA_STYLE_COLOUR('Paint - Enamel Glossy (Black)',#459494);
#459489=FILL_AREA_STYLE_COLOUR('Aluminum - Polished',#459495);
#459490=FILL_AREA_STYLE_COLOUR('Brass - Polished',#459496);
#459491=FILL_AREA_STYLE_COLOUR('Stainless Steel - Polished',#459497);
#459492=FILL_AREA_STYLE_COLOUR('Paint - Enamel Glossy (Grey)',#459498);
#459493=COLOUR_RGB('Steel - Satin',0.627450980392157,0.627450980392157,
0.627450980392157);
#459494=COLOUR_RGB('Paint - Enamel Glossy (Black)',0.0980392156862745,0.0980392156862745,
0.0980392156862745);
#459495=COLOUR_RGB('Aluminum - Polished',0.96078431372549,0.96078431372549,
0.964705882352941);
#459496=COLOUR_RGB('Brass - Polished',0.952941176470588,0.796078431372549,
0.486274509803922);
#459497=COLOUR_RGB('Stainless Steel - Polished',0.796078431372549,0.796078431372549,
0.796078431372549);
#459498=COLOUR_RGB('Paint - Enamel Glossy (Grey)',0.525490196078431,0.525490196078431,
0.525490196078431);
#459499=COLOUR_RGB('Dark Blue',0.08,0.2,0.34);
#459500=FILL_AREA_STYLE_COLOUR('',#459499);
#459501=FILL_AREA_STYLE('',(#459500));
#459502=SURFACE_STYLE_FILL_AREA(#459501);
#459503=SURFACE_SIDE_STYLE('',(#459502));
#459504=SURFACE_STYLE_USAGE(.BOTH.,#459503);
#459505=PRESENTATION_STYLE_ASSIGNMENT((#459504));
#459506=COLOUR_RGB('Light Blue',0.38,0.62,0.78);
#459507=FILL_AREA_STYLE_COLOUR('',#459506);
#459508=FILL_AREA_STYLE('',(#459507));
#459509=SURFACE_STYLE_FILL_AREA(#459508);
#459510=SURFACE_SIDE_STYLE('',(#459509));
#459511=SURFACE_STYLE_USAGE(.BOTH.,#459510);
#459512=PRESENTATION_STYLE_ASSIGNMENT((#459511));
#459513=COLOUR_RGB('Sky Blue',0.24,0.69,0.87);
#459514=FILL_AREA_STYLE_COLOUR('',#459513);
#459515=FILL_AREA_STYLE('',(#459514));
#459516=SURFACE_STYLE_FILL_AREA(#459515);
#459517=SURFACE_SIDE_STYLE('',(#459516));
#459518=SURFACE_STYLE_USAGE(.BOTH.,#459517);
#459519=PRESENTATION_STYLE_ASSIGNMENT((#459518));
#459520=COLOUR_RGB('Grey',0.48,0.52,0.57);
#459521=FILL_AREA_STYLE_COLOUR('',#459520);
#459522=FILL_AREA_STYLE('',(#459521));
#459523=SURFACE_STYLE_FILL_AREA(#459522);
#459524=SURFACE_SIDE_STYLE('',(#459523));
#459525=SURFACE_STYLE_USAGE(.BOTH.,#459524);
#459526=PRESENTATION_STYLE_ASSIGNMENT((#459525));
#459527=COLOUR_RGB('Black',0.12,0.14,0.17);
#459528=FILL_AREA_STYLE_COLOUR('',#459527);
#459529=FILL_AREA_STYLE('',(#459528));
#459530=SURFACE_STYLE_FILL_AREA(#459529);
#459531=SURFACE_SIDE_STYLE('',(#459530));
#459532=SURFACE_STYLE_USAGE(.BOTH.,#459531);
#459533=PRESENTATION_STYLE_ASSIGNMENT((#459532));
#459534=COLOUR_RGB('Off White',0.89,0.88,0.83);
#459535=FILL_AREA_STYLE_COLOUR('',#459534);
#459536=FILL_AREA_STYLE('',(#459535));
#459537=SURFACE_STYLE_FILL_AREA(#459536);
#459538=SURFACE_SIDE_STYLE('',(#459537));
#459539=SURFACE_STYLE_USAGE(.BOTH.,#459538);
#459540=PRESENTATION_STYLE_ASSIGNMENT((#459539));
ENDSEC;
END-ISO-10303-21;
